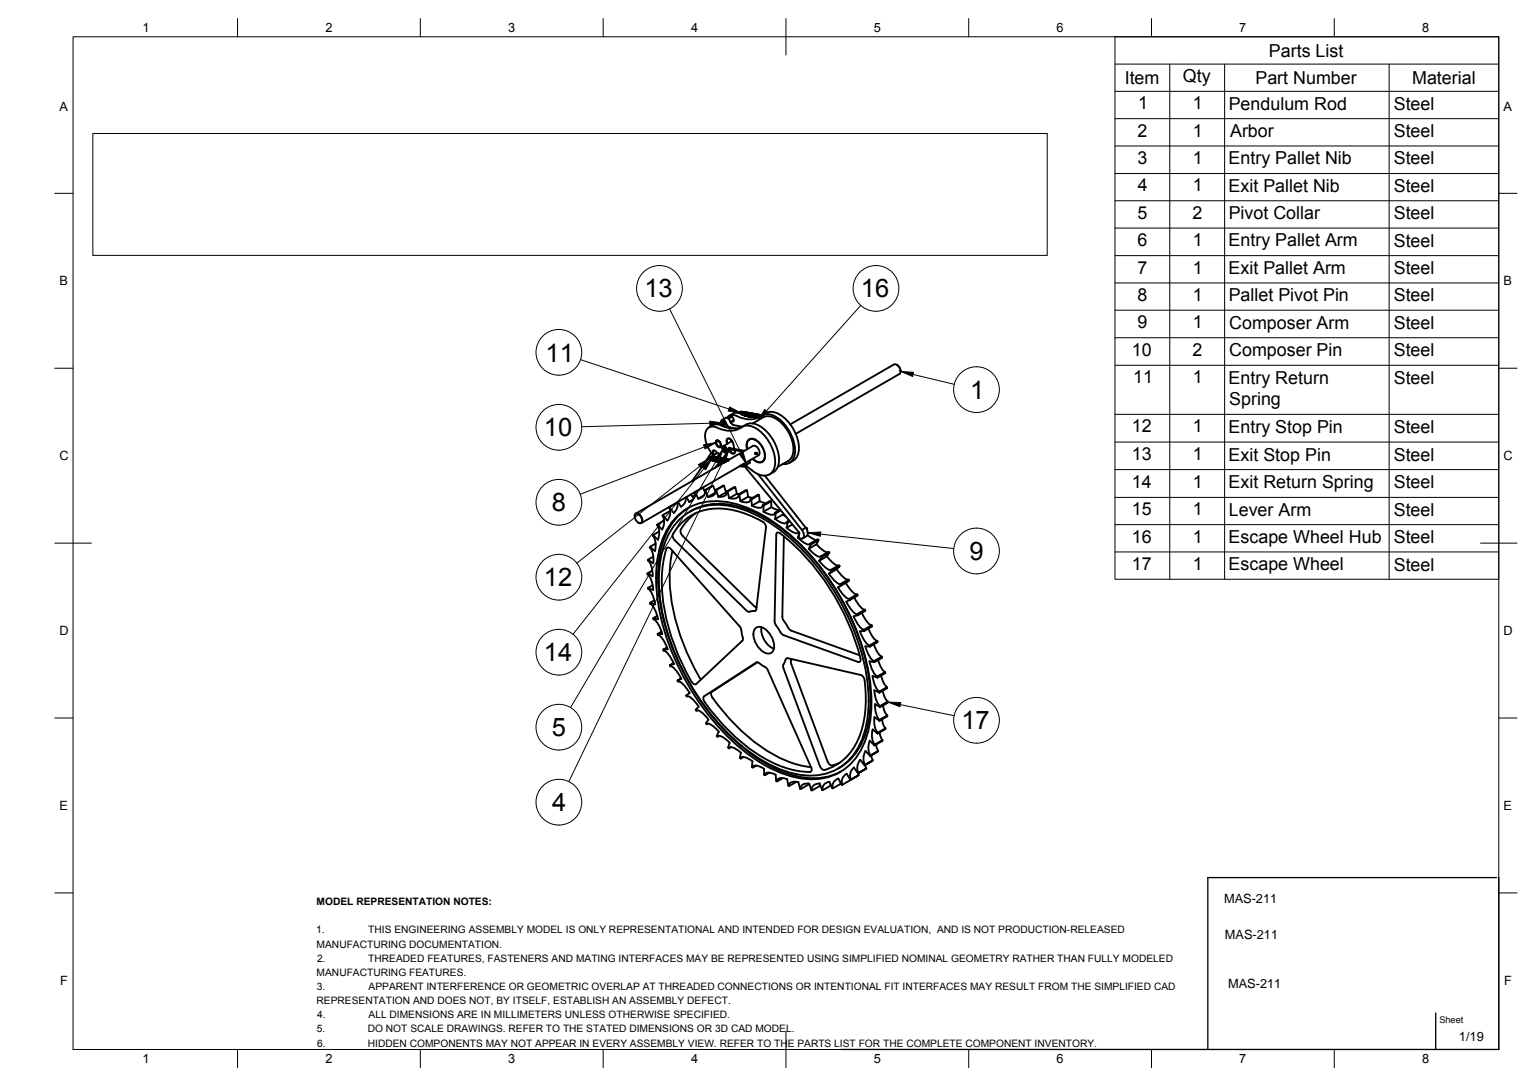
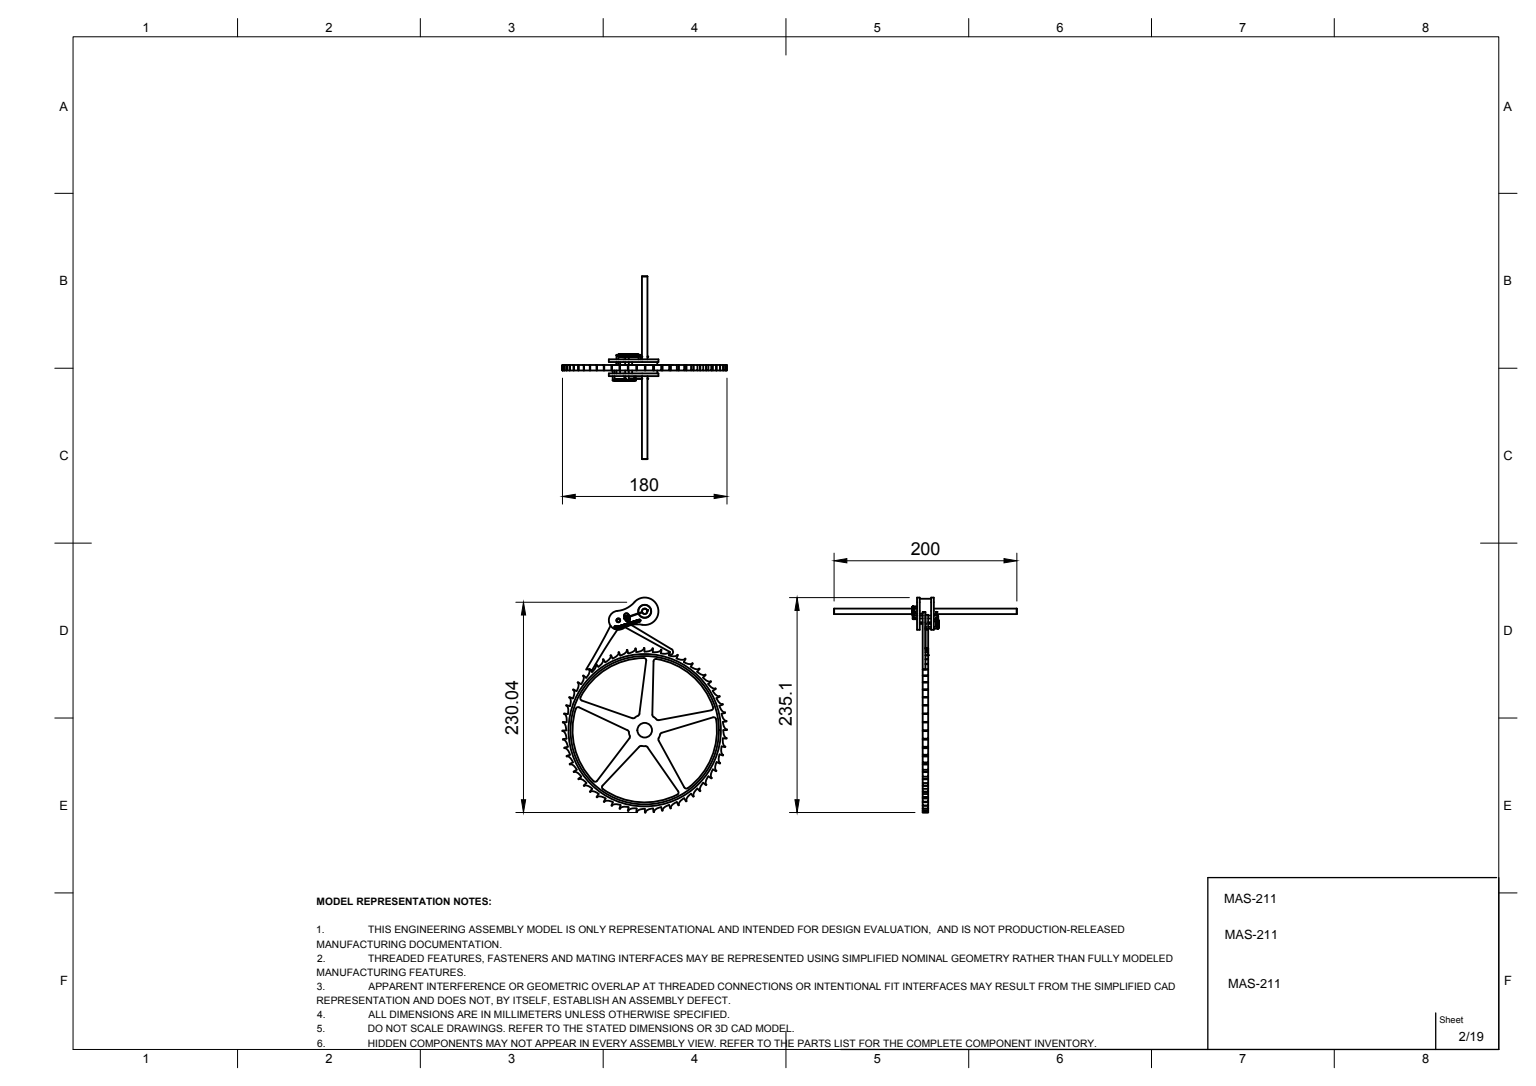
ISO-10303-21;
HEADER;
FILE_DESCRIPTION(
 (''),
 '2;1');
FILE_NAME ( 'MAS-211', '2026-10-05T20:07:59+06:00', ( '' ), ( '' ), 'STEP AP214', 'Unspecified', '' );
FILE_SCHEMA (('AUTOMOTIVE_DESIGN { 1 0 10303 214 3 1 1 }'));
ENDSEC;
DATA;
#10 = MECHANICAL_DESIGN_GEOMETRIC_PRESENTATION_REPRESENTATION('',(#319,#320,
#321,#322,#323,#324,#325,#326,#327,#328,#329,#330,#331,#332,#333,#334,#335,
#336,#337),#196741) ;
#17 = (
BOUNDED_CURVE()
B_SPLINE_CURVE(2,(#114139,#114140,#114141,#114142,#114143,#114144,#114145,
#114146,#114147),.UNSPECIFIED.,.F.,.F.)
B_SPLINE_CURVE_WITH_KNOTS((3,2,2,2,3),(1.42918797785348,1.62618617063892,
1.86180561965816,2.09742506867739,2.29442326146283),.UNSPECIFIED.)
CURVE()
GEOMETRIC_REPRESENTATION_ITEM()
RATIONAL_B_SPLINE_CURVE((1.,1.,1.,0.707106781186548,1.,0.707106781186548,
1.,1.,1.))
REPRESENTATION_ITEM('')
) ;
#18 = (
BOUNDED_CURVE()
B_SPLINE_CURVE(2,(#114327,#114328,#114329,#114330,#114331,#114332,#114333,
#114334,#114335),.UNSPECIFIED.,.F.,.F.)
B_SPLINE_CURVE_WITH_KNOTS((3,2,2,2,3),(1.42918797785348,1.62618617063892,
1.86180561965816,2.09742506867739,2.29442326146283),.UNSPECIFIED.)
CURVE()
GEOMETRIC_REPRESENTATION_ITEM()
RATIONAL_B_SPLINE_CURVE((1.,1.,1.,0.707106781186548,1.,0.707106781186548,
1.,1.,1.))
REPRESENTATION_ITEM('')
) ;
#19 = (
BOUNDED_CURVE()
B_SPLINE_CURVE(3,(#132841,#132842,#132843,#132844,#132845,#132846,#132847,
#132848,#132849,#132850,#132851,#132852,#132853,#132854,#132855,#132856,
#132857,#132858,#132859,#132860,#132861,#132862,#132863,#132864,#132865,
#132866,#132867,#132868,#132869,#132870,#132871,#132872,#132873,#132874,
#132875,#132876,#132877,#132878,#132879,#132880,#132881,#132882,#132883,
#132884,#132885,#132886,#132887,#132888,#132889,#132890,#132891,#132892,
#132893,#132894,#132895,#132896,#132897,#132898,#132899,#132900,#132901,
#132902,#132903,#132904,#132905,#132906,#132907,#132908,#132909,#132910,
#132911,#132912,#132913,#132914,#132915,#132916,#132917,#132918,#132919,
#132920,#132921,#132922,#132923,#132924,#132925,#132926,#132927,#132928,
#132929,#132930,#132931,#132932,#132933,#132934,#132935,#132936,#132937,
#132938,#132939,#132940,#132941,#132942,#132943,#132944,#132945,#132946,
#132947,#132948,#132949,#132950,#132951,#132952,#132953,#132954,#132955,
#132956,#132957,#132958,#132959,#132960,#132961,#132962,#132963,#132964,
#132965,#132966,#132967,#132968,#132969,#132970,#132971,#132972,#132973,
#132974,#132975,#132976,#132977,#132978,#132979,#132980,#132981,#132982,
#132983,#132984,#132985,#132986,#132987,#132988,#132989,#132990,#132991,
#132992,#132993,#132994,#132995,#132996,#132997,#132998,#132999,#133000,
#133001,#133002,#133003,#133004,#133005,#133006,#133007,#133008,#133009,
#133010,#133011,#133012,#133013,#133014,#133015,#133016,#133017,#133018,
#133019,#133020,#133021,#133022,#133023,#133024,#133025,#133026,#133027,
#133028,#133029,#133030,#133031,#133032,#133033,#133034,#133035,#133036,
#133037,#133038,#133039,#133040,#133041,#133042,#133043,#133044,#133045,
#133046,#133047,#133048,#133049,#133050,#133051,#133052,#133053,#133054,
#133055,#133056,#133057,#133058,#133059,#133060,#133061,#133062,#133063,
#133064,#133065,#133066,#133067,#133068,#133069,#133070,#133071,#133072,
#133073,#133074,#133075,#133076,#133077,#133078,#133079,#133080,#133081,
#133082,#133083,#133084,#133085,#133086,#133087,#133088,#133089,#133090,
#133091,#133092,#133093,#133094,#133095,#133096,#133097,#133098,#133099,
#133100,#133101,#133102,#133103,#133104,#133105,#133106,#133107,#133108,
#133109,#133110,#133111,#133112,#133113,#133114,#133115,#133116,#133117,
#133118,#133119,#133120,#133121,#133122,#133123,#133124,#133125,#133126,
#133127,#133128,#133129,#133130,#133131,#133132,#133133,#133134,#133135,
#133136,#133137,#133138,#133139,#133140,#133141,#133142,#133143,#133144,
#133145,#133146,#133147,#133148,#133149,#133150,#133151,#133152,#133153,
#133154,#133155,#133156,#133157,#133158,#133159,#133160,#133161,#133162,
#133163,#133164,#133165,#133166,#133167,#133168,#133169,#133170,#133171,
#133172,#133173,#133174,#133175,#133176,#133177,#133178,#133179,#133180,
#133181,#133182,#133183,#133184,#133185,#133186,#133187,#133188,#133189,
#133190,#133191,#133192,#133193,#133194,#133195,#133196,#133197,#133198,
#133199,#133200,#133201,#133202,#133203,#133204,#133205,#133206,#133207,
#133208,#133209,#133210,#133211,#133212,#133213,#133214,#133215,#133216,
#133217,#133218,#133219,#133220,#133221,#133222,#133223,#133224,#133225,
#133226,#133227,#133228,#133229,#133230,#133231,#133232,#133233,#133234,
#133235,#133236,#133237,#133238,#133239,#133240,#133241,#133242,#133243,
#133244,#133245,#133246,#133247,#133248,#133249,#133250,#133251,#133252,
#133253,#133254,#133255,#133256,#133257,#133258,#133259,#133260,#133261,
#133262,#133263,#133264,#133265,#133266,#133267,#133268,#133269,#133270,
#133271,#133272,#133273,#133274,#133275,#133276,#133277,#133278,#133279,
#133280,#133281,#133282,#133283,#133284,#133285,#133286,#133287,#133288,
#133289,#133290,#133291,#133292,#133293,#133294,#133295,#133296,#133297,
#133298,#133299,#133300,#133301,#133302,#133303,#133304,#133305,#133306,
#133307,#133308,#133309,#133310,#133311,#133312,#133313,#133314,#133315,
#133316,#133317,#133318,#133319,#133320,#133321,#133322,#133323,#133324,
#133325,#133326,#133327,#133328,#133329,#133330,#133331,#133332,#133333,
#133334,#133335,#133336,#133337,#133338,#133339,#133340,#133341,#133342,
#133343,#133344,#133345,#133346,#133347,#133348,#133349,#133350,#133351,
#133352,#133353,#133354,#133355,#133356,#133357,#133358,#133359,#133360,
#133361,#133362,#133363,#133364,#133365,#133366,#133367,#133368,#133369,
#133370,#133371,#133372,#133373,#133374,#133375,#133376,#133377,#133378,
#133379,#133380,#133381,#133382,#133383,#133384,#133385,#133386,#133387,
#133388,#133389,#133390,#133391,#133392,#133393,#133394,#133395,#133396,
#133397,#133398,#133399,#133400,#133401,#133402,#133403,#133404,#133405,
#133406,#133407,#133408,#133409,#133410,#133411,#133412,#133413,#133414,
#133415,#133416,#133417,#133418,#133419,#133420,#133421,#133422,#133423,
#133424,#133425,#133426,#133427,#133428,#133429,#133430,#133431,#133432,
#133433,#133434,#133435,#133436,#133437,#133438,#133439,#133440,#133441,
#133442,#133443,#133444,#133445,#133446,#133447,#133448,#133449,#133450,
#133451,#133452,#133453,#133454,#133455,#133456,#133457,#133458,#133459,
#133460,#133461,#133462,#133463,#133464,#133465,#133466,#133467,#133468,
#133469,#133470,#133471,#133472,#133473,#133474,#133475,#133476,#133477,
#133478,#133479,#133480,#133481,#133482,#133483,#133484,#133485,#133486,
#133487,#133488,#133489,#133490,#133491,#133492,#133493,#133494,#133495,
#133496,#133497,#133498,#133499,#133500,#133501,#133502,#133503,#133504,
#133505,#133506,#133507,#133508,#133509,#133510,#133511,#133512,#133513,
#133514,#133515,#133516,#133517,#133518,#133519,#133520,#133521,#133522,
#133523,#133524,#133525,#133526,#133527,#133528,#133529,#133530,#133531,
#133532,#133533,#133534,#133535,#133536,#133537,#133538,#133539,#133540,
#133541,#133542,#133543,#133544,#133545,#133546,#133547,#133548,#133549,
#133550,#133551,#133552,#133553,#133554,#133555,#133556,#133557,#133558,
#133559,#133560,#133561,#133562,#133563,#133564,#133565,#133566,#133567,
#133568,#133569,#133570,#133571,#133572,#133573,#133574,#133575,#133576,
#133577,#133578,#133579,#133580,#133581,#133582,#133583,#133584,#133585,
#133586,#133587,#133588,#133589,#133590,#133591,#133592,#133593,#133594,
#133595,#133596,#133597,#133598,#133599,#133600,#133601,#133602,#133603,
#133604,#133605,#133606,#133607,#133608,#133609,#133610,#133611,#133612,
#133613,#133614,#133615,#133616,#133617,#133618,#133619,#133620,#133621,
#133622,#133623,#133624,#133625,#133626,#133627,#133628,#133629,#133630,
#133631,#133632,#133633,#133634,#133635,#133636,#133637,#133638,#133639,
#133640,#133641,#133642,#133643,#133644,#133645,#133646,#133647,#133648,
#133649,#133650,#133651,#133652,#133653,#133654,#133655,#133656,#133657,
#133658,#133659,#133660,#133661,#133662,#133663,#133664,#133665,#133666,
#133667,#133668,#133669,#133670,#133671,#133672,#133673,#133674,#133675,
#133676,#133677,#133678,#133679,#133680,#133681,#133682,#133683,#133684,
#133685,#133686,#133687,#133688,#133689,#133690,#133691,#133692,#133693,
#133694,#133695,#133696,#133697,#133698,#133699,#133700,#133701,#133702,
#133703,#133704,#133705,#133706,#133707,#133708,#133709,#133710,#133711,
#133712,#133713,#133714,#133715,#133716,#133717,#133718,#133719,#133720,
#133721,#133722,#133723,#133724,#133725,#133726,#133727,#133728,#133729,
#133730,#133731,#133732,#133733,#133734,#133735,#133736,#133737,#133738,
#133739,#133740,#133741,#133742,#133743,#133744,#133745,#133746,#133747,
#133748,#133749,#133750,#133751,#133752,#133753,#133754,#133755,#133756,
#133757,#133758,#133759,#133760,#133761,#133762,#133763,#133764,#133765,
#133766,#133767,#133768,#133769,#133770,#133771,#133772,#133773,#133774,
#133775,#133776,#133777,#133778,#133779,#133780,#133781,#133782,#133783,
#133784,#133785,#133786,#133787,#133788,#133789,#133790,#133791,#133792,
#133793,#133794,#133795,#133796,#133797,#133798,#133799,#133800,#133801,
#133802,#133803,#133804,#133805,#133806,#133807,#133808,#133809,#133810,
#133811,#133812,#133813,#133814,#133815,#133816,#133817,#133818,#133819,
#133820,#133821,#133822,#133823,#133824,#133825,#133826,#133827,#133828,
#133829,#133830,#133831,#133832,#133833,#133834,#133835,#133836,#133837,
#133838,#133839,#133840,#133841,#133842,#133843,#133844,#133845,#133846,
#133847,#133848,#133849,#133850,#133851,#133852,#133853,#133854,#133855,
#133856,#133857,#133858,#133859,#133860,#133861,#133862,#133863,#133864,
#133865,#133866,#133867,#133868,#133869,#133870,#133871,#133872,#133873,
#133874,#133875,#133876,#133877,#133878,#133879,#133880,#133881,#133882,
#133883,#133884,#133885,#133886,#133887,#133888,#133889,#133890,#133891,
#133892,#133893,#133894,#133895,#133896,#133897,#133898),.UNSPECIFIED.,
 .F.,.F.)
B_SPLINE_CURVE_WITH_KNOTS((4,1,1,1,1,1,1,1,1,1,1,1,1,1,1,1,1,1,1,1,1,1,
1,1,1,1,1,1,1,1,1,1,1,1,1,1,1,1,1,1,1,1,1,1,1,1,1,1,1,1,1,1,1,1,1,1,1,1,
1,1,1,1,1,1,1,1,1,1,1,1,1,1,1,1,1,1,1,1,1,1,1,1,1,1,1,1,1,1,1,1,1,1,1,1,
1,1,1,1,1,1,1,1,1,1,1,1,1,1,1,1,1,1,1,1,1,1,1,1,1,1,1,1,1,1,1,1,1,1,1,1,
1,1,1,1,1,1,1,1,1,1,1,1,1,1,1,1,1,1,1,1,1,1,1,1,1,1,1,1,1,1,1,1,1,1,1,1,
1,1,1,1,1,1,1,1,1,1,1,1,1,1,1,1,1,1,1,1,1,1,1,1,1,1,1,1,1,1,1,1,1,1,1,1,
1,1,1,1,1,1,1,1,1,1,1,1,1,1,1,1,1,1,1,1,1,1,1,1,1,1,1,1,1,1,1,1,1,1,1,1,
1,1,1,1,1,1,1,1,1,1,1,1,1,1,1,1,1,1,1,1,1,1,1,1,1,1,1,1,1,1,1,1,1,1,1,1,
1,1,1,1,1,1,1,1,1,1,1,1,1,1,1,1,1,1,1,1,1,1,1,1,1,1,1,1,1,1,1,1,1,1,1,1,
1,1,1,1,1,1,1,1,1,1,1,1,1,1,1,1,1,1,1,1,1,1,1,1,1,1,1,1,1,1,1,1,1,1,1,1,
1,1,1,1,1,1,1,1,1,1,1,1,1,1,1,1,1,1,1,1,1,1,1,1,1,1,1,1,1,1,1,1,1,1,1,1,
1,1,1,1,1,1,1,1,1,1,1,1,1,1,1,1,1,1,1,1,1,1,1,1,1,1,1,1,1,1,1,1,1,1,1,1,
1,1,1,1,1,1,1,1,1,1,1,1,1,1,1,1,1,1,1,1,1,1,1,1,1,1,1,1,1,1,1,1,1,1,1,1,
1,1,1,1,1,1,1,1,1,1,1,1,1,1,1,1,1,1,1,1,1,1,1,1,1,1,1,1,1,1,1,1,1,1,1,1,
1,1,1,1,1,1,1,1,1,1,1,1,1,1,1,1,1,1,1,1,1,1,1,1,1,1,1,1,1,1,1,1,1,1,1,1,
1,1,1,1,1,1,1,1,1,1,1,1,1,1,1,1,1,1,1,1,1,1,1,1,1,1,1,1,1,1,1,1,1,1,1,1,
1,1,1,1,1,1,1,1,1,1,1,1,1,1,1,1,1,1,1,1,1,1,1,1,1,1,1,1,1,1,1,1,1,1,1,1,
1,1,1,1,1,1,1,1,1,1,1,1,1,1,1,1,1,1,1,1,1,1,1,1,1,1,1,1,1,1,1,1,1,1,1,1,
1,1,1,1,1,1,1,1,1,1,1,1,1,1,1,1,1,1,1,1,1,1,1,1,1,1,1,1,1,1,1,1,1,1,1,1,
1,1,1,1,1,1,1,1,1,1,1,1,1,1,1,1,1,1,1,1,1,1,1,1,1,1,1,1,1,1,1,1,1,1,1,1,
1,1,1,1,1,1,1,1,1,1,1,1,1,1,1,1,1,1,1,1,1,1,1,1,1,1,1,1,1,1,1,1,1,1,1,1,
1,1,1,1,1,1,1,1,1,1,1,1,1,1,1,1,1,1,1,1,1,1,1,1,1,1,1,1,1,1,1,1,1,1,1,1,
1,1,1,1,1,1,1,1,1,1,1,1,1,1,1,1,1,1,1,1,1,1,1,1,1,1,1,1,1,1,1,1,1,1,1,1,
1,1,1,1,1,1,1,1,1,1,1,1,1,1,1,1,1,1,1,1,1,1,1,1,1,1,1,1,1,1,1,1,1,1,1,1,
1,1,1,1,1,1,1,1,1,1,1,1,1,1,1,1,1,1,1,1,1,1,1,1,1,1,1,1,1,1,1,1,1,1,1,1,
1,1,1,1,1,1,1,1,1,1,1,1,1,1,1,1,1,1,1,1,1,1,1,1,1,1,1,1,1,1,1,1,1,1,1,1,
1,1,1,1,1,1,1,1,1,1,1,1,1,1,1,1,1,1,1,1,1,1,1,1,1,1,1,1,1,1,1,1,1,1,1,1,
1,1,1,1,1,1,1,1,1,1,1,1,1,1,1,1,1,1,1,1,1,1,1,1,1,1,1,1,1,1,1,1,1,1,1,1,
1,1,1,1,1,1,1,1,1,1,1,1,1,1,1,1,1,1,1,1,1,1,1,1,1,1,1,1,1,1,1,1,1,1,1,1,
1,1,1,1,1,1,1,1,1,1,1,1,1,1,1,1,1,1,1,1,1,1,1,1,1,4),(0.,0.01797683372391,
0.286633051710584,0.555289278308216,0.823945516665782,1.09260176953922,
1.36125803873948,1.62991432588463,1.89857063164012,2.16722695661301,2.43588330050525,
2.70453966304674,2.9731960431531,3.24185243981471,3.51050885133453,3.77916527610465,
4.04782171198515,4.31647815691489,4.58513460847725,4.85379106430677,5.12244752187208,
5.39110397865606,5.65976043217153,5.92841687990537,6.19707331956994,6.46572974881596,
6.73438616570634,7.00304256821933,7.2716989549161,7.5403553242696,7.809011675483,
8.07766800769526,8.34632432089157,8.61498061505147,8.8836368910788,9.15229314997201,
9.4209493936865,9.68960562442157,9.95826184531348,10.226918059948,10.4955742727586,
10.7642304884925,11.0328867113173,11.3015429448574,11.5701991918227,11.8388554546081,
12.1075117346518,12.3761680332469,12.6448243507434,12.9134806874637,13.1821370428496,
13.450793416388,13.7194498067883,13.9881062128412,14.2567626326955,14.5254190645885,
14.7940755062772,15.0627319555912,15.3313884100611,15.6000448672586,15.8687013246492,
16.1373577797,16.4060142299691,16.6746706729765,16.9433271065265,17.2119835283531,
17.4806399366567,17.7492963295502,18.0179527057767,18.286609063996,18.555265403637,
18.8239217240786,19.0925780255742,19.3612343083975,19.6298905737625,19.898546823017,
20.1672030584666,20.4358592827168,20.7045154992928,20.973171712245,21.2418279262962,
21.5104841459723,21.7791403749736,22.0477966165324,22.316452872948,22.585109146262,
22.8537654375589,23.1224217478187,23.3910780770929,23.6597344254327,23.9283907920352,
24.197047176159,24.4657035763222,24.7343599911301,25.0030164185931,25.2716728568073,
25.5403293034427,25.8089857562333,26.0776422126729,26.3462986702843,26.6149551265448,
26.8836115789212,27.1522680250308,27.4209244624423,27.6895808890659,27.9582373027346,
28.2268937018004,28.4955500845261,28.7642064498512,29.0328627966379,29.3015191245544,
29.5701754332357,29.838831723217,30.1074879950829,30.3761442503694,30.6448004907916,
30.9134567190168,31.1821129380756,31.450769151893,31.7194253649682,31.9880815819663,
32.2567378070174,32.5253940433706,32.7940502938785,33.0627065604467,33.3313628447765,
33.6000191476151,33.8686754696427,34.1373318106287,34.405988170366,34.6746445478242,
34.9433009420458,35.2119573513747,35.480613774244,35.7492702085419,36.0179266522368,
36.2865831029275,36.5552395582669,36.8238960157264,37.0925524727952,37.3612089269773,
37.6298653757534,37.8985218168153,38.1671782477952,38.4358346667239,38.7044910715485,
38.9731474607866,39.2418038328672,39.5104601869391,39.7791165220837,40.0477728382212,
40.3164291352602,40.5850854140292,40.8537416754418,41.1223979213679,41.3910541539077,
41.6597103761025,41.9283665914244,42.1970228042084,42.4656790192,42.7343352406829,
43.0029914723808,43.2716477171096,43.540303977354,43.8089602546436,44.0776165503516,
44.3462728649052,44.614929198697,44.883585551232,45.1522419220568,45.4208983099307,
45.6895547136931,45.9582111315299,46.2268675617156,46.4955240020317,46.7641804503338,
47.0328369041642,47.3014933611089,47.5701498186329,47.8388062742058,48.107462725373,
48.3761191696448,48.6447756048012,48.9134320285537,49.1820884390673,49.4507448344197,
49.7194012133072,49.9880575743413,50.2567139168934,50.5253702402807,50.7940265446884,
51.0626828303152,51.3313390982961,51.5999953498901,51.8686515873141,52.1373078130706,
52.4059640305862,52.6746202437936,52.9432764573682,53.211932675918,53.480588903259,
53.7492451427202,54.0179013967021,54.2865576673334,54.5552139557853,54.823870263115,
55.0925265894471,55.3611829348992,55.6298392987282,55.8984956802486,56.1671520780245,
56.4358084907065,56.7044649163381,56.9731213530494,57.2417777985307,57.5104342505384,
57.7790907065743,58.0477471641719,58.3164036208043,58.5850600739368,58.8537165211707,
59.1223729600609,59.39102938849,59.6596858042645,59.9283422056975,60.1969985910129,
60.4656549590995,60.7343113087676,61.0029676396243,61.2716239512389,61.540280244075,
61.808936518638,62.0775927763821,62.3462490189291,62.6149052488546,62.8835614690812,
63.1522176834332,63.4208738963055,63.6895301124163,63.9581863359981,64.2268425704115,
64.4954988186027,64.7641550825741,65.0328113641112,65.3014676640435,65.5701239831253,
65.8387803211949,66.1074366781083,66.3760930528907,66.6447494446373,66.9134058517341,
67.1820622726558,67.4507187053199,67.7193751477252,67.988031597487,68.256688052277,
68.5253445095709,68.7940009668648,69.0626574216546,69.3313138714164,69.5999703138218,
69.8686267464858,70.1372831674076,70.4059395745042,70.6745959662509,70.9432523410334,
71.2119086979469,71.4805650360164,71.7492213550982,72.0178776550306,72.2865339365675,
72.5551902005389,72.8238464487301,73.0925026831433,73.3611589067251,73.6298151228357,
73.8984713357081,74.1671275500599,74.4357837702864,74.7044400002118,74.9730962427587,
75.2417525005027,75.5104087750655,75.7790650679015,76.047721379516,76.3163777103726,
76.5850340600405,76.853690428127,77.1223468134422,77.391003214875,77.6596596306495,
77.9283160590784,78.1969724979684,78.4656289452021,78.7342853983344,79.0029418549666,
79.2715983125641,79.5402547685998,79.8089112206075,80.0775676660886,80.3462241027997,
80.6148805284312,80.8835369411131,81.1521933388889,81.4208497204091,81.689506084238,
81.9581624296899,82.2268187560219,82.4954750633515,82.7641313518033,83.0327876224345,
83.3014438764161,83.5701001158772,83.838756343218,84.1074125617677,84.3760687753422,
84.6447249885494,84.913381206065,85.1820374318212,85.4506936692451,85.719349920839,
85.9880061888197,86.2566624744465,86.5253187788541,86.7939751022413,87.0626314447932,
87.3312878058273,87.5999441847146,87.8686005800667,88.1372569905802,88.4059134143327,
88.6745698494889,88.9432262937606,89.2118827449277,89.4805392005005,89.7491956580243,
90.0178521149689,90.2865085687992,90.5551650171012,90.8238214574172,91.0924778876028,
91.3611343054394,91.6297907092016,91.8984470970753,92.1671034679,92.4357598204347,
92.7044161542264,92.9730724687798,93.2417287644878,93.5103850417773,93.7790413020216,
94.0476975467502,94.3163537784479,94.5850099999307,94.8536662149221,95.1223224277061,
95.390978643028,95.6596348652226,95.9282910977624,96.1969473436883,96.4656036051009,
96.7342598838697,97.0029161809086,97.2715724970461,97.5402288321905,97.8088851862623,
98.0775415583427,98.3461979475807,98.6148543524051,98.8835107713336,99.1521672023136,
99.4208236433754,99.6894800921513,99.9581365463333,100.226793003402,100.495449460861,
100.7641059162,101.032762366891,101.301418810586,101.570075244884,101.838731667753,
102.107388077082,102.376044471303,102.644700848761,102.913357208498,103.182013549484,
103.450669871511,103.71932617435,103.98798245868,104.256638725248,104.525294975755,
104.793951212108,105.062607437159,105.331263654157,105.599919867233,105.86857608105,
106.137232300108,106.405888528334,106.674544768756,106.943201024042,107.211857295908,
107.480513585889,107.74916989457,108.017826222487,108.286482569273,108.555138934598,
108.823795317324,109.09245171639,109.361108130058,109.629764556682,109.898420994093,
110.167077440202,110.435733892579,110.704390348839,110.97304680645,111.24170326289,
111.51035971568,111.779016162316,112.04767260053,112.316329027993,112.5849854428,
112.853641842963,113.122298227087,113.39095459369,113.659610942029,113.928267271303,
114.196923581563,114.46557987286,114.734236146174,115.002892402589,115.271548644148,
115.540204873149,115.808861092825,116.077517306876,116.346173519828,116.614829736404,
116.883485960654,117.152142196103,117.420798445358,117.689454710722,117.958110993546,
118.226767295041,118.495423615483,118.764079955123,119.032736313343,119.301392689569,
119.570049082462,119.838705490766,120.107361912592,120.376018346142,120.644674789149,
120.913331239418,121.181987694469,121.45064415186,121.719300609057,121.987957063527,
122.256613512841,122.525269954529,122.793926386422,123.062582806276,123.331239212329,
123.599895602729,123.868551976268,124.137208331653,124.405864668374,124.67452098587,
124.943177284465,125.211833564508,125.480489827294,125.749146074259,126.017802307799,
126.286458530624,126.555114746357,126.823770959168,127.092427173802,127.361083394694,
127.629739625429,127.898395869143,128.167052128037,128.435708404064,128.704364698224,
128.97302101142,129.241677343633,129.510333694846,129.7789900642,130.047646450897,
130.31630285341,130.5849592703,130.853615699547,131.122272139211,131.390928586945,
131.659585040461,131.928241497245,132.19689795481,132.46555441064,132.734210862202,
133.002867307132,133.271523743013,133.540180167783,133.808836579303,134.077492975965,
134.346149356071,134.614805718613,134.883462062505,135.152118387478,135.420774693234,
135.689430980379,135.958087249579,136.226743502453,136.49539974081,136.76405596741,
137.032712185392,137.301368398783,137.570024612174,137.838680830155,138.107337056755,
138.375993295112,138.644649547986,138.913305817186,139.181962104332,139.450618410087,
139.71927473506,139.987931078952,140.256587441494,140.525243821601,140.793900218262,
141.062556629782,141.331213054552,141.599869490433,141.868525935363,142.137182386925,
142.405838842755,142.67449530032,142.943151757104,143.21180821062,143.480464658354,
143.749121098019,144.017777527265,144.286433944155,144.555090346668,144.823746733365,
145.092403102719,145.361059453932,145.629715786145,145.898372099341,146.167028393501,
146.435684669529,146.704340928422,146.972997172137,147.241653402872,147.510309623764,
147.778965838398,148.047622051209,148.316278266943,148.584934489768,148.853590723308,
149.122246970274,149.390903233059,149.659559513103,149.928215811698,150.196872129195,
150.465528465915,150.734184821301,151.00284119484,151.27149758524,151.540153991293,
151.808810411148,152.077466843041,152.34612328473,152.614779734044,152.883436188514,
153.152092645711,153.420749103102,153.689405558153,153.958062008422,154.22671845143,
154.49537488498,154.764031306806,155.03268771511,155.301344108004,155.57000048423,
155.838656842449,156.107313182091,156.375969502532,156.644625804028,156.913282086851,
157.181938352216,157.450594601471,157.719250836921,157.987907061171,158.256563277747,
158.525219490699,158.793875704751,159.062531924427,159.331188153428,159.599844394987,
159.868500651403,160.137156924717,160.405813216014,160.674469526274,160.943125855548,
161.211782203888,161.480438570491,161.749094954615,162.017751354778,162.286407769586,
162.555064197049,162.823720635263,163.092377081899,163.361033534689,163.629689991129,
163.898346448741,164.167002905001,164.435659357378,164.704315803488,164.972972240899,
165.241628667523,165.510285081192,165.778941480257,166.047597862983,166.316254228308,
166.584910575095,166.853566903012,167.122223211693,167.390879501675,167.659535773541,
167.928192028827,168.19684826925,168.465504497475,168.734160716534,169.002816930351,
169.271473143427,169.540129360425,169.808785585476,170.077441821829,170.346098072337,
170.614754338905,170.883410623235,171.152066926074,171.420723248102,171.689379589088,
171.958035948825,172.226692326284,172.495348720505,172.764005129834,173.032661552704,
173.301317987002,173.569974430697,173.838630881388,174.107287336727,174.375943794187,
174.644600251255,174.913256705437,175.181913154214,175.450569595276,175.719226026256,
175.987882445184,176.256538850009,176.525195239247,176.793851611328,177.0625079654,
177.331164300545,177.599820616682,177.868476913721,178.137133192491,178.405789453903,
178.674445699829,178.943101932369,179.211758154564,179.480414369886,179.74907058267,
180.017726797662,180.286383019145,180.555039250843,180.823695495572,181.092351755816,
181.361008033106,181.629664328814,181.898320643368,182.16697697716,182.435633329695,
182.70428970052,182.972946088394,183.241602492156,183.510258909993,183.778915340179,
184.047571780495,184.316228228797,184.584884682628,184.853541139572,185.122197597096,
185.39085405267,185.659510503837,185.928166948109,186.196823383265,186.465479807018,
186.734136217531,187.002792612884,187.271448991771,187.540105352806,187.808761695358,
188.077418018745,188.346074323153,188.61473060878,188.883386876761,189.152043128355,
189.420699365779,189.689355591536,189.958011809051,190.226668022259,190.495324235834,
190.763980454383,191.032636681725,191.301292921186,191.569949175168,191.838605445799,
192.107261734251,192.375918041581,192.644574367913,192.913230713365,193.181887077194,
193.450543458715,193.719199856491,193.987856269173,194.256512694805,194.525169131516,
194.793825576997,195.062482029005,195.331138485041,195.599794942639,195.868451399271,
196.137107852404,196.405764299638,196.674420738528,196.943077166957,197.211733582732,
197.480389984165,197.749046369481,198.017702737567,198.286359087236,198.555015418092,
198.823671729707,199.092328022543,199.360984297106,199.62964055485,199.898296797397,
200.166953027323,200.43560924755,200.704265461902,200.972921674774,201.241577890885,
201.510234114467,201.77889034888,202.047546597072,202.316202861043,202.584859142581,
202.853515442513,203.122171761595,203.390828099665,203.659484456579,203.928140831361,
204.196797223108,204.465453630205,204.734110051127,205.002766483791,205.271422926197,
205.540079375959,205.808735830749,206.077392288043,206.346048745337,206.614705200127,
206.883361649889,207.152018092295,207.420674524959,207.689330945881,207.957987352978,
208.226643744725,208.495300119508,208.763956476421,209.032612814491,209.301269133573,
209.569925433505,209.838581715043,210.107237979014,210.375894227206,210.644550461619,
210.913206685201,211.181862901312,211.450519114184,211.719175328536,211.987831548763,
212.256487778689,212.525144021236,212.79380027898,213.062456553543,213.331112846379,
213.599769157994,213.868425488851,214.137081838519,214.405738206606,214.674394591921,
214.943050993354,215.211707409129,215.480363837558,215.749020276448,216.017676723682,
216.286333176815,216.554989633447,216.823646091045,217.092302547081,217.360958999089,
217.62961544457,217.898271881281,218.166928306913,218.435584719595,218.704241117371,
218.972897498892,219.241553862721,219.510210208173,219.778866534505,220.047522841835,
220.316179130287,220.584835400918,220.8534916549,221.122147894361,221.390804121702,
221.659460340252,221.928116553827,222.196772767034,222.46542898455,222.734085210306,
223.00274144773,223.271397699324,223.540053967305,223.808710252932,224.07736655734,
224.346022880728,224.61467922328,224.883335584314,225.151991963201,225.420648358554,
225.689304769068,225.95796119282,226.226617627977,226.495274072249,226.763930523416,
227.032586978989,227.301243436513,227.569899893458,227.838556347288,228.10721279559,
228.375869235907,228.644525666093,228.913182083929,229.181838487692,229.450494875566,
229.719151246391,229.987807598926,230.256463932718,230.525120247271,230.79377654298,
231.062432820269,231.331089080514,231.599745325243,231.868401556941,232.137057778424,
232.405713993415,232.674370206199,232.943026421521,233.211682643716,233.480338876256,
233.748995122182,234.017651383595,234.286307662364,234.554963959403,234.823620275541,
235.092276610685,235.360932964757,235.629589336838,235.898245726076,236.166902130901,
236.43555854983,236.70421498081,236.972871421872,237.241527870648,237.51018432483,
237.778840781899,238.047497239359,238.316153694698,238.584810145389,238.853466589084,
239.122123023382,239.390779446251,239.65943585558,239.928092249802,240.19674862726,
240.465404986998,240.734061327984,241.002717650011,241.27137395285,241.54003023718,
241.808686503748,242.077342754256,242.345998990609,242.614655215661,242.883311432659,
243.151967645734,243.420623859552,243.68928007861,243.957936306836,244.226592547258,
244.495248802545,244.763905074411,245.032561364392,245.301217673074,245.56987400099,
245.838530347777,246.107186713102,246.375843095828,246.644499494894,246.913155908563,
247.181812335186,247.450468772598,247.719125218708,247.987781671084,248.256438127345,
248.525094584956,248.793751041396,249.062407494187,249.331063940822,249.599720379036,
249.8683768065,250.137033221308,250.405689621471,250.674346005595,250.943002372197,
251.211658720537,251.480315049812,251.748971360071,252.017627651368,252.286283924683,
252.554940181098,252.823596422657,253.092252651658,253.360908871335,253.629565085386,
253.898221298338,254.166877514914,254.435533739165,254.704189974614,254.972846223869,
255.241502489234,255.510158772057,255.778815073553,256.047471393995,256.316127733635,
256.584784091854,256.85344046808,257.122096860973,257.390753269276,257.659409691102,
257.928066124652,258.196722567659,258.465379017928,258.734035472978,259.002691930368,
259.271348387566,259.540004842035,259.808661291349,260.077317733037,260.345974164929,
260.614630584783,260.883286990836,261.151943381235,261.420599754774,261.689256110159,
261.957912446879,262.226568764375,262.49522506297,262.763881343014,263.032537605798,
263.301193852763,263.569850086303,263.838506309127,264.107162524861,264.375818737671,
264.644474952305,264.913131173196,265.181787403931,265.450443647645,265.719099906538,
265.987756182565,266.256412476724,266.52506878992,266.793725122132,267.062381473345,
267.331037842698,267.599694229394,267.868350631907,268.137007048797,268.405663478042,
268.674319917706,268.94297636544,269.211632818955,269.480289275739,269.748945733304,
270.017602189133,270.286258640695,270.554915085624,270.823571521504,271.092227946274,
271.360884357793,271.629540754454,271.89819713456,272.166853497101,272.435509840993,
272.704166165965,272.97282247172,273.241478758865,273.510135028065,273.778791280938,
274.047447519295,274.316103745894,274.584759963875,274.853416177266,275.122072390656,
275.390728608637,275.659384835237,275.928041073593,276.196697326466,276.465353595666,
276.734009882811,277.002666188566,277.271322513539,277.53997885743,277.808635219972,
278.077291600077,278.345947996739,278.614604408258,278.883260833028,279.151917268908,
279.420573713837,279.689230165399,279.957886621228,280.226543078793,280.495199535576,
280.763855989092,281.032512436825,281.301168876489,281.569825305735,281.838481722625,
282.107138125138,282.375794511834,282.644450881187,282.9131072324,283.140531716307),
 .UNSPECIFIED.)
CURVE()
GEOMETRIC_REPRESENTATION_ITEM()
RATIONAL_B_SPLINE_CURVE((1.,1.,1.,1.,1.,1.,1.,1.,1.,1.,1.,1.,1.,1.,1.,1.,
1.,1.,1.,1.,1.,1.,1.,1.,1.,1.,1.,1.,1.,1.,1.,1.,1.,1.,1.,1.,1.,1.,1.,1.,
1.,1.,1.,1.,1.,1.,1.,1.,1.,1.,1.,1.,1.,1.,1.,1.,1.,1.,1.,1.,1.,1.,1.,1.,
1.,1.,1.,1.,1.,1.,1.,1.,1.,1.,1.,1.,1.,1.,1.,1.,1.,1.,1.,1.,1.,1.,1.,1.,
1.,1.,1.,1.,1.,1.,1.,1.,1.,1.,1.,1.,1.,1.,1.,1.,1.,1.,1.,1.,1.,1.,1.,1.,
1.,1.,1.,1.,1.,1.,1.,1.,1.,1.,1.,1.,1.,1.,1.,1.,1.,1.,1.,1.,1.,1.,1.,1.,
1.,1.,1.,1.,1.,1.,1.,1.,1.,1.,1.,1.,1.,1.,1.,1.,1.,1.,1.,1.,1.,1.,1.,1.,
1.,1.,1.,1.,1.,1.,1.,1.,1.,1.,1.,1.,1.,1.,1.,1.,1.,1.,1.,1.,1.,1.,1.,1.,
1.,1.,1.,1.,1.,1.,1.,1.,1.,1.,1.,1.,1.,1.,1.,1.,1.,1.,1.,1.,1.,1.,1.,1.,
1.,1.,1.,1.,1.,1.,1.,1.,1.,1.,1.,1.,1.,1.,1.,1.,1.,1.,1.,1.,1.,1.,1.,1.,
1.,1.,1.,1.,1.,1.,1.,1.,1.,1.,1.,1.,1.,1.,1.,1.,1.,1.,1.,1.,1.,1.,1.,1.,
1.,1.,1.,1.,1.,1.,1.,1.,1.,1.,1.,1.,1.,1.,1.,1.,1.,1.,1.,1.,1.,1.,1.,1.,
1.,1.,1.,1.,1.,1.,1.,1.,1.,1.,1.,1.,1.,1.,1.,1.,1.,1.,1.,1.,1.,1.,1.,1.,
1.,1.,1.,1.,1.,1.,1.,1.,1.,1.,1.,1.,1.,1.,1.,1.,1.,1.,1.,1.,1.,1.,1.,1.,
1.,1.,1.,1.,1.,1.,1.,1.,1.,1.,1.,1.,1.,1.,1.,1.,1.,1.,1.,1.,1.,1.,1.,1.,
1.,1.,1.,1.,1.,1.,1.,1.,1.,1.,1.,1.,1.,1.,1.,1.,1.,1.,1.,1.,1.,1.,1.,1.,
1.,1.,1.,1.,1.,1.,1.,1.,1.,1.,1.,1.,1.,1.,1.,1.,1.,1.,1.,1.,1.,1.,1.,1.,
1.,1.,1.,1.,1.,1.,1.,1.,1.,1.,1.,1.,1.,1.,1.,1.,1.,1.,1.,1.,1.,1.,1.,1.,
1.,1.,1.,1.,1.,1.,1.,1.,1.,1.,1.,1.,1.,1.,1.,1.,1.,1.,1.,1.,1.,1.,1.,1.,
1.,1.,1.,1.,1.,1.,1.,1.,1.,1.,1.,1.,1.,1.,1.,1.,1.,1.,1.,1.,1.,1.,1.,1.,
1.,1.,1.,1.,1.,1.,1.,1.,1.,1.,1.,1.,1.,1.,1.,1.,1.,1.,1.,1.,1.,1.,1.,1.,
1.,1.,1.,1.,1.,1.,1.,1.,1.,1.,1.,1.,1.,1.,1.,1.,1.,1.,1.,1.,1.,1.,1.,1.,
1.,1.,1.,1.,1.,1.,1.,1.,1.,1.,1.,1.,1.,1.,1.,1.,1.,1.,1.,1.,1.,1.,1.,1.,
1.,1.,1.,1.,1.,1.,1.,1.,1.,1.,1.,1.,1.,1.,1.,1.,1.,1.,1.,1.,1.,1.,1.,1.,
1.,1.,1.,1.,1.,1.,1.,1.,1.,1.,1.,1.,1.,1.,1.,1.,1.,1.,1.,1.,1.,1.,1.,1.,
1.,1.,1.,1.,1.,1.,1.,1.,1.,1.,1.,1.,1.,1.,1.,1.,1.,1.,1.,1.,1.,1.,1.,1.,
1.,1.,1.,1.,1.,1.,1.,1.,1.,1.,1.,1.,1.,1.,1.,1.,1.,1.,1.,1.,1.,1.,1.,1.,
1.,1.,1.,1.,1.,1.,1.,1.,1.,1.,1.,1.,1.,1.,1.,1.,1.,1.,1.,1.,1.,1.,1.,1.,
1.,1.,1.,1.,1.,1.,1.,1.,1.,1.,1.,1.,1.,1.,1.,1.,1.,1.,1.,1.,1.,1.,1.,1.,
1.,1.,1.,1.,1.,1.,1.,1.,1.,1.,1.,1.,1.,1.,1.,1.,1.,1.,1.,1.,1.,1.,1.,1.,
1.,1.,1.,1.,1.,1.,1.,1.,1.,1.,1.,1.,1.,1.,1.,1.,1.,1.,1.,1.,1.,1.,1.,1.,
1.,1.,1.,1.,1.,1.,1.,1.,1.,1.,1.,1.,1.,1.,1.,1.,1.,1.,1.,1.,1.,1.,1.,1.,
1.,1.,1.,1.,1.,1.,1.,1.,1.,1.,1.,1.,1.,1.,1.,1.,1.,1.,1.,1.,1.,1.,1.,1.,
1.,1.,1.,1.,1.,1.,1.,1.,1.,1.,1.,1.,1.,1.,1.,1.,1.,1.,1.,1.,1.,1.,1.,1.,
1.,1.,1.,1.,1.,1.,1.,1.,1.,1.,1.,1.,1.,1.,1.,1.,1.,1.,1.,1.,1.,1.,1.,1.,
1.,1.,1.,1.,1.,1.,1.,1.,1.,1.,1.,1.,1.,1.,1.,1.,1.,1.,1.,1.,1.,1.,1.,1.,
1.,1.,1.,1.,1.,1.,1.,1.,1.,1.,1.,1.,1.,1.,1.,1.,1.,1.,1.,1.,1.,1.,1.,1.,
1.,1.,1.,1.,1.,1.,1.,1.,1.,1.,1.,1.,1.,1.,1.,1.,1.,1.,1.,1.,1.,1.,1.,1.,
1.,1.,1.,1.,1.,1.,1.,1.,1.,1.,1.,1.,1.,1.,1.,1.,1.,1.,1.,1.,1.,1.,1.,1.,
1.,1.,1.,1.,1.,1.,1.,1.,1.,1.,1.,1.,1.,1.,1.,1.,1.,1.,1.,1.,1.,1.,1.,1.,
1.,1.,1.,1.,1.,1.,1.,1.,1.,1.,1.,1.,1.,1.,1.,1.,1.,1.,1.,1.,1.,1.,1.,1.,
1.,1.,1.,1.,1.,1.,1.,1.,1.,1.,1.,1.,1.,1.,1.,1.,1.,1.,1.,1.,1.,1.,1.,1.,
1.,1.,1.,1.,1.,1.,1.,1.,1.,1.,1.,1.,1.,1.,1.,1.,1.,1.,1.,1.,1.,1.,1.,1.,
1.,1.,1.,1.,1.,1.,1.,1.,1.,1.,1.,1.,1.,1.,1.,1.,1.,1.,1.,1.,1.,1.,1.,1.,
1.,1.,1.,1.,1.,1.,1.,1.,1.,1.))
REPRESENTATION_ITEM('')
) ;
#20 = (
BOUNDED_CURVE()
B_SPLINE_CURVE(3,(#134125,#134126,#134127,#134128,#134129,#134130,#134131),
 .UNSPECIFIED.,.F.,.F.)
B_SPLINE_CURVE_WITH_KNOTS((4,1,1,1,4),(0.,0.0911446219616379,0.182289243923276,
0.273433865884915,0.364578487846551),.UNSPECIFIED.)
CURVE()
GEOMETRIC_REPRESENTATION_ITEM()
RATIONAL_B_SPLINE_CURVE((1.,1.,1.,1.,1.,1.,1.))
REPRESENTATION_ITEM('')
) ;
#21 = (
BOUNDED_CURVE()
B_SPLINE_CURVE(3,(#134347,#134348,#134349,#134350,#134351,#134352,#134353,
#134354,#134355,#134356,#134357,#134358,#134359,#134360,#134361,#134362,
#134363,#134364,#134365),.UNSPECIFIED.,.F.,.F.)
B_SPLINE_CURVE_WITH_KNOTS((4,1,1,1,1,1,1,1,1,1,1,1,1,1,1,1,4),(0.,0.226732296973331,
0.464902013928651,0.70307173088397,0.9298040278573,1.15653632483063,1.39470604178595,
1.63287575874127,1.8596080557146,2.08634035268793,2.32451006964325,2.56267978659857,
2.7894120835719,3.01614438054523,3.25431409750055,3.49248381445586,3.7192161114292),
 .UNSPECIFIED.)
CURVE()
GEOMETRIC_REPRESENTATION_ITEM()
RATIONAL_B_SPLINE_CURVE((1.,1.,1.,1.,1.,1.,1.,1.,1.,1.,1.,1.,1.,1.,1.,1.,
1.,1.,1.))
REPRESENTATION_ITEM('')
) ;
#22 = (
BOUNDED_CURVE()
B_SPLINE_CURVE(3,(#152830,#152831,#152832,#152833,#152834,#152835,#152836,
#152837,#152838,#152839,#152840,#152841,#152842,#152843,#152844,#152845,
#152846,#152847,#152848,#152849,#152850,#152851,#152852,#152853,#152854,
#152855,#152856,#152857,#152858,#152859,#152860,#152861,#152862,#152863,
#152864,#152865,#152866,#152867,#152868,#152869,#152870,#152871,#152872,
#152873,#152874,#152875,#152876,#152877,#152878,#152879,#152880,#152881,
#152882,#152883,#152884,#152885,#152886,#152887,#152888,#152889,#152890,
#152891,#152892,#152893,#152894,#152895,#152896,#152897,#152898,#152899,
#152900,#152901,#152902,#152903,#152904,#152905,#152906,#152907,#152908,
#152909,#152910,#152911,#152912,#152913,#152914,#152915,#152916,#152917,
#152918,#152919,#152920,#152921,#152922,#152923,#152924,#152925,#152926,
#152927,#152928,#152929,#152930,#152931,#152932,#152933,#152934,#152935,
#152936,#152937,#152938,#152939,#152940,#152941,#152942,#152943,#152944,
#152945,#152946,#152947,#152948,#152949,#152950,#152951,#152952,#152953,
#152954,#152955,#152956,#152957,#152958,#152959,#152960,#152961,#152962,
#152963,#152964,#152965,#152966,#152967,#152968,#152969,#152970,#152971,
#152972,#152973,#152974,#152975,#152976,#152977,#152978,#152979,#152980,
#152981,#152982,#152983,#152984,#152985,#152986,#152987,#152988,#152989,
#152990,#152991,#152992,#152993,#152994,#152995,#152996,#152997,#152998,
#152999,#153000,#153001,#153002,#153003,#153004,#153005,#153006,#153007,
#153008,#153009,#153010,#153011,#153012,#153013,#153014,#153015,#153016,
#153017,#153018,#153019,#153020,#153021,#153022,#153023,#153024,#153025,
#153026,#153027,#153028,#153029,#153030,#153031,#153032,#153033,#153034,
#153035,#153036,#153037,#153038,#153039,#153040,#153041,#153042,#153043,
#153044,#153045,#153046,#153047,#153048,#153049,#153050,#153051,#153052,
#153053,#153054,#153055,#153056,#153057,#153058,#153059,#153060,#153061,
#153062,#153063,#153064,#153065,#153066,#153067,#153068,#153069,#153070,
#153071,#153072,#153073,#153074,#153075,#153076,#153077,#153078,#153079,
#153080,#153081,#153082,#153083,#153084,#153085,#153086,#153087,#153088,
#153089,#153090,#153091,#153092,#153093,#153094,#153095,#153096,#153097,
#153098,#153099,#153100,#153101,#153102,#153103,#153104,#153105,#153106,
#153107,#153108,#153109,#153110,#153111,#153112,#153113,#153114,#153115,
#153116,#153117,#153118,#153119,#153120,#153121,#153122,#153123,#153124,
#153125,#153126,#153127,#153128,#153129,#153130,#153131,#153132,#153133,
#153134,#153135,#153136,#153137,#153138,#153139,#153140,#153141,#153142,
#153143,#153144,#153145,#153146,#153147,#153148,#153149,#153150,#153151,
#153152,#153153,#153154,#153155,#153156,#153157,#153158,#153159,#153160,
#153161,#153162,#153163,#153164,#153165,#153166,#153167,#153168,#153169,
#153170,#153171,#153172,#153173,#153174,#153175,#153176,#153177,#153178,
#153179,#153180,#153181,#153182,#153183,#153184,#153185,#153186,#153187,
#153188,#153189,#153190,#153191,#153192,#153193,#153194,#153195,#153196,
#153197,#153198,#153199,#153200,#153201,#153202,#153203,#153204,#153205,
#153206,#153207,#153208,#153209,#153210,#153211,#153212,#153213,#153214,
#153215,#153216,#153217,#153218,#153219,#153220,#153221,#153222,#153223,
#153224,#153225,#153226,#153227,#153228,#153229,#153230,#153231,#153232,
#153233,#153234,#153235,#153236,#153237,#153238,#153239,#153240,#153241,
#153242,#153243,#153244,#153245,#153246,#153247,#153248,#153249,#153250,
#153251,#153252,#153253,#153254,#153255,#153256,#153257,#153258,#153259,
#153260,#153261,#153262,#153263,#153264,#153265,#153266,#153267,#153268,
#153269,#153270,#153271,#153272,#153273,#153274,#153275,#153276,#153277,
#153278,#153279,#153280,#153281,#153282,#153283,#153284,#153285,#153286,
#153287,#153288,#153289,#153290,#153291,#153292,#153293,#153294,#153295,
#153296,#153297,#153298,#153299,#153300,#153301,#153302,#153303,#153304,
#153305,#153306,#153307,#153308,#153309,#153310,#153311,#153312,#153313,
#153314,#153315,#153316,#153317,#153318,#153319,#153320,#153321,#153322,
#153323,#153324,#153325,#153326,#153327,#153328,#153329,#153330,#153331,
#153332,#153333,#153334,#153335,#153336,#153337,#153338,#153339,#153340,
#153341,#153342,#153343,#153344,#153345,#153346,#153347,#153348,#153349,
#153350,#153351,#153352,#153353,#153354,#153355,#153356,#153357,#153358,
#153359,#153360,#153361,#153362,#153363,#153364,#153365,#153366,#153367,
#153368,#153369,#153370,#153371,#153372,#153373,#153374,#153375,#153376,
#153377,#153378,#153379,#153380,#153381,#153382,#153383,#153384,#153385,
#153386,#153387,#153388,#153389,#153390,#153391,#153392,#153393,#153394,
#153395,#153396,#153397,#153398,#153399,#153400,#153401,#153402,#153403,
#153404,#153405,#153406,#153407,#153408,#153409,#153410,#153411,#153412,
#153413,#153414,#153415,#153416,#153417,#153418,#153419,#153420,#153421,
#153422,#153423,#153424,#153425,#153426,#153427,#153428,#153429,#153430,
#153431,#153432,#153433,#153434,#153435,#153436,#153437,#153438,#153439,
#153440,#153441,#153442,#153443,#153444,#153445,#153446,#153447,#153448,
#153449,#153450,#153451,#153452,#153453,#153454,#153455,#153456,#153457,
#153458,#153459,#153460,#153461,#153462,#153463,#153464,#153465,#153466,
#153467,#153468,#153469,#153470,#153471,#153472,#153473,#153474,#153475,
#153476,#153477,#153478,#153479,#153480,#153481,#153482,#153483,#153484,
#153485,#153486,#153487,#153488,#153489,#153490,#153491,#153492,#153493,
#153494,#153495,#153496,#153497,#153498,#153499,#153500,#153501,#153502,
#153503,#153504,#153505,#153506,#153507,#153508,#153509,#153510,#153511,
#153512,#153513,#153514,#153515,#153516,#153517,#153518,#153519,#153520,
#153521,#153522,#153523,#153524,#153525,#153526,#153527,#153528,#153529,
#153530,#153531,#153532,#153533,#153534,#153535,#153536,#153537,#153538,
#153539,#153540,#153541,#153542,#153543,#153544,#153545,#153546,#153547,
#153548,#153549,#153550,#153551,#153552,#153553,#153554,#153555,#153556,
#153557,#153558,#153559,#153560,#153561,#153562,#153563,#153564,#153565,
#153566,#153567,#153568,#153569,#153570,#153571,#153572,#153573,#153574,
#153575,#153576,#153577,#153578,#153579,#153580,#153581,#153582,#153583,
#153584,#153585,#153586,#153587,#153588,#153589,#153590,#153591,#153592,
#153593,#153594,#153595,#153596,#153597,#153598,#153599,#153600,#153601,
#153602,#153603,#153604,#153605,#153606,#153607,#153608,#153609,#153610,
#153611,#153612,#153613,#153614,#153615,#153616,#153617,#153618,#153619,
#153620,#153621,#153622,#153623,#153624,#153625,#153626,#153627,#153628,
#153629,#153630,#153631,#153632,#153633,#153634,#153635,#153636,#153637,
#153638,#153639,#153640,#153641,#153642,#153643,#153644,#153645,#153646,
#153647,#153648,#153649,#153650,#153651,#153652,#153653,#153654,#153655,
#153656,#153657,#153658,#153659,#153660,#153661,#153662,#153663,#153664,
#153665,#153666,#153667,#153668,#153669,#153670,#153671,#153672,#153673,
#153674,#153675,#153676,#153677,#153678,#153679,#153680,#153681,#153682,
#153683,#153684,#153685,#153686,#153687,#153688,#153689,#153690,#153691,
#153692,#153693,#153694,#153695,#153696,#153697,#153698,#153699,#153700,
#153701,#153702,#153703,#153704,#153705,#153706,#153707,#153708,#153709,
#153710,#153711,#153712,#153713,#153714,#153715,#153716,#153717,#153718,
#153719,#153720,#153721,#153722,#153723,#153724,#153725,#153726,#153727,
#153728,#153729,#153730,#153731,#153732,#153733,#153734,#153735,#153736,
#153737,#153738,#153739,#153740,#153741,#153742,#153743,#153744,#153745,
#153746,#153747,#153748,#153749,#153750,#153751,#153752,#153753,#153754,
#153755,#153756,#153757,#153758,#153759,#153760,#153761,#153762,#153763,
#153764,#153765,#153766,#153767,#153768,#153769,#153770,#153771,#153772,
#153773,#153774,#153775,#153776,#153777,#153778,#153779,#153780,#153781,
#153782,#153783,#153784,#153785,#153786,#153787,#153788,#153789,#153790,
#153791,#153792,#153793,#153794,#153795,#153796,#153797,#153798,#153799,
#153800,#153801,#153802,#153803,#153804,#153805,#153806,#153807,#153808,
#153809,#153810,#153811,#153812,#153813,#153814,#153815,#153816,#153817,
#153818,#153819,#153820,#153821,#153822,#153823,#153824,#153825,#153826,
#153827,#153828,#153829,#153830,#153831,#153832,#153833,#153834,#153835,
#153836,#153837,#153838,#153839,#153840,#153841,#153842,#153843,#153844,
#153845,#153846,#153847,#153848,#153849,#153850,#153851,#153852,#153853,
#153854,#153855,#153856,#153857,#153858,#153859,#153860,#153861,#153862,
#153863,#153864,#153865,#153866,#153867,#153868,#153869,#153870,#153871,
#153872,#153873,#153874,#153875,#153876,#153877,#153878,#153879,#153880,
#153881,#153882,#153883,#153884,#153885,#153886,#153887),.UNSPECIFIED.,
 .F.,.F.)
B_SPLINE_CURVE_WITH_KNOTS((4,1,1,1,1,1,1,1,1,1,1,1,1,1,1,1,1,1,1,1,1,1,
1,1,1,1,1,1,1,1,1,1,1,1,1,1,1,1,1,1,1,1,1,1,1,1,1,1,1,1,1,1,1,1,1,1,1,1,
1,1,1,1,1,1,1,1,1,1,1,1,1,1,1,1,1,1,1,1,1,1,1,1,1,1,1,1,1,1,1,1,1,1,1,1,
1,1,1,1,1,1,1,1,1,1,1,1,1,1,1,1,1,1,1,1,1,1,1,1,1,1,1,1,1,1,1,1,1,1,1,1,
1,1,1,1,1,1,1,1,1,1,1,1,1,1,1,1,1,1,1,1,1,1,1,1,1,1,1,1,1,1,1,1,1,1,1,1,
1,1,1,1,1,1,1,1,1,1,1,1,1,1,1,1,1,1,1,1,1,1,1,1,1,1,1,1,1,1,1,1,1,1,1,1,
1,1,1,1,1,1,1,1,1,1,1,1,1,1,1,1,1,1,1,1,1,1,1,1,1,1,1,1,1,1,1,1,1,1,1,1,
1,1,1,1,1,1,1,1,1,1,1,1,1,1,1,1,1,1,1,1,1,1,1,1,1,1,1,1,1,1,1,1,1,1,1,1,
1,1,1,1,1,1,1,1,1,1,1,1,1,1,1,1,1,1,1,1,1,1,1,1,1,1,1,1,1,1,1,1,1,1,1,1,
1,1,1,1,1,1,1,1,1,1,1,1,1,1,1,1,1,1,1,1,1,1,1,1,1,1,1,1,1,1,1,1,1,1,1,1,
1,1,1,1,1,1,1,1,1,1,1,1,1,1,1,1,1,1,1,1,1,1,1,1,1,1,1,1,1,1,1,1,1,1,1,1,
1,1,1,1,1,1,1,1,1,1,1,1,1,1,1,1,1,1,1,1,1,1,1,1,1,1,1,1,1,1,1,1,1,1,1,1,
1,1,1,1,1,1,1,1,1,1,1,1,1,1,1,1,1,1,1,1,1,1,1,1,1,1,1,1,1,1,1,1,1,1,1,1,
1,1,1,1,1,1,1,1,1,1,1,1,1,1,1,1,1,1,1,1,1,1,1,1,1,1,1,1,1,1,1,1,1,1,1,1,
1,1,1,1,1,1,1,1,1,1,1,1,1,1,1,1,1,1,1,1,1,1,1,1,1,1,1,1,1,1,1,1,1,1,1,1,
1,1,1,1,1,1,1,1,1,1,1,1,1,1,1,1,1,1,1,1,1,1,1,1,1,1,1,1,1,1,1,1,1,1,1,1,
1,1,1,1,1,1,1,1,1,1,1,1,1,1,1,1,1,1,1,1,1,1,1,1,1,1,1,1,1,1,1,1,1,1,1,1,
1,1,1,1,1,1,1,1,1,1,1,1,1,1,1,1,1,1,1,1,1,1,1,1,1,1,1,1,1,1,1,1,1,1,1,1,
1,1,1,1,1,1,1,1,1,1,1,1,1,1,1,1,1,1,1,1,1,1,1,1,1,1,1,1,1,1,1,1,1,1,1,1,
1,1,1,1,1,1,1,1,1,1,1,1,1,1,1,1,1,1,1,1,1,1,1,1,1,1,1,1,1,1,1,1,1,1,1,1,
1,1,1,1,1,1,1,1,1,1,1,1,1,1,1,1,1,1,1,1,1,1,1,1,1,1,1,1,1,1,1,1,1,1,1,1,
1,1,1,1,1,1,1,1,1,1,1,1,1,1,1,1,1,1,1,1,1,1,1,1,1,1,1,1,1,1,1,1,1,1,1,1,
1,1,1,1,1,1,1,1,1,1,1,1,1,1,1,1,1,1,1,1,1,1,1,1,1,1,1,1,1,1,1,1,1,1,1,1,
1,1,1,1,1,1,1,1,1,1,1,1,1,1,1,1,1,1,1,1,1,1,1,1,1,1,1,1,1,1,1,1,1,1,1,1,
1,1,1,1,1,1,1,1,1,1,1,1,1,1,1,1,1,1,1,1,1,1,1,1,1,1,1,1,1,1,1,1,1,1,1,1,
1,1,1,1,1,1,1,1,1,1,1,1,1,1,1,1,1,1,1,1,1,1,1,1,1,1,1,1,1,1,1,1,1,1,1,1,
1,1,1,1,1,1,1,1,1,1,1,1,1,1,1,1,1,1,1,1,1,1,1,1,1,1,1,1,1,1,1,1,1,1,1,1,
1,1,1,1,1,1,1,1,1,1,1,1,1,1,1,1,1,1,1,1,1,1,1,1,1,1,1,1,1,1,1,1,1,1,1,1,
1,1,1,1,1,1,1,1,1,1,1,1,1,1,1,1,1,1,1,1,1,1,1,1,1,1,1,1,1,1,1,1,1,1,1,1,
1,1,1,1,1,1,1,1,1,1,1,1,1,1,1,1,1,1,1,1,1,1,1,1,1,4),(0.,0.01797683372391,
0.286633051710584,0.555289278308216,0.823945516665782,1.09260176953922,
1.36125803873948,1.62991432588463,1.89857063164012,2.16722695661301,2.43588330050525,
2.70453966304674,2.9731960431531,3.24185243981471,3.51050885133453,3.77916527610465,
4.04782171198515,4.31647815691489,4.58513460847725,4.85379106430677,5.12244752187208,
5.39110397865606,5.65976043217153,5.92841687990537,6.19707331956994,6.46572974881596,
6.73438616570634,7.00304256821933,7.2716989549161,7.5403553242696,7.809011675483,
8.07766800769526,8.34632432089157,8.61498061505147,8.8836368910788,9.15229314997201,
9.4209493936865,9.68960562442157,9.95826184531348,10.226918059948,10.4955742727586,
10.7642304884925,11.0328867113173,11.3015429448574,11.5701991918227,11.8388554546081,
12.1075117346518,12.3761680332469,12.6448243507434,12.9134806874637,13.1821370428496,
13.450793416388,13.7194498067883,13.9881062128412,14.2567626326955,14.5254190645885,
14.7940755062772,15.0627319555912,15.3313884100611,15.6000448672586,15.8687013246492,
16.1373577797,16.4060142299691,16.6746706729765,16.9433271065265,17.2119835283531,
17.4806399366567,17.7492963295502,18.0179527057767,18.286609063996,18.555265403637,
18.8239217240786,19.0925780255742,19.3612343083975,19.6298905737625,19.898546823017,
20.1672030584666,20.4358592827168,20.7045154992928,20.973171712245,21.2418279262962,
21.5104841459723,21.7791403749736,22.0477966165324,22.316452872948,22.585109146262,
22.8537654375589,23.1224217478187,23.3910780770929,23.6597344254327,23.9283907920352,
24.197047176159,24.4657035763222,24.7343599911301,25.0030164185931,25.2716728568073,
25.5403293034427,25.8089857562333,26.0776422126729,26.3462986702843,26.6149551265448,
26.8836115789212,27.1522680250308,27.4209244624423,27.6895808890659,27.9582373027346,
28.2268937018004,28.4955500845261,28.7642064498512,29.0328627966379,29.3015191245544,
29.5701754332357,29.838831723217,30.1074879950829,30.3761442503694,30.6448004907916,
30.9134567190168,31.1821129380756,31.450769151893,31.7194253649682,31.9880815819663,
32.2567378070174,32.5253940433706,32.7940502938785,33.0627065604467,33.3313628447765,
33.6000191476151,33.8686754696427,34.1373318106287,34.405988170366,34.6746445478242,
34.9433009420458,35.2119573513747,35.480613774244,35.7492702085419,36.0179266522368,
36.2865831029275,36.5552395582669,36.8238960157264,37.0925524727952,37.3612089269773,
37.6298653757534,37.8985218168153,38.1671782477952,38.4358346667239,38.7044910715485,
38.9731474607866,39.2418038328672,39.5104601869391,39.7791165220837,40.0477728382212,
40.3164291352602,40.5850854140292,40.8537416754418,41.1223979213679,41.3910541539077,
41.6597103761025,41.9283665914244,42.1970228042084,42.4656790192,42.7343352406829,
43.0029914723808,43.2716477171096,43.540303977354,43.8089602546436,44.0776165503516,
44.3462728649052,44.614929198697,44.883585551232,45.1522419220568,45.4208983099307,
45.6895547136931,45.9582111315299,46.2268675617156,46.4955240020317,46.7641804503338,
47.0328369041642,47.3014933611089,47.5701498186329,47.8388062742058,48.107462725373,
48.3761191696448,48.6447756048012,48.9134320285537,49.1820884390673,49.4507448344197,
49.7194012133072,49.9880575743413,50.2567139168934,50.5253702402807,50.7940265446884,
51.0626828303152,51.3313390982961,51.5999953498901,51.8686515873141,52.1373078130706,
52.4059640305862,52.6746202437936,52.9432764573682,53.211932675918,53.480588903259,
53.7492451427202,54.0179013967021,54.2865576673334,54.5552139557853,54.823870263115,
55.0925265894471,55.3611829348992,55.6298392987282,55.8984956802486,56.1671520780245,
56.4358084907065,56.7044649163381,56.9731213530494,57.2417777985307,57.5104342505384,
57.7790907065743,58.0477471641719,58.3164036208043,58.5850600739368,58.8537165211707,
59.1223729600609,59.39102938849,59.6596858042645,59.9283422056975,60.1969985910129,
60.4656549590995,60.7343113087676,61.0029676396243,61.2716239512389,61.540280244075,
61.808936518638,62.0775927763821,62.3462490189291,62.6149052488546,62.8835614690812,
63.1522176834332,63.4208738963055,63.6895301124163,63.9581863359981,64.2268425704115,
64.4954988186027,64.7641550825741,65.0328113641112,65.3014676640435,65.5701239831253,
65.8387803211949,66.1074366781083,66.3760930528907,66.6447494446373,66.9134058517341,
67.1820622726558,67.4507187053199,67.7193751477252,67.988031597487,68.256688052277,
68.5253445095709,68.7940009668648,69.0626574216546,69.3313138714164,69.5999703138218,
69.8686267464858,70.1372831674076,70.4059395745042,70.6745959662509,70.9432523410334,
71.2119086979469,71.4805650360164,71.7492213550982,72.0178776550306,72.2865339365675,
72.5551902005389,72.8238464487301,73.0925026831433,73.3611589067251,73.6298151228357,
73.8984713357081,74.1671275500599,74.4357837702864,74.7044400002118,74.9730962427587,
75.2417525005027,75.5104087750655,75.7790650679015,76.047721379516,76.3163777103726,
76.5850340600405,76.853690428127,77.1223468134422,77.391003214875,77.6596596306495,
77.9283160590784,78.1969724979684,78.4656289452021,78.7342853983344,79.0029418549666,
79.2715983125641,79.5402547685998,79.8089112206075,80.0775676660886,80.3462241027997,
80.6148805284312,80.8835369411131,81.1521933388889,81.4208497204091,81.689506084238,
81.9581624296899,82.2268187560219,82.4954750633515,82.7641313518033,83.0327876224345,
83.3014438764161,83.5701001158772,83.838756343218,84.1074125617677,84.3760687753422,
84.6447249885494,84.913381206065,85.1820374318212,85.4506936692451,85.719349920839,
85.9880061888197,86.2566624744465,86.5253187788541,86.7939751022413,87.0626314447932,
87.3312878058273,87.5999441847146,87.8686005800667,88.1372569905802,88.4059134143327,
88.6745698494889,88.9432262937606,89.2118827449277,89.4805392005005,89.7491956580243,
90.0178521149689,90.2865085687992,90.5551650171012,90.8238214574172,91.0924778876028,
91.3611343054394,91.6297907092016,91.8984470970753,92.1671034679,92.4357598204347,
92.7044161542264,92.9730724687798,93.2417287644878,93.5103850417773,93.7790413020216,
94.0476975467502,94.3163537784479,94.5850099999307,94.8536662149221,95.1223224277061,
95.390978643028,95.6596348652226,95.9282910977624,96.1969473436883,96.4656036051009,
96.7342598838697,97.0029161809086,97.2715724970461,97.5402288321905,97.8088851862623,
98.0775415583427,98.3461979475807,98.6148543524051,98.8835107713336,99.1521672023136,
99.4208236433754,99.6894800921513,99.9581365463333,100.226793003402,100.495449460861,
100.7641059162,101.032762366891,101.301418810586,101.570075244884,101.838731667753,
102.107388077082,102.376044471303,102.644700848761,102.913357208498,103.182013549484,
103.450669871511,103.71932617435,103.98798245868,104.256638725248,104.525294975755,
104.793951212108,105.062607437159,105.331263654157,105.599919867233,105.86857608105,
106.137232300108,106.405888528334,106.674544768756,106.943201024042,107.211857295908,
107.480513585889,107.74916989457,108.017826222487,108.286482569273,108.555138934598,
108.823795317324,109.09245171639,109.361108130058,109.629764556682,109.898420994093,
110.167077440202,110.435733892579,110.704390348839,110.97304680645,111.24170326289,
111.51035971568,111.779016162316,112.04767260053,112.316329027993,112.5849854428,
112.853641842963,113.122298227087,113.39095459369,113.659610942029,113.928267271303,
114.196923581563,114.46557987286,114.734236146174,115.002892402589,115.271548644148,
115.540204873149,115.808861092825,116.077517306876,116.346173519828,116.614829736404,
116.883485960654,117.152142196103,117.420798445358,117.689454710722,117.958110993546,
118.226767295041,118.495423615483,118.764079955123,119.032736313343,119.301392689569,
119.570049082462,119.838705490766,120.107361912592,120.376018346142,120.644674789149,
120.913331239418,121.181987694469,121.45064415186,121.719300609057,121.987957063527,
122.256613512841,122.525269954529,122.793926386422,123.062582806276,123.331239212329,
123.599895602729,123.868551976268,124.137208331653,124.405864668374,124.67452098587,
124.943177284465,125.211833564508,125.480489827294,125.749146074259,126.017802307799,
126.286458530624,126.555114746357,126.823770959168,127.092427173802,127.361083394694,
127.629739625429,127.898395869143,128.167052128037,128.435708404064,128.704364698224,
128.97302101142,129.241677343633,129.510333694846,129.7789900642,130.047646450897,
130.31630285341,130.5849592703,130.853615699547,131.122272139211,131.390928586945,
131.659585040461,131.928241497245,132.19689795481,132.46555441064,132.734210862202,
133.002867307132,133.271523743013,133.540180167783,133.808836579303,134.077492975965,
134.346149356071,134.614805718613,134.883462062505,135.152118387478,135.420774693234,
135.689430980379,135.958087249579,136.226743502453,136.49539974081,136.76405596741,
137.032712185392,137.301368398783,137.570024612174,137.838680830155,138.107337056755,
138.375993295112,138.644649547986,138.913305817186,139.181962104332,139.450618410087,
139.71927473506,139.987931078952,140.256587441494,140.525243821601,140.793900218262,
141.062556629782,141.331213054552,141.599869490433,141.868525935363,142.137182386925,
142.405838842755,142.67449530032,142.943151757104,143.21180821062,143.480464658354,
143.749121098019,144.017777527265,144.286433944155,144.555090346668,144.823746733365,
145.092403102719,145.361059453932,145.629715786145,145.898372099341,146.167028393501,
146.435684669529,146.704340928422,146.972997172137,147.241653402872,147.510309623764,
147.778965838398,148.047622051209,148.316278266943,148.584934489768,148.853590723308,
149.122246970274,149.390903233059,149.659559513103,149.928215811698,150.196872129195,
150.465528465915,150.734184821301,151.00284119484,151.27149758524,151.540153991293,
151.808810411148,152.077466843041,152.34612328473,152.614779734044,152.883436188514,
153.152092645711,153.420749103102,153.689405558153,153.958062008422,154.22671845143,
154.49537488498,154.764031306806,155.03268771511,155.301344108004,155.57000048423,
155.838656842449,156.107313182091,156.375969502532,156.644625804028,156.913282086851,
157.181938352216,157.450594601471,157.719250836921,157.987907061171,158.256563277747,
158.525219490699,158.793875704751,159.062531924427,159.331188153428,159.599844394987,
159.868500651403,160.137156924717,160.405813216014,160.674469526274,160.943125855548,
161.211782203888,161.480438570491,161.749094954615,162.017751354778,162.286407769586,
162.555064197049,162.823720635263,163.092377081899,163.361033534689,163.629689991129,
163.898346448741,164.167002905001,164.435659357378,164.704315803488,164.972972240899,
165.241628667523,165.510285081192,165.778941480257,166.047597862983,166.316254228308,
166.584910575095,166.853566903012,167.122223211693,167.390879501675,167.659535773541,
167.928192028827,168.19684826925,168.465504497475,168.734160716534,169.002816930351,
169.271473143427,169.540129360425,169.808785585476,170.077441821829,170.346098072337,
170.614754338905,170.883410623235,171.152066926074,171.420723248102,171.689379589088,
171.958035948825,172.226692326284,172.495348720505,172.764005129834,173.032661552704,
173.301317987002,173.569974430697,173.838630881388,174.107287336727,174.375943794187,
174.644600251255,174.913256705437,175.181913154214,175.450569595276,175.719226026256,
175.987882445184,176.256538850009,176.525195239247,176.793851611328,177.0625079654,
177.331164300545,177.599820616682,177.868476913721,178.137133192491,178.405789453903,
178.674445699829,178.943101932369,179.211758154564,179.480414369886,179.74907058267,
180.017726797662,180.286383019145,180.555039250843,180.823695495572,181.092351755816,
181.361008033106,181.629664328814,181.898320643368,182.16697697716,182.435633329695,
182.70428970052,182.972946088394,183.241602492156,183.510258909993,183.778915340179,
184.047571780495,184.316228228797,184.584884682628,184.853541139572,185.122197597096,
185.39085405267,185.659510503837,185.928166948109,186.196823383265,186.465479807018,
186.734136217531,187.002792612884,187.271448991771,187.540105352806,187.808761695358,
188.077418018745,188.346074323153,188.61473060878,188.883386876761,189.152043128355,
189.420699365779,189.689355591536,189.958011809051,190.226668022259,190.495324235834,
190.763980454383,191.032636681725,191.301292921186,191.569949175168,191.838605445799,
192.107261734251,192.375918041581,192.644574367913,192.913230713365,193.181887077194,
193.450543458715,193.719199856491,193.987856269173,194.256512694805,194.525169131516,
194.793825576997,195.062482029005,195.331138485041,195.599794942639,195.868451399271,
196.137107852404,196.405764299638,196.674420738528,196.943077166957,197.211733582732,
197.480389984165,197.749046369481,198.017702737567,198.286359087236,198.555015418092,
198.823671729707,199.092328022543,199.360984297106,199.62964055485,199.898296797397,
200.166953027323,200.43560924755,200.704265461902,200.972921674774,201.241577890885,
201.510234114467,201.77889034888,202.047546597072,202.316202861043,202.584859142581,
202.853515442513,203.122171761595,203.390828099665,203.659484456579,203.928140831361,
204.196797223108,204.465453630205,204.734110051127,205.002766483791,205.271422926197,
205.540079375959,205.808735830749,206.077392288043,206.346048745337,206.614705200127,
206.883361649889,207.152018092295,207.420674524959,207.689330945881,207.957987352978,
208.226643744725,208.495300119508,208.763956476421,209.032612814491,209.301269133573,
209.569925433505,209.838581715043,210.107237979014,210.375894227206,210.644550461619,
210.913206685201,211.181862901312,211.450519114184,211.719175328536,211.987831548763,
212.256487778689,212.525144021236,212.79380027898,213.062456553543,213.331112846379,
213.599769157994,213.868425488851,214.137081838519,214.405738206606,214.674394591921,
214.943050993354,215.211707409129,215.480363837558,215.749020276448,216.017676723682,
216.286333176815,216.554989633447,216.823646091045,217.092302547081,217.360958999089,
217.62961544457,217.898271881281,218.166928306913,218.435584719595,218.704241117371,
218.972897498892,219.241553862721,219.510210208173,219.778866534505,220.047522841835,
220.316179130287,220.584835400918,220.8534916549,221.122147894361,221.390804121702,
221.659460340252,221.928116553827,222.196772767034,222.46542898455,222.734085210306,
223.00274144773,223.271397699324,223.540053967305,223.808710252932,224.07736655734,
224.346022880728,224.61467922328,224.883335584314,225.151991963201,225.420648358554,
225.689304769068,225.95796119282,226.226617627977,226.495274072249,226.763930523416,
227.032586978989,227.301243436513,227.569899893458,227.838556347288,228.10721279559,
228.375869235907,228.644525666093,228.913182083929,229.181838487692,229.450494875566,
229.719151246391,229.987807598926,230.256463932718,230.525120247271,230.79377654298,
231.062432820269,231.331089080514,231.599745325243,231.868401556941,232.137057778424,
232.405713993415,232.674370206199,232.943026421521,233.211682643716,233.480338876256,
233.748995122182,234.017651383595,234.286307662364,234.554963959403,234.823620275541,
235.092276610685,235.360932964757,235.629589336838,235.898245726076,236.166902130901,
236.43555854983,236.70421498081,236.972871421872,237.241527870648,237.51018432483,
237.778840781899,238.047497239359,238.316153694698,238.584810145389,238.853466589084,
239.122123023382,239.390779446251,239.65943585558,239.928092249802,240.19674862726,
240.465404986998,240.734061327984,241.002717650011,241.27137395285,241.54003023718,
241.808686503748,242.077342754256,242.345998990609,242.614655215661,242.883311432659,
243.151967645734,243.420623859552,243.68928007861,243.957936306836,244.226592547258,
244.495248802545,244.763905074411,245.032561364392,245.301217673074,245.56987400099,
245.838530347777,246.107186713102,246.375843095828,246.644499494894,246.913155908563,
247.181812335186,247.450468772598,247.719125218708,247.987781671084,248.256438127345,
248.525094584956,248.793751041396,249.062407494187,249.331063940822,249.599720379036,
249.8683768065,250.137033221308,250.405689621471,250.674346005595,250.943002372197,
251.211658720537,251.480315049812,251.748971360071,252.017627651368,252.286283924683,
252.554940181098,252.823596422657,253.092252651658,253.360908871335,253.629565085386,
253.898221298338,254.166877514914,254.435533739165,254.704189974614,254.972846223869,
255.241502489234,255.510158772057,255.778815073553,256.047471393995,256.316127733635,
256.584784091854,256.85344046808,257.122096860973,257.390753269276,257.659409691102,
257.928066124652,258.196722567659,258.465379017928,258.734035472978,259.002691930368,
259.271348387566,259.540004842035,259.808661291349,260.077317733037,260.345974164929,
260.614630584783,260.883286990836,261.151943381235,261.420599754774,261.689256110159,
261.957912446879,262.226568764375,262.49522506297,262.763881343014,263.032537605798,
263.301193852763,263.569850086303,263.838506309127,264.107162524861,264.375818737671,
264.644474952305,264.913131173196,265.181787403931,265.450443647645,265.719099906538,
265.987756182565,266.256412476724,266.52506878992,266.793725122132,267.062381473345,
267.331037842698,267.599694229394,267.868350631907,268.137007048797,268.405663478042,
268.674319917706,268.94297636544,269.211632818955,269.480289275739,269.748945733304,
270.017602189133,270.286258640695,270.554915085624,270.823571521504,271.092227946274,
271.360884357793,271.629540754454,271.89819713456,272.166853497101,272.435509840993,
272.704166165965,272.97282247172,273.241478758865,273.510135028065,273.778791280938,
274.047447519295,274.316103745894,274.584759963875,274.853416177266,275.122072390656,
275.390728608637,275.659384835237,275.928041073593,276.196697326466,276.465353595666,
276.734009882811,277.002666188566,277.271322513539,277.53997885743,277.808635219972,
278.077291600077,278.345947996739,278.614604408258,278.883260833028,279.151917268908,
279.420573713837,279.689230165399,279.957886621228,280.226543078793,280.495199535576,
280.763855989092,281.032512436825,281.301168876489,281.569825305735,281.838481722625,
282.107138125138,282.375794511834,282.644450881187,282.9131072324,283.140531716307),
 .UNSPECIFIED.)
CURVE()
GEOMETRIC_REPRESENTATION_ITEM()
RATIONAL_B_SPLINE_CURVE((1.,1.,1.,1.,1.,1.,1.,1.,1.,1.,1.,1.,1.,1.,1.,1.,
1.,1.,1.,1.,1.,1.,1.,1.,1.,1.,1.,1.,1.,1.,1.,1.,1.,1.,1.,1.,1.,1.,1.,1.,
1.,1.,1.,1.,1.,1.,1.,1.,1.,1.,1.,1.,1.,1.,1.,1.,1.,1.,1.,1.,1.,1.,1.,1.,
1.,1.,1.,1.,1.,1.,1.,1.,1.,1.,1.,1.,1.,1.,1.,1.,1.,1.,1.,1.,1.,1.,1.,1.,
1.,1.,1.,1.,1.,1.,1.,1.,1.,1.,1.,1.,1.,1.,1.,1.,1.,1.,1.,1.,1.,1.,1.,1.,
1.,1.,1.,1.,1.,1.,1.,1.,1.,1.,1.,1.,1.,1.,1.,1.,1.,1.,1.,1.,1.,1.,1.,1.,
1.,1.,1.,1.,1.,1.,1.,1.,1.,1.,1.,1.,1.,1.,1.,1.,1.,1.,1.,1.,1.,1.,1.,1.,
1.,1.,1.,1.,1.,1.,1.,1.,1.,1.,1.,1.,1.,1.,1.,1.,1.,1.,1.,1.,1.,1.,1.,1.,
1.,1.,1.,1.,1.,1.,1.,1.,1.,1.,1.,1.,1.,1.,1.,1.,1.,1.,1.,1.,1.,1.,1.,1.,
1.,1.,1.,1.,1.,1.,1.,1.,1.,1.,1.,1.,1.,1.,1.,1.,1.,1.,1.,1.,1.,1.,1.,1.,
1.,1.,1.,1.,1.,1.,1.,1.,1.,1.,1.,1.,1.,1.,1.,1.,1.,1.,1.,1.,1.,1.,1.,1.,
1.,1.,1.,1.,1.,1.,1.,1.,1.,1.,1.,1.,1.,1.,1.,1.,1.,1.,1.,1.,1.,1.,1.,1.,
1.,1.,1.,1.,1.,1.,1.,1.,1.,1.,1.,1.,1.,1.,1.,1.,1.,1.,1.,1.,1.,1.,1.,1.,
1.,1.,1.,1.,1.,1.,1.,1.,1.,1.,1.,1.,1.,1.,1.,1.,1.,1.,1.,1.,1.,1.,1.,1.,
1.,1.,1.,1.,1.,1.,1.,1.,1.,1.,1.,1.,1.,1.,1.,1.,1.,1.,1.,1.,1.,1.,1.,1.,
1.,1.,1.,1.,1.,1.,1.,1.,1.,1.,1.,1.,1.,1.,1.,1.,1.,1.,1.,1.,1.,1.,1.,1.,
1.,1.,1.,1.,1.,1.,1.,1.,1.,1.,1.,1.,1.,1.,1.,1.,1.,1.,1.,1.,1.,1.,1.,1.,
1.,1.,1.,1.,1.,1.,1.,1.,1.,1.,1.,1.,1.,1.,1.,1.,1.,1.,1.,1.,1.,1.,1.,1.,
1.,1.,1.,1.,1.,1.,1.,1.,1.,1.,1.,1.,1.,1.,1.,1.,1.,1.,1.,1.,1.,1.,1.,1.,
1.,1.,1.,1.,1.,1.,1.,1.,1.,1.,1.,1.,1.,1.,1.,1.,1.,1.,1.,1.,1.,1.,1.,1.,
1.,1.,1.,1.,1.,1.,1.,1.,1.,1.,1.,1.,1.,1.,1.,1.,1.,1.,1.,1.,1.,1.,1.,1.,
1.,1.,1.,1.,1.,1.,1.,1.,1.,1.,1.,1.,1.,1.,1.,1.,1.,1.,1.,1.,1.,1.,1.,1.,
1.,1.,1.,1.,1.,1.,1.,1.,1.,1.,1.,1.,1.,1.,1.,1.,1.,1.,1.,1.,1.,1.,1.,1.,
1.,1.,1.,1.,1.,1.,1.,1.,1.,1.,1.,1.,1.,1.,1.,1.,1.,1.,1.,1.,1.,1.,1.,1.,
1.,1.,1.,1.,1.,1.,1.,1.,1.,1.,1.,1.,1.,1.,1.,1.,1.,1.,1.,1.,1.,1.,1.,1.,
1.,1.,1.,1.,1.,1.,1.,1.,1.,1.,1.,1.,1.,1.,1.,1.,1.,1.,1.,1.,1.,1.,1.,1.,
1.,1.,1.,1.,1.,1.,1.,1.,1.,1.,1.,1.,1.,1.,1.,1.,1.,1.,1.,1.,1.,1.,1.,1.,
1.,1.,1.,1.,1.,1.,1.,1.,1.,1.,1.,1.,1.,1.,1.,1.,1.,1.,1.,1.,1.,1.,1.,1.,
1.,1.,1.,1.,1.,1.,1.,1.,1.,1.,1.,1.,1.,1.,1.,1.,1.,1.,1.,1.,1.,1.,1.,1.,
1.,1.,1.,1.,1.,1.,1.,1.,1.,1.,1.,1.,1.,1.,1.,1.,1.,1.,1.,1.,1.,1.,1.,1.,
1.,1.,1.,1.,1.,1.,1.,1.,1.,1.,1.,1.,1.,1.,1.,1.,1.,1.,1.,1.,1.,1.,1.,1.,
1.,1.,1.,1.,1.,1.,1.,1.,1.,1.,1.,1.,1.,1.,1.,1.,1.,1.,1.,1.,1.,1.,1.,1.,
1.,1.,1.,1.,1.,1.,1.,1.,1.,1.,1.,1.,1.,1.,1.,1.,1.,1.,1.,1.,1.,1.,1.,1.,
1.,1.,1.,1.,1.,1.,1.,1.,1.,1.,1.,1.,1.,1.,1.,1.,1.,1.,1.,1.,1.,1.,1.,1.,
1.,1.,1.,1.,1.,1.,1.,1.,1.,1.,1.,1.,1.,1.,1.,1.,1.,1.,1.,1.,1.,1.,1.,1.,
1.,1.,1.,1.,1.,1.,1.,1.,1.,1.,1.,1.,1.,1.,1.,1.,1.,1.,1.,1.,1.,1.,1.,1.,
1.,1.,1.,1.,1.,1.,1.,1.,1.,1.,1.,1.,1.,1.,1.,1.,1.,1.,1.,1.,1.,1.,1.,1.,
1.,1.,1.,1.,1.,1.,1.,1.,1.,1.,1.,1.,1.,1.,1.,1.,1.,1.,1.,1.,1.,1.,1.,1.,
1.,1.,1.,1.,1.,1.,1.,1.,1.,1.,1.,1.,1.,1.,1.,1.,1.,1.,1.,1.,1.,1.,1.,1.,
1.,1.,1.,1.,1.,1.,1.,1.,1.,1.,1.,1.,1.,1.,1.,1.,1.,1.,1.,1.,1.,1.,1.,1.,
1.,1.,1.,1.,1.,1.,1.,1.,1.,1.,1.,1.,1.,1.,1.,1.,1.,1.,1.,1.,1.,1.,1.,1.,
1.,1.,1.,1.,1.,1.,1.,1.,1.,1.,1.,1.,1.,1.,1.,1.,1.,1.,1.,1.,1.,1.,1.,1.,
1.,1.,1.,1.,1.,1.,1.,1.,1.,1.,1.,1.,1.,1.,1.,1.,1.,1.,1.,1.,1.,1.,1.,1.,
1.,1.,1.,1.,1.,1.,1.,1.,1.,1.,1.,1.,1.,1.,1.,1.,1.,1.,1.,1.,1.,1.,1.,1.,
1.,1.,1.,1.,1.,1.,1.,1.,1.,1.))
REPRESENTATION_ITEM('')
) ;
#23 = (
BOUNDED_CURVE()
B_SPLINE_CURVE(3,(#154112,#154113,#154114,#154115,#154116,#154117,#154118),
 .UNSPECIFIED.,.F.,.F.)
B_SPLINE_CURVE_WITH_KNOTS((4,1,1,1,4),(0.,0.0911446219616379,0.182289243923276,
0.273433865884915,0.364578487846551),.UNSPECIFIED.)
CURVE()
GEOMETRIC_REPRESENTATION_ITEM()
RATIONAL_B_SPLINE_CURVE((1.,1.,1.,1.,1.,1.,1.))
REPRESENTATION_ITEM('')
) ;
#24 = (
BOUNDED_CURVE()
B_SPLINE_CURVE(3,(#154334,#154335,#154336,#154337,#154338,#154339,#154340,
#154341,#154342,#154343,#154344,#154345,#154346,#154347,#154348,#154349,
#154350,#154351,#154352),.UNSPECIFIED.,.F.,.F.)
B_SPLINE_CURVE_WITH_KNOTS((4,1,1,1,1,1,1,1,1,1,1,1,1,1,1,1,4),(0.,0.226732296973331,
0.464902013928651,0.70307173088397,0.9298040278573,1.15653632483063,1.39470604178595,
1.63287575874127,1.8596080557146,2.08634035268793,2.32451006964325,2.56267978659857,
2.7894120835719,3.01614438054523,3.25431409750055,3.49248381445586,3.7192161114292),
 .UNSPECIFIED.)
CURVE()
GEOMETRIC_REPRESENTATION_ITEM()
RATIONAL_B_SPLINE_CURVE((1.,1.,1.,1.,1.,1.,1.,1.,1.,1.,1.,1.,1.,1.,1.,1.,
1.,1.,1.))
REPRESENTATION_ITEM('')
) ;
#25 = (
BOUNDED_CURVE()
B_SPLINE_CURVE(2,(#154494,#154495,#154496,#154497,#154498,#154499,#154500,
#154501,#154502),.UNSPECIFIED.,.F.,.F.)
B_SPLINE_CURVE_WITH_KNOTS((3,2,2,2,3),(1.42918797785348,1.62618617063892,
1.86180561965816,2.09742506867739,2.29442326146283),.UNSPECIFIED.)
CURVE()
GEOMETRIC_REPRESENTATION_ITEM()
RATIONAL_B_SPLINE_CURVE((1.,1.,1.,0.707106781186548,1.,0.707106781186548,
1.,1.,1.))
REPRESENTATION_ITEM('')
) ;
#26 = (
BOUNDED_CURVE()
B_SPLINE_CURVE(2,(#154684,#154685,#154686,#154687,#154688,#154689,#154690,
#154691,#154692),.UNSPECIFIED.,.F.,.F.)
B_SPLINE_CURVE_WITH_KNOTS((3,2,2,2,3),(1.42918797785348,1.62618617063892,
1.86180561965816,2.09742506867739,2.29442326146283),.UNSPECIFIED.)
CURVE()
GEOMETRIC_REPRESENTATION_ITEM()
RATIONAL_B_SPLINE_CURVE((1.,1.,1.,0.707106781186548,1.,0.707106781186548,
1.,1.,1.))
REPRESENTATION_ITEM('')
) ;
#27 = (
BOUNDED_CURVE()
B_SPLINE_CURVE(3,(#173354,#173355,#173356,#173357,#173358,#173359,#173360,
#173361,#173362,#173363,#173364,#173365,#173366,#173367,#173368,#173369,
#173370,#173371,#173372,#173373,#173374,#173375,#173376,#173377,#173378,
#173379,#173380,#173381,#173382,#173383,#173384,#173385,#173386,#173387,
#173388,#173389,#173390,#173391,#173392,#173393,#173394,#173395,#173396,
#173397,#173398,#173399,#173400,#173401,#173402,#173403,#173404,#173405,
#173406,#173407,#173408,#173409,#173410,#173411,#173412,#173413,#173414,
#173415,#173416,#173417,#173418,#173419,#173420,#173421,#173422,#173423,
#173424,#173425,#173426,#173427,#173428,#173429,#173430,#173431,#173432,
#173433,#173434,#173435,#173436,#173437,#173438,#173439,#173440,#173441,
#173442,#173443,#173444,#173445,#173446,#173447,#173448,#173449,#173450,
#173451,#173452,#173453,#173454,#173455,#173456,#173457,#173458,#173459,
#173460,#173461,#173462,#173463,#173464,#173465,#173466,#173467,#173468,
#173469,#173470,#173471,#173472,#173473,#173474,#173475,#173476,#173477,
#173478,#173479,#173480,#173481,#173482,#173483,#173484,#173485,#173486,
#173487,#173488,#173489,#173490,#173491,#173492,#173493,#173494,#173495,
#173496,#173497,#173498,#173499,#173500,#173501,#173502,#173503,#173504,
#173505,#173506,#173507,#173508,#173509,#173510,#173511,#173512,#173513,
#173514,#173515,#173516,#173517,#173518,#173519,#173520,#173521,#173522,
#173523,#173524,#173525,#173526,#173527,#173528,#173529,#173530,#173531,
#173532,#173533,#173534,#173535,#173536,#173537,#173538,#173539,#173540,
#173541,#173542,#173543,#173544,#173545,#173546,#173547,#173548,#173549,
#173550,#173551,#173552,#173553,#173554,#173555,#173556,#173557,#173558,
#173559,#173560,#173561,#173562,#173563,#173564,#173565,#173566,#173567,
#173568,#173569,#173570,#173571,#173572,#173573,#173574,#173575,#173576,
#173577,#173578,#173579,#173580,#173581,#173582,#173583,#173584,#173585,
#173586,#173587,#173588,#173589,#173590,#173591,#173592,#173593,#173594,
#173595,#173596,#173597,#173598,#173599,#173600,#173601,#173602,#173603,
#173604,#173605,#173606,#173607,#173608,#173609,#173610,#173611,#173612,
#173613,#173614,#173615,#173616,#173617,#173618,#173619,#173620,#173621,
#173622,#173623,#173624,#173625,#173626,#173627,#173628,#173629,#173630,
#173631,#173632,#173633,#173634,#173635,#173636,#173637,#173638,#173639,
#173640,#173641,#173642,#173643,#173644,#173645,#173646,#173647,#173648,
#173649,#173650,#173651,#173652,#173653,#173654,#173655,#173656,#173657,
#173658,#173659,#173660,#173661,#173662,#173663,#173664,#173665,#173666,
#173667,#173668,#173669,#173670,#173671,#173672,#173673,#173674,#173675,
#173676,#173677,#173678,#173679,#173680,#173681,#173682,#173683,#173684,
#173685,#173686,#173687,#173688,#173689,#173690,#173691,#173692,#173693,
#173694,#173695,#173696,#173697,#173698,#173699,#173700,#173701,#173702,
#173703,#173704,#173705,#173706,#173707,#173708,#173709,#173710,#173711,
#173712,#173713,#173714,#173715,#173716,#173717,#173718,#173719,#173720,
#173721,#173722,#173723,#173724,#173725,#173726,#173727,#173728,#173729,
#173730,#173731,#173732,#173733,#173734,#173735,#173736,#173737,#173738,
#173739,#173740,#173741,#173742,#173743,#173744,#173745,#173746,#173747,
#173748,#173749,#173750,#173751,#173752,#173753,#173754,#173755,#173756,
#173757,#173758,#173759,#173760,#173761,#173762,#173763,#173764,#173765,
#173766,#173767,#173768,#173769,#173770,#173771,#173772,#173773,#173774,
#173775,#173776,#173777,#173778,#173779,#173780,#173781,#173782,#173783,
#173784,#173785,#173786,#173787,#173788,#173789,#173790,#173791,#173792,
#173793,#173794,#173795,#173796,#173797,#173798,#173799,#173800,#173801,
#173802,#173803,#173804,#173805,#173806,#173807,#173808,#173809,#173810,
#173811,#173812,#173813,#173814,#173815,#173816,#173817,#173818,#173819,
#173820,#173821,#173822,#173823,#173824,#173825,#173826,#173827,#173828,
#173829,#173830,#173831,#173832,#173833,#173834,#173835,#173836,#173837,
#173838,#173839,#173840,#173841,#173842,#173843,#173844,#173845,#173846,
#173847,#173848,#173849,#173850,#173851,#173852,#173853,#173854,#173855,
#173856,#173857,#173858,#173859,#173860,#173861,#173862,#173863,#173864,
#173865,#173866,#173867,#173868,#173869,#173870,#173871,#173872,#173873,
#173874,#173875,#173876,#173877,#173878,#173879,#173880,#173881,#173882,
#173883,#173884,#173885,#173886,#173887,#173888,#173889,#173890,#173891,
#173892,#173893,#173894,#173895,#173896,#173897,#173898,#173899,#173900,
#173901,#173902,#173903,#173904,#173905,#173906,#173907,#173908,#173909,
#173910,#173911,#173912,#173913,#173914,#173915,#173916,#173917,#173918,
#173919,#173920,#173921,#173922,#173923,#173924,#173925,#173926,#173927,
#173928,#173929,#173930,#173931,#173932,#173933,#173934,#173935,#173936,
#173937,#173938,#173939,#173940,#173941,#173942,#173943,#173944,#173945,
#173946,#173947,#173948,#173949,#173950,#173951,#173952,#173953,#173954,
#173955,#173956,#173957,#173958,#173959,#173960,#173961,#173962,#173963,
#173964,#173965,#173966,#173967,#173968,#173969,#173970,#173971,#173972,
#173973,#173974,#173975,#173976,#173977,#173978,#173979,#173980,#173981,
#173982,#173983,#173984,#173985,#173986,#173987,#173988,#173989,#173990,
#173991,#173992,#173993,#173994,#173995,#173996,#173997,#173998,#173999,
#174000,#174001,#174002,#174003,#174004,#174005,#174006,#174007,#174008,
#174009,#174010,#174011,#174012,#174013,#174014,#174015,#174016,#174017,
#174018,#174019,#174020,#174021,#174022,#174023,#174024,#174025,#174026,
#174027,#174028,#174029,#174030,#174031,#174032,#174033,#174034,#174035,
#174036,#174037,#174038,#174039,#174040,#174041,#174042,#174043,#174044,
#174045,#174046,#174047,#174048,#174049,#174050,#174051,#174052,#174053,
#174054,#174055,#174056,#174057,#174058,#174059,#174060,#174061,#174062,
#174063,#174064,#174065,#174066,#174067,#174068,#174069,#174070,#174071,
#174072,#174073,#174074,#174075,#174076,#174077,#174078,#174079,#174080,
#174081,#174082,#174083,#174084,#174085,#174086,#174087,#174088,#174089,
#174090,#174091,#174092,#174093,#174094,#174095,#174096,#174097,#174098,
#174099,#174100,#174101,#174102,#174103,#174104,#174105,#174106,#174107,
#174108,#174109,#174110,#174111,#174112,#174113,#174114,#174115,#174116,
#174117,#174118,#174119,#174120,#174121,#174122,#174123,#174124,#174125,
#174126,#174127,#174128,#174129,#174130,#174131,#174132,#174133,#174134,
#174135,#174136,#174137,#174138,#174139,#174140,#174141,#174142,#174143,
#174144,#174145,#174146,#174147,#174148,#174149,#174150,#174151,#174152,
#174153,#174154,#174155,#174156,#174157,#174158,#174159,#174160,#174161,
#174162,#174163,#174164,#174165,#174166,#174167,#174168,#174169,#174170,
#174171,#174172,#174173,#174174,#174175,#174176,#174177,#174178,#174179,
#174180,#174181,#174182,#174183,#174184,#174185,#174186,#174187,#174188,
#174189,#174190,#174191,#174192,#174193,#174194,#174195,#174196,#174197,
#174198,#174199,#174200,#174201,#174202,#174203,#174204,#174205,#174206,
#174207,#174208,#174209,#174210,#174211,#174212,#174213,#174214,#174215,
#174216,#174217,#174218,#174219,#174220,#174221,#174222,#174223,#174224,
#174225,#174226,#174227,#174228,#174229,#174230,#174231,#174232,#174233,
#174234,#174235,#174236,#174237,#174238,#174239,#174240,#174241,#174242,
#174243,#174244,#174245,#174246,#174247,#174248,#174249,#174250,#174251,
#174252,#174253,#174254,#174255,#174256,#174257,#174258,#174259,#174260,
#174261,#174262,#174263,#174264,#174265,#174266,#174267,#174268,#174269,
#174270,#174271,#174272,#174273,#174274,#174275,#174276,#174277,#174278,
#174279,#174280,#174281,#174282,#174283,#174284,#174285,#174286,#174287,
#174288,#174289,#174290,#174291,#174292,#174293,#174294,#174295,#174296,
#174297,#174298,#174299,#174300,#174301,#174302,#174303,#174304,#174305,
#174306,#174307,#174308,#174309,#174310,#174311,#174312,#174313,#174314,
#174315,#174316,#174317,#174318,#174319,#174320,#174321,#174322,#174323,
#174324,#174325,#174326,#174327,#174328,#174329,#174330,#174331,#174332,
#174333,#174334,#174335,#174336,#174337,#174338,#174339,#174340,#174341,
#174342,#174343,#174344,#174345,#174346,#174347,#174348,#174349,#174350,
#174351,#174352,#174353,#174354,#174355,#174356,#174357,#174358,#174359,
#174360,#174361,#174362,#174363,#174364,#174365,#174366,#174367,#174368,
#174369,#174370,#174371,#174372,#174373,#174374,#174375,#174376,#174377,
#174378,#174379,#174380,#174381,#174382,#174383,#174384,#174385,#174386,
#174387,#174388,#174389,#174390,#174391,#174392,#174393,#174394,#174395,
#174396,#174397,#174398,#174399,#174400,#174401,#174402,#174403,#174404,
#174405,#174406,#174407,#174408,#174409,#174410,#174411),.UNSPECIFIED.,
 .F.,.F.)
B_SPLINE_CURVE_WITH_KNOTS((4,1,1,1,1,1,1,1,1,1,1,1,1,1,1,1,1,1,1,1,1,1,
1,1,1,1,1,1,1,1,1,1,1,1,1,1,1,1,1,1,1,1,1,1,1,1,1,1,1,1,1,1,1,1,1,1,1,1,
1,1,1,1,1,1,1,1,1,1,1,1,1,1,1,1,1,1,1,1,1,1,1,1,1,1,1,1,1,1,1,1,1,1,1,1,
1,1,1,1,1,1,1,1,1,1,1,1,1,1,1,1,1,1,1,1,1,1,1,1,1,1,1,1,1,1,1,1,1,1,1,1,
1,1,1,1,1,1,1,1,1,1,1,1,1,1,1,1,1,1,1,1,1,1,1,1,1,1,1,1,1,1,1,1,1,1,1,1,
1,1,1,1,1,1,1,1,1,1,1,1,1,1,1,1,1,1,1,1,1,1,1,1,1,1,1,1,1,1,1,1,1,1,1,1,
1,1,1,1,1,1,1,1,1,1,1,1,1,1,1,1,1,1,1,1,1,1,1,1,1,1,1,1,1,1,1,1,1,1,1,1,
1,1,1,1,1,1,1,1,1,1,1,1,1,1,1,1,1,1,1,1,1,1,1,1,1,1,1,1,1,1,1,1,1,1,1,1,
1,1,1,1,1,1,1,1,1,1,1,1,1,1,1,1,1,1,1,1,1,1,1,1,1,1,1,1,1,1,1,1,1,1,1,1,
1,1,1,1,1,1,1,1,1,1,1,1,1,1,1,1,1,1,1,1,1,1,1,1,1,1,1,1,1,1,1,1,1,1,1,1,
1,1,1,1,1,1,1,1,1,1,1,1,1,1,1,1,1,1,1,1,1,1,1,1,1,1,1,1,1,1,1,1,1,1,1,1,
1,1,1,1,1,1,1,1,1,1,1,1,1,1,1,1,1,1,1,1,1,1,1,1,1,1,1,1,1,1,1,1,1,1,1,1,
1,1,1,1,1,1,1,1,1,1,1,1,1,1,1,1,1,1,1,1,1,1,1,1,1,1,1,1,1,1,1,1,1,1,1,1,
1,1,1,1,1,1,1,1,1,1,1,1,1,1,1,1,1,1,1,1,1,1,1,1,1,1,1,1,1,1,1,1,1,1,1,1,
1,1,1,1,1,1,1,1,1,1,1,1,1,1,1,1,1,1,1,1,1,1,1,1,1,1,1,1,1,1,1,1,1,1,1,1,
1,1,1,1,1,1,1,1,1,1,1,1,1,1,1,1,1,1,1,1,1,1,1,1,1,1,1,1,1,1,1,1,1,1,1,1,
1,1,1,1,1,1,1,1,1,1,1,1,1,1,1,1,1,1,1,1,1,1,1,1,1,1,1,1,1,1,1,1,1,1,1,1,
1,1,1,1,1,1,1,1,1,1,1,1,1,1,1,1,1,1,1,1,1,1,1,1,1,1,1,1,1,1,1,1,1,1,1,1,
1,1,1,1,1,1,1,1,1,1,1,1,1,1,1,1,1,1,1,1,1,1,1,1,1,1,1,1,1,1,1,1,1,1,1,1,
1,1,1,1,1,1,1,1,1,1,1,1,1,1,1,1,1,1,1,1,1,1,1,1,1,1,1,1,1,1,1,1,1,1,1,1,
1,1,1,1,1,1,1,1,1,1,1,1,1,1,1,1,1,1,1,1,1,1,1,1,1,1,1,1,1,1,1,1,1,1,1,1,
1,1,1,1,1,1,1,1,1,1,1,1,1,1,1,1,1,1,1,1,1,1,1,1,1,1,1,1,1,1,1,1,1,1,1,1,
1,1,1,1,1,1,1,1,1,1,1,1,1,1,1,1,1,1,1,1,1,1,1,1,1,1,1,1,1,1,1,1,1,1,1,1,
1,1,1,1,1,1,1,1,1,1,1,1,1,1,1,1,1,1,1,1,1,1,1,1,1,1,1,1,1,1,1,1,1,1,1,1,
1,1,1,1,1,1,1,1,1,1,1,1,1,1,1,1,1,1,1,1,1,1,1,1,1,1,1,1,1,1,1,1,1,1,1,1,
1,1,1,1,1,1,1,1,1,1,1,1,1,1,1,1,1,1,1,1,1,1,1,1,1,1,1,1,1,1,1,1,1,1,1,1,
1,1,1,1,1,1,1,1,1,1,1,1,1,1,1,1,1,1,1,1,1,1,1,1,1,1,1,1,1,1,1,1,1,1,1,1,
1,1,1,1,1,1,1,1,1,1,1,1,1,1,1,1,1,1,1,1,1,1,1,1,1,1,1,1,1,1,1,1,1,1,1,1,
1,1,1,1,1,1,1,1,1,1,1,1,1,1,1,1,1,1,1,1,1,1,1,1,1,1,1,1,1,1,1,1,1,1,1,1,
1,1,1,1,1,1,1,1,1,1,1,1,1,1,1,1,1,1,1,1,1,1,1,1,1,4),(0.,0.01797683372391,
0.286633051710584,0.555289278308216,0.823945516665782,1.09260176953922,
1.36125803873948,1.62991432588463,1.89857063164012,2.16722695661301,2.43588330050525,
2.70453966304674,2.9731960431531,3.24185243981471,3.51050885133453,3.77916527610465,
4.04782171198515,4.31647815691489,4.58513460847725,4.85379106430677,5.12244752187208,
5.39110397865606,5.65976043217153,5.92841687990537,6.19707331956994,6.46572974881596,
6.73438616570634,7.00304256821933,7.2716989549161,7.5403553242696,7.809011675483,
8.07766800769526,8.34632432089157,8.61498061505147,8.8836368910788,9.15229314997201,
9.4209493936865,9.68960562442157,9.95826184531348,10.226918059948,10.4955742727586,
10.7642304884925,11.0328867113173,11.3015429448574,11.5701991918227,11.8388554546081,
12.1075117346518,12.3761680332469,12.6448243507434,12.9134806874637,13.1821370428496,
13.450793416388,13.7194498067883,13.9881062128412,14.2567626326955,14.5254190645885,
14.7940755062772,15.0627319555912,15.3313884100611,15.6000448672586,15.8687013246492,
16.1373577797,16.4060142299691,16.6746706729765,16.9433271065265,17.2119835283531,
17.4806399366567,17.7492963295502,18.0179527057767,18.286609063996,18.555265403637,
18.8239217240786,19.0925780255742,19.3612343083975,19.6298905737625,19.898546823017,
20.1672030584666,20.4358592827168,20.7045154992928,20.973171712245,21.2418279262962,
21.5104841459723,21.7791403749736,22.0477966165324,22.316452872948,22.585109146262,
22.8537654375589,23.1224217478187,23.3910780770929,23.6597344254327,23.9283907920352,
24.197047176159,24.4657035763222,24.7343599911301,25.0030164185931,25.2716728568073,
25.5403293034427,25.8089857562333,26.0776422126729,26.3462986702843,26.6149551265448,
26.8836115789212,27.1522680250308,27.4209244624423,27.6895808890659,27.9582373027346,
28.2268937018004,28.4955500845261,28.7642064498512,29.0328627966379,29.3015191245544,
29.5701754332357,29.838831723217,30.1074879950829,30.3761442503694,30.6448004907916,
30.9134567190168,31.1821129380756,31.450769151893,31.7194253649682,31.9880815819663,
32.2567378070174,32.5253940433706,32.7940502938785,33.0627065604467,33.3313628447765,
33.6000191476151,33.8686754696427,34.1373318106287,34.405988170366,34.6746445478242,
34.9433009420458,35.2119573513747,35.480613774244,35.7492702085419,36.0179266522368,
36.2865831029275,36.5552395582669,36.8238960157264,37.0925524727952,37.3612089269773,
37.6298653757534,37.8985218168153,38.1671782477952,38.4358346667239,38.7044910715485,
38.9731474607866,39.2418038328672,39.5104601869391,39.7791165220837,40.0477728382212,
40.3164291352602,40.5850854140292,40.8537416754418,41.1223979213679,41.3910541539077,
41.6597103761025,41.9283665914244,42.1970228042084,42.4656790192,42.7343352406829,
43.0029914723808,43.2716477171096,43.540303977354,43.8089602546436,44.0776165503516,
44.3462728649052,44.614929198697,44.883585551232,45.1522419220568,45.4208983099307,
45.6895547136931,45.9582111315299,46.2268675617156,46.4955240020317,46.7641804503338,
47.0328369041642,47.3014933611089,47.5701498186329,47.8388062742058,48.107462725373,
48.3761191696448,48.6447756048012,48.9134320285537,49.1820884390673,49.4507448344197,
49.7194012133072,49.9880575743413,50.2567139168934,50.5253702402807,50.7940265446884,
51.0626828303152,51.3313390982961,51.5999953498901,51.8686515873141,52.1373078130706,
52.4059640305862,52.6746202437936,52.9432764573682,53.211932675918,53.480588903259,
53.7492451427202,54.0179013967021,54.2865576673334,54.5552139557853,54.823870263115,
55.0925265894471,55.3611829348992,55.6298392987282,55.8984956802486,56.1671520780245,
56.4358084907065,56.7044649163381,56.9731213530494,57.2417777985307,57.5104342505384,
57.7790907065743,58.0477471641719,58.3164036208043,58.5850600739368,58.8537165211707,
59.1223729600609,59.39102938849,59.6596858042645,59.9283422056975,60.1969985910129,
60.4656549590995,60.7343113087676,61.0029676396243,61.2716239512389,61.540280244075,
61.808936518638,62.0775927763821,62.3462490189291,62.6149052488546,62.8835614690812,
63.1522176834332,63.4208738963055,63.6895301124163,63.9581863359981,64.2268425704115,
64.4954988186027,64.7641550825741,65.0328113641112,65.3014676640435,65.5701239831253,
65.8387803211949,66.1074366781083,66.3760930528907,66.6447494446373,66.9134058517341,
67.1820622726558,67.4507187053199,67.7193751477252,67.988031597487,68.256688052277,
68.5253445095709,68.7940009668648,69.0626574216546,69.3313138714164,69.5999703138218,
69.8686267464858,70.1372831674076,70.4059395745042,70.6745959662509,70.9432523410334,
71.2119086979469,71.4805650360164,71.7492213550982,72.0178776550306,72.2865339365675,
72.5551902005389,72.8238464487301,73.0925026831433,73.3611589067251,73.6298151228357,
73.8984713357081,74.1671275500599,74.4357837702864,74.7044400002118,74.9730962427587,
75.2417525005027,75.5104087750655,75.7790650679015,76.047721379516,76.3163777103726,
76.5850340600405,76.853690428127,77.1223468134422,77.391003214875,77.6596596306495,
77.9283160590784,78.1969724979684,78.4656289452021,78.7342853983344,79.0029418549666,
79.2715983125641,79.5402547685998,79.8089112206075,80.0775676660886,80.3462241027997,
80.6148805284312,80.8835369411131,81.1521933388889,81.4208497204091,81.689506084238,
81.9581624296899,82.2268187560219,82.4954750633515,82.7641313518033,83.0327876224345,
83.3014438764161,83.5701001158772,83.838756343218,84.1074125617677,84.3760687753422,
84.6447249885494,84.913381206065,85.1820374318212,85.4506936692451,85.719349920839,
85.9880061888197,86.2566624744465,86.5253187788541,86.7939751022413,87.0626314447932,
87.3312878058273,87.5999441847146,87.8686005800667,88.1372569905802,88.4059134143327,
88.6745698494889,88.9432262937606,89.2118827449277,89.4805392005005,89.7491956580243,
90.0178521149689,90.2865085687992,90.5551650171012,90.8238214574172,91.0924778876028,
91.3611343054394,91.6297907092016,91.8984470970753,92.1671034679,92.4357598204347,
92.7044161542264,92.9730724687798,93.2417287644878,93.5103850417773,93.7790413020216,
94.0476975467502,94.3163537784479,94.5850099999307,94.8536662149221,95.1223224277061,
95.390978643028,95.6596348652226,95.9282910977624,96.1969473436883,96.4656036051009,
96.7342598838697,97.0029161809086,97.2715724970461,97.5402288321905,97.8088851862623,
98.0775415583427,98.3461979475807,98.6148543524051,98.8835107713336,99.1521672023136,
99.4208236433754,99.6894800921513,99.9581365463333,100.226793003402,100.495449460861,
100.7641059162,101.032762366891,101.301418810586,101.570075244884,101.838731667753,
102.107388077082,102.376044471303,102.644700848761,102.913357208498,103.182013549484,
103.450669871511,103.71932617435,103.98798245868,104.256638725248,104.525294975755,
104.793951212108,105.062607437159,105.331263654157,105.599919867233,105.86857608105,
106.137232300108,106.405888528334,106.674544768756,106.943201024042,107.211857295908,
107.480513585889,107.74916989457,108.017826222487,108.286482569273,108.555138934598,
108.823795317324,109.09245171639,109.361108130058,109.629764556682,109.898420994093,
110.167077440202,110.435733892579,110.704390348839,110.97304680645,111.24170326289,
111.51035971568,111.779016162316,112.04767260053,112.316329027993,112.5849854428,
112.853641842963,113.122298227087,113.39095459369,113.659610942029,113.928267271303,
114.196923581563,114.46557987286,114.734236146174,115.002892402589,115.271548644148,
115.540204873149,115.808861092825,116.077517306876,116.346173519828,116.614829736404,
116.883485960654,117.152142196103,117.420798445358,117.689454710722,117.958110993546,
118.226767295041,118.495423615483,118.764079955123,119.032736313343,119.301392689569,
119.570049082462,119.838705490766,120.107361912592,120.376018346142,120.644674789149,
120.913331239418,121.181987694469,121.45064415186,121.719300609057,121.987957063527,
122.256613512841,122.525269954529,122.793926386422,123.062582806276,123.331239212329,
123.599895602729,123.868551976268,124.137208331653,124.405864668374,124.67452098587,
124.943177284465,125.211833564508,125.480489827294,125.749146074259,126.017802307799,
126.286458530624,126.555114746357,126.823770959168,127.092427173802,127.361083394694,
127.629739625429,127.898395869143,128.167052128037,128.435708404064,128.704364698224,
128.97302101142,129.241677343633,129.510333694846,129.7789900642,130.047646450897,
130.31630285341,130.5849592703,130.853615699547,131.122272139211,131.390928586945,
131.659585040461,131.928241497245,132.19689795481,132.46555441064,132.734210862202,
133.002867307132,133.271523743013,133.540180167783,133.808836579303,134.077492975965,
134.346149356071,134.614805718613,134.883462062505,135.152118387478,135.420774693234,
135.689430980379,135.958087249579,136.226743502453,136.49539974081,136.76405596741,
137.032712185392,137.301368398783,137.570024612174,137.838680830155,138.107337056755,
138.375993295112,138.644649547986,138.913305817186,139.181962104332,139.450618410087,
139.71927473506,139.987931078952,140.256587441494,140.525243821601,140.793900218262,
141.062556629782,141.331213054552,141.599869490433,141.868525935363,142.137182386925,
142.405838842755,142.67449530032,142.943151757104,143.21180821062,143.480464658354,
143.749121098019,144.017777527265,144.286433944155,144.555090346668,144.823746733365,
145.092403102719,145.361059453932,145.629715786145,145.898372099341,146.167028393501,
146.435684669529,146.704340928422,146.972997172137,147.241653402872,147.510309623764,
147.778965838398,148.047622051209,148.316278266943,148.584934489768,148.853590723308,
149.122246970274,149.390903233059,149.659559513103,149.928215811698,150.196872129195,
150.465528465915,150.734184821301,151.00284119484,151.27149758524,151.540153991293,
151.808810411148,152.077466843041,152.34612328473,152.614779734044,152.883436188514,
153.152092645711,153.420749103102,153.689405558153,153.958062008422,154.22671845143,
154.49537488498,154.764031306806,155.03268771511,155.301344108004,155.57000048423,
155.838656842449,156.107313182091,156.375969502532,156.644625804028,156.913282086851,
157.181938352216,157.450594601471,157.719250836921,157.987907061171,158.256563277747,
158.525219490699,158.793875704751,159.062531924427,159.331188153428,159.599844394987,
159.868500651403,160.137156924717,160.405813216014,160.674469526274,160.943125855548,
161.211782203888,161.480438570491,161.749094954615,162.017751354778,162.286407769586,
162.555064197049,162.823720635263,163.092377081899,163.361033534689,163.629689991129,
163.898346448741,164.167002905001,164.435659357378,164.704315803488,164.972972240899,
165.241628667523,165.510285081192,165.778941480257,166.047597862983,166.316254228308,
166.584910575095,166.853566903012,167.122223211693,167.390879501675,167.659535773541,
167.928192028827,168.19684826925,168.465504497475,168.734160716534,169.002816930351,
169.271473143427,169.540129360425,169.808785585476,170.077441821829,170.346098072337,
170.614754338905,170.883410623235,171.152066926074,171.420723248102,171.689379589088,
171.958035948825,172.226692326284,172.495348720505,172.764005129834,173.032661552704,
173.301317987002,173.569974430697,173.838630881388,174.107287336727,174.375943794187,
174.644600251255,174.913256705437,175.181913154214,175.450569595276,175.719226026256,
175.987882445184,176.256538850009,176.525195239247,176.793851611328,177.0625079654,
177.331164300545,177.599820616682,177.868476913721,178.137133192491,178.405789453903,
178.674445699829,178.943101932369,179.211758154564,179.480414369886,179.74907058267,
180.017726797662,180.286383019145,180.555039250843,180.823695495572,181.092351755816,
181.361008033106,181.629664328814,181.898320643368,182.16697697716,182.435633329695,
182.70428970052,182.972946088394,183.241602492156,183.510258909993,183.778915340179,
184.047571780495,184.316228228797,184.584884682628,184.853541139572,185.122197597096,
185.39085405267,185.659510503837,185.928166948109,186.196823383265,186.465479807018,
186.734136217531,187.002792612884,187.271448991771,187.540105352806,187.808761695358,
188.077418018745,188.346074323153,188.61473060878,188.883386876761,189.152043128355,
189.420699365779,189.689355591536,189.958011809051,190.226668022259,190.495324235834,
190.763980454383,191.032636681725,191.301292921186,191.569949175168,191.838605445799,
192.107261734251,192.375918041581,192.644574367913,192.913230713365,193.181887077194,
193.450543458715,193.719199856491,193.987856269173,194.256512694805,194.525169131516,
194.793825576997,195.062482029005,195.331138485041,195.599794942639,195.868451399271,
196.137107852404,196.405764299638,196.674420738528,196.943077166957,197.211733582732,
197.480389984165,197.749046369481,198.017702737567,198.286359087236,198.555015418092,
198.823671729707,199.092328022543,199.360984297106,199.62964055485,199.898296797397,
200.166953027323,200.43560924755,200.704265461902,200.972921674774,201.241577890885,
201.510234114467,201.77889034888,202.047546597072,202.316202861043,202.584859142581,
202.853515442513,203.122171761595,203.390828099665,203.659484456579,203.928140831361,
204.196797223108,204.465453630205,204.734110051127,205.002766483791,205.271422926197,
205.540079375959,205.808735830749,206.077392288043,206.346048745337,206.614705200127,
206.883361649889,207.152018092295,207.420674524959,207.689330945881,207.957987352978,
208.226643744725,208.495300119508,208.763956476421,209.032612814491,209.301269133573,
209.569925433505,209.838581715043,210.107237979014,210.375894227206,210.644550461619,
210.913206685201,211.181862901312,211.450519114184,211.719175328536,211.987831548763,
212.256487778689,212.525144021236,212.79380027898,213.062456553543,213.331112846379,
213.599769157994,213.868425488851,214.137081838519,214.405738206606,214.674394591921,
214.943050993354,215.211707409129,215.480363837558,215.749020276448,216.017676723682,
216.286333176815,216.554989633447,216.823646091045,217.092302547081,217.360958999089,
217.62961544457,217.898271881281,218.166928306913,218.435584719595,218.704241117371,
218.972897498892,219.241553862721,219.510210208173,219.778866534505,220.047522841835,
220.316179130287,220.584835400918,220.8534916549,221.122147894361,221.390804121702,
221.659460340252,221.928116553827,222.196772767034,222.46542898455,222.734085210306,
223.00274144773,223.271397699324,223.540053967305,223.808710252932,224.07736655734,
224.346022880728,224.61467922328,224.883335584314,225.151991963201,225.420648358554,
225.689304769068,225.95796119282,226.226617627977,226.495274072249,226.763930523416,
227.032586978989,227.301243436513,227.569899893458,227.838556347288,228.10721279559,
228.375869235907,228.644525666093,228.913182083929,229.181838487692,229.450494875566,
229.719151246391,229.987807598926,230.256463932718,230.525120247271,230.79377654298,
231.062432820269,231.331089080514,231.599745325243,231.868401556941,232.137057778424,
232.405713993415,232.674370206199,232.943026421521,233.211682643716,233.480338876256,
233.748995122182,234.017651383595,234.286307662364,234.554963959403,234.823620275541,
235.092276610685,235.360932964757,235.629589336838,235.898245726076,236.166902130901,
236.43555854983,236.70421498081,236.972871421872,237.241527870648,237.51018432483,
237.778840781899,238.047497239359,238.316153694698,238.584810145389,238.853466589084,
239.122123023382,239.390779446251,239.65943585558,239.928092249802,240.19674862726,
240.465404986998,240.734061327984,241.002717650011,241.27137395285,241.54003023718,
241.808686503748,242.077342754256,242.345998990609,242.614655215661,242.883311432659,
243.151967645734,243.420623859552,243.68928007861,243.957936306836,244.226592547258,
244.495248802545,244.763905074411,245.032561364392,245.301217673074,245.56987400099,
245.838530347777,246.107186713102,246.375843095828,246.644499494894,246.913155908563,
247.181812335186,247.450468772598,247.719125218708,247.987781671084,248.256438127345,
248.525094584956,248.793751041396,249.062407494187,249.331063940822,249.599720379036,
249.8683768065,250.137033221308,250.405689621471,250.674346005595,250.943002372197,
251.211658720537,251.480315049812,251.748971360071,252.017627651368,252.286283924683,
252.554940181098,252.823596422657,253.092252651658,253.360908871335,253.629565085386,
253.898221298338,254.166877514914,254.435533739165,254.704189974614,254.972846223869,
255.241502489234,255.510158772057,255.778815073553,256.047471393995,256.316127733635,
256.584784091854,256.85344046808,257.122096860973,257.390753269276,257.659409691102,
257.928066124652,258.196722567659,258.465379017928,258.734035472978,259.002691930368,
259.271348387566,259.540004842035,259.808661291349,260.077317733037,260.345974164929,
260.614630584783,260.883286990836,261.151943381235,261.420599754774,261.689256110159,
261.957912446879,262.226568764375,262.49522506297,262.763881343014,263.032537605798,
263.301193852763,263.569850086303,263.838506309127,264.107162524861,264.375818737671,
264.644474952305,264.913131173196,265.181787403931,265.450443647645,265.719099906538,
265.987756182565,266.256412476724,266.52506878992,266.793725122132,267.062381473345,
267.331037842698,267.599694229394,267.868350631907,268.137007048797,268.405663478042,
268.674319917706,268.94297636544,269.211632818955,269.480289275739,269.748945733304,
270.017602189133,270.286258640695,270.554915085624,270.823571521504,271.092227946274,
271.360884357793,271.629540754454,271.89819713456,272.166853497101,272.435509840993,
272.704166165965,272.97282247172,273.241478758865,273.510135028065,273.778791280938,
274.047447519295,274.316103745894,274.584759963875,274.853416177266,275.122072390656,
275.390728608637,275.659384835237,275.928041073593,276.196697326466,276.465353595666,
276.734009882811,277.002666188566,277.271322513539,277.53997885743,277.808635219972,
278.077291600077,278.345947996739,278.614604408258,278.883260833028,279.151917268908,
279.420573713837,279.689230165399,279.957886621228,280.226543078793,280.495199535576,
280.763855989092,281.032512436825,281.301168876489,281.569825305735,281.838481722625,
282.107138125138,282.375794511834,282.644450881187,282.9131072324,283.140531716307),
 .UNSPECIFIED.)
CURVE()
GEOMETRIC_REPRESENTATION_ITEM()
RATIONAL_B_SPLINE_CURVE((1.,1.,1.,1.,1.,1.,1.,1.,1.,1.,1.,1.,1.,1.,1.,1.,
1.,1.,1.,1.,1.,1.,1.,1.,1.,1.,1.,1.,1.,1.,1.,1.,1.,1.,1.,1.,1.,1.,1.,1.,
1.,1.,1.,1.,1.,1.,1.,1.,1.,1.,1.,1.,1.,1.,1.,1.,1.,1.,1.,1.,1.,1.,1.,1.,
1.,1.,1.,1.,1.,1.,1.,1.,1.,1.,1.,1.,1.,1.,1.,1.,1.,1.,1.,1.,1.,1.,1.,1.,
1.,1.,1.,1.,1.,1.,1.,1.,1.,1.,1.,1.,1.,1.,1.,1.,1.,1.,1.,1.,1.,1.,1.,1.,
1.,1.,1.,1.,1.,1.,1.,1.,1.,1.,1.,1.,1.,1.,1.,1.,1.,1.,1.,1.,1.,1.,1.,1.,
1.,1.,1.,1.,1.,1.,1.,1.,1.,1.,1.,1.,1.,1.,1.,1.,1.,1.,1.,1.,1.,1.,1.,1.,
1.,1.,1.,1.,1.,1.,1.,1.,1.,1.,1.,1.,1.,1.,1.,1.,1.,1.,1.,1.,1.,1.,1.,1.,
1.,1.,1.,1.,1.,1.,1.,1.,1.,1.,1.,1.,1.,1.,1.,1.,1.,1.,1.,1.,1.,1.,1.,1.,
1.,1.,1.,1.,1.,1.,1.,1.,1.,1.,1.,1.,1.,1.,1.,1.,1.,1.,1.,1.,1.,1.,1.,1.,
1.,1.,1.,1.,1.,1.,1.,1.,1.,1.,1.,1.,1.,1.,1.,1.,1.,1.,1.,1.,1.,1.,1.,1.,
1.,1.,1.,1.,1.,1.,1.,1.,1.,1.,1.,1.,1.,1.,1.,1.,1.,1.,1.,1.,1.,1.,1.,1.,
1.,1.,1.,1.,1.,1.,1.,1.,1.,1.,1.,1.,1.,1.,1.,1.,1.,1.,1.,1.,1.,1.,1.,1.,
1.,1.,1.,1.,1.,1.,1.,1.,1.,1.,1.,1.,1.,1.,1.,1.,1.,1.,1.,1.,1.,1.,1.,1.,
1.,1.,1.,1.,1.,1.,1.,1.,1.,1.,1.,1.,1.,1.,1.,1.,1.,1.,1.,1.,1.,1.,1.,1.,
1.,1.,1.,1.,1.,1.,1.,1.,1.,1.,1.,1.,1.,1.,1.,1.,1.,1.,1.,1.,1.,1.,1.,1.,
1.,1.,1.,1.,1.,1.,1.,1.,1.,1.,1.,1.,1.,1.,1.,1.,1.,1.,1.,1.,1.,1.,1.,1.,
1.,1.,1.,1.,1.,1.,1.,1.,1.,1.,1.,1.,1.,1.,1.,1.,1.,1.,1.,1.,1.,1.,1.,1.,
1.,1.,1.,1.,1.,1.,1.,1.,1.,1.,1.,1.,1.,1.,1.,1.,1.,1.,1.,1.,1.,1.,1.,1.,
1.,1.,1.,1.,1.,1.,1.,1.,1.,1.,1.,1.,1.,1.,1.,1.,1.,1.,1.,1.,1.,1.,1.,1.,
1.,1.,1.,1.,1.,1.,1.,1.,1.,1.,1.,1.,1.,1.,1.,1.,1.,1.,1.,1.,1.,1.,1.,1.,
1.,1.,1.,1.,1.,1.,1.,1.,1.,1.,1.,1.,1.,1.,1.,1.,1.,1.,1.,1.,1.,1.,1.,1.,
1.,1.,1.,1.,1.,1.,1.,1.,1.,1.,1.,1.,1.,1.,1.,1.,1.,1.,1.,1.,1.,1.,1.,1.,
1.,1.,1.,1.,1.,1.,1.,1.,1.,1.,1.,1.,1.,1.,1.,1.,1.,1.,1.,1.,1.,1.,1.,1.,
1.,1.,1.,1.,1.,1.,1.,1.,1.,1.,1.,1.,1.,1.,1.,1.,1.,1.,1.,1.,1.,1.,1.,1.,
1.,1.,1.,1.,1.,1.,1.,1.,1.,1.,1.,1.,1.,1.,1.,1.,1.,1.,1.,1.,1.,1.,1.,1.,
1.,1.,1.,1.,1.,1.,1.,1.,1.,1.,1.,1.,1.,1.,1.,1.,1.,1.,1.,1.,1.,1.,1.,1.,
1.,1.,1.,1.,1.,1.,1.,1.,1.,1.,1.,1.,1.,1.,1.,1.,1.,1.,1.,1.,1.,1.,1.,1.,
1.,1.,1.,1.,1.,1.,1.,1.,1.,1.,1.,1.,1.,1.,1.,1.,1.,1.,1.,1.,1.,1.,1.,1.,
1.,1.,1.,1.,1.,1.,1.,1.,1.,1.,1.,1.,1.,1.,1.,1.,1.,1.,1.,1.,1.,1.,1.,1.,
1.,1.,1.,1.,1.,1.,1.,1.,1.,1.,1.,1.,1.,1.,1.,1.,1.,1.,1.,1.,1.,1.,1.,1.,
1.,1.,1.,1.,1.,1.,1.,1.,1.,1.,1.,1.,1.,1.,1.,1.,1.,1.,1.,1.,1.,1.,1.,1.,
1.,1.,1.,1.,1.,1.,1.,1.,1.,1.,1.,1.,1.,1.,1.,1.,1.,1.,1.,1.,1.,1.,1.,1.,
1.,1.,1.,1.,1.,1.,1.,1.,1.,1.,1.,1.,1.,1.,1.,1.,1.,1.,1.,1.,1.,1.,1.,1.,
1.,1.,1.,1.,1.,1.,1.,1.,1.,1.,1.,1.,1.,1.,1.,1.,1.,1.,1.,1.,1.,1.,1.,1.,
1.,1.,1.,1.,1.,1.,1.,1.,1.,1.,1.,1.,1.,1.,1.,1.,1.,1.,1.,1.,1.,1.,1.,1.,
1.,1.,1.,1.,1.,1.,1.,1.,1.,1.,1.,1.,1.,1.,1.,1.,1.,1.,1.,1.,1.,1.,1.,1.,
1.,1.,1.,1.,1.,1.,1.,1.,1.,1.,1.,1.,1.,1.,1.,1.,1.,1.,1.,1.,1.,1.,1.,1.,
1.,1.,1.,1.,1.,1.,1.,1.,1.,1.,1.,1.,1.,1.,1.,1.,1.,1.,1.,1.,1.,1.,1.,1.,
1.,1.,1.,1.,1.,1.,1.,1.,1.,1.,1.,1.,1.,1.,1.,1.,1.,1.,1.,1.,1.,1.,1.,1.,
1.,1.,1.,1.,1.,1.,1.,1.,1.,1.,1.,1.,1.,1.,1.,1.,1.,1.,1.,1.,1.,1.,1.,1.,
1.,1.,1.,1.,1.,1.,1.,1.,1.,1.,1.,1.,1.,1.,1.,1.,1.,1.,1.,1.,1.,1.,1.,1.,
1.,1.,1.,1.,1.,1.,1.,1.,1.,1.,1.,1.,1.,1.,1.,1.,1.,1.,1.,1.,1.,1.,1.,1.,
1.,1.,1.,1.,1.,1.,1.,1.,1.,1.,1.,1.,1.,1.,1.,1.,1.,1.,1.,1.,1.,1.,1.,1.,
1.,1.,1.,1.,1.,1.,1.,1.,1.,1.))
REPRESENTATION_ITEM('')
) ;
#28 = (
BOUNDED_CURVE()
B_SPLINE_CURVE(3,(#174481,#174482,#174483,#174484,#174485,#174486,#174487),
 .UNSPECIFIED.,.F.,.F.)
B_SPLINE_CURVE_WITH_KNOTS((4,1,1,1,4),(0.,0.0911446219616379,0.182289243923276,
0.273433865884915,0.364578487846551),.UNSPECIFIED.)
CURVE()
GEOMETRIC_REPRESENTATION_ITEM()
RATIONAL_B_SPLINE_CURVE((1.,1.,1.,1.,1.,1.,1.))
REPRESENTATION_ITEM('')
) ;
#29 = (
BOUNDED_CURVE()
B_SPLINE_CURVE(3,(#174703,#174704,#174705,#174706,#174707,#174708,#174709,
#174710,#174711,#174712,#174713,#174714,#174715,#174716,#174717,#174718,
#174719,#174720,#174721),.UNSPECIFIED.,.F.,.F.)
B_SPLINE_CURVE_WITH_KNOTS((4,1,1,1,1,1,1,1,1,1,1,1,1,1,1,1,4),(0.,0.226732296973331,
0.464902013928651,0.70307173088397,0.9298040278573,1.15653632483063,1.39470604178595,
1.63287575874127,1.8596080557146,2.08634035268793,2.32451006964325,2.56267978659857,
2.7894120835719,3.01614438054523,3.25431409750055,3.49248381445586,3.7192161114292),
 .UNSPECIFIED.)
CURVE()
GEOMETRIC_REPRESENTATION_ITEM()
RATIONAL_B_SPLINE_CURVE((1.,1.,1.,1.,1.,1.,1.,1.,1.,1.,1.,1.,1.,1.,1.,1.,
1.,1.,1.))
REPRESENTATION_ITEM('')
) ;
#30 = (
BOUNDED_CURVE()
B_SPLINE_CURVE(3,(#193341,#193342,#193343,#193344,#193345,#193346,#193347,
#193348,#193349,#193350,#193351,#193352,#193353,#193354,#193355,#193356,
#193357,#193358,#193359,#193360,#193361,#193362,#193363,#193364,#193365,
#193366,#193367,#193368,#193369,#193370,#193371,#193372,#193373,#193374,
#193375,#193376,#193377,#193378,#193379,#193380,#193381,#193382,#193383,
#193384,#193385,#193386,#193387,#193388,#193389,#193390,#193391,#193392,
#193393,#193394,#193395,#193396,#193397,#193398,#193399,#193400,#193401,
#193402,#193403,#193404,#193405,#193406,#193407,#193408,#193409,#193410,
#193411,#193412,#193413,#193414,#193415,#193416,#193417,#193418,#193419,
#193420,#193421,#193422,#193423,#193424,#193425,#193426,#193427,#193428,
#193429,#193430,#193431,#193432,#193433,#193434,#193435,#193436,#193437,
#193438,#193439,#193440,#193441,#193442,#193443,#193444,#193445,#193446,
#193447,#193448,#193449,#193450,#193451,#193452,#193453,#193454,#193455,
#193456,#193457,#193458,#193459,#193460,#193461,#193462,#193463,#193464,
#193465,#193466,#193467,#193468,#193469,#193470,#193471,#193472,#193473,
#193474,#193475,#193476,#193477,#193478,#193479,#193480,#193481,#193482,
#193483,#193484,#193485,#193486,#193487,#193488,#193489,#193490,#193491,
#193492,#193493,#193494,#193495,#193496,#193497,#193498,#193499,#193500,
#193501,#193502,#193503,#193504,#193505,#193506,#193507,#193508,#193509,
#193510,#193511,#193512,#193513,#193514,#193515,#193516,#193517,#193518,
#193519,#193520,#193521,#193522,#193523,#193524,#193525,#193526,#193527,
#193528,#193529,#193530,#193531,#193532,#193533,#193534,#193535,#193536,
#193537,#193538,#193539,#193540,#193541,#193542,#193543,#193544,#193545,
#193546,#193547,#193548,#193549,#193550,#193551,#193552,#193553,#193554,
#193555,#193556,#193557,#193558,#193559,#193560,#193561,#193562,#193563,
#193564,#193565,#193566,#193567,#193568,#193569,#193570,#193571,#193572,
#193573,#193574,#193575,#193576,#193577,#193578,#193579,#193580,#193581,
#193582,#193583,#193584,#193585,#193586,#193587,#193588,#193589,#193590,
#193591,#193592,#193593,#193594,#193595,#193596,#193597,#193598,#193599,
#193600,#193601,#193602,#193603,#193604,#193605,#193606,#193607,#193608,
#193609,#193610,#193611,#193612,#193613,#193614,#193615,#193616,#193617,
#193618,#193619,#193620,#193621,#193622,#193623,#193624,#193625,#193626,
#193627,#193628,#193629,#193630,#193631,#193632,#193633,#193634,#193635,
#193636,#193637,#193638,#193639,#193640,#193641,#193642,#193643,#193644,
#193645,#193646,#193647,#193648,#193649,#193650,#193651,#193652,#193653,
#193654,#193655,#193656,#193657,#193658,#193659,#193660,#193661,#193662,
#193663,#193664,#193665,#193666,#193667,#193668,#193669,#193670,#193671,
#193672,#193673,#193674,#193675,#193676,#193677,#193678,#193679,#193680,
#193681,#193682,#193683,#193684,#193685,#193686,#193687,#193688,#193689,
#193690,#193691,#193692,#193693,#193694,#193695,#193696,#193697,#193698,
#193699,#193700,#193701,#193702,#193703,#193704,#193705,#193706,#193707,
#193708,#193709,#193710,#193711,#193712,#193713,#193714,#193715,#193716,
#193717,#193718,#193719,#193720,#193721,#193722,#193723,#193724,#193725,
#193726,#193727,#193728,#193729,#193730,#193731,#193732,#193733,#193734,
#193735,#193736,#193737,#193738,#193739,#193740,#193741,#193742,#193743,
#193744,#193745,#193746,#193747,#193748,#193749,#193750,#193751,#193752,
#193753,#193754,#193755,#193756,#193757,#193758,#193759,#193760,#193761,
#193762,#193763,#193764,#193765,#193766,#193767,#193768,#193769,#193770,
#193771,#193772,#193773,#193774,#193775,#193776,#193777,#193778,#193779,
#193780,#193781,#193782,#193783,#193784,#193785,#193786,#193787,#193788,
#193789,#193790,#193791,#193792,#193793,#193794,#193795,#193796,#193797,
#193798,#193799,#193800,#193801,#193802,#193803,#193804,#193805,#193806,
#193807,#193808,#193809,#193810,#193811,#193812,#193813,#193814,#193815,
#193816,#193817,#193818,#193819,#193820,#193821,#193822,#193823,#193824,
#193825,#193826,#193827,#193828,#193829,#193830,#193831,#193832,#193833,
#193834,#193835,#193836,#193837,#193838,#193839,#193840,#193841,#193842,
#193843,#193844,#193845,#193846,#193847,#193848,#193849,#193850,#193851,
#193852,#193853,#193854,#193855,#193856,#193857,#193858,#193859,#193860,
#193861,#193862,#193863,#193864,#193865,#193866,#193867,#193868,#193869,
#193870,#193871,#193872,#193873,#193874,#193875,#193876,#193877,#193878,
#193879,#193880,#193881,#193882,#193883,#193884,#193885,#193886,#193887,
#193888,#193889,#193890,#193891,#193892,#193893,#193894,#193895,#193896,
#193897,#193898,#193899,#193900,#193901,#193902,#193903,#193904,#193905,
#193906,#193907,#193908,#193909,#193910,#193911,#193912,#193913,#193914,
#193915,#193916,#193917,#193918,#193919,#193920,#193921,#193922,#193923,
#193924,#193925,#193926,#193927,#193928,#193929,#193930,#193931,#193932,
#193933,#193934,#193935,#193936,#193937,#193938,#193939,#193940,#193941,
#193942,#193943,#193944,#193945,#193946,#193947,#193948,#193949,#193950,
#193951,#193952,#193953,#193954,#193955,#193956,#193957,#193958,#193959,
#193960,#193961,#193962,#193963,#193964,#193965,#193966,#193967,#193968,
#193969,#193970,#193971,#193972,#193973,#193974,#193975,#193976,#193977,
#193978,#193979,#193980,#193981,#193982,#193983,#193984,#193985,#193986,
#193987,#193988,#193989,#193990,#193991,#193992,#193993,#193994,#193995,
#193996,#193997,#193998,#193999,#194000,#194001,#194002,#194003,#194004,
#194005,#194006,#194007,#194008,#194009,#194010,#194011,#194012,#194013,
#194014,#194015,#194016,#194017,#194018,#194019,#194020,#194021,#194022,
#194023,#194024,#194025,#194026,#194027,#194028,#194029,#194030,#194031,
#194032,#194033,#194034,#194035,#194036,#194037,#194038,#194039,#194040,
#194041,#194042,#194043,#194044,#194045,#194046,#194047,#194048,#194049,
#194050,#194051,#194052,#194053,#194054,#194055,#194056,#194057,#194058,
#194059,#194060,#194061,#194062,#194063,#194064,#194065,#194066,#194067,
#194068,#194069,#194070,#194071,#194072,#194073,#194074,#194075,#194076,
#194077,#194078,#194079,#194080,#194081,#194082,#194083,#194084,#194085,
#194086,#194087,#194088,#194089,#194090,#194091,#194092,#194093,#194094,
#194095,#194096,#194097,#194098,#194099,#194100,#194101,#194102,#194103,
#194104,#194105,#194106,#194107,#194108,#194109,#194110,#194111,#194112,
#194113,#194114,#194115,#194116,#194117,#194118,#194119,#194120,#194121,
#194122,#194123,#194124,#194125,#194126,#194127,#194128,#194129,#194130,
#194131,#194132,#194133,#194134,#194135,#194136,#194137,#194138,#194139,
#194140,#194141,#194142,#194143,#194144,#194145,#194146,#194147,#194148,
#194149,#194150,#194151,#194152,#194153,#194154,#194155,#194156,#194157,
#194158,#194159,#194160,#194161,#194162,#194163,#194164,#194165,#194166,
#194167,#194168,#194169,#194170,#194171,#194172,#194173,#194174,#194175,
#194176,#194177,#194178,#194179,#194180,#194181,#194182,#194183,#194184,
#194185,#194186,#194187,#194188,#194189,#194190,#194191,#194192,#194193,
#194194,#194195,#194196,#194197,#194198,#194199,#194200,#194201,#194202,
#194203,#194204,#194205,#194206,#194207,#194208,#194209,#194210,#194211,
#194212,#194213,#194214,#194215,#194216,#194217,#194218,#194219,#194220,
#194221,#194222,#194223,#194224,#194225,#194226,#194227,#194228,#194229,
#194230,#194231,#194232,#194233,#194234,#194235,#194236,#194237,#194238,
#194239,#194240,#194241,#194242,#194243,#194244,#194245,#194246,#194247,
#194248,#194249,#194250,#194251,#194252,#194253,#194254,#194255,#194256,
#194257,#194258,#194259,#194260,#194261,#194262,#194263,#194264,#194265,
#194266,#194267,#194268,#194269,#194270,#194271,#194272,#194273,#194274,
#194275,#194276,#194277,#194278,#194279,#194280,#194281,#194282,#194283,
#194284,#194285,#194286,#194287,#194288,#194289,#194290,#194291,#194292,
#194293,#194294,#194295,#194296,#194297,#194298,#194299,#194300,#194301,
#194302,#194303,#194304,#194305,#194306,#194307,#194308,#194309,#194310,
#194311,#194312,#194313,#194314,#194315,#194316,#194317,#194318,#194319,
#194320,#194321,#194322,#194323,#194324,#194325,#194326,#194327,#194328,
#194329,#194330,#194331,#194332,#194333,#194334,#194335,#194336,#194337,
#194338,#194339,#194340,#194341,#194342,#194343,#194344,#194345,#194346,
#194347,#194348,#194349,#194350,#194351,#194352,#194353,#194354,#194355,
#194356,#194357,#194358,#194359,#194360,#194361,#194362,#194363,#194364,
#194365,#194366,#194367,#194368,#194369,#194370,#194371,#194372,#194373,
#194374,#194375,#194376,#194377,#194378,#194379,#194380,#194381,#194382,
#194383,#194384,#194385,#194386,#194387,#194388,#194389,#194390,#194391,
#194392,#194393,#194394,#194395,#194396,#194397,#194398),.UNSPECIFIED.,
 .F.,.F.)
B_SPLINE_CURVE_WITH_KNOTS((4,1,1,1,1,1,1,1,1,1,1,1,1,1,1,1,1,1,1,1,1,1,
1,1,1,1,1,1,1,1,1,1,1,1,1,1,1,1,1,1,1,1,1,1,1,1,1,1,1,1,1,1,1,1,1,1,1,1,
1,1,1,1,1,1,1,1,1,1,1,1,1,1,1,1,1,1,1,1,1,1,1,1,1,1,1,1,1,1,1,1,1,1,1,1,
1,1,1,1,1,1,1,1,1,1,1,1,1,1,1,1,1,1,1,1,1,1,1,1,1,1,1,1,1,1,1,1,1,1,1,1,
1,1,1,1,1,1,1,1,1,1,1,1,1,1,1,1,1,1,1,1,1,1,1,1,1,1,1,1,1,1,1,1,1,1,1,1,
1,1,1,1,1,1,1,1,1,1,1,1,1,1,1,1,1,1,1,1,1,1,1,1,1,1,1,1,1,1,1,1,1,1,1,1,
1,1,1,1,1,1,1,1,1,1,1,1,1,1,1,1,1,1,1,1,1,1,1,1,1,1,1,1,1,1,1,1,1,1,1,1,
1,1,1,1,1,1,1,1,1,1,1,1,1,1,1,1,1,1,1,1,1,1,1,1,1,1,1,1,1,1,1,1,1,1,1,1,
1,1,1,1,1,1,1,1,1,1,1,1,1,1,1,1,1,1,1,1,1,1,1,1,1,1,1,1,1,1,1,1,1,1,1,1,
1,1,1,1,1,1,1,1,1,1,1,1,1,1,1,1,1,1,1,1,1,1,1,1,1,1,1,1,1,1,1,1,1,1,1,1,
1,1,1,1,1,1,1,1,1,1,1,1,1,1,1,1,1,1,1,1,1,1,1,1,1,1,1,1,1,1,1,1,1,1,1,1,
1,1,1,1,1,1,1,1,1,1,1,1,1,1,1,1,1,1,1,1,1,1,1,1,1,1,1,1,1,1,1,1,1,1,1,1,
1,1,1,1,1,1,1,1,1,1,1,1,1,1,1,1,1,1,1,1,1,1,1,1,1,1,1,1,1,1,1,1,1,1,1,1,
1,1,1,1,1,1,1,1,1,1,1,1,1,1,1,1,1,1,1,1,1,1,1,1,1,1,1,1,1,1,1,1,1,1,1,1,
1,1,1,1,1,1,1,1,1,1,1,1,1,1,1,1,1,1,1,1,1,1,1,1,1,1,1,1,1,1,1,1,1,1,1,1,
1,1,1,1,1,1,1,1,1,1,1,1,1,1,1,1,1,1,1,1,1,1,1,1,1,1,1,1,1,1,1,1,1,1,1,1,
1,1,1,1,1,1,1,1,1,1,1,1,1,1,1,1,1,1,1,1,1,1,1,1,1,1,1,1,1,1,1,1,1,1,1,1,
1,1,1,1,1,1,1,1,1,1,1,1,1,1,1,1,1,1,1,1,1,1,1,1,1,1,1,1,1,1,1,1,1,1,1,1,
1,1,1,1,1,1,1,1,1,1,1,1,1,1,1,1,1,1,1,1,1,1,1,1,1,1,1,1,1,1,1,1,1,1,1,1,
1,1,1,1,1,1,1,1,1,1,1,1,1,1,1,1,1,1,1,1,1,1,1,1,1,1,1,1,1,1,1,1,1,1,1,1,
1,1,1,1,1,1,1,1,1,1,1,1,1,1,1,1,1,1,1,1,1,1,1,1,1,1,1,1,1,1,1,1,1,1,1,1,
1,1,1,1,1,1,1,1,1,1,1,1,1,1,1,1,1,1,1,1,1,1,1,1,1,1,1,1,1,1,1,1,1,1,1,1,
1,1,1,1,1,1,1,1,1,1,1,1,1,1,1,1,1,1,1,1,1,1,1,1,1,1,1,1,1,1,1,1,1,1,1,1,
1,1,1,1,1,1,1,1,1,1,1,1,1,1,1,1,1,1,1,1,1,1,1,1,1,1,1,1,1,1,1,1,1,1,1,1,
1,1,1,1,1,1,1,1,1,1,1,1,1,1,1,1,1,1,1,1,1,1,1,1,1,1,1,1,1,1,1,1,1,1,1,1,
1,1,1,1,1,1,1,1,1,1,1,1,1,1,1,1,1,1,1,1,1,1,1,1,1,1,1,1,1,1,1,1,1,1,1,1,
1,1,1,1,1,1,1,1,1,1,1,1,1,1,1,1,1,1,1,1,1,1,1,1,1,1,1,1,1,1,1,1,1,1,1,1,
1,1,1,1,1,1,1,1,1,1,1,1,1,1,1,1,1,1,1,1,1,1,1,1,1,1,1,1,1,1,1,1,1,1,1,1,
1,1,1,1,1,1,1,1,1,1,1,1,1,1,1,1,1,1,1,1,1,1,1,1,1,1,1,1,1,1,1,1,1,1,1,1,
1,1,1,1,1,1,1,1,1,1,1,1,1,1,1,1,1,1,1,1,1,1,1,1,1,4),(0.,0.01797683372391,
0.286633051710584,0.555289278308216,0.823945516665782,1.09260176953922,
1.36125803873948,1.62991432588463,1.89857063164012,2.16722695661301,2.43588330050525,
2.70453966304674,2.9731960431531,3.24185243981471,3.51050885133453,3.77916527610465,
4.04782171198515,4.31647815691489,4.58513460847725,4.85379106430677,5.12244752187208,
5.39110397865606,5.65976043217153,5.92841687990537,6.19707331956994,6.46572974881596,
6.73438616570634,7.00304256821933,7.2716989549161,7.5403553242696,7.809011675483,
8.07766800769526,8.34632432089157,8.61498061505147,8.8836368910788,9.15229314997201,
9.4209493936865,9.68960562442157,9.95826184531348,10.226918059948,10.4955742727586,
10.7642304884925,11.0328867113173,11.3015429448574,11.5701991918227,11.8388554546081,
12.1075117346518,12.3761680332469,12.6448243507434,12.9134806874637,13.1821370428496,
13.450793416388,13.7194498067883,13.9881062128412,14.2567626326955,14.5254190645885,
14.7940755062772,15.0627319555912,15.3313884100611,15.6000448672586,15.8687013246492,
16.1373577797,16.4060142299691,16.6746706729765,16.9433271065265,17.2119835283531,
17.4806399366567,17.7492963295502,18.0179527057767,18.286609063996,18.555265403637,
18.8239217240786,19.0925780255742,19.3612343083975,19.6298905737625,19.898546823017,
20.1672030584666,20.4358592827168,20.7045154992928,20.973171712245,21.2418279262962,
21.5104841459723,21.7791403749736,22.0477966165324,22.316452872948,22.585109146262,
22.8537654375589,23.1224217478187,23.3910780770929,23.6597344254327,23.9283907920352,
24.197047176159,24.4657035763222,24.7343599911301,25.0030164185931,25.2716728568073,
25.5403293034427,25.8089857562333,26.0776422126729,26.3462986702843,26.6149551265448,
26.8836115789212,27.1522680250308,27.4209244624423,27.6895808890659,27.9582373027346,
28.2268937018004,28.4955500845261,28.7642064498512,29.0328627966379,29.3015191245544,
29.5701754332357,29.838831723217,30.1074879950829,30.3761442503694,30.6448004907916,
30.9134567190168,31.1821129380756,31.450769151893,31.7194253649682,31.9880815819663,
32.2567378070174,32.5253940433706,32.7940502938785,33.0627065604467,33.3313628447765,
33.6000191476151,33.8686754696427,34.1373318106287,34.405988170366,34.6746445478242,
34.9433009420458,35.2119573513747,35.480613774244,35.7492702085419,36.0179266522368,
36.2865831029275,36.5552395582669,36.8238960157264,37.0925524727952,37.3612089269773,
37.6298653757534,37.8985218168153,38.1671782477952,38.4358346667239,38.7044910715485,
38.9731474607866,39.2418038328672,39.5104601869391,39.7791165220837,40.0477728382212,
40.3164291352602,40.5850854140292,40.8537416754418,41.1223979213679,41.3910541539077,
41.6597103761025,41.9283665914244,42.1970228042084,42.4656790192,42.7343352406829,
43.0029914723808,43.2716477171096,43.540303977354,43.8089602546436,44.0776165503516,
44.3462728649052,44.614929198697,44.883585551232,45.1522419220568,45.4208983099307,
45.6895547136931,45.9582111315299,46.2268675617156,46.4955240020317,46.7641804503338,
47.0328369041642,47.3014933611089,47.5701498186329,47.8388062742058,48.107462725373,
48.3761191696448,48.6447756048012,48.9134320285537,49.1820884390673,49.4507448344197,
49.7194012133072,49.9880575743413,50.2567139168934,50.5253702402807,50.7940265446884,
51.0626828303152,51.3313390982961,51.5999953498901,51.8686515873141,52.1373078130706,
52.4059640305862,52.6746202437936,52.9432764573682,53.211932675918,53.480588903259,
53.7492451427202,54.0179013967021,54.2865576673334,54.5552139557853,54.823870263115,
55.0925265894471,55.3611829348992,55.6298392987282,55.8984956802486,56.1671520780245,
56.4358084907065,56.7044649163381,56.9731213530494,57.2417777985307,57.5104342505384,
57.7790907065743,58.0477471641719,58.3164036208043,58.5850600739368,58.8537165211707,
59.1223729600609,59.39102938849,59.6596858042645,59.9283422056975,60.1969985910129,
60.4656549590995,60.7343113087676,61.0029676396243,61.2716239512389,61.540280244075,
61.808936518638,62.0775927763821,62.3462490189291,62.6149052488546,62.8835614690812,
63.1522176834332,63.4208738963055,63.6895301124163,63.9581863359981,64.2268425704115,
64.4954988186027,64.7641550825741,65.0328113641112,65.3014676640435,65.5701239831253,
65.8387803211949,66.1074366781083,66.3760930528907,66.6447494446373,66.9134058517341,
67.1820622726558,67.4507187053199,67.7193751477252,67.988031597487,68.256688052277,
68.5253445095709,68.7940009668648,69.0626574216546,69.3313138714164,69.5999703138218,
69.8686267464858,70.1372831674076,70.4059395745042,70.6745959662509,70.9432523410334,
71.2119086979469,71.4805650360164,71.7492213550982,72.0178776550306,72.2865339365675,
72.5551902005389,72.8238464487301,73.0925026831433,73.3611589067251,73.6298151228357,
73.8984713357081,74.1671275500599,74.4357837702864,74.7044400002118,74.9730962427587,
75.2417525005027,75.5104087750655,75.7790650679015,76.047721379516,76.3163777103726,
76.5850340600405,76.853690428127,77.1223468134422,77.391003214875,77.6596596306495,
77.9283160590784,78.1969724979684,78.4656289452021,78.7342853983344,79.0029418549666,
79.2715983125641,79.5402547685998,79.8089112206075,80.0775676660886,80.3462241027997,
80.6148805284312,80.8835369411131,81.1521933388889,81.4208497204091,81.689506084238,
81.9581624296899,82.2268187560219,82.4954750633515,82.7641313518033,83.0327876224345,
83.3014438764161,83.5701001158772,83.838756343218,84.1074125617677,84.3760687753422,
84.6447249885494,84.913381206065,85.1820374318212,85.4506936692451,85.719349920839,
85.9880061888197,86.2566624744465,86.5253187788541,86.7939751022413,87.0626314447932,
87.3312878058273,87.5999441847146,87.8686005800667,88.1372569905802,88.4059134143327,
88.6745698494889,88.9432262937606,89.2118827449277,89.4805392005005,89.7491956580243,
90.0178521149689,90.2865085687992,90.5551650171012,90.8238214574172,91.0924778876028,
91.3611343054394,91.6297907092016,91.8984470970753,92.1671034679,92.4357598204347,
92.7044161542264,92.9730724687798,93.2417287644878,93.5103850417773,93.7790413020216,
94.0476975467502,94.3163537784479,94.5850099999307,94.8536662149221,95.1223224277061,
95.390978643028,95.6596348652226,95.9282910977624,96.1969473436883,96.4656036051009,
96.7342598838697,97.0029161809086,97.2715724970461,97.5402288321905,97.8088851862623,
98.0775415583427,98.3461979475807,98.6148543524051,98.8835107713336,99.1521672023136,
99.4208236433754,99.6894800921513,99.9581365463333,100.226793003402,100.495449460861,
100.7641059162,101.032762366891,101.301418810586,101.570075244884,101.838731667753,
102.107388077082,102.376044471303,102.644700848761,102.913357208498,103.182013549484,
103.450669871511,103.71932617435,103.98798245868,104.256638725248,104.525294975755,
104.793951212108,105.062607437159,105.331263654157,105.599919867233,105.86857608105,
106.137232300108,106.405888528334,106.674544768756,106.943201024042,107.211857295908,
107.480513585889,107.74916989457,108.017826222487,108.286482569273,108.555138934598,
108.823795317324,109.09245171639,109.361108130058,109.629764556682,109.898420994093,
110.167077440202,110.435733892579,110.704390348839,110.97304680645,111.24170326289,
111.51035971568,111.779016162316,112.04767260053,112.316329027993,112.5849854428,
112.853641842963,113.122298227087,113.39095459369,113.659610942029,113.928267271303,
114.196923581563,114.46557987286,114.734236146174,115.002892402589,115.271548644148,
115.540204873149,115.808861092825,116.077517306876,116.346173519828,116.614829736404,
116.883485960654,117.152142196103,117.420798445358,117.689454710722,117.958110993546,
118.226767295041,118.495423615483,118.764079955123,119.032736313343,119.301392689569,
119.570049082462,119.838705490766,120.107361912592,120.376018346142,120.644674789149,
120.913331239418,121.181987694469,121.45064415186,121.719300609057,121.987957063527,
122.256613512841,122.525269954529,122.793926386422,123.062582806276,123.331239212329,
123.599895602729,123.868551976268,124.137208331653,124.405864668374,124.67452098587,
124.943177284465,125.211833564508,125.480489827294,125.749146074259,126.017802307799,
126.286458530624,126.555114746357,126.823770959168,127.092427173802,127.361083394694,
127.629739625429,127.898395869143,128.167052128037,128.435708404064,128.704364698224,
128.97302101142,129.241677343633,129.510333694846,129.7789900642,130.047646450897,
130.31630285341,130.5849592703,130.853615699547,131.122272139211,131.390928586945,
131.659585040461,131.928241497245,132.19689795481,132.46555441064,132.734210862202,
133.002867307132,133.271523743013,133.540180167783,133.808836579303,134.077492975965,
134.346149356071,134.614805718613,134.883462062505,135.152118387478,135.420774693234,
135.689430980379,135.958087249579,136.226743502453,136.49539974081,136.76405596741,
137.032712185392,137.301368398783,137.570024612174,137.838680830155,138.107337056755,
138.375993295112,138.644649547986,138.913305817186,139.181962104332,139.450618410087,
139.71927473506,139.987931078952,140.256587441494,140.525243821601,140.793900218262,
141.062556629782,141.331213054552,141.599869490433,141.868525935363,142.137182386925,
142.405838842755,142.67449530032,142.943151757104,143.21180821062,143.480464658354,
143.749121098019,144.017777527265,144.286433944155,144.555090346668,144.823746733365,
145.092403102719,145.361059453932,145.629715786145,145.898372099341,146.167028393501,
146.435684669529,146.704340928422,146.972997172137,147.241653402872,147.510309623764,
147.778965838398,148.047622051209,148.316278266943,148.584934489768,148.853590723308,
149.122246970274,149.390903233059,149.659559513103,149.928215811698,150.196872129195,
150.465528465915,150.734184821301,151.00284119484,151.27149758524,151.540153991293,
151.808810411148,152.077466843041,152.34612328473,152.614779734044,152.883436188514,
153.152092645711,153.420749103102,153.689405558153,153.958062008422,154.22671845143,
154.49537488498,154.764031306806,155.03268771511,155.301344108004,155.57000048423,
155.838656842449,156.107313182091,156.375969502532,156.644625804028,156.913282086851,
157.181938352216,157.450594601471,157.719250836921,157.987907061171,158.256563277747,
158.525219490699,158.793875704751,159.062531924427,159.331188153428,159.599844394987,
159.868500651403,160.137156924717,160.405813216014,160.674469526274,160.943125855548,
161.211782203888,161.480438570491,161.749094954615,162.017751354778,162.286407769586,
162.555064197049,162.823720635263,163.092377081899,163.361033534689,163.629689991129,
163.898346448741,164.167002905001,164.435659357378,164.704315803488,164.972972240899,
165.241628667523,165.510285081192,165.778941480257,166.047597862983,166.316254228308,
166.584910575095,166.853566903012,167.122223211693,167.390879501675,167.659535773541,
167.928192028827,168.19684826925,168.465504497475,168.734160716534,169.002816930351,
169.271473143427,169.540129360425,169.808785585476,170.077441821829,170.346098072337,
170.614754338905,170.883410623235,171.152066926074,171.420723248102,171.689379589088,
171.958035948825,172.226692326284,172.495348720505,172.764005129834,173.032661552704,
173.301317987002,173.569974430697,173.838630881388,174.107287336727,174.375943794187,
174.644600251255,174.913256705437,175.181913154214,175.450569595276,175.719226026256,
175.987882445184,176.256538850009,176.525195239247,176.793851611328,177.0625079654,
177.331164300545,177.599820616682,177.868476913721,178.137133192491,178.405789453903,
178.674445699829,178.943101932369,179.211758154564,179.480414369886,179.74907058267,
180.017726797662,180.286383019145,180.555039250843,180.823695495572,181.092351755816,
181.361008033106,181.629664328814,181.898320643368,182.16697697716,182.435633329695,
182.70428970052,182.972946088394,183.241602492156,183.510258909993,183.778915340179,
184.047571780495,184.316228228797,184.584884682628,184.853541139572,185.122197597096,
185.39085405267,185.659510503837,185.928166948109,186.196823383265,186.465479807018,
186.734136217531,187.002792612884,187.271448991771,187.540105352806,187.808761695358,
188.077418018745,188.346074323153,188.61473060878,188.883386876761,189.152043128355,
189.420699365779,189.689355591536,189.958011809051,190.226668022259,190.495324235834,
190.763980454383,191.032636681725,191.301292921186,191.569949175168,191.838605445799,
192.107261734251,192.375918041581,192.644574367913,192.913230713365,193.181887077194,
193.450543458715,193.719199856491,193.987856269173,194.256512694805,194.525169131516,
194.793825576997,195.062482029005,195.331138485041,195.599794942639,195.868451399271,
196.137107852404,196.405764299638,196.674420738528,196.943077166957,197.211733582732,
197.480389984165,197.749046369481,198.017702737567,198.286359087236,198.555015418092,
198.823671729707,199.092328022543,199.360984297106,199.62964055485,199.898296797397,
200.166953027323,200.43560924755,200.704265461902,200.972921674774,201.241577890885,
201.510234114467,201.77889034888,202.047546597072,202.316202861043,202.584859142581,
202.853515442513,203.122171761595,203.390828099665,203.659484456579,203.928140831361,
204.196797223108,204.465453630205,204.734110051127,205.002766483791,205.271422926197,
205.540079375959,205.808735830749,206.077392288043,206.346048745337,206.614705200127,
206.883361649889,207.152018092295,207.420674524959,207.689330945881,207.957987352978,
208.226643744725,208.495300119508,208.763956476421,209.032612814491,209.301269133573,
209.569925433505,209.838581715043,210.107237979014,210.375894227206,210.644550461619,
210.913206685201,211.181862901312,211.450519114184,211.719175328536,211.987831548763,
212.256487778689,212.525144021236,212.79380027898,213.062456553543,213.331112846379,
213.599769157994,213.868425488851,214.137081838519,214.405738206606,214.674394591921,
214.943050993354,215.211707409129,215.480363837558,215.749020276448,216.017676723682,
216.286333176815,216.554989633447,216.823646091045,217.092302547081,217.360958999089,
217.62961544457,217.898271881281,218.166928306913,218.435584719595,218.704241117371,
218.972897498892,219.241553862721,219.510210208173,219.778866534505,220.047522841835,
220.316179130287,220.584835400918,220.8534916549,221.122147894361,221.390804121702,
221.659460340252,221.928116553827,222.196772767034,222.46542898455,222.734085210306,
223.00274144773,223.271397699324,223.540053967305,223.808710252932,224.07736655734,
224.346022880728,224.61467922328,224.883335584314,225.151991963201,225.420648358554,
225.689304769068,225.95796119282,226.226617627977,226.495274072249,226.763930523416,
227.032586978989,227.301243436513,227.569899893458,227.838556347288,228.10721279559,
228.375869235907,228.644525666093,228.913182083929,229.181838487692,229.450494875566,
229.719151246391,229.987807598926,230.256463932718,230.525120247271,230.79377654298,
231.062432820269,231.331089080514,231.599745325243,231.868401556941,232.137057778424,
232.405713993415,232.674370206199,232.943026421521,233.211682643716,233.480338876256,
233.748995122182,234.017651383595,234.286307662364,234.554963959403,234.823620275541,
235.092276610685,235.360932964757,235.629589336838,235.898245726076,236.166902130901,
236.43555854983,236.70421498081,236.972871421872,237.241527870648,237.51018432483,
237.778840781899,238.047497239359,238.316153694698,238.584810145389,238.853466589084,
239.122123023382,239.390779446251,239.65943585558,239.928092249802,240.19674862726,
240.465404986998,240.734061327984,241.002717650011,241.27137395285,241.54003023718,
241.808686503748,242.077342754256,242.345998990609,242.614655215661,242.883311432659,
243.151967645734,243.420623859552,243.68928007861,243.957936306836,244.226592547258,
244.495248802545,244.763905074411,245.032561364392,245.301217673074,245.56987400099,
245.838530347777,246.107186713102,246.375843095828,246.644499494894,246.913155908563,
247.181812335186,247.450468772598,247.719125218708,247.987781671084,248.256438127345,
248.525094584956,248.793751041396,249.062407494187,249.331063940822,249.599720379036,
249.8683768065,250.137033221308,250.405689621471,250.674346005595,250.943002372197,
251.211658720537,251.480315049812,251.748971360071,252.017627651368,252.286283924683,
252.554940181098,252.823596422657,253.092252651658,253.360908871335,253.629565085386,
253.898221298338,254.166877514914,254.435533739165,254.704189974614,254.972846223869,
255.241502489234,255.510158772057,255.778815073553,256.047471393995,256.316127733635,
256.584784091854,256.85344046808,257.122096860973,257.390753269276,257.659409691102,
257.928066124652,258.196722567659,258.465379017928,258.734035472978,259.002691930368,
259.271348387566,259.540004842035,259.808661291349,260.077317733037,260.345974164929,
260.614630584783,260.883286990836,261.151943381235,261.420599754774,261.689256110159,
261.957912446879,262.226568764375,262.49522506297,262.763881343014,263.032537605798,
263.301193852763,263.569850086303,263.838506309127,264.107162524861,264.375818737671,
264.644474952305,264.913131173196,265.181787403931,265.450443647645,265.719099906538,
265.987756182565,266.256412476724,266.52506878992,266.793725122132,267.062381473345,
267.331037842698,267.599694229394,267.868350631907,268.137007048797,268.405663478042,
268.674319917706,268.94297636544,269.211632818955,269.480289275739,269.748945733304,
270.017602189133,270.286258640695,270.554915085624,270.823571521504,271.092227946274,
271.360884357793,271.629540754454,271.89819713456,272.166853497101,272.435509840993,
272.704166165965,272.97282247172,273.241478758865,273.510135028065,273.778791280938,
274.047447519295,274.316103745894,274.584759963875,274.853416177266,275.122072390656,
275.390728608637,275.659384835237,275.928041073593,276.196697326466,276.465353595666,
276.734009882811,277.002666188566,277.271322513539,277.53997885743,277.808635219972,
278.077291600077,278.345947996739,278.614604408258,278.883260833028,279.151917268908,
279.420573713837,279.689230165399,279.957886621228,280.226543078793,280.495199535576,
280.763855989092,281.032512436825,281.301168876489,281.569825305735,281.838481722625,
282.107138125138,282.375794511834,282.644450881187,282.9131072324,283.140531716307),
 .UNSPECIFIED.)
CURVE()
GEOMETRIC_REPRESENTATION_ITEM()
RATIONAL_B_SPLINE_CURVE((1.,1.,1.,1.,1.,1.,1.,1.,1.,1.,1.,1.,1.,1.,1.,1.,
1.,1.,1.,1.,1.,1.,1.,1.,1.,1.,1.,1.,1.,1.,1.,1.,1.,1.,1.,1.,1.,1.,1.,1.,
1.,1.,1.,1.,1.,1.,1.,1.,1.,1.,1.,1.,1.,1.,1.,1.,1.,1.,1.,1.,1.,1.,1.,1.,
1.,1.,1.,1.,1.,1.,1.,1.,1.,1.,1.,1.,1.,1.,1.,1.,1.,1.,1.,1.,1.,1.,1.,1.,
1.,1.,1.,1.,1.,1.,1.,1.,1.,1.,1.,1.,1.,1.,1.,1.,1.,1.,1.,1.,1.,1.,1.,1.,
1.,1.,1.,1.,1.,1.,1.,1.,1.,1.,1.,1.,1.,1.,1.,1.,1.,1.,1.,1.,1.,1.,1.,1.,
1.,1.,1.,1.,1.,1.,1.,1.,1.,1.,1.,1.,1.,1.,1.,1.,1.,1.,1.,1.,1.,1.,1.,1.,
1.,1.,1.,1.,1.,1.,1.,1.,1.,1.,1.,1.,1.,1.,1.,1.,1.,1.,1.,1.,1.,1.,1.,1.,
1.,1.,1.,1.,1.,1.,1.,1.,1.,1.,1.,1.,1.,1.,1.,1.,1.,1.,1.,1.,1.,1.,1.,1.,
1.,1.,1.,1.,1.,1.,1.,1.,1.,1.,1.,1.,1.,1.,1.,1.,1.,1.,1.,1.,1.,1.,1.,1.,
1.,1.,1.,1.,1.,1.,1.,1.,1.,1.,1.,1.,1.,1.,1.,1.,1.,1.,1.,1.,1.,1.,1.,1.,
1.,1.,1.,1.,1.,1.,1.,1.,1.,1.,1.,1.,1.,1.,1.,1.,1.,1.,1.,1.,1.,1.,1.,1.,
1.,1.,1.,1.,1.,1.,1.,1.,1.,1.,1.,1.,1.,1.,1.,1.,1.,1.,1.,1.,1.,1.,1.,1.,
1.,1.,1.,1.,1.,1.,1.,1.,1.,1.,1.,1.,1.,1.,1.,1.,1.,1.,1.,1.,1.,1.,1.,1.,
1.,1.,1.,1.,1.,1.,1.,1.,1.,1.,1.,1.,1.,1.,1.,1.,1.,1.,1.,1.,1.,1.,1.,1.,
1.,1.,1.,1.,1.,1.,1.,1.,1.,1.,1.,1.,1.,1.,1.,1.,1.,1.,1.,1.,1.,1.,1.,1.,
1.,1.,1.,1.,1.,1.,1.,1.,1.,1.,1.,1.,1.,1.,1.,1.,1.,1.,1.,1.,1.,1.,1.,1.,
1.,1.,1.,1.,1.,1.,1.,1.,1.,1.,1.,1.,1.,1.,1.,1.,1.,1.,1.,1.,1.,1.,1.,1.,
1.,1.,1.,1.,1.,1.,1.,1.,1.,1.,1.,1.,1.,1.,1.,1.,1.,1.,1.,1.,1.,1.,1.,1.,
1.,1.,1.,1.,1.,1.,1.,1.,1.,1.,1.,1.,1.,1.,1.,1.,1.,1.,1.,1.,1.,1.,1.,1.,
1.,1.,1.,1.,1.,1.,1.,1.,1.,1.,1.,1.,1.,1.,1.,1.,1.,1.,1.,1.,1.,1.,1.,1.,
1.,1.,1.,1.,1.,1.,1.,1.,1.,1.,1.,1.,1.,1.,1.,1.,1.,1.,1.,1.,1.,1.,1.,1.,
1.,1.,1.,1.,1.,1.,1.,1.,1.,1.,1.,1.,1.,1.,1.,1.,1.,1.,1.,1.,1.,1.,1.,1.,
1.,1.,1.,1.,1.,1.,1.,1.,1.,1.,1.,1.,1.,1.,1.,1.,1.,1.,1.,1.,1.,1.,1.,1.,
1.,1.,1.,1.,1.,1.,1.,1.,1.,1.,1.,1.,1.,1.,1.,1.,1.,1.,1.,1.,1.,1.,1.,1.,
1.,1.,1.,1.,1.,1.,1.,1.,1.,1.,1.,1.,1.,1.,1.,1.,1.,1.,1.,1.,1.,1.,1.,1.,
1.,1.,1.,1.,1.,1.,1.,1.,1.,1.,1.,1.,1.,1.,1.,1.,1.,1.,1.,1.,1.,1.,1.,1.,
1.,1.,1.,1.,1.,1.,1.,1.,1.,1.,1.,1.,1.,1.,1.,1.,1.,1.,1.,1.,1.,1.,1.,1.,
1.,1.,1.,1.,1.,1.,1.,1.,1.,1.,1.,1.,1.,1.,1.,1.,1.,1.,1.,1.,1.,1.,1.,1.,
1.,1.,1.,1.,1.,1.,1.,1.,1.,1.,1.,1.,1.,1.,1.,1.,1.,1.,1.,1.,1.,1.,1.,1.,
1.,1.,1.,1.,1.,1.,1.,1.,1.,1.,1.,1.,1.,1.,1.,1.,1.,1.,1.,1.,1.,1.,1.,1.,
1.,1.,1.,1.,1.,1.,1.,1.,1.,1.,1.,1.,1.,1.,1.,1.,1.,1.,1.,1.,1.,1.,1.,1.,
1.,1.,1.,1.,1.,1.,1.,1.,1.,1.,1.,1.,1.,1.,1.,1.,1.,1.,1.,1.,1.,1.,1.,1.,
1.,1.,1.,1.,1.,1.,1.,1.,1.,1.,1.,1.,1.,1.,1.,1.,1.,1.,1.,1.,1.,1.,1.,1.,
1.,1.,1.,1.,1.,1.,1.,1.,1.,1.,1.,1.,1.,1.,1.,1.,1.,1.,1.,1.,1.,1.,1.,1.,
1.,1.,1.,1.,1.,1.,1.,1.,1.,1.,1.,1.,1.,1.,1.,1.,1.,1.,1.,1.,1.,1.,1.,1.,
1.,1.,1.,1.,1.,1.,1.,1.,1.,1.,1.,1.,1.,1.,1.,1.,1.,1.,1.,1.,1.,1.,1.,1.,
1.,1.,1.,1.,1.,1.,1.,1.,1.,1.,1.,1.,1.,1.,1.,1.,1.,1.,1.,1.,1.,1.,1.,1.,
1.,1.,1.,1.,1.,1.,1.,1.,1.,1.,1.,1.,1.,1.,1.,1.,1.,1.,1.,1.,1.,1.,1.,1.,
1.,1.,1.,1.,1.,1.,1.,1.,1.,1.,1.,1.,1.,1.,1.,1.,1.,1.,1.,1.,1.,1.,1.,1.,
1.,1.,1.,1.,1.,1.,1.,1.,1.,1.,1.,1.,1.,1.,1.,1.,1.,1.,1.,1.,1.,1.,1.,1.,
1.,1.,1.,1.,1.,1.,1.,1.,1.,1.,1.,1.,1.,1.,1.,1.,1.,1.,1.,1.,1.,1.,1.,1.,
1.,1.,1.,1.,1.,1.,1.,1.,1.,1.,1.,1.,1.,1.,1.,1.,1.,1.,1.,1.,1.,1.,1.,1.,
1.,1.,1.,1.,1.,1.,1.,1.,1.,1.,1.,1.,1.,1.,1.,1.,1.,1.,1.,1.,1.,1.,1.,1.,
1.,1.,1.,1.,1.,1.,1.,1.,1.,1.))
REPRESENTATION_ITEM('')
) ;
#31 = (
BOUNDED_CURVE()
B_SPLINE_CURVE(3,(#194468,#194469,#194470,#194471,#194472,#194473,#194474),
 .UNSPECIFIED.,.F.,.F.)
B_SPLINE_CURVE_WITH_KNOTS((4,1,1,1,4),(0.,0.0911446219616379,0.182289243923276,
0.273433865884915,0.364578487846551),.UNSPECIFIED.)
CURVE()
GEOMETRIC_REPRESENTATION_ITEM()
RATIONAL_B_SPLINE_CURVE((1.,1.,1.,1.,1.,1.,1.))
REPRESENTATION_ITEM('')
) ;
#32 = (
BOUNDED_CURVE()
B_SPLINE_CURVE(3,(#194690,#194691,#194692,#194693,#194694,#194695,#194696,
#194697,#194698,#194699,#194700,#194701,#194702,#194703,#194704,#194705,
#194706,#194707,#194708),.UNSPECIFIED.,.F.,.F.)
B_SPLINE_CURVE_WITH_KNOTS((4,1,1,1,1,1,1,1,1,1,1,1,1,1,1,1,4),(0.,0.226732296973331,
0.464902013928651,0.70307173088397,0.9298040278573,1.15653632483063,1.39470604178595,
1.63287575874127,1.8596080557146,2.08634035268793,2.32451006964325,2.56267978659857,
2.7894120835719,3.01614438054523,3.25431409750055,3.49248381445586,3.7192161114292),
 .UNSPECIFIED.)
CURVE()
GEOMETRIC_REPRESENTATION_ITEM()
RATIONAL_B_SPLINE_CURVE((1.,1.,1.,1.,1.,1.,1.,1.,1.,1.,1.,1.,1.,1.,1.,1.,
1.,1.,1.))
REPRESENTATION_ITEM('')
) ;
#33 = (
BOUNDED_SURFACE()
B_SPLINE_SURFACE(2,2,((#114004,#114005,#114006,#114007,#114008,#114009,
#114010,#114011,#114012),(#114013,#114014,#114015,#114016,#114017,#114018,
#114019,#114020,#114021),(#114022,#114023,#114024,#114025,#114026,#114027,
#114028,#114029,#114030)),.UNSPECIFIED.,.F.,.T.,.F.)
B_SPLINE_SURFACE_WITH_KNOTS((3,3),(3,2,2,2,3),(0.,1.05013832301181),(0.,
1.5707963267949,3.1415926535898,4.71238898038469,6.28318530717959),
 .UNSPECIFIED.)
GEOMETRIC_REPRESENTATION_ITEM()
RATIONAL_B_SPLINE_SURFACE(((1.,0.707106781186548,1.,0.707106781186548,1.,
0.707106781186548,1.,0.707106781186548,1.),(0.963886720506905,0.681570836366095,
0.963886720506905,0.681570836366095,0.963886720506905,0.681570836366095,
0.963886720506905,0.681570836366095,0.963886720506905),(1.,0.707106781186548,
1.,0.707106781186548,1.,0.707106781186548,1.,0.707106781186548,1.)))
REPRESENTATION_ITEM('')
SURFACE()
) ;
#34 = (
BOUNDED_SURFACE()
B_SPLINE_SURFACE(2,1,((#114035,#114036),(#114037,#114038),(#114039,#114040),
(#114041,#114042),(#114043,#114044),(#114045,#114046),(#114047,#114048),
(#114049,#114050),(#114051,#114052)),.UNSPECIFIED.,.T.,.F.,.F.)
B_SPLINE_SURFACE_WITH_KNOTS((3,2,2,2,3),(2,2),(0.,1.5707963267949,3.1415926535898,
4.71238898038469,6.28318530717959),(0.,0.0454859585810009),
 .UNSPECIFIED.)
GEOMETRIC_REPRESENTATION_ITEM()
RATIONAL_B_SPLINE_SURFACE(((1.,1.),(0.707106781186548,0.707106781186548),
(1.,1.),(0.707106781186548,0.707106781186548),(1.,1.),(0.707106781186548,
0.707106781186548),(1.,1.),(0.707106781186548,0.707106781186548),(1.,1.)))
REPRESENTATION_ITEM('')
SURFACE()
) ;
#35 = (
BOUNDED_SURFACE()
B_SPLINE_SURFACE(2,2,((#114056,#114057,#114058,#114059,#114060,#114061,
#114062,#114063,#114064),(#114065,#114066,#114067,#114068,#114069,#114070,
#114071,#114072,#114073),(#114074,#114075,#114076,#114077,#114078,#114079,
#114080,#114081,#114082),(#114083,#114084,#114085,#114086,#114087,#114088,
#114089,#114090,#114091),(#114092,#114093,#114094,#114095,#114096,#114097,
#114098,#114099,#114100),(#114101,#114102,#114103,#114104,#114105,#114106,
#114107,#114108,#114109),(#114110,#114111,#114112,#114113,#114114,#114115,
#114116,#114117,#114118),(#114119,#114120,#114121,#114122,#114123,#114124,
#114125,#114126,#114127),(#114128,#114129,#114130,#114131,#114132,#114133,
#114134,#114135,#114136)),.UNSPECIFIED.,.F.,.T.,.F.)
B_SPLINE_SURFACE_WITH_KNOTS((3,2,2,2,3),(3,2,2,2,3),(1.42918797785348,1.62618617063892,
1.86180561965816,2.09742506867739,2.29442326146283),(0.,1.5707963267949,
3.1415926535898,4.71238898038469,6.28318530717959),.UNSPECIFIED.)
GEOMETRIC_REPRESENTATION_ITEM()
RATIONAL_B_SPLINE_SURFACE(((1.,0.707106781186548,1.,0.707106781186548,1.,
0.707106781186548,1.,0.707106781186548,1.),(1.,0.707106781186548,1.,0.707106781186548,
1.,0.707106781186548,1.,0.707106781186548,1.),(1.,0.707106781186548,1.,
0.707106781186548,1.,0.707106781186548,1.,0.707106781186548,1.),(0.707106781186548,
0.5,0.707106781186548,0.5,0.707106781186548,0.5,0.707106781186548,0.5,0.707106781186548),
(1.,0.707106781186548,1.,0.707106781186548,1.,0.707106781186548,1.,0.707106781186548,
1.),(0.707106781186548,0.5,0.707106781186548,0.5,0.707106781186548,0.5,
0.707106781186548,0.5,0.707106781186548),(1.,0.707106781186548,1.,0.707106781186548,
1.,0.707106781186548,1.,0.707106781186548,1.),(1.,0.707106781186548,1.,
0.707106781186548,1.,0.707106781186548,1.,0.707106781186548,1.),(1.,0.707106781186548,
1.,0.707106781186548,1.,0.707106781186548,1.,0.707106781186548,1.)))
REPRESENTATION_ITEM('')
SURFACE()
) ;
#36 = (
BOUNDED_SURFACE()
B_SPLINE_SURFACE(2,1,((#114148,#114149),(#114150,#114151),(#114152,#114153),
(#114154,#114155),(#114156,#114157),(#114158,#114159),(#114160,#114161),
(#114162,#114163),(#114164,#114165)),.UNSPECIFIED.,.T.,.F.,.F.)
B_SPLINE_SURFACE_WITH_KNOTS((3,2,2,2,3),(2,2),(0.,1.5707963267949,3.1415926535898,
4.71238898038469,6.28318530717959),(0.,1.586514041419),.UNSPECIFIED.)
GEOMETRIC_REPRESENTATION_ITEM()
RATIONAL_B_SPLINE_SURFACE(((1.,1.),(0.707106781186548,0.707106781186548),
(1.,1.),(0.707106781186548,0.707106781186548),(1.,1.),(0.707106781186548,
0.707106781186548),(1.,1.),(0.707106781186548,0.707106781186548),(1.,1.)))
REPRESENTATION_ITEM('')
SURFACE()
) ;
#37 = (
BOUNDED_SURFACE()
B_SPLINE_SURFACE(1,2,((#114169,#114170,#114171,#114172,#114173,#114174,
#114175,#114176,#114177),(#114178,#114179,#114180,#114181,#114182,#114183,
#114184,#114185,#114186)),.UNSPECIFIED.,.F.,.T.,.F.)
B_SPLINE_SURFACE_WITH_KNOTS((2,2),(3,2,2,2,3),(15.5153736066212,15.6567949628585),
(0.,1.5707963267949,3.1415926535898,4.71238898038469,6.28318530717959),
 .UNSPECIFIED.)
GEOMETRIC_REPRESENTATION_ITEM()
RATIONAL_B_SPLINE_SURFACE(((1.,0.707106781186548,1.,0.707106781186548,1.,
0.707106781186548,1.,0.707106781186548,1.),(1.,0.707106781186548,1.,0.707106781186548,
1.,0.707106781186548,1.,0.707106781186548,1.)))
REPRESENTATION_ITEM('')
SURFACE()
) ;
#38 = (
BOUNDED_SURFACE()
B_SPLINE_SURFACE(2,2,((#114193,#114194,#114195),(#114196,#114197,#114198),
(#114199,#114200,#114201),(#114202,#114203,#114204),(#114205,#114206,#114207),
(#114208,#114209,#114210),(#114211,#114212,#114213),(#114214,#114215,#114216),
(#114217,#114218,#114219)),.UNSPECIFIED.,.T.,.F.,.F.)
B_SPLINE_SURFACE_WITH_KNOTS((3,2,2,2,3),(3,3),(0.,1.5707963267949,3.1415926535898,
4.71238898038469,6.28318530717959),(0.,1.05013832301181),.UNSPECIFIED.)
GEOMETRIC_REPRESENTATION_ITEM()
RATIONAL_B_SPLINE_SURFACE(((1.,0.963886720506905,1.),(0.707106781186548,
0.681570836366095,0.707106781186548),(1.,0.963886720506905,1.),(0.707106781186548,
0.681570836366095,0.707106781186548),(1.,0.963886720506905,1.),(0.707106781186548,
0.681570836366095,0.707106781186548),(1.,0.963886720506905,1.),(0.707106781186548,
0.681570836366095,0.707106781186548),(1.,0.963886720506905,1.)))
REPRESENTATION_ITEM('')
SURFACE()
) ;
#39 = (
BOUNDED_SURFACE()
B_SPLINE_SURFACE(2,1,((#114224,#114225),(#114226,#114227),(#114228,#114229),
(#114230,#114231),(#114232,#114233),(#114234,#114235),(#114236,#114237),
(#114238,#114239),(#114240,#114241)),.UNSPECIFIED.,.T.,.F.,.F.)
B_SPLINE_SURFACE_WITH_KNOTS((3,2,2,2,3),(2,2),(0.,1.5707963267949,3.1415926535898,
4.71238898038469,6.28318530717959),(0.,0.0454859585810009),
 .UNSPECIFIED.)
GEOMETRIC_REPRESENTATION_ITEM()
RATIONAL_B_SPLINE_SURFACE(((1.,1.),(0.707106781186548,0.707106781186548),
(1.,1.),(0.707106781186548,0.707106781186548),(1.,1.),(0.707106781186548,
0.707106781186548),(1.,1.),(0.707106781186548,0.707106781186548),(1.,1.)))
REPRESENTATION_ITEM('')
SURFACE()
) ;
#40 = (
BOUNDED_SURFACE()
B_SPLINE_SURFACE(2,2,((#114245,#114246,#114247,#114248,#114249,#114250,
#114251,#114252,#114253),(#114254,#114255,#114256,#114257,#114258,#114259,
#114260,#114261,#114262),(#114263,#114264,#114265,#114266,#114267,#114268,
#114269,#114270,#114271),(#114272,#114273,#114274,#114275,#114276,#114277,
#114278,#114279,#114280),(#114281,#114282,#114283,#114284,#114285,#114286,
#114287,#114288,#114289),(#114290,#114291,#114292,#114293,#114294,#114295,
#114296,#114297,#114298),(#114299,#114300,#114301,#114302,#114303,#114304,
#114305,#114306,#114307),(#114308,#114309,#114310,#114311,#114312,#114313,
#114314,#114315,#114316),(#114317,#114318,#114319,#114320,#114321,#114322,
#114323,#114324,#114325)),.UNSPECIFIED.,.T.,.F.,.F.)
B_SPLINE_SURFACE_WITH_KNOTS((3,2,2,2,3),(3,2,2,2,3),(0.,1.5707963267949,
3.1415926535898,4.71238898038469,6.28318530717959),(1.42918797785348,1.62618617063892,
1.86180561965816,2.09742506867739,2.29442326146283),.UNSPECIFIED.)
GEOMETRIC_REPRESENTATION_ITEM()
RATIONAL_B_SPLINE_SURFACE(((1.,1.,1.,0.707106781186548,1.,0.707106781186548,
1.,1.,1.),(0.707106781186548,0.707106781186548,0.707106781186548,0.5,0.707106781186548,
0.5,0.707106781186548,0.707106781186548,0.707106781186548),(1.,1.,1.,0.707106781186548,
1.,0.707106781186548,1.,1.,1.),(0.707106781186548,0.707106781186548,0.707106781186548,
0.5,0.707106781186548,0.5,0.707106781186548,0.707106781186548,0.707106781186548),
(1.,1.,1.,0.707106781186548,1.,0.707106781186548,1.,1.,1.),(0.707106781186548,
0.707106781186548,0.707106781186548,0.5,0.707106781186548,0.5,0.707106781186548,
0.707106781186548,0.707106781186548),(1.,1.,1.,0.707106781186548,1.,0.707106781186548,
1.,1.,1.),(0.707106781186548,0.707106781186548,0.707106781186548,0.5,0.707106781186548,
0.5,0.707106781186548,0.707106781186548,0.707106781186548),(1.,1.,1.,0.707106781186548,
1.,0.707106781186548,1.,1.,1.)))
REPRESENTATION_ITEM('')
SURFACE()
) ;
#41 = (
BOUNDED_SURFACE()
B_SPLINE_SURFACE(2,1,((#114337,#114338),(#114339,#114340),(#114341,#114342),
(#114343,#114344),(#114345,#114346),(#114347,#114348),(#114349,#114350),
(#114351,#114352),(#114353,#114354)),.UNSPECIFIED.,.T.,.F.,.F.)
B_SPLINE_SURFACE_WITH_KNOTS((3,2,2,2,3),(2,2),(0.,1.5707963267949,3.1415926535898,
4.71238898038469,6.28318530717959),(0.,1.586514041419),.UNSPECIFIED.)
GEOMETRIC_REPRESENTATION_ITEM()
RATIONAL_B_SPLINE_SURFACE(((1.,1.),(0.707106781186548,0.707106781186548),
(1.,1.),(0.707106781186548,0.707106781186548),(1.,1.),(0.707106781186548,
0.707106781186548),(1.,1.),(0.707106781186548,0.707106781186548),(1.,1.)))
REPRESENTATION_ITEM('')
SURFACE()
) ;
#42 = (
BOUNDED_SURFACE()
B_SPLINE_SURFACE(2,1,((#114358,#114359),(#114360,#114361),(#114362,#114363),
(#114364,#114365),(#114366,#114367),(#114368,#114369),(#114370,#114371),
(#114372,#114373),(#114374,#114375)),.UNSPECIFIED.,.T.,.F.,.F.)
B_SPLINE_SURFACE_WITH_KNOTS((3,2,2,2,3),(2,2),(0.,1.5707963267949,3.1415926535898,
4.71238898038469,6.28318530717959),(15.5153736066212,15.6567949628585),
 .UNSPECIFIED.)
GEOMETRIC_REPRESENTATION_ITEM()
RATIONAL_B_SPLINE_SURFACE(((1.,1.),(0.707106781186548,0.707106781186548),
(1.,1.),(0.707106781186548,0.707106781186548),(1.,1.),(0.707106781186548,
0.707106781186548),(1.,1.),(0.707106781186548,0.707106781186548),(1.,1.)))
REPRESENTATION_ITEM('')
SURFACE()
) ;
#43 = (
BOUNDED_SURFACE()
B_SPLINE_SURFACE(2,3,((#114380,#114381,#114382,#114383,#114384,#114385,
#114386,#114387,#114388,#114389,#114390,#114391,#114392,#114393,#114394,
#114395,#114396,#114397,#114398,#114399,#114400,#114401,#114402,#114403,
#114404,#114405,#114406,#114407,#114408,#114409,#114410,#114411,#114412,
#114413,#114414,#114415,#114416,#114417,#114418,#114419,#114420,#114421,
#114422,#114423,#114424,#114425,#114426,#114427,#114428,#114429,#114430,
#114431,#114432,#114433,#114434,#114435,#114436,#114437,#114438,#114439,
#114440,#114441,#114442,#114443,#114444,#114445,#114446,#114447,#114448,
#114449,#114450,#114451,#114452,#114453,#114454,#114455,#114456,#114457,
#114458,#114459,#114460,#114461,#114462,#114463,#114464,#114465,#114466,
#114467,#114468,#114469,#114470,#114471,#114472,#114473,#114474,#114475,
#114476,#114477,#114478,#114479,#114480,#114481,#114482,#114483,#114484,
#114485,#114486,#114487,#114488,#114489,#114490,#114491,#114492,#114493,
#114494,#114495,#114496,#114497,#114498,#114499,#114500,#114501,#114502,
#114503,#114504,#114505,#114506,#114507,#114508,#114509,#114510,#114511,
#114512,#114513,#114514,#114515,#114516,#114517,#114518,#114519,#114520,
#114521,#114522,#114523,#114524,#114525,#114526,#114527,#114528,#114529,
#114530,#114531,#114532,#114533,#114534,#114535,#114536,#114537,#114538,
#114539,#114540,#114541,#114542,#114543,#114544,#114545,#114546,#114547,
#114548,#114549,#114550,#114551,#114552,#114553,#114554,#114555,#114556,
#114557,#114558,#114559,#114560,#114561,#114562,#114563,#114564,#114565,
#114566,#114567,#114568,#114569,#114570,#114571,#114572,#114573,#114574,
#114575,#114576,#114577,#114578,#114579,#114580,#114581,#114582,#114583,
#114584,#114585,#114586,#114587,#114588,#114589,#114590,#114591,#114592,
#114593,#114594,#114595,#114596,#114597,#114598,#114599,#114600,#114601,
#114602,#114603,#114604,#114605,#114606,#114607,#114608,#114609,#114610,
#114611,#114612,#114613,#114614,#114615,#114616,#114617,#114618,#114619,
#114620,#114621,#114622,#114623,#114624,#114625,#114626,#114627,#114628,
#114629,#114630,#114631,#114632,#114633,#114634,#114635,#114636,#114637,
#114638,#114639,#114640,#114641,#114642,#114643,#114644,#114645,#114646,
#114647,#114648,#114649,#114650,#114651,#114652,#114653,#114654,#114655,
#114656,#114657,#114658,#114659,#114660,#114661,#114662,#114663,#114664,
#114665,#114666,#114667,#114668,#114669,#114670,#114671,#114672,#114673,
#114674,#114675,#114676,#114677,#114678,#114679,#114680,#114681,#114682,
#114683,#114684,#114685,#114686,#114687,#114688,#114689,#114690,#114691,
#114692,#114693,#114694,#114695,#114696,#114697,#114698,#114699,#114700,
#114701,#114702,#114703,#114704,#114705,#114706,#114707,#114708,#114709,
#114710,#114711,#114712,#114713,#114714,#114715,#114716,#114717,#114718,
#114719,#114720,#114721,#114722,#114723,#114724,#114725,#114726,#114727,
#114728,#114729,#114730,#114731,#114732,#114733,#114734,#114735,#114736,
#114737,#114738,#114739,#114740,#114741,#114742,#114743,#114744,#114745,
#114746,#114747,#114748,#114749,#114750,#114751,#114752,#114753,#114754,
#114755,#114756,#114757,#114758,#114759,#114760,#114761,#114762,#114763,
#114764,#114765,#114766,#114767,#114768,#114769,#114770,#114771,#114772,
#114773,#114774,#114775,#114776,#114777,#114778,#114779,#114780,#114781,
#114782,#114783,#114784,#114785,#114786,#114787,#114788,#114789,#114790,
#114791,#114792,#114793,#114794,#114795,#114796,#114797,#114798,#114799,
#114800,#114801,#114802,#114803,#114804,#114805,#114806,#114807,#114808,
#114809,#114810,#114811,#114812,#114813,#114814,#114815,#114816,#114817,
#114818,#114819,#114820,#114821,#114822,#114823,#114824,#114825,#114826,
#114827,#114828,#114829,#114830,#114831,#114832,#114833,#114834,#114835,
#114836,#114837,#114838,#114839,#114840,#114841,#114842,#114843,#114844,
#114845,#114846,#114847,#114848,#114849,#114850,#114851,#114852,#114853,
#114854,#114855,#114856,#114857,#114858,#114859,#114860,#114861,#114862,
#114863,#114864,#114865,#114866,#114867,#114868,#114869,#114870,#114871,
#114872,#114873,#114874,#114875,#114876,#114877,#114878,#114879,#114880,
#114881,#114882,#114883,#114884,#114885,#114886,#114887,#114888,#114889,
#114890,#114891,#114892,#114893,#114894,#114895,#114896,#114897,#114898,
#114899,#114900,#114901,#114902,#114903,#114904,#114905,#114906,#114907,
#114908,#114909,#114910,#114911,#114912,#114913,#114914,#114915,#114916,
#114917,#114918,#114919,#114920,#114921,#114922,#114923,#114924,#114925,
#114926,#114927,#114928,#114929,#114930,#114931,#114932,#114933,#114934,
#114935,#114936,#114937,#114938,#114939,#114940,#114941,#114942,#114943,
#114944,#114945,#114946,#114947,#114948,#114949,#114950,#114951,#114952,
#114953,#114954,#114955,#114956,#114957,#114958,#114959,#114960,#114961,
#114962,#114963,#114964,#114965,#114966,#114967,#114968,#114969,#114970,
#114971,#114972,#114973,#114974,#114975,#114976,#114977,#114978,#114979,
#114980,#114981,#114982,#114983,#114984,#114985,#114986,#114987,#114988,
#114989,#114990,#114991,#114992,#114993,#114994,#114995,#114996,#114997,
#114998,#114999,#115000,#115001,#115002,#115003,#115004,#115005,#115006,
#115007,#115008,#115009,#115010,#115011,#115012,#115013,#115014,#115015,
#115016,#115017,#115018,#115019,#115020,#115021,#115022,#115023,#115024,
#115025,#115026,#115027,#115028,#115029,#115030,#115031,#115032,#115033,
#115034,#115035,#115036,#115037,#115038,#115039,#115040,#115041,#115042,
#115043,#115044,#115045,#115046,#115047,#115048,#115049,#115050,#115051,
#115052,#115053,#115054,#115055,#115056,#115057,#115058,#115059,#115060,
#115061,#115062,#115063,#115064,#115065,#115066,#115067,#115068,#115069,
#115070,#115071,#115072,#115073,#115074,#115075,#115076,#115077,#115078,
#115079,#115080,#115081,#115082,#115083,#115084,#115085,#115086,#115087,
#115088,#115089,#115090,#115091,#115092,#115093,#115094,#115095,#115096,
#115097,#115098,#115099,#115100,#115101,#115102,#115103,#115104,#115105,
#115106,#115107,#115108,#115109,#115110,#115111,#115112,#115113,#115114,
#115115,#115116,#115117,#115118,#115119,#115120,#115121,#115122,#115123,
#115124,#115125,#115126,#115127,#115128,#115129,#115130,#115131,#115132,
#115133,#115134,#115135,#115136,#115137,#115138,#115139,#115140,#115141,
#115142,#115143,#115144,#115145,#115146,#115147,#115148,#115149,#115150,
#115151,#115152,#115153,#115154,#115155,#115156,#115157,#115158,#115159,
#115160,#115161,#115162,#115163,#115164,#115165,#115166,#115167,#115168,
#115169,#115170,#115171,#115172,#115173,#115174,#115175,#115176,#115177,
#115178,#115179,#115180,#115181,#115182,#115183,#115184,#115185,#115186,
#115187,#115188,#115189,#115190,#115191,#115192,#115193,#115194,#115195,
#115196,#115197,#115198,#115199,#115200,#115201,#115202,#115203,#115204,
#115205,#115206,#115207,#115208,#115209,#115210,#115211,#115212,#115213,
#115214,#115215,#115216,#115217,#115218,#115219,#115220,#115221,#115222,
#115223,#115224,#115225,#115226,#115227,#115228,#115229,#115230,#115231,
#115232,#115233,#115234,#115235,#115236,#115237,#115238,#115239,#115240,
#115241,#115242,#115243,#115244,#115245,#115246,#115247,#115248,#115249,
#115250,#115251,#115252,#115253,#115254,#115255,#115256,#115257,#115258,
#115259,#115260,#115261,#115262,#115263,#115264,#115265,#115266,#115267,
#115268,#115269,#115270,#115271,#115272,#115273,#115274,#115275,#115276,
#115277,#115278,#115279,#115280,#115281,#115282,#115283,#115284,#115285,
#115286,#115287,#115288,#115289,#115290,#115291,#115292,#115293,#115294,
#115295,#115296,#115297,#115298,#115299,#115300,#115301,#115302,#115303,
#115304,#115305,#115306,#115307,#115308,#115309,#115310,#115311,#115312,
#115313,#115314,#115315,#115316,#115317,#115318,#115319,#115320,#115321,
#115322,#115323,#115324,#115325,#115326,#115327,#115328,#115329,#115330,
#115331,#115332,#115333,#115334,#115335,#115336,#115337,#115338,#115339,
#115340,#115341,#115342,#115343,#115344,#115345,#115346,#115347,#115348,
#115349,#115350,#115351,#115352,#115353,#115354,#115355,#115356,#115357,
#115358,#115359,#115360,#115361,#115362,#115363,#115364,#115365,#115366,
#115367,#115368,#115369,#115370,#115371,#115372,#115373,#115374,#115375,
#115376,#115377,#115378,#115379,#115380,#115381,#115382,#115383,#115384,
#115385,#115386,#115387,#115388,#115389,#115390,#115391,#115392,#115393,
#115394,#115395,#115396,#115397,#115398,#115399,#115400,#115401,#115402,
#115403,#115404,#115405,#115406,#115407,#115408,#115409,#115410,#115411,
#115412,#115413,#115414,#115415,#115416,#115417,#115418,#115419,#115420,
#115421,#115422,#115423,#115424,#115425,#115426,#115427,#115428,#115429,
#115430,#115431,#115432,#115433,#115434,#115435,#115436,#115437,#115438,
#115439,#115440,#115441,#115442,#115443,#115444,#115445,#115446,#115447,
#115448,#115449,#115450,#115451,#115452,#115453,#115454,#115455,#115456,
#115457,#115458,#115459,#115460,#115461,#115462,#115463,#115464,#115465,
#115466,#115467,#115468,#115469,#115470,#115471,#115472,#115473,#115474,
#115475,#115476,#115477,#115478,#115479,#115480,#115481,#115482,#115483,
#115484,#115485,#115486,#115487,#115488,#115489,#115490,#115491,#115492,
#115493,#115494,#115495,#115496,#115497,#115498,#115499,#115500,#115501,
#115502,#115503,#115504,#115505,#115506,#115507,#115508,#115509,#115510,
#115511,#115512,#115513,#115514,#115515,#115516,#115517,#115518,#115519,
#115520,#115521,#115522,#115523,#115524,#115525,#115526,#115527,#115528,
#115529,#115530,#115531,#115532,#115533,#115534,#115535,#115536,#115537,
#115538,#115539,#115540,#115541,#115542,#115543,#115544,#115545,#115546,
#115547,#115548,#115549,#115550,#115551,#115552,#115553,#115554,#115555,
#115556,#115557,#115558,#115559,#115560,#115561,#115562,#115563,#115564,
#115565,#115566,#115567,#115568,#115569,#115570,#115571,#115572,#115573,
#115574,#115575,#115576,#115577,#115578,#115579,#115580,#115581,#115582,
#115583,#115584,#115585,#115586,#115587,#115588,#115589,#115590,#115591,
#115592,#115593,#115594,#115595,#115596,#115597,#115598,#115599,#115600,
#115601,#115602,#115603,#115604,#115605,#115606,#115607,#115608,#115609,
#115610,#115611,#115612,#115613,#115614,#115615,#115616,#115617,#115618,
#115619,#115620,#115621,#115622,#115623,#115624,#115625,#115626,#115627,
#115628,#115629,#115630,#115631,#115632,#115633,#115634,#115635,#115636,
#115637,#115638,#115639,#115640,#115641,#115642,#115643,#115644,#115645,
#115646,#115647,#115648,#115649,#115650,#115651,#115652,#115653,#115654,
#115655,#115656,#115657,#115658,#115659,#115660,#115661,#115662,#115663,
#115664,#115665,#115666,#115667,#115668,#115669,#115670,#115671,#115672,
#115673,#115674,#115675,#115676,#115677,#115678,#115679,#115680,#115681,
#115682,#115683,#115684,#115685,#115686,#115687,#115688,#115689,#115690,
#115691,#115692,#115693,#115694,#115695,#115696,#115697,#115698,#115699,
#115700,#115701,#115702,#115703,#115704,#115705,#115706,#115707,#115708,
#115709,#115710,#115711,#115712,#115713,#115714,#115715,#115716,#115717,
#115718,#115719,#115720,#115721,#115722,#115723,#115724,#115725,#115726,
#115727,#115728,#115729,#115730,#115731,#115732,#115733,#115734,#115735,
#115736,#115737,#115738,#115739,#115740,#115741,#115742,#115743,#115744,
#115745,#115746,#115747,#115748,#115749,#115750,#115751,#115752,#115753,
#115754,#115755,#115756,#115757,#115758,#115759,#115760,#115761,#115762,
#115763,#115764,#115765,#115766,#115767,#115768,#115769,#115770,#115771,
#115772,#115773,#115774,#115775,#115776,#115777,#115778,#115779,#115780,
#115781,#115782,#115783,#115784,#115785,#115786,#115787,#115788,#115789,
#115790,#115791,#115792,#115793,#115794,#115795,#115796,#115797,#115798,
#115799,#115800,#115801,#115802,#115803,#115804,#115805,#115806,#115807,
#115808,#115809,#115810,#115811,#115812,#115813,#115814,#115815,#115816,
#115817,#115818,#115819,#115820,#115821,#115822,#115823,#115824,#115825,
#115826,#115827,#115828,#115829,#115830,#115831,#115832,#115833,#115834,
#115835,#115836,#115837,#115838,#115839,#115840,#115841,#115842,#115843,
#115844,#115845,#115846,#115847,#115848,#115849,#115850,#115851,#115852,
#115853,#115854,#115855,#115856,#115857,#115858,#115859,#115860,#115861,
#115862,#115863,#115864,#115865,#115866,#115867,#115868,#115869,#115870,
#115871,#115872,#115873,#115874,#115875,#115876,#115877,#115878,#115879,
#115880,#115881,#115882,#115883,#115884,#115885,#115886,#115887,#115888,
#115889,#115890,#115891,#115892,#115893,#115894,#115895,#115896,#115897,
#115898,#115899,#115900,#115901,#115902,#115903,#115904,#115905,#115906,
#115907,#115908,#115909,#115910,#115911,#115912,#115913,#115914,#115915,
#115916,#115917,#115918,#115919,#115920,#115921,#115922,#115923,#115924,
#115925,#115926,#115927,#115928,#115929,#115930,#115931,#115932,#115933,
#115934,#115935,#115936,#115937,#115938,#115939,#115940,#115941,#115942,
#115943,#115944,#115945,#115946,#115947,#115948,#115949,#115950,#115951,
#115952,#115953,#115954,#115955,#115956,#115957,#115958,#115959,#115960,
#115961,#115962,#115963,#115964,#115965,#115966,#115967,#115968,#115969,
#115970,#115971,#115972,#115973,#115974,#115975,#115976,#115977,#115978,
#115979,#115980,#115981,#115982,#115983,#115984,#115985,#115986,#115987,
#115988,#115989,#115990,#115991,#115992,#115993,#115994,#115995,#115996,
#115997,#115998,#115999,#116000,#116001,#116002,#116003,#116004,#116005,
#116006,#116007,#116008,#116009,#116010,#116011,#116012,#116013,#116014,
#116015,#116016,#116017,#116018,#116019,#116020,#116021,#116022,#116023,
#116024,#116025,#116026,#116027,#116028,#116029,#116030,#116031,#116032,
#116033,#116034,#116035,#116036,#116037,#116038,#116039,#116040,#116041,
#116042,#116043,#116044,#116045,#116046,#116047,#116048,#116049,#116050,
#116051,#116052,#116053,#116054,#116055,#116056,#116057,#116058,#116059,
#116060,#116061,#116062,#116063,#116064,#116065,#116066,#116067,#116068,
#116069,#116070,#116071,#116072,#116073,#116074,#116075,#116076,#116077,
#116078,#116079,#116080,#116081,#116082,#116083,#116084,#116085,#116086,
#116087,#116088,#116089,#116090,#116091,#116092,#116093,#116094,#116095,
#116096,#116097,#116098,#116099,#116100,#116101,#116102,#116103,#116104,
#116105,#116106,#116107,#116108,#116109,#116110,#116111,#116112,#116113,
#116114,#116115,#116116,#116117,#116118,#116119,#116120,#116121,#116122,
#116123,#116124,#116125,#116126,#116127,#116128,#116129,#116130,#116131,
#116132,#116133,#116134,#116135,#116136,#116137,#116138,#116139,#116140,
#116141,#116142,#116143,#116144,#116145,#116146,#116147,#116148,#116149,
#116150,#116151,#116152,#116153,#116154,#116155,#116156,#116157,#116158,
#116159,#116160,#116161,#116162,#116163,#116164,#116165,#116166,#116167,
#116168,#116169,#116170,#116171,#116172,#116173,#116174,#116175,#116176,
#116177,#116178,#116179,#116180,#116181,#116182,#116183,#116184,#116185,
#116186,#116187,#116188,#116189,#116190,#116191,#116192,#116193,#116194,
#116195,#116196,#116197,#116198,#116199,#116200,#116201,#116202,#116203,
#116204,#116205,#116206,#116207,#116208,#116209,#116210,#116211,#116212,
#116213,#116214,#116215,#116216,#116217,#116218,#116219,#116220,#116221,
#116222,#116223,#116224,#116225,#116226,#116227,#116228,#116229,#116230,
#116231,#116232,#116233,#116234,#116235,#116236,#116237,#116238,#116239,
#116240,#116241,#116242,#116243,#116244,#116245,#116246,#116247,#116248,
#116249,#116250,#116251,#116252,#116253,#116254,#116255,#116256,#116257,
#116258,#116259,#116260,#116261,#116262,#116263,#116264,#116265,#116266,
#116267,#116268,#116269,#116270,#116271,#116272,#116273,#116274,#116275,
#116276,#116277,#116278,#116279,#116280,#116281,#116282,#116283,#116284,
#116285,#116286,#116287,#116288,#116289,#116290,#116291,#116292,#116293,
#116294,#116295,#116296,#116297,#116298,#116299,#116300,#116301,#116302,
#116303,#116304,#116305,#116306,#116307,#116308,#116309,#116310,#116311,
#116312,#116313,#116314,#116315,#116316,#116317,#116318,#116319,#116320,
#116321,#116322,#116323,#116324,#116325,#116326,#116327,#116328,#116329,
#116330,#116331,#116332,#116333,#116334,#116335,#116336,#116337,#116338,
#116339,#116340,#116341,#116342,#116343,#116344,#116345,#116346,#116347,
#116348,#116349,#116350,#116351,#116352,#116353,#116354,#116355,#116356,
#116357,#116358,#116359,#116360,#116361,#116362,#116363,#116364,#116365,
#116366,#116367,#116368,#116369,#116370,#116371,#116372,#116373,#116374,
#116375,#116376,#116377,#116378,#116379,#116380,#116381,#116382,#116383,
#116384,#116385,#116386,#116387,#116388,#116389,#116390,#116391,#116392,
#116393,#116394,#116395,#116396,#116397,#116398,#116399,#116400,#116401,
#116402,#116403,#116404,#116405,#116406,#116407,#116408,#116409,#116410,
#116411,#116412,#116413,#116414,#116415,#116416,#116417,#116418,#116419,
#116420,#116421,#116422,#116423,#116424,#116425,#116426,#116427,#116428,
#116429,#116430),(#116431,#116432,#116433,#116434,#116435,#116436,#116437,
#116438,#116439,#116440,#116441,#116442,#116443,#116444,#116445,#116446,
#116447,#116448,#116449,#116450,#116451,#116452,#116453,#116454,#116455,
#116456,#116457,#116458,#116459,#116460,#116461,#116462,#116463,#116464,
#116465,#116466,#116467,#116468,#116469,#116470,#116471,#116472,#116473,
#116474,#116475,#116476,#116477,#116478,#116479,#116480,#116481,#116482,
#116483,#116484,#116485,#116486,#116487,#116488,#116489,#116490,#116491,
#116492,#116493,#116494,#116495,#116496,#116497,#116498,#116499,#116500,
#116501,#116502,#116503,#116504,#116505,#116506,#116507,#116508,#116509,
#116510,#116511,#116512,#116513,#116514,#116515,#116516,#116517,#116518,
#116519,#116520,#116521,#116522,#116523,#116524,#116525,#116526,#116527,
#116528,#116529,#116530,#116531,#116532,#116533,#116534,#116535,#116536,
#116537,#116538,#116539,#116540,#116541,#116542,#116543,#116544,#116545,
#116546,#116547,#116548,#116549,#116550,#116551,#116552,#116553,#116554,
#116555,#116556,#116557,#116558,#116559,#116560,#116561,#116562,#116563,
#116564,#116565,#116566,#116567,#116568,#116569,#116570,#116571,#116572,
#116573,#116574,#116575,#116576,#116577,#116578,#116579,#116580,#116581,
#116582,#116583,#116584,#116585,#116586,#116587,#116588,#116589,#116590,
#116591,#116592,#116593,#116594,#116595,#116596,#116597,#116598,#116599,
#116600,#116601,#116602,#116603,#116604,#116605,#116606,#116607,#116608,
#116609,#116610,#116611,#116612,#116613,#116614,#116615,#116616,#116617,
#116618,#116619,#116620,#116621,#116622,#116623,#116624,#116625,#116626,
#116627,#116628,#116629,#116630,#116631,#116632,#116633,#116634,#116635,
#116636,#116637,#116638,#116639,#116640,#116641,#116642,#116643,#116644,
#116645,#116646,#116647,#116648,#116649,#116650,#116651,#116652,#116653,
#116654,#116655,#116656,#116657,#116658,#116659,#116660,#116661,#116662,
#116663,#116664,#116665,#116666,#116667,#116668,#116669,#116670,#116671,
#116672,#116673,#116674,#116675,#116676,#116677,#116678,#116679,#116680,
#116681,#116682,#116683,#116684,#116685,#116686,#116687,#116688,#116689,
#116690,#116691,#116692,#116693,#116694,#116695,#116696,#116697,#116698,
#116699,#116700,#116701,#116702,#116703,#116704,#116705,#116706,#116707,
#116708,#116709,#116710,#116711,#116712,#116713,#116714,#116715,#116716,
#116717,#116718,#116719,#116720,#116721,#116722,#116723,#116724,#116725,
#116726,#116727,#116728,#116729,#116730,#116731,#116732,#116733,#116734,
#116735,#116736,#116737,#116738,#116739,#116740,#116741,#116742,#116743,
#116744,#116745,#116746,#116747,#116748,#116749,#116750,#116751,#116752,
#116753,#116754,#116755,#116756,#116757,#116758,#116759,#116760,#116761,
#116762,#116763,#116764,#116765,#116766,#116767,#116768,#116769,#116770,
#116771,#116772,#116773,#116774,#116775,#116776,#116777,#116778,#116779,
#116780,#116781,#116782,#116783,#116784,#116785,#116786,#116787,#116788,
#116789,#116790,#116791,#116792,#116793,#116794,#116795,#116796,#116797,
#116798,#116799,#116800,#116801,#116802,#116803,#116804,#116805,#116806,
#116807,#116808,#116809,#116810,#116811,#116812,#116813,#116814,#116815,
#116816,#116817,#116818,#116819,#116820,#116821,#116822,#116823,#116824,
#116825,#116826,#116827,#116828,#116829,#116830,#116831,#116832,#116833,
#116834,#116835,#116836,#116837,#116838,#116839,#116840,#116841,#116842,
#116843,#116844,#116845,#116846,#116847,#116848,#116849,#116850,#116851,
#116852,#116853,#116854,#116855,#116856,#116857,#116858,#116859,#116860,
#116861,#116862,#116863,#116864,#116865,#116866,#116867,#116868,#116869,
#116870,#116871,#116872,#116873,#116874,#116875,#116876,#116877,#116878,
#116879,#116880,#116881,#116882,#116883,#116884,#116885,#116886,#116887,
#116888,#116889,#116890,#116891,#116892,#116893,#116894,#116895,#116896,
#116897,#116898,#116899,#116900,#116901,#116902,#116903,#116904,#116905,
#116906,#116907,#116908,#116909,#116910,#116911,#116912,#116913,#116914,
#116915,#116916,#116917,#116918,#116919,#116920,#116921,#116922,#116923,
#116924,#116925,#116926,#116927,#116928,#116929,#116930,#116931,#116932,
#116933,#116934,#116935,#116936,#116937,#116938,#116939,#116940,#116941,
#116942,#116943,#116944,#116945,#116946,#116947,#116948,#116949,#116950,
#116951,#116952,#116953,#116954,#116955,#116956,#116957,#116958,#116959,
#116960,#116961,#116962,#116963,#116964,#116965,#116966,#116967,#116968,
#116969,#116970,#116971,#116972,#116973,#116974,#116975,#116976,#116977,
#116978,#116979,#116980,#116981,#116982,#116983,#116984,#116985,#116986,
#116987,#116988,#116989,#116990,#116991,#116992,#116993,#116994,#116995,
#116996,#116997,#116998,#116999,#117000,#117001,#117002,#117003,#117004,
#117005,#117006,#117007,#117008,#117009,#117010,#117011,#117012,#117013,
#117014,#117015,#117016,#117017,#117018,#117019,#117020,#117021,#117022,
#117023,#117024,#117025,#117026,#117027,#117028,#117029,#117030,#117031,
#117032,#117033,#117034,#117035,#117036,#117037,#117038,#117039,#117040,
#117041,#117042,#117043,#117044,#117045,#117046,#117047,#117048,#117049,
#117050,#117051,#117052,#117053,#117054,#117055,#117056,#117057,#117058,
#117059,#117060,#117061,#117062,#117063,#117064,#117065,#117066,#117067,
#117068,#117069,#117070,#117071,#117072,#117073,#117074,#117075,#117076,
#117077,#117078,#117079,#117080,#117081,#117082,#117083,#117084,#117085,
#117086,#117087,#117088,#117089,#117090,#117091,#117092,#117093,#117094,
#117095,#117096,#117097,#117098,#117099,#117100,#117101,#117102,#117103,
#117104,#117105,#117106,#117107,#117108,#117109,#117110,#117111,#117112,
#117113,#117114,#117115,#117116,#117117,#117118,#117119,#117120,#117121,
#117122,#117123,#117124,#117125,#117126,#117127,#117128,#117129,#117130,
#117131,#117132,#117133,#117134,#117135,#117136,#117137,#117138,#117139,
#117140,#117141,#117142,#117143,#117144,#117145,#117146,#117147,#117148,
#117149,#117150,#117151,#117152,#117153,#117154,#117155,#117156,#117157,
#117158,#117159,#117160,#117161,#117162,#117163,#117164,#117165,#117166,
#117167,#117168,#117169,#117170,#117171,#117172,#117173,#117174,#117175,
#117176,#117177,#117178,#117179,#117180,#117181,#117182,#117183,#117184,
#117185,#117186,#117187,#117188,#117189,#117190,#117191,#117192,#117193,
#117194,#117195,#117196,#117197,#117198,#117199,#117200,#117201,#117202,
#117203,#117204,#117205,#117206,#117207,#117208,#117209,#117210,#117211,
#117212,#117213,#117214,#117215,#117216,#117217,#117218,#117219,#117220,
#117221,#117222,#117223,#117224,#117225,#117226,#117227,#117228,#117229,
#117230,#117231,#117232,#117233,#117234,#117235,#117236,#117237,#117238,
#117239,#117240,#117241,#117242,#117243,#117244,#117245,#117246,#117247,
#117248,#117249,#117250,#117251,#117252,#117253,#117254,#117255,#117256,
#117257,#117258,#117259,#117260,#117261,#117262,#117263,#117264,#117265,
#117266,#117267,#117268,#117269,#117270,#117271,#117272,#117273,#117274,
#117275,#117276,#117277,#117278,#117279,#117280,#117281,#117282,#117283,
#117284,#117285,#117286,#117287,#117288,#117289,#117290,#117291,#117292,
#117293,#117294,#117295,#117296,#117297,#117298,#117299,#117300,#117301,
#117302,#117303,#117304,#117305,#117306,#117307,#117308,#117309,#117310,
#117311,#117312,#117313,#117314,#117315,#117316,#117317,#117318,#117319,
#117320,#117321,#117322,#117323,#117324,#117325,#117326,#117327,#117328,
#117329,#117330,#117331,#117332,#117333,#117334,#117335,#117336,#117337,
#117338,#117339,#117340,#117341,#117342,#117343,#117344,#117345,#117346,
#117347,#117348,#117349,#117350,#117351,#117352,#117353,#117354,#117355,
#117356,#117357,#117358,#117359,#117360,#117361,#117362,#117363,#117364,
#117365,#117366,#117367,#117368,#117369,#117370,#117371,#117372,#117373,
#117374,#117375,#117376,#117377,#117378,#117379,#117380,#117381,#117382,
#117383,#117384,#117385,#117386,#117387,#117388,#117389,#117390,#117391,
#117392,#117393,#117394,#117395,#117396,#117397,#117398,#117399,#117400,
#117401,#117402,#117403,#117404,#117405,#117406,#117407,#117408,#117409,
#117410,#117411,#117412,#117413,#117414,#117415,#117416,#117417,#117418,
#117419,#117420,#117421,#117422,#117423,#117424,#117425,#117426,#117427,
#117428,#117429,#117430,#117431,#117432,#117433,#117434,#117435,#117436,
#117437,#117438,#117439,#117440,#117441,#117442,#117443,#117444,#117445,
#117446,#117447,#117448,#117449,#117450,#117451,#117452,#117453,#117454,
#117455,#117456,#117457,#117458,#117459,#117460,#117461,#117462,#117463,
#117464,#117465,#117466,#117467,#117468,#117469,#117470,#117471,#117472,
#117473,#117474,#117475,#117476,#117477,#117478,#117479,#117480,#117481,
#117482,#117483,#117484,#117485,#117486,#117487,#117488,#117489,#117490,
#117491,#117492,#117493,#117494,#117495,#117496,#117497,#117498,#117499,
#117500,#117501,#117502,#117503,#117504,#117505,#117506,#117507,#117508,
#117509,#117510,#117511,#117512,#117513,#117514,#117515,#117516,#117517,
#117518,#117519,#117520,#117521,#117522,#117523,#117524,#117525,#117526,
#117527,#117528,#117529,#117530,#117531,#117532,#117533,#117534,#117535,
#117536,#117537,#117538,#117539,#117540,#117541,#117542,#117543,#117544,
#117545,#117546,#117547,#117548,#117549,#117550,#117551,#117552,#117553,
#117554,#117555,#117556,#117557,#117558,#117559,#117560,#117561,#117562,
#117563,#117564,#117565,#117566,#117567,#117568,#117569,#117570,#117571,
#117572,#117573,#117574,#117575,#117576,#117577,#117578,#117579,#117580,
#117581,#117582,#117583,#117584,#117585,#117586,#117587,#117588,#117589,
#117590,#117591,#117592,#117593,#117594,#117595,#117596,#117597,#117598,
#117599,#117600,#117601,#117602,#117603,#117604,#117605,#117606,#117607,
#117608,#117609,#117610,#117611,#117612,#117613,#117614,#117615,#117616,
#117617,#117618,#117619,#117620,#117621,#117622,#117623,#117624,#117625,
#117626,#117627,#117628,#117629,#117630,#117631,#117632,#117633,#117634,
#117635,#117636,#117637,#117638,#117639,#117640,#117641,#117642,#117643,
#117644,#117645,#117646,#117647,#117648,#117649,#117650,#117651,#117652,
#117653,#117654,#117655,#117656,#117657,#117658,#117659,#117660,#117661,
#117662,#117663,#117664,#117665,#117666,#117667,#117668,#117669,#117670,
#117671,#117672,#117673,#117674,#117675,#117676,#117677,#117678,#117679,
#117680,#117681,#117682,#117683,#117684,#117685,#117686,#117687,#117688,
#117689,#117690,#117691,#117692,#117693,#117694,#117695,#117696,#117697,
#117698,#117699,#117700,#117701,#117702,#117703,#117704,#117705,#117706,
#117707,#117708,#117709,#117710,#117711,#117712,#117713,#117714,#117715,
#117716,#117717,#117718,#117719,#117720,#117721,#117722,#117723,#117724,
#117725,#117726,#117727,#117728,#117729,#117730,#117731,#117732,#117733,
#117734,#117735,#117736,#117737,#117738,#117739,#117740,#117741,#117742,
#117743,#117744,#117745,#117746,#117747,#117748,#117749,#117750,#117751,
#117752,#117753,#117754,#117755,#117756,#117757,#117758,#117759,#117760,
#117761,#117762,#117763,#117764,#117765,#117766,#117767,#117768,#117769,
#117770,#117771,#117772,#117773,#117774,#117775,#117776,#117777,#117778,
#117779,#117780,#117781,#117782,#117783,#117784,#117785,#117786,#117787,
#117788,#117789,#117790,#117791,#117792,#117793,#117794,#117795,#117796,
#117797,#117798,#117799,#117800,#117801,#117802,#117803,#117804,#117805,
#117806,#117807,#117808,#117809,#117810,#117811,#117812,#117813,#117814,
#117815,#117816,#117817,#117818,#117819,#117820,#117821,#117822,#117823,
#117824,#117825,#117826,#117827,#117828,#117829,#117830,#117831,#117832,
#117833,#117834,#117835,#117836,#117837,#117838,#117839,#117840,#117841,
#117842,#117843,#117844,#117845,#117846,#117847,#117848,#117849,#117850,
#117851,#117852,#117853,#117854,#117855,#117856,#117857,#117858,#117859,
#117860,#117861,#117862,#117863,#117864,#117865,#117866,#117867,#117868,
#117869,#117870,#117871,#117872,#117873,#117874,#117875,#117876,#117877,
#117878,#117879,#117880,#117881,#117882,#117883,#117884,#117885,#117886,
#117887,#117888,#117889,#117890,#117891,#117892,#117893,#117894,#117895,
#117896,#117897,#117898,#117899,#117900,#117901,#117902,#117903,#117904,
#117905,#117906,#117907,#117908,#117909,#117910,#117911,#117912,#117913,
#117914,#117915,#117916,#117917,#117918,#117919,#117920,#117921,#117922,
#117923,#117924,#117925,#117926,#117927,#117928,#117929,#117930,#117931,
#117932,#117933,#117934,#117935,#117936,#117937,#117938,#117939,#117940,
#117941,#117942,#117943,#117944,#117945,#117946,#117947,#117948,#117949,
#117950,#117951,#117952,#117953,#117954,#117955,#117956,#117957,#117958,
#117959,#117960,#117961,#117962,#117963,#117964,#117965,#117966,#117967,
#117968,#117969,#117970,#117971,#117972,#117973,#117974,#117975,#117976,
#117977,#117978,#117979,#117980,#117981,#117982,#117983,#117984,#117985,
#117986,#117987,#117988,#117989,#117990,#117991,#117992,#117993,#117994,
#117995,#117996,#117997,#117998,#117999,#118000,#118001,#118002,#118003,
#118004,#118005,#118006,#118007,#118008,#118009,#118010,#118011,#118012,
#118013,#118014,#118015,#118016,#118017,#118018,#118019,#118020,#118021,
#118022,#118023,#118024,#118025,#118026,#118027,#118028,#118029,#118030,
#118031,#118032,#118033,#118034,#118035,#118036,#118037,#118038,#118039,
#118040,#118041,#118042,#118043,#118044,#118045,#118046,#118047,#118048,
#118049,#118050,#118051,#118052,#118053,#118054,#118055,#118056,#118057,
#118058,#118059,#118060,#118061,#118062,#118063,#118064,#118065,#118066,
#118067,#118068,#118069,#118070,#118071,#118072,#118073,#118074,#118075,
#118076,#118077,#118078,#118079,#118080,#118081,#118082,#118083,#118084,
#118085,#118086,#118087,#118088,#118089,#118090,#118091,#118092,#118093,
#118094,#118095,#118096,#118097,#118098,#118099,#118100,#118101,#118102,
#118103,#118104,#118105,#118106,#118107,#118108,#118109,#118110,#118111,
#118112,#118113,#118114,#118115,#118116,#118117,#118118,#118119,#118120,
#118121,#118122,#118123,#118124,#118125,#118126,#118127,#118128,#118129,
#118130,#118131,#118132,#118133,#118134,#118135,#118136,#118137,#118138,
#118139,#118140,#118141,#118142,#118143,#118144,#118145,#118146,#118147,
#118148,#118149,#118150,#118151,#118152,#118153,#118154,#118155,#118156,
#118157,#118158,#118159,#118160,#118161,#118162,#118163,#118164,#118165,
#118166,#118167,#118168,#118169,#118170,#118171,#118172,#118173,#118174,
#118175,#118176,#118177,#118178,#118179,#118180,#118181,#118182,#118183,
#118184,#118185,#118186,#118187,#118188,#118189,#118190,#118191,#118192,
#118193,#118194,#118195,#118196,#118197,#118198,#118199,#118200,#118201,
#118202,#118203,#118204,#118205,#118206,#118207,#118208,#118209,#118210,
#118211,#118212,#118213,#118214,#118215,#118216,#118217,#118218,#118219,
#118220,#118221,#118222,#118223,#118224,#118225,#118226,#118227,#118228,
#118229,#118230,#118231,#118232,#118233,#118234,#118235,#118236,#118237,
#118238,#118239,#118240,#118241,#118242,#118243,#118244,#118245,#118246,
#118247,#118248,#118249,#118250,#118251,#118252,#118253,#118254,#118255,
#118256,#118257,#118258,#118259,#118260,#118261,#118262,#118263,#118264,
#118265,#118266,#118267,#118268,#118269,#118270,#118271,#118272,#118273,
#118274,#118275,#118276,#118277,#118278,#118279,#118280,#118281,#118282,
#118283,#118284,#118285,#118286,#118287,#118288,#118289,#118290,#118291,
#118292,#118293,#118294,#118295,#118296,#118297,#118298,#118299,#118300,
#118301,#118302,#118303,#118304,#118305,#118306,#118307,#118308,#118309,
#118310,#118311,#118312,#118313,#118314,#118315,#118316,#118317,#118318,
#118319,#118320,#118321,#118322,#118323,#118324,#118325,#118326,#118327,
#118328,#118329,#118330,#118331,#118332,#118333,#118334,#118335,#118336,
#118337,#118338,#118339,#118340,#118341,#118342,#118343,#118344,#118345,
#118346,#118347,#118348,#118349,#118350,#118351,#118352,#118353,#118354,
#118355,#118356,#118357,#118358,#118359,#118360,#118361,#118362,#118363,
#118364,#118365,#118366,#118367,#118368,#118369,#118370,#118371,#118372,
#118373,#118374,#118375,#118376,#118377,#118378,#118379,#118380,#118381,
#118382,#118383,#118384,#118385,#118386,#118387,#118388,#118389,#118390,
#118391,#118392,#118393,#118394,#118395,#118396,#118397,#118398,#118399,
#118400,#118401,#118402,#118403,#118404,#118405,#118406,#118407,#118408,
#118409,#118410,#118411,#118412,#118413,#118414,#118415,#118416,#118417,
#118418,#118419,#118420,#118421,#118422,#118423,#118424,#118425,#118426,
#118427,#118428,#118429,#118430,#118431,#118432,#118433,#118434,#118435,
#118436,#118437,#118438,#118439,#118440,#118441,#118442,#118443,#118444,
#118445,#118446,#118447,#118448,#118449,#118450,#118451,#118452,#118453,
#118454,#118455,#118456,#118457,#118458,#118459,#118460,#118461,#118462,
#118463,#118464,#118465,#118466,#118467,#118468,#118469,#118470,#118471,
#118472,#118473,#118474,#118475,#118476,#118477,#118478,#118479,#118480,
#118481),(#118482,#118483,#118484,#118485,#118486,#118487,#118488,#118489,
#118490,#118491,#118492,#118493,#118494,#118495,#118496,#118497,#118498,
#118499,#118500,#118501,#118502,#118503,#118504,#118505,#118506,#118507,
#118508,#118509,#118510,#118511,#118512,#118513,#118514,#118515,#118516,
#118517,#118518,#118519,#118520,#118521,#118522,#118523,#118524,#118525,
#118526,#118527,#118528,#118529,#118530,#118531,#118532,#118533,#118534,
#118535,#118536,#118537,#118538,#118539,#118540,#118541,#118542,#118543,
#118544,#118545,#118546,#118547,#118548,#118549,#118550,#118551,#118552,
#118553,#118554,#118555,#118556,#118557,#118558,#118559,#118560,#118561,
#118562,#118563,#118564,#118565,#118566,#118567,#118568,#118569,#118570,
#118571,#118572,#118573,#118574,#118575,#118576,#118577,#118578,#118579,
#118580,#118581,#118582,#118583,#118584,#118585,#118586,#118587,#118588,
#118589,#118590,#118591,#118592,#118593,#118594,#118595,#118596,#118597,
#118598,#118599,#118600,#118601,#118602,#118603,#118604,#118605,#118606,
#118607,#118608,#118609,#118610,#118611,#118612,#118613,#118614,#118615,
#118616,#118617,#118618,#118619,#118620,#118621,#118622,#118623,#118624,
#118625,#118626,#118627,#118628,#118629,#118630,#118631,#118632,#118633,
#118634,#118635,#118636,#118637,#118638,#118639,#118640,#118641,#118642,
#118643,#118644,#118645,#118646,#118647,#118648,#118649,#118650,#118651,
#118652,#118653,#118654,#118655,#118656,#118657,#118658,#118659,#118660,
#118661,#118662,#118663,#118664,#118665,#118666,#118667,#118668,#118669,
#118670,#118671,#118672,#118673,#118674,#118675,#118676,#118677,#118678,
#118679,#118680,#118681,#118682,#118683,#118684,#118685,#118686,#118687,
#118688,#118689,#118690,#118691,#118692,#118693,#118694,#118695,#118696,
#118697,#118698,#118699,#118700,#118701,#118702,#118703,#118704,#118705,
#118706,#118707,#118708,#118709,#118710,#118711,#118712,#118713,#118714,
#118715,#118716,#118717,#118718,#118719,#118720,#118721,#118722,#118723,
#118724,#118725,#118726,#118727,#118728,#118729,#118730,#118731,#118732,
#118733,#118734,#118735,#118736,#118737,#118738,#118739,#118740,#118741,
#118742,#118743,#118744,#118745,#118746,#118747,#118748,#118749,#118750,
#118751,#118752,#118753,#118754,#118755,#118756,#118757,#118758,#118759,
#118760,#118761,#118762,#118763,#118764,#118765,#118766,#118767,#118768,
#118769,#118770,#118771,#118772,#118773,#118774,#118775,#118776,#118777,
#118778,#118779,#118780,#118781,#118782,#118783,#118784,#118785,#118786,
#118787,#118788,#118789,#118790,#118791,#118792,#118793,#118794,#118795,
#118796,#118797,#118798,#118799,#118800,#118801,#118802,#118803,#118804,
#118805,#118806,#118807,#118808,#118809,#118810,#118811,#118812,#118813,
#118814,#118815,#118816,#118817,#118818,#118819,#118820,#118821,#118822,
#118823,#118824,#118825,#118826,#118827,#118828,#118829,#118830,#118831,
#118832,#118833,#118834,#118835,#118836,#118837,#118838,#118839,#118840,
#118841,#118842,#118843,#118844,#118845,#118846,#118847,#118848,#118849,
#118850,#118851,#118852,#118853,#118854,#118855,#118856,#118857,#118858,
#118859,#118860,#118861,#118862,#118863,#118864,#118865,#118866,#118867,
#118868,#118869,#118870,#118871,#118872,#118873,#118874,#118875,#118876,
#118877,#118878,#118879,#118880,#118881,#118882,#118883,#118884,#118885,
#118886,#118887,#118888,#118889,#118890,#118891,#118892,#118893,#118894,
#118895,#118896,#118897,#118898,#118899,#118900,#118901,#118902,#118903,
#118904,#118905,#118906,#118907,#118908,#118909,#118910,#118911,#118912,
#118913,#118914,#118915,#118916,#118917,#118918,#118919,#118920,#118921,
#118922,#118923,#118924,#118925,#118926,#118927,#118928,#118929,#118930,
#118931,#118932,#118933,#118934,#118935,#118936,#118937,#118938,#118939,
#118940,#118941,#118942,#118943,#118944,#118945,#118946,#118947,#118948,
#118949,#118950,#118951,#118952,#118953,#118954,#118955,#118956,#118957,
#118958,#118959,#118960,#118961,#118962,#118963,#118964,#118965,#118966,
#118967,#118968,#118969,#118970,#118971,#118972,#118973,#118974,#118975,
#118976,#118977,#118978,#118979,#118980,#118981,#118982,#118983,#118984,
#118985,#118986,#118987,#118988,#118989,#118990,#118991,#118992,#118993,
#118994,#118995,#118996,#118997,#118998,#118999,#119000,#119001,#119002,
#119003,#119004,#119005,#119006,#119007,#119008,#119009,#119010,#119011,
#119012,#119013,#119014,#119015,#119016,#119017,#119018,#119019,#119020,
#119021,#119022,#119023,#119024,#119025,#119026,#119027,#119028,#119029,
#119030,#119031,#119032,#119033,#119034,#119035,#119036,#119037,#119038,
#119039,#119040,#119041,#119042,#119043,#119044,#119045,#119046,#119047,
#119048,#119049,#119050,#119051,#119052,#119053,#119054,#119055,#119056,
#119057,#119058,#119059,#119060,#119061,#119062,#119063,#119064,#119065,
#119066,#119067,#119068,#119069,#119070,#119071,#119072,#119073,#119074,
#119075,#119076,#119077,#119078,#119079,#119080,#119081,#119082,#119083,
#119084,#119085,#119086,#119087,#119088,#119089,#119090,#119091,#119092,
#119093,#119094,#119095,#119096,#119097,#119098,#119099,#119100,#119101,
#119102,#119103,#119104,#119105,#119106,#119107,#119108,#119109,#119110,
#119111,#119112,#119113,#119114,#119115,#119116,#119117,#119118,#119119,
#119120,#119121,#119122,#119123,#119124,#119125,#119126,#119127,#119128,
#119129,#119130,#119131,#119132,#119133,#119134,#119135,#119136,#119137,
#119138,#119139,#119140,#119141,#119142,#119143,#119144,#119145,#119146,
#119147,#119148,#119149,#119150,#119151,#119152,#119153,#119154,#119155,
#119156,#119157,#119158,#119159,#119160,#119161,#119162,#119163,#119164,
#119165,#119166,#119167,#119168,#119169,#119170,#119171,#119172,#119173,
#119174,#119175,#119176,#119177,#119178,#119179,#119180,#119181,#119182,
#119183,#119184,#119185,#119186,#119187,#119188,#119189,#119190,#119191,
#119192,#119193,#119194,#119195,#119196,#119197,#119198,#119199,#119200,
#119201,#119202,#119203,#119204,#119205,#119206,#119207,#119208,#119209,
#119210,#119211,#119212,#119213,#119214,#119215,#119216,#119217,#119218,
#119219,#119220,#119221,#119222,#119223,#119224,#119225,#119226,#119227,
#119228,#119229,#119230,#119231,#119232,#119233,#119234,#119235,#119236,
#119237,#119238,#119239,#119240,#119241,#119242,#119243,#119244,#119245,
#119246,#119247,#119248,#119249,#119250,#119251,#119252,#119253,#119254,
#119255,#119256,#119257,#119258,#119259,#119260,#119261,#119262,#119263,
#119264,#119265,#119266,#119267,#119268,#119269,#119270,#119271,#119272,
#119273,#119274,#119275,#119276,#119277,#119278,#119279,#119280,#119281,
#119282,#119283,#119284,#119285,#119286,#119287,#119288,#119289,#119290,
#119291,#119292,#119293,#119294,#119295,#119296,#119297,#119298,#119299,
#119300,#119301,#119302,#119303,#119304,#119305,#119306,#119307,#119308,
#119309,#119310,#119311,#119312,#119313,#119314,#119315,#119316,#119317,
#119318,#119319,#119320,#119321,#119322,#119323,#119324,#119325,#119326,
#119327,#119328,#119329,#119330,#119331,#119332,#119333,#119334,#119335,
#119336,#119337,#119338,#119339,#119340,#119341,#119342,#119343,#119344,
#119345,#119346,#119347,#119348,#119349,#119350,#119351,#119352,#119353,
#119354,#119355,#119356,#119357,#119358,#119359,#119360,#119361,#119362,
#119363,#119364,#119365,#119366,#119367,#119368,#119369,#119370,#119371,
#119372,#119373,#119374,#119375,#119376,#119377,#119378,#119379,#119380,
#119381,#119382,#119383,#119384,#119385,#119386,#119387,#119388,#119389,
#119390,#119391,#119392,#119393,#119394,#119395,#119396,#119397,#119398,
#119399,#119400,#119401,#119402,#119403,#119404,#119405,#119406,#119407,
#119408,#119409,#119410,#119411,#119412,#119413,#119414,#119415,#119416,
#119417,#119418,#119419,#119420,#119421,#119422,#119423,#119424,#119425,
#119426,#119427,#119428,#119429,#119430,#119431,#119432,#119433,#119434,
#119435,#119436,#119437,#119438,#119439,#119440,#119441,#119442,#119443,
#119444,#119445,#119446,#119447,#119448,#119449,#119450,#119451,#119452,
#119453,#119454,#119455,#119456,#119457,#119458,#119459,#119460,#119461,
#119462,#119463,#119464,#119465,#119466,#119467,#119468,#119469,#119470,
#119471,#119472,#119473,#119474,#119475,#119476,#119477,#119478,#119479,
#119480,#119481,#119482,#119483,#119484,#119485,#119486,#119487,#119488,
#119489,#119490,#119491,#119492,#119493,#119494,#119495,#119496,#119497,
#119498,#119499,#119500,#119501,#119502,#119503,#119504,#119505,#119506,
#119507,#119508,#119509,#119510,#119511,#119512,#119513,#119514,#119515,
#119516,#119517,#119518,#119519,#119520,#119521,#119522,#119523,#119524,
#119525,#119526,#119527,#119528,#119529,#119530,#119531,#119532,#119533,
#119534,#119535,#119536,#119537,#119538,#119539,#119540,#119541,#119542,
#119543,#119544,#119545,#119546,#119547,#119548,#119549,#119550,#119551,
#119552,#119553,#119554,#119555,#119556,#119557,#119558,#119559,#119560,
#119561,#119562,#119563,#119564,#119565,#119566,#119567,#119568,#119569,
#119570,#119571,#119572,#119573,#119574,#119575,#119576,#119577,#119578,
#119579,#119580,#119581,#119582,#119583,#119584,#119585,#119586,#119587,
#119588,#119589,#119590,#119591,#119592,#119593,#119594,#119595,#119596,
#119597,#119598,#119599,#119600,#119601,#119602,#119603,#119604,#119605,
#119606,#119607,#119608,#119609,#119610,#119611,#119612,#119613,#119614,
#119615,#119616,#119617,#119618,#119619,#119620,#119621,#119622,#119623,
#119624,#119625,#119626,#119627,#119628,#119629,#119630,#119631,#119632,
#119633,#119634,#119635,#119636,#119637,#119638,#119639,#119640,#119641,
#119642,#119643,#119644,#119645,#119646,#119647,#119648,#119649,#119650,
#119651,#119652,#119653,#119654,#119655,#119656,#119657,#119658,#119659,
#119660,#119661,#119662,#119663,#119664,#119665,#119666,#119667,#119668,
#119669,#119670,#119671,#119672,#119673,#119674,#119675,#119676,#119677,
#119678,#119679,#119680,#119681,#119682,#119683,#119684,#119685,#119686,
#119687,#119688,#119689,#119690,#119691,#119692,#119693,#119694,#119695,
#119696,#119697,#119698,#119699,#119700,#119701,#119702,#119703,#119704,
#119705,#119706,#119707,#119708,#119709,#119710,#119711,#119712,#119713,
#119714,#119715,#119716,#119717,#119718,#119719,#119720,#119721,#119722,
#119723,#119724,#119725,#119726,#119727,#119728,#119729,#119730,#119731,
#119732,#119733,#119734,#119735,#119736,#119737,#119738,#119739,#119740,
#119741,#119742,#119743,#119744,#119745,#119746,#119747,#119748,#119749,
#119750,#119751,#119752,#119753,#119754,#119755,#119756,#119757,#119758,
#119759,#119760,#119761,#119762,#119763,#119764,#119765,#119766,#119767,
#119768,#119769,#119770,#119771,#119772,#119773,#119774,#119775,#119776,
#119777,#119778,#119779,#119780,#119781,#119782,#119783,#119784,#119785,
#119786,#119787,#119788,#119789,#119790,#119791,#119792,#119793,#119794,
#119795,#119796,#119797,#119798,#119799,#119800,#119801,#119802,#119803,
#119804,#119805,#119806,#119807,#119808,#119809,#119810,#119811,#119812,
#119813,#119814,#119815,#119816,#119817,#119818,#119819,#119820,#119821,
#119822,#119823,#119824,#119825,#119826,#119827,#119828,#119829,#119830,
#119831,#119832,#119833,#119834,#119835,#119836,#119837,#119838,#119839,
#119840,#119841,#119842,#119843,#119844,#119845,#119846,#119847,#119848,
#119849,#119850,#119851,#119852,#119853,#119854,#119855,#119856,#119857,
#119858,#119859,#119860,#119861,#119862,#119863,#119864,#119865,#119866,
#119867,#119868,#119869,#119870,#119871,#119872,#119873,#119874,#119875,
#119876,#119877,#119878,#119879,#119880,#119881,#119882,#119883,#119884,
#119885,#119886,#119887,#119888,#119889,#119890,#119891,#119892,#119893,
#119894,#119895,#119896,#119897,#119898,#119899,#119900,#119901,#119902,
#119903,#119904,#119905,#119906,#119907,#119908,#119909,#119910,#119911,
#119912,#119913,#119914,#119915,#119916,#119917,#119918,#119919,#119920,
#119921,#119922,#119923,#119924,#119925,#119926,#119927,#119928,#119929,
#119930,#119931,#119932,#119933,#119934,#119935,#119936,#119937,#119938,
#119939,#119940,#119941,#119942,#119943,#119944,#119945,#119946,#119947,
#119948,#119949,#119950,#119951,#119952,#119953,#119954,#119955,#119956,
#119957,#119958,#119959,#119960,#119961,#119962,#119963,#119964,#119965,
#119966,#119967,#119968,#119969,#119970,#119971,#119972,#119973,#119974,
#119975,#119976,#119977,#119978,#119979,#119980,#119981,#119982,#119983,
#119984,#119985,#119986,#119987,#119988,#119989,#119990,#119991,#119992,
#119993,#119994,#119995,#119996,#119997,#119998,#119999,#120000,#120001,
#120002,#120003,#120004,#120005,#120006,#120007,#120008,#120009,#120010,
#120011,#120012,#120013,#120014,#120015,#120016,#120017,#120018,#120019,
#120020,#120021,#120022,#120023,#120024,#120025,#120026,#120027,#120028,
#120029,#120030,#120031,#120032,#120033,#120034,#120035,#120036,#120037,
#120038,#120039,#120040,#120041,#120042,#120043,#120044,#120045,#120046,
#120047,#120048,#120049,#120050,#120051,#120052,#120053,#120054,#120055,
#120056,#120057,#120058,#120059,#120060,#120061,#120062,#120063,#120064,
#120065,#120066,#120067,#120068,#120069,#120070,#120071,#120072,#120073,
#120074,#120075,#120076,#120077,#120078,#120079,#120080,#120081,#120082,
#120083,#120084,#120085,#120086,#120087,#120088,#120089,#120090,#120091,
#120092,#120093,#120094,#120095,#120096,#120097,#120098,#120099,#120100,
#120101,#120102,#120103,#120104,#120105,#120106,#120107,#120108,#120109,
#120110,#120111,#120112,#120113,#120114,#120115,#120116,#120117,#120118,
#120119,#120120,#120121,#120122,#120123,#120124,#120125,#120126,#120127,
#120128,#120129,#120130,#120131,#120132,#120133,#120134,#120135,#120136,
#120137,#120138,#120139,#120140,#120141,#120142,#120143,#120144,#120145,
#120146,#120147,#120148,#120149,#120150,#120151,#120152,#120153,#120154,
#120155,#120156,#120157,#120158,#120159,#120160,#120161,#120162,#120163,
#120164,#120165,#120166,#120167,#120168,#120169,#120170,#120171,#120172,
#120173,#120174,#120175,#120176,#120177,#120178,#120179,#120180,#120181,
#120182,#120183,#120184,#120185,#120186,#120187,#120188,#120189,#120190,
#120191,#120192,#120193,#120194,#120195,#120196,#120197,#120198,#120199,
#120200,#120201,#120202,#120203,#120204,#120205,#120206,#120207,#120208,
#120209,#120210,#120211,#120212,#120213,#120214,#120215,#120216,#120217,
#120218,#120219,#120220,#120221,#120222,#120223,#120224,#120225,#120226,
#120227,#120228,#120229,#120230,#120231,#120232,#120233,#120234,#120235,
#120236,#120237,#120238,#120239,#120240,#120241,#120242,#120243,#120244,
#120245,#120246,#120247,#120248,#120249,#120250,#120251,#120252,#120253,
#120254,#120255,#120256,#120257,#120258,#120259,#120260,#120261,#120262,
#120263,#120264,#120265,#120266,#120267,#120268,#120269,#120270,#120271,
#120272,#120273,#120274,#120275,#120276,#120277,#120278,#120279,#120280,
#120281,#120282,#120283,#120284,#120285,#120286,#120287,#120288,#120289,
#120290,#120291,#120292,#120293,#120294,#120295,#120296,#120297,#120298,
#120299,#120300,#120301,#120302,#120303,#120304,#120305,#120306,#120307,
#120308,#120309,#120310,#120311,#120312,#120313,#120314,#120315,#120316,
#120317,#120318,#120319,#120320,#120321,#120322,#120323,#120324,#120325,
#120326,#120327,#120328,#120329,#120330,#120331,#120332,#120333,#120334,
#120335,#120336,#120337,#120338,#120339,#120340,#120341,#120342,#120343,
#120344,#120345,#120346,#120347,#120348,#120349,#120350,#120351,#120352,
#120353,#120354,#120355,#120356,#120357,#120358,#120359,#120360,#120361,
#120362,#120363,#120364,#120365,#120366,#120367,#120368,#120369,#120370,
#120371,#120372,#120373,#120374,#120375,#120376,#120377,#120378,#120379,
#120380,#120381,#120382,#120383,#120384,#120385,#120386,#120387,#120388,
#120389,#120390,#120391,#120392,#120393,#120394,#120395,#120396,#120397,
#120398,#120399,#120400,#120401,#120402,#120403,#120404,#120405,#120406,
#120407,#120408,#120409,#120410,#120411,#120412,#120413,#120414,#120415,
#120416,#120417,#120418,#120419,#120420,#120421,#120422,#120423,#120424,
#120425,#120426,#120427,#120428,#120429,#120430,#120431,#120432,#120433,
#120434,#120435,#120436,#120437,#120438,#120439,#120440,#120441,#120442,
#120443,#120444,#120445,#120446,#120447,#120448,#120449,#120450,#120451,
#120452,#120453,#120454,#120455,#120456,#120457,#120458,#120459,#120460,
#120461,#120462,#120463,#120464,#120465,#120466,#120467,#120468,#120469,
#120470,#120471,#120472,#120473,#120474,#120475,#120476,#120477,#120478,
#120479,#120480,#120481,#120482,#120483,#120484,#120485,#120486,#120487,
#120488,#120489,#120490,#120491,#120492,#120493,#120494,#120495,#120496,
#120497,#120498,#120499,#120500,#120501,#120502,#120503,#120504,#120505,
#120506,#120507,#120508,#120509,#120510,#120511,#120512,#120513,#120514,
#120515,#120516,#120517,#120518,#120519,#120520,#120521,#120522,#120523,
#120524,#120525,#120526,#120527,#120528,#120529,#120530,#120531,#120532),
(#120533,#120534,#120535,#120536,#120537,#120538,#120539,#120540,#120541,
#120542,#120543,#120544,#120545,#120546,#120547,#120548,#120549,#120550,
#120551,#120552,#120553,#120554,#120555,#120556,#120557,#120558,#120559,
#120560,#120561,#120562,#120563,#120564,#120565,#120566,#120567,#120568,
#120569,#120570,#120571,#120572,#120573,#120574,#120575,#120576,#120577,
#120578,#120579,#120580,#120581,#120582,#120583,#120584,#120585,#120586,
#120587,#120588,#120589,#120590,#120591,#120592,#120593,#120594,#120595,
#120596,#120597,#120598,#120599,#120600,#120601,#120602,#120603,#120604,
#120605,#120606,#120607,#120608,#120609,#120610,#120611,#120612,#120613,
#120614,#120615,#120616,#120617,#120618,#120619,#120620,#120621,#120622,
#120623,#120624,#120625,#120626,#120627,#120628,#120629,#120630,#120631,
#120632,#120633,#120634,#120635,#120636,#120637,#120638,#120639,#120640,
#120641,#120642,#120643,#120644,#120645,#120646,#120647,#120648,#120649,
#120650,#120651,#120652,#120653,#120654,#120655,#120656,#120657,#120658,
#120659,#120660,#120661,#120662,#120663,#120664,#120665,#120666,#120667,
#120668,#120669,#120670,#120671,#120672,#120673,#120674,#120675,#120676,
#120677,#120678,#120679,#120680,#120681,#120682,#120683,#120684,#120685,
#120686,#120687,#120688,#120689,#120690,#120691,#120692,#120693,#120694,
#120695,#120696,#120697,#120698,#120699,#120700,#120701,#120702,#120703,
#120704,#120705,#120706,#120707,#120708,#120709,#120710,#120711,#120712,
#120713,#120714,#120715,#120716,#120717,#120718,#120719,#120720,#120721,
#120722,#120723,#120724,#120725,#120726,#120727,#120728,#120729,#120730,
#120731,#120732,#120733,#120734,#120735,#120736,#120737,#120738,#120739,
#120740,#120741,#120742,#120743,#120744,#120745,#120746,#120747,#120748,
#120749,#120750,#120751,#120752,#120753,#120754,#120755,#120756,#120757,
#120758,#120759,#120760,#120761,#120762,#120763,#120764,#120765,#120766,
#120767,#120768,#120769,#120770,#120771,#120772,#120773,#120774,#120775,
#120776,#120777,#120778,#120779,#120780,#120781,#120782,#120783,#120784,
#120785,#120786,#120787,#120788,#120789,#120790,#120791,#120792,#120793,
#120794,#120795,#120796,#120797,#120798,#120799,#120800,#120801,#120802,
#120803,#120804,#120805,#120806,#120807,#120808,#120809,#120810,#120811,
#120812,#120813,#120814,#120815,#120816,#120817,#120818,#120819,#120820,
#120821,#120822,#120823,#120824,#120825,#120826,#120827,#120828,#120829,
#120830,#120831,#120832,#120833,#120834,#120835,#120836,#120837,#120838,
#120839,#120840,#120841,#120842,#120843,#120844,#120845,#120846,#120847,
#120848,#120849,#120850,#120851,#120852,#120853,#120854,#120855,#120856,
#120857,#120858,#120859,#120860,#120861,#120862,#120863,#120864,#120865,
#120866,#120867,#120868,#120869,#120870,#120871,#120872,#120873,#120874,
#120875,#120876,#120877,#120878,#120879,#120880,#120881,#120882,#120883,
#120884,#120885,#120886,#120887,#120888,#120889,#120890,#120891,#120892,
#120893,#120894,#120895,#120896,#120897,#120898,#120899,#120900,#120901,
#120902,#120903,#120904,#120905,#120906,#120907,#120908,#120909,#120910,
#120911,#120912,#120913,#120914,#120915,#120916,#120917,#120918,#120919,
#120920,#120921,#120922,#120923,#120924,#120925,#120926,#120927,#120928,
#120929,#120930,#120931,#120932,#120933,#120934,#120935,#120936,#120937,
#120938,#120939,#120940,#120941,#120942,#120943,#120944,#120945,#120946,
#120947,#120948,#120949,#120950,#120951,#120952,#120953,#120954,#120955,
#120956,#120957,#120958,#120959,#120960,#120961,#120962,#120963,#120964,
#120965,#120966,#120967,#120968,#120969,#120970,#120971,#120972,#120973,
#120974,#120975,#120976,#120977,#120978,#120979,#120980,#120981,#120982,
#120983,#120984,#120985,#120986,#120987,#120988,#120989,#120990,#120991,
#120992,#120993,#120994,#120995,#120996,#120997,#120998,#120999,#121000,
#121001,#121002,#121003,#121004,#121005,#121006,#121007,#121008,#121009,
#121010,#121011,#121012,#121013,#121014,#121015,#121016,#121017,#121018,
#121019,#121020,#121021,#121022,#121023,#121024,#121025,#121026,#121027,
#121028,#121029,#121030,#121031,#121032,#121033,#121034,#121035,#121036,
#121037,#121038,#121039,#121040,#121041,#121042,#121043,#121044,#121045,
#121046,#121047,#121048,#121049,#121050,#121051,#121052,#121053,#121054,
#121055,#121056,#121057,#121058,#121059,#121060,#121061,#121062,#121063,
#121064,#121065,#121066,#121067,#121068,#121069,#121070,#121071,#121072,
#121073,#121074,#121075,#121076,#121077,#121078,#121079,#121080,#121081,
#121082,#121083,#121084,#121085,#121086,#121087,#121088,#121089,#121090,
#121091,#121092,#121093,#121094,#121095,#121096,#121097,#121098,#121099,
#121100,#121101,#121102,#121103,#121104,#121105,#121106,#121107,#121108,
#121109,#121110,#121111,#121112,#121113,#121114,#121115,#121116,#121117,
#121118,#121119,#121120,#121121,#121122,#121123,#121124,#121125,#121126,
#121127,#121128,#121129,#121130,#121131,#121132,#121133,#121134,#121135,
#121136,#121137,#121138,#121139,#121140,#121141,#121142,#121143,#121144,
#121145,#121146,#121147,#121148,#121149,#121150,#121151,#121152,#121153,
#121154,#121155,#121156,#121157,#121158,#121159,#121160,#121161,#121162,
#121163,#121164,#121165,#121166,#121167,#121168,#121169,#121170,#121171,
#121172,#121173,#121174,#121175,#121176,#121177,#121178,#121179,#121180,
#121181,#121182,#121183,#121184,#121185,#121186,#121187,#121188,#121189,
#121190,#121191,#121192,#121193,#121194,#121195,#121196,#121197,#121198,
#121199,#121200,#121201,#121202,#121203,#121204,#121205,#121206,#121207,
#121208,#121209,#121210,#121211,#121212,#121213,#121214,#121215,#121216,
#121217,#121218,#121219,#121220,#121221,#121222,#121223,#121224,#121225,
#121226,#121227,#121228,#121229,#121230,#121231,#121232,#121233,#121234,
#121235,#121236,#121237,#121238,#121239,#121240,#121241,#121242,#121243,
#121244,#121245,#121246,#121247,#121248,#121249,#121250,#121251,#121252,
#121253,#121254,#121255,#121256,#121257,#121258,#121259,#121260,#121261,
#121262,#121263,#121264,#121265,#121266,#121267,#121268,#121269,#121270,
#121271,#121272,#121273,#121274,#121275,#121276,#121277,#121278,#121279,
#121280,#121281,#121282,#121283,#121284,#121285,#121286,#121287,#121288,
#121289,#121290,#121291,#121292,#121293,#121294,#121295,#121296,#121297,
#121298,#121299,#121300,#121301,#121302,#121303,#121304,#121305,#121306,
#121307,#121308,#121309,#121310,#121311,#121312,#121313,#121314,#121315,
#121316,#121317,#121318,#121319,#121320,#121321,#121322,#121323,#121324,
#121325,#121326,#121327,#121328,#121329,#121330,#121331,#121332,#121333,
#121334,#121335,#121336,#121337,#121338,#121339,#121340,#121341,#121342,
#121343,#121344,#121345,#121346,#121347,#121348,#121349,#121350,#121351,
#121352,#121353,#121354,#121355,#121356,#121357,#121358,#121359,#121360,
#121361,#121362,#121363,#121364,#121365,#121366,#121367,#121368,#121369,
#121370,#121371,#121372,#121373,#121374,#121375,#121376,#121377,#121378,
#121379,#121380,#121381,#121382,#121383,#121384,#121385,#121386,#121387,
#121388,#121389,#121390,#121391,#121392,#121393,#121394,#121395,#121396,
#121397,#121398,#121399,#121400,#121401,#121402,#121403,#121404,#121405,
#121406,#121407,#121408,#121409,#121410,#121411,#121412,#121413,#121414,
#121415,#121416,#121417,#121418,#121419,#121420,#121421,#121422,#121423,
#121424,#121425,#121426,#121427,#121428,#121429,#121430,#121431,#121432,
#121433,#121434,#121435,#121436,#121437,#121438,#121439,#121440,#121441,
#121442,#121443,#121444,#121445,#121446,#121447,#121448,#121449,#121450,
#121451,#121452,#121453,#121454,#121455,#121456,#121457,#121458,#121459,
#121460,#121461,#121462,#121463,#121464,#121465,#121466,#121467,#121468,
#121469,#121470,#121471,#121472,#121473,#121474,#121475,#121476,#121477,
#121478,#121479,#121480,#121481,#121482,#121483,#121484,#121485,#121486,
#121487,#121488,#121489,#121490,#121491,#121492,#121493,#121494,#121495,
#121496,#121497,#121498,#121499,#121500,#121501,#121502,#121503,#121504,
#121505,#121506,#121507,#121508,#121509,#121510,#121511,#121512,#121513,
#121514,#121515,#121516,#121517,#121518,#121519,#121520,#121521,#121522,
#121523,#121524,#121525,#121526,#121527,#121528,#121529,#121530,#121531,
#121532,#121533,#121534,#121535,#121536,#121537,#121538,#121539,#121540,
#121541,#121542,#121543,#121544,#121545,#121546,#121547,#121548,#121549,
#121550,#121551,#121552,#121553,#121554,#121555,#121556,#121557,#121558,
#121559,#121560,#121561,#121562,#121563,#121564,#121565,#121566,#121567,
#121568,#121569,#121570,#121571,#121572,#121573,#121574,#121575,#121576,
#121577,#121578,#121579,#121580,#121581,#121582,#121583,#121584,#121585,
#121586,#121587,#121588,#121589,#121590,#121591,#121592,#121593,#121594,
#121595,#121596,#121597,#121598,#121599,#121600,#121601,#121602,#121603,
#121604,#121605,#121606,#121607,#121608,#121609,#121610,#121611,#121612,
#121613,#121614,#121615,#121616,#121617,#121618,#121619,#121620,#121621,
#121622,#121623,#121624,#121625,#121626,#121627,#121628,#121629,#121630,
#121631,#121632,#121633,#121634,#121635,#121636,#121637,#121638,#121639,
#121640,#121641,#121642,#121643,#121644,#121645,#121646,#121647,#121648,
#121649,#121650,#121651,#121652,#121653,#121654,#121655,#121656,#121657,
#121658,#121659,#121660,#121661,#121662,#121663,#121664,#121665,#121666,
#121667,#121668,#121669,#121670,#121671,#121672,#121673,#121674,#121675,
#121676,#121677,#121678,#121679,#121680,#121681,#121682,#121683,#121684,
#121685,#121686,#121687,#121688,#121689,#121690,#121691,#121692,#121693,
#121694,#121695,#121696,#121697,#121698,#121699,#121700,#121701,#121702,
#121703,#121704,#121705,#121706,#121707,#121708,#121709,#121710,#121711,
#121712,#121713,#121714,#121715,#121716,#121717,#121718,#121719,#121720,
#121721,#121722,#121723,#121724,#121725,#121726,#121727,#121728,#121729,
#121730,#121731,#121732,#121733,#121734,#121735,#121736,#121737,#121738,
#121739,#121740,#121741,#121742,#121743,#121744,#121745,#121746,#121747,
#121748,#121749,#121750,#121751,#121752,#121753,#121754,#121755,#121756,
#121757,#121758,#121759,#121760,#121761,#121762,#121763,#121764,#121765,
#121766,#121767,#121768,#121769,#121770,#121771,#121772,#121773,#121774,
#121775,#121776,#121777,#121778,#121779,#121780,#121781,#121782,#121783,
#121784,#121785,#121786,#121787,#121788,#121789,#121790,#121791,#121792,
#121793,#121794,#121795,#121796,#121797,#121798,#121799,#121800,#121801,
#121802,#121803,#121804,#121805,#121806,#121807,#121808,#121809,#121810,
#121811,#121812,#121813,#121814,#121815,#121816,#121817,#121818,#121819,
#121820,#121821,#121822,#121823,#121824,#121825,#121826,#121827,#121828,
#121829,#121830,#121831,#121832,#121833,#121834,#121835,#121836,#121837,
#121838,#121839,#121840,#121841,#121842,#121843,#121844,#121845,#121846,
#121847,#121848,#121849,#121850,#121851,#121852,#121853,#121854,#121855,
#121856,#121857,#121858,#121859,#121860,#121861,#121862,#121863,#121864,
#121865,#121866,#121867,#121868,#121869,#121870,#121871,#121872,#121873,
#121874,#121875,#121876,#121877,#121878,#121879,#121880,#121881,#121882,
#121883,#121884,#121885,#121886,#121887,#121888,#121889,#121890,#121891,
#121892,#121893,#121894,#121895,#121896,#121897,#121898,#121899,#121900,
#121901,#121902,#121903,#121904,#121905,#121906,#121907,#121908,#121909,
#121910,#121911,#121912,#121913,#121914,#121915,#121916,#121917,#121918,
#121919,#121920,#121921,#121922,#121923,#121924,#121925,#121926,#121927,
#121928,#121929,#121930,#121931,#121932,#121933,#121934,#121935,#121936,
#121937,#121938,#121939,#121940,#121941,#121942,#121943,#121944,#121945,
#121946,#121947,#121948,#121949,#121950,#121951,#121952,#121953,#121954,
#121955,#121956,#121957,#121958,#121959,#121960,#121961,#121962,#121963,
#121964,#121965,#121966,#121967,#121968,#121969,#121970,#121971,#121972,
#121973,#121974,#121975,#121976,#121977,#121978,#121979,#121980,#121981,
#121982,#121983,#121984,#121985,#121986,#121987,#121988,#121989,#121990,
#121991,#121992,#121993,#121994,#121995,#121996,#121997,#121998,#121999,
#122000,#122001,#122002,#122003,#122004,#122005,#122006,#122007,#122008,
#122009,#122010,#122011,#122012,#122013,#122014,#122015,#122016,#122017,
#122018,#122019,#122020,#122021,#122022,#122023,#122024,#122025,#122026,
#122027,#122028,#122029,#122030,#122031,#122032,#122033,#122034,#122035,
#122036,#122037,#122038,#122039,#122040,#122041,#122042,#122043,#122044,
#122045,#122046,#122047,#122048,#122049,#122050,#122051,#122052,#122053,
#122054,#122055,#122056,#122057,#122058,#122059,#122060,#122061,#122062,
#122063,#122064,#122065,#122066,#122067,#122068,#122069,#122070,#122071,
#122072,#122073,#122074,#122075,#122076,#122077,#122078,#122079,#122080,
#122081,#122082,#122083,#122084,#122085,#122086,#122087,#122088,#122089,
#122090,#122091,#122092,#122093,#122094,#122095,#122096,#122097,#122098,
#122099,#122100,#122101,#122102,#122103,#122104,#122105,#122106,#122107,
#122108,#122109,#122110,#122111,#122112,#122113,#122114,#122115,#122116,
#122117,#122118,#122119,#122120,#122121,#122122,#122123,#122124,#122125,
#122126,#122127,#122128,#122129,#122130,#122131,#122132,#122133,#122134,
#122135,#122136,#122137,#122138,#122139,#122140,#122141,#122142,#122143,
#122144,#122145,#122146,#122147,#122148,#122149,#122150,#122151,#122152,
#122153,#122154,#122155,#122156,#122157,#122158,#122159,#122160,#122161,
#122162,#122163,#122164,#122165,#122166,#122167,#122168,#122169,#122170,
#122171,#122172,#122173,#122174,#122175,#122176,#122177,#122178,#122179,
#122180,#122181,#122182,#122183,#122184,#122185,#122186,#122187,#122188,
#122189,#122190,#122191,#122192,#122193,#122194,#122195,#122196,#122197,
#122198,#122199,#122200,#122201,#122202,#122203,#122204,#122205,#122206,
#122207,#122208,#122209,#122210,#122211,#122212,#122213,#122214,#122215,
#122216,#122217,#122218,#122219,#122220,#122221,#122222,#122223,#122224,
#122225,#122226,#122227,#122228,#122229,#122230,#122231,#122232,#122233,
#122234,#122235,#122236,#122237,#122238,#122239,#122240,#122241,#122242,
#122243,#122244,#122245,#122246,#122247,#122248,#122249,#122250,#122251,
#122252,#122253,#122254,#122255,#122256,#122257,#122258,#122259,#122260,
#122261,#122262,#122263,#122264,#122265,#122266,#122267,#122268,#122269,
#122270,#122271,#122272,#122273,#122274,#122275,#122276,#122277,#122278,
#122279,#122280,#122281,#122282,#122283,#122284,#122285,#122286,#122287,
#122288,#122289,#122290,#122291,#122292,#122293,#122294,#122295,#122296,
#122297,#122298,#122299,#122300,#122301,#122302,#122303,#122304,#122305,
#122306,#122307,#122308,#122309,#122310,#122311,#122312,#122313,#122314,
#122315,#122316,#122317,#122318,#122319,#122320,#122321,#122322,#122323,
#122324,#122325,#122326,#122327,#122328,#122329,#122330,#122331,#122332,
#122333,#122334,#122335,#122336,#122337,#122338,#122339,#122340,#122341,
#122342,#122343,#122344,#122345,#122346,#122347,#122348,#122349,#122350,
#122351,#122352,#122353,#122354,#122355,#122356,#122357,#122358,#122359,
#122360,#122361,#122362,#122363,#122364,#122365,#122366,#122367,#122368,
#122369,#122370,#122371,#122372,#122373,#122374,#122375,#122376,#122377,
#122378,#122379,#122380,#122381,#122382,#122383,#122384,#122385,#122386,
#122387,#122388,#122389,#122390,#122391,#122392,#122393,#122394,#122395,
#122396,#122397,#122398,#122399,#122400,#122401,#122402,#122403,#122404,
#122405,#122406,#122407,#122408,#122409,#122410,#122411,#122412,#122413,
#122414,#122415,#122416,#122417,#122418,#122419,#122420,#122421,#122422,
#122423,#122424,#122425,#122426,#122427,#122428,#122429,#122430,#122431,
#122432,#122433,#122434,#122435,#122436,#122437,#122438,#122439,#122440,
#122441,#122442,#122443,#122444,#122445,#122446,#122447,#122448,#122449,
#122450,#122451,#122452,#122453,#122454,#122455,#122456,#122457,#122458,
#122459,#122460,#122461,#122462,#122463,#122464,#122465,#122466,#122467,
#122468,#122469,#122470,#122471,#122472,#122473,#122474,#122475,#122476,
#122477,#122478,#122479,#122480,#122481,#122482,#122483,#122484,#122485,
#122486,#122487,#122488,#122489,#122490,#122491,#122492,#122493,#122494,
#122495,#122496,#122497,#122498,#122499,#122500,#122501,#122502,#122503,
#122504,#122505,#122506,#122507,#122508,#122509,#122510,#122511,#122512,
#122513,#122514,#122515,#122516,#122517,#122518,#122519,#122520,#122521,
#122522,#122523,#122524,#122525,#122526,#122527,#122528,#122529,#122530,
#122531,#122532,#122533,#122534,#122535,#122536,#122537,#122538,#122539,
#122540,#122541,#122542,#122543,#122544,#122545,#122546,#122547,#122548,
#122549,#122550,#122551,#122552,#122553,#122554,#122555,#122556,#122557,
#122558,#122559,#122560,#122561,#122562,#122563,#122564,#122565,#122566,
#122567,#122568,#122569,#122570,#122571,#122572,#122573,#122574,#122575,
#122576,#122577,#122578,#122579,#122580,#122581,#122582,#122583),(#122584,
#122585,#122586,#122587,#122588,#122589,#122590,#122591,#122592,#122593,
#122594,#122595,#122596,#122597,#122598,#122599,#122600,#122601,#122602,
#122603,#122604,#122605,#122606,#122607,#122608,#122609,#122610,#122611,
#122612,#122613,#122614,#122615,#122616,#122617,#122618,#122619,#122620,
#122621,#122622,#122623,#122624,#122625,#122626,#122627,#122628,#122629,
#122630,#122631,#122632,#122633,#122634,#122635,#122636,#122637,#122638,
#122639,#122640,#122641,#122642,#122643,#122644,#122645,#122646,#122647,
#122648,#122649,#122650,#122651,#122652,#122653,#122654,#122655,#122656,
#122657,#122658,#122659,#122660,#122661,#122662,#122663,#122664,#122665,
#122666,#122667,#122668,#122669,#122670,#122671,#122672,#122673,#122674,
#122675,#122676,#122677,#122678,#122679,#122680,#122681,#122682,#122683,
#122684,#122685,#122686,#122687,#122688,#122689,#122690,#122691,#122692,
#122693,#122694,#122695,#122696,#122697,#122698,#122699,#122700,#122701,
#122702,#122703,#122704,#122705,#122706,#122707,#122708,#122709,#122710,
#122711,#122712,#122713,#122714,#122715,#122716,#122717,#122718,#122719,
#122720,#122721,#122722,#122723,#122724,#122725,#122726,#122727,#122728,
#122729,#122730,#122731,#122732,#122733,#122734,#122735,#122736,#122737,
#122738,#122739,#122740,#122741,#122742,#122743,#122744,#122745,#122746,
#122747,#122748,#122749,#122750,#122751,#122752,#122753,#122754,#122755,
#122756,#122757,#122758,#122759,#122760,#122761,#122762,#122763,#122764,
#122765,#122766,#122767,#122768,#122769,#122770,#122771,#122772,#122773,
#122774,#122775,#122776,#122777,#122778,#122779,#122780,#122781,#122782,
#122783,#122784,#122785,#122786,#122787,#122788,#122789,#122790,#122791,
#122792,#122793,#122794,#122795,#122796,#122797,#122798,#122799,#122800,
#122801,#122802,#122803,#122804,#122805,#122806,#122807,#122808,#122809,
#122810,#122811,#122812,#122813,#122814,#122815,#122816,#122817,#122818,
#122819,#122820,#122821,#122822,#122823,#122824,#122825,#122826,#122827,
#122828,#122829,#122830,#122831,#122832,#122833,#122834,#122835,#122836,
#122837,#122838,#122839,#122840,#122841,#122842,#122843,#122844,#122845,
#122846,#122847,#122848,#122849,#122850,#122851,#122852,#122853,#122854,
#122855,#122856,#122857,#122858,#122859,#122860,#122861,#122862,#122863,
#122864,#122865,#122866,#122867,#122868,#122869,#122870,#122871,#122872,
#122873,#122874,#122875,#122876,#122877,#122878,#122879,#122880,#122881,
#122882,#122883,#122884,#122885,#122886,#122887,#122888,#122889,#122890,
#122891,#122892,#122893,#122894,#122895,#122896,#122897,#122898,#122899,
#122900,#122901,#122902,#122903,#122904,#122905,#122906,#122907,#122908,
#122909,#122910,#122911,#122912,#122913,#122914,#122915,#122916,#122917,
#122918,#122919,#122920,#122921,#122922,#122923,#122924,#122925,#122926,
#122927,#122928,#122929,#122930,#122931,#122932,#122933,#122934,#122935,
#122936,#122937,#122938,#122939,#122940,#122941,#122942,#122943,#122944,
#122945,#122946,#122947,#122948,#122949,#122950,#122951,#122952,#122953,
#122954,#122955,#122956,#122957,#122958,#122959,#122960,#122961,#122962,
#122963,#122964,#122965,#122966,#122967,#122968,#122969,#122970,#122971,
#122972,#122973,#122974,#122975,#122976,#122977,#122978,#122979,#122980,
#122981,#122982,#122983,#122984,#122985,#122986,#122987,#122988,#122989,
#122990,#122991,#122992,#122993,#122994,#122995,#122996,#122997,#122998,
#122999,#123000,#123001,#123002,#123003,#123004,#123005,#123006,#123007,
#123008,#123009,#123010,#123011,#123012,#123013,#123014,#123015,#123016,
#123017,#123018,#123019,#123020,#123021,#123022,#123023,#123024,#123025,
#123026,#123027,#123028,#123029,#123030,#123031,#123032,#123033,#123034,
#123035,#123036,#123037,#123038,#123039,#123040,#123041,#123042,#123043,
#123044,#123045,#123046,#123047,#123048,#123049,#123050,#123051,#123052,
#123053,#123054,#123055,#123056,#123057,#123058,#123059,#123060,#123061,
#123062,#123063,#123064,#123065,#123066,#123067,#123068,#123069,#123070,
#123071,#123072,#123073,#123074,#123075,#123076,#123077,#123078,#123079,
#123080,#123081,#123082,#123083,#123084,#123085,#123086,#123087,#123088,
#123089,#123090,#123091,#123092,#123093,#123094,#123095,#123096,#123097,
#123098,#123099,#123100,#123101,#123102,#123103,#123104,#123105,#123106,
#123107,#123108,#123109,#123110,#123111,#123112,#123113,#123114,#123115,
#123116,#123117,#123118,#123119,#123120,#123121,#123122,#123123,#123124,
#123125,#123126,#123127,#123128,#123129,#123130,#123131,#123132,#123133,
#123134,#123135,#123136,#123137,#123138,#123139,#123140,#123141,#123142,
#123143,#123144,#123145,#123146,#123147,#123148,#123149,#123150,#123151,
#123152,#123153,#123154,#123155,#123156,#123157,#123158,#123159,#123160,
#123161,#123162,#123163,#123164,#123165,#123166,#123167,#123168,#123169,
#123170,#123171,#123172,#123173,#123174,#123175,#123176,#123177,#123178,
#123179,#123180,#123181,#123182,#123183,#123184,#123185,#123186,#123187,
#123188,#123189,#123190,#123191,#123192,#123193,#123194,#123195,#123196,
#123197,#123198,#123199,#123200,#123201,#123202,#123203,#123204,#123205,
#123206,#123207,#123208,#123209,#123210,#123211,#123212,#123213,#123214,
#123215,#123216,#123217,#123218,#123219,#123220,#123221,#123222,#123223,
#123224,#123225,#123226,#123227,#123228,#123229,#123230,#123231,#123232,
#123233,#123234,#123235,#123236,#123237,#123238,#123239,#123240,#123241,
#123242,#123243,#123244,#123245,#123246,#123247,#123248,#123249,#123250,
#123251,#123252,#123253,#123254,#123255,#123256,#123257,#123258,#123259,
#123260,#123261,#123262,#123263,#123264,#123265,#123266,#123267,#123268,
#123269,#123270,#123271,#123272,#123273,#123274,#123275,#123276,#123277,
#123278,#123279,#123280,#123281,#123282,#123283,#123284,#123285,#123286,
#123287,#123288,#123289,#123290,#123291,#123292,#123293,#123294,#123295,
#123296,#123297,#123298,#123299,#123300,#123301,#123302,#123303,#123304,
#123305,#123306,#123307,#123308,#123309,#123310,#123311,#123312,#123313,
#123314,#123315,#123316,#123317,#123318,#123319,#123320,#123321,#123322,
#123323,#123324,#123325,#123326,#123327,#123328,#123329,#123330,#123331,
#123332,#123333,#123334,#123335,#123336,#123337,#123338,#123339,#123340,
#123341,#123342,#123343,#123344,#123345,#123346,#123347,#123348,#123349,
#123350,#123351,#123352,#123353,#123354,#123355,#123356,#123357,#123358,
#123359,#123360,#123361,#123362,#123363,#123364,#123365,#123366,#123367,
#123368,#123369,#123370,#123371,#123372,#123373,#123374,#123375,#123376,
#123377,#123378,#123379,#123380,#123381,#123382,#123383,#123384,#123385,
#123386,#123387,#123388,#123389,#123390,#123391,#123392,#123393,#123394,
#123395,#123396,#123397,#123398,#123399,#123400,#123401,#123402,#123403,
#123404,#123405,#123406,#123407,#123408,#123409,#123410,#123411,#123412,
#123413,#123414,#123415,#123416,#123417,#123418,#123419,#123420,#123421,
#123422,#123423,#123424,#123425,#123426,#123427,#123428,#123429,#123430,
#123431,#123432,#123433,#123434,#123435,#123436,#123437,#123438,#123439,
#123440,#123441,#123442,#123443,#123444,#123445,#123446,#123447,#123448,
#123449,#123450,#123451,#123452,#123453,#123454,#123455,#123456,#123457,
#123458,#123459,#123460,#123461,#123462,#123463,#123464,#123465,#123466,
#123467,#123468,#123469,#123470,#123471,#123472,#123473,#123474,#123475,
#123476,#123477,#123478,#123479,#123480,#123481,#123482,#123483,#123484,
#123485,#123486,#123487,#123488,#123489,#123490,#123491,#123492,#123493,
#123494,#123495,#123496,#123497,#123498,#123499,#123500,#123501,#123502,
#123503,#123504,#123505,#123506,#123507,#123508,#123509,#123510,#123511,
#123512,#123513,#123514,#123515,#123516,#123517,#123518,#123519,#123520,
#123521,#123522,#123523,#123524,#123525,#123526,#123527,#123528,#123529,
#123530,#123531,#123532,#123533,#123534,#123535,#123536,#123537,#123538,
#123539,#123540,#123541,#123542,#123543,#123544,#123545,#123546,#123547,
#123548,#123549,#123550,#123551,#123552,#123553,#123554,#123555,#123556,
#123557,#123558,#123559,#123560,#123561,#123562,#123563,#123564,#123565,
#123566,#123567,#123568,#123569,#123570,#123571,#123572,#123573,#123574,
#123575,#123576,#123577,#123578,#123579,#123580,#123581,#123582,#123583,
#123584,#123585,#123586,#123587,#123588,#123589,#123590,#123591,#123592,
#123593,#123594,#123595,#123596,#123597,#123598,#123599,#123600,#123601,
#123602,#123603,#123604,#123605,#123606,#123607,#123608,#123609,#123610,
#123611,#123612,#123613,#123614,#123615,#123616,#123617,#123618,#123619,
#123620,#123621,#123622,#123623,#123624,#123625,#123626,#123627,#123628,
#123629,#123630,#123631,#123632,#123633,#123634,#123635,#123636,#123637,
#123638,#123639,#123640,#123641,#123642,#123643,#123644,#123645,#123646,
#123647,#123648,#123649,#123650,#123651,#123652,#123653,#123654,#123655,
#123656,#123657,#123658,#123659,#123660,#123661,#123662,#123663,#123664,
#123665,#123666,#123667,#123668,#123669,#123670,#123671,#123672,#123673,
#123674,#123675,#123676,#123677,#123678,#123679,#123680,#123681,#123682,
#123683,#123684,#123685,#123686,#123687,#123688,#123689,#123690,#123691,
#123692,#123693,#123694,#123695,#123696,#123697,#123698,#123699,#123700,
#123701,#123702,#123703,#123704,#123705,#123706,#123707,#123708,#123709,
#123710,#123711,#123712,#123713,#123714,#123715,#123716,#123717,#123718,
#123719,#123720,#123721,#123722,#123723,#123724,#123725,#123726,#123727,
#123728,#123729,#123730,#123731,#123732,#123733,#123734,#123735,#123736,
#123737,#123738,#123739,#123740,#123741,#123742,#123743,#123744,#123745,
#123746,#123747,#123748,#123749,#123750,#123751,#123752,#123753,#123754,
#123755,#123756,#123757,#123758,#123759,#123760,#123761,#123762,#123763,
#123764,#123765,#123766,#123767,#123768,#123769,#123770,#123771,#123772,
#123773,#123774,#123775,#123776,#123777,#123778,#123779,#123780,#123781,
#123782,#123783,#123784,#123785,#123786,#123787,#123788,#123789,#123790,
#123791,#123792,#123793,#123794,#123795,#123796,#123797,#123798,#123799,
#123800,#123801,#123802,#123803,#123804,#123805,#123806,#123807,#123808,
#123809,#123810,#123811,#123812,#123813,#123814,#123815,#123816,#123817,
#123818,#123819,#123820,#123821,#123822,#123823,#123824,#123825,#123826,
#123827,#123828,#123829,#123830,#123831,#123832,#123833,#123834,#123835,
#123836,#123837,#123838,#123839,#123840,#123841,#123842,#123843,#123844,
#123845,#123846,#123847,#123848,#123849,#123850,#123851,#123852,#123853,
#123854,#123855,#123856,#123857,#123858,#123859,#123860,#123861,#123862,
#123863,#123864,#123865,#123866,#123867,#123868,#123869,#123870,#123871,
#123872,#123873,#123874,#123875,#123876,#123877,#123878,#123879,#123880,
#123881,#123882,#123883,#123884,#123885,#123886,#123887,#123888,#123889,
#123890,#123891,#123892,#123893,#123894,#123895,#123896,#123897,#123898,
#123899,#123900,#123901,#123902,#123903,#123904,#123905,#123906,#123907,
#123908,#123909,#123910,#123911,#123912,#123913,#123914,#123915,#123916,
#123917,#123918,#123919,#123920,#123921,#123922,#123923,#123924,#123925,
#123926,#123927,#123928,#123929,#123930,#123931,#123932,#123933,#123934,
#123935,#123936,#123937,#123938,#123939,#123940,#123941,#123942,#123943,
#123944,#123945,#123946,#123947,#123948,#123949,#123950,#123951,#123952,
#123953,#123954,#123955,#123956,#123957,#123958,#123959,#123960,#123961,
#123962,#123963,#123964,#123965,#123966,#123967,#123968,#123969,#123970,
#123971,#123972,#123973,#123974,#123975,#123976,#123977,#123978,#123979,
#123980,#123981,#123982,#123983,#123984,#123985,#123986,#123987,#123988,
#123989,#123990,#123991,#123992,#123993,#123994,#123995,#123996,#123997,
#123998,#123999,#124000,#124001,#124002,#124003,#124004,#124005,#124006,
#124007,#124008,#124009,#124010,#124011,#124012,#124013,#124014,#124015,
#124016,#124017,#124018,#124019,#124020,#124021,#124022,#124023,#124024,
#124025,#124026,#124027,#124028,#124029,#124030,#124031,#124032,#124033,
#124034,#124035,#124036,#124037,#124038,#124039,#124040,#124041,#124042,
#124043,#124044,#124045,#124046,#124047,#124048,#124049,#124050,#124051,
#124052,#124053,#124054,#124055,#124056,#124057,#124058,#124059,#124060,
#124061,#124062,#124063,#124064,#124065,#124066,#124067,#124068,#124069,
#124070,#124071,#124072,#124073,#124074,#124075,#124076,#124077,#124078,
#124079,#124080,#124081,#124082,#124083,#124084,#124085,#124086,#124087,
#124088,#124089,#124090,#124091,#124092,#124093,#124094,#124095,#124096,
#124097,#124098,#124099,#124100,#124101,#124102,#124103,#124104,#124105,
#124106,#124107,#124108,#124109,#124110,#124111,#124112,#124113,#124114,
#124115,#124116,#124117,#124118,#124119,#124120,#124121,#124122,#124123,
#124124,#124125,#124126,#124127,#124128,#124129,#124130,#124131,#124132,
#124133,#124134,#124135,#124136,#124137,#124138,#124139,#124140,#124141,
#124142,#124143,#124144,#124145,#124146,#124147,#124148,#124149,#124150,
#124151,#124152,#124153,#124154,#124155,#124156,#124157,#124158,#124159,
#124160,#124161,#124162,#124163,#124164,#124165,#124166,#124167,#124168,
#124169,#124170,#124171,#124172,#124173,#124174,#124175,#124176,#124177,
#124178,#124179,#124180,#124181,#124182,#124183,#124184,#124185,#124186,
#124187,#124188,#124189,#124190,#124191,#124192,#124193,#124194,#124195,
#124196,#124197,#124198,#124199,#124200,#124201,#124202,#124203,#124204,
#124205,#124206,#124207,#124208,#124209,#124210,#124211,#124212,#124213,
#124214,#124215,#124216,#124217,#124218,#124219,#124220,#124221,#124222,
#124223,#124224,#124225,#124226,#124227,#124228,#124229,#124230,#124231,
#124232,#124233,#124234,#124235,#124236,#124237,#124238,#124239,#124240,
#124241,#124242,#124243,#124244,#124245,#124246,#124247,#124248,#124249,
#124250,#124251,#124252,#124253,#124254,#124255,#124256,#124257,#124258,
#124259,#124260,#124261,#124262,#124263,#124264,#124265,#124266,#124267,
#124268,#124269,#124270,#124271,#124272,#124273,#124274,#124275,#124276,
#124277,#124278,#124279,#124280,#124281,#124282,#124283,#124284,#124285,
#124286,#124287,#124288,#124289,#124290,#124291,#124292,#124293,#124294,
#124295,#124296,#124297,#124298,#124299,#124300,#124301,#124302,#124303,
#124304,#124305,#124306,#124307,#124308,#124309,#124310,#124311,#124312,
#124313,#124314,#124315,#124316,#124317,#124318,#124319,#124320,#124321,
#124322,#124323,#124324,#124325,#124326,#124327,#124328,#124329,#124330,
#124331,#124332,#124333,#124334,#124335,#124336,#124337,#124338,#124339,
#124340,#124341,#124342,#124343,#124344,#124345,#124346,#124347,#124348,
#124349,#124350,#124351,#124352,#124353,#124354,#124355,#124356,#124357,
#124358,#124359,#124360,#124361,#124362,#124363,#124364,#124365,#124366,
#124367,#124368,#124369,#124370,#124371,#124372,#124373,#124374,#124375,
#124376,#124377,#124378,#124379,#124380,#124381,#124382,#124383,#124384,
#124385,#124386,#124387,#124388,#124389,#124390,#124391,#124392,#124393,
#124394,#124395,#124396,#124397,#124398,#124399,#124400,#124401,#124402,
#124403,#124404,#124405,#124406,#124407,#124408,#124409,#124410,#124411,
#124412,#124413,#124414,#124415,#124416,#124417,#124418,#124419,#124420,
#124421,#124422,#124423,#124424,#124425,#124426,#124427,#124428,#124429,
#124430,#124431,#124432,#124433,#124434,#124435,#124436,#124437,#124438,
#124439,#124440,#124441,#124442,#124443,#124444,#124445,#124446,#124447,
#124448,#124449,#124450,#124451,#124452,#124453,#124454,#124455,#124456,
#124457,#124458,#124459,#124460,#124461,#124462,#124463,#124464,#124465,
#124466,#124467,#124468,#124469,#124470,#124471,#124472,#124473,#124474,
#124475,#124476,#124477,#124478,#124479,#124480,#124481,#124482,#124483,
#124484,#124485,#124486,#124487,#124488,#124489,#124490,#124491,#124492,
#124493,#124494,#124495,#124496,#124497,#124498,#124499,#124500,#124501,
#124502,#124503,#124504,#124505,#124506,#124507,#124508,#124509,#124510,
#124511,#124512,#124513,#124514,#124515,#124516,#124517,#124518,#124519,
#124520,#124521,#124522,#124523,#124524,#124525,#124526,#124527,#124528,
#124529,#124530,#124531,#124532,#124533,#124534,#124535,#124536,#124537,
#124538,#124539,#124540,#124541,#124542,#124543,#124544,#124545,#124546,
#124547,#124548,#124549,#124550,#124551,#124552,#124553,#124554,#124555,
#124556,#124557,#124558,#124559,#124560,#124561,#124562,#124563,#124564,
#124565,#124566,#124567,#124568,#124569,#124570,#124571,#124572,#124573,
#124574,#124575,#124576,#124577,#124578,#124579,#124580,#124581,#124582,
#124583,#124584,#124585,#124586,#124587,#124588,#124589,#124590,#124591,
#124592,#124593,#124594,#124595,#124596,#124597,#124598,#124599,#124600,
#124601,#124602,#124603,#124604,#124605,#124606,#124607,#124608,#124609,
#124610,#124611,#124612,#124613,#124614,#124615,#124616,#124617,#124618,
#124619,#124620,#124621,#124622,#124623,#124624,#124625,#124626,#124627,
#124628,#124629,#124630,#124631,#124632,#124633,#124634),(#124635,#124636,
#124637,#124638,#124639,#124640,#124641,#124642,#124643,#124644,#124645,
#124646,#124647,#124648,#124649,#124650,#124651,#124652,#124653,#124654,
#124655,#124656,#124657,#124658,#124659,#124660,#124661,#124662,#124663,
#124664,#124665,#124666,#124667,#124668,#124669,#124670,#124671,#124672,
#124673,#124674,#124675,#124676,#124677,#124678,#124679,#124680,#124681,
#124682,#124683,#124684,#124685,#124686,#124687,#124688,#124689,#124690,
#124691,#124692,#124693,#124694,#124695,#124696,#124697,#124698,#124699,
#124700,#124701,#124702,#124703,#124704,#124705,#124706,#124707,#124708,
#124709,#124710,#124711,#124712,#124713,#124714,#124715,#124716,#124717,
#124718,#124719,#124720,#124721,#124722,#124723,#124724,#124725,#124726,
#124727,#124728,#124729,#124730,#124731,#124732,#124733,#124734,#124735,
#124736,#124737,#124738,#124739,#124740,#124741,#124742,#124743,#124744,
#124745,#124746,#124747,#124748,#124749,#124750,#124751,#124752,#124753,
#124754,#124755,#124756,#124757,#124758,#124759,#124760,#124761,#124762,
#124763,#124764,#124765,#124766,#124767,#124768,#124769,#124770,#124771,
#124772,#124773,#124774,#124775,#124776,#124777,#124778,#124779,#124780,
#124781,#124782,#124783,#124784,#124785,#124786,#124787,#124788,#124789,
#124790,#124791,#124792,#124793,#124794,#124795,#124796,#124797,#124798,
#124799,#124800,#124801,#124802,#124803,#124804,#124805,#124806,#124807,
#124808,#124809,#124810,#124811,#124812,#124813,#124814,#124815,#124816,
#124817,#124818,#124819,#124820,#124821,#124822,#124823,#124824,#124825,
#124826,#124827,#124828,#124829,#124830,#124831,#124832,#124833,#124834,
#124835,#124836,#124837,#124838,#124839,#124840,#124841,#124842,#124843,
#124844,#124845,#124846,#124847,#124848,#124849,#124850,#124851,#124852,
#124853,#124854,#124855,#124856,#124857,#124858,#124859,#124860,#124861,
#124862,#124863,#124864,#124865,#124866,#124867,#124868,#124869,#124870,
#124871,#124872,#124873,#124874,#124875,#124876,#124877,#124878,#124879,
#124880,#124881,#124882,#124883,#124884,#124885,#124886,#124887,#124888,
#124889,#124890,#124891,#124892,#124893,#124894,#124895,#124896,#124897,
#124898,#124899,#124900,#124901,#124902,#124903,#124904,#124905,#124906,
#124907,#124908,#124909,#124910,#124911,#124912,#124913,#124914,#124915,
#124916,#124917,#124918,#124919,#124920,#124921,#124922,#124923,#124924,
#124925,#124926,#124927,#124928,#124929,#124930,#124931,#124932,#124933,
#124934,#124935,#124936,#124937,#124938,#124939,#124940,#124941,#124942,
#124943,#124944,#124945,#124946,#124947,#124948,#124949,#124950,#124951,
#124952,#124953,#124954,#124955,#124956,#124957,#124958,#124959,#124960,
#124961,#124962,#124963,#124964,#124965,#124966,#124967,#124968,#124969,
#124970,#124971,#124972,#124973,#124974,#124975,#124976,#124977,#124978,
#124979,#124980,#124981,#124982,#124983,#124984,#124985,#124986,#124987,
#124988,#124989,#124990,#124991,#124992,#124993,#124994,#124995,#124996,
#124997,#124998,#124999,#125000,#125001,#125002,#125003,#125004,#125005,
#125006,#125007,#125008,#125009,#125010,#125011,#125012,#125013,#125014,
#125015,#125016,#125017,#125018,#125019,#125020,#125021,#125022,#125023,
#125024,#125025,#125026,#125027,#125028,#125029,#125030,#125031,#125032,
#125033,#125034,#125035,#125036,#125037,#125038,#125039,#125040,#125041,
#125042,#125043,#125044,#125045,#125046,#125047,#125048,#125049,#125050,
#125051,#125052,#125053,#125054,#125055,#125056,#125057,#125058,#125059,
#125060,#125061,#125062,#125063,#125064,#125065,#125066,#125067,#125068,
#125069,#125070,#125071,#125072,#125073,#125074,#125075,#125076,#125077,
#125078,#125079,#125080,#125081,#125082,#125083,#125084,#125085,#125086,
#125087,#125088,#125089,#125090,#125091,#125092,#125093,#125094,#125095,
#125096,#125097,#125098,#125099,#125100,#125101,#125102,#125103,#125104,
#125105,#125106,#125107,#125108,#125109,#125110,#125111,#125112,#125113,
#125114,#125115,#125116,#125117,#125118,#125119,#125120,#125121,#125122,
#125123,#125124,#125125,#125126,#125127,#125128,#125129,#125130,#125131,
#125132,#125133,#125134,#125135,#125136,#125137,#125138,#125139,#125140,
#125141,#125142,#125143,#125144,#125145,#125146,#125147,#125148,#125149,
#125150,#125151,#125152,#125153,#125154,#125155,#125156,#125157,#125158,
#125159,#125160,#125161,#125162,#125163,#125164,#125165,#125166,#125167,
#125168,#125169,#125170,#125171,#125172,#125173,#125174,#125175,#125176,
#125177,#125178,#125179,#125180,#125181,#125182,#125183,#125184,#125185,
#125186,#125187,#125188,#125189,#125190,#125191,#125192,#125193,#125194,
#125195,#125196,#125197,#125198,#125199,#125200,#125201,#125202,#125203,
#125204,#125205,#125206,#125207,#125208,#125209,#125210,#125211,#125212,
#125213,#125214,#125215,#125216,#125217,#125218,#125219,#125220,#125221,
#125222,#125223,#125224,#125225,#125226,#125227,#125228,#125229,#125230,
#125231,#125232,#125233,#125234,#125235,#125236,#125237,#125238,#125239,
#125240,#125241,#125242,#125243,#125244,#125245,#125246,#125247,#125248,
#125249,#125250,#125251,#125252,#125253,#125254,#125255,#125256,#125257,
#125258,#125259,#125260,#125261,#125262,#125263,#125264,#125265,#125266,
#125267,#125268,#125269,#125270,#125271,#125272,#125273,#125274,#125275,
#125276,#125277,#125278,#125279,#125280,#125281,#125282,#125283,#125284,
#125285,#125286,#125287,#125288,#125289,#125290,#125291,#125292,#125293,
#125294,#125295,#125296,#125297,#125298,#125299,#125300,#125301,#125302,
#125303,#125304,#125305,#125306,#125307,#125308,#125309,#125310,#125311,
#125312,#125313,#125314,#125315,#125316,#125317,#125318,#125319,#125320,
#125321,#125322,#125323,#125324,#125325,#125326,#125327,#125328,#125329,
#125330,#125331,#125332,#125333,#125334,#125335,#125336,#125337,#125338,
#125339,#125340,#125341,#125342,#125343,#125344,#125345,#125346,#125347,
#125348,#125349,#125350,#125351,#125352,#125353,#125354,#125355,#125356,
#125357,#125358,#125359,#125360,#125361,#125362,#125363,#125364,#125365,
#125366,#125367,#125368,#125369,#125370,#125371,#125372,#125373,#125374,
#125375,#125376,#125377,#125378,#125379,#125380,#125381,#125382,#125383,
#125384,#125385,#125386,#125387,#125388,#125389,#125390,#125391,#125392,
#125393,#125394,#125395,#125396,#125397,#125398,#125399,#125400,#125401,
#125402,#125403,#125404,#125405,#125406,#125407,#125408,#125409,#125410,
#125411,#125412,#125413,#125414,#125415,#125416,#125417,#125418,#125419,
#125420,#125421,#125422,#125423,#125424,#125425,#125426,#125427,#125428,
#125429,#125430,#125431,#125432,#125433,#125434,#125435,#125436,#125437,
#125438,#125439,#125440,#125441,#125442,#125443,#125444,#125445,#125446,
#125447,#125448,#125449,#125450,#125451,#125452,#125453,#125454,#125455,
#125456,#125457,#125458,#125459,#125460,#125461,#125462,#125463,#125464,
#125465,#125466,#125467,#125468,#125469,#125470,#125471,#125472,#125473,
#125474,#125475,#125476,#125477,#125478,#125479,#125480,#125481,#125482,
#125483,#125484,#125485,#125486,#125487,#125488,#125489,#125490,#125491,
#125492,#125493,#125494,#125495,#125496,#125497,#125498,#125499,#125500,
#125501,#125502,#125503,#125504,#125505,#125506,#125507,#125508,#125509,
#125510,#125511,#125512,#125513,#125514,#125515,#125516,#125517,#125518,
#125519,#125520,#125521,#125522,#125523,#125524,#125525,#125526,#125527,
#125528,#125529,#125530,#125531,#125532,#125533,#125534,#125535,#125536,
#125537,#125538,#125539,#125540,#125541,#125542,#125543,#125544,#125545,
#125546,#125547,#125548,#125549,#125550,#125551,#125552,#125553,#125554,
#125555,#125556,#125557,#125558,#125559,#125560,#125561,#125562,#125563,
#125564,#125565,#125566,#125567,#125568,#125569,#125570,#125571,#125572,
#125573,#125574,#125575,#125576,#125577,#125578,#125579,#125580,#125581,
#125582,#125583,#125584,#125585,#125586,#125587,#125588,#125589,#125590,
#125591,#125592,#125593,#125594,#125595,#125596,#125597,#125598,#125599,
#125600,#125601,#125602,#125603,#125604,#125605,#125606,#125607,#125608,
#125609,#125610,#125611,#125612,#125613,#125614,#125615,#125616,#125617,
#125618,#125619,#125620,#125621,#125622,#125623,#125624,#125625,#125626,
#125627,#125628,#125629,#125630,#125631,#125632,#125633,#125634,#125635,
#125636,#125637,#125638,#125639,#125640,#125641,#125642,#125643,#125644,
#125645,#125646,#125647,#125648,#125649,#125650,#125651,#125652,#125653,
#125654,#125655,#125656,#125657,#125658,#125659,#125660,#125661,#125662,
#125663,#125664,#125665,#125666,#125667,#125668,#125669,#125670,#125671,
#125672,#125673,#125674,#125675,#125676,#125677,#125678,#125679,#125680,
#125681,#125682,#125683,#125684,#125685,#125686,#125687,#125688,#125689,
#125690,#125691,#125692,#125693,#125694,#125695,#125696,#125697,#125698,
#125699,#125700,#125701,#125702,#125703,#125704,#125705,#125706,#125707,
#125708,#125709,#125710,#125711,#125712,#125713,#125714,#125715,#125716,
#125717,#125718,#125719,#125720,#125721,#125722,#125723,#125724,#125725,
#125726,#125727,#125728,#125729,#125730,#125731,#125732,#125733,#125734,
#125735,#125736,#125737,#125738,#125739,#125740,#125741,#125742,#125743,
#125744,#125745,#125746,#125747,#125748,#125749,#125750,#125751,#125752,
#125753,#125754,#125755,#125756,#125757,#125758,#125759,#125760,#125761,
#125762,#125763,#125764,#125765,#125766,#125767,#125768,#125769,#125770,
#125771,#125772,#125773,#125774,#125775,#125776,#125777,#125778,#125779,
#125780,#125781,#125782,#125783,#125784,#125785,#125786,#125787,#125788,
#125789,#125790,#125791,#125792,#125793,#125794,#125795,#125796,#125797,
#125798,#125799,#125800,#125801,#125802,#125803,#125804,#125805,#125806,
#125807,#125808,#125809,#125810,#125811,#125812,#125813,#125814,#125815,
#125816,#125817,#125818,#125819,#125820,#125821,#125822,#125823,#125824,
#125825,#125826,#125827,#125828,#125829,#125830,#125831,#125832,#125833,
#125834,#125835,#125836,#125837,#125838,#125839,#125840,#125841,#125842,
#125843,#125844,#125845,#125846,#125847,#125848,#125849,#125850,#125851,
#125852,#125853,#125854,#125855,#125856,#125857,#125858,#125859,#125860,
#125861,#125862,#125863,#125864,#125865,#125866,#125867,#125868,#125869,
#125870,#125871,#125872,#125873,#125874,#125875,#125876,#125877,#125878,
#125879,#125880,#125881,#125882,#125883,#125884,#125885,#125886,#125887,
#125888,#125889,#125890,#125891,#125892,#125893,#125894,#125895,#125896,
#125897,#125898,#125899,#125900,#125901,#125902,#125903,#125904,#125905,
#125906,#125907,#125908,#125909,#125910,#125911,#125912,#125913,#125914,
#125915,#125916,#125917,#125918,#125919,#125920,#125921,#125922,#125923,
#125924,#125925,#125926,#125927,#125928,#125929,#125930,#125931,#125932,
#125933,#125934,#125935,#125936,#125937,#125938,#125939,#125940,#125941,
#125942,#125943,#125944,#125945,#125946,#125947,#125948,#125949,#125950,
#125951,#125952,#125953,#125954,#125955,#125956,#125957,#125958,#125959,
#125960,#125961,#125962,#125963,#125964,#125965,#125966,#125967,#125968,
#125969,#125970,#125971,#125972,#125973,#125974,#125975,#125976,#125977,
#125978,#125979,#125980,#125981,#125982,#125983,#125984,#125985,#125986,
#125987,#125988,#125989,#125990,#125991,#125992,#125993,#125994,#125995,
#125996,#125997,#125998,#125999,#126000,#126001,#126002,#126003,#126004,
#126005,#126006,#126007,#126008,#126009,#126010,#126011,#126012,#126013,
#126014,#126015,#126016,#126017,#126018,#126019,#126020,#126021,#126022,
#126023,#126024,#126025,#126026,#126027,#126028,#126029,#126030,#126031,
#126032,#126033,#126034,#126035,#126036,#126037,#126038,#126039,#126040,
#126041,#126042,#126043,#126044,#126045,#126046,#126047,#126048,#126049,
#126050,#126051,#126052,#126053,#126054,#126055,#126056,#126057,#126058,
#126059,#126060,#126061,#126062,#126063,#126064,#126065,#126066,#126067,
#126068,#126069,#126070,#126071,#126072,#126073,#126074,#126075,#126076,
#126077,#126078,#126079,#126080,#126081,#126082,#126083,#126084,#126085,
#126086,#126087,#126088,#126089,#126090,#126091,#126092,#126093,#126094,
#126095,#126096,#126097,#126098,#126099,#126100,#126101,#126102,#126103,
#126104,#126105,#126106,#126107,#126108,#126109,#126110,#126111,#126112,
#126113,#126114,#126115,#126116,#126117,#126118,#126119,#126120,#126121,
#126122,#126123,#126124,#126125,#126126,#126127,#126128,#126129,#126130,
#126131,#126132,#126133,#126134,#126135,#126136,#126137,#126138,#126139,
#126140,#126141,#126142,#126143,#126144,#126145,#126146,#126147,#126148,
#126149,#126150,#126151,#126152,#126153,#126154,#126155,#126156,#126157,
#126158,#126159,#126160,#126161,#126162,#126163,#126164,#126165,#126166,
#126167,#126168,#126169,#126170,#126171,#126172,#126173,#126174,#126175,
#126176,#126177,#126178,#126179,#126180,#126181,#126182,#126183,#126184,
#126185,#126186,#126187,#126188,#126189,#126190,#126191,#126192,#126193,
#126194,#126195,#126196,#126197,#126198,#126199,#126200,#126201,#126202,
#126203,#126204,#126205,#126206,#126207,#126208,#126209,#126210,#126211,
#126212,#126213,#126214,#126215,#126216,#126217,#126218,#126219,#126220,
#126221,#126222,#126223,#126224,#126225,#126226,#126227,#126228,#126229,
#126230,#126231,#126232,#126233,#126234,#126235,#126236,#126237,#126238,
#126239,#126240,#126241,#126242,#126243,#126244,#126245,#126246,#126247,
#126248,#126249,#126250,#126251,#126252,#126253,#126254,#126255,#126256,
#126257,#126258,#126259,#126260,#126261,#126262,#126263,#126264,#126265,
#126266,#126267,#126268,#126269,#126270,#126271,#126272,#126273,#126274,
#126275,#126276,#126277,#126278,#126279,#126280,#126281,#126282,#126283,
#126284,#126285,#126286,#126287,#126288,#126289,#126290,#126291,#126292,
#126293,#126294,#126295,#126296,#126297,#126298,#126299,#126300,#126301,
#126302,#126303,#126304,#126305,#126306,#126307,#126308,#126309,#126310,
#126311,#126312,#126313,#126314,#126315,#126316,#126317,#126318,#126319,
#126320,#126321,#126322,#126323,#126324,#126325,#126326,#126327,#126328,
#126329,#126330,#126331,#126332,#126333,#126334,#126335,#126336,#126337,
#126338,#126339,#126340,#126341,#126342,#126343,#126344,#126345,#126346,
#126347,#126348,#126349,#126350,#126351,#126352,#126353,#126354,#126355,
#126356,#126357,#126358,#126359,#126360,#126361,#126362,#126363,#126364,
#126365,#126366,#126367,#126368,#126369,#126370,#126371,#126372,#126373,
#126374,#126375,#126376,#126377,#126378,#126379,#126380,#126381,#126382,
#126383,#126384,#126385,#126386,#126387,#126388,#126389,#126390,#126391,
#126392,#126393,#126394,#126395,#126396,#126397,#126398,#126399,#126400,
#126401,#126402,#126403,#126404,#126405,#126406,#126407,#126408,#126409,
#126410,#126411,#126412,#126413,#126414,#126415,#126416,#126417,#126418,
#126419,#126420,#126421,#126422,#126423,#126424,#126425,#126426,#126427,
#126428,#126429,#126430,#126431,#126432,#126433,#126434,#126435,#126436,
#126437,#126438,#126439,#126440,#126441,#126442,#126443,#126444,#126445,
#126446,#126447,#126448,#126449,#126450,#126451,#126452,#126453,#126454,
#126455,#126456,#126457,#126458,#126459,#126460,#126461,#126462,#126463,
#126464,#126465,#126466,#126467,#126468,#126469,#126470,#126471,#126472,
#126473,#126474,#126475,#126476,#126477,#126478,#126479,#126480,#126481,
#126482,#126483,#126484,#126485,#126486,#126487,#126488,#126489,#126490,
#126491,#126492,#126493,#126494,#126495,#126496,#126497,#126498,#126499,
#126500,#126501,#126502,#126503,#126504,#126505,#126506,#126507,#126508,
#126509,#126510,#126511,#126512,#126513,#126514,#126515,#126516,#126517,
#126518,#126519,#126520,#126521,#126522,#126523,#126524,#126525,#126526,
#126527,#126528,#126529,#126530,#126531,#126532,#126533,#126534,#126535,
#126536,#126537,#126538,#126539,#126540,#126541,#126542,#126543,#126544,
#126545,#126546,#126547,#126548,#126549,#126550,#126551,#126552,#126553,
#126554,#126555,#126556,#126557,#126558,#126559,#126560,#126561,#126562,
#126563,#126564,#126565,#126566,#126567,#126568,#126569,#126570,#126571,
#126572,#126573,#126574,#126575,#126576,#126577,#126578,#126579,#126580,
#126581,#126582,#126583,#126584,#126585,#126586,#126587,#126588,#126589,
#126590,#126591,#126592,#126593,#126594,#126595,#126596,#126597,#126598,
#126599,#126600,#126601,#126602,#126603,#126604,#126605,#126606,#126607,
#126608,#126609,#126610,#126611,#126612,#126613,#126614,#126615,#126616,
#126617,#126618,#126619,#126620,#126621,#126622,#126623,#126624,#126625,
#126626,#126627,#126628,#126629,#126630,#126631,#126632,#126633,#126634,
#126635,#126636,#126637,#126638,#126639,#126640,#126641,#126642,#126643,
#126644,#126645,#126646,#126647,#126648,#126649,#126650,#126651,#126652,
#126653,#126654,#126655,#126656,#126657,#126658,#126659,#126660,#126661,
#126662,#126663,#126664,#126665,#126666,#126667,#126668,#126669,#126670,
#126671,#126672,#126673,#126674,#126675,#126676,#126677,#126678,#126679,
#126680,#126681,#126682,#126683,#126684,#126685),(#126686,#126687,#126688,
#126689,#126690,#126691,#126692,#126693,#126694,#126695,#126696,#126697,
#126698,#126699,#126700,#126701,#126702,#126703,#126704,#126705,#126706,
#126707,#126708,#126709,#126710,#126711,#126712,#126713,#126714,#126715,
#126716,#126717,#126718,#126719,#126720,#126721,#126722,#126723,#126724,
#126725,#126726,#126727,#126728,#126729,#126730,#126731,#126732,#126733,
#126734,#126735,#126736,#126737,#126738,#126739,#126740,#126741,#126742,
#126743,#126744,#126745,#126746,#126747,#126748,#126749,#126750,#126751,
#126752,#126753,#126754,#126755,#126756,#126757,#126758,#126759,#126760,
#126761,#126762,#126763,#126764,#126765,#126766,#126767,#126768,#126769,
#126770,#126771,#126772,#126773,#126774,#126775,#126776,#126777,#126778,
#126779,#126780,#126781,#126782,#126783,#126784,#126785,#126786,#126787,
#126788,#126789,#126790,#126791,#126792,#126793,#126794,#126795,#126796,
#126797,#126798,#126799,#126800,#126801,#126802,#126803,#126804,#126805,
#126806,#126807,#126808,#126809,#126810,#126811,#126812,#126813,#126814,
#126815,#126816,#126817,#126818,#126819,#126820,#126821,#126822,#126823,
#126824,#126825,#126826,#126827,#126828,#126829,#126830,#126831,#126832,
#126833,#126834,#126835,#126836,#126837,#126838,#126839,#126840,#126841,
#126842,#126843,#126844,#126845,#126846,#126847,#126848,#126849,#126850,
#126851,#126852,#126853,#126854,#126855,#126856,#126857,#126858,#126859,
#126860,#126861,#126862,#126863,#126864,#126865,#126866,#126867,#126868,
#126869,#126870,#126871,#126872,#126873,#126874,#126875,#126876,#126877,
#126878,#126879,#126880,#126881,#126882,#126883,#126884,#126885,#126886,
#126887,#126888,#126889,#126890,#126891,#126892,#126893,#126894,#126895,
#126896,#126897,#126898,#126899,#126900,#126901,#126902,#126903,#126904,
#126905,#126906,#126907,#126908,#126909,#126910,#126911,#126912,#126913,
#126914,#126915,#126916,#126917,#126918,#126919,#126920,#126921,#126922,
#126923,#126924,#126925,#126926,#126927,#126928,#126929,#126930,#126931,
#126932,#126933,#126934,#126935,#126936,#126937,#126938,#126939,#126940,
#126941,#126942,#126943,#126944,#126945,#126946,#126947,#126948,#126949,
#126950,#126951,#126952,#126953,#126954,#126955,#126956,#126957,#126958,
#126959,#126960,#126961,#126962,#126963,#126964,#126965,#126966,#126967,
#126968,#126969,#126970,#126971,#126972,#126973,#126974,#126975,#126976,
#126977,#126978,#126979,#126980,#126981,#126982,#126983,#126984,#126985,
#126986,#126987,#126988,#126989,#126990,#126991,#126992,#126993,#126994,
#126995,#126996,#126997,#126998,#126999,#127000,#127001,#127002,#127003,
#127004,#127005,#127006,#127007,#127008,#127009,#127010,#127011,#127012,
#127013,#127014,#127015,#127016,#127017,#127018,#127019,#127020,#127021,
#127022,#127023,#127024,#127025,#127026,#127027,#127028,#127029,#127030,
#127031,#127032,#127033,#127034,#127035,#127036,#127037,#127038,#127039,
#127040,#127041,#127042,#127043,#127044,#127045,#127046,#127047,#127048,
#127049,#127050,#127051,#127052,#127053,#127054,#127055,#127056,#127057,
#127058,#127059,#127060,#127061,#127062,#127063,#127064,#127065,#127066,
#127067,#127068,#127069,#127070,#127071,#127072,#127073,#127074,#127075,
#127076,#127077,#127078,#127079,#127080,#127081,#127082,#127083,#127084,
#127085,#127086,#127087,#127088,#127089,#127090,#127091,#127092,#127093,
#127094,#127095,#127096,#127097,#127098,#127099,#127100,#127101,#127102,
#127103,#127104,#127105,#127106,#127107,#127108,#127109,#127110,#127111,
#127112,#127113,#127114,#127115,#127116,#127117,#127118,#127119,#127120,
#127121,#127122,#127123,#127124,#127125,#127126,#127127,#127128,#127129,
#127130,#127131,#127132,#127133,#127134,#127135,#127136,#127137,#127138,
#127139,#127140,#127141,#127142,#127143,#127144,#127145,#127146,#127147,
#127148,#127149,#127150,#127151,#127152,#127153,#127154,#127155,#127156,
#127157,#127158,#127159,#127160,#127161,#127162,#127163,#127164,#127165,
#127166,#127167,#127168,#127169,#127170,#127171,#127172,#127173,#127174,
#127175,#127176,#127177,#127178,#127179,#127180,#127181,#127182,#127183,
#127184,#127185,#127186,#127187,#127188,#127189,#127190,#127191,#127192,
#127193,#127194,#127195,#127196,#127197,#127198,#127199,#127200,#127201,
#127202,#127203,#127204,#127205,#127206,#127207,#127208,#127209,#127210,
#127211,#127212,#127213,#127214,#127215,#127216,#127217,#127218,#127219,
#127220,#127221,#127222,#127223,#127224,#127225,#127226,#127227,#127228,
#127229,#127230,#127231,#127232,#127233,#127234,#127235,#127236,#127237,
#127238,#127239,#127240,#127241,#127242,#127243,#127244,#127245,#127246,
#127247,#127248,#127249,#127250,#127251,#127252,#127253,#127254,#127255,
#127256,#127257,#127258,#127259,#127260,#127261,#127262,#127263,#127264,
#127265,#127266,#127267,#127268,#127269,#127270,#127271,#127272,#127273,
#127274,#127275,#127276,#127277,#127278,#127279,#127280,#127281,#127282,
#127283,#127284,#127285,#127286,#127287,#127288,#127289,#127290,#127291,
#127292,#127293,#127294,#127295,#127296,#127297,#127298,#127299,#127300,
#127301,#127302,#127303,#127304,#127305,#127306,#127307,#127308,#127309,
#127310,#127311,#127312,#127313,#127314,#127315,#127316,#127317,#127318,
#127319,#127320,#127321,#127322,#127323,#127324,#127325,#127326,#127327,
#127328,#127329,#127330,#127331,#127332,#127333,#127334,#127335,#127336,
#127337,#127338,#127339,#127340,#127341,#127342,#127343,#127344,#127345,
#127346,#127347,#127348,#127349,#127350,#127351,#127352,#127353,#127354,
#127355,#127356,#127357,#127358,#127359,#127360,#127361,#127362,#127363,
#127364,#127365,#127366,#127367,#127368,#127369,#127370,#127371,#127372,
#127373,#127374,#127375,#127376,#127377,#127378,#127379,#127380,#127381,
#127382,#127383,#127384,#127385,#127386,#127387,#127388,#127389,#127390,
#127391,#127392,#127393,#127394,#127395,#127396,#127397,#127398,#127399,
#127400,#127401,#127402,#127403,#127404,#127405,#127406,#127407,#127408,
#127409,#127410,#127411,#127412,#127413,#127414,#127415,#127416,#127417,
#127418,#127419,#127420,#127421,#127422,#127423,#127424,#127425,#127426,
#127427,#127428,#127429,#127430,#127431,#127432,#127433,#127434,#127435,
#127436,#127437,#127438,#127439,#127440,#127441,#127442,#127443,#127444,
#127445,#127446,#127447,#127448,#127449,#127450,#127451,#127452,#127453,
#127454,#127455,#127456,#127457,#127458,#127459,#127460,#127461,#127462,
#127463,#127464,#127465,#127466,#127467,#127468,#127469,#127470,#127471,
#127472,#127473,#127474,#127475,#127476,#127477,#127478,#127479,#127480,
#127481,#127482,#127483,#127484,#127485,#127486,#127487,#127488,#127489,
#127490,#127491,#127492,#127493,#127494,#127495,#127496,#127497,#127498,
#127499,#127500,#127501,#127502,#127503,#127504,#127505,#127506,#127507,
#127508,#127509,#127510,#127511,#127512,#127513,#127514,#127515,#127516,
#127517,#127518,#127519,#127520,#127521,#127522,#127523,#127524,#127525,
#127526,#127527,#127528,#127529,#127530,#127531,#127532,#127533,#127534,
#127535,#127536,#127537,#127538,#127539,#127540,#127541,#127542,#127543,
#127544,#127545,#127546,#127547,#127548,#127549,#127550,#127551,#127552,
#127553,#127554,#127555,#127556,#127557,#127558,#127559,#127560,#127561,
#127562,#127563,#127564,#127565,#127566,#127567,#127568,#127569,#127570,
#127571,#127572,#127573,#127574,#127575,#127576,#127577,#127578,#127579,
#127580,#127581,#127582,#127583,#127584,#127585,#127586,#127587,#127588,
#127589,#127590,#127591,#127592,#127593,#127594,#127595,#127596,#127597,
#127598,#127599,#127600,#127601,#127602,#127603,#127604,#127605,#127606,
#127607,#127608,#127609,#127610,#127611,#127612,#127613,#127614,#127615,
#127616,#127617,#127618,#127619,#127620,#127621,#127622,#127623,#127624,
#127625,#127626,#127627,#127628,#127629,#127630,#127631,#127632,#127633,
#127634,#127635,#127636,#127637,#127638,#127639,#127640,#127641,#127642,
#127643,#127644,#127645,#127646,#127647,#127648,#127649,#127650,#127651,
#127652,#127653,#127654,#127655,#127656,#127657,#127658,#127659,#127660,
#127661,#127662,#127663,#127664,#127665,#127666,#127667,#127668,#127669,
#127670,#127671,#127672,#127673,#127674,#127675,#127676,#127677,#127678,
#127679,#127680,#127681,#127682,#127683,#127684,#127685,#127686,#127687,
#127688,#127689,#127690,#127691,#127692,#127693,#127694,#127695,#127696,
#127697,#127698,#127699,#127700,#127701,#127702,#127703,#127704,#127705,
#127706,#127707,#127708,#127709,#127710,#127711,#127712,#127713,#127714,
#127715,#127716,#127717,#127718,#127719,#127720,#127721,#127722,#127723,
#127724,#127725,#127726,#127727,#127728,#127729,#127730,#127731,#127732,
#127733,#127734,#127735,#127736,#127737,#127738,#127739,#127740,#127741,
#127742,#127743,#127744,#127745,#127746,#127747,#127748,#127749,#127750,
#127751,#127752,#127753,#127754,#127755,#127756,#127757,#127758,#127759,
#127760,#127761,#127762,#127763,#127764,#127765,#127766,#127767,#127768,
#127769,#127770,#127771,#127772,#127773,#127774,#127775,#127776,#127777,
#127778,#127779,#127780,#127781,#127782,#127783,#127784,#127785,#127786,
#127787,#127788,#127789,#127790,#127791,#127792,#127793,#127794,#127795,
#127796,#127797,#127798,#127799,#127800,#127801,#127802,#127803,#127804,
#127805,#127806,#127807,#127808,#127809,#127810,#127811,#127812,#127813,
#127814,#127815,#127816,#127817,#127818,#127819,#127820,#127821,#127822,
#127823,#127824,#127825,#127826,#127827,#127828,#127829,#127830,#127831,
#127832,#127833,#127834,#127835,#127836,#127837,#127838,#127839,#127840,
#127841,#127842,#127843,#127844,#127845,#127846,#127847,#127848,#127849,
#127850,#127851,#127852,#127853,#127854,#127855,#127856,#127857,#127858,
#127859,#127860,#127861,#127862,#127863,#127864,#127865,#127866,#127867,
#127868,#127869,#127870,#127871,#127872,#127873,#127874,#127875,#127876,
#127877,#127878,#127879,#127880,#127881,#127882,#127883,#127884,#127885,
#127886,#127887,#127888,#127889,#127890,#127891,#127892,#127893,#127894,
#127895,#127896,#127897,#127898,#127899,#127900,#127901,#127902,#127903,
#127904,#127905,#127906,#127907,#127908,#127909,#127910,#127911,#127912,
#127913,#127914,#127915,#127916,#127917,#127918,#127919,#127920,#127921,
#127922,#127923,#127924,#127925,#127926,#127927,#127928,#127929,#127930,
#127931,#127932,#127933,#127934,#127935,#127936,#127937,#127938,#127939,
#127940,#127941,#127942,#127943,#127944,#127945,#127946,#127947,#127948,
#127949,#127950,#127951,#127952,#127953,#127954,#127955,#127956,#127957,
#127958,#127959,#127960,#127961,#127962,#127963,#127964,#127965,#127966,
#127967,#127968,#127969,#127970,#127971,#127972,#127973,#127974,#127975,
#127976,#127977,#127978,#127979,#127980,#127981,#127982,#127983,#127984,
#127985,#127986,#127987,#127988,#127989,#127990,#127991,#127992,#127993,
#127994,#127995,#127996,#127997,#127998,#127999,#128000,#128001,#128002,
#128003,#128004,#128005,#128006,#128007,#128008,#128009,#128010,#128011,
#128012,#128013,#128014,#128015,#128016,#128017,#128018,#128019,#128020,
#128021,#128022,#128023,#128024,#128025,#128026,#128027,#128028,#128029,
#128030,#128031,#128032,#128033,#128034,#128035,#128036,#128037,#128038,
#128039,#128040,#128041,#128042,#128043,#128044,#128045,#128046,#128047,
#128048,#128049,#128050,#128051,#128052,#128053,#128054,#128055,#128056,
#128057,#128058,#128059,#128060,#128061,#128062,#128063,#128064,#128065,
#128066,#128067,#128068,#128069,#128070,#128071,#128072,#128073,#128074,
#128075,#128076,#128077,#128078,#128079,#128080,#128081,#128082,#128083,
#128084,#128085,#128086,#128087,#128088,#128089,#128090,#128091,#128092,
#128093,#128094,#128095,#128096,#128097,#128098,#128099,#128100,#128101,
#128102,#128103,#128104,#128105,#128106,#128107,#128108,#128109,#128110,
#128111,#128112,#128113,#128114,#128115,#128116,#128117,#128118,#128119,
#128120,#128121,#128122,#128123,#128124,#128125,#128126,#128127,#128128,
#128129,#128130,#128131,#128132,#128133,#128134,#128135,#128136,#128137,
#128138,#128139,#128140,#128141,#128142,#128143,#128144,#128145,#128146,
#128147,#128148,#128149,#128150,#128151,#128152,#128153,#128154,#128155,
#128156,#128157,#128158,#128159,#128160,#128161,#128162,#128163,#128164,
#128165,#128166,#128167,#128168,#128169,#128170,#128171,#128172,#128173,
#128174,#128175,#128176,#128177,#128178,#128179,#128180,#128181,#128182,
#128183,#128184,#128185,#128186,#128187,#128188,#128189,#128190,#128191,
#128192,#128193,#128194,#128195,#128196,#128197,#128198,#128199,#128200,
#128201,#128202,#128203,#128204,#128205,#128206,#128207,#128208,#128209,
#128210,#128211,#128212,#128213,#128214,#128215,#128216,#128217,#128218,
#128219,#128220,#128221,#128222,#128223,#128224,#128225,#128226,#128227,
#128228,#128229,#128230,#128231,#128232,#128233,#128234,#128235,#128236,
#128237,#128238,#128239,#128240,#128241,#128242,#128243,#128244,#128245,
#128246,#128247,#128248,#128249,#128250,#128251,#128252,#128253,#128254,
#128255,#128256,#128257,#128258,#128259,#128260,#128261,#128262,#128263,
#128264,#128265,#128266,#128267,#128268,#128269,#128270,#128271,#128272,
#128273,#128274,#128275,#128276,#128277,#128278,#128279,#128280,#128281,
#128282,#128283,#128284,#128285,#128286,#128287,#128288,#128289,#128290,
#128291,#128292,#128293,#128294,#128295,#128296,#128297,#128298,#128299,
#128300,#128301,#128302,#128303,#128304,#128305,#128306,#128307,#128308,
#128309,#128310,#128311,#128312,#128313,#128314,#128315,#128316,#128317,
#128318,#128319,#128320,#128321,#128322,#128323,#128324,#128325,#128326,
#128327,#128328,#128329,#128330,#128331,#128332,#128333,#128334,#128335,
#128336,#128337,#128338,#128339,#128340,#128341,#128342,#128343,#128344,
#128345,#128346,#128347,#128348,#128349,#128350,#128351,#128352,#128353,
#128354,#128355,#128356,#128357,#128358,#128359,#128360,#128361,#128362,
#128363,#128364,#128365,#128366,#128367,#128368,#128369,#128370,#128371,
#128372,#128373,#128374,#128375,#128376,#128377,#128378,#128379,#128380,
#128381,#128382,#128383,#128384,#128385,#128386,#128387,#128388,#128389,
#128390,#128391,#128392,#128393,#128394,#128395,#128396,#128397,#128398,
#128399,#128400,#128401,#128402,#128403,#128404,#128405,#128406,#128407,
#128408,#128409,#128410,#128411,#128412,#128413,#128414,#128415,#128416,
#128417,#128418,#128419,#128420,#128421,#128422,#128423,#128424,#128425,
#128426,#128427,#128428,#128429,#128430,#128431,#128432,#128433,#128434,
#128435,#128436,#128437,#128438,#128439,#128440,#128441,#128442,#128443,
#128444,#128445,#128446,#128447,#128448,#128449,#128450,#128451,#128452,
#128453,#128454,#128455,#128456,#128457,#128458,#128459,#128460,#128461,
#128462,#128463,#128464,#128465,#128466,#128467,#128468,#128469,#128470,
#128471,#128472,#128473,#128474,#128475,#128476,#128477,#128478,#128479,
#128480,#128481,#128482,#128483,#128484,#128485,#128486,#128487,#128488,
#128489,#128490,#128491,#128492,#128493,#128494,#128495,#128496,#128497,
#128498,#128499,#128500,#128501,#128502,#128503,#128504,#128505,#128506,
#128507,#128508,#128509,#128510,#128511,#128512,#128513,#128514,#128515,
#128516,#128517,#128518,#128519,#128520,#128521,#128522,#128523,#128524,
#128525,#128526,#128527,#128528,#128529,#128530,#128531,#128532,#128533,
#128534,#128535,#128536,#128537,#128538,#128539,#128540,#128541,#128542,
#128543,#128544,#128545,#128546,#128547,#128548,#128549,#128550,#128551,
#128552,#128553,#128554,#128555,#128556,#128557,#128558,#128559,#128560,
#128561,#128562,#128563,#128564,#128565,#128566,#128567,#128568,#128569,
#128570,#128571,#128572,#128573,#128574,#128575,#128576,#128577,#128578,
#128579,#128580,#128581,#128582,#128583,#128584,#128585,#128586,#128587,
#128588,#128589,#128590,#128591,#128592,#128593,#128594,#128595,#128596,
#128597,#128598,#128599,#128600,#128601,#128602,#128603,#128604,#128605,
#128606,#128607,#128608,#128609,#128610,#128611,#128612,#128613,#128614,
#128615,#128616,#128617,#128618,#128619,#128620,#128621,#128622,#128623,
#128624,#128625,#128626,#128627,#128628,#128629,#128630,#128631,#128632,
#128633,#128634,#128635,#128636,#128637,#128638,#128639,#128640,#128641,
#128642,#128643,#128644,#128645,#128646,#128647,#128648,#128649,#128650,
#128651,#128652,#128653,#128654,#128655,#128656,#128657,#128658,#128659,
#128660,#128661,#128662,#128663,#128664,#128665,#128666,#128667,#128668,
#128669,#128670,#128671,#128672,#128673,#128674,#128675,#128676,#128677,
#128678,#128679,#128680,#128681,#128682,#128683,#128684,#128685,#128686,
#128687,#128688,#128689,#128690,#128691,#128692,#128693,#128694,#128695,
#128696,#128697,#128698,#128699,#128700,#128701,#128702,#128703,#128704,
#128705,#128706,#128707,#128708,#128709,#128710,#128711,#128712,#128713,
#128714,#128715,#128716,#128717,#128718,#128719,#128720,#128721,#128722,
#128723,#128724,#128725,#128726,#128727,#128728,#128729,#128730,#128731,
#128732,#128733,#128734,#128735,#128736),(#128737,#128738,#128739,#128740,
#128741,#128742,#128743,#128744,#128745,#128746,#128747,#128748,#128749,
#128750,#128751,#128752,#128753,#128754,#128755,#128756,#128757,#128758,
#128759,#128760,#128761,#128762,#128763,#128764,#128765,#128766,#128767,
#128768,#128769,#128770,#128771,#128772,#128773,#128774,#128775,#128776,
#128777,#128778,#128779,#128780,#128781,#128782,#128783,#128784,#128785,
#128786,#128787,#128788,#128789,#128790,#128791,#128792,#128793,#128794,
#128795,#128796,#128797,#128798,#128799,#128800,#128801,#128802,#128803,
#128804,#128805,#128806,#128807,#128808,#128809,#128810,#128811,#128812,
#128813,#128814,#128815,#128816,#128817,#128818,#128819,#128820,#128821,
#128822,#128823,#128824,#128825,#128826,#128827,#128828,#128829,#128830,
#128831,#128832,#128833,#128834,#128835,#128836,#128837,#128838,#128839,
#128840,#128841,#128842,#128843,#128844,#128845,#128846,#128847,#128848,
#128849,#128850,#128851,#128852,#128853,#128854,#128855,#128856,#128857,
#128858,#128859,#128860,#128861,#128862,#128863,#128864,#128865,#128866,
#128867,#128868,#128869,#128870,#128871,#128872,#128873,#128874,#128875,
#128876,#128877,#128878,#128879,#128880,#128881,#128882,#128883,#128884,
#128885,#128886,#128887,#128888,#128889,#128890,#128891,#128892,#128893,
#128894,#128895,#128896,#128897,#128898,#128899,#128900,#128901,#128902,
#128903,#128904,#128905,#128906,#128907,#128908,#128909,#128910,#128911,
#128912,#128913,#128914,#128915,#128916,#128917,#128918,#128919,#128920,
#128921,#128922,#128923,#128924,#128925,#128926,#128927,#128928,#128929,
#128930,#128931,#128932,#128933,#128934,#128935,#128936,#128937,#128938,
#128939,#128940,#128941,#128942,#128943,#128944,#128945,#128946,#128947,
#128948,#128949,#128950,#128951,#128952,#128953,#128954,#128955,#128956,
#128957,#128958,#128959,#128960,#128961,#128962,#128963,#128964,#128965,
#128966,#128967,#128968,#128969,#128970,#128971,#128972,#128973,#128974,
#128975,#128976,#128977,#128978,#128979,#128980,#128981,#128982,#128983,
#128984,#128985,#128986,#128987,#128988,#128989,#128990,#128991,#128992,
#128993,#128994,#128995,#128996,#128997,#128998,#128999,#129000,#129001,
#129002,#129003,#129004,#129005,#129006,#129007,#129008,#129009,#129010,
#129011,#129012,#129013,#129014,#129015,#129016,#129017,#129018,#129019,
#129020,#129021,#129022,#129023,#129024,#129025,#129026,#129027,#129028,
#129029,#129030,#129031,#129032,#129033,#129034,#129035,#129036,#129037,
#129038,#129039,#129040,#129041,#129042,#129043,#129044,#129045,#129046,
#129047,#129048,#129049,#129050,#129051,#129052,#129053,#129054,#129055,
#129056,#129057,#129058,#129059,#129060,#129061,#129062,#129063,#129064,
#129065,#129066,#129067,#129068,#129069,#129070,#129071,#129072,#129073,
#129074,#129075,#129076,#129077,#129078,#129079,#129080,#129081,#129082,
#129083,#129084,#129085,#129086,#129087,#129088,#129089,#129090,#129091,
#129092,#129093,#129094,#129095,#129096,#129097,#129098,#129099,#129100,
#129101,#129102,#129103,#129104,#129105,#129106,#129107,#129108,#129109,
#129110,#129111,#129112,#129113,#129114,#129115,#129116,#129117,#129118,
#129119,#129120,#129121,#129122,#129123,#129124,#129125,#129126,#129127,
#129128,#129129,#129130,#129131,#129132,#129133,#129134,#129135,#129136,
#129137,#129138,#129139,#129140,#129141,#129142,#129143,#129144,#129145,
#129146,#129147,#129148,#129149,#129150,#129151,#129152,#129153,#129154,
#129155,#129156,#129157,#129158,#129159,#129160,#129161,#129162,#129163,
#129164,#129165,#129166,#129167,#129168,#129169,#129170,#129171,#129172,
#129173,#129174,#129175,#129176,#129177,#129178,#129179,#129180,#129181,
#129182,#129183,#129184,#129185,#129186,#129187,#129188,#129189,#129190,
#129191,#129192,#129193,#129194,#129195,#129196,#129197,#129198,#129199,
#129200,#129201,#129202,#129203,#129204,#129205,#129206,#129207,#129208,
#129209,#129210,#129211,#129212,#129213,#129214,#129215,#129216,#129217,
#129218,#129219,#129220,#129221,#129222,#129223,#129224,#129225,#129226,
#129227,#129228,#129229,#129230,#129231,#129232,#129233,#129234,#129235,
#129236,#129237,#129238,#129239,#129240,#129241,#129242,#129243,#129244,
#129245,#129246,#129247,#129248,#129249,#129250,#129251,#129252,#129253,
#129254,#129255,#129256,#129257,#129258,#129259,#129260,#129261,#129262,
#129263,#129264,#129265,#129266,#129267,#129268,#129269,#129270,#129271,
#129272,#129273,#129274,#129275,#129276,#129277,#129278,#129279,#129280,
#129281,#129282,#129283,#129284,#129285,#129286,#129287,#129288,#129289,
#129290,#129291,#129292,#129293,#129294,#129295,#129296,#129297,#129298,
#129299,#129300,#129301,#129302,#129303,#129304,#129305,#129306,#129307,
#129308,#129309,#129310,#129311,#129312,#129313,#129314,#129315,#129316,
#129317,#129318,#129319,#129320,#129321,#129322,#129323,#129324,#129325,
#129326,#129327,#129328,#129329,#129330,#129331,#129332,#129333,#129334,
#129335,#129336,#129337,#129338,#129339,#129340,#129341,#129342,#129343,
#129344,#129345,#129346,#129347,#129348,#129349,#129350,#129351,#129352,
#129353,#129354,#129355,#129356,#129357,#129358,#129359,#129360,#129361,
#129362,#129363,#129364,#129365,#129366,#129367,#129368,#129369,#129370,
#129371,#129372,#129373,#129374,#129375,#129376,#129377,#129378,#129379,
#129380,#129381,#129382,#129383,#129384,#129385,#129386,#129387,#129388,
#129389,#129390,#129391,#129392,#129393,#129394,#129395,#129396,#129397,
#129398,#129399,#129400,#129401,#129402,#129403,#129404,#129405,#129406,
#129407,#129408,#129409,#129410,#129411,#129412,#129413,#129414,#129415,
#129416,#129417,#129418,#129419,#129420,#129421,#129422,#129423,#129424,
#129425,#129426,#129427,#129428,#129429,#129430,#129431,#129432,#129433,
#129434,#129435,#129436,#129437,#129438,#129439,#129440,#129441,#129442,
#129443,#129444,#129445,#129446,#129447,#129448,#129449,#129450,#129451,
#129452,#129453,#129454,#129455,#129456,#129457,#129458,#129459,#129460,
#129461,#129462,#129463,#129464,#129465,#129466,#129467,#129468,#129469,
#129470,#129471,#129472,#129473,#129474,#129475,#129476,#129477,#129478,
#129479,#129480,#129481,#129482,#129483,#129484,#129485,#129486,#129487,
#129488,#129489,#129490,#129491,#129492,#129493,#129494,#129495,#129496,
#129497,#129498,#129499,#129500,#129501,#129502,#129503,#129504,#129505,
#129506,#129507,#129508,#129509,#129510,#129511,#129512,#129513,#129514,
#129515,#129516,#129517,#129518,#129519,#129520,#129521,#129522,#129523,
#129524,#129525,#129526,#129527,#129528,#129529,#129530,#129531,#129532,
#129533,#129534,#129535,#129536,#129537,#129538,#129539,#129540,#129541,
#129542,#129543,#129544,#129545,#129546,#129547,#129548,#129549,#129550,
#129551,#129552,#129553,#129554,#129555,#129556,#129557,#129558,#129559,
#129560,#129561,#129562,#129563,#129564,#129565,#129566,#129567,#129568,
#129569,#129570,#129571,#129572,#129573,#129574,#129575,#129576,#129577,
#129578,#129579,#129580,#129581,#129582,#129583,#129584,#129585,#129586,
#129587,#129588,#129589,#129590,#129591,#129592,#129593,#129594,#129595,
#129596,#129597,#129598,#129599,#129600,#129601,#129602,#129603,#129604,
#129605,#129606,#129607,#129608,#129609,#129610,#129611,#129612,#129613,
#129614,#129615,#129616,#129617,#129618,#129619,#129620,#129621,#129622,
#129623,#129624,#129625,#129626,#129627,#129628,#129629,#129630,#129631,
#129632,#129633,#129634,#129635,#129636,#129637,#129638,#129639,#129640,
#129641,#129642,#129643,#129644,#129645,#129646,#129647,#129648,#129649,
#129650,#129651,#129652,#129653,#129654,#129655,#129656,#129657,#129658,
#129659,#129660,#129661,#129662,#129663,#129664,#129665,#129666,#129667,
#129668,#129669,#129670,#129671,#129672,#129673,#129674,#129675,#129676,
#129677,#129678,#129679,#129680,#129681,#129682,#129683,#129684,#129685,
#129686,#129687,#129688,#129689,#129690,#129691,#129692,#129693,#129694,
#129695,#129696,#129697,#129698,#129699,#129700,#129701,#129702,#129703,
#129704,#129705,#129706,#129707,#129708,#129709,#129710,#129711,#129712,
#129713,#129714,#129715,#129716,#129717,#129718,#129719,#129720,#129721,
#129722,#129723,#129724,#129725,#129726,#129727,#129728,#129729,#129730,
#129731,#129732,#129733,#129734,#129735,#129736,#129737,#129738,#129739,
#129740,#129741,#129742,#129743,#129744,#129745,#129746,#129747,#129748,
#129749,#129750,#129751,#129752,#129753,#129754,#129755,#129756,#129757,
#129758,#129759,#129760,#129761,#129762,#129763,#129764,#129765,#129766,
#129767,#129768,#129769,#129770,#129771,#129772,#129773,#129774,#129775,
#129776,#129777,#129778,#129779,#129780,#129781,#129782,#129783,#129784,
#129785,#129786,#129787,#129788,#129789,#129790,#129791,#129792,#129793,
#129794,#129795,#129796,#129797,#129798,#129799,#129800,#129801,#129802,
#129803,#129804,#129805,#129806,#129807,#129808,#129809,#129810,#129811,
#129812,#129813,#129814,#129815,#129816,#129817,#129818,#129819,#129820,
#129821,#129822,#129823,#129824,#129825,#129826,#129827,#129828,#129829,
#129830,#129831,#129832,#129833,#129834,#129835,#129836,#129837,#129838,
#129839,#129840,#129841,#129842,#129843,#129844,#129845,#129846,#129847,
#129848,#129849,#129850,#129851,#129852,#129853,#129854,#129855,#129856,
#129857,#129858,#129859,#129860,#129861,#129862,#129863,#129864,#129865,
#129866,#129867,#129868,#129869,#129870,#129871,#129872,#129873,#129874,
#129875,#129876,#129877,#129878,#129879,#129880,#129881,#129882,#129883,
#129884,#129885,#129886,#129887,#129888,#129889,#129890,#129891,#129892,
#129893,#129894,#129895,#129896,#129897,#129898,#129899,#129900,#129901,
#129902,#129903,#129904,#129905,#129906,#129907,#129908,#129909,#129910,
#129911,#129912,#129913,#129914,#129915,#129916,#129917,#129918,#129919,
#129920,#129921,#129922,#129923,#129924,#129925,#129926,#129927,#129928,
#129929,#129930,#129931,#129932,#129933,#129934,#129935,#129936,#129937,
#129938,#129939,#129940,#129941,#129942,#129943,#129944,#129945,#129946,
#129947,#129948,#129949,#129950,#129951,#129952,#129953,#129954,#129955,
#129956,#129957,#129958,#129959,#129960,#129961,#129962,#129963,#129964,
#129965,#129966,#129967,#129968,#129969,#129970,#129971,#129972,#129973,
#129974,#129975,#129976,#129977,#129978,#129979,#129980,#129981,#129982,
#129983,#129984,#129985,#129986,#129987,#129988,#129989,#129990,#129991,
#129992,#129993,#129994,#129995,#129996,#129997,#129998,#129999,#130000,
#130001,#130002,#130003,#130004,#130005,#130006,#130007,#130008,#130009,
#130010,#130011,#130012,#130013,#130014,#130015,#130016,#130017,#130018,
#130019,#130020,#130021,#130022,#130023,#130024,#130025,#130026,#130027,
#130028,#130029,#130030,#130031,#130032,#130033,#130034,#130035,#130036,
#130037,#130038,#130039,#130040,#130041,#130042,#130043,#130044,#130045,
#130046,#130047,#130048,#130049,#130050,#130051,#130052,#130053,#130054,
#130055,#130056,#130057,#130058,#130059,#130060,#130061,#130062,#130063,
#130064,#130065,#130066,#130067,#130068,#130069,#130070,#130071,#130072,
#130073,#130074,#130075,#130076,#130077,#130078,#130079,#130080,#130081,
#130082,#130083,#130084,#130085,#130086,#130087,#130088,#130089,#130090,
#130091,#130092,#130093,#130094,#130095,#130096,#130097,#130098,#130099,
#130100,#130101,#130102,#130103,#130104,#130105,#130106,#130107,#130108,
#130109,#130110,#130111,#130112,#130113,#130114,#130115,#130116,#130117,
#130118,#130119,#130120,#130121,#130122,#130123,#130124,#130125,#130126,
#130127,#130128,#130129,#130130,#130131,#130132,#130133,#130134,#130135,
#130136,#130137,#130138,#130139,#130140,#130141,#130142,#130143,#130144,
#130145,#130146,#130147,#130148,#130149,#130150,#130151,#130152,#130153,
#130154,#130155,#130156,#130157,#130158,#130159,#130160,#130161,#130162,
#130163,#130164,#130165,#130166,#130167,#130168,#130169,#130170,#130171,
#130172,#130173,#130174,#130175,#130176,#130177,#130178,#130179,#130180,
#130181,#130182,#130183,#130184,#130185,#130186,#130187,#130188,#130189,
#130190,#130191,#130192,#130193,#130194,#130195,#130196,#130197,#130198,
#130199,#130200,#130201,#130202,#130203,#130204,#130205,#130206,#130207,
#130208,#130209,#130210,#130211,#130212,#130213,#130214,#130215,#130216,
#130217,#130218,#130219,#130220,#130221,#130222,#130223,#130224,#130225,
#130226,#130227,#130228,#130229,#130230,#130231,#130232,#130233,#130234,
#130235,#130236,#130237,#130238,#130239,#130240,#130241,#130242,#130243,
#130244,#130245,#130246,#130247,#130248,#130249,#130250,#130251,#130252,
#130253,#130254,#130255,#130256,#130257,#130258,#130259,#130260,#130261,
#130262,#130263,#130264,#130265,#130266,#130267,#130268,#130269,#130270,
#130271,#130272,#130273,#130274,#130275,#130276,#130277,#130278,#130279,
#130280,#130281,#130282,#130283,#130284,#130285,#130286,#130287,#130288,
#130289,#130290,#130291,#130292,#130293,#130294,#130295,#130296,#130297,
#130298,#130299,#130300,#130301,#130302,#130303,#130304,#130305,#130306,
#130307,#130308,#130309,#130310,#130311,#130312,#130313,#130314,#130315,
#130316,#130317,#130318,#130319,#130320,#130321,#130322,#130323,#130324,
#130325,#130326,#130327,#130328,#130329,#130330,#130331,#130332,#130333,
#130334,#130335,#130336,#130337,#130338,#130339,#130340,#130341,#130342,
#130343,#130344,#130345,#130346,#130347,#130348,#130349,#130350,#130351,
#130352,#130353,#130354,#130355,#130356,#130357,#130358,#130359,#130360,
#130361,#130362,#130363,#130364,#130365,#130366,#130367,#130368,#130369,
#130370,#130371,#130372,#130373,#130374,#130375,#130376,#130377,#130378,
#130379,#130380,#130381,#130382,#130383,#130384,#130385,#130386,#130387,
#130388,#130389,#130390,#130391,#130392,#130393,#130394,#130395,#130396,
#130397,#130398,#130399,#130400,#130401,#130402,#130403,#130404,#130405,
#130406,#130407,#130408,#130409,#130410,#130411,#130412,#130413,#130414,
#130415,#130416,#130417,#130418,#130419,#130420,#130421,#130422,#130423,
#130424,#130425,#130426,#130427,#130428,#130429,#130430,#130431,#130432,
#130433,#130434,#130435,#130436,#130437,#130438,#130439,#130440,#130441,
#130442,#130443,#130444,#130445,#130446,#130447,#130448,#130449,#130450,
#130451,#130452,#130453,#130454,#130455,#130456,#130457,#130458,#130459,
#130460,#130461,#130462,#130463,#130464,#130465,#130466,#130467,#130468,
#130469,#130470,#130471,#130472,#130473,#130474,#130475,#130476,#130477,
#130478,#130479,#130480,#130481,#130482,#130483,#130484,#130485,#130486,
#130487,#130488,#130489,#130490,#130491,#130492,#130493,#130494,#130495,
#130496,#130497,#130498,#130499,#130500,#130501,#130502,#130503,#130504,
#130505,#130506,#130507,#130508,#130509,#130510,#130511,#130512,#130513,
#130514,#130515,#130516,#130517,#130518,#130519,#130520,#130521,#130522,
#130523,#130524,#130525,#130526,#130527,#130528,#130529,#130530,#130531,
#130532,#130533,#130534,#130535,#130536,#130537,#130538,#130539,#130540,
#130541,#130542,#130543,#130544,#130545,#130546,#130547,#130548,#130549,
#130550,#130551,#130552,#130553,#130554,#130555,#130556,#130557,#130558,
#130559,#130560,#130561,#130562,#130563,#130564,#130565,#130566,#130567,
#130568,#130569,#130570,#130571,#130572,#130573,#130574,#130575,#130576,
#130577,#130578,#130579,#130580,#130581,#130582,#130583,#130584,#130585,
#130586,#130587,#130588,#130589,#130590,#130591,#130592,#130593,#130594,
#130595,#130596,#130597,#130598,#130599,#130600,#130601,#130602,#130603,
#130604,#130605,#130606,#130607,#130608,#130609,#130610,#130611,#130612,
#130613,#130614,#130615,#130616,#130617,#130618,#130619,#130620,#130621,
#130622,#130623,#130624,#130625,#130626,#130627,#130628,#130629,#130630,
#130631,#130632,#130633,#130634,#130635,#130636,#130637,#130638,#130639,
#130640,#130641,#130642,#130643,#130644,#130645,#130646,#130647,#130648,
#130649,#130650,#130651,#130652,#130653,#130654,#130655,#130656,#130657,
#130658,#130659,#130660,#130661,#130662,#130663,#130664,#130665,#130666,
#130667,#130668,#130669,#130670,#130671,#130672,#130673,#130674,#130675,
#130676,#130677,#130678,#130679,#130680,#130681,#130682,#130683,#130684,
#130685,#130686,#130687,#130688,#130689,#130690,#130691,#130692,#130693,
#130694,#130695,#130696,#130697,#130698,#130699,#130700,#130701,#130702,
#130703,#130704,#130705,#130706,#130707,#130708,#130709,#130710,#130711,
#130712,#130713,#130714,#130715,#130716,#130717,#130718,#130719,#130720,
#130721,#130722,#130723,#130724,#130725,#130726,#130727,#130728,#130729,
#130730,#130731,#130732,#130733,#130734,#130735,#130736,#130737,#130738,
#130739,#130740,#130741,#130742,#130743,#130744,#130745,#130746,#130747,
#130748,#130749,#130750,#130751,#130752,#130753,#130754,#130755,#130756,
#130757,#130758,#130759,#130760,#130761,#130762,#130763,#130764,#130765,
#130766,#130767,#130768,#130769,#130770,#130771,#130772,#130773,#130774,
#130775,#130776,#130777,#130778,#130779,#130780,#130781,#130782,#130783,
#130784,#130785,#130786,#130787),(#130788,#130789,#130790,#130791,#130792,
#130793,#130794,#130795,#130796,#130797,#130798,#130799,#130800,#130801,
#130802,#130803,#130804,#130805,#130806,#130807,#130808,#130809,#130810,
#130811,#130812,#130813,#130814,#130815,#130816,#130817,#130818,#130819,
#130820,#130821,#130822,#130823,#130824,#130825,#130826,#130827,#130828,
#130829,#130830,#130831,#130832,#130833,#130834,#130835,#130836,#130837,
#130838,#130839,#130840,#130841,#130842,#130843,#130844,#130845,#130846,
#130847,#130848,#130849,#130850,#130851,#130852,#130853,#130854,#130855,
#130856,#130857,#130858,#130859,#130860,#130861,#130862,#130863,#130864,
#130865,#130866,#130867,#130868,#130869,#130870,#130871,#130872,#130873,
#130874,#130875,#130876,#130877,#130878,#130879,#130880,#130881,#130882,
#130883,#130884,#130885,#130886,#130887,#130888,#130889,#130890,#130891,
#130892,#130893,#130894,#130895,#130896,#130897,#130898,#130899,#130900,
#130901,#130902,#130903,#130904,#130905,#130906,#130907,#130908,#130909,
#130910,#130911,#130912,#130913,#130914,#130915,#130916,#130917,#130918,
#130919,#130920,#130921,#130922,#130923,#130924,#130925,#130926,#130927,
#130928,#130929,#130930,#130931,#130932,#130933,#130934,#130935,#130936,
#130937,#130938,#130939,#130940,#130941,#130942,#130943,#130944,#130945,
#130946,#130947,#130948,#130949,#130950,#130951,#130952,#130953,#130954,
#130955,#130956,#130957,#130958,#130959,#130960,#130961,#130962,#130963,
#130964,#130965,#130966,#130967,#130968,#130969,#130970,#130971,#130972,
#130973,#130974,#130975,#130976,#130977,#130978,#130979,#130980,#130981,
#130982,#130983,#130984,#130985,#130986,#130987,#130988,#130989,#130990,
#130991,#130992,#130993,#130994,#130995,#130996,#130997,#130998,#130999,
#131000,#131001,#131002,#131003,#131004,#131005,#131006,#131007,#131008,
#131009,#131010,#131011,#131012,#131013,#131014,#131015,#131016,#131017,
#131018,#131019,#131020,#131021,#131022,#131023,#131024,#131025,#131026,
#131027,#131028,#131029,#131030,#131031,#131032,#131033,#131034,#131035,
#131036,#131037,#131038,#131039,#131040,#131041,#131042,#131043,#131044,
#131045,#131046,#131047,#131048,#131049,#131050,#131051,#131052,#131053,
#131054,#131055,#131056,#131057,#131058,#131059,#131060,#131061,#131062,
#131063,#131064,#131065,#131066,#131067,#131068,#131069,#131070,#131071,
#131072,#131073,#131074,#131075,#131076,#131077,#131078,#131079,#131080,
#131081,#131082,#131083,#131084,#131085,#131086,#131087,#131088,#131089,
#131090,#131091,#131092,#131093,#131094,#131095,#131096,#131097,#131098,
#131099,#131100,#131101,#131102,#131103,#131104,#131105,#131106,#131107,
#131108,#131109,#131110,#131111,#131112,#131113,#131114,#131115,#131116,
#131117,#131118,#131119,#131120,#131121,#131122,#131123,#131124,#131125,
#131126,#131127,#131128,#131129,#131130,#131131,#131132,#131133,#131134,
#131135,#131136,#131137,#131138,#131139,#131140,#131141,#131142,#131143,
#131144,#131145,#131146,#131147,#131148,#131149,#131150,#131151,#131152,
#131153,#131154,#131155,#131156,#131157,#131158,#131159,#131160,#131161,
#131162,#131163,#131164,#131165,#131166,#131167,#131168,#131169,#131170,
#131171,#131172,#131173,#131174,#131175,#131176,#131177,#131178,#131179,
#131180,#131181,#131182,#131183,#131184,#131185,#131186,#131187,#131188,
#131189,#131190,#131191,#131192,#131193,#131194,#131195,#131196,#131197,
#131198,#131199,#131200,#131201,#131202,#131203,#131204,#131205,#131206,
#131207,#131208,#131209,#131210,#131211,#131212,#131213,#131214,#131215,
#131216,#131217,#131218,#131219,#131220,#131221,#131222,#131223,#131224,
#131225,#131226,#131227,#131228,#131229,#131230,#131231,#131232,#131233,
#131234,#131235,#131236,#131237,#131238,#131239,#131240,#131241,#131242,
#131243,#131244,#131245,#131246,#131247,#131248,#131249,#131250,#131251,
#131252,#131253,#131254,#131255,#131256,#131257,#131258,#131259,#131260,
#131261,#131262,#131263,#131264,#131265,#131266,#131267,#131268,#131269,
#131270,#131271,#131272,#131273,#131274,#131275,#131276,#131277,#131278,
#131279,#131280,#131281,#131282,#131283,#131284,#131285,#131286,#131287,
#131288,#131289,#131290,#131291,#131292,#131293,#131294,#131295,#131296,
#131297,#131298,#131299,#131300,#131301,#131302,#131303,#131304,#131305,
#131306,#131307,#131308,#131309,#131310,#131311,#131312,#131313,#131314,
#131315,#131316,#131317,#131318,#131319,#131320,#131321,#131322,#131323,
#131324,#131325,#131326,#131327,#131328,#131329,#131330,#131331,#131332,
#131333,#131334,#131335,#131336,#131337,#131338,#131339,#131340,#131341,
#131342,#131343,#131344,#131345,#131346,#131347,#131348,#131349,#131350,
#131351,#131352,#131353,#131354,#131355,#131356,#131357,#131358,#131359,
#131360,#131361,#131362,#131363,#131364,#131365,#131366,#131367,#131368,
#131369,#131370,#131371,#131372,#131373,#131374,#131375,#131376,#131377,
#131378,#131379,#131380,#131381,#131382,#131383,#131384,#131385,#131386,
#131387,#131388,#131389,#131390,#131391,#131392,#131393,#131394,#131395,
#131396,#131397,#131398,#131399,#131400,#131401,#131402,#131403,#131404,
#131405,#131406,#131407,#131408,#131409,#131410,#131411,#131412,#131413,
#131414,#131415,#131416,#131417,#131418,#131419,#131420,#131421,#131422,
#131423,#131424,#131425,#131426,#131427,#131428,#131429,#131430,#131431,
#131432,#131433,#131434,#131435,#131436,#131437,#131438,#131439,#131440,
#131441,#131442,#131443,#131444,#131445,#131446,#131447,#131448,#131449,
#131450,#131451,#131452,#131453,#131454,#131455,#131456,#131457,#131458,
#131459,#131460,#131461,#131462,#131463,#131464,#131465,#131466,#131467,
#131468,#131469,#131470,#131471,#131472,#131473,#131474,#131475,#131476,
#131477,#131478,#131479,#131480,#131481,#131482,#131483,#131484,#131485,
#131486,#131487,#131488,#131489,#131490,#131491,#131492,#131493,#131494,
#131495,#131496,#131497,#131498,#131499,#131500,#131501,#131502,#131503,
#131504,#131505,#131506,#131507,#131508,#131509,#131510,#131511,#131512,
#131513,#131514,#131515,#131516,#131517,#131518,#131519,#131520,#131521,
#131522,#131523,#131524,#131525,#131526,#131527,#131528,#131529,#131530,
#131531,#131532,#131533,#131534,#131535,#131536,#131537,#131538,#131539,
#131540,#131541,#131542,#131543,#131544,#131545,#131546,#131547,#131548,
#131549,#131550,#131551,#131552,#131553,#131554,#131555,#131556,#131557,
#131558,#131559,#131560,#131561,#131562,#131563,#131564,#131565,#131566,
#131567,#131568,#131569,#131570,#131571,#131572,#131573,#131574,#131575,
#131576,#131577,#131578,#131579,#131580,#131581,#131582,#131583,#131584,
#131585,#131586,#131587,#131588,#131589,#131590,#131591,#131592,#131593,
#131594,#131595,#131596,#131597,#131598,#131599,#131600,#131601,#131602,
#131603,#131604,#131605,#131606,#131607,#131608,#131609,#131610,#131611,
#131612,#131613,#131614,#131615,#131616,#131617,#131618,#131619,#131620,
#131621,#131622,#131623,#131624,#131625,#131626,#131627,#131628,#131629,
#131630,#131631,#131632,#131633,#131634,#131635,#131636,#131637,#131638,
#131639,#131640,#131641,#131642,#131643,#131644,#131645,#131646,#131647,
#131648,#131649,#131650,#131651,#131652,#131653,#131654,#131655,#131656,
#131657,#131658,#131659,#131660,#131661,#131662,#131663,#131664,#131665,
#131666,#131667,#131668,#131669,#131670,#131671,#131672,#131673,#131674,
#131675,#131676,#131677,#131678,#131679,#131680,#131681,#131682,#131683,
#131684,#131685,#131686,#131687,#131688,#131689,#131690,#131691,#131692,
#131693,#131694,#131695,#131696,#131697,#131698,#131699,#131700,#131701,
#131702,#131703,#131704,#131705,#131706,#131707,#131708,#131709,#131710,
#131711,#131712,#131713,#131714,#131715,#131716,#131717,#131718,#131719,
#131720,#131721,#131722,#131723,#131724,#131725,#131726,#131727,#131728,
#131729,#131730,#131731,#131732,#131733,#131734,#131735,#131736,#131737,
#131738,#131739,#131740,#131741,#131742,#131743,#131744,#131745,#131746,
#131747,#131748,#131749,#131750,#131751,#131752,#131753,#131754,#131755,
#131756,#131757,#131758,#131759,#131760,#131761,#131762,#131763,#131764,
#131765,#131766,#131767,#131768,#131769,#131770,#131771,#131772,#131773,
#131774,#131775,#131776,#131777,#131778,#131779,#131780,#131781,#131782,
#131783,#131784,#131785,#131786,#131787,#131788,#131789,#131790,#131791,
#131792,#131793,#131794,#131795,#131796,#131797,#131798,#131799,#131800,
#131801,#131802,#131803,#131804,#131805,#131806,#131807,#131808,#131809,
#131810,#131811,#131812,#131813,#131814,#131815,#131816,#131817,#131818,
#131819,#131820,#131821,#131822,#131823,#131824,#131825,#131826,#131827,
#131828,#131829,#131830,#131831,#131832,#131833,#131834,#131835,#131836,
#131837,#131838,#131839,#131840,#131841,#131842,#131843,#131844,#131845,
#131846,#131847,#131848,#131849,#131850,#131851,#131852,#131853,#131854,
#131855,#131856,#131857,#131858,#131859,#131860,#131861,#131862,#131863,
#131864,#131865,#131866,#131867,#131868,#131869,#131870,#131871,#131872,
#131873,#131874,#131875,#131876,#131877,#131878,#131879,#131880,#131881,
#131882,#131883,#131884,#131885,#131886,#131887,#131888,#131889,#131890,
#131891,#131892,#131893,#131894,#131895,#131896,#131897,#131898,#131899,
#131900,#131901,#131902,#131903,#131904,#131905,#131906,#131907,#131908,
#131909,#131910,#131911,#131912,#131913,#131914,#131915,#131916,#131917,
#131918,#131919,#131920,#131921,#131922,#131923,#131924,#131925,#131926,
#131927,#131928,#131929,#131930,#131931,#131932,#131933,#131934,#131935,
#131936,#131937,#131938,#131939,#131940,#131941,#131942,#131943,#131944,
#131945,#131946,#131947,#131948,#131949,#131950,#131951,#131952,#131953,
#131954,#131955,#131956,#131957,#131958,#131959,#131960,#131961,#131962,
#131963,#131964,#131965,#131966,#131967,#131968,#131969,#131970,#131971,
#131972,#131973,#131974,#131975,#131976,#131977,#131978,#131979,#131980,
#131981,#131982,#131983,#131984,#131985,#131986,#131987,#131988,#131989,
#131990,#131991,#131992,#131993,#131994,#131995,#131996,#131997,#131998,
#131999,#132000,#132001,#132002,#132003,#132004,#132005,#132006,#132007,
#132008,#132009,#132010,#132011,#132012,#132013,#132014,#132015,#132016,
#132017,#132018,#132019,#132020,#132021,#132022,#132023,#132024,#132025,
#132026,#132027,#132028,#132029,#132030,#132031,#132032,#132033,#132034,
#132035,#132036,#132037,#132038,#132039,#132040,#132041,#132042,#132043,
#132044,#132045,#132046,#132047,#132048,#132049,#132050,#132051,#132052,
#132053,#132054,#132055,#132056,#132057,#132058,#132059,#132060,#132061,
#132062,#132063,#132064,#132065,#132066,#132067,#132068,#132069,#132070,
#132071,#132072,#132073,#132074,#132075,#132076,#132077,#132078,#132079,
#132080,#132081,#132082,#132083,#132084,#132085,#132086,#132087,#132088,
#132089,#132090,#132091,#132092,#132093,#132094,#132095,#132096,#132097,
#132098,#132099,#132100,#132101,#132102,#132103,#132104,#132105,#132106,
#132107,#132108,#132109,#132110,#132111,#132112,#132113,#132114,#132115,
#132116,#132117,#132118,#132119,#132120,#132121,#132122,#132123,#132124,
#132125,#132126,#132127,#132128,#132129,#132130,#132131,#132132,#132133,
#132134,#132135,#132136,#132137,#132138,#132139,#132140,#132141,#132142,
#132143,#132144,#132145,#132146,#132147,#132148,#132149,#132150,#132151,
#132152,#132153,#132154,#132155,#132156,#132157,#132158,#132159,#132160,
#132161,#132162,#132163,#132164,#132165,#132166,#132167,#132168,#132169,
#132170,#132171,#132172,#132173,#132174,#132175,#132176,#132177,#132178,
#132179,#132180,#132181,#132182,#132183,#132184,#132185,#132186,#132187,
#132188,#132189,#132190,#132191,#132192,#132193,#132194,#132195,#132196,
#132197,#132198,#132199,#132200,#132201,#132202,#132203,#132204,#132205,
#132206,#132207,#132208,#132209,#132210,#132211,#132212,#132213,#132214,
#132215,#132216,#132217,#132218,#132219,#132220,#132221,#132222,#132223,
#132224,#132225,#132226,#132227,#132228,#132229,#132230,#132231,#132232,
#132233,#132234,#132235,#132236,#132237,#132238,#132239,#132240,#132241,
#132242,#132243,#132244,#132245,#132246,#132247,#132248,#132249,#132250,
#132251,#132252,#132253,#132254,#132255,#132256,#132257,#132258,#132259,
#132260,#132261,#132262,#132263,#132264,#132265,#132266,#132267,#132268,
#132269,#132270,#132271,#132272,#132273,#132274,#132275,#132276,#132277,
#132278,#132279,#132280,#132281,#132282,#132283,#132284,#132285,#132286,
#132287,#132288,#132289,#132290,#132291,#132292,#132293,#132294,#132295,
#132296,#132297,#132298,#132299,#132300,#132301,#132302,#132303,#132304,
#132305,#132306,#132307,#132308,#132309,#132310,#132311,#132312,#132313,
#132314,#132315,#132316,#132317,#132318,#132319,#132320,#132321,#132322,
#132323,#132324,#132325,#132326,#132327,#132328,#132329,#132330,#132331,
#132332,#132333,#132334,#132335,#132336,#132337,#132338,#132339,#132340,
#132341,#132342,#132343,#132344,#132345,#132346,#132347,#132348,#132349,
#132350,#132351,#132352,#132353,#132354,#132355,#132356,#132357,#132358,
#132359,#132360,#132361,#132362,#132363,#132364,#132365,#132366,#132367,
#132368,#132369,#132370,#132371,#132372,#132373,#132374,#132375,#132376,
#132377,#132378,#132379,#132380,#132381,#132382,#132383,#132384,#132385,
#132386,#132387,#132388,#132389,#132390,#132391,#132392,#132393,#132394,
#132395,#132396,#132397,#132398,#132399,#132400,#132401,#132402,#132403,
#132404,#132405,#132406,#132407,#132408,#132409,#132410,#132411,#132412,
#132413,#132414,#132415,#132416,#132417,#132418,#132419,#132420,#132421,
#132422,#132423,#132424,#132425,#132426,#132427,#132428,#132429,#132430,
#132431,#132432,#132433,#132434,#132435,#132436,#132437,#132438,#132439,
#132440,#132441,#132442,#132443,#132444,#132445,#132446,#132447,#132448,
#132449,#132450,#132451,#132452,#132453,#132454,#132455,#132456,#132457,
#132458,#132459,#132460,#132461,#132462,#132463,#132464,#132465,#132466,
#132467,#132468,#132469,#132470,#132471,#132472,#132473,#132474,#132475,
#132476,#132477,#132478,#132479,#132480,#132481,#132482,#132483,#132484,
#132485,#132486,#132487,#132488,#132489,#132490,#132491,#132492,#132493,
#132494,#132495,#132496,#132497,#132498,#132499,#132500,#132501,#132502,
#132503,#132504,#132505,#132506,#132507,#132508,#132509,#132510,#132511,
#132512,#132513,#132514,#132515,#132516,#132517,#132518,#132519,#132520,
#132521,#132522,#132523,#132524,#132525,#132526,#132527,#132528,#132529,
#132530,#132531,#132532,#132533,#132534,#132535,#132536,#132537,#132538,
#132539,#132540,#132541,#132542,#132543,#132544,#132545,#132546,#132547,
#132548,#132549,#132550,#132551,#132552,#132553,#132554,#132555,#132556,
#132557,#132558,#132559,#132560,#132561,#132562,#132563,#132564,#132565,
#132566,#132567,#132568,#132569,#132570,#132571,#132572,#132573,#132574,
#132575,#132576,#132577,#132578,#132579,#132580,#132581,#132582,#132583,
#132584,#132585,#132586,#132587,#132588,#132589,#132590,#132591,#132592,
#132593,#132594,#132595,#132596,#132597,#132598,#132599,#132600,#132601,
#132602,#132603,#132604,#132605,#132606,#132607,#132608,#132609,#132610,
#132611,#132612,#132613,#132614,#132615,#132616,#132617,#132618,#132619,
#132620,#132621,#132622,#132623,#132624,#132625,#132626,#132627,#132628,
#132629,#132630,#132631,#132632,#132633,#132634,#132635,#132636,#132637,
#132638,#132639,#132640,#132641,#132642,#132643,#132644,#132645,#132646,
#132647,#132648,#132649,#132650,#132651,#132652,#132653,#132654,#132655,
#132656,#132657,#132658,#132659,#132660,#132661,#132662,#132663,#132664,
#132665,#132666,#132667,#132668,#132669,#132670,#132671,#132672,#132673,
#132674,#132675,#132676,#132677,#132678,#132679,#132680,#132681,#132682,
#132683,#132684,#132685,#132686,#132687,#132688,#132689,#132690,#132691,
#132692,#132693,#132694,#132695,#132696,#132697,#132698,#132699,#132700,
#132701,#132702,#132703,#132704,#132705,#132706,#132707,#132708,#132709,
#132710,#132711,#132712,#132713,#132714,#132715,#132716,#132717,#132718,
#132719,#132720,#132721,#132722,#132723,#132724,#132725,#132726,#132727,
#132728,#132729,#132730,#132731,#132732,#132733,#132734,#132735,#132736,
#132737,#132738,#132739,#132740,#132741,#132742,#132743,#132744,#132745,
#132746,#132747,#132748,#132749,#132750,#132751,#132752,#132753,#132754,
#132755,#132756,#132757,#132758,#132759,#132760,#132761,#132762,#132763,
#132764,#132765,#132766,#132767,#132768,#132769,#132770,#132771,#132772,
#132773,#132774,#132775,#132776,#132777,#132778,#132779,#132780,#132781,
#132782,#132783,#132784,#132785,#132786,#132787,#132788,#132789,#132790,
#132791,#132792,#132793,#132794,#132795,#132796,#132797,#132798,#132799,
#132800,#132801,#132802,#132803,#132804,#132805,#132806,#132807,#132808,
#132809,#132810,#132811,#132812,#132813,#132814,#132815,#132816,#132817,
#132818,#132819,#132820,#132821,#132822,#132823,#132824,#132825,#132826,
#132827,#132828,#132829,#132830,#132831,#132832,#132833,#132834,#132835,
#132836,#132837,#132838)),.UNSPECIFIED.,.T.,.F.,.F.)
B_SPLINE_SURFACE_WITH_KNOTS((3,2,2,2,3),(4,1,1,1,1,1,1,1,1,1,1,1,1,1,1,
1,1,1,1,1,1,1,1,1,1,1,1,1,1,1,1,1,1,1,1,1,1,1,1,1,1,1,1,1,1,1,1,1,1,1,1,
1,1,1,1,1,1,1,1,1,1,1,1,1,1,1,1,1,1,1,1,1,1,1,1,1,1,1,1,1,1,1,1,1,1,1,1,
1,1,1,1,1,1,1,1,1,1,1,1,1,1,1,1,1,1,1,1,1,1,1,1,1,1,1,1,1,1,1,1,1,1,1,1,
1,1,1,1,1,1,1,1,1,1,1,1,1,1,1,1,1,1,1,1,1,1,1,1,1,1,1,1,1,1,1,1,1,1,1,1,
1,1,1,1,1,1,1,1,1,1,1,1,1,1,1,1,1,1,1,1,1,1,1,1,1,1,1,1,1,1,1,1,1,1,1,1,
1,1,1,1,1,1,1,1,1,1,1,1,1,1,1,1,1,1,1,1,1,1,1,1,1,1,1,1,1,1,1,1,1,1,1,1,
1,1,1,1,1,1,1,1,1,1,1,1,1,1,1,1,1,1,1,1,1,1,1,1,1,1,1,1,1,1,1,1,1,1,1,1,
1,1,1,1,1,1,1,1,1,1,1,1,1,1,1,1,1,1,1,1,1,1,1,1,1,1,1,1,1,1,1,1,1,1,1,1,
1,1,1,1,1,1,1,1,1,1,1,1,1,1,1,1,1,1,1,1,1,1,1,1,1,1,1,1,1,1,1,1,1,1,1,1,
1,1,1,1,1,1,1,1,1,1,1,1,1,1,1,1,1,1,1,1,1,1,1,1,1,1,1,1,1,1,1,1,1,1,1,1,
1,1,1,1,1,1,1,1,1,1,1,1,1,1,1,1,1,1,1,1,1,1,1,1,1,1,1,1,1,1,1,1,1,1,1,1,
1,1,1,1,1,1,1,1,1,1,1,1,1,1,1,1,1,1,1,1,1,1,1,1,1,1,1,1,1,1,1,1,1,1,1,1,
1,1,1,1,1,1,1,1,1,1,1,1,1,1,1,1,1,1,1,1,1,1,1,1,1,1,1,1,1,1,1,1,1,1,1,1,
1,1,1,1,1,1,1,1,1,1,1,1,1,1,1,1,1,1,1,1,1,1,1,1,1,1,1,1,1,1,1,1,1,1,1,1,
1,1,1,1,1,1,1,1,1,1,1,1,1,1,1,1,1,1,1,1,1,1,1,1,1,1,1,1,1,1,1,1,1,1,1,1,
1,1,1,1,1,1,1,1,1,1,1,1,1,1,1,1,1,1,1,1,1,1,1,1,1,1,1,1,1,1,1,1,1,1,1,1,
1,1,1,1,1,1,1,1,1,1,1,1,1,1,1,1,1,1,1,1,1,1,1,1,1,1,1,1,1,1,1,1,1,1,1,1,
1,1,1,1,1,1,1,1,1,1,1,1,1,1,1,1,1,1,1,1,1,1,1,1,1,1,1,1,1,1,1,1,1,1,1,1,
1,1,1,1,1,1,1,1,1,1,1,1,1,1,1,1,1,1,1,1,1,1,1,1,1,1,1,1,1,1,1,1,1,1,1,1,
1,1,1,1,1,1,1,1,1,1,1,1,1,1,1,1,1,1,1,1,1,1,1,1,1,1,1,1,1,1,1,1,1,1,1,1,
1,1,1,1,1,1,1,1,1,1,1,1,1,1,1,1,1,1,1,1,1,1,1,1,1,1,1,1,1,1,1,1,1,1,1,1,
1,1,1,1,1,1,1,1,1,1,1,1,1,1,1,1,1,1,1,1,1,1,1,1,1,1,1,1,1,1,1,1,1,1,1,1,
1,1,1,1,1,1,1,1,1,1,1,1,1,1,1,1,1,1,1,1,1,1,1,1,1,1,1,1,1,1,1,1,1,1,1,1,
1,1,1,1,1,1,1,1,1,1,1,1,1,1,1,1,1,1,1,1,1,1,1,1,1,1,1,1,1,1,1,1,1,1,1,1,
1,1,1,1,1,1,1,1,1,1,1,1,1,1,1,1,1,1,1,1,1,1,1,1,1,1,1,1,1,1,1,1,1,1,1,1,
1,1,1,1,1,1,1,1,1,1,1,1,1,1,1,1,1,1,1,1,1,1,1,1,1,1,1,1,1,1,1,1,1,1,1,1,
1,1,1,1,1,1,1,1,1,1,1,1,1,1,1,1,1,1,1,1,1,1,1,1,1,1,1,1,1,1,1,1,1,1,1,1,
1,1,1,1,1,1,1,1,1,1,1,1,1,1,1,1,1,1,1,1,1,1,1,1,1,1,1,1,1,1,1,1,1,1,1,1,
1,1,1,1,1,1,1,1,1,1,1,1,1,1,1,1,1,1,1,1,1,1,1,1,1,1,1,1,1,1,1,1,1,1,1,1,
1,1,1,1,1,1,1,1,1,1,1,1,1,1,1,1,1,1,1,1,1,1,1,1,1,1,1,1,1,1,1,1,1,1,1,1,
1,1,1,1,1,1,1,1,1,1,1,1,1,1,1,1,1,1,1,1,1,1,1,1,1,1,1,1,1,1,1,1,1,1,1,1,
1,1,1,1,1,1,1,1,1,1,1,1,1,1,1,1,1,1,1,1,1,1,1,1,1,1,1,1,1,1,1,1,1,1,1,1,
1,1,1,1,1,1,1,1,1,1,1,1,1,1,1,1,1,1,1,1,1,1,1,1,1,1,1,1,1,1,1,1,1,1,1,1,
1,1,1,1,1,1,1,1,1,1,1,1,1,1,1,1,1,1,1,1,1,1,1,1,1,1,1,1,1,1,1,1,1,1,1,1,
1,1,1,1,1,1,1,1,1,1,1,1,1,1,1,1,1,1,1,1,1,1,1,1,1,1,1,1,1,1,1,1,1,1,1,1,
1,1,1,1,1,1,1,1,1,1,1,1,1,1,1,1,1,1,1,1,1,1,1,1,1,1,1,1,1,1,1,1,1,1,1,1,
1,1,1,1,1,1,1,1,1,1,1,1,1,1,1,1,1,1,1,1,1,1,1,1,1,1,1,1,1,1,1,1,1,1,1,1,
1,1,1,1,1,1,1,1,1,1,1,1,1,1,1,1,1,1,1,1,1,1,1,1,1,1,1,1,1,1,1,1,1,1,1,1,
1,1,1,1,1,1,1,1,1,1,1,1,1,1,1,1,1,1,1,1,1,1,1,1,1,1,1,1,1,1,1,1,1,1,1,1,
1,1,1,1,1,1,1,1,1,1,1,1,1,1,1,1,1,1,1,1,1,1,1,1,1,1,1,1,1,1,1,1,1,1,1,1,
1,1,1,1,1,1,1,1,1,1,1,1,1,1,1,1,1,1,1,1,1,1,1,1,1,1,1,1,1,1,1,1,1,1,1,1,
1,1,1,1,1,1,1,1,1,1,1,1,1,1,1,1,1,1,1,1,1,1,1,1,1,1,1,1,1,1,1,1,1,1,1,1,
1,1,1,1,1,1,1,1,1,1,1,1,1,1,1,1,1,1,1,1,1,1,1,1,1,1,1,1,1,1,1,1,1,1,1,1,
1,1,1,1,1,1,1,1,1,1,1,1,1,1,1,1,1,1,1,1,1,1,1,1,1,1,1,1,1,1,1,1,1,1,1,1,
1,1,1,1,1,1,1,1,1,1,1,1,1,1,1,1,1,1,1,1,1,1,1,1,1,1,1,1,1,1,1,1,1,1,1,1,
1,1,1,1,1,1,1,1,1,1,1,1,1,1,1,1,1,1,1,1,1,1,1,1,1,1,1,1,1,1,1,1,1,1,1,1,
1,1,1,1,1,1,1,1,1,1,1,1,1,1,1,1,1,1,1,1,1,1,1,1,1,1,1,1,1,1,1,1,1,1,1,1,
1,1,1,1,1,1,1,1,1,1,1,1,1,1,1,1,1,1,1,1,1,1,1,1,1,1,1,1,1,1,1,1,1,1,1,1,
1,1,1,1,1,1,1,1,1,1,1,1,1,1,1,1,1,1,1,1,1,1,1,1,1,1,1,1,1,1,1,1,1,1,1,1,
1,1,1,1,1,1,1,1,1,1,1,1,1,1,1,1,1,1,1,1,1,1,1,1,1,1,1,1,1,1,1,1,1,1,1,1,
1,1,1,1,1,1,1,1,1,1,1,1,1,1,1,1,1,1,1,1,1,1,1,1,1,1,1,1,1,1,1,1,1,1,1,1,
1,1,1,1,1,1,1,1,1,1,1,1,1,1,1,1,1,1,1,1,1,1,1,1,1,1,1,1,1,1,1,1,1,1,1,1,
1,1,1,1,1,1,1,1,1,1,1,1,1,1,1,1,1,1,1,1,1,1,1,1,1,1,1,1,1,1,1,1,1,1,1,1,
1,1,1,1,1,1,1,1,1,1,1,1,1,1,1,1,1,1,1,1,1,1,1,1,1,1,1,1,1,1,1,1,1,1,1,1,
1,1,1,1,1,1,1,1,1,1,1,1,1,1,1,1,1,1,1,1,1,1,1,1,1,1,1,1,1,1,1,1,1,1,1,1,
1,1,1,1,1,1,1,1,1,1,1,1,1,1,1,1,1,1,1,1,1,1,1,1,1,1,1,1,1,1,1,1,1,1,1,1,
1,1,1,1,1,1,1,1,1,1,1,1,1,1,1,1,1,4),(0.,0.117809724509617,0.235619449019234,
0.353429173528852,0.471238898038469),(0.,0.01797683372391,0.286633051710584,
0.555289278308216,0.823945516665782,1.09260176953922,1.36125803873948,1.62991432588463,
1.89857063164012,2.16722695661301,2.43588330050525,2.70453966304674,2.9731960431531,
3.24185243981471,3.51050885133453,3.77916527610465,4.04782171198515,4.31647815691489,
4.58513460847725,4.85379106430677,5.12244752187208,5.39110397865606,5.65976043217153,
5.92841687990537,6.19707331956994,6.46572974881596,6.73438616570634,7.00304256821933,
7.2716989549161,7.5403553242696,7.809011675483,8.07766800769526,8.34632432089157,
8.61498061505147,8.8836368910788,9.15229314997201,9.4209493936865,9.68960562442157,
9.95826184531348,10.226918059948,10.4955742727586,10.7642304884925,11.0328867113173,
11.3015429448574,11.5701991918227,11.8388554546081,12.1075117346518,12.3761680332469,
12.6448243507434,12.9134806874637,13.1821370428496,13.450793416388,13.7194498067883,
13.9881062128412,14.2567626326955,14.5254190645885,14.7940755062772,15.0627319555912,
15.3313884100611,15.6000448672586,15.8687013246492,16.1373577797,16.4060142299691,
16.6746706729765,16.9433271065265,17.2119835283531,17.4806399366567,17.7492963295502,
18.0179527057767,18.286609063996,18.555265403637,18.8239217240786,19.0925780255742,
19.3612343083975,19.6298905737625,19.898546823017,20.1672030584666,20.4358592827168,
20.7045154992928,20.973171712245,21.2418279262962,21.5104841459723,21.7791403749736,
22.0477966165324,22.316452872948,22.585109146262,22.8537654375589,23.1224217478187,
23.3910780770929,23.6597344254327,23.9283907920352,24.197047176159,24.4657035763222,
24.7343599911301,25.0030164185931,25.2716728568073,25.5403293034427,25.8089857562333,
26.0776422126729,26.3462986702843,26.6149551265448,26.8836115789212,27.1522680250308,
27.4209244624423,27.6895808890659,27.9582373027346,28.2268937018004,28.4955500845261,
28.7642064498512,29.0328627966379,29.3015191245544,29.5701754332357,29.838831723217,
30.1074879950829,30.3761442503694,30.6448004907916,30.9134567190168,31.1821129380756,
31.450769151893,31.7194253649682,31.9880815819663,32.2567378070174,32.5253940433706,
32.7940502938785,33.0627065604467,33.3313628447765,33.6000191476151,33.8686754696427,
34.1373318106287,34.405988170366,34.6746445478242,34.9433009420458,35.2119573513747,
35.480613774244,35.7492702085419,36.0179266522368,36.2865831029275,36.5552395582669,
36.8238960157264,37.0925524727952,37.3612089269773,37.6298653757534,37.8985218168153,
38.1671782477952,38.4358346667239,38.7044910715485,38.9731474607866,39.2418038328672,
39.5104601869391,39.7791165220837,40.0477728382212,40.3164291352602,40.5850854140292,
40.8537416754418,41.1223979213679,41.3910541539077,41.6597103761025,41.9283665914244,
42.1970228042084,42.4656790192,42.7343352406829,43.0029914723808,43.2716477171096,
43.540303977354,43.8089602546436,44.0776165503516,44.3462728649052,44.614929198697,
44.883585551232,45.1522419220568,45.4208983099307,45.6895547136931,45.9582111315299,
46.2268675617156,46.4955240020317,46.7641804503338,47.0328369041642,47.3014933611089,
47.5701498186329,47.8388062742058,48.107462725373,48.3761191696448,48.6447756048012,
48.9134320285537,49.1820884390673,49.4507448344197,49.7194012133072,49.9880575743413,
50.2567139168934,50.5253702402807,50.7940265446884,51.0626828303152,51.3313390982961,
51.5999953498901,51.8686515873141,52.1373078130706,52.4059640305862,52.6746202437936,
52.9432764573682,53.211932675918,53.480588903259,53.7492451427202,54.0179013967021,
54.2865576673334,54.5552139557853,54.823870263115,55.0925265894471,55.3611829348992,
55.6298392987282,55.8984956802486,56.1671520780245,56.4358084907065,56.7044649163381,
56.9731213530494,57.2417777985307,57.5104342505384,57.7790907065743,58.0477471641719,
58.3164036208043,58.5850600739368,58.8537165211707,59.1223729600609,59.39102938849,
59.6596858042645,59.9283422056975,60.1969985910129,60.4656549590995,60.7343113087676,
61.0029676396243,61.2716239512389,61.540280244075,61.808936518638,62.0775927763821,
62.3462490189291,62.6149052488546,62.8835614690812,63.1522176834332,63.4208738963055,
63.6895301124163,63.9581863359981,64.2268425704115,64.4954988186027,64.7641550825741,
65.0328113641112,65.3014676640435,65.5701239831253,65.8387803211949,66.1074366781083,
66.3760930528907,66.6447494446373,66.9134058517341,67.1820622726558,67.4507187053199,
67.7193751477252,67.988031597487,68.256688052277,68.5253445095709,68.7940009668648,
69.0626574216546,69.3313138714164,69.5999703138218,69.8686267464858,70.1372831674076,
70.4059395745042,70.6745959662509,70.9432523410334,71.2119086979469,71.4805650360164,
71.7492213550982,72.0178776550306,72.2865339365675,72.5551902005389,72.8238464487301,
73.0925026831433,73.3611589067251,73.6298151228357,73.8984713357081,74.1671275500599,
74.4357837702864,74.7044400002118,74.9730962427587,75.2417525005027,75.5104087750655,
75.7790650679015,76.047721379516,76.3163777103726,76.5850340600405,76.853690428127,
77.1223468134422,77.391003214875,77.6596596306495,77.9283160590784,78.1969724979684,
78.4656289452021,78.7342853983344,79.0029418549666,79.2715983125641,79.5402547685998,
79.8089112206075,80.0775676660886,80.3462241027997,80.6148805284312,80.8835369411131,
81.1521933388889,81.4208497204091,81.689506084238,81.9581624296899,82.2268187560219,
82.4954750633515,82.7641313518033,83.0327876224345,83.3014438764161,83.5701001158772,
83.838756343218,84.1074125617677,84.3760687753422,84.6447249885494,84.913381206065,
85.1820374318212,85.4506936692451,85.719349920839,85.9880061888197,86.2566624744465,
86.5253187788541,86.7939751022413,87.0626314447932,87.3312878058273,87.5999441847146,
87.8686005800667,88.1372569905802,88.4059134143327,88.6745698494889,88.9432262937606,
89.2118827449277,89.4805392005005,89.7491956580243,90.0178521149689,90.2865085687992,
90.5551650171012,90.8238214574172,91.0924778876028,91.3611343054394,91.6297907092016,
91.8984470970753,92.1671034679,92.4357598204347,92.7044161542264,92.9730724687798,
93.2417287644878,93.5103850417773,93.7790413020216,94.0476975467502,94.3163537784479,
94.5850099999307,94.8536662149221,95.1223224277061,95.390978643028,95.6596348652226,
95.9282910977624,96.1969473436883,96.4656036051009,96.7342598838697,97.0029161809086,
97.2715724970461,97.5402288321905,97.8088851862623,98.0775415583427,98.3461979475807,
98.6148543524051,98.8835107713336,99.1521672023136,99.4208236433754,99.6894800921513,
99.9581365463333,100.226793003402,100.495449460861,100.7641059162,101.032762366891,
101.301418810586,101.570075244884,101.838731667753,102.107388077082,102.376044471303,
102.644700848761,102.913357208498,103.182013549484,103.450669871511,103.71932617435,
103.98798245868,104.256638725248,104.525294975755,104.793951212108,105.062607437159,
105.331263654157,105.599919867233,105.86857608105,106.137232300108,106.405888528334,
106.674544768756,106.943201024042,107.211857295908,107.480513585889,107.74916989457,
108.017826222487,108.286482569273,108.555138934598,108.823795317324,109.09245171639,
109.361108130058,109.629764556682,109.898420994093,110.167077440202,110.435733892579,
110.704390348839,110.97304680645,111.24170326289,111.51035971568,111.779016162316,
112.04767260053,112.316329027993,112.5849854428,112.853641842963,113.122298227087,
113.39095459369,113.659610942029,113.928267271303,114.196923581563,114.46557987286,
114.734236146174,115.002892402589,115.271548644148,115.540204873149,115.808861092825,
116.077517306876,116.346173519828,116.614829736404,116.883485960654,117.152142196103,
117.420798445358,117.689454710722,117.958110993546,118.226767295041,118.495423615483,
118.764079955123,119.032736313343,119.301392689569,119.570049082462,119.838705490766,
120.107361912592,120.376018346142,120.644674789149,120.913331239418,121.181987694469,
121.45064415186,121.719300609057,121.987957063527,122.256613512841,122.525269954529,
122.793926386422,123.062582806276,123.331239212329,123.599895602729,123.868551976268,
124.137208331653,124.405864668374,124.67452098587,124.943177284465,125.211833564508,
125.480489827294,125.749146074259,126.017802307799,126.286458530624,126.555114746357,
126.823770959168,127.092427173802,127.361083394694,127.629739625429,127.898395869143,
128.167052128037,128.435708404064,128.704364698224,128.97302101142,129.241677343633,
129.510333694846,129.7789900642,130.047646450897,130.31630285341,130.5849592703,
130.853615699547,131.122272139211,131.390928586945,131.659585040461,131.928241497245,
132.19689795481,132.46555441064,132.734210862202,133.002867307132,133.271523743013,
133.540180167783,133.808836579303,134.077492975965,134.346149356071,134.614805718613,
134.883462062505,135.152118387478,135.420774693234,135.689430980379,135.958087249579,
136.226743502453,136.49539974081,136.76405596741,137.032712185392,137.301368398783,
137.570024612174,137.838680830155,138.107337056755,138.375993295112,138.644649547986,
138.913305817186,139.181962104332,139.450618410087,139.71927473506,139.987931078952,
140.256587441494,140.525243821601,140.793900218262,141.062556629782,141.331213054552,
141.599869490433,141.868525935363,142.137182386925,142.405838842755,142.67449530032,
142.943151757104,143.21180821062,143.480464658354,143.749121098019,144.017777527265,
144.286433944155,144.555090346668,144.823746733365,145.092403102719,145.361059453932,
145.629715786145,145.898372099341,146.167028393501,146.435684669529,146.704340928422,
146.972997172137,147.241653402872,147.510309623764,147.778965838398,148.047622051209,
148.316278266943,148.584934489768,148.853590723308,149.122246970274,149.390903233059,
149.659559513103,149.928215811698,150.196872129195,150.465528465915,150.734184821301,
151.00284119484,151.27149758524,151.540153991293,151.808810411148,152.077466843041,
152.34612328473,152.614779734044,152.883436188514,153.152092645711,153.420749103102,
153.689405558153,153.958062008422,154.22671845143,154.49537488498,154.764031306806,
155.03268771511,155.301344108004,155.57000048423,155.838656842449,156.107313182091,
156.375969502532,156.644625804028,156.913282086851,157.181938352216,157.450594601471,
157.719250836921,157.987907061171,158.256563277747,158.525219490699,158.793875704751,
159.062531924427,159.331188153428,159.599844394987,159.868500651403,160.137156924717,
160.405813216014,160.674469526274,160.943125855548,161.211782203888,161.480438570491,
161.749094954615,162.017751354778,162.286407769586,162.555064197049,162.823720635263,
163.092377081899,163.361033534689,163.629689991129,163.898346448741,164.167002905001,
164.435659357378,164.704315803488,164.972972240899,165.241628667523,165.510285081192,
165.778941480257,166.047597862983,166.316254228308,166.584910575095,166.853566903012,
167.122223211693,167.390879501675,167.659535773541,167.928192028827,168.19684826925,
168.465504497475,168.734160716534,169.002816930351,169.271473143427,169.540129360425,
169.808785585476,170.077441821829,170.346098072337,170.614754338905,170.883410623235,
171.152066926074,171.420723248102,171.689379589088,171.958035948825,172.226692326284,
172.495348720505,172.764005129834,173.032661552704,173.301317987002,173.569974430697,
173.838630881388,174.107287336727,174.375943794187,174.644600251255,174.913256705437,
175.181913154214,175.450569595276,175.719226026256,175.987882445184,176.256538850009,
176.525195239247,176.793851611328,177.0625079654,177.331164300545,177.599820616682,
177.868476913721,178.137133192491,178.405789453903,178.674445699829,178.943101932369,
179.211758154564,179.480414369886,179.74907058267,180.017726797662,180.286383019145,
180.555039250843,180.823695495572,181.092351755816,181.361008033106,181.629664328814,
181.898320643368,182.16697697716,182.435633329695,182.70428970052,182.972946088394,
183.241602492156,183.510258909993,183.778915340179,184.047571780495,184.316228228797,
184.584884682628,184.853541139572,185.122197597096,185.39085405267,185.659510503837,
185.928166948109,186.196823383265,186.465479807018,186.734136217531,187.002792612884,
187.271448991771,187.540105352806,187.808761695358,188.077418018745,188.346074323153,
188.61473060878,188.883386876761,189.152043128355,189.420699365779,189.689355591536,
189.958011809051,190.226668022259,190.495324235834,190.763980454383,191.032636681725,
191.301292921186,191.569949175168,191.838605445799,192.107261734251,192.375918041581,
192.644574367913,192.913230713365,193.181887077194,193.450543458715,193.719199856491,
193.987856269173,194.256512694805,194.525169131516,194.793825576997,195.062482029005,
195.331138485041,195.599794942639,195.868451399271,196.137107852404,196.405764299638,
196.674420738528,196.943077166957,197.211733582732,197.480389984165,197.749046369481,
198.017702737567,198.286359087236,198.555015418092,198.823671729707,199.092328022543,
199.360984297106,199.62964055485,199.898296797397,200.166953027323,200.43560924755,
200.704265461902,200.972921674774,201.241577890885,201.510234114467,201.77889034888,
202.047546597072,202.316202861043,202.584859142581,202.853515442513,203.122171761595,
203.390828099665,203.659484456579,203.928140831361,204.196797223108,204.465453630205,
204.734110051127,205.002766483791,205.271422926197,205.540079375959,205.808735830749,
206.077392288043,206.346048745337,206.614705200127,206.883361649889,207.152018092295,
207.420674524959,207.689330945881,207.957987352978,208.226643744725,208.495300119508,
208.763956476421,209.032612814491,209.301269133573,209.569925433505,209.838581715043,
210.107237979014,210.375894227206,210.644550461619,210.913206685201,211.181862901312,
211.450519114184,211.719175328536,211.987831548763,212.256487778689,212.525144021236,
212.79380027898,213.062456553543,213.331112846379,213.599769157994,213.868425488851,
214.137081838519,214.405738206606,214.674394591921,214.943050993354,215.211707409129,
215.480363837558,215.749020276448,216.017676723682,216.286333176815,216.554989633447,
216.823646091045,217.092302547081,217.360958999089,217.62961544457,217.898271881281,
218.166928306913,218.435584719595,218.704241117371,218.972897498892,219.241553862721,
219.510210208173,219.778866534505,220.047522841835,220.316179130287,220.584835400918,
220.8534916549,221.122147894361,221.390804121702,221.659460340252,221.928116553827,
222.196772767034,222.46542898455,222.734085210306,223.00274144773,223.271397699324,
223.540053967305,223.808710252932,224.07736655734,224.346022880728,224.61467922328,
224.883335584314,225.151991963201,225.420648358554,225.689304769068,225.95796119282,
226.226617627977,226.495274072249,226.763930523416,227.032586978989,227.301243436513,
227.569899893458,227.838556347288,228.10721279559,228.375869235907,228.644525666093,
228.913182083929,229.181838487692,229.450494875566,229.719151246391,229.987807598926,
230.256463932718,230.525120247271,230.79377654298,231.062432820269,231.331089080514,
231.599745325243,231.868401556941,232.137057778424,232.405713993415,232.674370206199,
232.943026421521,233.211682643716,233.480338876256,233.748995122182,234.017651383595,
234.286307662364,234.554963959403,234.823620275541,235.092276610685,235.360932964757,
235.629589336838,235.898245726076,236.166902130901,236.43555854983,236.70421498081,
236.972871421872,237.241527870648,237.51018432483,237.778840781899,238.047497239359,
238.316153694698,238.584810145389,238.853466589084,239.122123023382,239.390779446251,
239.65943585558,239.928092249802,240.19674862726,240.465404986998,240.734061327984,
241.002717650011,241.27137395285,241.54003023718,241.808686503748,242.077342754256,
242.345998990609,242.614655215661,242.883311432659,243.151967645734,243.420623859552,
243.68928007861,243.957936306836,244.226592547258,244.495248802545,244.763905074411,
245.032561364392,245.301217673074,245.56987400099,245.838530347777,246.107186713102,
246.375843095828,246.644499494894,246.913155908563,247.181812335186,247.450468772598,
247.719125218708,247.987781671084,248.256438127345,248.525094584956,248.793751041396,
249.062407494187,249.331063940822,249.599720379036,249.8683768065,250.137033221308,
250.405689621471,250.674346005595,250.943002372197,251.211658720537,251.480315049812,
251.748971360071,252.017627651368,252.286283924683,252.554940181098,252.823596422657,
253.092252651658,253.360908871335,253.629565085386,253.898221298338,254.166877514914,
254.435533739165,254.704189974614,254.972846223869,255.241502489234,255.510158772057,
255.778815073553,256.047471393995,256.316127733635,256.584784091854,256.85344046808,
257.122096860973,257.390753269276,257.659409691102,257.928066124652,258.196722567659,
258.465379017928,258.734035472978,259.002691930368,259.271348387566,259.540004842035,
259.808661291349,260.077317733037,260.345974164929,260.614630584783,260.883286990836,
261.151943381235,261.420599754774,261.689256110159,261.957912446879,262.226568764375,
262.49522506297,262.763881343014,263.032537605798,263.301193852763,263.569850086303,
263.838506309127,264.107162524861,264.375818737671,264.644474952305,264.913131173196,
265.181787403931,265.450443647645,265.719099906538,265.987756182565,266.256412476724,
266.52506878992,266.793725122132,267.062381473345,267.331037842698,267.599694229394,
267.868350631907,268.137007048797,268.405663478042,268.674319917706,268.94297636544,
269.211632818955,269.480289275739,269.748945733304,270.017602189133,270.286258640695,
270.554915085624,270.823571521504,271.092227946274,271.360884357793,271.629540754454,
271.89819713456,272.166853497101,272.435509840993,272.704166165965,272.97282247172,
273.241478758865,273.510135028065,273.778791280938,274.047447519295,274.316103745894,
274.584759963875,274.853416177266,275.122072390656,275.390728608637,275.659384835237,
275.928041073593,276.196697326466,276.465353595666,276.734009882811,277.002666188566,
277.271322513539,277.53997885743,277.808635219972,278.077291600077,278.345947996739,
278.614604408258,278.883260833028,279.151917268908,279.420573713837,279.689230165399,
279.957886621228,280.226543078793,280.495199535576,280.763855989092,281.032512436825,
281.301168876489,281.569825305735,281.838481722625,282.107138125138,282.375794511834,
282.644450881187,282.9131072324,283.181763564612,283.450419877808,283.719076171967,
283.987732447994,284.256388706887,284.525044950601,284.793701181336,285.062357402228,
285.331013616862,285.599669829672,285.868326045405,286.136982268229,286.405638501769,
286.674294748734,286.942951011519,287.211607291562,287.480263590157,287.748919907653,
288.017576244373,288.286232599758,288.554888973296,288.823545363696,289.092201769749,
289.360858189603,289.629514621495,289.898171063183,290.166827512497,290.435483966966,
290.704140424163,290.972796881554,291.241453336604,291.510109786873,291.77876622988,
292.047422663429,292.316079085255,292.584735493559,292.853391886452,293.122048262678,
293.390704620897,293.659360960537,293.928017280978,294.196673582474,294.465329865297,
294.733986130661,295.002642379915,295.271298615364,295.539954839614,295.808611056189,
296.077267269141,296.345923483192,296.614579702867,296.883235931868,297.151892173427,
297.420548429842,297.689204703155,297.957860994452,298.226517304711,298.495173633985,
298.763829982324,299.032486348927,299.30114273305,299.569799133212,299.83845554802,
300.107111975482,300.375768413696,300.644424860331,300.913081313121,301.181737769561,
301.450394227172,301.719050683432,301.987707135808,302.256363581917,302.525020019328,
302.793676445951,303.062332859619,303.330989258684,303.59964564141,303.868302006734,
304.136958353521,304.405614681437,304.674270990118,304.942927280098,305.211583551964,
305.48023980725,305.748896047671,306.017552275896,306.286208494954,306.554864708772,
306.823520921846,307.092177138844,307.360833363895,307.629489600247,307.898145850755,
308.166802117323,308.435458401652,308.70411470449,308.972771026517,309.241427367503,
309.51008372724,309.778740104698,310.047396498919,310.316052908247,310.584709331116,
310.853365765414,311.122022209108,311.390678659798,311.659335115137,311.927991572596,
312.196648029665,312.465304483846,312.733960932622,313.002617373684,313.271273804663,
313.539930223591,313.808586628416,314.077243017653,314.345899389733,314.614555743805,
314.883212078949,315.151868395086,315.420524692125,315.689180970894,315.957837232306,
316.226493478231,316.495149710771,316.763805932965,317.032462148286,317.30111836107,
317.569774576061,317.838430797543,318.107087029241,318.375743273969,318.644399534213,
318.913055811502,319.18171210721,319.450368421763,319.719024755555,319.987681108089,
320.256337478914,320.524993866787,320.793650270549,321.062306688385,321.33096311857,
321.599619558886,321.868276007188,322.136932461018,322.405588917962,322.674245375486,
322.942901831059,323.211558282225,323.480214726497,323.748871161653,324.017527585405,
324.286183995918,324.55484039127,324.823496770157,325.09215313119,325.360809473742,
325.629465797129,325.898122101536,326.166778387163,326.435434655143,326.704090906737,
326.97274714416,327.241403369916,327.510059587432,327.778715800638,328.047372014213,
328.316028232762,328.584684460102,328.853340699563,329.121996953545,329.390653224175,
329.659309512627,329.927965819956,330.196622146288,330.46527849174,330.733934855568,
331.002591237088,331.271247634863,331.539904047545,331.808560473176,332.077216909887,
332.345873355368,332.614529807375,332.883186263411,333.151842721008,333.42049917764,
333.689155630772,333.957812078005,334.226468516895,334.495124945324,334.763781361098,
335.03243776253,335.301094147845,335.569750515931,335.838406865599,336.107063196455,
336.375719508069,336.644375800905,336.913032075468,337.181688333211,337.450344575758,
337.719000805683,337.987657025909,338.256313240261,338.524969453133,338.793625669243,
339.062281892824,339.330938127237,339.599594375428,339.868250639399,340.136906920936,
340.405563220868,340.674219539949,340.942875878019,341.211532234932,341.480188609714,
341.74884500146,342.017501408557,342.286157829478,342.554814262142,342.823470704547,
343.092127154308,343.360783609098,343.629440066391,343.898096523685,344.166752978475,
344.435409428236,344.704065870641,344.972722303305,345.241378724226,345.510035131323,
345.778691523069,346.047347897851,346.316004254764,346.584660592834,346.853316911915,
347.121973211847,347.390629493384,347.659285757355,347.927942005546,348.196598239959,
348.46525446354,348.733910679651,349.002566892523,349.271223106874,349.5398793271,
349.808535557025,350.077191799572,350.345848057315,350.614504331878,350.883160624714,
351.151816936328,351.420473267184,351.689129616852,351.957785984938,352.226442370253,
352.495098771685,352.76375518746,353.032411615888,353.301068054778,353.569724502012,
353.838380955144,354.107037411776,354.375693869373,354.644350325408,354.913006777416,
355.181663222896,355.450319659607,355.718976085238,355.98763249792,356.256288895695,
356.524945277215,356.793601641044,357.062257986496,357.330914312827,357.599570620156,
357.868226908608,358.136883179239,358.40553943322,358.674195672681,358.942851900021,
359.211508118571,359.480164332145,359.748820545352,360.017476762867,360.286132988623,
360.554789226047,360.82344547764,361.09210174562,361.360758031247,361.629414335654,
361.898070659041,362.166727001593,362.435383362626,362.704039741513,362.972696136865,
363.241352547378,363.510008971131,363.778665406287,364.047321850558,364.315978301725,
364.584634757297,364.853291214821,365.121947671765,365.390604125595,365.659260573897,
365.927917014213,366.196573444398,366.465229862234,366.733886265996,367.002542653869,
367.271199024694,367.539855377228,367.808511711019,368.077168025573,368.34582432128,
368.614480598569,368.883136858813,369.151793103542,369.420449335239,369.689105556722,
369.957761771713,370.226417984496,370.495074199818,370.763730422012,371.032386654551,
371.301042900477,371.569699161889,371.838355440658,372.107011737697,372.375668053834,
372.644324388978,372.912980743049,373.18163711513,373.450293504367,373.718949909191,
373.98760632812,374.256262759099,374.524919200161,374.793575648936,375.062232103118,
375.330888560186,375.599545017646,375.868201472985,376.136857923675,376.40551436737,
376.674170801667,376.942827224536,377.211483633864,377.480140028085,377.748796405543,
378.01745276528,378.286109106266,378.554765428293,378.823421731131,379.092078015461,
379.360734282028,379.629390532536,379.898046768888,380.166702993939,380.435359210937,
380.704015424011,380.972671637828,381.241327856887,381.509984085112,381.778640325533,
382.047296580819,382.315952852685,382.584609142666,382.853265451347,383.121921779263,
383.390578126049,383.659234491374,383.927890874099,384.196547273165,384.465203686833,
384.733860113456,385.002516550867,385.271172996977,385.539829449352,385.808485905613,
386.077142363224,386.345798819663,386.614455272453,386.883111719088,387.151768157302,
387.420424584764,387.689080999572,387.957737399735,388.226393783858,388.49505015046,
388.7637064988,389.032362828074,389.301019138333,389.56967542963,389.838331702943,
390.106987959358,390.375644200917,390.644300429918,390.912956649593,391.181612863644,
391.450269076596,391.718925293171,391.987581517421,392.25623775287,392.524894002124,
392.793550267489,393.062206550312,393.330862851807,393.599519172248,393.868175511888,
394.136831870107,394.405488246334,394.674144639227,394.94280104753,395.211457469356,
395.480113902905,395.748770345913,396.017426796181,396.286083251232,396.554739708622,
396.823396165819,397.092052620289,397.360709069602,397.629365511291,397.898021943183,
398.166678363037,398.43533476909,398.703991159489,398.972647533028,399.241303888413,
399.509960225133,399.778616542629,400.047272841224,400.315929121267,400.584585384052,
400.853241631017,401.121897864557,401.390554087381,401.659210303115,401.927866515925,
402.196522730559,402.465178951451,402.733835182185,403.002491425899,403.271147684792,
403.539803960819,403.808460254978,404.077116568174,404.345772900386,404.614429251599,
404.883085620952,405.151742007649,405.420398410161,405.689054827051,405.957711256297,
406.226367695961,406.495024143695,406.76368059721,407.032337053993,407.300993511558,
407.569649967387,407.838306418949,408.106962863879,408.375619299759,408.644275724528,
408.912932136048,409.181588532709,409.450244912815,409.718901275356,409.987557619248,
410.25621394422,410.524870249975,410.79352653712,411.06218280632,411.330839059193,
411.599495297549,411.868151524149,412.13680774213,412.40546395552,412.674120168911,
412.942776386892,413.211432613491,413.480088851848,413.748745104721,414.017401373921,
414.286057661065,414.55471396682,414.823370291793,415.092026635685,415.360682998226,
415.629339378332,415.897995774993,416.166652186512,416.435308611282,416.703965047162,
416.972621492092,417.241277943654,417.509934399483,417.778590857048,418.047247313831,
418.315903767346,418.58456021508,418.853216654744,419.121873083989,419.390529500879,
419.659185903392,419.927842290088,420.196498659441,420.465155010654,420.733811342866,
421.002467656062,421.271123950222,421.539780226249,421.808436485141,422.077092728855,
422.34574895959,422.614405180482,422.883061395116,423.151717607926,423.42037382366,
423.689030046484,423.957686280024,424.226342526988,424.494998789773,424.763655069817,
425.032311368411,425.300967685907,425.569624022627,425.838280378013,426.106936751551,
426.375593141951,426.644249548003,426.912905967857,427.18156239975,427.450218841438,
427.718875290752,427.987531745221,428.256188202418,428.524844659809,428.793501114859,
429.062157565128,429.330814008135,429.599470441684,429.868126863511,430.136783271814,
430.405439664707,430.674096040933,430.942752399152,431.211408738792,431.480065059233,
431.748721360729,432.017377643552,432.286033908916,432.554690158171,432.823346393619,
433.092002617869,433.360658834445,433.629315047397,433.897971261447,434.166627481123,
434.435283710124,434.703939951682,434.972596208097,435.241252481411,435.509908772707,
435.778565082967,436.047221412241,436.31587776058,436.584534127182,436.853190511305,
437.121846911468,437.390503326275,437.659159753738,437.927816191952,438.196472638587,
438.465129091377,438.733785547816,439.002442005427,439.271098461688,439.539754914064,
439.808411360173,440.077067797584,440.345724224207,440.614380637875,440.883037036941,
441.151693419666,441.420349784991,441.689006131777,441.957662459693,442.226318768374,
442.494975058355,442.763631330221,443.032287585506,443.300943825928,443.569600054153,
443.838256273211,444.106912487028,444.375568700103,444.644224917101,444.912881142151,
445.181537378504,445.450193629011,445.718849895579,445.987506179909,446.256162482747,
446.524818804774,446.79347514576,447.062131505496,447.330787882954,447.599444277176,
447.868100686504,448.136757109373,448.40541354367,448.674069987365,448.942726438055,
449.211382893394,449.480039350853,449.748695807921,450.017352262103,450.286008710879,
450.55466515194,450.82332158292,451.091978001848,451.360634406672,451.62929079591,
451.89794716799,452.166603522061,452.435259857205,452.703916173343,452.972572470381,
453.24122874915,453.509885010562,453.778541256488,454.047197489028,454.315853711222,
454.584509926543,454.853166139327,455.121822354318,455.3904785758,455.659134807498,
455.927791052226,456.19644731247,456.465103589759,456.733759885467,457.00241620002,
457.271072533811,457.539728886346,457.80838525717,458.077041645044,458.345698048806,
458.614354466642,458.883010896827,459.151667337143,459.420323785445,459.688980239275,
459.957636696219,460.226293153743,460.494949609316,460.763606060482,461.032262504754,
461.300918939909,461.569575363662,461.838231774175,462.106888169527,462.375544548414,
462.644200909447,462.912857251999,463.181513575386,463.450169879794,463.71882616542,
463.987482433401,464.256138684994,464.524794922418,464.793451148174,465.062107365689,
465.330763578896,465.59941979247,465.86807601102,466.13673223836,466.405388477821,
466.674044731802,466.942701002433,467.211357290885,467.480013598214,467.748669924546,
468.017326269997,468.285982633826,468.554639015346,468.823295413121,469.091951825803,
469.360608251434,469.629264688145,469.897921133626,470.166577585633,470.435234041669,
470.703890499266,470.972546955898,471.24120340903,471.509859856263,471.778516295153,
472.047172723582,472.315829139356,472.584485540789,472.853141926103,473.12179829419,
473.390454643857,473.659110974714,473.927767286328,474.196423579164,474.465079853726,
474.73373611147,475.002392354016,475.271048583941,475.539704804167,475.808361018519,
476.077017231391,476.345673447501,476.614329671083,476.882985905496,477.151642153686,
477.420298417658,477.688954699194,477.957610999126,478.226267318208,478.494923656277,
478.76358001319,479.032236387973,479.300892779719,479.569549186815,479.838205607737,
480.106862040401,480.375518482806,480.644174932567,480.912831387357,481.18148784465,
481.450144301944,481.718800756733,481.987457206495,482.2561136489,482.524770081563,
482.793426502485,483.062082909582,483.330739301328,483.59939567611,483.868052033023,
484.136708371092,484.405364690174,484.674020990106,484.942677271643,485.211333535614,
485.479989783805,485.748646018218,486.017302241799,486.28595845791,486.554614670781,
486.823270885133,487.091927105359,487.360583335284,487.629239577831,487.897895835574,
488.166552110137,488.435208402973,488.703864714587,488.972521045443,489.241177395111,
489.509833763197,489.778490148512,490.047146549945,490.315802965719,490.584459394147,
490.853115833037,491.12177228027,491.390428733402,491.659085190034,491.927741647632,
492.196398103667,492.465054555674,492.733711001155,493.002367437866,493.271023863497,
493.539680276179,493.808336673954,494.076993055474,494.345649419303,494.614305764754,
494.882962091086,495.151618398416,495.420274686867,495.688930957498,495.95758721148,
496.22624345094,496.494899678281,496.76355589683,497.032212110404,497.300868323611,
497.569524541126,497.838180766882,498.106837004306,498.3754932559,498.64414952388,
498.912805809507,499.181462113914,499.450118437301,499.718774779852,499.987431140886,
500.256087519773,500.524743915125,500.793400325638,501.06205674939,501.330713184546,
501.599369628818,501.868026079984,502.136682535557,502.40533899308,502.673995450025,
502.942651903855,503.211308352156,503.479964792472,503.748621222657,504.017277640494,
504.285934044256,504.554590432129,504.823246802954,505.091903155488,505.360559489279,
505.629215803832,505.89787209954,506.166528376829,506.435184637073,506.703840881801,
506.972497113499,507.241153334981,507.509809549972,507.778465762756,508.047121978078,
508.315778200272,508.584434432811,508.853090678737,509.121746940149,509.390403218918,
509.659059515956,509.927715832093,510.196372167238,510.465028521309,510.733684893389,
511.002341282627,511.270997687451,511.53965410638,511.808310537359,512.076966978421,
512.345623427198,512.614279881382,512.882936338452,513.151592795914,513.420249251254,
513.688905701946,513.957562145643,514.226218579942,514.494875002812,514.763531412143,
515.032187806366,515.300844183826,515.569500543564,515.838156884552,516.106813206581,
516.375469509421,516.644125793752,516.912782060321,517.181438310831,517.450094547186,
517.718750772238,517.987406989238,518.256063202315,518.524719416134,518.793375635194,
519.062031863421,519.330688103845,519.599344359133,519.868000631,520.136656920983,
520.405313229665,520.673969557583,520.942625904371,521.211282269698,521.479938652425,
521.748595051492,522.017251465163,522.285907891788,522.554564329201,522.823220775312,
523.091877227689,523.360533683951,523.629190141564,523.897846598005,524.166503050797,
524.435159497434,524.70381593565,524.972472363114,525.241128777924,525.509785178088,
525.778441562214,526.047097928818,526.315754277159,526.584410606435,526.853066916696,
527.121723207994,527.390379481309,527.659035737726,527.927691979287,528.19634820829,
528.465004427967,528.73366064202,529.002316854973,529.270973071551,529.539629295803,
529.808285531254,530.07694178051,530.345598045876,530.614254328701,530.882910630198,
531.151566950641,531.420223290284,531.688879648504,531.957536024733,532.226192417628,
532.494848825933,532.76350524776,533.032161681312,533.30081812432,533.569474574591,
533.838131029643,534.106787487035,534.375443944235,534.644100398706,534.912756848021,
535.181413289711,535.450069721605,535.718726141461,535.987382547516,536.256038937917,
536.524695311458,536.793351666845,537.062008003567,537.330664321065,537.599320619661,
537.867976899706,538.136633162493,538.40528940946,538.673945643001,538.942601865828,
539.211258081563,539.479914294375,539.748570509011,540.017226729904,540.285882960641,
540.554539204357,540.823195463252,541.09185173928,541.360508033441,541.629164346639,
541.897820678853,542.166477030068,542.435133399423,542.703789786121,542.972446188636,
543.241102605527,543.509759034775,543.778415474441,544.047071922176,544.315728375693,
544.584384832479,544.853041290046,545.121697745877,545.390354197441,545.659010642372,
545.927667078254,546.196323503025,546.464979914547,546.733636311202,547.002292691334,
547.270949053789,547.539605397955,547.808261722147,548.076918029812,548.345574313508,
548.614230583738,548.882886864851,549.151542935882,549.420199787641,549.68885445376,
549.957511414581),.UNSPECIFIED.)
GEOMETRIC_REPRESENTATION_ITEM()
RATIONAL_B_SPLINE_SURFACE(((1.,1.,1.,1.,1.,1.,1.,1.,1.,1.,1.,1.,1.,1.,1.,
1.,1.,1.,1.,1.,1.,1.,1.,1.,1.,1.,1.,1.,1.,1.,1.,1.,1.,1.,1.,1.,1.,1.,1.,
1.,1.,1.,1.,1.,1.,1.,1.,1.,1.,1.,1.,1.,1.,1.,1.,1.,1.,1.,1.,1.,1.,1.,1.,
1.,1.,1.,1.,1.,1.,1.,1.,1.,1.,1.,1.,1.,1.,1.,1.,1.,1.,1.,1.,1.,1.,1.,1.,
1.,1.,1.,1.,1.,1.,1.,1.,1.,1.,1.,1.,1.,1.,1.,1.,1.,1.,1.,1.,1.,1.,1.,1.,
1.,1.,1.,1.,1.,1.,1.,1.,1.,1.,1.,1.,1.,1.,1.,1.,1.,1.,1.,1.,1.,1.,1.,1.,
1.,1.,1.,1.,1.,1.,1.,1.,1.,1.,1.,1.,1.,1.,1.,1.,1.,1.,1.,1.,1.,1.,1.,1.,
1.,1.,1.,1.,1.,1.,1.,1.,1.,1.,1.,1.,1.,1.,1.,1.,1.,1.,1.,1.,1.,1.,1.,1.,
1.,1.,1.,1.,1.,1.,1.,1.,1.,1.,1.,1.,1.,1.,1.,1.,1.,1.,1.,1.,1.,1.,1.,1.,
1.,1.,1.,1.,1.,1.,1.,1.,1.,1.,1.,1.,1.,1.,1.,1.,1.,1.,1.,1.,1.,1.,1.,1.,
1.,1.,1.,1.,1.,1.,1.,1.,1.,1.,1.,1.,1.,1.,1.,1.,1.,1.,1.,1.,1.,1.,1.,1.,
1.,1.,1.,1.,1.,1.,1.,1.,1.,1.,1.,1.,1.,1.,1.,1.,1.,1.,1.,1.,1.,1.,1.,1.,
1.,1.,1.,1.,1.,1.,1.,1.,1.,1.,1.,1.,1.,1.,1.,1.,1.,1.,1.,1.,1.,1.,1.,1.,
1.,1.,1.,1.,1.,1.,1.,1.,1.,1.,1.,1.,1.,1.,1.,1.,1.,1.,1.,1.,1.,1.,1.,1.,
1.,1.,1.,1.,1.,1.,1.,1.,1.,1.,1.,1.,1.,1.,1.,1.,1.,1.,1.,1.,1.,1.,1.,1.,
1.,1.,1.,1.,1.,1.,1.,1.,1.,1.,1.,1.,1.,1.,1.,1.,1.,1.,1.,1.,1.,1.,1.,1.,
1.,1.,1.,1.,1.,1.,1.,1.,1.,1.,1.,1.,1.,1.,1.,1.,1.,1.,1.,1.,1.,1.,1.,1.,
1.,1.,1.,1.,1.,1.,1.,1.,1.,1.,1.,1.,1.,1.,1.,1.,1.,1.,1.,1.,1.,1.,1.,1.,
1.,1.,1.,1.,1.,1.,1.,1.,1.,1.,1.,1.,1.,1.,1.,1.,1.,1.,1.,1.,1.,1.,1.,1.,
1.,1.,1.,1.,1.,1.,1.,1.,1.,1.,1.,1.,1.,1.,1.,1.,1.,1.,1.,1.,1.,1.,1.,1.,
1.,1.,1.,1.,1.,1.,1.,1.,1.,1.,1.,1.,1.,1.,1.,1.,1.,1.,1.,1.,1.,1.,1.,1.,
1.,1.,1.,1.,1.,1.,1.,1.,1.,1.,1.,1.,1.,1.,1.,1.,1.,1.,1.,1.,1.,1.,1.,1.,
1.,1.,1.,1.,1.,1.,1.,1.,1.,1.,1.,1.,1.,1.,1.,1.,1.,1.,1.,1.,1.,1.,1.,1.,
1.,1.,1.,1.,1.,1.,1.,1.,1.,1.,1.,1.,1.,1.,1.,1.,1.,1.,1.,1.,1.,1.,1.,1.,
1.,1.,1.,1.,1.,1.,1.,1.,1.,1.,1.,1.,1.,1.,1.,1.,1.,1.,1.,1.,1.,1.,1.,1.,
1.,1.,1.,1.,1.,1.,1.,1.,1.,1.,1.,1.,1.,1.,1.,1.,1.,1.,1.,1.,1.,1.,1.,1.,
1.,1.,1.,1.,1.,1.,1.,1.,1.,1.,1.,1.,1.,1.,1.,1.,1.,1.,1.,1.,1.,1.,1.,1.,
1.,1.,1.,1.,1.,1.,1.,1.,1.,1.,1.,1.,1.,1.,1.,1.,1.,1.,1.,1.,1.,1.,1.,1.,
1.,1.,1.,1.,1.,1.,1.,1.,1.,1.,1.,1.,1.,1.,1.,1.,1.,1.,1.,1.,1.,1.,1.,1.,
1.,1.,1.,1.,1.,1.,1.,1.,1.,1.,1.,1.,1.,1.,1.,1.,1.,1.,1.,1.,1.,1.,1.,1.,
1.,1.,1.,1.,1.,1.,1.,1.,1.,1.,1.,1.,1.,1.,1.,1.,1.,1.,1.,1.,1.,1.,1.,1.,
1.,1.,1.,1.,1.,1.,1.,1.,1.,1.,1.,1.,1.,1.,1.,1.,1.,1.,1.,1.,1.,1.,1.,1.,
1.,1.,1.,1.,1.,1.,1.,1.,1.,1.,1.,1.,1.,1.,1.,1.,1.,1.,1.,1.,1.,1.,1.,1.,
1.,1.,1.,1.,1.,1.,1.,1.,1.,1.,1.,1.,1.,1.,1.,1.,1.,1.,1.,1.,1.,1.,1.,1.,
1.,1.,1.,1.,1.,1.,1.,1.,1.,1.,1.,1.,1.,1.,1.,1.,1.,1.,1.,1.,1.,1.,1.,1.,
1.,1.,1.,1.,1.,1.,1.,1.,1.,1.,1.,1.,1.,1.,1.,1.,1.,1.,1.,1.,1.,1.,1.,1.,
1.,1.,1.,1.,1.,1.,1.,1.,1.,1.,1.,1.,1.,1.,1.,1.,1.,1.,1.,1.,1.,1.,1.,1.,
1.,1.,1.,1.,1.,1.,1.,1.,1.,1.,1.,1.,1.,1.,1.,1.,1.,1.,1.,1.,1.,1.,1.,1.,
1.,1.,1.,1.,1.,1.,1.,1.,1.,1.,1.,1.,1.,1.,1.,1.,1.,1.,1.,1.,1.,1.,1.,1.,
1.,1.,1.,1.,1.,1.,1.,1.,1.,1.,1.,1.,1.,1.,1.,1.,1.,1.,1.,1.,1.,1.,1.,1.,
1.,1.,1.,1.,1.,1.,1.,1.,1.,1.,1.,1.,1.,1.,1.,1.,1.,1.,1.,1.,1.,1.,1.,1.,
1.,1.,1.,1.,1.,1.,1.,1.,1.,1.,1.,1.,1.,1.,1.,1.,1.,1.,1.,1.,1.,1.,1.,1.,
1.,1.,1.,1.,1.,1.,1.,1.,1.,1.,1.,1.,1.,1.,1.,1.,1.,1.,1.,1.,1.,1.,1.,1.,
1.,1.,1.,1.,1.,1.,1.,1.,1.,1.,1.,1.,1.,1.,1.,1.,1.,1.,1.,1.,1.,1.,1.,1.,
1.,1.,1.,1.,1.,1.,1.,1.,1.,1.,1.,1.,1.,1.,1.,1.,1.,1.,1.,1.,1.,1.,1.,1.,
1.,1.,1.,1.,1.,1.,1.,1.,1.,1.,1.,1.,1.,1.,1.,1.,1.,1.,1.,1.,1.,1.,1.,1.,
1.,1.,1.,1.,1.,1.,1.,1.,1.,1.,1.,1.,1.,1.,1.,1.,1.,1.,1.,1.,1.,1.,1.,1.,
1.,1.,1.,1.,1.,1.,1.,1.,1.,1.,1.,1.,1.,1.,1.,1.,1.,1.,1.,1.,1.,1.,1.,1.,
1.,1.,1.,1.,1.,1.,1.,1.,1.,1.,1.,1.,1.,1.,1.,1.,1.,1.,1.,1.,1.,1.,1.,1.,
1.,1.,1.,1.,1.,1.,1.,1.,1.,1.,1.,1.,1.,1.,1.,1.,1.,1.,1.,1.,1.,1.,1.,1.,
1.,1.,1.,1.,1.,1.,1.,1.,1.,1.,1.,1.,1.,1.,1.,1.,1.,1.,1.,1.,1.,1.,1.,1.,
1.,1.,1.,1.,1.,1.,1.,1.,1.,1.,1.,1.,1.,1.,1.,1.,1.,1.,1.,1.,1.,1.,1.,1.,
1.,1.,1.,1.,1.,1.,1.,1.,1.,1.,1.,1.,1.,1.,1.,1.,1.,1.,1.,1.,1.,1.,1.,1.,
1.,1.,1.,1.,1.,1.,1.,1.,1.,1.,1.,1.,1.,1.,1.,1.,1.,1.,1.,1.,1.,1.,1.,1.,
1.,1.,1.,1.,1.,1.,1.,1.,1.,1.,1.,1.,1.,1.,1.,1.,1.,1.,1.,1.,1.,1.,1.,1.,
1.,1.,1.,1.,1.,1.,1.,1.,1.,1.,1.,1.,1.,1.,1.,1.,1.,1.,1.,1.,1.,1.,1.,1.,
1.,1.,1.,1.,1.,1.,1.,1.,1.,1.,1.,1.,1.,1.,1.,1.,1.,1.,1.,1.,1.,1.,1.,1.,
1.,1.,1.,1.,1.,1.,1.,1.,1.,1.,1.,1.,1.,1.,1.,1.,1.,1.,1.,1.,1.,1.,1.,1.,
1.,1.,1.,1.,1.,1.,1.,1.,1.,1.,1.,1.,1.,1.,1.,1.,1.,1.,1.,1.,1.,1.,1.,1.,
1.,1.,1.,1.,1.,1.,1.,1.,1.,1.,1.,1.,1.,1.,1.,1.,1.,1.,1.,1.,1.,1.,1.,1.,
1.,1.,1.,1.,1.,1.,1.,1.,1.,1.,1.,1.,1.,1.,1.,1.,1.,1.,1.,1.,1.,1.,1.,1.,
1.,1.,1.,1.,1.,1.,1.,1.,1.,1.,1.,1.,1.,1.,1.,1.,1.,1.,1.,1.,1.,1.,1.,1.,
1.,1.,1.,1.,1.,1.,1.,1.,1.,1.,1.,1.,1.,1.,1.,1.,1.,1.,1.,1.,1.,1.,1.,1.,
1.,1.,1.,1.,1.,1.,1.,1.,1.,1.,1.,1.,1.,1.,1.,1.,1.,1.,1.,1.,1.,1.,1.,1.,
1.,1.,1.,1.,1.,1.,1.,1.,1.,1.,1.,1.,1.,1.,1.,1.,1.,1.,1.,1.,1.,1.,1.,1.,
1.,1.,1.,1.,1.,1.,1.,1.,1.,1.,1.,1.,1.,1.,1.,1.,1.,1.,1.,1.,1.,1.,1.,1.,
1.,1.,1.,1.,1.,1.,1.,1.,1.,1.,1.,1.,1.,1.,1.,1.,1.,1.,1.,1.,1.,1.,1.,1.,
1.,1.,1.,1.,1.,1.,1.,1.,1.,1.,1.,1.,1.,1.,1.,1.,1.,1.,1.,1.,1.,1.,1.,1.,
1.,1.,1.,1.,1.,1.,1.,1.,1.,1.,1.,1.,1.,1.,1.,1.,1.,1.,1.,1.,1.,1.,1.,1.,
1.,1.,1.,1.,1.,1.,1.,1.,1.,1.,1.,1.,1.,1.,1.,1.,1.,1.,1.,1.,1.,1.,1.,1.,
1.,1.,1.,1.,1.,1.,1.,1.,1.,1.,1.,1.,1.,1.,1.,1.,1.,1.,1.,1.,1.,1.,1.,1.,
1.,1.,1.,1.,1.,1.,1.,1.,1.,1.,1.,1.,1.,1.,1.,1.,1.,1.,1.,1.,1.,1.,1.,1.,
1.,1.,1.,1.,1.,1.,1.,1.,1.,1.,1.,1.,1.,1.,1.,1.,1.,1.,1.,1.,1.,1.,1.,1.,
1.,1.,1.,1.,1.,1.,1.,1.,1.,1.,1.,1.,1.,1.,1.,1.,1.,1.,1.,1.,1.,1.,1.,1.,
1.,1.,1.,1.,1.,1.,1.,1.,1.,1.,1.,1.,1.,1.,1.,1.,1.,1.,1.,1.,1.,1.,1.,1.,
1.,1.,1.,1.,1.,1.,1.,1.,1.,1.,1.,1.,1.,1.,1.,1.,1.,1.,1.,1.,1.,1.,1.,1.,
1.,1.,1.,1.,1.,1.,1.,1.,1.,1.,1.,1.,1.,1.,1.,1.,1.,1.,1.,1.,1.,1.,1.,1.,
1.,1.,1.,1.,1.,1.,1.,1.,1.,1.,1.,1.,1.,1.,1.,1.,1.,1.,1.,1.,1.,1.,1.,1.,
1.,1.,1.,1.,1.,1.,1.,1.,1.,1.,1.,1.,1.,1.,1.,1.,1.,1.,1.,1.,1.,1.,1.,1.,
1.,1.,1.,1.,1.,1.,1.,1.,1.,1.,1.,1.,1.,1.,1.,1.,1.,1.,1.,1.,1.,1.,1.,1.,
1.,1.,1.,1.,1.,1.,1.,1.,1.,1.,1.,1.,1.,1.,1.,1.,1.,1.,1.,1.,1.,1.,1.,1.,
1.,1.,1.,1.,1.,1.,1.,1.,1.,1.,1.,1.,1.,1.,1.,1.,1.,1.,1.,1.,1.,1.,1.,1.,
1.,1.,1.,1.,1.,1.,1.,1.,1.,1.,1.,1.,1.,1.,1.,1.,1.,1.,1.,1.,1.,1.,1.,1.,
1.,1.,1.,1.,1.,1.,1.,1.,1.,1.,1.,1.,1.,1.,1.,1.,1.,1.,1.,1.,1.,1.,1.,1.,
1.,1.,1.,1.,1.,1.,1.,1.,1.,1.,1.,1.,1.,1.,1.,1.,1.,1.,1.,1.,1.,1.,1.,1.,
1.,1.,1.,1.,1.,1.,1.,1.,1.,1.,1.,1.,1.,1.,1.,1.,1.,1.,1.,1.),(0.707106781186548,
0.707106781186548,0.707106781186548,0.707106781186547,0.707106781186547,
0.707106781186548,0.707106781186547,0.707106781186547,0.707106781186547,
0.707106781186547,0.707106781186547,0.707106781186548,0.707106781186548,
0.707106781186548,0.707106781186547,0.707106781186548,0.707106781186547,
0.707106781186547,0.707106781186548,0.707106781186547,0.707106781186548,
0.707106781186547,0.707106781186548,0.707106781186547,0.707106781186548,
0.707106781186547,0.707106781186547,0.707106781186547,0.707106781186547,
0.707106781186547,0.707106781186548,0.707106781186547,0.707106781186547,
0.707106781186548,0.707106781186547,0.707106781186547,0.707106781186548,
0.707106781186547,0.707106781186547,0.707106781186548,0.707106781186548,
0.707106781186547,0.707106781186548,0.707106781186547,0.707106781186547,
0.707106781186547,0.707106781186548,0.707106781186548,0.707106781186547,
0.707106781186547,0.707106781186548,0.707106781186547,0.707106781186548,
0.707106781186547,0.707106781186547,0.707106781186547,0.707106781186547,
0.707106781186547,0.707106781186548,0.707106781186547,0.707106781186548,
0.707106781186547,0.707106781186548,0.707106781186547,0.707106781186548,
0.707106781186547,0.707106781186547,0.707106781186548,0.707106781186547,
0.707106781186547,0.707106781186548,0.707106781186547,0.707106781186548,
0.707106781186547,0.707106781186548,0.707106781186548,0.707106781186547,
0.707106781186548,0.707106781186547,0.707106781186547,0.707106781186548,
0.707106781186547,0.707106781186547,0.707106781186547,0.707106781186548,
0.707106781186547,0.707106781186547,0.707106781186547,0.707106781186547,
0.707106781186547,0.707106781186547,0.707106781186548,0.707106781186548,
0.707106781186547,0.707106781186548,0.707106781186547,0.707106781186548,
0.707106781186548,0.707106781186547,0.707106781186548,0.707106781186548,
0.707106781186548,0.707106781186547,0.707106781186548,0.707106781186547,
0.707106781186548,0.707106781186548,0.707106781186548,0.707106781186547,
0.707106781186547,0.707106781186547,0.707106781186548,0.707106781186548,
0.707106781186548,0.707106781186547,0.707106781186547,0.707106781186547,
0.707106781186548,0.707106781186548,0.707106781186547,0.707106781186547,
0.707106781186548,0.707106781186547,0.707106781186547,0.707106781186547,
0.707106781186547,0.707106781186548,0.707106781186547,0.707106781186548,
0.707106781186547,0.707106781186547,0.707106781186547,0.707106781186548,
0.707106781186548,0.707106781186547,0.707106781186548,0.707106781186548,
0.707106781186547,0.707106781186548,0.707106781186547,0.707106781186548,
0.707106781186547,0.707106781186548,0.707106781186547,0.707106781186547,
0.707106781186548,0.707106781186547,0.707106781186547,0.707106781186548,
0.707106781186547,0.707106781186547,0.707106781186548,0.707106781186547,
0.707106781186548,0.707106781186547,0.707106781186547,0.707106781186548,
0.707106781186548,0.707106781186547,0.707106781186548,0.707106781186547,
0.707106781186548,0.707106781186547,0.707106781186548,0.707106781186547,
0.707106781186548,0.707106781186547,0.707106781186548,0.707106781186547,
0.707106781186548,0.707106781186547,0.707106781186548,0.707106781186547,
0.707106781186547,0.707106781186548,0.707106781186547,0.707106781186548,
0.707106781186547,0.707106781186548,0.707106781186547,0.707106781186548,
0.707106781186547,0.707106781186547,0.707106781186548,0.707106781186547,
0.707106781186548,0.707106781186548,0.707106781186548,0.707106781186547,
0.707106781186547,0.707106781186547,0.707106781186547,0.707106781186548,
0.707106781186547,0.707106781186548,0.707106781186548,0.707106781186547,
0.707106781186547,0.707106781186548,0.707106781186548,0.707106781186547,
0.707106781186547,0.707106781186548,0.707106781186547,0.707106781186548,
0.707106781186547,0.707106781186547,0.707106781186547,0.707106781186547,
0.707106781186547,0.707106781186547,0.707106781186547,0.707106781186548,
0.707106781186547,0.707106781186548,0.707106781186547,0.707106781186548,
0.707106781186548,0.707106781186547,0.707106781186548,0.707106781186548,
0.707106781186548,0.707106781186548,0.707106781186547,0.707106781186548,
0.707106781186547,0.707106781186548,0.707106781186547,0.707106781186547,
0.707106781186548,0.707106781186548,0.707106781186547,0.707106781186547,
0.707106781186547,0.707106781186547,0.707106781186547,0.707106781186548,
0.707106781186548,0.707106781186547,0.707106781186547,0.707106781186548,
0.707106781186548,0.707106781186547,0.707106781186548,0.707106781186547,
0.707106781186548,0.707106781186548,0.707106781186547,0.707106781186547,
0.707106781186548,0.707106781186547,0.707106781186547,0.707106781186548,
0.707106781186547,0.707106781186548,0.707106781186547,0.707106781186548,
0.707106781186547,0.707106781186547,0.707106781186548,0.707106781186548,
0.707106781186547,0.707106781186547,0.707106781186548,0.707106781186547,
0.707106781186547,0.707106781186548,0.707106781186547,0.707106781186548,
0.707106781186547,0.707106781186548,0.707106781186547,0.707106781186548,
0.707106781186547,0.707106781186547,0.707106781186547,0.707106781186547,
0.707106781186547,0.707106781186547,0.707106781186548,0.707106781186547,
0.707106781186548,0.707106781186547,0.707106781186548,0.707106781186548,
0.707106781186547,0.707106781186548,0.707106781186548,0.707106781186547,
0.707106781186548,0.707106781186547,0.707106781186547,0.707106781186547,
0.707106781186548,0.707106781186547,0.707106781186547,0.707106781186548,
0.707106781186547,0.707106781186548,0.707106781186547,0.707106781186547,
0.707106781186547,0.707106781186548,0.707106781186548,0.707106781186547,
0.707106781186548,0.707106781186548,0.707106781186547,0.707106781186548,
0.707106781186547,0.707106781186548,0.707106781186548,0.707106781186547,
0.707106781186548,0.707106781186548,0.707106781186548,0.707106781186547,
0.707106781186547,0.707106781186548,0.707106781186547,0.707106781186548,
0.707106781186547,0.707106781186547,0.707106781186548,0.707106781186548,
0.707106781186548,0.707106781186547,0.707106781186547,0.707106781186548,
0.707106781186548,0.707106781186547,0.707106781186547,0.707106781186548,
0.707106781186547,0.707106781186547,0.707106781186548,0.707106781186548,
0.707106781186547,0.707106781186547,0.707106781186547,0.707106781186548,
0.707106781186547,0.707106781186547,0.707106781186547,0.707106781186548,
0.707106781186548,0.707106781186547,0.707106781186548,0.707106781186547,
0.707106781186548,0.707106781186547,0.707106781186548,0.707106781186548,
0.707106781186547,0.707106781186547,0.707106781186548,0.707106781186547,
0.707106781186547,0.707106781186548,0.707106781186547,0.707106781186548,
0.707106781186548,0.707106781186547,0.707106781186548,0.707106781186547,
0.707106781186547,0.707106781186547,0.707106781186548,0.707106781186548,
0.707106781186548,0.707106781186547,0.707106781186548,0.707106781186547,
0.707106781186548,0.707106781186547,0.707106781186547,0.707106781186547,
0.707106781186547,0.707106781186548,0.707106781186548,0.707106781186547,
0.707106781186547,0.707106781186548,0.707106781186547,0.707106781186548,
0.707106781186547,0.707106781186548,0.707106781186547,0.707106781186547,
0.707106781186548,0.707106781186547,0.707106781186548,0.707106781186547,
0.707106781186548,0.707106781186548,0.707106781186547,0.707106781186548,
0.707106781186547,0.707106781186548,0.707106781186548,0.707106781186547,
0.707106781186548,0.707106781186547,0.707106781186547,0.707106781186548,
0.707106781186547,0.707106781186548,0.707106781186547,0.707106781186548,
0.707106781186547,0.707106781186547,0.707106781186548,0.707106781186548,
0.707106781186548,0.707106781186548,0.707106781186547,0.707106781186548,
0.707106781186548,0.707106781186548,0.707106781186547,0.707106781186548,
0.707106781186548,0.707106781186548,0.707106781186547,0.707106781186547,
0.707106781186548,0.707106781186547,0.707106781186548,0.707106781186547,
0.707106781186548,0.707106781186548,0.707106781186547,0.707106781186547,
0.707106781186548,0.707106781186547,0.707106781186548,0.707106781186547,
0.707106781186548,0.707106781186548,0.707106781186547,0.707106781186547,
0.707106781186547,0.707106781186548,0.707106781186548,0.707106781186547,
0.707106781186547,0.707106781186548,0.707106781186548,0.707106781186548,
0.707106781186548,0.707106781186547,0.707106781186547,0.707106781186548,
0.707106781186548,0.707106781186547,0.707106781186548,0.707106781186547,
0.707106781186548,0.707106781186547,0.707106781186548,0.707106781186547,
0.707106781186547,0.707106781186548,0.707106781186547,0.707106781186547,
0.707106781186548,0.707106781186547,0.707106781186548,0.707106781186547,
0.707106781186548,0.707106781186547,0.707106781186548,0.707106781186547,
0.707106781186548,0.707106781186547,0.707106781186548,0.707106781186547,
0.707106781186547,0.707106781186548,0.707106781186548,0.707106781186547,
0.707106781186547,0.707106781186547,0.707106781186548,0.707106781186547,
0.707106781186548,0.707106781186547,0.707106781186548,0.707106781186547,
0.707106781186548,0.707106781186547,0.707106781186547,0.707106781186547,
0.707106781186548,0.707106781186547,0.707106781186548,0.707106781186548,
0.707106781186547,0.707106781186548,0.707106781186547,0.707106781186547,
0.707106781186548,0.707106781186547,0.707106781186547,0.707106781186548,
0.707106781186547,0.707106781186547,0.707106781186547,0.707106781186547,
0.707106781186548,0.707106781186547,0.707106781186547,0.707106781186547,
0.707106781186548,0.707106781186547,0.707106781186547,0.707106781186548,
0.707106781186548,0.707106781186547,0.707106781186548,0.707106781186548,
0.707106781186547,0.707106781186547,0.707106781186548,0.707106781186547,
0.707106781186547,0.707106781186548,0.707106781186547,0.707106781186547,
0.707106781186547,0.707106781186548,0.707106781186547,0.707106781186548,
0.707106781186547,0.707106781186548,0.707106781186547,0.707106781186548,
0.707106781186547,0.707106781186548,0.707106781186547,0.707106781186548,
0.707106781186548,0.707106781186547,0.707106781186547,0.707106781186548,
0.707106781186547,0.707106781186548,0.707106781186547,0.707106781186548,
0.707106781186548,0.707106781186547,0.707106781186548,0.707106781186547,
0.707106781186548,0.707106781186548,0.707106781186547,0.707106781186547,
0.707106781186548,0.707106781186547,0.707106781186548,0.707106781186547,
0.707106781186548,0.707106781186547,0.707106781186548,0.707106781186547,
0.707106781186547,0.707106781186547,0.707106781186547,0.707106781186547,
0.707106781186547,0.707106781186547,0.707106781186547,0.707106781186548,
0.707106781186547,0.707106781186548,0.707106781186547,0.707106781186547,
0.707106781186548,0.707106781186547,0.707106781186548,0.707106781186547,
0.707106781186547,0.707106781186548,0.707106781186547,0.707106781186548,
0.707106781186547,0.707106781186548,0.707106781186547,0.707106781186548,
0.707106781186547,0.707106781186548,0.707106781186547,0.707106781186548,
0.707106781186547,0.707106781186548,0.707106781186548,0.707106781186547,
0.707106781186548,0.707106781186547,0.707106781186547,0.707106781186547,
0.707106781186548,0.707106781186547,0.707106781186547,0.707106781186547,
0.707106781186548,0.707106781186547,0.707106781186547,0.707106781186548,
0.707106781186547,0.707106781186547,0.707106781186547,0.707106781186547,
0.707106781186548,0.707106781186547,0.707106781186547,0.707106781186547,
0.707106781186548,0.707106781186548,0.707106781186548,0.707106781186548,
0.707106781186547,0.707106781186548,0.707106781186547,0.707106781186547,
0.707106781186548,0.707106781186547,0.707106781186548,0.707106781186547,
0.707106781186547,0.707106781186548,0.707106781186547,0.707106781186547,
0.707106781186547,0.707106781186547,0.707106781186548,0.707106781186548,
0.707106781186547,0.707106781186547,0.707106781186548,0.707106781186547,
0.707106781186548,0.707106781186547,0.707106781186548,0.707106781186548,
0.707106781186547,0.707106781186547,0.707106781186548,0.707106781186548,
0.707106781186547,0.707106781186548,0.707106781186548,0.707106781186547,
0.707106781186548,0.707106781186548,0.707106781186548,0.707106781186547,
0.707106781186548,0.707106781186547,0.707106781186548,0.707106781186547,
0.707106781186548,0.707106781186547,0.707106781186548,0.707106781186547,
0.707106781186548,0.707106781186548,0.707106781186547,0.707106781186547,
0.707106781186548,0.707106781186547,0.707106781186548,0.707106781186547,
0.707106781186548,0.707106781186548,0.707106781186548,0.707106781186548,
0.707106781186548,0.707106781186547,0.707106781186547,0.707106781186547,
0.707106781186547,0.707106781186548,0.707106781186547,0.707106781186548,
0.707106781186547,0.707106781186547,0.707106781186548,0.707106781186548,
0.707106781186547,0.707106781186548,0.707106781186547,0.707106781186548,
0.707106781186548,0.707106781186547,0.707106781186547,0.707106781186548,
0.707106781186547,0.707106781186548,0.707106781186547,0.707106781186548,
0.707106781186547,0.707106781186548,0.707106781186547,0.707106781186548,
0.707106781186547,0.707106781186548,0.707106781186547,0.707106781186548,
0.707106781186548,0.707106781186547,0.707106781186548,0.707106781186547,
0.707106781186548,0.707106781186547,0.707106781186548,0.707106781186548,
0.707106781186548,0.707106781186547,0.707106781186547,0.707106781186548,
0.707106781186548,0.707106781186547,0.707106781186547,0.707106781186547,
0.707106781186548,0.707106781186547,0.707106781186548,0.707106781186547,
0.707106781186548,0.707106781186547,0.707106781186547,0.707106781186547,
0.707106781186548,0.707106781186547,0.707106781186548,0.707106781186547,
0.707106781186548,0.707106781186547,0.707106781186548,0.707106781186547,
0.707106781186547,0.707106781186548,0.707106781186547,0.707106781186547,
0.707106781186548,0.707106781186547,0.707106781186547,0.707106781186548,
0.707106781186547,0.707106781186547,0.707106781186547,0.707106781186548,
0.707106781186547,0.707106781186548,0.707106781186547,0.707106781186547,
0.707106781186547,0.707106781186548,0.707106781186548,0.707106781186547,
0.707106781186547,0.707106781186548,0.707106781186548,0.707106781186548,
0.707106781186547,0.707106781186548,0.707106781186547,0.707106781186548,
0.707106781186547,0.707106781186548,0.707106781186547,0.707106781186547,
0.707106781186547,0.707106781186547,0.707106781186548,0.707106781186547,
0.707106781186548,0.707106781186548,0.707106781186547,0.707106781186548,
0.707106781186547,0.707106781186547,0.707106781186547,0.707106781186547,
0.707106781186548,0.707106781186547,0.707106781186548,0.707106781186547,
0.707106781186548,0.707106781186548,0.707106781186547,0.707106781186548,
0.707106781186547,0.707106781186547,0.707106781186547,0.707106781186547,
0.707106781186548,0.707106781186547,0.707106781186548,0.707106781186548,
0.707106781186547,0.707106781186548,0.707106781186547,0.707106781186548,
0.707106781186547,0.707106781186547,0.707106781186548,0.707106781186547,
0.707106781186548,0.707106781186548,0.707106781186547,0.707106781186547,
0.707106781186548,0.707106781186548,0.707106781186547,0.707106781186547,
0.707106781186548,0.707106781186547,0.707106781186547,0.707106781186548,
0.707106781186547,0.707106781186547,0.707106781186548,0.707106781186547,
0.707106781186548,0.707106781186547,0.707106781186547,0.707106781186548,
0.707106781186547,0.707106781186548,0.707106781186547,0.707106781186548,
0.707106781186547,0.707106781186547,0.707106781186547,0.707106781186548,
0.707106781186547,0.707106781186548,0.707106781186547,0.707106781186548,
0.707106781186548,0.707106781186548,0.707106781186548,0.707106781186547,
0.707106781186547,0.707106781186547,0.707106781186548,0.707106781186547,
0.707106781186548,0.707106781186547,0.707106781186547,0.707106781186548,
0.707106781186547,0.707106781186547,0.707106781186548,0.707106781186547,
0.707106781186547,0.707106781186548,0.707106781186548,0.707106781186547,
0.707106781186548,0.707106781186547,0.707106781186547,0.707106781186548,
0.707106781186547,0.707106781186548,0.707106781186547,0.707106781186548,
0.707106781186547,0.707106781186547,0.707106781186547,0.707106781186548,
0.707106781186547,0.707106781186548,0.707106781186547,0.707106781186548,
0.707106781186547,0.707106781186547,0.707106781186548,0.707106781186548,
0.707106781186548,0.707106781186547,0.707106781186548,0.707106781186547,
0.707106781186548,0.707106781186547,0.707106781186548,0.707106781186547,
0.707106781186548,0.707106781186548,0.707106781186547,0.707106781186547,
0.707106781186547,0.707106781186548,0.707106781186547,0.707106781186547,
0.707106781186548,0.707106781186547,0.707106781186547,0.707106781186548,
0.707106781186547,0.707106781186548,0.707106781186548,0.707106781186548,
0.707106781186547,0.707106781186548,0.707106781186547,0.707106781186548,
0.707106781186547,0.707106781186548,0.707106781186547,0.707106781186548,
0.707106781186547,0.707106781186548,0.707106781186547,0.707106781186548,
0.707106781186548,0.707106781186547,0.707106781186548,0.707106781186547,
0.707106781186548,0.707106781186548,0.707106781186547,0.707106781186547,
0.707106781186548,0.707106781186547,0.707106781186547,0.707106781186548,
0.707106781186547,0.707106781186548,0.707106781186548,0.707106781186547,
0.707106781186548,0.707106781186548,0.707106781186548,0.707106781186548,
0.707106781186548,0.707106781186547,0.707106781186548,0.707106781186548,
0.707106781186548,0.707106781186547,0.707106781186548,0.707106781186547,
0.707106781186548,0.707106781186547,0.707106781186548,0.707106781186547,
0.707106781186548,0.707106781186547,0.707106781186548,0.707106781186547,
0.707106781186547,0.707106781186548,0.707106781186547,0.707106781186547,
0.707106781186548,0.707106781186547,0.707106781186548,0.707106781186547,
0.707106781186548,0.707106781186547,0.707106781186548,0.707106781186547,
0.707106781186547,0.707106781186548,0.707106781186547,0.707106781186547,
0.707106781186548,0.707106781186547,0.707106781186548,0.707106781186547,
0.707106781186547,0.707106781186548,0.707106781186548,0.707106781186547,
0.707106781186548,0.707106781186547,0.707106781186547,0.707106781186547,
0.707106781186548,0.707106781186547,0.707106781186547,0.707106781186548,
0.707106781186547,0.707106781186547,0.707106781186547,0.707106781186548,
0.707106781186548,0.707106781186547,0.707106781186548,0.707106781186547,
0.707106781186548,0.707106781186547,0.707106781186547,0.707106781186548,
0.707106781186547,0.707106781186548,0.707106781186547,0.707106781186547,
0.707106781186547,0.707106781186547,0.707106781186548,0.707106781186547,
0.707106781186547,0.707106781186547,0.707106781186547,0.707106781186547,
0.707106781186548,0.707106781186547,0.707106781186547,0.707106781186547,
0.707106781186547,0.707106781186548,0.707106781186547,0.707106781186548,
0.707106781186547,0.707106781186547,0.707106781186548,0.707106781186547,
0.707106781186548,0.707106781186547,0.707106781186547,0.707106781186548,
0.707106781186547,0.707106781186547,0.707106781186548,0.707106781186547,
0.707106781186547,0.707106781186547,0.707106781186547,0.707106781186548,
0.707106781186547,0.707106781186548,0.707106781186548,0.707106781186547,
0.707106781186548,0.707106781186548,0.707106781186547,0.707106781186547,
0.707106781186548,0.707106781186547,0.707106781186547,0.707106781186547,
0.707106781186548,0.707106781186547,0.707106781186547,0.707106781186548,
0.707106781186547,0.707106781186548,0.707106781186547,0.707106781186548,
0.707106781186547,0.707106781186547,0.707106781186548,0.707106781186547,
0.707106781186548,0.707106781186547,0.707106781186548,0.707106781186547,
0.707106781186548,0.707106781186547,0.707106781186548,0.707106781186547,
0.707106781186547,0.707106781186547,0.707106781186547,0.707106781186548,
0.707106781186548,0.707106781186547,0.707106781186548,0.707106781186548,
0.707106781186547,0.707106781186548,0.707106781186547,0.707106781186547,
0.707106781186548,0.707106781186547,0.707106781186547,0.707106781186547,
0.707106781186547,0.707106781186548,0.707106781186547,0.707106781186547,
0.707106781186547,0.707106781186548,0.707106781186547,0.707106781186547,
0.707106781186548,0.707106781186547,0.707106781186548,0.707106781186548,
0.707106781186547,0.707106781186548,0.707106781186547,0.707106781186548,
0.707106781186547,0.707106781186548,0.707106781186547,0.707106781186547,
0.707106781186548,0.707106781186547,0.707106781186548,0.707106781186548,
0.707106781186547,0.707106781186547,0.707106781186548,0.707106781186547,
0.707106781186548,0.707106781186547,0.707106781186548,0.707106781186547,
0.707106781186547,0.707106781186548,0.707106781186548,0.707106781186547,
0.707106781186548,0.707106781186548,0.707106781186547,0.707106781186548,
0.707106781186548,0.707106781186547,0.707106781186548,0.707106781186547,
0.707106781186548,0.707106781186547,0.707106781186548,0.707106781186547,
0.707106781186548,0.707106781186547,0.707106781186547,0.707106781186548,
0.707106781186547,0.707106781186547,0.707106781186548,0.707106781186547,
0.707106781186548,0.707106781186548,0.707106781186547,0.707106781186547,
0.707106781186547,0.707106781186548,0.707106781186547,0.707106781186548,
0.707106781186548,0.707106781186547,0.707106781186548,0.707106781186547,
0.707106781186548,0.707106781186547,0.707106781186548,0.707106781186547,
0.707106781186547,0.707106781186548,0.707106781186548,0.707106781186548,
0.707106781186547,0.707106781186548,0.707106781186548,0.707106781186547,
0.707106781186548,0.707106781186547,0.707106781186548,0.707106781186548,
0.707106781186548,0.707106781186548,0.707106781186548,0.707106781186548,
0.707106781186547,0.707106781186547,0.707106781186548,0.707106781186547,
0.707106781186547,0.707106781186548,0.707106781186547,0.707106781186547,
0.707106781186548,0.707106781186547,0.707106781186548,0.707106781186547,
0.707106781186548,0.707106781186547,0.707106781186547,0.707106781186547,
0.707106781186548,0.707106781186547,0.707106781186547,0.707106781186548,
0.707106781186547,0.707106781186548,0.707106781186547,0.707106781186548,
0.707106781186547,0.707106781186547,0.707106781186547,0.707106781186547,
0.707106781186548,0.707106781186547,0.707106781186547,0.707106781186548,
0.707106781186548,0.707106781186547,0.707106781186548,0.707106781186547,
0.707106781186548,0.707106781186547,0.707106781186547,0.707106781186548,
0.707106781186547,0.707106781186548,0.707106781186547,0.707106781186548,
0.707106781186547,0.707106781186548,0.707106781186548,0.707106781186547,
0.707106781186548,0.707106781186547,0.707106781186547,0.707106781186548,
0.707106781186547,0.707106781186547,0.707106781186548,0.707106781186548,
0.707106781186548,0.707106781186547,0.707106781186548,0.707106781186547,
0.707106781186547,0.707106781186547,0.707106781186548,0.707106781186547,
0.707106781186548,0.707106781186548,0.707106781186548,0.707106781186547,
0.707106781186547,0.707106781186547,0.707106781186547,0.707106781186548,
0.707106781186547,0.707106781186547,0.707106781186548,0.707106781186547,
0.707106781186548,0.707106781186547,0.707106781186547,0.707106781186548,
0.707106781186547,0.707106781186548,0.707106781186547,0.707106781186548,
0.707106781186547,0.707106781186547,0.707106781186547,0.707106781186547,
0.707106781186547,0.707106781186547,0.707106781186548,0.707106781186547,
0.707106781186547,0.707106781186548,0.707106781186548,0.707106781186547,
0.707106781186548,0.707106781186548,0.707106781186547,0.707106781186547,
0.707106781186548,0.707106781186547,0.707106781186547,0.707106781186548,
0.707106781186547,0.707106781186548,0.707106781186548,0.707106781186548,
0.707106781186547,0.707106781186547,0.707106781186547,0.707106781186547,
0.707106781186548,0.707106781186548,0.707106781186548,0.707106781186547,
0.707106781186548,0.707106781186547,0.707106781186548,0.707106781186548,
0.707106781186547,0.707106781186548,0.707106781186547,0.707106781186548,
0.707106781186548,0.707106781186547,0.707106781186547,0.707106781186548,
0.707106781186547,0.707106781186548,0.707106781186547,0.707106781186548,
0.707106781186548,0.707106781186548,0.707106781186547,0.707106781186548,
0.707106781186547,0.707106781186547,0.707106781186547,0.707106781186547,
0.707106781186548,0.707106781186548,0.707106781186547,0.707106781186547,
0.707106781186547,0.707106781186548,0.707106781186547,0.707106781186547,
0.707106781186548,0.707106781186547,0.707106781186548,0.707106781186548,
0.707106781186548,0.707106781186547,0.707106781186547,0.707106781186547,
0.707106781186547,0.707106781186548,0.707106781186548,0.707106781186547,
0.707106781186548,0.707106781186547,0.707106781186548,0.707106781186548,
0.707106781186547,0.707106781186548,0.707106781186547,0.707106781186548,
0.707106781186547,0.707106781186547,0.707106781186547,0.707106781186548,
0.707106781186547,0.707106781186548,0.707106781186547,0.707106781186548,
0.707106781186547,0.707106781186548,0.707106781186547,0.707106781186548,
0.707106781186547,0.707106781186547,0.707106781186548,0.707106781186547,
0.707106781186548,0.707106781186547,0.707106781186547,0.707106781186548,
0.707106781186548,0.707106781186547,0.707106781186548,0.707106781186548,
0.707106781186547,0.707106781186548,0.707106781186547,0.707106781186548,
0.707106781186547,0.707106781186547,0.707106781186547,0.707106781186548,
0.707106781186547,0.707106781186547,0.707106781186548,0.707106781186547,
0.707106781186548,0.707106781186547,0.707106781186548,0.707106781186548,
0.707106781186547,0.707106781186548,0.707106781186547,0.707106781186548,
0.707106781186548,0.707106781186548,0.707106781186548,0.707106781186547,
0.707106781186547,0.707106781186548,0.707106781186547,0.707106781186547,
0.707106781186548,0.707106781186548,0.707106781186547,0.707106781186547,
0.707106781186548,0.707106781186547,0.707106781186547,0.707106781186548,
0.707106781186547,0.707106781186548,0.707106781186547,0.707106781186548,
0.707106781186547,0.707106781186547,0.707106781186547,0.707106781186548,
0.707106781186547,0.707106781186547,0.707106781186548,0.707106781186547,
0.707106781186548,0.707106781186548,0.707106781186548,0.707106781186547,
0.707106781186547,0.707106781186547,0.707106781186548,0.707106781186548,
0.707106781186547,0.707106781186547,0.707106781186547,0.707106781186547,
0.707106781186548,0.707106781186548,0.707106781186547,0.707106781186547,
0.707106781186547,0.707106781186548,0.707106781186548,0.707106781186547,
0.707106781186548,0.707106781186547,0.707106781186548,0.707106781186547,
0.707106781186548,0.707106781186548,0.707106781186547,0.707106781186548,
0.707106781186548,0.707106781186548,0.707106781186547,0.707106781186547,
0.707106781186547,0.707106781186548,0.707106781186548,0.707106781186548,
0.707106781186547,0.707106781186547,0.707106781186548,0.707106781186548,
0.707106781186547,0.707106781186548,0.707106781186547,0.707106781186547,
0.707106781186548,0.707106781186547,0.707106781186548,0.707106781186547,
0.707106781186547,0.707106781186548,0.707106781186547,0.707106781186548,
0.707106781186548,0.707106781186547,0.707106781186547,0.707106781186548,
0.707106781186547,0.707106781186548,0.707106781186547,0.707106781186547,
0.707106781186548,0.707106781186547,0.707106781186548,0.707106781186547,
0.707106781186548,0.707106781186547,0.707106781186547,0.707106781186548,
0.707106781186547,0.707106781186547,0.707106781186547,0.707106781186547,
0.707106781186547,0.707106781186547,0.707106781186548,0.707106781186547,
0.707106781186548,0.707106781186548,0.707106781186548,0.707106781186547,
0.707106781186547,0.707106781186547,0.707106781186548,0.707106781186547,
0.707106781186548,0.707106781186547,0.707106781186547,0.707106781186548,
0.707106781186547,0.707106781186547,0.707106781186547,0.707106781186547,
0.707106781186547,0.707106781186548,0.707106781186547,0.707106781186548,
0.707106781186547,0.707106781186547,0.707106781186548,0.707106781186548,
0.707106781186547,0.707106781186547,0.707106781186547,0.707106781186548,
0.707106781186547,0.707106781186547,0.707106781186548,0.707106781186548,
0.707106781186547,0.707106781186548,0.707106781186547,0.707106781186548,
0.707106781186548,0.707106781186547,0.707106781186547,0.707106781186547,
0.707106781186548,0.707106781186548,0.707106781186547,0.707106781186548,
0.707106781186547,0.707106781186548,0.707106781186548,0.707106781186547,
0.707106781186548,0.707106781186547,0.707106781186547,0.707106781186547,
0.707106781186548,0.707106781186547,0.707106781186548,0.707106781186547,
0.707106781186548,0.707106781186547,0.707106781186547,0.707106781186547,
0.707106781186547,0.707106781186547,0.707106781186548,0.707106781186547,
0.707106781186548,0.707106781186547,0.707106781186548,0.707106781186547,
0.707106781186548,0.707106781186547,0.707106781186547,0.707106781186547,
0.707106781186547,0.707106781186547,0.707106781186548,0.707106781186548,
0.707106781186548,0.707106781186547,0.707106781186548,0.707106781186547,
0.707106781186548,0.707106781186547,0.707106781186547,0.707106781186548,
0.707106781186547,0.707106781186548,0.707106781186547,0.707106781186547,
0.707106781186547,0.707106781186548,0.707106781186548,0.707106781186547,
0.707106781186548,0.707106781186547,0.707106781186548,0.707106781186548,
0.707106781186547,0.707106781186548,0.707106781186547,0.707106781186548,
0.707106781186548,0.707106781186547,0.707106781186547,0.707106781186547,
0.707106781186547,0.707106781186547,0.707106781186547,0.707106781186548,
0.707106781186548,0.707106781186547,0.707106781186548,0.707106781186547,
0.707106781186547,0.707106781186548,0.707106781186547,0.707106781186547,
0.707106781186548,0.707106781186547,0.707106781186547,0.707106781186547,
0.707106781186548,0.707106781186547,0.707106781186547,0.707106781186548,
0.707106781186547,0.707106781186548,0.707106781186548,0.707106781186547,
0.707106781186547,0.707106781186547,0.707106781186548,0.707106781186547,
0.707106781186547,0.707106781186548,0.707106781186548,0.707106781186548,
0.707106781186548,0.707106781186547,0.707106781186548,0.707106781186548,
0.707106781186547,0.707106781186547,0.707106781186548,0.707106781186547,
0.707106781186548,0.707106781186547,0.707106781186547,0.707106781186548,
0.707106781186547,0.707106781186547,0.707106781186548,0.707106781186547,
0.707106781186548,0.707106781186547,0.707106781186548,0.707106781186547,
0.707106781186548,0.707106781186547,0.707106781186548,0.707106781186547,
0.707106781186548,0.707106781186548,0.707106781186547,0.707106781186547,
0.707106781186548,0.707106781186548,0.707106781186547,0.707106781186547,
0.707106781186547,0.707106781186547,0.707106781186547,0.707106781186548,
0.707106781186547,0.707106781186547,0.707106781186548,0.707106781186547,
0.707106781186548,0.707106781186548,0.707106781186547,0.707106781186548,
0.707106781186547,0.707106781186548,0.707106781186547,0.707106781186548,
0.707106781186547,0.707106781186547,0.707106781186547,0.707106781186547,
0.707106781186547,0.707106781186547,0.707106781186548,0.707106781186547,
0.707106781186548,0.707106781186547,0.707106781186547,0.707106781186547,
0.707106781186548,0.707106781186547,0.707106781186548,0.707106781186548,
0.707106781186547,0.707106781186547,0.707106781186548,0.707106781186547,
0.707106781186548,0.707106781186547,0.707106781186548,0.707106781186547,
0.707106781186548,0.707106781186547,0.707106781186547,0.707106781186548,
0.707106781186547,0.707106781186548,0.707106781186547,0.707106781186548,
0.707106781186548,0.707106781186548,0.707106781186548,0.707106781186547,
0.707106781186548,0.707106781186548,0.707106781186548,0.707106781186547,
0.707106781186548,0.707106781186548,0.707106781186547,0.707106781186548,
0.707106781186547,0.707106781186548,0.707106781186547,0.707106781186547,
0.707106781186547,0.707106781186548,0.707106781186548,0.707106781186547,
0.707106781186548,0.707106781186547,0.707106781186548,0.707106781186547,
0.707106781186548,0.707106781186548,0.707106781186547,0.707106781186548,
0.707106781186547,0.707106781186547,0.707106781186548,0.707106781186547,
0.707106781186547,0.707106781186547,0.707106781186548,0.707106781186547,
0.707106781186548,0.707106781186548,0.707106781186547,0.707106781186548,
0.707106781186547,0.707106781186548,0.707106781186548,0.707106781186548,
0.707106781186548,0.707106781186547,0.707106781186548,0.707106781186547,
0.707106781186548,0.707106781186547,0.707106781186548,0.707106781186547,
0.707106781186547,0.707106781186547,0.707106781186547,0.707106781186548,
0.707106781186547,0.707106781186548,0.707106781186547,0.707106781186547,
0.707106781186548,0.707106781186547,0.707106781186548,0.707106781186547,
0.707106781186548,0.707106781186547,0.707106781186548,0.707106781186548,
0.707106781186548,0.707106781186548,0.707106781186547,0.707106781186548,
0.707106781186548,0.707106781186547,0.707106781186548,0.707106781186547,
0.707106781186548,0.707106781186547,0.707106781186548,0.707106781186547,
0.707106781186547,0.707106781186548,0.707106781186547,0.707106781186548,
0.707106781186547,0.707106781186547,0.707106781186548,0.707106781186547,
0.707106781186548,0.707106781186547,0.707106781186547,0.707106781186548,
0.707106781186548,0.707106781186548,0.707106781186548,0.707106781186548,
0.707106781186548,0.707106781186548,0.707106781186548,0.707106781186548,
0.707106781186547,0.707106781186548,0.707106781186547,0.707106781186547,
0.707106781186548,0.707106781186547,0.707106781186548,0.707106781186548,
0.707106781186547,0.707106781186547,0.707106781186548,0.707106781186548,
0.707106781186547,0.707106781186547,0.707106781186547,0.707106781186547,
0.707106781186547,0.707106781186548,0.707106781186547,0.707106781186548,
0.707106781186548,0.707106781186548,0.707106781186547,0.707106781186548,
0.707106781186547,0.707106781186548,0.707106781186547,0.707106781186548,
0.707106781186547,0.707106781186548,0.707106781186548,0.707106781186547,
0.707106781186547,0.707106781186548,0.707106781186548,0.707106781186548,
0.707106781186547,0.707106781186547,0.707106781186548,0.707106781186547,
0.707106781186547,0.707106781186548,0.707106781186547,0.707106781186548,
0.707106781186547,0.707106781186547,0.707106781186548,0.707106781186548,
0.707106781186548,0.707106781186547,0.707106781186547,0.707106781186548,
0.707106781186547,0.707106781186548,0.707106781186547,0.707106781186548,
0.707106781186547,0.707106781186548,0.707106781186548,0.707106781186547,
0.707106781186548,0.707106781186547,0.707106781186548,0.707106781186547,
0.707106781186547,0.707106781186547,0.707106781186548,0.707106781186547,
0.707106781186548,0.707106781186547,0.707106781186547,0.707106781186547,
0.707106781186548,0.707106781186547,0.707106781186547,0.707106781186548,
0.707106781186548,0.707106781186547,0.707106781186548,0.707106781186547,
0.707106781186548,0.707106781186548,0.707106781186547,0.707106781186548,
0.707106781186547,0.707106781186547,0.707106781186548,0.707106781186547,
0.707106781186547,0.707106781186547,0.707106781186548,0.707106781186547,
0.707106781186548,0.707106781186547,0.707106781186548,0.707106781186548,
0.707106781186548,0.707106781186547,0.707106781186548,0.707106781186548,
0.707106781186548,0.707106781186547,0.707106781186548,0.707106781186547,
0.707106781186547,0.707106781186548,0.707106781186547,0.707106781186547,
0.707106781186548,0.707106781186548,0.707106781186547,0.707106781186548,
0.707106781186547,0.707106781186548,0.707106781186548,0.707106781186547,
0.707106781186548,0.707106781186547,0.707106781186548,0.707106781186547,
0.707106781186548,0.707106781186547,0.707106781186548,0.707106781186548,
0.707106781186548,0.707106781186547,0.707106781186548,0.707106781186548,
0.707106781186547,0.707106781186547,0.707106781186548,0.707106781186547,
0.707106781186548,0.707106781186548,0.707106781186547,0.707106781186548,
0.707106781186548,0.707106781186547,0.707106781186548,0.707106781186548,
0.707106781186547,0.707106781186547,0.707106781186548,0.707106781186547,
0.707106781186548,0.707106781186547,0.707106781186548,0.707106781186547,
0.707106781186548,0.707106781186548,0.707106781186548,0.707106781186547,
0.707106781186548,0.707106781186547,0.707106781186548,0.707106781186547,
0.707106781186548,0.707106781186547,0.707106781186548,0.707106781186547,
0.707106781186548,0.707106781186547,0.707106781186548,0.707106781186547,
0.707106781186547,0.707106781186547,0.707106781186548,0.707106781186547,
0.707106781186548,0.707106781186547,0.707106781186548,0.707106781186547,
0.707106781186548,0.707106781186547,0.707106781186548,0.707106781186548,
0.707106781186548,0.707106781186547,0.707106781186548,0.707106781186547,
0.707106781186548,0.707106781186548,0.707106781186547,0.707106781186548,
0.707106781186547,0.707106781186548,0.707106781186547,0.707106781186548,
0.707106781186547,0.707106781186548,0.707106781186547,0.707106781186547,
0.707106781186547,0.707106781186548,0.707106781186547,0.707106781186547,
0.707106781186548,0.707106781186547,0.707106781186548,0.707106781186547,
0.707106781186547,0.707106781186548,0.707106781186547,0.707106781186548,
0.707106781186547,0.707106781186548,0.707106781186548,0.707106781186548,
0.707106781186547,0.707106781186547,0.707106781186548,0.707106781186548,
0.707106781186547,0.707106781186548,0.707106781186547,0.707106781186547,
0.707106781186547,0.707106781186548,0.707106781186547,0.707106781186548,
0.707106781186547,0.707106781186548,0.707106781186548,0.707106781186548,
0.707106781186547,0.707106781186547,0.707106781186547,0.707106781186547,
0.707106781186547,0.707106781186547,0.707106781186548,0.707106781186547,
0.707106781186548,0.707106781186547,0.707106781186548,0.707106781186547,
0.707106781186547,0.707106781186548,0.707106781186547,0.707106781186547,
0.707106781186548,0.707106781186548,0.707106781186547,0.707106781186547,
0.707106781186547,0.707106781186548,0.707106781186547,0.707106781186547,
0.707106781186548,0.707106781186548),(1.,1.,1.,1.,1.,1.,1.,1.,1.,1.,1.,
1.,1.,1.,1.,1.,1.,1.,1.,1.,1.,1.,1.,1.,1.,1.,1.,1.,1.,1.,1.,1.,1.,1.,1.,
1.,1.,1.,1.,1.,1.,1.,1.,1.,1.,1.,1.,1.,1.,1.,1.,1.,1.,1.,1.,1.,1.,1.,1.,
1.,1.,1.,1.,1.,1.,1.,1.,1.,1.,1.,1.,1.,1.,1.,1.,1.,1.,1.,1.,1.,1.,1.,1.,
1.,1.,1.,1.,1.,1.,1.,1.,1.,1.,1.,1.,1.,1.,1.,1.,1.,1.,1.,1.,1.,1.,1.,1.,
1.,1.,1.,1.,1.,1.,1.,1.,1.,1.,1.,1.,1.,1.,1.,1.,1.,1.,1.,1.,1.,1.,1.,1.,
1.,1.,1.,1.,1.,1.,1.,1.,1.,1.,1.,1.,1.,1.,1.,1.,1.,1.,1.,1.,1.,1.,1.,1.,
1.,1.,1.,1.,1.,1.,1.,1.,1.,1.,1.,1.,1.,1.,1.,1.,1.,1.,1.,1.,1.,1.,1.,1.,
1.,1.,1.,1.,1.,1.,1.,1.,1.,1.,1.,1.,1.,1.,1.,1.,1.,1.,1.,1.,1.,1.,1.,1.,
1.,1.,1.,1.,1.,1.,1.,1.,1.,1.,1.,1.,1.,1.,1.,1.,1.,1.,1.,1.,1.,1.,1.,1.,
1.,1.,1.,1.,1.,1.,1.,1.,1.,1.,1.,1.,1.,1.,1.,1.,1.,1.,1.,1.,1.,1.,1.,1.,
1.,1.,1.,1.,1.,1.,1.,1.,1.,1.,1.,1.,1.,1.,1.,1.,1.,1.,1.,1.,1.,1.,1.,1.,
1.,1.,1.,1.,1.,1.,1.,1.,1.,1.,1.,1.,1.,1.,1.,1.,1.,1.,1.,1.,1.,1.,1.,1.,
1.,1.,1.,1.,1.,1.,1.,1.,1.,1.,1.,1.,1.,1.,1.,1.,1.,1.,1.,1.,1.,1.,1.,1.,
1.,1.,1.,1.,1.,1.,1.,1.,1.,1.,1.,1.,1.,1.,1.,1.,1.,1.,1.,1.,1.,1.,1.,1.,
1.,1.,1.,1.,1.,1.,1.,1.,1.,1.,1.,1.,1.,1.,1.,1.,1.,1.,1.,1.,1.,1.,1.,1.,
1.,1.,1.,1.,1.,1.,1.,1.,1.,1.,1.,1.,1.,1.,1.,1.,1.,1.,1.,1.,1.,1.,1.,1.,
1.,1.,1.,1.,1.,1.,1.,1.,1.,1.,1.,1.,1.,1.,1.,1.,1.,1.,1.,1.,1.,1.,1.,1.,
1.,1.,1.,1.,1.,1.,1.,1.,1.,1.,1.,1.,1.,1.,1.,1.,1.,1.,1.,1.,1.,1.,1.,1.,
1.,1.,1.,1.,1.,1.,1.,1.,1.,1.,1.,1.,1.,1.,1.,1.,1.,1.,1.,1.,1.,1.,1.,1.,
1.,1.,1.,1.,1.,1.,1.,1.,1.,1.,1.,1.,1.,1.,1.,1.,1.,1.,1.,1.,1.,1.,1.,1.,
1.,1.,1.,1.,1.,1.,1.,1.,1.,1.,1.,1.,1.,1.,1.,1.,1.,1.,1.,1.,1.,1.,1.,1.,
1.,1.,1.,1.,1.,1.,1.,1.,1.,1.,1.,1.,1.,1.,1.,1.,1.,1.,1.,1.,1.,1.,1.,1.,
1.,1.,1.,1.,1.,1.,1.,1.,1.,1.,1.,1.,1.,1.,1.,1.,1.,1.,1.,1.,1.,1.,1.,1.,
1.,1.,1.,1.,1.,1.,1.,1.,1.,1.,1.,1.,1.,1.,1.,1.,1.,1.,1.,1.,1.,1.,1.,1.,
1.,1.,1.,1.,1.,1.,1.,1.,1.,1.,1.,1.,1.,1.,1.,1.,1.,1.,1.,1.,1.,1.,1.,1.,
1.,1.,1.,1.,1.,1.,1.,1.,1.,1.,1.,1.,1.,1.,1.,1.,1.,1.,1.,1.,1.,1.,1.,1.,
1.,1.,1.,1.,1.,1.,1.,1.,1.,1.,1.,1.,1.,1.,1.,1.,1.,1.,1.,1.,1.,1.,1.,1.,
1.,1.,1.,1.,1.,1.,1.,1.,1.,1.,1.,1.,1.,1.,1.,1.,1.,1.,1.,1.,1.,1.,1.,1.,
1.,1.,1.,1.,1.,1.,1.,1.,1.,1.,1.,1.,1.,1.,1.,1.,1.,1.,1.,1.,1.,1.,1.,1.,
1.,1.,1.,1.,1.,1.,1.,1.,1.,1.,1.,1.,1.,1.,1.,1.,1.,1.,1.,1.,1.,1.,1.,1.,
1.,1.,1.,1.,1.,1.,1.,1.,1.,1.,1.,1.,1.,1.,1.,1.,1.,1.,1.,1.,1.,1.,1.,1.,
1.,1.,1.,1.,1.,1.,1.,1.,1.,1.,1.,1.,1.,1.,1.,1.,1.,1.,1.,1.,1.,1.,1.,1.,
1.,1.,1.,1.,1.,1.,1.,1.,1.,1.,1.,1.,1.,1.,1.,1.,1.,1.,1.,1.,1.,1.,1.,1.,
1.,1.,1.,1.,1.,1.,1.,1.,1.,1.,1.,1.,1.,1.,1.,1.,1.,1.,1.,1.,1.,1.,1.,1.,
1.,1.,1.,1.,1.,1.,1.,1.,1.,1.,1.,1.,1.,1.,1.,1.,1.,1.,1.,1.,1.,1.,1.,1.,
1.,1.,1.,1.,1.,1.,1.,1.,1.,1.,1.,1.,1.,1.,1.,1.,1.,1.,1.,1.,1.,1.,1.,1.,
1.,1.,1.,1.,1.,1.,1.,1.,1.,1.,1.,1.,1.,1.,1.,1.,1.,1.,1.,1.,1.,1.,1.,1.,
1.,1.,1.,1.,1.,1.,1.,1.,1.,1.,1.,1.,1.,1.,1.,1.,1.,1.,1.,1.,1.,1.,1.,1.,
1.,1.,1.,1.,1.,1.,1.,1.,1.,1.,1.,1.,1.,1.,1.,1.,1.,1.,1.,1.,1.,1.,1.,1.,
1.,1.,1.,1.,1.,1.,1.,1.,1.,1.,1.,1.,1.,1.,1.,1.,1.,1.,1.,1.,1.,1.,1.,1.,
1.,1.,1.,1.,1.,1.,1.,1.,1.,1.,1.,1.,1.,1.,1.,1.,1.,1.,1.,1.,1.,1.,1.,1.,
1.,1.,1.,1.,1.,1.,1.,1.,1.,1.,1.,1.,1.,1.,1.,1.,1.,1.,1.,1.,1.,1.,1.,1.,
1.,1.,1.,1.,1.,1.,1.,1.,1.,1.,1.,1.,1.,1.,1.,1.,1.,1.,1.,1.,1.,1.,1.,1.,
1.,1.,1.,1.,1.,1.,1.,1.,1.,1.,1.,1.,1.,1.,1.,1.,1.,1.,1.,1.,1.,1.,1.,1.,
1.,1.,1.,1.,1.,1.,1.,1.,1.,1.,1.,1.,1.,1.,1.,1.,1.,1.,1.,1.,1.,1.,1.,1.,
1.,1.,1.,1.,1.,1.,1.,1.,1.,1.,1.,1.,1.,1.,1.,1.,1.,1.,1.,1.,1.,1.,1.,1.,
1.,1.,1.,1.,1.,1.,1.,1.,1.,1.,1.,1.,1.,1.,1.,1.,1.,1.,1.,1.,1.,1.,1.,1.,
1.,1.,1.,1.,1.,1.,1.,1.,1.,1.,1.,1.,1.,1.,1.,1.,1.,1.,1.,1.,1.,1.,1.,1.,
1.,1.,1.,1.,1.,1.,1.,1.,1.,1.,1.,1.,1.,1.,1.,1.,1.,1.,1.,1.,1.,1.,1.,1.,
1.,1.,1.,1.,1.,1.,1.,1.,1.,1.,1.,1.,1.,1.,1.,1.,1.,1.,1.,1.,1.,1.,1.,1.,
1.,1.,1.,1.,1.,1.,1.,1.,1.,1.,1.,1.,1.,1.,1.,1.,1.,1.,1.,1.,1.,1.,1.,1.,
1.,1.,1.,1.,1.,1.,1.,1.,1.,1.,1.,1.,1.,1.,1.,1.,1.,1.,1.,1.,1.,1.,1.,1.,
1.,1.,1.,1.,1.,1.,1.,1.,1.,1.,1.,1.,1.,1.,1.,1.,1.,1.,1.,1.,1.,1.,1.,1.,
1.,1.,1.,1.,1.,1.,1.,1.,1.,1.,1.,1.,1.,1.,1.,1.,1.,1.,1.,1.,1.,1.,1.,1.,
1.,1.,1.,1.,1.,1.,1.,1.,1.,1.,1.,1.,1.,1.,1.,1.,1.,1.,1.,1.,1.,1.,1.,1.,
1.,1.,1.,1.,1.,1.,1.,1.,1.,1.,1.,1.,1.,1.,1.,1.,1.,1.,1.,1.,1.,1.,1.,1.,
1.,1.,1.,1.,1.,1.,1.,1.,1.,1.,1.,1.,1.,1.,1.,1.,1.,1.,1.,1.,1.,1.,1.,1.,
1.,1.,1.,1.,1.,1.,1.,1.,1.,1.,1.,1.,1.,1.,1.,1.,1.,1.,1.,1.,1.,1.,1.,1.,
1.,1.,1.,1.,1.,1.,1.,1.,1.,1.,1.,1.,1.,1.,1.,1.,1.,1.,1.,1.,1.,1.,1.,1.,
1.,1.,1.,1.,1.,1.,1.,1.,1.,1.,1.,1.,1.,1.,1.,1.,1.,1.,1.,1.,1.,1.,1.,1.,
1.,1.,1.,1.,1.,1.,1.,1.,1.,1.,1.,1.,1.,1.,1.,1.,1.,1.,1.,1.,1.,1.,1.,1.,
1.,1.,1.,1.,1.,1.,1.,1.,1.,1.,1.,1.,1.,1.,1.,1.,1.,1.,1.,1.,1.,1.,1.,1.,
1.,1.,1.,1.,1.,1.,1.,1.,1.,1.,1.,1.,1.,1.,1.,1.,1.,1.,1.,1.,1.,1.,1.,1.,
1.,1.,1.,1.,1.,1.,1.,1.,1.,1.,1.,1.,1.,1.,1.,1.,1.,1.,1.,1.,1.,1.,1.,1.,
1.,1.,1.,1.,1.,1.,1.,1.,1.,1.,1.,1.,1.,1.,1.,1.,1.,1.,1.,1.,1.,1.,1.,1.,
1.,1.,1.,1.,1.,1.,1.,1.,1.,1.,1.,1.,1.,1.,1.,1.,1.,1.,1.,1.,1.,1.,1.,1.,
1.,1.,1.,1.,1.,1.,1.,1.,1.,1.,1.,1.,1.,1.,1.,1.,1.,1.,1.,1.,1.,1.,1.,1.,
1.,1.,1.,1.,1.,1.,1.,1.,1.,1.,1.,1.,1.,1.,1.,1.,1.,1.,1.,1.,1.,1.,1.,1.,
1.,1.,1.,1.,1.,1.,1.,1.,1.,1.,1.,1.,1.,1.,1.,1.,1.,1.,1.,1.,1.,1.,1.,1.,
1.,1.,1.,1.,1.,1.,1.,1.,1.,1.,1.,1.,1.,1.,1.,1.,1.,1.,1.,1.,1.,1.,1.,1.,
1.,1.,1.,1.,1.,1.,1.,1.,1.,1.,1.,1.,1.,1.,1.,1.,1.,1.,1.,1.,1.,1.,1.,1.,
1.,1.,1.,1.,1.,1.,1.,1.,1.,1.,1.,1.,1.,1.,1.,1.,1.,1.,1.,1.,1.,1.,1.,1.,
1.,1.,1.,1.,1.,1.,1.,1.,1.,1.,1.,1.,1.,1.,1.,1.,1.,1.,1.,1.,1.,1.,1.,1.,
1.,1.,1.,1.,1.,1.,1.,1.,1.,1.,1.,1.,1.,1.,1.,1.,1.,1.,1.,1.,1.,1.,1.,1.,
1.,1.,1.,1.,1.,1.,1.,1.,1.,1.,1.,1.,1.,1.,1.,1.,1.,1.,1.,1.,1.,1.,1.,1.,
1.,1.,1.,1.,1.,1.,1.,1.,1.,1.,1.,1.,1.,1.,1.,1.,1.,1.,1.,1.,1.,1.,1.,1.,
1.,1.,1.,1.,1.,1.,1.,1.,1.,1.,1.,1.,1.,1.,1.,1.,1.,1.,1.,1.,1.,1.,1.,1.,
1.,1.,1.,1.,1.,1.,1.,1.,1.,1.,1.,1.,1.,1.,1.,1.,1.,1.,1.,1.,1.,1.,1.,1.,
1.,1.,1.,1.,1.,1.,1.,1.,1.,1.,1.,1.,1.,1.,1.,1.,1.,1.,1.,1.,1.,1.,1.,1.,
1.,1.,1.,1.,1.,1.,1.,1.,1.,1.,1.,1.,1.,1.,1.,1.,1.,1.,1.,1.,1.,1.,1.,1.,
1.,1.,1.,1.,1.,1.,1.,1.,1.,1.,1.,1.,1.,1.,1.,1.,1.,1.,1.,1.,1.,1.,1.,1.,
1.,1.,1.,1.,1.,1.,1.,1.,1.,1.,1.,1.,1.,1.,1.,1.,1.,1.,1.,1.,1.,1.,1.,1.,
1.,1.,1.,1.,1.,1.,1.,1.,1.,1.,1.,1.,1.,1.,1.,1.,1.,1.,1.,1.,1.,1.,1.,1.,
1.,1.,1.,1.,1.,1.,1.,1.,1.,1.,1.,1.,1.,1.,1.,1.,1.,1.,1.,1.,1.,1.,1.,1.,
1.,1.,1.,1.,1.,1.,1.,1.,1.,1.,1.,1.,1.,1.,1.,1.,1.,1.,1.,1.,1.,1.,1.,1.),
(0.707106781186548,0.707106781186548,0.707106781186548,0.707106781186547,
0.707106781186547,0.707106781186548,0.707106781186547,0.707106781186547,
0.707106781186547,0.707106781186547,0.707106781186547,0.707106781186548,
0.707106781186548,0.707106781186548,0.707106781186547,0.707106781186548,
0.707106781186547,0.707106781186547,0.707106781186548,0.707106781186547,
0.707106781186548,0.707106781186547,0.707106781186548,0.707106781186547,
0.707106781186548,0.707106781186547,0.707106781186547,0.707106781186547,
0.707106781186547,0.707106781186547,0.707106781186548,0.707106781186547,
0.707106781186547,0.707106781186548,0.707106781186547,0.707106781186547,
0.707106781186548,0.707106781186547,0.707106781186547,0.707106781186548,
0.707106781186548,0.707106781186547,0.707106781186548,0.707106781186547,
0.707106781186547,0.707106781186547,0.707106781186548,0.707106781186548,
0.707106781186547,0.707106781186547,0.707106781186548,0.707106781186547,
0.707106781186548,0.707106781186547,0.707106781186547,0.707106781186547,
0.707106781186547,0.707106781186547,0.707106781186548,0.707106781186547,
0.707106781186548,0.707106781186547,0.707106781186548,0.707106781186547,
0.707106781186548,0.707106781186547,0.707106781186547,0.707106781186548,
0.707106781186547,0.707106781186547,0.707106781186548,0.707106781186547,
0.707106781186548,0.707106781186547,0.707106781186548,0.707106781186548,
0.707106781186547,0.707106781186548,0.707106781186547,0.707106781186547,
0.707106781186548,0.707106781186547,0.707106781186547,0.707106781186547,
0.707106781186548,0.707106781186547,0.707106781186547,0.707106781186547,
0.707106781186547,0.707106781186547,0.707106781186547,0.707106781186548,
0.707106781186548,0.707106781186547,0.707106781186548,0.707106781186547,
0.707106781186548,0.707106781186548,0.707106781186547,0.707106781186548,
0.707106781186548,0.707106781186548,0.707106781186547,0.707106781186548,
0.707106781186547,0.707106781186548,0.707106781186548,0.707106781186548,
0.707106781186547,0.707106781186547,0.707106781186547,0.707106781186548,
0.707106781186548,0.707106781186548,0.707106781186547,0.707106781186547,
0.707106781186547,0.707106781186548,0.707106781186548,0.707106781186547,
0.707106781186547,0.707106781186548,0.707106781186547,0.707106781186547,
0.707106781186547,0.707106781186547,0.707106781186548,0.707106781186547,
0.707106781186548,0.707106781186547,0.707106781186547,0.707106781186547,
0.707106781186548,0.707106781186548,0.707106781186547,0.707106781186548,
0.707106781186548,0.707106781186547,0.707106781186548,0.707106781186547,
0.707106781186548,0.707106781186547,0.707106781186548,0.707106781186547,
0.707106781186547,0.707106781186548,0.707106781186547,0.707106781186547,
0.707106781186548,0.707106781186547,0.707106781186547,0.707106781186548,
0.707106781186547,0.707106781186548,0.707106781186547,0.707106781186547,
0.707106781186548,0.707106781186548,0.707106781186547,0.707106781186548,
0.707106781186547,0.707106781186548,0.707106781186547,0.707106781186548,
0.707106781186547,0.707106781186548,0.707106781186547,0.707106781186548,
0.707106781186547,0.707106781186548,0.707106781186547,0.707106781186548,
0.707106781186547,0.707106781186547,0.707106781186548,0.707106781186547,
0.707106781186548,0.707106781186547,0.707106781186548,0.707106781186547,
0.707106781186548,0.707106781186547,0.707106781186547,0.707106781186548,
0.707106781186547,0.707106781186548,0.707106781186548,0.707106781186548,
0.707106781186547,0.707106781186547,0.707106781186547,0.707106781186547,
0.707106781186548,0.707106781186547,0.707106781186548,0.707106781186548,
0.707106781186547,0.707106781186547,0.707106781186548,0.707106781186548,
0.707106781186547,0.707106781186547,0.707106781186548,0.707106781186547,
0.707106781186548,0.707106781186547,0.707106781186547,0.707106781186547,
0.707106781186547,0.707106781186547,0.707106781186547,0.707106781186547,
0.707106781186548,0.707106781186547,0.707106781186548,0.707106781186547,
0.707106781186548,0.707106781186548,0.707106781186547,0.707106781186548,
0.707106781186548,0.707106781186548,0.707106781186548,0.707106781186547,
0.707106781186548,0.707106781186547,0.707106781186548,0.707106781186547,
0.707106781186547,0.707106781186548,0.707106781186548,0.707106781186547,
0.707106781186547,0.707106781186547,0.707106781186547,0.707106781186547,
0.707106781186548,0.707106781186548,0.707106781186547,0.707106781186547,
0.707106781186548,0.707106781186548,0.707106781186547,0.707106781186548,
0.707106781186547,0.707106781186548,0.707106781186548,0.707106781186547,
0.707106781186547,0.707106781186548,0.707106781186547,0.707106781186547,
0.707106781186548,0.707106781186547,0.707106781186548,0.707106781186547,
0.707106781186548,0.707106781186547,0.707106781186547,0.707106781186548,
0.707106781186548,0.707106781186547,0.707106781186547,0.707106781186548,
0.707106781186547,0.707106781186547,0.707106781186548,0.707106781186547,
0.707106781186548,0.707106781186547,0.707106781186548,0.707106781186547,
0.707106781186548,0.707106781186547,0.707106781186547,0.707106781186547,
0.707106781186547,0.707106781186547,0.707106781186547,0.707106781186548,
0.707106781186547,0.707106781186548,0.707106781186547,0.707106781186548,
0.707106781186548,0.707106781186547,0.707106781186548,0.707106781186548,
0.707106781186547,0.707106781186548,0.707106781186547,0.707106781186547,
0.707106781186547,0.707106781186548,0.707106781186547,0.707106781186547,
0.707106781186548,0.707106781186547,0.707106781186548,0.707106781186547,
0.707106781186547,0.707106781186547,0.707106781186548,0.707106781186548,
0.707106781186547,0.707106781186548,0.707106781186548,0.707106781186547,
0.707106781186548,0.707106781186547,0.707106781186548,0.707106781186548,
0.707106781186547,0.707106781186548,0.707106781186548,0.707106781186548,
0.707106781186547,0.707106781186547,0.707106781186548,0.707106781186547,
0.707106781186548,0.707106781186547,0.707106781186547,0.707106781186548,
0.707106781186548,0.707106781186548,0.707106781186547,0.707106781186547,
0.707106781186548,0.707106781186548,0.707106781186547,0.707106781186547,
0.707106781186548,0.707106781186547,0.707106781186547,0.707106781186548,
0.707106781186548,0.707106781186547,0.707106781186547,0.707106781186547,
0.707106781186548,0.707106781186547,0.707106781186547,0.707106781186547,
0.707106781186548,0.707106781186548,0.707106781186547,0.707106781186548,
0.707106781186547,0.707106781186548,0.707106781186547,0.707106781186548,
0.707106781186548,0.707106781186547,0.707106781186547,0.707106781186548,
0.707106781186547,0.707106781186547,0.707106781186548,0.707106781186547,
0.707106781186548,0.707106781186548,0.707106781186547,0.707106781186548,
0.707106781186547,0.707106781186547,0.707106781186547,0.707106781186548,
0.707106781186548,0.707106781186548,0.707106781186547,0.707106781186548,
0.707106781186547,0.707106781186548,0.707106781186547,0.707106781186547,
0.707106781186547,0.707106781186547,0.707106781186548,0.707106781186548,
0.707106781186547,0.707106781186547,0.707106781186548,0.707106781186547,
0.707106781186548,0.707106781186547,0.707106781186548,0.707106781186547,
0.707106781186547,0.707106781186548,0.707106781186547,0.707106781186548,
0.707106781186547,0.707106781186548,0.707106781186548,0.707106781186547,
0.707106781186548,0.707106781186547,0.707106781186548,0.707106781186548,
0.707106781186547,0.707106781186548,0.707106781186547,0.707106781186547,
0.707106781186548,0.707106781186547,0.707106781186548,0.707106781186547,
0.707106781186548,0.707106781186547,0.707106781186547,0.707106781186548,
0.707106781186548,0.707106781186548,0.707106781186548,0.707106781186547,
0.707106781186548,0.707106781186548,0.707106781186548,0.707106781186547,
0.707106781186548,0.707106781186548,0.707106781186548,0.707106781186547,
0.707106781186547,0.707106781186548,0.707106781186547,0.707106781186548,
0.707106781186547,0.707106781186548,0.707106781186548,0.707106781186547,
0.707106781186547,0.707106781186548,0.707106781186547,0.707106781186548,
0.707106781186547,0.707106781186548,0.707106781186548,0.707106781186547,
0.707106781186547,0.707106781186547,0.707106781186548,0.707106781186548,
0.707106781186547,0.707106781186547,0.707106781186548,0.707106781186548,
0.707106781186548,0.707106781186548,0.707106781186547,0.707106781186547,
0.707106781186548,0.707106781186548,0.707106781186547,0.707106781186548,
0.707106781186547,0.707106781186548,0.707106781186547,0.707106781186548,
0.707106781186547,0.707106781186547,0.707106781186548,0.707106781186547,
0.707106781186547,0.707106781186548,0.707106781186547,0.707106781186548,
0.707106781186547,0.707106781186548,0.707106781186547,0.707106781186548,
0.707106781186547,0.707106781186548,0.707106781186547,0.707106781186548,
0.707106781186547,0.707106781186547,0.707106781186548,0.707106781186548,
0.707106781186547,0.707106781186547,0.707106781186547,0.707106781186548,
0.707106781186547,0.707106781186548,0.707106781186547,0.707106781186548,
0.707106781186547,0.707106781186548,0.707106781186547,0.707106781186547,
0.707106781186547,0.707106781186548,0.707106781186547,0.707106781186548,
0.707106781186548,0.707106781186547,0.707106781186548,0.707106781186547,
0.707106781186547,0.707106781186548,0.707106781186547,0.707106781186547,
0.707106781186548,0.707106781186547,0.707106781186547,0.707106781186547,
0.707106781186547,0.707106781186548,0.707106781186547,0.707106781186547,
0.707106781186547,0.707106781186548,0.707106781186547,0.707106781186547,
0.707106781186548,0.707106781186548,0.707106781186547,0.707106781186548,
0.707106781186548,0.707106781186547,0.707106781186547,0.707106781186548,
0.707106781186547,0.707106781186547,0.707106781186548,0.707106781186547,
0.707106781186547,0.707106781186547,0.707106781186548,0.707106781186547,
0.707106781186548,0.707106781186547,0.707106781186548,0.707106781186547,
0.707106781186548,0.707106781186547,0.707106781186548,0.707106781186547,
0.707106781186548,0.707106781186548,0.707106781186547,0.707106781186547,
0.707106781186548,0.707106781186547,0.707106781186548,0.707106781186547,
0.707106781186548,0.707106781186548,0.707106781186547,0.707106781186548,
0.707106781186547,0.707106781186548,0.707106781186548,0.707106781186547,
0.707106781186547,0.707106781186548,0.707106781186547,0.707106781186548,
0.707106781186547,0.707106781186548,0.707106781186547,0.707106781186548,
0.707106781186547,0.707106781186547,0.707106781186547,0.707106781186547,
0.707106781186547,0.707106781186547,0.707106781186547,0.707106781186547,
0.707106781186548,0.707106781186547,0.707106781186548,0.707106781186547,
0.707106781186547,0.707106781186548,0.707106781186547,0.707106781186548,
0.707106781186547,0.707106781186547,0.707106781186548,0.707106781186547,
0.707106781186548,0.707106781186547,0.707106781186548,0.707106781186547,
0.707106781186548,0.707106781186547,0.707106781186548,0.707106781186547,
0.707106781186548,0.707106781186547,0.707106781186548,0.707106781186548,
0.707106781186547,0.707106781186548,0.707106781186547,0.707106781186547,
0.707106781186547,0.707106781186548,0.707106781186547,0.707106781186547,
0.707106781186547,0.707106781186548,0.707106781186547,0.707106781186547,
0.707106781186548,0.707106781186547,0.707106781186547,0.707106781186547,
0.707106781186547,0.707106781186548,0.707106781186547,0.707106781186547,
0.707106781186547,0.707106781186548,0.707106781186548,0.707106781186548,
0.707106781186548,0.707106781186547,0.707106781186548,0.707106781186547,
0.707106781186547,0.707106781186548,0.707106781186547,0.707106781186548,
0.707106781186547,0.707106781186547,0.707106781186548,0.707106781186547,
0.707106781186547,0.707106781186547,0.707106781186547,0.707106781186548,
0.707106781186548,0.707106781186547,0.707106781186547,0.707106781186548,
0.707106781186547,0.707106781186548,0.707106781186547,0.707106781186548,
0.707106781186548,0.707106781186547,0.707106781186547,0.707106781186548,
0.707106781186548,0.707106781186547,0.707106781186548,0.707106781186548,
0.707106781186547,0.707106781186548,0.707106781186548,0.707106781186548,
0.707106781186547,0.707106781186548,0.707106781186547,0.707106781186548,
0.707106781186547,0.707106781186548,0.707106781186547,0.707106781186548,
0.707106781186547,0.707106781186548,0.707106781186548,0.707106781186547,
0.707106781186547,0.707106781186548,0.707106781186547,0.707106781186548,
0.707106781186547,0.707106781186548,0.707106781186548,0.707106781186548,
0.707106781186548,0.707106781186548,0.707106781186547,0.707106781186547,
0.707106781186547,0.707106781186547,0.707106781186548,0.707106781186547,
0.707106781186548,0.707106781186547,0.707106781186547,0.707106781186548,
0.707106781186548,0.707106781186547,0.707106781186548,0.707106781186547,
0.707106781186548,0.707106781186548,0.707106781186547,0.707106781186547,
0.707106781186548,0.707106781186547,0.707106781186548,0.707106781186547,
0.707106781186548,0.707106781186547,0.707106781186548,0.707106781186547,
0.707106781186548,0.707106781186547,0.707106781186548,0.707106781186547,
0.707106781186548,0.707106781186548,0.707106781186547,0.707106781186548,
0.707106781186547,0.707106781186548,0.707106781186547,0.707106781186548,
0.707106781186548,0.707106781186548,0.707106781186547,0.707106781186547,
0.707106781186548,0.707106781186548,0.707106781186547,0.707106781186547,
0.707106781186547,0.707106781186548,0.707106781186547,0.707106781186548,
0.707106781186547,0.707106781186548,0.707106781186547,0.707106781186547,
0.707106781186547,0.707106781186548,0.707106781186547,0.707106781186548,
0.707106781186547,0.707106781186548,0.707106781186547,0.707106781186548,
0.707106781186547,0.707106781186547,0.707106781186548,0.707106781186547,
0.707106781186547,0.707106781186548,0.707106781186547,0.707106781186547,
0.707106781186548,0.707106781186547,0.707106781186547,0.707106781186547,
0.707106781186548,0.707106781186547,0.707106781186548,0.707106781186547,
0.707106781186547,0.707106781186547,0.707106781186548,0.707106781186548,
0.707106781186547,0.707106781186547,0.707106781186548,0.707106781186548,
0.707106781186548,0.707106781186547,0.707106781186548,0.707106781186547,
0.707106781186548,0.707106781186547,0.707106781186548,0.707106781186547,
0.707106781186547,0.707106781186547,0.707106781186547,0.707106781186548,
0.707106781186547,0.707106781186548,0.707106781186548,0.707106781186547,
0.707106781186548,0.707106781186547,0.707106781186547,0.707106781186547,
0.707106781186547,0.707106781186548,0.707106781186547,0.707106781186548,
0.707106781186547,0.707106781186548,0.707106781186548,0.707106781186547,
0.707106781186548,0.707106781186547,0.707106781186547,0.707106781186547,
0.707106781186547,0.707106781186548,0.707106781186547,0.707106781186548,
0.707106781186548,0.707106781186547,0.707106781186548,0.707106781186547,
0.707106781186548,0.707106781186547,0.707106781186547,0.707106781186548,
0.707106781186547,0.707106781186548,0.707106781186548,0.707106781186547,
0.707106781186547,0.707106781186548,0.707106781186548,0.707106781186547,
0.707106781186547,0.707106781186548,0.707106781186547,0.707106781186547,
0.707106781186548,0.707106781186547,0.707106781186547,0.707106781186548,
0.707106781186547,0.707106781186548,0.707106781186547,0.707106781186547,
0.707106781186548,0.707106781186547,0.707106781186548,0.707106781186547,
0.707106781186548,0.707106781186547,0.707106781186547,0.707106781186547,
0.707106781186548,0.707106781186547,0.707106781186548,0.707106781186547,
0.707106781186548,0.707106781186548,0.707106781186548,0.707106781186548,
0.707106781186547,0.707106781186547,0.707106781186547,0.707106781186548,
0.707106781186547,0.707106781186548,0.707106781186547,0.707106781186547,
0.707106781186548,0.707106781186547,0.707106781186547,0.707106781186548,
0.707106781186547,0.707106781186547,0.707106781186548,0.707106781186548,
0.707106781186547,0.707106781186548,0.707106781186547,0.707106781186547,
0.707106781186548,0.707106781186547,0.707106781186548,0.707106781186547,
0.707106781186548,0.707106781186547,0.707106781186547,0.707106781186547,
0.707106781186548,0.707106781186547,0.707106781186548,0.707106781186547,
0.707106781186548,0.707106781186547,0.707106781186547,0.707106781186548,
0.707106781186548,0.707106781186548,0.707106781186547,0.707106781186548,
0.707106781186547,0.707106781186548,0.707106781186547,0.707106781186548,
0.707106781186547,0.707106781186548,0.707106781186548,0.707106781186547,
0.707106781186547,0.707106781186547,0.707106781186548,0.707106781186547,
0.707106781186547,0.707106781186548,0.707106781186547,0.707106781186547,
0.707106781186548,0.707106781186547,0.707106781186548,0.707106781186548,
0.707106781186548,0.707106781186547,0.707106781186548,0.707106781186547,
0.707106781186548,0.707106781186547,0.707106781186548,0.707106781186547,
0.707106781186548,0.707106781186547,0.707106781186548,0.707106781186547,
0.707106781186548,0.707106781186548,0.707106781186547,0.707106781186548,
0.707106781186547,0.707106781186548,0.707106781186548,0.707106781186547,
0.707106781186547,0.707106781186548,0.707106781186547,0.707106781186547,
0.707106781186548,0.707106781186547,0.707106781186548,0.707106781186548,
0.707106781186547,0.707106781186548,0.707106781186548,0.707106781186548,
0.707106781186548,0.707106781186548,0.707106781186547,0.707106781186548,
0.707106781186548,0.707106781186548,0.707106781186547,0.707106781186548,
0.707106781186547,0.707106781186548,0.707106781186547,0.707106781186548,
0.707106781186547,0.707106781186548,0.707106781186547,0.707106781186548,
0.707106781186547,0.707106781186547,0.707106781186548,0.707106781186547,
0.707106781186547,0.707106781186548,0.707106781186547,0.707106781186548,
0.707106781186547,0.707106781186548,0.707106781186547,0.707106781186548,
0.707106781186547,0.707106781186547,0.707106781186548,0.707106781186547,
0.707106781186547,0.707106781186548,0.707106781186547,0.707106781186548,
0.707106781186547,0.707106781186547,0.707106781186548,0.707106781186548,
0.707106781186547,0.707106781186548,0.707106781186547,0.707106781186547,
0.707106781186547,0.707106781186548,0.707106781186547,0.707106781186547,
0.707106781186548,0.707106781186547,0.707106781186547,0.707106781186547,
0.707106781186548,0.707106781186548,0.707106781186547,0.707106781186548,
0.707106781186547,0.707106781186548,0.707106781186547,0.707106781186547,
0.707106781186548,0.707106781186547,0.707106781186548,0.707106781186547,
0.707106781186547,0.707106781186547,0.707106781186547,0.707106781186548,
0.707106781186547,0.707106781186547,0.707106781186547,0.707106781186547,
0.707106781186547,0.707106781186548,0.707106781186547,0.707106781186547,
0.707106781186547,0.707106781186547,0.707106781186548,0.707106781186547,
0.707106781186548,0.707106781186547,0.707106781186547,0.707106781186548,
0.707106781186547,0.707106781186548,0.707106781186547,0.707106781186547,
0.707106781186548,0.707106781186547,0.707106781186547,0.707106781186548,
0.707106781186547,0.707106781186547,0.707106781186547,0.707106781186547,
0.707106781186548,0.707106781186547,0.707106781186548,0.707106781186548,
0.707106781186547,0.707106781186548,0.707106781186548,0.707106781186547,
0.707106781186547,0.707106781186548,0.707106781186547,0.707106781186547,
0.707106781186547,0.707106781186548,0.707106781186547,0.707106781186547,
0.707106781186548,0.707106781186547,0.707106781186548,0.707106781186547,
0.707106781186548,0.707106781186547,0.707106781186547,0.707106781186548,
0.707106781186547,0.707106781186548,0.707106781186547,0.707106781186548,
0.707106781186547,0.707106781186548,0.707106781186547,0.707106781186548,
0.707106781186547,0.707106781186547,0.707106781186547,0.707106781186547,
0.707106781186548,0.707106781186548,0.707106781186547,0.707106781186548,
0.707106781186548,0.707106781186547,0.707106781186548,0.707106781186547,
0.707106781186547,0.707106781186548,0.707106781186547,0.707106781186547,
0.707106781186547,0.707106781186547,0.707106781186548,0.707106781186547,
0.707106781186547,0.707106781186547,0.707106781186548,0.707106781186547,
0.707106781186547,0.707106781186548,0.707106781186547,0.707106781186548,
0.707106781186548,0.707106781186547,0.707106781186548,0.707106781186547,
0.707106781186548,0.707106781186547,0.707106781186548,0.707106781186547,
0.707106781186547,0.707106781186548,0.707106781186547,0.707106781186548,
0.707106781186548,0.707106781186547,0.707106781186547,0.707106781186548,
0.707106781186547,0.707106781186548,0.707106781186547,0.707106781186548,
0.707106781186547,0.707106781186547,0.707106781186548,0.707106781186548,
0.707106781186547,0.707106781186548,0.707106781186548,0.707106781186547,
0.707106781186548,0.707106781186548,0.707106781186547,0.707106781186548,
0.707106781186547,0.707106781186548,0.707106781186547,0.707106781186548,
0.707106781186547,0.707106781186548,0.707106781186547,0.707106781186547,
0.707106781186548,0.707106781186547,0.707106781186547,0.707106781186548,
0.707106781186547,0.707106781186548,0.707106781186548,0.707106781186547,
0.707106781186547,0.707106781186547,0.707106781186548,0.707106781186547,
0.707106781186548,0.707106781186548,0.707106781186547,0.707106781186548,
0.707106781186547,0.707106781186548,0.707106781186547,0.707106781186548,
0.707106781186547,0.707106781186547,0.707106781186548,0.707106781186548,
0.707106781186548,0.707106781186547,0.707106781186548,0.707106781186548,
0.707106781186547,0.707106781186548,0.707106781186547,0.707106781186548,
0.707106781186548,0.707106781186548,0.707106781186548,0.707106781186548,
0.707106781186548,0.707106781186547,0.707106781186547,0.707106781186548,
0.707106781186547,0.707106781186547,0.707106781186548,0.707106781186547,
0.707106781186547,0.707106781186548,0.707106781186547,0.707106781186548,
0.707106781186547,0.707106781186548,0.707106781186547,0.707106781186547,
0.707106781186547,0.707106781186548,0.707106781186547,0.707106781186547,
0.707106781186548,0.707106781186547,0.707106781186548,0.707106781186547,
0.707106781186548,0.707106781186547,0.707106781186547,0.707106781186547,
0.707106781186547,0.707106781186548,0.707106781186547,0.707106781186547,
0.707106781186548,0.707106781186548,0.707106781186547,0.707106781186548,
0.707106781186547,0.707106781186548,0.707106781186547,0.707106781186547,
0.707106781186548,0.707106781186547,0.707106781186548,0.707106781186547,
0.707106781186548,0.707106781186547,0.707106781186548,0.707106781186548,
0.707106781186547,0.707106781186548,0.707106781186547,0.707106781186547,
0.707106781186548,0.707106781186547,0.707106781186547,0.707106781186548,
0.707106781186548,0.707106781186548,0.707106781186547,0.707106781186548,
0.707106781186547,0.707106781186547,0.707106781186547,0.707106781186548,
0.707106781186547,0.707106781186548,0.707106781186548,0.707106781186548,
0.707106781186547,0.707106781186547,0.707106781186547,0.707106781186547,
0.707106781186548,0.707106781186547,0.707106781186547,0.707106781186548,
0.707106781186547,0.707106781186548,0.707106781186547,0.707106781186547,
0.707106781186548,0.707106781186547,0.707106781186548,0.707106781186547,
0.707106781186548,0.707106781186547,0.707106781186547,0.707106781186547,
0.707106781186547,0.707106781186547,0.707106781186547,0.707106781186548,
0.707106781186547,0.707106781186547,0.707106781186548,0.707106781186548,
0.707106781186547,0.707106781186548,0.707106781186548,0.707106781186547,
0.707106781186547,0.707106781186548,0.707106781186547,0.707106781186547,
0.707106781186548,0.707106781186547,0.707106781186548,0.707106781186548,
0.707106781186548,0.707106781186547,0.707106781186547,0.707106781186547,
0.707106781186547,0.707106781186548,0.707106781186548,0.707106781186548,
0.707106781186547,0.707106781186548,0.707106781186547,0.707106781186548,
0.707106781186548,0.707106781186547,0.707106781186548,0.707106781186547,
0.707106781186548,0.707106781186548,0.707106781186547,0.707106781186547,
0.707106781186548,0.707106781186547,0.707106781186548,0.707106781186547,
0.707106781186548,0.707106781186548,0.707106781186548,0.707106781186547,
0.707106781186548,0.707106781186547,0.707106781186547,0.707106781186547,
0.707106781186547,0.707106781186548,0.707106781186548,0.707106781186547,
0.707106781186547,0.707106781186547,0.707106781186548,0.707106781186547,
0.707106781186547,0.707106781186548,0.707106781186547,0.707106781186548,
0.707106781186548,0.707106781186548,0.707106781186547,0.707106781186547,
0.707106781186547,0.707106781186547,0.707106781186548,0.707106781186548,
0.707106781186547,0.707106781186548,0.707106781186547,0.707106781186548,
0.707106781186548,0.707106781186547,0.707106781186548,0.707106781186547,
0.707106781186548,0.707106781186547,0.707106781186547,0.707106781186547,
0.707106781186548,0.707106781186547,0.707106781186548,0.707106781186547,
0.707106781186548,0.707106781186547,0.707106781186548,0.707106781186547,
0.707106781186548,0.707106781186547,0.707106781186547,0.707106781186548,
0.707106781186547,0.707106781186548,0.707106781186547,0.707106781186547,
0.707106781186548,0.707106781186548,0.707106781186547,0.707106781186548,
0.707106781186548,0.707106781186547,0.707106781186548,0.707106781186547,
0.707106781186548,0.707106781186547,0.707106781186547,0.707106781186547,
0.707106781186548,0.707106781186547,0.707106781186547,0.707106781186548,
0.707106781186547,0.707106781186548,0.707106781186547,0.707106781186548,
0.707106781186548,0.707106781186547,0.707106781186548,0.707106781186547,
0.707106781186548,0.707106781186548,0.707106781186548,0.707106781186548,
0.707106781186547,0.707106781186547,0.707106781186548,0.707106781186547,
0.707106781186547,0.707106781186548,0.707106781186548,0.707106781186547,
0.707106781186547,0.707106781186548,0.707106781186547,0.707106781186547,
0.707106781186548,0.707106781186547,0.707106781186548,0.707106781186547,
0.707106781186548,0.707106781186547,0.707106781186547,0.707106781186547,
0.707106781186548,0.707106781186547,0.707106781186547,0.707106781186548,
0.707106781186547,0.707106781186548,0.707106781186548,0.707106781186548,
0.707106781186547,0.707106781186547,0.707106781186547,0.707106781186548,
0.707106781186548,0.707106781186547,0.707106781186547,0.707106781186547,
0.707106781186547,0.707106781186548,0.707106781186548,0.707106781186547,
0.707106781186547,0.707106781186547,0.707106781186548,0.707106781186548,
0.707106781186547,0.707106781186548,0.707106781186547,0.707106781186548,
0.707106781186547,0.707106781186548,0.707106781186548,0.707106781186547,
0.707106781186548,0.707106781186548,0.707106781186548,0.707106781186547,
0.707106781186547,0.707106781186547,0.707106781186548,0.707106781186548,
0.707106781186548,0.707106781186547,0.707106781186547,0.707106781186548,
0.707106781186548,0.707106781186547,0.707106781186548,0.707106781186547,
0.707106781186547,0.707106781186548,0.707106781186547,0.707106781186548,
0.707106781186547,0.707106781186547,0.707106781186548,0.707106781186547,
0.707106781186548,0.707106781186548,0.707106781186547,0.707106781186547,
0.707106781186548,0.707106781186547,0.707106781186548,0.707106781186547,
0.707106781186547,0.707106781186548,0.707106781186547,0.707106781186548,
0.707106781186547,0.707106781186548,0.707106781186547,0.707106781186547,
0.707106781186548,0.707106781186547,0.707106781186547,0.707106781186547,
0.707106781186547,0.707106781186547,0.707106781186547,0.707106781186548,
0.707106781186547,0.707106781186548,0.707106781186548,0.707106781186548,
0.707106781186547,0.707106781186547,0.707106781186547,0.707106781186548,
0.707106781186547,0.707106781186548,0.707106781186547,0.707106781186547,
0.707106781186548,0.707106781186547,0.707106781186547,0.707106781186547,
0.707106781186547,0.707106781186547,0.707106781186548,0.707106781186547,
0.707106781186548,0.707106781186547,0.707106781186547,0.707106781186548,
0.707106781186548,0.707106781186547,0.707106781186547,0.707106781186547,
0.707106781186548,0.707106781186547,0.707106781186547,0.707106781186548,
0.707106781186548,0.707106781186547,0.707106781186548,0.707106781186547,
0.707106781186548,0.707106781186548,0.707106781186547,0.707106781186547,
0.707106781186547,0.707106781186548,0.707106781186548,0.707106781186547,
0.707106781186548,0.707106781186547,0.707106781186548,0.707106781186548,
0.707106781186547,0.707106781186548,0.707106781186547,0.707106781186547,
0.707106781186547,0.707106781186548,0.707106781186547,0.707106781186548,
0.707106781186547,0.707106781186548,0.707106781186547,0.707106781186547,
0.707106781186547,0.707106781186547,0.707106781186547,0.707106781186548,
0.707106781186547,0.707106781186548,0.707106781186547,0.707106781186548,
0.707106781186547,0.707106781186548,0.707106781186547,0.707106781186547,
0.707106781186547,0.707106781186547,0.707106781186547,0.707106781186548,
0.707106781186548,0.707106781186548,0.707106781186547,0.707106781186548,
0.707106781186547,0.707106781186548,0.707106781186547,0.707106781186547,
0.707106781186548,0.707106781186547,0.707106781186548,0.707106781186547,
0.707106781186547,0.707106781186547,0.707106781186548,0.707106781186548,
0.707106781186547,0.707106781186548,0.707106781186547,0.707106781186548,
0.707106781186548,0.707106781186547,0.707106781186548,0.707106781186547,
0.707106781186548,0.707106781186548,0.707106781186547,0.707106781186547,
0.707106781186547,0.707106781186547,0.707106781186547,0.707106781186547,
0.707106781186548,0.707106781186548,0.707106781186547,0.707106781186548,
0.707106781186547,0.707106781186547,0.707106781186548,0.707106781186547,
0.707106781186547,0.707106781186548,0.707106781186547,0.707106781186547,
0.707106781186547,0.707106781186548,0.707106781186547,0.707106781186547,
0.707106781186548,0.707106781186547,0.707106781186548,0.707106781186548,
0.707106781186547,0.707106781186547,0.707106781186547,0.707106781186548,
0.707106781186547,0.707106781186547,0.707106781186548,0.707106781186548,
0.707106781186548,0.707106781186548,0.707106781186547,0.707106781186548,
0.707106781186548,0.707106781186547,0.707106781186547,0.707106781186548,
0.707106781186547,0.707106781186548,0.707106781186547,0.707106781186547,
0.707106781186548,0.707106781186547,0.707106781186547,0.707106781186548,
0.707106781186547,0.707106781186548,0.707106781186547,0.707106781186548,
0.707106781186547,0.707106781186548,0.707106781186547,0.707106781186548,
0.707106781186547,0.707106781186548,0.707106781186548,0.707106781186547,
0.707106781186547,0.707106781186548,0.707106781186548,0.707106781186547,
0.707106781186547,0.707106781186547,0.707106781186547,0.707106781186547,
0.707106781186548,0.707106781186547,0.707106781186547,0.707106781186548,
0.707106781186547,0.707106781186548,0.707106781186548,0.707106781186547,
0.707106781186548,0.707106781186547,0.707106781186548,0.707106781186547,
0.707106781186548,0.707106781186547,0.707106781186547,0.707106781186547,
0.707106781186547,0.707106781186547,0.707106781186547,0.707106781186548,
0.707106781186547,0.707106781186548,0.707106781186547,0.707106781186547,
0.707106781186547,0.707106781186548,0.707106781186547,0.707106781186548,
0.707106781186548,0.707106781186547,0.707106781186547,0.707106781186548,
0.707106781186547,0.707106781186548,0.707106781186547,0.707106781186548,
0.707106781186547,0.707106781186548,0.707106781186547,0.707106781186547,
0.707106781186548,0.707106781186547,0.707106781186548,0.707106781186547,
0.707106781186548,0.707106781186548,0.707106781186548,0.707106781186548,
0.707106781186547,0.707106781186548,0.707106781186548,0.707106781186548,
0.707106781186547,0.707106781186548,0.707106781186548,0.707106781186547,
0.707106781186548,0.707106781186547,0.707106781186548,0.707106781186547,
0.707106781186547,0.707106781186547,0.707106781186548,0.707106781186548,
0.707106781186547,0.707106781186548,0.707106781186547,0.707106781186548,
0.707106781186547,0.707106781186548,0.707106781186548,0.707106781186547,
0.707106781186548,0.707106781186547,0.707106781186547,0.707106781186548,
0.707106781186547,0.707106781186547,0.707106781186547,0.707106781186548,
0.707106781186547,0.707106781186548,0.707106781186548,0.707106781186547,
0.707106781186548,0.707106781186547,0.707106781186548,0.707106781186548,
0.707106781186548,0.707106781186548,0.707106781186547,0.707106781186548,
0.707106781186547,0.707106781186548,0.707106781186547,0.707106781186548,
0.707106781186547,0.707106781186547,0.707106781186547,0.707106781186547,
0.707106781186548,0.707106781186547,0.707106781186548,0.707106781186547,
0.707106781186547,0.707106781186548,0.707106781186547,0.707106781186548,
0.707106781186547,0.707106781186548,0.707106781186547,0.707106781186548,
0.707106781186548,0.707106781186548,0.707106781186548,0.707106781186547,
0.707106781186548,0.707106781186548,0.707106781186547,0.707106781186548,
0.707106781186547,0.707106781186548,0.707106781186547,0.707106781186548,
0.707106781186547,0.707106781186547,0.707106781186548,0.707106781186547,
0.707106781186548,0.707106781186547,0.707106781186547,0.707106781186548,
0.707106781186547,0.707106781186548,0.707106781186547,0.707106781186547,
0.707106781186548,0.707106781186548,0.707106781186548,0.707106781186548,
0.707106781186548,0.707106781186548,0.707106781186548,0.707106781186548,
0.707106781186548,0.707106781186547,0.707106781186548,0.707106781186547,
0.707106781186547,0.707106781186548,0.707106781186547,0.707106781186548,
0.707106781186548,0.707106781186547,0.707106781186547,0.707106781186548,
0.707106781186548,0.707106781186547,0.707106781186547,0.707106781186547,
0.707106781186547,0.707106781186547,0.707106781186548,0.707106781186547,
0.707106781186548,0.707106781186548,0.707106781186548,0.707106781186547,
0.707106781186548,0.707106781186547,0.707106781186548,0.707106781186547,
0.707106781186548,0.707106781186547,0.707106781186548,0.707106781186548,
0.707106781186547,0.707106781186547,0.707106781186548,0.707106781186548,
0.707106781186548,0.707106781186547,0.707106781186547,0.707106781186548,
0.707106781186547,0.707106781186547,0.707106781186548,0.707106781186547,
0.707106781186548,0.707106781186547,0.707106781186547,0.707106781186548,
0.707106781186548,0.707106781186548,0.707106781186547,0.707106781186547,
0.707106781186548,0.707106781186547,0.707106781186548,0.707106781186547,
0.707106781186548,0.707106781186547,0.707106781186548,0.707106781186548,
0.707106781186547,0.707106781186548,0.707106781186547,0.707106781186548,
0.707106781186547,0.707106781186547,0.707106781186547,0.707106781186548,
0.707106781186547,0.707106781186548,0.707106781186547,0.707106781186547,
0.707106781186547,0.707106781186548,0.707106781186547,0.707106781186547,
0.707106781186548,0.707106781186548,0.707106781186547,0.707106781186548,
0.707106781186547,0.707106781186548,0.707106781186548,0.707106781186547,
0.707106781186548,0.707106781186547,0.707106781186547,0.707106781186548,
0.707106781186547,0.707106781186547,0.707106781186547,0.707106781186548,
0.707106781186547,0.707106781186548,0.707106781186547,0.707106781186548,
0.707106781186548,0.707106781186548,0.707106781186547,0.707106781186548,
0.707106781186548,0.707106781186548,0.707106781186547,0.707106781186548,
0.707106781186547,0.707106781186547,0.707106781186548,0.707106781186547,
0.707106781186547,0.707106781186548,0.707106781186548,0.707106781186547,
0.707106781186548,0.707106781186547,0.707106781186548,0.707106781186548,
0.707106781186547,0.707106781186548,0.707106781186547,0.707106781186548,
0.707106781186547,0.707106781186548,0.707106781186547,0.707106781186548,
0.707106781186548,0.707106781186548,0.707106781186547,0.707106781186548,
0.707106781186548,0.707106781186547,0.707106781186547,0.707106781186548,
0.707106781186547,0.707106781186548,0.707106781186548,0.707106781186547,
0.707106781186548,0.707106781186548,0.707106781186547,0.707106781186548,
0.707106781186548,0.707106781186547,0.707106781186547,0.707106781186548,
0.707106781186547,0.707106781186548,0.707106781186547,0.707106781186548,
0.707106781186547,0.707106781186548,0.707106781186548,0.707106781186548,
0.707106781186547,0.707106781186548,0.707106781186547,0.707106781186548,
0.707106781186547,0.707106781186548,0.707106781186547,0.707106781186548,
0.707106781186547,0.707106781186548,0.707106781186547,0.707106781186548,
0.707106781186547,0.707106781186547,0.707106781186547,0.707106781186548,
0.707106781186547,0.707106781186548,0.707106781186547,0.707106781186548,
0.707106781186547,0.707106781186548,0.707106781186547,0.707106781186548,
0.707106781186548,0.707106781186548,0.707106781186547,0.707106781186548,
0.707106781186547,0.707106781186548,0.707106781186548,0.707106781186547,
0.707106781186548,0.707106781186547,0.707106781186548,0.707106781186547,
0.707106781186548,0.707106781186547,0.707106781186548,0.707106781186547,
0.707106781186547,0.707106781186547,0.707106781186548,0.707106781186547,
0.707106781186547,0.707106781186548,0.707106781186547,0.707106781186548,
0.707106781186547,0.707106781186547,0.707106781186548,0.707106781186547,
0.707106781186548,0.707106781186547,0.707106781186548,0.707106781186548,
0.707106781186548,0.707106781186547,0.707106781186547,0.707106781186548,
0.707106781186548,0.707106781186547,0.707106781186548,0.707106781186547,
0.707106781186547,0.707106781186547,0.707106781186548,0.707106781186547,
0.707106781186548,0.707106781186547,0.707106781186548,0.707106781186548,
0.707106781186548,0.707106781186547,0.707106781186547,0.707106781186547,
0.707106781186547,0.707106781186547,0.707106781186547,0.707106781186548,
0.707106781186547,0.707106781186548,0.707106781186547,0.707106781186548,
0.707106781186547,0.707106781186547,0.707106781186548,0.707106781186547,
0.707106781186547,0.707106781186548,0.707106781186548,0.707106781186547,
0.707106781186547,0.707106781186547,0.707106781186548,0.707106781186547,
0.707106781186547,0.707106781186548,0.707106781186548),(1.,1.,1.,1.,1.,
1.,1.,1.,1.,1.,1.,1.,1.,1.,1.,1.,1.,1.,1.,1.,1.,1.,1.,1.,1.,1.,1.,1.,1.,
1.,1.,1.,1.,1.,1.,1.,1.,1.,1.,1.,1.,1.,1.,1.,1.,1.,1.,1.,1.,1.,1.,1.,1.,
1.,1.,1.,1.,1.,1.,1.,1.,1.,1.,1.,1.,1.,1.,1.,1.,1.,1.,1.,1.,1.,1.,1.,1.,
1.,1.,1.,1.,1.,1.,1.,1.,1.,1.,1.,1.,1.,1.,1.,1.,1.,1.,1.,1.,1.,1.,1.,1.,
1.,1.,1.,1.,1.,1.,1.,1.,1.,1.,1.,1.,1.,1.,1.,1.,1.,1.,1.,1.,1.,1.,1.,1.,
1.,1.,1.,1.,1.,1.,1.,1.,1.,1.,1.,1.,1.,1.,1.,1.,1.,1.,1.,1.,1.,1.,1.,1.,
1.,1.,1.,1.,1.,1.,1.,1.,1.,1.,1.,1.,1.,1.,1.,1.,1.,1.,1.,1.,1.,1.,1.,1.,
1.,1.,1.,1.,1.,1.,1.,1.,1.,1.,1.,1.,1.,1.,1.,1.,1.,1.,1.,1.,1.,1.,1.,1.,
1.,1.,1.,1.,1.,1.,1.,1.,1.,1.,1.,1.,1.,1.,1.,1.,1.,1.,1.,1.,1.,1.,1.,1.,
1.,1.,1.,1.,1.,1.,1.,1.,1.,1.,1.,1.,1.,1.,1.,1.,1.,1.,1.,1.,1.,1.,1.,1.,
1.,1.,1.,1.,1.,1.,1.,1.,1.,1.,1.,1.,1.,1.,1.,1.,1.,1.,1.,1.,1.,1.,1.,1.,
1.,1.,1.,1.,1.,1.,1.,1.,1.,1.,1.,1.,1.,1.,1.,1.,1.,1.,1.,1.,1.,1.,1.,1.,
1.,1.,1.,1.,1.,1.,1.,1.,1.,1.,1.,1.,1.,1.,1.,1.,1.,1.,1.,1.,1.,1.,1.,1.,
1.,1.,1.,1.,1.,1.,1.,1.,1.,1.,1.,1.,1.,1.,1.,1.,1.,1.,1.,1.,1.,1.,1.,1.,
1.,1.,1.,1.,1.,1.,1.,1.,1.,1.,1.,1.,1.,1.,1.,1.,1.,1.,1.,1.,1.,1.,1.,1.,
1.,1.,1.,1.,1.,1.,1.,1.,1.,1.,1.,1.,1.,1.,1.,1.,1.,1.,1.,1.,1.,1.,1.,1.,
1.,1.,1.,1.,1.,1.,1.,1.,1.,1.,1.,1.,1.,1.,1.,1.,1.,1.,1.,1.,1.,1.,1.,1.,
1.,1.,1.,1.,1.,1.,1.,1.,1.,1.,1.,1.,1.,1.,1.,1.,1.,1.,1.,1.,1.,1.,1.,1.,
1.,1.,1.,1.,1.,1.,1.,1.,1.,1.,1.,1.,1.,1.,1.,1.,1.,1.,1.,1.,1.,1.,1.,1.,
1.,1.,1.,1.,1.,1.,1.,1.,1.,1.,1.,1.,1.,1.,1.,1.,1.,1.,1.,1.,1.,1.,1.,1.,
1.,1.,1.,1.,1.,1.,1.,1.,1.,1.,1.,1.,1.,1.,1.,1.,1.,1.,1.,1.,1.,1.,1.,1.,
1.,1.,1.,1.,1.,1.,1.,1.,1.,1.,1.,1.,1.,1.,1.,1.,1.,1.,1.,1.,1.,1.,1.,1.,
1.,1.,1.,1.,1.,1.,1.,1.,1.,1.,1.,1.,1.,1.,1.,1.,1.,1.,1.,1.,1.,1.,1.,1.,
1.,1.,1.,1.,1.,1.,1.,1.,1.,1.,1.,1.,1.,1.,1.,1.,1.,1.,1.,1.,1.,1.,1.,1.,
1.,1.,1.,1.,1.,1.,1.,1.,1.,1.,1.,1.,1.,1.,1.,1.,1.,1.,1.,1.,1.,1.,1.,1.,
1.,1.,1.,1.,1.,1.,1.,1.,1.,1.,1.,1.,1.,1.,1.,1.,1.,1.,1.,1.,1.,1.,1.,1.,
1.,1.,1.,1.,1.,1.,1.,1.,1.,1.,1.,1.,1.,1.,1.,1.,1.,1.,1.,1.,1.,1.,1.,1.,
1.,1.,1.,1.,1.,1.,1.,1.,1.,1.,1.,1.,1.,1.,1.,1.,1.,1.,1.,1.,1.,1.,1.,1.,
1.,1.,1.,1.,1.,1.,1.,1.,1.,1.,1.,1.,1.,1.,1.,1.,1.,1.,1.,1.,1.,1.,1.,1.,
1.,1.,1.,1.,1.,1.,1.,1.,1.,1.,1.,1.,1.,1.,1.,1.,1.,1.,1.,1.,1.,1.,1.,1.,
1.,1.,1.,1.,1.,1.,1.,1.,1.,1.,1.,1.,1.,1.,1.,1.,1.,1.,1.,1.,1.,1.,1.,1.,
1.,1.,1.,1.,1.,1.,1.,1.,1.,1.,1.,1.,1.,1.,1.,1.,1.,1.,1.,1.,1.,1.,1.,1.,
1.,1.,1.,1.,1.,1.,1.,1.,1.,1.,1.,1.,1.,1.,1.,1.,1.,1.,1.,1.,1.,1.,1.,1.,
1.,1.,1.,1.,1.,1.,1.,1.,1.,1.,1.,1.,1.,1.,1.,1.,1.,1.,1.,1.,1.,1.,1.,1.,
1.,1.,1.,1.,1.,1.,1.,1.,1.,1.,1.,1.,1.,1.,1.,1.,1.,1.,1.,1.,1.,1.,1.,1.,
1.,1.,1.,1.,1.,1.,1.,1.,1.,1.,1.,1.,1.,1.,1.,1.,1.,1.,1.,1.,1.,1.,1.,1.,
1.,1.,1.,1.,1.,1.,1.,1.,1.,1.,1.,1.,1.,1.,1.,1.,1.,1.,1.,1.,1.,1.,1.,1.,
1.,1.,1.,1.,1.,1.,1.,1.,1.,1.,1.,1.,1.,1.,1.,1.,1.,1.,1.,1.,1.,1.,1.,1.,
1.,1.,1.,1.,1.,1.,1.,1.,1.,1.,1.,1.,1.,1.,1.,1.,1.,1.,1.,1.,1.,1.,1.,1.,
1.,1.,1.,1.,1.,1.,1.,1.,1.,1.,1.,1.,1.,1.,1.,1.,1.,1.,1.,1.,1.,1.,1.,1.,
1.,1.,1.,1.,1.,1.,1.,1.,1.,1.,1.,1.,1.,1.,1.,1.,1.,1.,1.,1.,1.,1.,1.,1.,
1.,1.,1.,1.,1.,1.,1.,1.,1.,1.,1.,1.,1.,1.,1.,1.,1.,1.,1.,1.,1.,1.,1.,1.,
1.,1.,1.,1.,1.,1.,1.,1.,1.,1.,1.,1.,1.,1.,1.,1.,1.,1.,1.,1.,1.,1.,1.,1.,
1.,1.,1.,1.,1.,1.,1.,1.,1.,1.,1.,1.,1.,1.,1.,1.,1.,1.,1.,1.,1.,1.,1.,1.,
1.,1.,1.,1.,1.,1.,1.,1.,1.,1.,1.,1.,1.,1.,1.,1.,1.,1.,1.,1.,1.,1.,1.,1.,
1.,1.,1.,1.,1.,1.,1.,1.,1.,1.,1.,1.,1.,1.,1.,1.,1.,1.,1.,1.,1.,1.,1.,1.,
1.,1.,1.,1.,1.,1.,1.,1.,1.,1.,1.,1.,1.,1.,1.,1.,1.,1.,1.,1.,1.,1.,1.,1.,
1.,1.,1.,1.,1.,1.,1.,1.,1.,1.,1.,1.,1.,1.,1.,1.,1.,1.,1.,1.,1.,1.,1.,1.,
1.,1.,1.,1.,1.,1.,1.,1.,1.,1.,1.,1.,1.,1.,1.,1.,1.,1.,1.,1.,1.,1.,1.,1.,
1.,1.,1.,1.,1.,1.,1.,1.,1.,1.,1.,1.,1.,1.,1.,1.,1.,1.,1.,1.,1.,1.,1.,1.,
1.,1.,1.,1.,1.,1.,1.,1.,1.,1.,1.,1.,1.,1.,1.,1.,1.,1.,1.,1.,1.,1.,1.,1.,
1.,1.,1.,1.,1.,1.,1.,1.,1.,1.,1.,1.,1.,1.,1.,1.,1.,1.,1.,1.,1.,1.,1.,1.,
1.,1.,1.,1.,1.,1.,1.,1.,1.,1.,1.,1.,1.,1.,1.,1.,1.,1.,1.,1.,1.,1.,1.,1.,
1.,1.,1.,1.,1.,1.,1.,1.,1.,1.,1.,1.,1.,1.,1.,1.,1.,1.,1.,1.,1.,1.,1.,1.,
1.,1.,1.,1.,1.,1.,1.,1.,1.,1.,1.,1.,1.,1.,1.,1.,1.,1.,1.,1.,1.,1.,1.,1.,
1.,1.,1.,1.,1.,1.,1.,1.,1.,1.,1.,1.,1.,1.,1.,1.,1.,1.,1.,1.,1.,1.,1.,1.,
1.,1.,1.,1.,1.,1.,1.,1.,1.,1.,1.,1.,1.,1.,1.,1.,1.,1.,1.,1.,1.,1.,1.,1.,
1.,1.,1.,1.,1.,1.,1.,1.,1.,1.,1.,1.,1.,1.,1.,1.,1.,1.,1.,1.,1.,1.,1.,1.,
1.,1.,1.,1.,1.,1.,1.,1.,1.,1.,1.,1.,1.,1.,1.,1.,1.,1.,1.,1.,1.,1.,1.,1.,
1.,1.,1.,1.,1.,1.,1.,1.,1.,1.,1.,1.,1.,1.,1.,1.,1.,1.,1.,1.,1.,1.,1.,1.,
1.,1.,1.,1.,1.,1.,1.,1.,1.,1.,1.,1.,1.,1.,1.,1.,1.,1.,1.,1.,1.,1.,1.,1.,
1.,1.,1.,1.,1.,1.,1.,1.,1.,1.,1.,1.,1.,1.,1.,1.,1.,1.,1.,1.,1.,1.,1.,1.,
1.,1.,1.,1.,1.,1.,1.,1.,1.,1.,1.,1.,1.,1.,1.,1.,1.,1.,1.,1.,1.,1.,1.,1.,
1.,1.,1.,1.,1.,1.,1.,1.,1.,1.,1.,1.,1.,1.,1.,1.,1.,1.,1.,1.,1.,1.,1.,1.,
1.,1.,1.,1.,1.,1.,1.,1.,1.,1.,1.,1.,1.,1.,1.,1.,1.,1.,1.,1.,1.,1.,1.,1.,
1.,1.,1.,1.,1.,1.,1.,1.,1.,1.,1.,1.,1.,1.,1.,1.,1.,1.,1.,1.,1.,1.,1.,1.,
1.,1.,1.,1.,1.,1.,1.,1.,1.,1.,1.,1.,1.,1.,1.,1.,1.,1.,1.,1.,1.,1.,1.,1.,
1.,1.,1.,1.,1.,1.,1.,1.,1.,1.,1.,1.,1.,1.,1.,1.,1.,1.,1.,1.,1.,1.,1.,1.,
1.,1.,1.,1.,1.,1.,1.,1.,1.,1.,1.,1.,1.,1.,1.,1.,1.,1.,1.,1.,1.,1.,1.,1.,
1.,1.,1.,1.,1.,1.,1.,1.,1.,1.,1.,1.,1.,1.,1.,1.,1.,1.,1.,1.,1.,1.,1.,1.,
1.,1.,1.,1.,1.,1.,1.,1.,1.,1.,1.,1.,1.,1.,1.,1.,1.,1.,1.,1.,1.,1.,1.,1.,
1.,1.,1.,1.,1.,1.,1.,1.,1.,1.,1.,1.,1.,1.,1.,1.,1.,1.,1.,1.,1.,1.,1.,1.,
1.,1.,1.,1.,1.,1.,1.,1.,1.,1.,1.,1.,1.,1.,1.,1.,1.,1.,1.,1.,1.,1.,1.,1.,
1.,1.,1.,1.,1.,1.,1.,1.,1.,1.,1.,1.,1.,1.,1.,1.,1.,1.,1.,1.,1.,1.,1.,1.,
1.,1.,1.,1.,1.,1.,1.,1.,1.,1.,1.,1.,1.,1.,1.,1.,1.,1.,1.,1.,1.,1.,1.,1.,
1.,1.,1.,1.,1.,1.,1.,1.,1.,1.,1.,1.,1.,1.,1.,1.,1.,1.,1.,1.,1.,1.,1.,1.,
1.,1.,1.,1.,1.,1.,1.,1.,1.,1.,1.,1.,1.,1.,1.,1.,1.,1.,1.,1.,1.,1.,1.,1.,
1.,1.,1.,1.,1.,1.,1.,1.,1.,1.,1.,1.,1.,1.,1.,1.,1.,1.,1.,1.,1.,1.,1.,1.,
1.,1.,1.,1.,1.,1.,1.,1.,1.,1.,1.,1.,1.,1.,1.,1.,1.,1.,1.,1.,1.,1.,1.,1.,
1.,1.,1.,1.,1.,1.,1.,1.,1.,1.,1.,1.,1.,1.,1.,1.,1.,1.,1.,1.,1.,1.,1.,1.,
1.,1.,1.,1.,1.,1.,1.,1.,1.,1.,1.,1.,1.,1.,1.,1.,1.,1.,1.,1.,1.,1.,1.,1.,
1.,1.,1.,1.,1.,1.,1.,1.,1.,1.,1.,1.,1.,1.,1.,1.,1.,1.,1.,1.,1.,1.,1.,1.,
1.,1.,1.,1.,1.,1.,1.,1.,1.,1.,1.,1.,1.,1.,1.,1.,1.,1.,1.,1.,1.,1.,1.,1.,
1.,1.,1.,1.,1.,1.,1.,1.,1.,1.,1.,1.,1.,1.,1.,1.,1.,1.,1.,1.,1.,1.,1.,1.,
1.,1.,1.,1.,1.,1.,1.,1.,1.,1.,1.,1.,1.,1.,1.,1.,1.,1.,1.,1.,1.,1.,1.,1.,
1.,1.,1.,1.,1.,1.),(0.707106781186548,0.707106781186548,0.707106781186548,
0.707106781186547,0.707106781186547,0.707106781186548,0.707106781186547,
0.707106781186547,0.707106781186547,0.707106781186547,0.707106781186547,
0.707106781186548,0.707106781186548,0.707106781186548,0.707106781186547,
0.707106781186548,0.707106781186547,0.707106781186547,0.707106781186548,
0.707106781186547,0.707106781186548,0.707106781186547,0.707106781186548,
0.707106781186547,0.707106781186548,0.707106781186547,0.707106781186547,
0.707106781186547,0.707106781186547,0.707106781186547,0.707106781186548,
0.707106781186547,0.707106781186547,0.707106781186548,0.707106781186547,
0.707106781186547,0.707106781186548,0.707106781186547,0.707106781186547,
0.707106781186548,0.707106781186548,0.707106781186547,0.707106781186548,
0.707106781186547,0.707106781186547,0.707106781186547,0.707106781186548,
0.707106781186548,0.707106781186547,0.707106781186547,0.707106781186548,
0.707106781186547,0.707106781186548,0.707106781186547,0.707106781186547,
0.707106781186547,0.707106781186547,0.707106781186547,0.707106781186548,
0.707106781186547,0.707106781186548,0.707106781186547,0.707106781186548,
0.707106781186547,0.707106781186548,0.707106781186547,0.707106781186547,
0.707106781186548,0.707106781186547,0.707106781186547,0.707106781186548,
0.707106781186547,0.707106781186548,0.707106781186547,0.707106781186548,
0.707106781186548,0.707106781186547,0.707106781186548,0.707106781186547,
0.707106781186547,0.707106781186548,0.707106781186547,0.707106781186547,
0.707106781186547,0.707106781186548,0.707106781186547,0.707106781186547,
0.707106781186547,0.707106781186547,0.707106781186547,0.707106781186547,
0.707106781186548,0.707106781186548,0.707106781186547,0.707106781186548,
0.707106781186547,0.707106781186548,0.707106781186548,0.707106781186547,
0.707106781186548,0.707106781186548,0.707106781186548,0.707106781186547,
0.707106781186548,0.707106781186547,0.707106781186548,0.707106781186548,
0.707106781186548,0.707106781186547,0.707106781186547,0.707106781186547,
0.707106781186548,0.707106781186548,0.707106781186548,0.707106781186547,
0.707106781186547,0.707106781186547,0.707106781186548,0.707106781186548,
0.707106781186547,0.707106781186547,0.707106781186548,0.707106781186547,
0.707106781186547,0.707106781186547,0.707106781186547,0.707106781186548,
0.707106781186547,0.707106781186548,0.707106781186547,0.707106781186547,
0.707106781186547,0.707106781186548,0.707106781186548,0.707106781186547,
0.707106781186548,0.707106781186548,0.707106781186547,0.707106781186548,
0.707106781186547,0.707106781186548,0.707106781186547,0.707106781186548,
0.707106781186547,0.707106781186547,0.707106781186548,0.707106781186547,
0.707106781186547,0.707106781186548,0.707106781186547,0.707106781186547,
0.707106781186548,0.707106781186547,0.707106781186548,0.707106781186547,
0.707106781186547,0.707106781186548,0.707106781186548,0.707106781186547,
0.707106781186548,0.707106781186547,0.707106781186548,0.707106781186547,
0.707106781186548,0.707106781186547,0.707106781186548,0.707106781186547,
0.707106781186548,0.707106781186547,0.707106781186548,0.707106781186547,
0.707106781186548,0.707106781186547,0.707106781186547,0.707106781186548,
0.707106781186547,0.707106781186548,0.707106781186547,0.707106781186548,
0.707106781186547,0.707106781186548,0.707106781186547,0.707106781186547,
0.707106781186548,0.707106781186547,0.707106781186548,0.707106781186548,
0.707106781186548,0.707106781186547,0.707106781186547,0.707106781186547,
0.707106781186547,0.707106781186548,0.707106781186547,0.707106781186548,
0.707106781186548,0.707106781186547,0.707106781186547,0.707106781186548,
0.707106781186548,0.707106781186547,0.707106781186547,0.707106781186548,
0.707106781186547,0.707106781186548,0.707106781186547,0.707106781186547,
0.707106781186547,0.707106781186547,0.707106781186547,0.707106781186547,
0.707106781186547,0.707106781186548,0.707106781186547,0.707106781186548,
0.707106781186547,0.707106781186548,0.707106781186548,0.707106781186547,
0.707106781186548,0.707106781186548,0.707106781186548,0.707106781186548,
0.707106781186547,0.707106781186548,0.707106781186547,0.707106781186548,
0.707106781186547,0.707106781186547,0.707106781186548,0.707106781186548,
0.707106781186547,0.707106781186547,0.707106781186547,0.707106781186547,
0.707106781186547,0.707106781186548,0.707106781186548,0.707106781186547,
0.707106781186547,0.707106781186548,0.707106781186548,0.707106781186547,
0.707106781186548,0.707106781186547,0.707106781186548,0.707106781186548,
0.707106781186547,0.707106781186547,0.707106781186548,0.707106781186547,
0.707106781186547,0.707106781186548,0.707106781186547,0.707106781186548,
0.707106781186547,0.707106781186548,0.707106781186547,0.707106781186547,
0.707106781186548,0.707106781186548,0.707106781186547,0.707106781186547,
0.707106781186548,0.707106781186547,0.707106781186547,0.707106781186548,
0.707106781186547,0.707106781186548,0.707106781186547,0.707106781186548,
0.707106781186547,0.707106781186548,0.707106781186547,0.707106781186547,
0.707106781186547,0.707106781186547,0.707106781186547,0.707106781186547,
0.707106781186548,0.707106781186547,0.707106781186548,0.707106781186547,
0.707106781186548,0.707106781186548,0.707106781186547,0.707106781186548,
0.707106781186548,0.707106781186547,0.707106781186548,0.707106781186547,
0.707106781186547,0.707106781186547,0.707106781186548,0.707106781186547,
0.707106781186547,0.707106781186548,0.707106781186547,0.707106781186548,
0.707106781186547,0.707106781186547,0.707106781186547,0.707106781186548,
0.707106781186548,0.707106781186547,0.707106781186548,0.707106781186548,
0.707106781186547,0.707106781186548,0.707106781186547,0.707106781186548,
0.707106781186548,0.707106781186547,0.707106781186548,0.707106781186548,
0.707106781186548,0.707106781186547,0.707106781186547,0.707106781186548,
0.707106781186547,0.707106781186548,0.707106781186547,0.707106781186547,
0.707106781186548,0.707106781186548,0.707106781186548,0.707106781186547,
0.707106781186547,0.707106781186548,0.707106781186548,0.707106781186547,
0.707106781186547,0.707106781186548,0.707106781186547,0.707106781186547,
0.707106781186548,0.707106781186548,0.707106781186547,0.707106781186547,
0.707106781186547,0.707106781186548,0.707106781186547,0.707106781186547,
0.707106781186547,0.707106781186548,0.707106781186548,0.707106781186547,
0.707106781186548,0.707106781186547,0.707106781186548,0.707106781186547,
0.707106781186548,0.707106781186548,0.707106781186547,0.707106781186547,
0.707106781186548,0.707106781186547,0.707106781186547,0.707106781186548,
0.707106781186547,0.707106781186548,0.707106781186548,0.707106781186547,
0.707106781186548,0.707106781186547,0.707106781186547,0.707106781186547,
0.707106781186548,0.707106781186548,0.707106781186548,0.707106781186547,
0.707106781186548,0.707106781186547,0.707106781186548,0.707106781186547,
0.707106781186547,0.707106781186547,0.707106781186547,0.707106781186548,
0.707106781186548,0.707106781186547,0.707106781186547,0.707106781186548,
0.707106781186547,0.707106781186548,0.707106781186547,0.707106781186548,
0.707106781186547,0.707106781186547,0.707106781186548,0.707106781186547,
0.707106781186548,0.707106781186547,0.707106781186548,0.707106781186548,
0.707106781186547,0.707106781186548,0.707106781186547,0.707106781186548,
0.707106781186548,0.707106781186547,0.707106781186548,0.707106781186547,
0.707106781186547,0.707106781186548,0.707106781186547,0.707106781186548,
0.707106781186547,0.707106781186548,0.707106781186547,0.707106781186547,
0.707106781186548,0.707106781186548,0.707106781186548,0.707106781186548,
0.707106781186547,0.707106781186548,0.707106781186548,0.707106781186548,
0.707106781186547,0.707106781186548,0.707106781186548,0.707106781186548,
0.707106781186547,0.707106781186547,0.707106781186548,0.707106781186547,
0.707106781186548,0.707106781186547,0.707106781186548,0.707106781186548,
0.707106781186547,0.707106781186547,0.707106781186548,0.707106781186547,
0.707106781186548,0.707106781186547,0.707106781186548,0.707106781186548,
0.707106781186547,0.707106781186547,0.707106781186547,0.707106781186548,
0.707106781186548,0.707106781186547,0.707106781186547,0.707106781186548,
0.707106781186548,0.707106781186548,0.707106781186548,0.707106781186547,
0.707106781186547,0.707106781186548,0.707106781186548,0.707106781186547,
0.707106781186548,0.707106781186547,0.707106781186548,0.707106781186547,
0.707106781186548,0.707106781186547,0.707106781186547,0.707106781186548,
0.707106781186547,0.707106781186547,0.707106781186548,0.707106781186547,
0.707106781186548,0.707106781186547,0.707106781186548,0.707106781186547,
0.707106781186548,0.707106781186547,0.707106781186548,0.707106781186547,
0.707106781186548,0.707106781186547,0.707106781186547,0.707106781186548,
0.707106781186548,0.707106781186547,0.707106781186547,0.707106781186547,
0.707106781186548,0.707106781186547,0.707106781186548,0.707106781186547,
0.707106781186548,0.707106781186547,0.707106781186548,0.707106781186547,
0.707106781186547,0.707106781186547,0.707106781186548,0.707106781186547,
0.707106781186548,0.707106781186548,0.707106781186547,0.707106781186548,
0.707106781186547,0.707106781186547,0.707106781186548,0.707106781186547,
0.707106781186547,0.707106781186548,0.707106781186547,0.707106781186547,
0.707106781186547,0.707106781186547,0.707106781186548,0.707106781186547,
0.707106781186547,0.707106781186547,0.707106781186548,0.707106781186547,
0.707106781186547,0.707106781186548,0.707106781186548,0.707106781186547,
0.707106781186548,0.707106781186548,0.707106781186547,0.707106781186547,
0.707106781186548,0.707106781186547,0.707106781186547,0.707106781186548,
0.707106781186547,0.707106781186547,0.707106781186547,0.707106781186548,
0.707106781186547,0.707106781186548,0.707106781186547,0.707106781186548,
0.707106781186547,0.707106781186548,0.707106781186547,0.707106781186548,
0.707106781186547,0.707106781186548,0.707106781186548,0.707106781186547,
0.707106781186547,0.707106781186548,0.707106781186547,0.707106781186548,
0.707106781186547,0.707106781186548,0.707106781186548,0.707106781186547,
0.707106781186548,0.707106781186547,0.707106781186548,0.707106781186548,
0.707106781186547,0.707106781186547,0.707106781186548,0.707106781186547,
0.707106781186548,0.707106781186547,0.707106781186548,0.707106781186547,
0.707106781186548,0.707106781186547,0.707106781186547,0.707106781186547,
0.707106781186547,0.707106781186547,0.707106781186547,0.707106781186547,
0.707106781186547,0.707106781186548,0.707106781186547,0.707106781186548,
0.707106781186547,0.707106781186547,0.707106781186548,0.707106781186547,
0.707106781186548,0.707106781186547,0.707106781186547,0.707106781186548,
0.707106781186547,0.707106781186548,0.707106781186547,0.707106781186548,
0.707106781186547,0.707106781186548,0.707106781186547,0.707106781186548,
0.707106781186547,0.707106781186548,0.707106781186547,0.707106781186548,
0.707106781186548,0.707106781186547,0.707106781186548,0.707106781186547,
0.707106781186547,0.707106781186547,0.707106781186548,0.707106781186547,
0.707106781186547,0.707106781186547,0.707106781186548,0.707106781186547,
0.707106781186547,0.707106781186548,0.707106781186547,0.707106781186547,
0.707106781186547,0.707106781186547,0.707106781186548,0.707106781186547,
0.707106781186547,0.707106781186547,0.707106781186548,0.707106781186548,
0.707106781186548,0.707106781186548,0.707106781186547,0.707106781186548,
0.707106781186547,0.707106781186547,0.707106781186548,0.707106781186547,
0.707106781186548,0.707106781186547,0.707106781186547,0.707106781186548,
0.707106781186547,0.707106781186547,0.707106781186547,0.707106781186547,
0.707106781186548,0.707106781186548,0.707106781186547,0.707106781186547,
0.707106781186548,0.707106781186547,0.707106781186548,0.707106781186547,
0.707106781186548,0.707106781186548,0.707106781186547,0.707106781186547,
0.707106781186548,0.707106781186548,0.707106781186547,0.707106781186548,
0.707106781186548,0.707106781186547,0.707106781186548,0.707106781186548,
0.707106781186548,0.707106781186547,0.707106781186548,0.707106781186547,
0.707106781186548,0.707106781186547,0.707106781186548,0.707106781186547,
0.707106781186548,0.707106781186547,0.707106781186548,0.707106781186548,
0.707106781186547,0.707106781186547,0.707106781186548,0.707106781186547,
0.707106781186548,0.707106781186547,0.707106781186548,0.707106781186548,
0.707106781186548,0.707106781186548,0.707106781186548,0.707106781186547,
0.707106781186547,0.707106781186547,0.707106781186547,0.707106781186548,
0.707106781186547,0.707106781186548,0.707106781186547,0.707106781186547,
0.707106781186548,0.707106781186548,0.707106781186547,0.707106781186548,
0.707106781186547,0.707106781186548,0.707106781186548,0.707106781186547,
0.707106781186547,0.707106781186548,0.707106781186547,0.707106781186548,
0.707106781186547,0.707106781186548,0.707106781186547,0.707106781186548,
0.707106781186547,0.707106781186548,0.707106781186547,0.707106781186548,
0.707106781186547,0.707106781186548,0.707106781186548,0.707106781186547,
0.707106781186548,0.707106781186547,0.707106781186548,0.707106781186547,
0.707106781186548,0.707106781186548,0.707106781186548,0.707106781186547,
0.707106781186547,0.707106781186548,0.707106781186548,0.707106781186547,
0.707106781186547,0.707106781186547,0.707106781186548,0.707106781186547,
0.707106781186548,0.707106781186547,0.707106781186548,0.707106781186547,
0.707106781186547,0.707106781186547,0.707106781186548,0.707106781186547,
0.707106781186548,0.707106781186547,0.707106781186548,0.707106781186547,
0.707106781186548,0.707106781186547,0.707106781186547,0.707106781186548,
0.707106781186547,0.707106781186547,0.707106781186548,0.707106781186547,
0.707106781186547,0.707106781186548,0.707106781186547,0.707106781186547,
0.707106781186547,0.707106781186548,0.707106781186547,0.707106781186548,
0.707106781186547,0.707106781186547,0.707106781186547,0.707106781186548,
0.707106781186548,0.707106781186547,0.707106781186547,0.707106781186548,
0.707106781186548,0.707106781186548,0.707106781186547,0.707106781186548,
0.707106781186547,0.707106781186548,0.707106781186547,0.707106781186548,
0.707106781186547,0.707106781186547,0.707106781186547,0.707106781186547,
0.707106781186548,0.707106781186547,0.707106781186548,0.707106781186548,
0.707106781186547,0.707106781186548,0.707106781186547,0.707106781186547,
0.707106781186547,0.707106781186547,0.707106781186548,0.707106781186547,
0.707106781186548,0.707106781186547,0.707106781186548,0.707106781186548,
0.707106781186547,0.707106781186548,0.707106781186547,0.707106781186547,
0.707106781186547,0.707106781186547,0.707106781186548,0.707106781186547,
0.707106781186548,0.707106781186548,0.707106781186547,0.707106781186548,
0.707106781186547,0.707106781186548,0.707106781186547,0.707106781186547,
0.707106781186548,0.707106781186547,0.707106781186548,0.707106781186548,
0.707106781186547,0.707106781186547,0.707106781186548,0.707106781186548,
0.707106781186547,0.707106781186547,0.707106781186548,0.707106781186547,
0.707106781186547,0.707106781186548,0.707106781186547,0.707106781186547,
0.707106781186548,0.707106781186547,0.707106781186548,0.707106781186547,
0.707106781186547,0.707106781186548,0.707106781186547,0.707106781186548,
0.707106781186547,0.707106781186548,0.707106781186547,0.707106781186547,
0.707106781186547,0.707106781186548,0.707106781186547,0.707106781186548,
0.707106781186547,0.707106781186548,0.707106781186548,0.707106781186548,
0.707106781186548,0.707106781186547,0.707106781186547,0.707106781186547,
0.707106781186548,0.707106781186547,0.707106781186548,0.707106781186547,
0.707106781186547,0.707106781186548,0.707106781186547,0.707106781186547,
0.707106781186548,0.707106781186547,0.707106781186547,0.707106781186548,
0.707106781186548,0.707106781186547,0.707106781186548,0.707106781186547,
0.707106781186547,0.707106781186548,0.707106781186547,0.707106781186548,
0.707106781186547,0.707106781186548,0.707106781186547,0.707106781186547,
0.707106781186547,0.707106781186548,0.707106781186547,0.707106781186548,
0.707106781186547,0.707106781186548,0.707106781186547,0.707106781186547,
0.707106781186548,0.707106781186548,0.707106781186548,0.707106781186547,
0.707106781186548,0.707106781186547,0.707106781186548,0.707106781186547,
0.707106781186548,0.707106781186547,0.707106781186548,0.707106781186548,
0.707106781186547,0.707106781186547,0.707106781186547,0.707106781186548,
0.707106781186547,0.707106781186547,0.707106781186548,0.707106781186547,
0.707106781186547,0.707106781186548,0.707106781186547,0.707106781186548,
0.707106781186548,0.707106781186548,0.707106781186547,0.707106781186548,
0.707106781186547,0.707106781186548,0.707106781186547,0.707106781186548,
0.707106781186547,0.707106781186548,0.707106781186547,0.707106781186548,
0.707106781186547,0.707106781186548,0.707106781186548,0.707106781186547,
0.707106781186548,0.707106781186547,0.707106781186548,0.707106781186548,
0.707106781186547,0.707106781186547,0.707106781186548,0.707106781186547,
0.707106781186547,0.707106781186548,0.707106781186547,0.707106781186548,
0.707106781186548,0.707106781186547,0.707106781186548,0.707106781186548,
0.707106781186548,0.707106781186548,0.707106781186548,0.707106781186547,
0.707106781186548,0.707106781186548,0.707106781186548,0.707106781186547,
0.707106781186548,0.707106781186547,0.707106781186548,0.707106781186547,
0.707106781186548,0.707106781186547,0.707106781186548,0.707106781186547,
0.707106781186548,0.707106781186547,0.707106781186547,0.707106781186548,
0.707106781186547,0.707106781186547,0.707106781186548,0.707106781186547,
0.707106781186548,0.707106781186547,0.707106781186548,0.707106781186547,
0.707106781186548,0.707106781186547,0.707106781186547,0.707106781186548,
0.707106781186547,0.707106781186547,0.707106781186548,0.707106781186547,
0.707106781186548,0.707106781186547,0.707106781186547,0.707106781186548,
0.707106781186548,0.707106781186547,0.707106781186548,0.707106781186547,
0.707106781186547,0.707106781186547,0.707106781186548,0.707106781186547,
0.707106781186547,0.707106781186548,0.707106781186547,0.707106781186547,
0.707106781186547,0.707106781186548,0.707106781186548,0.707106781186547,
0.707106781186548,0.707106781186547,0.707106781186548,0.707106781186547,
0.707106781186547,0.707106781186548,0.707106781186547,0.707106781186548,
0.707106781186547,0.707106781186547,0.707106781186547,0.707106781186547,
0.707106781186548,0.707106781186547,0.707106781186547,0.707106781186547,
0.707106781186547,0.707106781186547,0.707106781186548,0.707106781186547,
0.707106781186547,0.707106781186547,0.707106781186547,0.707106781186548,
0.707106781186547,0.707106781186548,0.707106781186547,0.707106781186547,
0.707106781186548,0.707106781186547,0.707106781186548,0.707106781186547,
0.707106781186547,0.707106781186548,0.707106781186547,0.707106781186547,
0.707106781186548,0.707106781186547,0.707106781186547,0.707106781186547,
0.707106781186547,0.707106781186548,0.707106781186547,0.707106781186548,
0.707106781186548,0.707106781186547,0.707106781186548,0.707106781186548,
0.707106781186547,0.707106781186547,0.707106781186548,0.707106781186547,
0.707106781186547,0.707106781186547,0.707106781186548,0.707106781186547,
0.707106781186547,0.707106781186548,0.707106781186547,0.707106781186548,
0.707106781186547,0.707106781186548,0.707106781186547,0.707106781186547,
0.707106781186548,0.707106781186547,0.707106781186548,0.707106781186547,
0.707106781186548,0.707106781186547,0.707106781186548,0.707106781186547,
0.707106781186548,0.707106781186547,0.707106781186547,0.707106781186547,
0.707106781186547,0.707106781186548,0.707106781186548,0.707106781186547,
0.707106781186548,0.707106781186548,0.707106781186547,0.707106781186548,
0.707106781186547,0.707106781186547,0.707106781186548,0.707106781186547,
0.707106781186547,0.707106781186547,0.707106781186547,0.707106781186548,
0.707106781186547,0.707106781186547,0.707106781186547,0.707106781186548,
0.707106781186547,0.707106781186547,0.707106781186548,0.707106781186547,
0.707106781186548,0.707106781186548,0.707106781186547,0.707106781186548,
0.707106781186547,0.707106781186548,0.707106781186547,0.707106781186548,
0.707106781186547,0.707106781186547,0.707106781186548,0.707106781186547,
0.707106781186548,0.707106781186548,0.707106781186547,0.707106781186547,
0.707106781186548,0.707106781186547,0.707106781186548,0.707106781186547,
0.707106781186548,0.707106781186547,0.707106781186547,0.707106781186548,
0.707106781186548,0.707106781186547,0.707106781186548,0.707106781186548,
0.707106781186547,0.707106781186548,0.707106781186548,0.707106781186547,
0.707106781186548,0.707106781186547,0.707106781186548,0.707106781186547,
0.707106781186548,0.707106781186547,0.707106781186548,0.707106781186547,
0.707106781186547,0.707106781186548,0.707106781186547,0.707106781186547,
0.707106781186548,0.707106781186547,0.707106781186548,0.707106781186548,
0.707106781186547,0.707106781186547,0.707106781186547,0.707106781186548,
0.707106781186547,0.707106781186548,0.707106781186548,0.707106781186547,
0.707106781186548,0.707106781186547,0.707106781186548,0.707106781186547,
0.707106781186548,0.707106781186547,0.707106781186547,0.707106781186548,
0.707106781186548,0.707106781186548,0.707106781186547,0.707106781186548,
0.707106781186548,0.707106781186547,0.707106781186548,0.707106781186547,
0.707106781186548,0.707106781186548,0.707106781186548,0.707106781186548,
0.707106781186548,0.707106781186548,0.707106781186547,0.707106781186547,
0.707106781186548,0.707106781186547,0.707106781186547,0.707106781186548,
0.707106781186547,0.707106781186547,0.707106781186548,0.707106781186547,
0.707106781186548,0.707106781186547,0.707106781186548,0.707106781186547,
0.707106781186547,0.707106781186547,0.707106781186548,0.707106781186547,
0.707106781186547,0.707106781186548,0.707106781186547,0.707106781186548,
0.707106781186547,0.707106781186548,0.707106781186547,0.707106781186547,
0.707106781186547,0.707106781186547,0.707106781186548,0.707106781186547,
0.707106781186547,0.707106781186548,0.707106781186548,0.707106781186547,
0.707106781186548,0.707106781186547,0.707106781186548,0.707106781186547,
0.707106781186547,0.707106781186548,0.707106781186547,0.707106781186548,
0.707106781186547,0.707106781186548,0.707106781186547,0.707106781186548,
0.707106781186548,0.707106781186547,0.707106781186548,0.707106781186547,
0.707106781186547,0.707106781186548,0.707106781186547,0.707106781186547,
0.707106781186548,0.707106781186548,0.707106781186548,0.707106781186547,
0.707106781186548,0.707106781186547,0.707106781186547,0.707106781186547,
0.707106781186548,0.707106781186547,0.707106781186548,0.707106781186548,
0.707106781186548,0.707106781186547,0.707106781186547,0.707106781186547,
0.707106781186547,0.707106781186548,0.707106781186547,0.707106781186547,
0.707106781186548,0.707106781186547,0.707106781186548,0.707106781186547,
0.707106781186547,0.707106781186548,0.707106781186547,0.707106781186548,
0.707106781186547,0.707106781186548,0.707106781186547,0.707106781186547,
0.707106781186547,0.707106781186547,0.707106781186547,0.707106781186547,
0.707106781186548,0.707106781186547,0.707106781186547,0.707106781186548,
0.707106781186548,0.707106781186547,0.707106781186548,0.707106781186548,
0.707106781186547,0.707106781186547,0.707106781186548,0.707106781186547,
0.707106781186547,0.707106781186548,0.707106781186547,0.707106781186548,
0.707106781186548,0.707106781186548,0.707106781186547,0.707106781186547,
0.707106781186547,0.707106781186547,0.707106781186548,0.707106781186548,
0.707106781186548,0.707106781186547,0.707106781186548,0.707106781186547,
0.707106781186548,0.707106781186548,0.707106781186547,0.707106781186548,
0.707106781186547,0.707106781186548,0.707106781186548,0.707106781186547,
0.707106781186547,0.707106781186548,0.707106781186547,0.707106781186548,
0.707106781186547,0.707106781186548,0.707106781186548,0.707106781186548,
0.707106781186547,0.707106781186548,0.707106781186547,0.707106781186547,
0.707106781186547,0.707106781186547,0.707106781186548,0.707106781186548,
0.707106781186547,0.707106781186547,0.707106781186547,0.707106781186548,
0.707106781186547,0.707106781186547,0.707106781186548,0.707106781186547,
0.707106781186548,0.707106781186548,0.707106781186548,0.707106781186547,
0.707106781186547,0.707106781186547,0.707106781186547,0.707106781186548,
0.707106781186548,0.707106781186547,0.707106781186548,0.707106781186547,
0.707106781186548,0.707106781186548,0.707106781186547,0.707106781186548,
0.707106781186547,0.707106781186548,0.707106781186547,0.707106781186547,
0.707106781186547,0.707106781186548,0.707106781186547,0.707106781186548,
0.707106781186547,0.707106781186548,0.707106781186547,0.707106781186548,
0.707106781186547,0.707106781186548,0.707106781186547,0.707106781186547,
0.707106781186548,0.707106781186547,0.707106781186548,0.707106781186547,
0.707106781186547,0.707106781186548,0.707106781186548,0.707106781186547,
0.707106781186548,0.707106781186548,0.707106781186547,0.707106781186548,
0.707106781186547,0.707106781186548,0.707106781186547,0.707106781186547,
0.707106781186547,0.707106781186548,0.707106781186547,0.707106781186547,
0.707106781186548,0.707106781186547,0.707106781186548,0.707106781186547,
0.707106781186548,0.707106781186548,0.707106781186547,0.707106781186548,
0.707106781186547,0.707106781186548,0.707106781186548,0.707106781186548,
0.707106781186548,0.707106781186547,0.707106781186547,0.707106781186548,
0.707106781186547,0.707106781186547,0.707106781186548,0.707106781186548,
0.707106781186547,0.707106781186547,0.707106781186548,0.707106781186547,
0.707106781186547,0.707106781186548,0.707106781186547,0.707106781186548,
0.707106781186547,0.707106781186548,0.707106781186547,0.707106781186547,
0.707106781186547,0.707106781186548,0.707106781186547,0.707106781186547,
0.707106781186548,0.707106781186547,0.707106781186548,0.707106781186548,
0.707106781186548,0.707106781186547,0.707106781186547,0.707106781186547,
0.707106781186548,0.707106781186548,0.707106781186547,0.707106781186547,
0.707106781186547,0.707106781186547,0.707106781186548,0.707106781186548,
0.707106781186547,0.707106781186547,0.707106781186547,0.707106781186548,
0.707106781186548,0.707106781186547,0.707106781186548,0.707106781186547,
0.707106781186548,0.707106781186547,0.707106781186548,0.707106781186548,
0.707106781186547,0.707106781186548,0.707106781186548,0.707106781186548,
0.707106781186547,0.707106781186547,0.707106781186547,0.707106781186548,
0.707106781186548,0.707106781186548,0.707106781186547,0.707106781186547,
0.707106781186548,0.707106781186548,0.707106781186547,0.707106781186548,
0.707106781186547,0.707106781186547,0.707106781186548,0.707106781186547,
0.707106781186548,0.707106781186547,0.707106781186547,0.707106781186548,
0.707106781186547,0.707106781186548,0.707106781186548,0.707106781186547,
0.707106781186547,0.707106781186548,0.707106781186547,0.707106781186548,
0.707106781186547,0.707106781186547,0.707106781186548,0.707106781186547,
0.707106781186548,0.707106781186547,0.707106781186548,0.707106781186547,
0.707106781186547,0.707106781186548,0.707106781186547,0.707106781186547,
0.707106781186547,0.707106781186547,0.707106781186547,0.707106781186547,
0.707106781186548,0.707106781186547,0.707106781186548,0.707106781186548,
0.707106781186548,0.707106781186547,0.707106781186547,0.707106781186547,
0.707106781186548,0.707106781186547,0.707106781186548,0.707106781186547,
0.707106781186547,0.707106781186548,0.707106781186547,0.707106781186547,
0.707106781186547,0.707106781186547,0.707106781186547,0.707106781186548,
0.707106781186547,0.707106781186548,0.707106781186547,0.707106781186547,
0.707106781186548,0.707106781186548,0.707106781186547,0.707106781186547,
0.707106781186547,0.707106781186548,0.707106781186547,0.707106781186547,
0.707106781186548,0.707106781186548,0.707106781186547,0.707106781186548,
0.707106781186547,0.707106781186548,0.707106781186548,0.707106781186547,
0.707106781186547,0.707106781186547,0.707106781186548,0.707106781186548,
0.707106781186547,0.707106781186548,0.707106781186547,0.707106781186548,
0.707106781186548,0.707106781186547,0.707106781186548,0.707106781186547,
0.707106781186547,0.707106781186547,0.707106781186548,0.707106781186547,
0.707106781186548,0.707106781186547,0.707106781186548,0.707106781186547,
0.707106781186547,0.707106781186547,0.707106781186547,0.707106781186547,
0.707106781186548,0.707106781186547,0.707106781186548,0.707106781186547,
0.707106781186548,0.707106781186547,0.707106781186548,0.707106781186547,
0.707106781186547,0.707106781186547,0.707106781186547,0.707106781186547,
0.707106781186548,0.707106781186548,0.707106781186548,0.707106781186547,
0.707106781186548,0.707106781186547,0.707106781186548,0.707106781186547,
0.707106781186547,0.707106781186548,0.707106781186547,0.707106781186548,
0.707106781186547,0.707106781186547,0.707106781186547,0.707106781186548,
0.707106781186548,0.707106781186547,0.707106781186548,0.707106781186547,
0.707106781186548,0.707106781186548,0.707106781186547,0.707106781186548,
0.707106781186547,0.707106781186548,0.707106781186548,0.707106781186547,
0.707106781186547,0.707106781186547,0.707106781186547,0.707106781186547,
0.707106781186547,0.707106781186548,0.707106781186548,0.707106781186547,
0.707106781186548,0.707106781186547,0.707106781186547,0.707106781186548,
0.707106781186547,0.707106781186547,0.707106781186548,0.707106781186547,
0.707106781186547,0.707106781186547,0.707106781186548,0.707106781186547,
0.707106781186547,0.707106781186548,0.707106781186547,0.707106781186548,
0.707106781186548,0.707106781186547,0.707106781186547,0.707106781186547,
0.707106781186548,0.707106781186547,0.707106781186547,0.707106781186548,
0.707106781186548,0.707106781186548,0.707106781186548,0.707106781186547,
0.707106781186548,0.707106781186548,0.707106781186547,0.707106781186547,
0.707106781186548,0.707106781186547,0.707106781186548,0.707106781186547,
0.707106781186547,0.707106781186548,0.707106781186547,0.707106781186547,
0.707106781186548,0.707106781186547,0.707106781186548,0.707106781186547,
0.707106781186548,0.707106781186547,0.707106781186548,0.707106781186547,
0.707106781186548,0.707106781186547,0.707106781186548,0.707106781186548,
0.707106781186547,0.707106781186547,0.707106781186548,0.707106781186548,
0.707106781186547,0.707106781186547,0.707106781186547,0.707106781186547,
0.707106781186547,0.707106781186548,0.707106781186547,0.707106781186547,
0.707106781186548,0.707106781186547,0.707106781186548,0.707106781186548,
0.707106781186547,0.707106781186548,0.707106781186547,0.707106781186548,
0.707106781186547,0.707106781186548,0.707106781186547,0.707106781186547,
0.707106781186547,0.707106781186547,0.707106781186547,0.707106781186547,
0.707106781186548,0.707106781186547,0.707106781186548,0.707106781186547,
0.707106781186547,0.707106781186547,0.707106781186548,0.707106781186547,
0.707106781186548,0.707106781186548,0.707106781186547,0.707106781186547,
0.707106781186548,0.707106781186547,0.707106781186548,0.707106781186547,
0.707106781186548,0.707106781186547,0.707106781186548,0.707106781186547,
0.707106781186547,0.707106781186548,0.707106781186547,0.707106781186548,
0.707106781186547,0.707106781186548,0.707106781186548,0.707106781186548,
0.707106781186548,0.707106781186547,0.707106781186548,0.707106781186548,
0.707106781186548,0.707106781186547,0.707106781186548,0.707106781186548,
0.707106781186547,0.707106781186548,0.707106781186547,0.707106781186548,
0.707106781186547,0.707106781186547,0.707106781186547,0.707106781186548,
0.707106781186548,0.707106781186547,0.707106781186548,0.707106781186547,
0.707106781186548,0.707106781186547,0.707106781186548,0.707106781186548,
0.707106781186547,0.707106781186548,0.707106781186547,0.707106781186547,
0.707106781186548,0.707106781186547,0.707106781186547,0.707106781186547,
0.707106781186548,0.707106781186547,0.707106781186548,0.707106781186548,
0.707106781186547,0.707106781186548,0.707106781186547,0.707106781186548,
0.707106781186548,0.707106781186548,0.707106781186548,0.707106781186547,
0.707106781186548,0.707106781186547,0.707106781186548,0.707106781186547,
0.707106781186548,0.707106781186547,0.707106781186547,0.707106781186547,
0.707106781186547,0.707106781186548,0.707106781186547,0.707106781186548,
0.707106781186547,0.707106781186547,0.707106781186548,0.707106781186547,
0.707106781186548,0.707106781186547,0.707106781186548,0.707106781186547,
0.707106781186548,0.707106781186548,0.707106781186548,0.707106781186548,
0.707106781186547,0.707106781186548,0.707106781186548,0.707106781186547,
0.707106781186548,0.707106781186547,0.707106781186548,0.707106781186547,
0.707106781186548,0.707106781186547,0.707106781186547,0.707106781186548,
0.707106781186547,0.707106781186548,0.707106781186547,0.707106781186547,
0.707106781186548,0.707106781186547,0.707106781186548,0.707106781186547,
0.707106781186547,0.707106781186548,0.707106781186548,0.707106781186548,
0.707106781186548,0.707106781186548,0.707106781186548,0.707106781186548,
0.707106781186548,0.707106781186548,0.707106781186547,0.707106781186548,
0.707106781186547,0.707106781186547,0.707106781186548,0.707106781186547,
0.707106781186548,0.707106781186548,0.707106781186547,0.707106781186547,
0.707106781186548,0.707106781186548,0.707106781186547,0.707106781186547,
0.707106781186547,0.707106781186547,0.707106781186547,0.707106781186548,
0.707106781186547,0.707106781186548,0.707106781186548,0.707106781186548,
0.707106781186547,0.707106781186548,0.707106781186547,0.707106781186548,
0.707106781186547,0.707106781186548,0.707106781186547,0.707106781186548,
0.707106781186548,0.707106781186547,0.707106781186547,0.707106781186548,
0.707106781186548,0.707106781186548,0.707106781186547,0.707106781186547,
0.707106781186548,0.707106781186547,0.707106781186547,0.707106781186548,
0.707106781186547,0.707106781186548,0.707106781186547,0.707106781186547,
0.707106781186548,0.707106781186548,0.707106781186548,0.707106781186547,
0.707106781186547,0.707106781186548,0.707106781186547,0.707106781186548,
0.707106781186547,0.707106781186548,0.707106781186547,0.707106781186548,
0.707106781186548,0.707106781186547,0.707106781186548,0.707106781186547,
0.707106781186548,0.707106781186547,0.707106781186547,0.707106781186547,
0.707106781186548,0.707106781186547,0.707106781186548,0.707106781186547,
0.707106781186547,0.707106781186547,0.707106781186548,0.707106781186547,
0.707106781186547,0.707106781186548,0.707106781186548,0.707106781186547,
0.707106781186548,0.707106781186547,0.707106781186548,0.707106781186548,
0.707106781186547,0.707106781186548,0.707106781186547,0.707106781186547,
0.707106781186548,0.707106781186547,0.707106781186547,0.707106781186547,
0.707106781186548,0.707106781186547,0.707106781186548,0.707106781186547,
0.707106781186548,0.707106781186548,0.707106781186548,0.707106781186547,
0.707106781186548,0.707106781186548,0.707106781186548,0.707106781186547,
0.707106781186548,0.707106781186547,0.707106781186547,0.707106781186548,
0.707106781186547,0.707106781186547,0.707106781186548,0.707106781186548,
0.707106781186547,0.707106781186548,0.707106781186547,0.707106781186548,
0.707106781186548,0.707106781186547,0.707106781186548,0.707106781186547,
0.707106781186548,0.707106781186547,0.707106781186548,0.707106781186547,
0.707106781186548,0.707106781186548,0.707106781186548,0.707106781186547,
0.707106781186548,0.707106781186548,0.707106781186547,0.707106781186547,
0.707106781186548,0.707106781186547,0.707106781186548,0.707106781186548,
0.707106781186547,0.707106781186548,0.707106781186548,0.707106781186547,
0.707106781186548,0.707106781186548,0.707106781186547,0.707106781186547,
0.707106781186548,0.707106781186547,0.707106781186548,0.707106781186547,
0.707106781186548,0.707106781186547,0.707106781186548,0.707106781186548,
0.707106781186548,0.707106781186547,0.707106781186548,0.707106781186547,
0.707106781186548,0.707106781186547,0.707106781186548,0.707106781186547,
0.707106781186548,0.707106781186547,0.707106781186548,0.707106781186547,
0.707106781186548,0.707106781186547,0.707106781186547,0.707106781186547,
0.707106781186548,0.707106781186547,0.707106781186548,0.707106781186547,
0.707106781186548,0.707106781186547,0.707106781186548,0.707106781186547,
0.707106781186548,0.707106781186548,0.707106781186548,0.707106781186547,
0.707106781186548,0.707106781186547,0.707106781186548,0.707106781186548,
0.707106781186547,0.707106781186548,0.707106781186547,0.707106781186548,
0.707106781186547,0.707106781186548,0.707106781186547,0.707106781186548,
0.707106781186547,0.707106781186547,0.707106781186547,0.707106781186548,
0.707106781186547,0.707106781186547,0.707106781186548,0.707106781186547,
0.707106781186548,0.707106781186547,0.707106781186547,0.707106781186548,
0.707106781186547,0.707106781186548,0.707106781186547,0.707106781186548,
0.707106781186548,0.707106781186548,0.707106781186547,0.707106781186547,
0.707106781186548,0.707106781186548,0.707106781186547,0.707106781186548,
0.707106781186547,0.707106781186547,0.707106781186547,0.707106781186548,
0.707106781186547,0.707106781186548,0.707106781186547,0.707106781186548,
0.707106781186548,0.707106781186548,0.707106781186547,0.707106781186547,
0.707106781186547,0.707106781186547,0.707106781186547,0.707106781186547,
0.707106781186548,0.707106781186547,0.707106781186548,0.707106781186547,
0.707106781186548,0.707106781186547,0.707106781186547,0.707106781186548,
0.707106781186547,0.707106781186547,0.707106781186548,0.707106781186548,
0.707106781186547,0.707106781186547,0.707106781186547,0.707106781186548,
0.707106781186547,0.707106781186547,0.707106781186548,0.707106781186548),
(1.,1.,1.,1.,1.,1.,1.,1.,1.,1.,1.,1.,1.,1.,1.,1.,1.,1.,1.,1.,1.,1.,1.,1.,
1.,1.,1.,1.,1.,1.,1.,1.,1.,1.,1.,1.,1.,1.,1.,1.,1.,1.,1.,1.,1.,1.,1.,1.,
1.,1.,1.,1.,1.,1.,1.,1.,1.,1.,1.,1.,1.,1.,1.,1.,1.,1.,1.,1.,1.,1.,1.,1.,
1.,1.,1.,1.,1.,1.,1.,1.,1.,1.,1.,1.,1.,1.,1.,1.,1.,1.,1.,1.,1.,1.,1.,1.,
1.,1.,1.,1.,1.,1.,1.,1.,1.,1.,1.,1.,1.,1.,1.,1.,1.,1.,1.,1.,1.,1.,1.,1.,
1.,1.,1.,1.,1.,1.,1.,1.,1.,1.,1.,1.,1.,1.,1.,1.,1.,1.,1.,1.,1.,1.,1.,1.,
1.,1.,1.,1.,1.,1.,1.,1.,1.,1.,1.,1.,1.,1.,1.,1.,1.,1.,1.,1.,1.,1.,1.,1.,
1.,1.,1.,1.,1.,1.,1.,1.,1.,1.,1.,1.,1.,1.,1.,1.,1.,1.,1.,1.,1.,1.,1.,1.,
1.,1.,1.,1.,1.,1.,1.,1.,1.,1.,1.,1.,1.,1.,1.,1.,1.,1.,1.,1.,1.,1.,1.,1.,
1.,1.,1.,1.,1.,1.,1.,1.,1.,1.,1.,1.,1.,1.,1.,1.,1.,1.,1.,1.,1.,1.,1.,1.,
1.,1.,1.,1.,1.,1.,1.,1.,1.,1.,1.,1.,1.,1.,1.,1.,1.,1.,1.,1.,1.,1.,1.,1.,
1.,1.,1.,1.,1.,1.,1.,1.,1.,1.,1.,1.,1.,1.,1.,1.,1.,1.,1.,1.,1.,1.,1.,1.,
1.,1.,1.,1.,1.,1.,1.,1.,1.,1.,1.,1.,1.,1.,1.,1.,1.,1.,1.,1.,1.,1.,1.,1.,
1.,1.,1.,1.,1.,1.,1.,1.,1.,1.,1.,1.,1.,1.,1.,1.,1.,1.,1.,1.,1.,1.,1.,1.,
1.,1.,1.,1.,1.,1.,1.,1.,1.,1.,1.,1.,1.,1.,1.,1.,1.,1.,1.,1.,1.,1.,1.,1.,
1.,1.,1.,1.,1.,1.,1.,1.,1.,1.,1.,1.,1.,1.,1.,1.,1.,1.,1.,1.,1.,1.,1.,1.,
1.,1.,1.,1.,1.,1.,1.,1.,1.,1.,1.,1.,1.,1.,1.,1.,1.,1.,1.,1.,1.,1.,1.,1.,
1.,1.,1.,1.,1.,1.,1.,1.,1.,1.,1.,1.,1.,1.,1.,1.,1.,1.,1.,1.,1.,1.,1.,1.,
1.,1.,1.,1.,1.,1.,1.,1.,1.,1.,1.,1.,1.,1.,1.,1.,1.,1.,1.,1.,1.,1.,1.,1.,
1.,1.,1.,1.,1.,1.,1.,1.,1.,1.,1.,1.,1.,1.,1.,1.,1.,1.,1.,1.,1.,1.,1.,1.,
1.,1.,1.,1.,1.,1.,1.,1.,1.,1.,1.,1.,1.,1.,1.,1.,1.,1.,1.,1.,1.,1.,1.,1.,
1.,1.,1.,1.,1.,1.,1.,1.,1.,1.,1.,1.,1.,1.,1.,1.,1.,1.,1.,1.,1.,1.,1.,1.,
1.,1.,1.,1.,1.,1.,1.,1.,1.,1.,1.,1.,1.,1.,1.,1.,1.,1.,1.,1.,1.,1.,1.,1.,
1.,1.,1.,1.,1.,1.,1.,1.,1.,1.,1.,1.,1.,1.,1.,1.,1.,1.,1.,1.,1.,1.,1.,1.,
1.,1.,1.,1.,1.,1.,1.,1.,1.,1.,1.,1.,1.,1.,1.,1.,1.,1.,1.,1.,1.,1.,1.,1.,
1.,1.,1.,1.,1.,1.,1.,1.,1.,1.,1.,1.,1.,1.,1.,1.,1.,1.,1.,1.,1.,1.,1.,1.,
1.,1.,1.,1.,1.,1.,1.,1.,1.,1.,1.,1.,1.,1.,1.,1.,1.,1.,1.,1.,1.,1.,1.,1.,
1.,1.,1.,1.,1.,1.,1.,1.,1.,1.,1.,1.,1.,1.,1.,1.,1.,1.,1.,1.,1.,1.,1.,1.,
1.,1.,1.,1.,1.,1.,1.,1.,1.,1.,1.,1.,1.,1.,1.,1.,1.,1.,1.,1.,1.,1.,1.,1.,
1.,1.,1.,1.,1.,1.,1.,1.,1.,1.,1.,1.,1.,1.,1.,1.,1.,1.,1.,1.,1.,1.,1.,1.,
1.,1.,1.,1.,1.,1.,1.,1.,1.,1.,1.,1.,1.,1.,1.,1.,1.,1.,1.,1.,1.,1.,1.,1.,
1.,1.,1.,1.,1.,1.,1.,1.,1.,1.,1.,1.,1.,1.,1.,1.,1.,1.,1.,1.,1.,1.,1.,1.,
1.,1.,1.,1.,1.,1.,1.,1.,1.,1.,1.,1.,1.,1.,1.,1.,1.,1.,1.,1.,1.,1.,1.,1.,
1.,1.,1.,1.,1.,1.,1.,1.,1.,1.,1.,1.,1.,1.,1.,1.,1.,1.,1.,1.,1.,1.,1.,1.,
1.,1.,1.,1.,1.,1.,1.,1.,1.,1.,1.,1.,1.,1.,1.,1.,1.,1.,1.,1.,1.,1.,1.,1.,
1.,1.,1.,1.,1.,1.,1.,1.,1.,1.,1.,1.,1.,1.,1.,1.,1.,1.,1.,1.,1.,1.,1.,1.,
1.,1.,1.,1.,1.,1.,1.,1.,1.,1.,1.,1.,1.,1.,1.,1.,1.,1.,1.,1.,1.,1.,1.,1.,
1.,1.,1.,1.,1.,1.,1.,1.,1.,1.,1.,1.,1.,1.,1.,1.,1.,1.,1.,1.,1.,1.,1.,1.,
1.,1.,1.,1.,1.,1.,1.,1.,1.,1.,1.,1.,1.,1.,1.,1.,1.,1.,1.,1.,1.,1.,1.,1.,
1.,1.,1.,1.,1.,1.,1.,1.,1.,1.,1.,1.,1.,1.,1.,1.,1.,1.,1.,1.,1.,1.,1.,1.,
1.,1.,1.,1.,1.,1.,1.,1.,1.,1.,1.,1.,1.,1.,1.,1.,1.,1.,1.,1.,1.,1.,1.,1.,
1.,1.,1.,1.,1.,1.,1.,1.,1.,1.,1.,1.,1.,1.,1.,1.,1.,1.,1.,1.,1.,1.,1.,1.,
1.,1.,1.,1.,1.,1.,1.,1.,1.,1.,1.,1.,1.,1.,1.,1.,1.,1.,1.,1.,1.,1.,1.,1.,
1.,1.,1.,1.,1.,1.,1.,1.,1.,1.,1.,1.,1.,1.,1.,1.,1.,1.,1.,1.,1.,1.,1.,1.,
1.,1.,1.,1.,1.,1.,1.,1.,1.,1.,1.,1.,1.,1.,1.,1.,1.,1.,1.,1.,1.,1.,1.,1.,
1.,1.,1.,1.,1.,1.,1.,1.,1.,1.,1.,1.,1.,1.,1.,1.,1.,1.,1.,1.,1.,1.,1.,1.,
1.,1.,1.,1.,1.,1.,1.,1.,1.,1.,1.,1.,1.,1.,1.,1.,1.,1.,1.,1.,1.,1.,1.,1.,
1.,1.,1.,1.,1.,1.,1.,1.,1.,1.,1.,1.,1.,1.,1.,1.,1.,1.,1.,1.,1.,1.,1.,1.,
1.,1.,1.,1.,1.,1.,1.,1.,1.,1.,1.,1.,1.,1.,1.,1.,1.,1.,1.,1.,1.,1.,1.,1.,
1.,1.,1.,1.,1.,1.,1.,1.,1.,1.,1.,1.,1.,1.,1.,1.,1.,1.,1.,1.,1.,1.,1.,1.,
1.,1.,1.,1.,1.,1.,1.,1.,1.,1.,1.,1.,1.,1.,1.,1.,1.,1.,1.,1.,1.,1.,1.,1.,
1.,1.,1.,1.,1.,1.,1.,1.,1.,1.,1.,1.,1.,1.,1.,1.,1.,1.,1.,1.,1.,1.,1.,1.,
1.,1.,1.,1.,1.,1.,1.,1.,1.,1.,1.,1.,1.,1.,1.,1.,1.,1.,1.,1.,1.,1.,1.,1.,
1.,1.,1.,1.,1.,1.,1.,1.,1.,1.,1.,1.,1.,1.,1.,1.,1.,1.,1.,1.,1.,1.,1.,1.,
1.,1.,1.,1.,1.,1.,1.,1.,1.,1.,1.,1.,1.,1.,1.,1.,1.,1.,1.,1.,1.,1.,1.,1.,
1.,1.,1.,1.,1.,1.,1.,1.,1.,1.,1.,1.,1.,1.,1.,1.,1.,1.,1.,1.,1.,1.,1.,1.,
1.,1.,1.,1.,1.,1.,1.,1.,1.,1.,1.,1.,1.,1.,1.,1.,1.,1.,1.,1.,1.,1.,1.,1.,
1.,1.,1.,1.,1.,1.,1.,1.,1.,1.,1.,1.,1.,1.,1.,1.,1.,1.,1.,1.,1.,1.,1.,1.,
1.,1.,1.,1.,1.,1.,1.,1.,1.,1.,1.,1.,1.,1.,1.,1.,1.,1.,1.,1.,1.,1.,1.,1.,
1.,1.,1.,1.,1.,1.,1.,1.,1.,1.,1.,1.,1.,1.,1.,1.,1.,1.,1.,1.,1.,1.,1.,1.,
1.,1.,1.,1.,1.,1.,1.,1.,1.,1.,1.,1.,1.,1.,1.,1.,1.,1.,1.,1.,1.,1.,1.,1.,
1.,1.,1.,1.,1.,1.,1.,1.,1.,1.,1.,1.,1.,1.,1.,1.,1.,1.,1.,1.,1.,1.,1.,1.,
1.,1.,1.,1.,1.,1.,1.,1.,1.,1.,1.,1.,1.,1.,1.,1.,1.,1.,1.,1.,1.,1.,1.,1.,
1.,1.,1.,1.,1.,1.,1.,1.,1.,1.,1.,1.,1.,1.,1.,1.,1.,1.,1.,1.,1.,1.,1.,1.,
1.,1.,1.,1.,1.,1.,1.,1.,1.,1.,1.,1.,1.,1.,1.,1.,1.,1.,1.,1.,1.,1.,1.,1.,
1.,1.,1.,1.,1.,1.,1.,1.,1.,1.,1.,1.,1.,1.,1.,1.,1.,1.,1.,1.,1.,1.,1.,1.,
1.,1.,1.,1.,1.,1.,1.,1.,1.,1.,1.,1.,1.,1.,1.,1.,1.,1.,1.,1.,1.,1.,1.,1.,
1.,1.,1.,1.,1.,1.,1.,1.,1.,1.,1.,1.,1.,1.,1.,1.,1.,1.,1.,1.,1.,1.,1.,1.,
1.,1.,1.,1.,1.,1.,1.,1.,1.,1.,1.,1.,1.,1.,1.,1.,1.,1.,1.,1.,1.,1.,1.,1.,
1.,1.,1.,1.,1.,1.,1.,1.,1.,1.,1.,1.,1.,1.,1.,1.,1.,1.,1.,1.,1.,1.,1.,1.,
1.,1.,1.,1.,1.,1.,1.,1.,1.,1.,1.,1.,1.,1.,1.,1.,1.,1.,1.,1.,1.,1.,1.,1.,
1.,1.,1.,1.,1.,1.,1.,1.,1.,1.,1.,1.,1.,1.,1.,1.,1.,1.,1.,1.,1.,1.,1.,1.,
1.,1.,1.,1.,1.,1.,1.,1.,1.,1.,1.,1.,1.,1.,1.,1.,1.,1.,1.,1.,1.,1.,1.,1.,
1.,1.,1.,1.,1.,1.,1.,1.,1.,1.,1.,1.,1.,1.,1.,1.,1.,1.,1.,1.,1.,1.,1.,1.,
1.,1.,1.,1.,1.,1.,1.,1.,1.,1.,1.,1.,1.,1.,1.,1.,1.,1.,1.,1.,1.,1.,1.,1.,
1.,1.,1.,1.,1.,1.,1.,1.,1.,1.,1.,1.,1.,1.,1.,1.,1.,1.,1.,1.,1.,1.,1.,1.,
1.,1.,1.,1.,1.,1.,1.,1.,1.,1.,1.,1.,1.,1.,1.,1.,1.,1.,1.,1.,1.,1.,1.,1.,
1.,1.,1.,1.,1.,1.,1.,1.,1.,1.,1.,1.,1.,1.,1.,1.,1.,1.,1.,1.,1.,1.,1.,1.,
1.,1.,1.,1.,1.,1.,1.,1.,1.,1.,1.,1.,1.,1.,1.,1.,1.,1.,1.,1.,1.,1.,1.,1.,
1.,1.,1.,1.,1.,1.,1.,1.,1.,1.,1.,1.,1.,1.,1.,1.,1.,1.,1.,1.,1.,1.,1.,1.,
1.,1.,1.,1.,1.,1.,1.,1.,1.,1.,1.,1.,1.,1.,1.,1.,1.,1.,1.,1.,1.,1.,1.,1.,
1.,1.,1.,1.,1.,1.,1.,1.,1.,1.,1.,1.,1.,1.,1.,1.,1.,1.,1.,1.,1.,1.,1.,1.,
1.,1.,1.,1.,1.,1.,1.,1.,1.,1.,1.,1.,1.,1.,1.,1.,1.,1.,1.,1.,1.,1.,1.,1.,
1.,1.,1.,1.,1.,1.,1.,1.,1.,1.,1.,1.,1.,1.,1.,1.,1.,1.,1.,1.,1.,1.,1.,1.,
1.,1.,1.,1.,1.,1.,1.,1.,1.,1.,1.,1.,1.,1.,1.,1.,1.,1.,1.,1.,1.,1.,1.,1.,
1.,1.,1.,1.,1.,1.,1.,1.,1.,1.,1.),(0.707106781186548,0.707106781186548,
0.707106781186548,0.707106781186547,0.707106781186547,0.707106781186548,
0.707106781186547,0.707106781186547,0.707106781186547,0.707106781186547,
0.707106781186547,0.707106781186548,0.707106781186548,0.707106781186548,
0.707106781186547,0.707106781186548,0.707106781186547,0.707106781186547,
0.707106781186548,0.707106781186547,0.707106781186548,0.707106781186547,
0.707106781186548,0.707106781186547,0.707106781186548,0.707106781186547,
0.707106781186547,0.707106781186547,0.707106781186547,0.707106781186547,
0.707106781186548,0.707106781186547,0.707106781186547,0.707106781186548,
0.707106781186547,0.707106781186547,0.707106781186548,0.707106781186547,
0.707106781186547,0.707106781186548,0.707106781186548,0.707106781186547,
0.707106781186548,0.707106781186547,0.707106781186547,0.707106781186547,
0.707106781186548,0.707106781186548,0.707106781186547,0.707106781186547,
0.707106781186548,0.707106781186547,0.707106781186548,0.707106781186547,
0.707106781186547,0.707106781186547,0.707106781186547,0.707106781186547,
0.707106781186548,0.707106781186547,0.707106781186548,0.707106781186547,
0.707106781186548,0.707106781186547,0.707106781186548,0.707106781186547,
0.707106781186547,0.707106781186548,0.707106781186547,0.707106781186547,
0.707106781186548,0.707106781186547,0.707106781186548,0.707106781186547,
0.707106781186548,0.707106781186548,0.707106781186547,0.707106781186548,
0.707106781186547,0.707106781186547,0.707106781186548,0.707106781186547,
0.707106781186547,0.707106781186547,0.707106781186548,0.707106781186547,
0.707106781186547,0.707106781186547,0.707106781186547,0.707106781186547,
0.707106781186547,0.707106781186548,0.707106781186548,0.707106781186547,
0.707106781186548,0.707106781186547,0.707106781186548,0.707106781186548,
0.707106781186547,0.707106781186548,0.707106781186548,0.707106781186548,
0.707106781186547,0.707106781186548,0.707106781186547,0.707106781186548,
0.707106781186548,0.707106781186548,0.707106781186547,0.707106781186547,
0.707106781186547,0.707106781186548,0.707106781186548,0.707106781186548,
0.707106781186547,0.707106781186547,0.707106781186547,0.707106781186548,
0.707106781186548,0.707106781186547,0.707106781186547,0.707106781186548,
0.707106781186547,0.707106781186547,0.707106781186547,0.707106781186547,
0.707106781186548,0.707106781186547,0.707106781186548,0.707106781186547,
0.707106781186547,0.707106781186547,0.707106781186548,0.707106781186548,
0.707106781186547,0.707106781186548,0.707106781186548,0.707106781186547,
0.707106781186548,0.707106781186547,0.707106781186548,0.707106781186547,
0.707106781186548,0.707106781186547,0.707106781186547,0.707106781186548,
0.707106781186547,0.707106781186547,0.707106781186548,0.707106781186547,
0.707106781186547,0.707106781186548,0.707106781186547,0.707106781186548,
0.707106781186547,0.707106781186547,0.707106781186548,0.707106781186548,
0.707106781186547,0.707106781186548,0.707106781186547,0.707106781186548,
0.707106781186547,0.707106781186548,0.707106781186547,0.707106781186548,
0.707106781186547,0.707106781186548,0.707106781186547,0.707106781186548,
0.707106781186547,0.707106781186548,0.707106781186547,0.707106781186547,
0.707106781186548,0.707106781186547,0.707106781186548,0.707106781186547,
0.707106781186548,0.707106781186547,0.707106781186548,0.707106781186547,
0.707106781186547,0.707106781186548,0.707106781186547,0.707106781186548,
0.707106781186548,0.707106781186548,0.707106781186547,0.707106781186547,
0.707106781186547,0.707106781186547,0.707106781186548,0.707106781186547,
0.707106781186548,0.707106781186548,0.707106781186547,0.707106781186547,
0.707106781186548,0.707106781186548,0.707106781186547,0.707106781186547,
0.707106781186548,0.707106781186547,0.707106781186548,0.707106781186547,
0.707106781186547,0.707106781186547,0.707106781186547,0.707106781186547,
0.707106781186547,0.707106781186547,0.707106781186548,0.707106781186547,
0.707106781186548,0.707106781186547,0.707106781186548,0.707106781186548,
0.707106781186547,0.707106781186548,0.707106781186548,0.707106781186548,
0.707106781186548,0.707106781186547,0.707106781186548,0.707106781186547,
0.707106781186548,0.707106781186547,0.707106781186547,0.707106781186548,
0.707106781186548,0.707106781186547,0.707106781186547,0.707106781186547,
0.707106781186547,0.707106781186547,0.707106781186548,0.707106781186548,
0.707106781186547,0.707106781186547,0.707106781186548,0.707106781186548,
0.707106781186547,0.707106781186548,0.707106781186547,0.707106781186548,
0.707106781186548,0.707106781186547,0.707106781186547,0.707106781186548,
0.707106781186547,0.707106781186547,0.707106781186548,0.707106781186547,
0.707106781186548,0.707106781186547,0.707106781186548,0.707106781186547,
0.707106781186547,0.707106781186548,0.707106781186548,0.707106781186547,
0.707106781186547,0.707106781186548,0.707106781186547,0.707106781186547,
0.707106781186548,0.707106781186547,0.707106781186548,0.707106781186547,
0.707106781186548,0.707106781186547,0.707106781186548,0.707106781186547,
0.707106781186547,0.707106781186547,0.707106781186547,0.707106781186547,
0.707106781186547,0.707106781186548,0.707106781186547,0.707106781186548,
0.707106781186547,0.707106781186548,0.707106781186548,0.707106781186547,
0.707106781186548,0.707106781186548,0.707106781186547,0.707106781186548,
0.707106781186547,0.707106781186547,0.707106781186547,0.707106781186548,
0.707106781186547,0.707106781186547,0.707106781186548,0.707106781186547,
0.707106781186548,0.707106781186547,0.707106781186547,0.707106781186547,
0.707106781186548,0.707106781186548,0.707106781186547,0.707106781186548,
0.707106781186548,0.707106781186547,0.707106781186548,0.707106781186547,
0.707106781186548,0.707106781186548,0.707106781186547,0.707106781186548,
0.707106781186548,0.707106781186548,0.707106781186547,0.707106781186547,
0.707106781186548,0.707106781186547,0.707106781186548,0.707106781186547,
0.707106781186547,0.707106781186548,0.707106781186548,0.707106781186548,
0.707106781186547,0.707106781186547,0.707106781186548,0.707106781186548,
0.707106781186547,0.707106781186547,0.707106781186548,0.707106781186547,
0.707106781186547,0.707106781186548,0.707106781186548,0.707106781186547,
0.707106781186547,0.707106781186547,0.707106781186548,0.707106781186547,
0.707106781186547,0.707106781186547,0.707106781186548,0.707106781186548,
0.707106781186547,0.707106781186548,0.707106781186547,0.707106781186548,
0.707106781186547,0.707106781186548,0.707106781186548,0.707106781186547,
0.707106781186547,0.707106781186548,0.707106781186547,0.707106781186547,
0.707106781186548,0.707106781186547,0.707106781186548,0.707106781186548,
0.707106781186547,0.707106781186548,0.707106781186547,0.707106781186547,
0.707106781186547,0.707106781186548,0.707106781186548,0.707106781186548,
0.707106781186547,0.707106781186548,0.707106781186547,0.707106781186548,
0.707106781186547,0.707106781186547,0.707106781186547,0.707106781186547,
0.707106781186548,0.707106781186548,0.707106781186547,0.707106781186547,
0.707106781186548,0.707106781186547,0.707106781186548,0.707106781186547,
0.707106781186548,0.707106781186547,0.707106781186547,0.707106781186548,
0.707106781186547,0.707106781186548,0.707106781186547,0.707106781186548,
0.707106781186548,0.707106781186547,0.707106781186548,0.707106781186547,
0.707106781186548,0.707106781186548,0.707106781186547,0.707106781186548,
0.707106781186547,0.707106781186547,0.707106781186548,0.707106781186547,
0.707106781186548,0.707106781186547,0.707106781186548,0.707106781186547,
0.707106781186547,0.707106781186548,0.707106781186548,0.707106781186548,
0.707106781186548,0.707106781186547,0.707106781186548,0.707106781186548,
0.707106781186548,0.707106781186547,0.707106781186548,0.707106781186548,
0.707106781186548,0.707106781186547,0.707106781186547,0.707106781186548,
0.707106781186547,0.707106781186548,0.707106781186547,0.707106781186548,
0.707106781186548,0.707106781186547,0.707106781186547,0.707106781186548,
0.707106781186547,0.707106781186548,0.707106781186547,0.707106781186548,
0.707106781186548,0.707106781186547,0.707106781186547,0.707106781186547,
0.707106781186548,0.707106781186548,0.707106781186547,0.707106781186547,
0.707106781186548,0.707106781186548,0.707106781186548,0.707106781186548,
0.707106781186547,0.707106781186547,0.707106781186548,0.707106781186548,
0.707106781186547,0.707106781186548,0.707106781186547,0.707106781186548,
0.707106781186547,0.707106781186548,0.707106781186547,0.707106781186547,
0.707106781186548,0.707106781186547,0.707106781186547,0.707106781186548,
0.707106781186547,0.707106781186548,0.707106781186547,0.707106781186548,
0.707106781186547,0.707106781186548,0.707106781186547,0.707106781186548,
0.707106781186547,0.707106781186548,0.707106781186547,0.707106781186547,
0.707106781186548,0.707106781186548,0.707106781186547,0.707106781186547,
0.707106781186547,0.707106781186548,0.707106781186547,0.707106781186548,
0.707106781186547,0.707106781186548,0.707106781186547,0.707106781186548,
0.707106781186547,0.707106781186547,0.707106781186547,0.707106781186548,
0.707106781186547,0.707106781186548,0.707106781186548,0.707106781186547,
0.707106781186548,0.707106781186547,0.707106781186547,0.707106781186548,
0.707106781186547,0.707106781186547,0.707106781186548,0.707106781186547,
0.707106781186547,0.707106781186547,0.707106781186547,0.707106781186548,
0.707106781186547,0.707106781186547,0.707106781186547,0.707106781186548,
0.707106781186547,0.707106781186547,0.707106781186548,0.707106781186548,
0.707106781186547,0.707106781186548,0.707106781186548,0.707106781186547,
0.707106781186547,0.707106781186548,0.707106781186547,0.707106781186547,
0.707106781186548,0.707106781186547,0.707106781186547,0.707106781186547,
0.707106781186548,0.707106781186547,0.707106781186548,0.707106781186547,
0.707106781186548,0.707106781186547,0.707106781186548,0.707106781186547,
0.707106781186548,0.707106781186547,0.707106781186548,0.707106781186548,
0.707106781186547,0.707106781186547,0.707106781186548,0.707106781186547,
0.707106781186548,0.707106781186547,0.707106781186548,0.707106781186548,
0.707106781186547,0.707106781186548,0.707106781186547,0.707106781186548,
0.707106781186548,0.707106781186547,0.707106781186547,0.707106781186548,
0.707106781186547,0.707106781186548,0.707106781186547,0.707106781186548,
0.707106781186547,0.707106781186548,0.707106781186547,0.707106781186547,
0.707106781186547,0.707106781186547,0.707106781186547,0.707106781186547,
0.707106781186547,0.707106781186547,0.707106781186548,0.707106781186547,
0.707106781186548,0.707106781186547,0.707106781186547,0.707106781186548,
0.707106781186547,0.707106781186548,0.707106781186547,0.707106781186547,
0.707106781186548,0.707106781186547,0.707106781186548,0.707106781186547,
0.707106781186548,0.707106781186547,0.707106781186548,0.707106781186547,
0.707106781186548,0.707106781186547,0.707106781186548,0.707106781186547,
0.707106781186548,0.707106781186548,0.707106781186547,0.707106781186548,
0.707106781186547,0.707106781186547,0.707106781186547,0.707106781186548,
0.707106781186547,0.707106781186547,0.707106781186547,0.707106781186548,
0.707106781186547,0.707106781186547,0.707106781186548,0.707106781186547,
0.707106781186547,0.707106781186547,0.707106781186547,0.707106781186548,
0.707106781186547,0.707106781186547,0.707106781186547,0.707106781186548,
0.707106781186548,0.707106781186548,0.707106781186548,0.707106781186547,
0.707106781186548,0.707106781186547,0.707106781186547,0.707106781186548,
0.707106781186547,0.707106781186548,0.707106781186547,0.707106781186547,
0.707106781186548,0.707106781186547,0.707106781186547,0.707106781186547,
0.707106781186547,0.707106781186548,0.707106781186548,0.707106781186547,
0.707106781186547,0.707106781186548,0.707106781186547,0.707106781186548,
0.707106781186547,0.707106781186548,0.707106781186548,0.707106781186547,
0.707106781186547,0.707106781186548,0.707106781186548,0.707106781186547,
0.707106781186548,0.707106781186548,0.707106781186547,0.707106781186548,
0.707106781186548,0.707106781186548,0.707106781186547,0.707106781186548,
0.707106781186547,0.707106781186548,0.707106781186547,0.707106781186548,
0.707106781186547,0.707106781186548,0.707106781186547,0.707106781186548,
0.707106781186548,0.707106781186547,0.707106781186547,0.707106781186548,
0.707106781186547,0.707106781186548,0.707106781186547,0.707106781186548,
0.707106781186548,0.707106781186548,0.707106781186548,0.707106781186548,
0.707106781186547,0.707106781186547,0.707106781186547,0.707106781186547,
0.707106781186548,0.707106781186547,0.707106781186548,0.707106781186547,
0.707106781186547,0.707106781186548,0.707106781186548,0.707106781186547,
0.707106781186548,0.707106781186547,0.707106781186548,0.707106781186548,
0.707106781186547,0.707106781186547,0.707106781186548,0.707106781186547,
0.707106781186548,0.707106781186547,0.707106781186548,0.707106781186547,
0.707106781186548,0.707106781186547,0.707106781186548,0.707106781186547,
0.707106781186548,0.707106781186547,0.707106781186548,0.707106781186548,
0.707106781186547,0.707106781186548,0.707106781186547,0.707106781186548,
0.707106781186547,0.707106781186548,0.707106781186548,0.707106781186548,
0.707106781186547,0.707106781186547,0.707106781186548,0.707106781186548,
0.707106781186547,0.707106781186547,0.707106781186547,0.707106781186548,
0.707106781186547,0.707106781186548,0.707106781186547,0.707106781186548,
0.707106781186547,0.707106781186547,0.707106781186547,0.707106781186548,
0.707106781186547,0.707106781186548,0.707106781186547,0.707106781186548,
0.707106781186547,0.707106781186548,0.707106781186547,0.707106781186547,
0.707106781186548,0.707106781186547,0.707106781186547,0.707106781186548,
0.707106781186547,0.707106781186547,0.707106781186548,0.707106781186547,
0.707106781186547,0.707106781186547,0.707106781186548,0.707106781186547,
0.707106781186548,0.707106781186547,0.707106781186547,0.707106781186547,
0.707106781186548,0.707106781186548,0.707106781186547,0.707106781186547,
0.707106781186548,0.707106781186548,0.707106781186548,0.707106781186547,
0.707106781186548,0.707106781186547,0.707106781186548,0.707106781186547,
0.707106781186548,0.707106781186547,0.707106781186547,0.707106781186547,
0.707106781186547,0.707106781186548,0.707106781186547,0.707106781186548,
0.707106781186548,0.707106781186547,0.707106781186548,0.707106781186547,
0.707106781186547,0.707106781186547,0.707106781186547,0.707106781186548,
0.707106781186547,0.707106781186548,0.707106781186547,0.707106781186548,
0.707106781186548,0.707106781186547,0.707106781186548,0.707106781186547,
0.707106781186547,0.707106781186547,0.707106781186547,0.707106781186548,
0.707106781186547,0.707106781186548,0.707106781186548,0.707106781186547,
0.707106781186548,0.707106781186547,0.707106781186548,0.707106781186547,
0.707106781186547,0.707106781186548,0.707106781186547,0.707106781186548,
0.707106781186548,0.707106781186547,0.707106781186547,0.707106781186548,
0.707106781186548,0.707106781186547,0.707106781186547,0.707106781186548,
0.707106781186547,0.707106781186547,0.707106781186548,0.707106781186547,
0.707106781186547,0.707106781186548,0.707106781186547,0.707106781186548,
0.707106781186547,0.707106781186547,0.707106781186548,0.707106781186547,
0.707106781186548,0.707106781186547,0.707106781186548,0.707106781186547,
0.707106781186547,0.707106781186547,0.707106781186548,0.707106781186547,
0.707106781186548,0.707106781186547,0.707106781186548,0.707106781186548,
0.707106781186548,0.707106781186548,0.707106781186547,0.707106781186547,
0.707106781186547,0.707106781186548,0.707106781186547,0.707106781186548,
0.707106781186547,0.707106781186547,0.707106781186548,0.707106781186547,
0.707106781186547,0.707106781186548,0.707106781186547,0.707106781186547,
0.707106781186548,0.707106781186548,0.707106781186547,0.707106781186548,
0.707106781186547,0.707106781186547,0.707106781186548,0.707106781186547,
0.707106781186548,0.707106781186547,0.707106781186548,0.707106781186547,
0.707106781186547,0.707106781186547,0.707106781186548,0.707106781186547,
0.707106781186548,0.707106781186547,0.707106781186548,0.707106781186547,
0.707106781186547,0.707106781186548,0.707106781186548,0.707106781186548,
0.707106781186547,0.707106781186548,0.707106781186547,0.707106781186548,
0.707106781186547,0.707106781186548,0.707106781186547,0.707106781186548,
0.707106781186548,0.707106781186547,0.707106781186547,0.707106781186547,
0.707106781186548,0.707106781186547,0.707106781186547,0.707106781186548,
0.707106781186547,0.707106781186547,0.707106781186548,0.707106781186547,
0.707106781186548,0.707106781186548,0.707106781186548,0.707106781186547,
0.707106781186548,0.707106781186547,0.707106781186548,0.707106781186547,
0.707106781186548,0.707106781186547,0.707106781186548,0.707106781186547,
0.707106781186548,0.707106781186547,0.707106781186548,0.707106781186548,
0.707106781186547,0.707106781186548,0.707106781186547,0.707106781186548,
0.707106781186548,0.707106781186547,0.707106781186547,0.707106781186548,
0.707106781186547,0.707106781186547,0.707106781186548,0.707106781186547,
0.707106781186548,0.707106781186548,0.707106781186547,0.707106781186548,
0.707106781186548,0.707106781186548,0.707106781186548,0.707106781186548,
0.707106781186547,0.707106781186548,0.707106781186548,0.707106781186548,
0.707106781186547,0.707106781186548,0.707106781186547,0.707106781186548,
0.707106781186547,0.707106781186548,0.707106781186547,0.707106781186548,
0.707106781186547,0.707106781186548,0.707106781186547,0.707106781186547,
0.707106781186548,0.707106781186547,0.707106781186547,0.707106781186548,
0.707106781186547,0.707106781186548,0.707106781186547,0.707106781186548,
0.707106781186547,0.707106781186548,0.707106781186547,0.707106781186547,
0.707106781186548,0.707106781186547,0.707106781186547,0.707106781186548,
0.707106781186547,0.707106781186548,0.707106781186547,0.707106781186547,
0.707106781186548,0.707106781186548,0.707106781186547,0.707106781186548,
0.707106781186547,0.707106781186547,0.707106781186547,0.707106781186548,
0.707106781186547,0.707106781186547,0.707106781186548,0.707106781186547,
0.707106781186547,0.707106781186547,0.707106781186548,0.707106781186548,
0.707106781186547,0.707106781186548,0.707106781186547,0.707106781186548,
0.707106781186547,0.707106781186547,0.707106781186548,0.707106781186547,
0.707106781186548,0.707106781186547,0.707106781186547,0.707106781186547,
0.707106781186547,0.707106781186548,0.707106781186547,0.707106781186547,
0.707106781186547,0.707106781186547,0.707106781186547,0.707106781186548,
0.707106781186547,0.707106781186547,0.707106781186547,0.707106781186547,
0.707106781186548,0.707106781186547,0.707106781186548,0.707106781186547,
0.707106781186547,0.707106781186548,0.707106781186547,0.707106781186548,
0.707106781186547,0.707106781186547,0.707106781186548,0.707106781186547,
0.707106781186547,0.707106781186548,0.707106781186547,0.707106781186547,
0.707106781186547,0.707106781186547,0.707106781186548,0.707106781186547,
0.707106781186548,0.707106781186548,0.707106781186547,0.707106781186548,
0.707106781186548,0.707106781186547,0.707106781186547,0.707106781186548,
0.707106781186547,0.707106781186547,0.707106781186547,0.707106781186548,
0.707106781186547,0.707106781186547,0.707106781186548,0.707106781186547,
0.707106781186548,0.707106781186547,0.707106781186548,0.707106781186547,
0.707106781186547,0.707106781186548,0.707106781186547,0.707106781186548,
0.707106781186547,0.707106781186548,0.707106781186547,0.707106781186548,
0.707106781186547,0.707106781186548,0.707106781186547,0.707106781186547,
0.707106781186547,0.707106781186547,0.707106781186548,0.707106781186548,
0.707106781186547,0.707106781186548,0.707106781186548,0.707106781186547,
0.707106781186548,0.707106781186547,0.707106781186547,0.707106781186548,
0.707106781186547,0.707106781186547,0.707106781186547,0.707106781186547,
0.707106781186548,0.707106781186547,0.707106781186547,0.707106781186547,
0.707106781186548,0.707106781186547,0.707106781186547,0.707106781186548,
0.707106781186547,0.707106781186548,0.707106781186548,0.707106781186547,
0.707106781186548,0.707106781186547,0.707106781186548,0.707106781186547,
0.707106781186548,0.707106781186547,0.707106781186547,0.707106781186548,
0.707106781186547,0.707106781186548,0.707106781186548,0.707106781186547,
0.707106781186547,0.707106781186548,0.707106781186547,0.707106781186548,
0.707106781186547,0.707106781186548,0.707106781186547,0.707106781186547,
0.707106781186548,0.707106781186548,0.707106781186547,0.707106781186548,
0.707106781186548,0.707106781186547,0.707106781186548,0.707106781186548,
0.707106781186547,0.707106781186548,0.707106781186547,0.707106781186548,
0.707106781186547,0.707106781186548,0.707106781186547,0.707106781186548,
0.707106781186547,0.707106781186547,0.707106781186548,0.707106781186547,
0.707106781186547,0.707106781186548,0.707106781186547,0.707106781186548,
0.707106781186548,0.707106781186547,0.707106781186547,0.707106781186547,
0.707106781186548,0.707106781186547,0.707106781186548,0.707106781186548,
0.707106781186547,0.707106781186548,0.707106781186547,0.707106781186548,
0.707106781186547,0.707106781186548,0.707106781186547,0.707106781186547,
0.707106781186548,0.707106781186548,0.707106781186548,0.707106781186547,
0.707106781186548,0.707106781186548,0.707106781186547,0.707106781186548,
0.707106781186547,0.707106781186548,0.707106781186548,0.707106781186548,
0.707106781186548,0.707106781186548,0.707106781186548,0.707106781186547,
0.707106781186547,0.707106781186548,0.707106781186547,0.707106781186547,
0.707106781186548,0.707106781186547,0.707106781186547,0.707106781186548,
0.707106781186547,0.707106781186548,0.707106781186547,0.707106781186548,
0.707106781186547,0.707106781186547,0.707106781186547,0.707106781186548,
0.707106781186547,0.707106781186547,0.707106781186548,0.707106781186547,
0.707106781186548,0.707106781186547,0.707106781186548,0.707106781186547,
0.707106781186547,0.707106781186547,0.707106781186547,0.707106781186548,
0.707106781186547,0.707106781186547,0.707106781186548,0.707106781186548,
0.707106781186547,0.707106781186548,0.707106781186547,0.707106781186548,
0.707106781186547,0.707106781186547,0.707106781186548,0.707106781186547,
0.707106781186548,0.707106781186547,0.707106781186548,0.707106781186547,
0.707106781186548,0.707106781186548,0.707106781186547,0.707106781186548,
0.707106781186547,0.707106781186547,0.707106781186548,0.707106781186547,
0.707106781186547,0.707106781186548,0.707106781186548,0.707106781186548,
0.707106781186547,0.707106781186548,0.707106781186547,0.707106781186547,
0.707106781186547,0.707106781186548,0.707106781186547,0.707106781186548,
0.707106781186548,0.707106781186548,0.707106781186547,0.707106781186547,
0.707106781186547,0.707106781186547,0.707106781186548,0.707106781186547,
0.707106781186547,0.707106781186548,0.707106781186547,0.707106781186548,
0.707106781186547,0.707106781186547,0.707106781186548,0.707106781186547,
0.707106781186548,0.707106781186547,0.707106781186548,0.707106781186547,
0.707106781186547,0.707106781186547,0.707106781186547,0.707106781186547,
0.707106781186547,0.707106781186548,0.707106781186547,0.707106781186547,
0.707106781186548,0.707106781186548,0.707106781186547,0.707106781186548,
0.707106781186548,0.707106781186547,0.707106781186547,0.707106781186548,
0.707106781186547,0.707106781186547,0.707106781186548,0.707106781186547,
0.707106781186548,0.707106781186548,0.707106781186548,0.707106781186547,
0.707106781186547,0.707106781186547,0.707106781186547,0.707106781186548,
0.707106781186548,0.707106781186548,0.707106781186547,0.707106781186548,
0.707106781186547,0.707106781186548,0.707106781186548,0.707106781186547,
0.707106781186548,0.707106781186547,0.707106781186548,0.707106781186548,
0.707106781186547,0.707106781186547,0.707106781186548,0.707106781186547,
0.707106781186548,0.707106781186547,0.707106781186548,0.707106781186548,
0.707106781186548,0.707106781186547,0.707106781186548,0.707106781186547,
0.707106781186547,0.707106781186547,0.707106781186547,0.707106781186548,
0.707106781186548,0.707106781186547,0.707106781186547,0.707106781186547,
0.707106781186548,0.707106781186547,0.707106781186547,0.707106781186548,
0.707106781186547,0.707106781186548,0.707106781186548,0.707106781186548,
0.707106781186547,0.707106781186547,0.707106781186547,0.707106781186547,
0.707106781186548,0.707106781186548,0.707106781186547,0.707106781186548,
0.707106781186547,0.707106781186548,0.707106781186548,0.707106781186547,
0.707106781186548,0.707106781186547,0.707106781186548,0.707106781186547,
0.707106781186547,0.707106781186547,0.707106781186548,0.707106781186547,
0.707106781186548,0.707106781186547,0.707106781186548,0.707106781186547,
0.707106781186548,0.707106781186547,0.707106781186548,0.707106781186547,
0.707106781186547,0.707106781186548,0.707106781186547,0.707106781186548,
0.707106781186547,0.707106781186547,0.707106781186548,0.707106781186548,
0.707106781186547,0.707106781186548,0.707106781186548,0.707106781186547,
0.707106781186548,0.707106781186547,0.707106781186548,0.707106781186547,
0.707106781186547,0.707106781186547,0.707106781186548,0.707106781186547,
0.707106781186547,0.707106781186548,0.707106781186547,0.707106781186548,
0.707106781186547,0.707106781186548,0.707106781186548,0.707106781186547,
0.707106781186548,0.707106781186547,0.707106781186548,0.707106781186548,
0.707106781186548,0.707106781186548,0.707106781186547,0.707106781186547,
0.707106781186548,0.707106781186547,0.707106781186547,0.707106781186548,
0.707106781186548,0.707106781186547,0.707106781186547,0.707106781186548,
0.707106781186547,0.707106781186547,0.707106781186548,0.707106781186547,
0.707106781186548,0.707106781186547,0.707106781186548,0.707106781186547,
0.707106781186547,0.707106781186547,0.707106781186548,0.707106781186547,
0.707106781186547,0.707106781186548,0.707106781186547,0.707106781186548,
0.707106781186548,0.707106781186548,0.707106781186547,0.707106781186547,
0.707106781186547,0.707106781186548,0.707106781186548,0.707106781186547,
0.707106781186547,0.707106781186547,0.707106781186547,0.707106781186548,
0.707106781186548,0.707106781186547,0.707106781186547,0.707106781186547,
0.707106781186548,0.707106781186548,0.707106781186547,0.707106781186548,
0.707106781186547,0.707106781186548,0.707106781186547,0.707106781186548,
0.707106781186548,0.707106781186547,0.707106781186548,0.707106781186548,
0.707106781186548,0.707106781186547,0.707106781186547,0.707106781186547,
0.707106781186548,0.707106781186548,0.707106781186548,0.707106781186547,
0.707106781186547,0.707106781186548,0.707106781186548,0.707106781186547,
0.707106781186548,0.707106781186547,0.707106781186547,0.707106781186548,
0.707106781186547,0.707106781186548,0.707106781186547,0.707106781186547,
0.707106781186548,0.707106781186547,0.707106781186548,0.707106781186548,
0.707106781186547,0.707106781186547,0.707106781186548,0.707106781186547,
0.707106781186548,0.707106781186547,0.707106781186547,0.707106781186548,
0.707106781186547,0.707106781186548,0.707106781186547,0.707106781186548,
0.707106781186547,0.707106781186547,0.707106781186548,0.707106781186547,
0.707106781186547,0.707106781186547,0.707106781186547,0.707106781186547,
0.707106781186547,0.707106781186548,0.707106781186547,0.707106781186548,
0.707106781186548,0.707106781186548,0.707106781186547,0.707106781186547,
0.707106781186547,0.707106781186548,0.707106781186547,0.707106781186548,
0.707106781186547,0.707106781186547,0.707106781186548,0.707106781186547,
0.707106781186547,0.707106781186547,0.707106781186547,0.707106781186547,
0.707106781186548,0.707106781186547,0.707106781186548,0.707106781186547,
0.707106781186547,0.707106781186548,0.707106781186548,0.707106781186547,
0.707106781186547,0.707106781186547,0.707106781186548,0.707106781186547,
0.707106781186547,0.707106781186548,0.707106781186548,0.707106781186547,
0.707106781186548,0.707106781186547,0.707106781186548,0.707106781186548,
0.707106781186547,0.707106781186547,0.707106781186547,0.707106781186548,
0.707106781186548,0.707106781186547,0.707106781186548,0.707106781186547,
0.707106781186548,0.707106781186548,0.707106781186547,0.707106781186548,
0.707106781186547,0.707106781186547,0.707106781186547,0.707106781186548,
0.707106781186547,0.707106781186548,0.707106781186547,0.707106781186548,
0.707106781186547,0.707106781186547,0.707106781186547,0.707106781186547,
0.707106781186547,0.707106781186548,0.707106781186547,0.707106781186548,
0.707106781186547,0.707106781186548,0.707106781186547,0.707106781186548,
0.707106781186547,0.707106781186547,0.707106781186547,0.707106781186547,
0.707106781186547,0.707106781186548,0.707106781186548,0.707106781186548,
0.707106781186547,0.707106781186548,0.707106781186547,0.707106781186548,
0.707106781186547,0.707106781186547,0.707106781186548,0.707106781186547,
0.707106781186548,0.707106781186547,0.707106781186547,0.707106781186547,
0.707106781186548,0.707106781186548,0.707106781186547,0.707106781186548,
0.707106781186547,0.707106781186548,0.707106781186548,0.707106781186547,
0.707106781186548,0.707106781186547,0.707106781186548,0.707106781186548,
0.707106781186547,0.707106781186547,0.707106781186547,0.707106781186547,
0.707106781186547,0.707106781186547,0.707106781186548,0.707106781186548,
0.707106781186547,0.707106781186548,0.707106781186547,0.707106781186547,
0.707106781186548,0.707106781186547,0.707106781186547,0.707106781186548,
0.707106781186547,0.707106781186547,0.707106781186547,0.707106781186548,
0.707106781186547,0.707106781186547,0.707106781186548,0.707106781186547,
0.707106781186548,0.707106781186548,0.707106781186547,0.707106781186547,
0.707106781186547,0.707106781186548,0.707106781186547,0.707106781186547,
0.707106781186548,0.707106781186548,0.707106781186548,0.707106781186548,
0.707106781186547,0.707106781186548,0.707106781186548,0.707106781186547,
0.707106781186547,0.707106781186548,0.707106781186547,0.707106781186548,
0.707106781186547,0.707106781186547,0.707106781186548,0.707106781186547,
0.707106781186547,0.707106781186548,0.707106781186547,0.707106781186548,
0.707106781186547,0.707106781186548,0.707106781186547,0.707106781186548,
0.707106781186547,0.707106781186548,0.707106781186547,0.707106781186548,
0.707106781186548,0.707106781186547,0.707106781186547,0.707106781186548,
0.707106781186548,0.707106781186547,0.707106781186547,0.707106781186547,
0.707106781186547,0.707106781186547,0.707106781186548,0.707106781186547,
0.707106781186547,0.707106781186548,0.707106781186547,0.707106781186548,
0.707106781186548,0.707106781186547,0.707106781186548,0.707106781186547,
0.707106781186548,0.707106781186547,0.707106781186548,0.707106781186547,
0.707106781186547,0.707106781186547,0.707106781186547,0.707106781186547,
0.707106781186547,0.707106781186548,0.707106781186547,0.707106781186548,
0.707106781186547,0.707106781186547,0.707106781186547,0.707106781186548,
0.707106781186547,0.707106781186548,0.707106781186548,0.707106781186547,
0.707106781186547,0.707106781186548,0.707106781186547,0.707106781186548,
0.707106781186547,0.707106781186548,0.707106781186547,0.707106781186548,
0.707106781186547,0.707106781186547,0.707106781186548,0.707106781186547,
0.707106781186548,0.707106781186547,0.707106781186548,0.707106781186548,
0.707106781186548,0.707106781186548,0.707106781186547,0.707106781186548,
0.707106781186548,0.707106781186548,0.707106781186547,0.707106781186548,
0.707106781186548,0.707106781186547,0.707106781186548,0.707106781186547,
0.707106781186548,0.707106781186547,0.707106781186547,0.707106781186547,
0.707106781186548,0.707106781186548,0.707106781186547,0.707106781186548,
0.707106781186547,0.707106781186548,0.707106781186547,0.707106781186548,
0.707106781186548,0.707106781186547,0.707106781186548,0.707106781186547,
0.707106781186547,0.707106781186548,0.707106781186547,0.707106781186547,
0.707106781186547,0.707106781186548,0.707106781186547,0.707106781186548,
0.707106781186548,0.707106781186547,0.707106781186548,0.707106781186547,
0.707106781186548,0.707106781186548,0.707106781186548,0.707106781186548,
0.707106781186547,0.707106781186548,0.707106781186547,0.707106781186548,
0.707106781186547,0.707106781186548,0.707106781186547,0.707106781186547,
0.707106781186547,0.707106781186547,0.707106781186548,0.707106781186547,
0.707106781186548,0.707106781186547,0.707106781186547,0.707106781186548,
0.707106781186547,0.707106781186548,0.707106781186547,0.707106781186548,
0.707106781186547,0.707106781186548,0.707106781186548,0.707106781186548,
0.707106781186548,0.707106781186547,0.707106781186548,0.707106781186548,
0.707106781186547,0.707106781186548,0.707106781186547,0.707106781186548,
0.707106781186547,0.707106781186548,0.707106781186547,0.707106781186547,
0.707106781186548,0.707106781186547,0.707106781186548,0.707106781186547,
0.707106781186547,0.707106781186548,0.707106781186547,0.707106781186548,
0.707106781186547,0.707106781186547,0.707106781186548,0.707106781186548,
0.707106781186548,0.707106781186548,0.707106781186548,0.707106781186548,
0.707106781186548,0.707106781186548,0.707106781186548,0.707106781186547,
0.707106781186548,0.707106781186547,0.707106781186547,0.707106781186548,
0.707106781186547,0.707106781186548,0.707106781186548,0.707106781186547,
0.707106781186547,0.707106781186548,0.707106781186548,0.707106781186547,
0.707106781186547,0.707106781186547,0.707106781186547,0.707106781186547,
0.707106781186548,0.707106781186547,0.707106781186548,0.707106781186548,
0.707106781186548,0.707106781186547,0.707106781186548,0.707106781186547,
0.707106781186548,0.707106781186547,0.707106781186548,0.707106781186547,
0.707106781186548,0.707106781186548,0.707106781186547,0.707106781186547,
0.707106781186548,0.707106781186548,0.707106781186548,0.707106781186547,
0.707106781186547,0.707106781186548,0.707106781186547,0.707106781186547,
0.707106781186548,0.707106781186547,0.707106781186548,0.707106781186547,
0.707106781186547,0.707106781186548,0.707106781186548,0.707106781186548,
0.707106781186547,0.707106781186547,0.707106781186548,0.707106781186547,
0.707106781186548,0.707106781186547,0.707106781186548,0.707106781186547,
0.707106781186548,0.707106781186548,0.707106781186547,0.707106781186548,
0.707106781186547,0.707106781186548,0.707106781186547,0.707106781186547,
0.707106781186547,0.707106781186548,0.707106781186547,0.707106781186548,
0.707106781186547,0.707106781186547,0.707106781186547,0.707106781186548,
0.707106781186547,0.707106781186547,0.707106781186548,0.707106781186548,
0.707106781186547,0.707106781186548,0.707106781186547,0.707106781186548,
0.707106781186548,0.707106781186547,0.707106781186548,0.707106781186547,
0.707106781186547,0.707106781186548,0.707106781186547,0.707106781186547,
0.707106781186547,0.707106781186548,0.707106781186547,0.707106781186548,
0.707106781186547,0.707106781186548,0.707106781186548,0.707106781186548,
0.707106781186547,0.707106781186548,0.707106781186548,0.707106781186548,
0.707106781186547,0.707106781186548,0.707106781186547,0.707106781186547,
0.707106781186548,0.707106781186547,0.707106781186547,0.707106781186548,
0.707106781186548,0.707106781186547,0.707106781186548,0.707106781186547,
0.707106781186548,0.707106781186548,0.707106781186547,0.707106781186548,
0.707106781186547,0.707106781186548,0.707106781186547,0.707106781186548,
0.707106781186547,0.707106781186548,0.707106781186548,0.707106781186548,
0.707106781186547,0.707106781186548,0.707106781186548,0.707106781186547,
0.707106781186547,0.707106781186548,0.707106781186547,0.707106781186548,
0.707106781186548,0.707106781186547,0.707106781186548,0.707106781186548,
0.707106781186547,0.707106781186548,0.707106781186548,0.707106781186547,
0.707106781186547,0.707106781186548,0.707106781186547,0.707106781186548,
0.707106781186547,0.707106781186548,0.707106781186547,0.707106781186548,
0.707106781186548,0.707106781186548,0.707106781186547,0.707106781186548,
0.707106781186547,0.707106781186548,0.707106781186547,0.707106781186548,
0.707106781186547,0.707106781186548,0.707106781186547,0.707106781186548,
0.707106781186547,0.707106781186548,0.707106781186547,0.707106781186547,
0.707106781186547,0.707106781186548,0.707106781186547,0.707106781186548,
0.707106781186547,0.707106781186548,0.707106781186547,0.707106781186548,
0.707106781186547,0.707106781186548,0.707106781186548,0.707106781186548,
0.707106781186547,0.707106781186548,0.707106781186547,0.707106781186548,
0.707106781186548,0.707106781186547,0.707106781186548,0.707106781186547,
0.707106781186548,0.707106781186547,0.707106781186548,0.707106781186547,
0.707106781186548,0.707106781186547,0.707106781186547,0.707106781186547,
0.707106781186548,0.707106781186547,0.707106781186547,0.707106781186548,
0.707106781186547,0.707106781186548,0.707106781186547,0.707106781186547,
0.707106781186548,0.707106781186547,0.707106781186548,0.707106781186547,
0.707106781186548,0.707106781186548,0.707106781186548,0.707106781186547,
0.707106781186547,0.707106781186548,0.707106781186548,0.707106781186547,
0.707106781186548,0.707106781186547,0.707106781186547,0.707106781186547,
0.707106781186548,0.707106781186547,0.707106781186548,0.707106781186547,
0.707106781186548,0.707106781186548,0.707106781186548,0.707106781186547,
0.707106781186547,0.707106781186547,0.707106781186547,0.707106781186547,
0.707106781186547,0.707106781186548,0.707106781186547,0.707106781186548,
0.707106781186547,0.707106781186548,0.707106781186547,0.707106781186547,
0.707106781186548,0.707106781186547,0.707106781186547,0.707106781186548,
0.707106781186548,0.707106781186547,0.707106781186547,0.707106781186547,
0.707106781186548,0.707106781186547,0.707106781186547,0.707106781186548,
0.707106781186548),(1.,1.,1.,1.,1.,1.,1.,1.,1.,1.,1.,1.,1.,1.,1.,1.,1.,
1.,1.,1.,1.,1.,1.,1.,1.,1.,1.,1.,1.,1.,1.,1.,1.,1.,1.,1.,1.,1.,1.,1.,1.,
1.,1.,1.,1.,1.,1.,1.,1.,1.,1.,1.,1.,1.,1.,1.,1.,1.,1.,1.,1.,1.,1.,1.,1.,
1.,1.,1.,1.,1.,1.,1.,1.,1.,1.,1.,1.,1.,1.,1.,1.,1.,1.,1.,1.,1.,1.,1.,1.,
1.,1.,1.,1.,1.,1.,1.,1.,1.,1.,1.,1.,1.,1.,1.,1.,1.,1.,1.,1.,1.,1.,1.,1.,
1.,1.,1.,1.,1.,1.,1.,1.,1.,1.,1.,1.,1.,1.,1.,1.,1.,1.,1.,1.,1.,1.,1.,1.,
1.,1.,1.,1.,1.,1.,1.,1.,1.,1.,1.,1.,1.,1.,1.,1.,1.,1.,1.,1.,1.,1.,1.,1.,
1.,1.,1.,1.,1.,1.,1.,1.,1.,1.,1.,1.,1.,1.,1.,1.,1.,1.,1.,1.,1.,1.,1.,1.,
1.,1.,1.,1.,1.,1.,1.,1.,1.,1.,1.,1.,1.,1.,1.,1.,1.,1.,1.,1.,1.,1.,1.,1.,
1.,1.,1.,1.,1.,1.,1.,1.,1.,1.,1.,1.,1.,1.,1.,1.,1.,1.,1.,1.,1.,1.,1.,1.,
1.,1.,1.,1.,1.,1.,1.,1.,1.,1.,1.,1.,1.,1.,1.,1.,1.,1.,1.,1.,1.,1.,1.,1.,
1.,1.,1.,1.,1.,1.,1.,1.,1.,1.,1.,1.,1.,1.,1.,1.,1.,1.,1.,1.,1.,1.,1.,1.,
1.,1.,1.,1.,1.,1.,1.,1.,1.,1.,1.,1.,1.,1.,1.,1.,1.,1.,1.,1.,1.,1.,1.,1.,
1.,1.,1.,1.,1.,1.,1.,1.,1.,1.,1.,1.,1.,1.,1.,1.,1.,1.,1.,1.,1.,1.,1.,1.,
1.,1.,1.,1.,1.,1.,1.,1.,1.,1.,1.,1.,1.,1.,1.,1.,1.,1.,1.,1.,1.,1.,1.,1.,
1.,1.,1.,1.,1.,1.,1.,1.,1.,1.,1.,1.,1.,1.,1.,1.,1.,1.,1.,1.,1.,1.,1.,1.,
1.,1.,1.,1.,1.,1.,1.,1.,1.,1.,1.,1.,1.,1.,1.,1.,1.,1.,1.,1.,1.,1.,1.,1.,
1.,1.,1.,1.,1.,1.,1.,1.,1.,1.,1.,1.,1.,1.,1.,1.,1.,1.,1.,1.,1.,1.,1.,1.,
1.,1.,1.,1.,1.,1.,1.,1.,1.,1.,1.,1.,1.,1.,1.,1.,1.,1.,1.,1.,1.,1.,1.,1.,
1.,1.,1.,1.,1.,1.,1.,1.,1.,1.,1.,1.,1.,1.,1.,1.,1.,1.,1.,1.,1.,1.,1.,1.,
1.,1.,1.,1.,1.,1.,1.,1.,1.,1.,1.,1.,1.,1.,1.,1.,1.,1.,1.,1.,1.,1.,1.,1.,
1.,1.,1.,1.,1.,1.,1.,1.,1.,1.,1.,1.,1.,1.,1.,1.,1.,1.,1.,1.,1.,1.,1.,1.,
1.,1.,1.,1.,1.,1.,1.,1.,1.,1.,1.,1.,1.,1.,1.,1.,1.,1.,1.,1.,1.,1.,1.,1.,
1.,1.,1.,1.,1.,1.,1.,1.,1.,1.,1.,1.,1.,1.,1.,1.,1.,1.,1.,1.,1.,1.,1.,1.,
1.,1.,1.,1.,1.,1.,1.,1.,1.,1.,1.,1.,1.,1.,1.,1.,1.,1.,1.,1.,1.,1.,1.,1.,
1.,1.,1.,1.,1.,1.,1.,1.,1.,1.,1.,1.,1.,1.,1.,1.,1.,1.,1.,1.,1.,1.,1.,1.,
1.,1.,1.,1.,1.,1.,1.,1.,1.,1.,1.,1.,1.,1.,1.,1.,1.,1.,1.,1.,1.,1.,1.,1.,
1.,1.,1.,1.,1.,1.,1.,1.,1.,1.,1.,1.,1.,1.,1.,1.,1.,1.,1.,1.,1.,1.,1.,1.,
1.,1.,1.,1.,1.,1.,1.,1.,1.,1.,1.,1.,1.,1.,1.,1.,1.,1.,1.,1.,1.,1.,1.,1.,
1.,1.,1.,1.,1.,1.,1.,1.,1.,1.,1.,1.,1.,1.,1.,1.,1.,1.,1.,1.,1.,1.,1.,1.,
1.,1.,1.,1.,1.,1.,1.,1.,1.,1.,1.,1.,1.,1.,1.,1.,1.,1.,1.,1.,1.,1.,1.,1.,
1.,1.,1.,1.,1.,1.,1.,1.,1.,1.,1.,1.,1.,1.,1.,1.,1.,1.,1.,1.,1.,1.,1.,1.,
1.,1.,1.,1.,1.,1.,1.,1.,1.,1.,1.,1.,1.,1.,1.,1.,1.,1.,1.,1.,1.,1.,1.,1.,
1.,1.,1.,1.,1.,1.,1.,1.,1.,1.,1.,1.,1.,1.,1.,1.,1.,1.,1.,1.,1.,1.,1.,1.,
1.,1.,1.,1.,1.,1.,1.,1.,1.,1.,1.,1.,1.,1.,1.,1.,1.,1.,1.,1.,1.,1.,1.,1.,
1.,1.,1.,1.,1.,1.,1.,1.,1.,1.,1.,1.,1.,1.,1.,1.,1.,1.,1.,1.,1.,1.,1.,1.,
1.,1.,1.,1.,1.,1.,1.,1.,1.,1.,1.,1.,1.,1.,1.,1.,1.,1.,1.,1.,1.,1.,1.,1.,
1.,1.,1.,1.,1.,1.,1.,1.,1.,1.,1.,1.,1.,1.,1.,1.,1.,1.,1.,1.,1.,1.,1.,1.,
1.,1.,1.,1.,1.,1.,1.,1.,1.,1.,1.,1.,1.,1.,1.,1.,1.,1.,1.,1.,1.,1.,1.,1.,
1.,1.,1.,1.,1.,1.,1.,1.,1.,1.,1.,1.,1.,1.,1.,1.,1.,1.,1.,1.,1.,1.,1.,1.,
1.,1.,1.,1.,1.,1.,1.,1.,1.,1.,1.,1.,1.,1.,1.,1.,1.,1.,1.,1.,1.,1.,1.,1.,
1.,1.,1.,1.,1.,1.,1.,1.,1.,1.,1.,1.,1.,1.,1.,1.,1.,1.,1.,1.,1.,1.,1.,1.,
1.,1.,1.,1.,1.,1.,1.,1.,1.,1.,1.,1.,1.,1.,1.,1.,1.,1.,1.,1.,1.,1.,1.,1.,
1.,1.,1.,1.,1.,1.,1.,1.,1.,1.,1.,1.,1.,1.,1.,1.,1.,1.,1.,1.,1.,1.,1.,1.,
1.,1.,1.,1.,1.,1.,1.,1.,1.,1.,1.,1.,1.,1.,1.,1.,1.,1.,1.,1.,1.,1.,1.,1.,
1.,1.,1.,1.,1.,1.,1.,1.,1.,1.,1.,1.,1.,1.,1.,1.,1.,1.,1.,1.,1.,1.,1.,1.,
1.,1.,1.,1.,1.,1.,1.,1.,1.,1.,1.,1.,1.,1.,1.,1.,1.,1.,1.,1.,1.,1.,1.,1.,
1.,1.,1.,1.,1.,1.,1.,1.,1.,1.,1.,1.,1.,1.,1.,1.,1.,1.,1.,1.,1.,1.,1.,1.,
1.,1.,1.,1.,1.,1.,1.,1.,1.,1.,1.,1.,1.,1.,1.,1.,1.,1.,1.,1.,1.,1.,1.,1.,
1.,1.,1.,1.,1.,1.,1.,1.,1.,1.,1.,1.,1.,1.,1.,1.,1.,1.,1.,1.,1.,1.,1.,1.,
1.,1.,1.,1.,1.,1.,1.,1.,1.,1.,1.,1.,1.,1.,1.,1.,1.,1.,1.,1.,1.,1.,1.,1.,
1.,1.,1.,1.,1.,1.,1.,1.,1.,1.,1.,1.,1.,1.,1.,1.,1.,1.,1.,1.,1.,1.,1.,1.,
1.,1.,1.,1.,1.,1.,1.,1.,1.,1.,1.,1.,1.,1.,1.,1.,1.,1.,1.,1.,1.,1.,1.,1.,
1.,1.,1.,1.,1.,1.,1.,1.,1.,1.,1.,1.,1.,1.,1.,1.,1.,1.,1.,1.,1.,1.,1.,1.,
1.,1.,1.,1.,1.,1.,1.,1.,1.,1.,1.,1.,1.,1.,1.,1.,1.,1.,1.,1.,1.,1.,1.,1.,
1.,1.,1.,1.,1.,1.,1.,1.,1.,1.,1.,1.,1.,1.,1.,1.,1.,1.,1.,1.,1.,1.,1.,1.,
1.,1.,1.,1.,1.,1.,1.,1.,1.,1.,1.,1.,1.,1.,1.,1.,1.,1.,1.,1.,1.,1.,1.,1.,
1.,1.,1.,1.,1.,1.,1.,1.,1.,1.,1.,1.,1.,1.,1.,1.,1.,1.,1.,1.,1.,1.,1.,1.,
1.,1.,1.,1.,1.,1.,1.,1.,1.,1.,1.,1.,1.,1.,1.,1.,1.,1.,1.,1.,1.,1.,1.,1.,
1.,1.,1.,1.,1.,1.,1.,1.,1.,1.,1.,1.,1.,1.,1.,1.,1.,1.,1.,1.,1.,1.,1.,1.,
1.,1.,1.,1.,1.,1.,1.,1.,1.,1.,1.,1.,1.,1.,1.,1.,1.,1.,1.,1.,1.,1.,1.,1.,
1.,1.,1.,1.,1.,1.,1.,1.,1.,1.,1.,1.,1.,1.,1.,1.,1.,1.,1.,1.,1.,1.,1.,1.,
1.,1.,1.,1.,1.,1.,1.,1.,1.,1.,1.,1.,1.,1.,1.,1.,1.,1.,1.,1.,1.,1.,1.,1.,
1.,1.,1.,1.,1.,1.,1.,1.,1.,1.,1.,1.,1.,1.,1.,1.,1.,1.,1.,1.,1.,1.,1.,1.,
1.,1.,1.,1.,1.,1.,1.,1.,1.,1.,1.,1.,1.,1.,1.,1.,1.,1.,1.,1.,1.,1.,1.,1.,
1.,1.,1.,1.,1.,1.,1.,1.,1.,1.,1.,1.,1.,1.,1.,1.,1.,1.,1.,1.,1.,1.,1.,1.,
1.,1.,1.,1.,1.,1.,1.,1.,1.,1.,1.,1.,1.,1.,1.,1.,1.,1.,1.,1.,1.,1.,1.,1.,
1.,1.,1.,1.,1.,1.,1.,1.,1.,1.,1.,1.,1.,1.,1.,1.,1.,1.,1.,1.,1.,1.,1.,1.,
1.,1.,1.,1.,1.,1.,1.,1.,1.,1.,1.,1.,1.,1.,1.,1.,1.,1.,1.,1.,1.,1.,1.,1.,
1.,1.,1.,1.,1.,1.,1.,1.,1.,1.,1.,1.,1.,1.,1.,1.,1.,1.,1.,1.,1.,1.,1.,1.,
1.,1.,1.,1.,1.,1.,1.,1.,1.,1.,1.,1.,1.,1.,1.,1.,1.,1.,1.,1.,1.,1.,1.,1.,
1.,1.,1.,1.,1.,1.,1.,1.,1.,1.,1.,1.,1.,1.,1.,1.,1.,1.,1.,1.,1.,1.,1.,1.,
1.,1.,1.,1.,1.,1.,1.,1.,1.,1.,1.,1.,1.,1.,1.,1.,1.,1.,1.,1.,1.,1.,1.,1.,
1.,1.,1.,1.,1.,1.,1.,1.,1.,1.,1.,1.,1.,1.,1.,1.,1.,1.,1.,1.,1.,1.,1.,1.,
1.,1.,1.,1.,1.,1.,1.,1.,1.,1.,1.,1.,1.,1.,1.,1.,1.,1.,1.,1.,1.,1.,1.,1.,
1.,1.,1.,1.,1.,1.,1.,1.,1.,1.,1.,1.,1.,1.,1.,1.,1.,1.,1.,1.,1.,1.,1.,1.,
1.,1.,1.,1.,1.,1.,1.,1.,1.,1.,1.,1.,1.,1.,1.,1.,1.,1.,1.,1.,1.,1.,1.,1.,
1.,1.,1.,1.,1.,1.,1.,1.,1.,1.,1.,1.,1.,1.,1.,1.,1.,1.,1.,1.,1.,1.,1.,1.,
1.,1.,1.,1.,1.,1.,1.,1.,1.,1.,1.,1.,1.,1.,1.,1.,1.,1.,1.,1.,1.,1.,1.,1.,
1.,1.,1.,1.,1.,1.,1.,1.,1.,1.,1.,1.,1.,1.,1.,1.,1.,1.,1.,1.,1.,1.,1.,1.,
1.,1.,1.,1.,1.,1.,1.,1.,1.,1.,1.,1.,1.,1.,1.,1.,1.,1.,1.,1.,1.,1.,1.,1.,
1.,1.,1.,1.,1.,1.,1.,1.,1.,1.,1.,1.,1.,1.,1.,1.,1.,1.,1.,1.,1.,1.,1.,1.,
1.,1.,1.,1.,1.,1.,1.,1.,1.,1.,1.,1.,1.,1.,1.,1.,1.,1.,1.,1.,1.,1.,1.,1.,
1.,1.,1.,1.,1.,1.,1.,1.,1.,1.,1.,1.,1.,1.,1.,1.,1.,1.,1.,1.,1.,1.,1.,1.,
1.,1.,1.,1.,1.,1.,1.,1.,1.,1.,1.,1.,1.,1.,1.,1.,1.,1.,1.,1.,1.,1.,1.,1.,
1.,1.,1.,1.,1.,1.,1.,1.,1.,1.,1.,1.,1.,1.,1.,1.,1.,1.)))
REPRESENTATION_ITEM('')
SURFACE()
) ;
#44 = (
BOUNDED_SURFACE()
B_SPLINE_SURFACE(3,2,((#134061,#134062,#134063,#134064,#134065,#134066,
#134067,#134068,#134069),(#134070,#134071,#134072,#134073,#134074,#134075,
#134076,#134077,#134078),(#134079,#134080,#134081,#134082,#134083,#134084,
#134085,#134086,#134087),(#134088,#134089,#134090,#134091,#134092,#134093,
#134094,#134095,#134096),(#134097,#134098,#134099,#134100,#134101,#134102,
#134103,#134104,#134105),(#134106,#134107,#134108,#134109,#134110,#134111,
#134112,#134113,#134114),(#134115,#134116,#134117,#134118,#134119,#134120,
#134121,#134122,#134123)),.UNSPECIFIED.,.F.,.T.,.F.)
B_SPLINE_SURFACE_WITH_KNOTS((4,1,1,1,4),(3,2,2,2,3),(0.,0.0911446219616379,
0.182289243923276,0.273433865884915,0.364578487846551),(0.,0.117809724509617,
0.235619449019234,0.353429173528852,0.471238898038469),.UNSPECIFIED.)
GEOMETRIC_REPRESENTATION_ITEM()
RATIONAL_B_SPLINE_SURFACE(((1.,0.707106781186548,1.,0.707106781186548,1.,
0.707106781186548,1.,0.707106781186548,1.),(1.,0.707106781186548,1.,0.707106781186548,
1.,0.707106781186548,1.,0.707106781186548,1.),(1.,0.707106781186547,1.,
0.707106781186547,1.,0.707106781186547,1.,0.707106781186547,1.),(1.,0.707106781186548,
1.,0.707106781186548,1.,0.707106781186548,1.,0.707106781186548,1.),(1.,
0.707106781186547,1.,0.707106781186547,1.,0.707106781186547,1.,0.707106781186547,
1.),(1.,0.707106781186548,1.,0.707106781186548,1.,0.707106781186548,1.,
0.707106781186548,1.),(1.,0.707106781186548,1.,0.707106781186548,1.,0.707106781186548,
1.,0.707106781186548,1.)))
REPRESENTATION_ITEM('')
SURFACE()
) ;
#45 = (
BOUNDED_SURFACE()
B_SPLINE_SURFACE(3,2,((#134133,#134134,#134135,#134136,#134137,#134138,
#134139,#134140,#134141),(#134142,#134143,#134144,#134145,#134146,#134147,
#134148,#134149,#134150),(#134151,#134152,#134153,#134154,#134155,#134156,
#134157,#134158,#134159),(#134160,#134161,#134162,#134163,#134164,#134165,
#134166,#134167,#134168)),.UNSPECIFIED.,.F.,.T.,.F.)
B_SPLINE_SURFACE_WITH_KNOTS((4,4),(3,2,2,2,3),(0.,1.1454147408364),(0.,
0.117809724509617,0.235619449019234,0.353429173528852,0.471238898038469),
 .UNSPECIFIED.)
GEOMETRIC_REPRESENTATION_ITEM()
RATIONAL_B_SPLINE_SURFACE(((1.,0.707106781186548,1.,0.707106781186548,1.,
0.707106781186548,1.,0.707106781186548,1.),(1.,0.707106781186548,1.,0.707106781186548,
1.,0.707106781186548,1.,0.707106781186548,1.),(1.,0.707106781186547,1.,
0.707106781186547,1.,0.707106781186547,1.,0.707106781186547,1.),(1.,0.707106781186548,
1.,0.707106781186548,1.,0.707106781186548,1.,0.707106781186548,1.)))
REPRESENTATION_ITEM('')
SURFACE()
) ;
#46 = (
BOUNDED_SURFACE()
B_SPLINE_SURFACE(3,2,((#134176,#134177,#134178,#134179,#134180,#134181,
#134182,#134183,#134184),(#134185,#134186,#134187,#134188,#134189,#134190,
#134191,#134192,#134193),(#134194,#134195,#134196,#134197,#134198,#134199,
#134200,#134201,#134202),(#134203,#134204,#134205,#134206,#134207,#134208,
#134209,#134210,#134211),(#134212,#134213,#134214,#134215,#134216,#134217,
#134218,#134219,#134220),(#134221,#134222,#134223,#134224,#134225,#134226,
#134227,#134228,#134229),(#134230,#134231,#134232,#134233,#134234,#134235,
#134236,#134237,#134238),(#134239,#134240,#134241,#134242,#134243,#134244,
#134245,#134246,#134247),(#134248,#134249,#134250,#134251,#134252,#134253,
#134254,#134255,#134256),(#134257,#134258,#134259,#134260,#134261,#134262,
#134263,#134264,#134265),(#134266,#134267,#134268,#134269,#134270,#134271,
#134272,#134273,#134274),(#134275,#134276,#134277,#134278,#134279,#134280,
#134281,#134282,#134283),(#134284,#134285,#134286,#134287,#134288,#134289,
#134290,#134291,#134292),(#134293,#134294,#134295,#134296,#134297,#134298,
#134299,#134300,#134301),(#134302,#134303,#134304,#134305,#134306,#134307,
#134308,#134309,#134310),(#134311,#134312,#134313,#134314,#134315,#134316,
#134317,#134318,#134319),(#134320,#134321,#134322,#134323,#134324,#134325,
#134326,#134327,#134328),(#134329,#134330,#134331,#134332,#134333,#134334,
#134335,#134336,#134337),(#134338,#134339,#134340,#134341,#134342,#134343,
#134344,#134345,#134346)),.UNSPECIFIED.,.F.,.T.,.F.)
B_SPLINE_SURFACE_WITH_KNOTS((4,1,1,1,1,1,1,1,1,1,1,1,1,1,1,1,4),(3,2,2,
2,3),(0.,0.226732296973331,0.464902013928651,0.70307173088397,0.9298040278573,
1.15653632483063,1.39470604178595,1.63287575874127,1.8596080557146,2.08634035268793,
2.32451006964325,2.56267978659857,2.7894120835719,3.01614438054523,3.25431409750055,
3.49248381445586,3.7192161114292),(0.,0.117809724509617,0.235619449019234,
0.353429173528852,0.471238898038469),.UNSPECIFIED.)
GEOMETRIC_REPRESENTATION_ITEM()
RATIONAL_B_SPLINE_SURFACE(((1.,0.707106781186548,1.,0.707106781186548,1.,
0.707106781186548,1.,0.707106781186548,1.),(1.,0.707106781186547,1.,0.707106781186547,
1.,0.707106781186547,1.,0.707106781186547,1.),(1.,0.707106781186548,1.,
0.707106781186548,1.,0.707106781186548,1.,0.707106781186548,1.),(1.,0.707106781186547,
1.,0.707106781186547,1.,0.707106781186547,1.,0.707106781186547,1.),(1.,
0.707106781186548,1.,0.707106781186548,1.,0.707106781186548,1.,0.707106781186548,
1.),(1.,0.707106781186547,1.,0.707106781186547,1.,0.707106781186547,1.,
0.707106781186547,1.),(1.,0.707106781186548,1.,0.707106781186548,1.,0.707106781186548,
1.,0.707106781186548,1.),(1.,0.707106781186547,1.,0.707106781186547,1.,
0.707106781186547,1.,0.707106781186547,1.),(1.,0.707106781186547,1.,0.707106781186547,
1.,0.707106781186547,1.,0.707106781186547,1.),(1.,0.707106781186547,1.,
0.707106781186547,1.,0.707106781186547,1.,0.707106781186547,1.),(1.,0.707106781186548,
1.,0.707106781186548,1.,0.707106781186548,1.,0.707106781186548,1.),(1.,
0.707106781186547,1.,0.707106781186547,1.,0.707106781186547,1.,0.707106781186547,
1.),(1.,0.707106781186547,1.,0.707106781186547,1.,0.707106781186547,1.,
0.707106781186547,1.),(1.,0.707106781186547,1.,0.707106781186547,1.,0.707106781186547,
1.,0.707106781186547,1.),(1.,0.707106781186547,1.,0.707106781186547,1.,
0.707106781186547,1.,0.707106781186547,1.),(1.,0.707106781186547,1.,0.707106781186547,
1.,0.707106781186547,1.,0.707106781186547,1.),(1.,0.707106781186548,1.,
0.707106781186548,1.,0.707106781186548,1.,0.707106781186548,1.),(1.,0.707106781186547,
1.,0.707106781186547,1.,0.707106781186547,1.,0.707106781186547,1.),(1.,
0.707106781186548,1.,0.707106781186548,1.,0.707106781186548,1.,0.707106781186548,
1.)))
REPRESENTATION_ITEM('')
SURFACE()
) ;
#47 = (
BOUNDED_SURFACE()
B_SPLINE_SURFACE(2,3,((#134369,#134370,#134371,#134372,#134373,#134374,
#134375,#134376,#134377,#134378,#134379,#134380,#134381,#134382,#134383,
#134384,#134385,#134386,#134387,#134388,#134389,#134390,#134391,#134392,
#134393,#134394,#134395,#134396,#134397,#134398,#134399,#134400,#134401,
#134402,#134403,#134404,#134405,#134406,#134407,#134408,#134409,#134410,
#134411,#134412,#134413,#134414,#134415,#134416,#134417,#134418,#134419,
#134420,#134421,#134422,#134423,#134424,#134425,#134426,#134427,#134428,
#134429,#134430,#134431,#134432,#134433,#134434,#134435,#134436,#134437,
#134438,#134439,#134440,#134441,#134442,#134443,#134444,#134445,#134446,
#134447,#134448,#134449,#134450,#134451,#134452,#134453,#134454,#134455,
#134456,#134457,#134458,#134459,#134460,#134461,#134462,#134463,#134464,
#134465,#134466,#134467,#134468,#134469,#134470,#134471,#134472,#134473,
#134474,#134475,#134476,#134477,#134478,#134479,#134480,#134481,#134482,
#134483,#134484,#134485,#134486,#134487,#134488,#134489,#134490,#134491,
#134492,#134493,#134494,#134495,#134496,#134497,#134498,#134499,#134500,
#134501,#134502,#134503,#134504,#134505,#134506,#134507,#134508,#134509,
#134510,#134511,#134512,#134513,#134514,#134515,#134516,#134517,#134518,
#134519,#134520,#134521,#134522,#134523,#134524,#134525,#134526,#134527,
#134528,#134529,#134530,#134531,#134532,#134533,#134534,#134535,#134536,
#134537,#134538,#134539,#134540,#134541,#134542,#134543,#134544,#134545,
#134546,#134547,#134548,#134549,#134550,#134551,#134552,#134553,#134554,
#134555,#134556,#134557,#134558,#134559,#134560,#134561,#134562,#134563,
#134564,#134565,#134566,#134567,#134568,#134569,#134570,#134571,#134572,
#134573,#134574,#134575,#134576,#134577,#134578,#134579,#134580,#134581,
#134582,#134583,#134584,#134585,#134586,#134587,#134588,#134589,#134590,
#134591,#134592,#134593,#134594,#134595,#134596,#134597,#134598,#134599,
#134600,#134601,#134602,#134603,#134604,#134605,#134606,#134607,#134608,
#134609,#134610,#134611,#134612,#134613,#134614,#134615,#134616,#134617,
#134618,#134619,#134620,#134621,#134622,#134623,#134624,#134625,#134626,
#134627,#134628,#134629,#134630,#134631,#134632,#134633,#134634,#134635,
#134636,#134637,#134638,#134639,#134640,#134641,#134642,#134643,#134644,
#134645,#134646,#134647,#134648,#134649,#134650,#134651,#134652,#134653,
#134654,#134655,#134656,#134657,#134658,#134659,#134660,#134661,#134662,
#134663,#134664,#134665,#134666,#134667,#134668,#134669,#134670,#134671,
#134672,#134673,#134674,#134675,#134676,#134677,#134678,#134679,#134680,
#134681,#134682,#134683,#134684,#134685,#134686,#134687,#134688,#134689,
#134690,#134691,#134692,#134693,#134694,#134695,#134696,#134697,#134698,
#134699,#134700,#134701,#134702,#134703,#134704,#134705,#134706,#134707,
#134708,#134709,#134710,#134711,#134712,#134713,#134714,#134715,#134716,
#134717,#134718,#134719,#134720,#134721,#134722,#134723,#134724,#134725,
#134726,#134727,#134728,#134729,#134730,#134731,#134732,#134733,#134734,
#134735,#134736,#134737,#134738,#134739,#134740,#134741,#134742,#134743,
#134744,#134745,#134746,#134747,#134748,#134749,#134750,#134751,#134752,
#134753,#134754,#134755,#134756,#134757,#134758,#134759,#134760,#134761,
#134762,#134763,#134764,#134765,#134766,#134767,#134768,#134769,#134770,
#134771,#134772,#134773,#134774,#134775,#134776,#134777,#134778,#134779,
#134780,#134781,#134782,#134783,#134784,#134785,#134786,#134787,#134788,
#134789,#134790,#134791,#134792,#134793,#134794,#134795,#134796,#134797,
#134798,#134799,#134800,#134801,#134802,#134803,#134804,#134805,#134806,
#134807,#134808,#134809,#134810,#134811,#134812,#134813,#134814,#134815,
#134816,#134817,#134818,#134819,#134820,#134821,#134822,#134823,#134824,
#134825,#134826,#134827,#134828,#134829,#134830,#134831,#134832,#134833,
#134834,#134835,#134836,#134837,#134838,#134839,#134840,#134841,#134842,
#134843,#134844,#134845,#134846,#134847,#134848,#134849,#134850,#134851,
#134852,#134853,#134854,#134855,#134856,#134857,#134858,#134859,#134860,
#134861,#134862,#134863,#134864,#134865,#134866,#134867,#134868,#134869,
#134870,#134871,#134872,#134873,#134874,#134875,#134876,#134877,#134878,
#134879,#134880,#134881,#134882,#134883,#134884,#134885,#134886,#134887,
#134888,#134889,#134890,#134891,#134892,#134893,#134894,#134895,#134896,
#134897,#134898,#134899,#134900,#134901,#134902,#134903,#134904,#134905,
#134906,#134907,#134908,#134909,#134910,#134911,#134912,#134913,#134914,
#134915,#134916,#134917,#134918,#134919,#134920,#134921,#134922,#134923,
#134924,#134925,#134926,#134927,#134928,#134929,#134930,#134931,#134932,
#134933,#134934,#134935,#134936,#134937,#134938,#134939,#134940,#134941,
#134942,#134943,#134944,#134945,#134946,#134947,#134948,#134949,#134950,
#134951,#134952,#134953,#134954,#134955,#134956,#134957,#134958,#134959,
#134960,#134961,#134962,#134963,#134964,#134965,#134966,#134967,#134968,
#134969,#134970,#134971,#134972,#134973,#134974,#134975,#134976,#134977,
#134978,#134979,#134980,#134981,#134982,#134983,#134984,#134985,#134986,
#134987,#134988,#134989,#134990,#134991,#134992,#134993,#134994,#134995,
#134996,#134997,#134998,#134999,#135000,#135001,#135002,#135003,#135004,
#135005,#135006,#135007,#135008,#135009,#135010,#135011,#135012,#135013,
#135014,#135015,#135016,#135017,#135018,#135019,#135020,#135021,#135022,
#135023,#135024,#135025,#135026,#135027,#135028,#135029,#135030,#135031,
#135032,#135033,#135034,#135035,#135036,#135037,#135038,#135039,#135040,
#135041,#135042,#135043,#135044,#135045,#135046,#135047,#135048,#135049,
#135050,#135051,#135052,#135053,#135054,#135055,#135056,#135057,#135058,
#135059,#135060,#135061,#135062,#135063,#135064,#135065,#135066,#135067,
#135068,#135069,#135070,#135071,#135072,#135073,#135074,#135075,#135076,
#135077,#135078,#135079,#135080,#135081,#135082,#135083,#135084,#135085,
#135086,#135087,#135088,#135089,#135090,#135091,#135092,#135093,#135094,
#135095,#135096,#135097,#135098,#135099,#135100,#135101,#135102,#135103,
#135104,#135105,#135106,#135107,#135108,#135109,#135110,#135111,#135112,
#135113,#135114,#135115,#135116,#135117,#135118,#135119,#135120,#135121,
#135122,#135123,#135124,#135125,#135126,#135127,#135128,#135129,#135130,
#135131,#135132,#135133,#135134,#135135,#135136,#135137,#135138,#135139,
#135140,#135141,#135142,#135143,#135144,#135145,#135146,#135147,#135148,
#135149,#135150,#135151,#135152,#135153,#135154,#135155,#135156,#135157,
#135158,#135159,#135160,#135161,#135162,#135163,#135164,#135165,#135166,
#135167,#135168,#135169,#135170,#135171,#135172,#135173,#135174,#135175,
#135176,#135177,#135178,#135179,#135180,#135181,#135182,#135183,#135184,
#135185,#135186,#135187,#135188,#135189,#135190,#135191,#135192,#135193,
#135194,#135195,#135196,#135197,#135198,#135199,#135200,#135201,#135202,
#135203,#135204,#135205,#135206,#135207,#135208,#135209,#135210,#135211,
#135212,#135213,#135214,#135215,#135216,#135217,#135218,#135219,#135220,
#135221,#135222,#135223,#135224,#135225,#135226,#135227,#135228,#135229,
#135230,#135231,#135232,#135233,#135234,#135235,#135236,#135237,#135238,
#135239,#135240,#135241,#135242,#135243,#135244,#135245,#135246,#135247,
#135248,#135249,#135250,#135251,#135252,#135253,#135254,#135255,#135256,
#135257,#135258,#135259,#135260,#135261,#135262,#135263,#135264,#135265,
#135266,#135267,#135268,#135269,#135270,#135271,#135272,#135273,#135274,
#135275,#135276,#135277,#135278,#135279,#135280,#135281,#135282,#135283,
#135284,#135285,#135286,#135287,#135288,#135289,#135290,#135291,#135292,
#135293,#135294,#135295,#135296,#135297,#135298,#135299,#135300,#135301,
#135302,#135303,#135304,#135305,#135306,#135307,#135308,#135309,#135310,
#135311,#135312,#135313,#135314,#135315,#135316,#135317,#135318,#135319,
#135320,#135321,#135322,#135323,#135324,#135325,#135326,#135327,#135328,
#135329,#135330,#135331,#135332,#135333,#135334,#135335,#135336,#135337,
#135338,#135339,#135340,#135341,#135342,#135343,#135344,#135345,#135346,
#135347,#135348,#135349,#135350,#135351,#135352,#135353,#135354,#135355,
#135356,#135357,#135358,#135359,#135360,#135361,#135362,#135363,#135364,
#135365,#135366,#135367,#135368,#135369,#135370,#135371,#135372,#135373,
#135374,#135375,#135376,#135377,#135378,#135379,#135380,#135381,#135382,
#135383,#135384,#135385,#135386,#135387,#135388,#135389,#135390,#135391,
#135392,#135393,#135394,#135395,#135396,#135397,#135398,#135399,#135400,
#135401,#135402,#135403,#135404,#135405,#135406,#135407,#135408,#135409,
#135410,#135411,#135412,#135413,#135414,#135415,#135416,#135417,#135418,
#135419,#135420,#135421,#135422,#135423,#135424,#135425,#135426,#135427,
#135428,#135429,#135430,#135431,#135432,#135433,#135434,#135435,#135436,
#135437,#135438,#135439,#135440,#135441,#135442,#135443,#135444,#135445,
#135446,#135447,#135448,#135449,#135450,#135451,#135452,#135453,#135454,
#135455,#135456,#135457,#135458,#135459,#135460,#135461,#135462,#135463,
#135464,#135465,#135466,#135467,#135468,#135469,#135470,#135471,#135472,
#135473,#135474,#135475,#135476,#135477,#135478,#135479,#135480,#135481,
#135482,#135483,#135484,#135485,#135486,#135487,#135488,#135489,#135490,
#135491,#135492,#135493,#135494,#135495,#135496,#135497,#135498,#135499,
#135500,#135501,#135502,#135503,#135504,#135505,#135506,#135507,#135508,
#135509,#135510,#135511,#135512,#135513,#135514,#135515,#135516,#135517,
#135518,#135519,#135520,#135521,#135522,#135523,#135524,#135525,#135526,
#135527,#135528,#135529,#135530,#135531,#135532,#135533,#135534,#135535,
#135536,#135537,#135538,#135539,#135540,#135541,#135542,#135543,#135544,
#135545,#135546,#135547,#135548,#135549,#135550,#135551,#135552,#135553,
#135554,#135555,#135556,#135557,#135558,#135559,#135560,#135561,#135562,
#135563,#135564,#135565,#135566,#135567,#135568,#135569,#135570,#135571,
#135572,#135573,#135574,#135575,#135576,#135577,#135578,#135579,#135580,
#135581,#135582,#135583,#135584,#135585,#135586,#135587,#135588,#135589,
#135590,#135591,#135592,#135593,#135594,#135595,#135596,#135597,#135598,
#135599,#135600,#135601,#135602,#135603,#135604,#135605,#135606,#135607,
#135608,#135609,#135610,#135611,#135612,#135613,#135614,#135615,#135616,
#135617,#135618,#135619,#135620,#135621,#135622,#135623,#135624,#135625,
#135626,#135627,#135628,#135629,#135630,#135631,#135632,#135633,#135634,
#135635,#135636,#135637,#135638,#135639,#135640,#135641,#135642,#135643,
#135644,#135645,#135646,#135647,#135648,#135649,#135650,#135651,#135652,
#135653,#135654,#135655,#135656,#135657,#135658,#135659,#135660,#135661,
#135662,#135663,#135664,#135665,#135666,#135667,#135668,#135669,#135670,
#135671,#135672,#135673,#135674,#135675,#135676,#135677,#135678,#135679,
#135680,#135681,#135682,#135683,#135684,#135685,#135686,#135687,#135688,
#135689,#135690,#135691,#135692,#135693,#135694,#135695,#135696,#135697,
#135698,#135699,#135700,#135701,#135702,#135703,#135704,#135705,#135706,
#135707,#135708,#135709,#135710,#135711,#135712,#135713,#135714,#135715,
#135716,#135717,#135718,#135719,#135720,#135721,#135722,#135723,#135724,
#135725,#135726,#135727,#135728,#135729,#135730,#135731,#135732,#135733,
#135734,#135735,#135736,#135737,#135738,#135739,#135740,#135741,#135742,
#135743,#135744,#135745,#135746,#135747,#135748,#135749,#135750,#135751,
#135752,#135753,#135754,#135755,#135756,#135757,#135758,#135759,#135760,
#135761,#135762,#135763,#135764,#135765,#135766,#135767,#135768,#135769,
#135770,#135771,#135772,#135773,#135774,#135775,#135776,#135777,#135778,
#135779,#135780,#135781,#135782,#135783,#135784,#135785,#135786,#135787,
#135788,#135789,#135790,#135791,#135792,#135793,#135794,#135795,#135796,
#135797,#135798,#135799,#135800,#135801,#135802,#135803,#135804,#135805,
#135806,#135807,#135808,#135809,#135810,#135811,#135812,#135813,#135814,
#135815,#135816,#135817,#135818,#135819,#135820,#135821,#135822,#135823,
#135824,#135825,#135826,#135827,#135828,#135829,#135830,#135831,#135832,
#135833,#135834,#135835,#135836,#135837,#135838,#135839,#135840,#135841,
#135842,#135843,#135844,#135845,#135846,#135847,#135848,#135849,#135850,
#135851,#135852,#135853,#135854,#135855,#135856,#135857,#135858,#135859,
#135860,#135861,#135862,#135863,#135864,#135865,#135866,#135867,#135868,
#135869,#135870,#135871,#135872,#135873,#135874,#135875,#135876,#135877,
#135878,#135879,#135880,#135881,#135882,#135883,#135884,#135885,#135886,
#135887,#135888,#135889,#135890,#135891,#135892,#135893,#135894,#135895,
#135896,#135897,#135898,#135899,#135900,#135901,#135902,#135903,#135904,
#135905,#135906,#135907,#135908,#135909,#135910,#135911,#135912,#135913,
#135914,#135915,#135916,#135917,#135918,#135919,#135920,#135921,#135922,
#135923,#135924,#135925,#135926,#135927,#135928,#135929,#135930,#135931,
#135932,#135933,#135934,#135935,#135936,#135937,#135938,#135939,#135940,
#135941,#135942,#135943,#135944,#135945,#135946,#135947,#135948,#135949,
#135950,#135951,#135952,#135953,#135954,#135955,#135956,#135957,#135958,
#135959,#135960,#135961,#135962,#135963,#135964,#135965,#135966,#135967,
#135968,#135969,#135970,#135971,#135972,#135973,#135974,#135975,#135976,
#135977,#135978,#135979,#135980,#135981,#135982,#135983,#135984,#135985,
#135986,#135987,#135988,#135989,#135990,#135991,#135992,#135993,#135994,
#135995,#135996,#135997,#135998,#135999,#136000,#136001,#136002,#136003,
#136004,#136005,#136006,#136007,#136008,#136009,#136010,#136011,#136012,
#136013,#136014,#136015,#136016,#136017,#136018,#136019,#136020,#136021,
#136022,#136023,#136024,#136025,#136026,#136027,#136028,#136029,#136030,
#136031,#136032,#136033,#136034,#136035,#136036,#136037,#136038,#136039,
#136040,#136041,#136042,#136043,#136044,#136045,#136046,#136047,#136048,
#136049,#136050,#136051,#136052,#136053,#136054,#136055,#136056,#136057,
#136058,#136059,#136060,#136061,#136062,#136063,#136064,#136065,#136066,
#136067,#136068,#136069,#136070,#136071,#136072,#136073,#136074,#136075,
#136076,#136077,#136078,#136079,#136080,#136081,#136082,#136083,#136084,
#136085,#136086,#136087,#136088,#136089,#136090,#136091,#136092,#136093,
#136094,#136095,#136096,#136097,#136098,#136099,#136100,#136101,#136102,
#136103,#136104,#136105,#136106,#136107,#136108,#136109,#136110,#136111,
#136112,#136113,#136114,#136115,#136116,#136117,#136118,#136119,#136120,
#136121,#136122,#136123,#136124,#136125,#136126,#136127,#136128,#136129,
#136130,#136131,#136132,#136133,#136134,#136135,#136136,#136137,#136138,
#136139,#136140,#136141,#136142,#136143,#136144,#136145,#136146,#136147,
#136148,#136149,#136150,#136151,#136152,#136153,#136154,#136155,#136156,
#136157,#136158,#136159,#136160,#136161,#136162,#136163,#136164,#136165,
#136166,#136167,#136168,#136169,#136170,#136171,#136172,#136173,#136174,
#136175,#136176,#136177,#136178,#136179,#136180,#136181,#136182,#136183,
#136184,#136185,#136186,#136187,#136188,#136189,#136190,#136191,#136192,
#136193,#136194,#136195,#136196,#136197,#136198,#136199,#136200,#136201,
#136202,#136203,#136204,#136205,#136206,#136207,#136208,#136209,#136210,
#136211,#136212,#136213,#136214,#136215,#136216,#136217,#136218,#136219,
#136220,#136221,#136222,#136223,#136224,#136225,#136226,#136227,#136228,
#136229,#136230,#136231,#136232,#136233,#136234,#136235,#136236,#136237,
#136238,#136239,#136240,#136241,#136242,#136243,#136244,#136245,#136246,
#136247,#136248,#136249,#136250,#136251,#136252,#136253,#136254,#136255,
#136256,#136257,#136258,#136259,#136260,#136261,#136262,#136263,#136264,
#136265,#136266,#136267,#136268,#136269,#136270,#136271,#136272,#136273,
#136274,#136275,#136276,#136277,#136278,#136279,#136280,#136281,#136282,
#136283,#136284,#136285,#136286,#136287,#136288,#136289,#136290,#136291,
#136292,#136293,#136294,#136295,#136296,#136297,#136298,#136299,#136300,
#136301,#136302,#136303,#136304,#136305,#136306,#136307,#136308,#136309,
#136310,#136311,#136312,#136313,#136314,#136315,#136316,#136317,#136318,
#136319,#136320,#136321,#136322,#136323,#136324,#136325,#136326,#136327,
#136328,#136329,#136330,#136331,#136332,#136333,#136334,#136335,#136336,
#136337,#136338,#136339,#136340,#136341,#136342,#136343,#136344,#136345,
#136346,#136347,#136348,#136349,#136350,#136351,#136352,#136353,#136354,
#136355,#136356,#136357,#136358,#136359,#136360,#136361,#136362,#136363,
#136364,#136365,#136366,#136367,#136368,#136369,#136370,#136371,#136372,
#136373,#136374,#136375,#136376,#136377,#136378,#136379,#136380,#136381,
#136382,#136383,#136384,#136385,#136386,#136387,#136388,#136389,#136390,
#136391,#136392,#136393,#136394,#136395,#136396,#136397,#136398,#136399,
#136400,#136401,#136402,#136403,#136404,#136405,#136406,#136407,#136408,
#136409,#136410,#136411,#136412,#136413,#136414,#136415,#136416,#136417,
#136418,#136419),(#136420,#136421,#136422,#136423,#136424,#136425,#136426,
#136427,#136428,#136429,#136430,#136431,#136432,#136433,#136434,#136435,
#136436,#136437,#136438,#136439,#136440,#136441,#136442,#136443,#136444,
#136445,#136446,#136447,#136448,#136449,#136450,#136451,#136452,#136453,
#136454,#136455,#136456,#136457,#136458,#136459,#136460,#136461,#136462,
#136463,#136464,#136465,#136466,#136467,#136468,#136469,#136470,#136471,
#136472,#136473,#136474,#136475,#136476,#136477,#136478,#136479,#136480,
#136481,#136482,#136483,#136484,#136485,#136486,#136487,#136488,#136489,
#136490,#136491,#136492,#136493,#136494,#136495,#136496,#136497,#136498,
#136499,#136500,#136501,#136502,#136503,#136504,#136505,#136506,#136507,
#136508,#136509,#136510,#136511,#136512,#136513,#136514,#136515,#136516,
#136517,#136518,#136519,#136520,#136521,#136522,#136523,#136524,#136525,
#136526,#136527,#136528,#136529,#136530,#136531,#136532,#136533,#136534,
#136535,#136536,#136537,#136538,#136539,#136540,#136541,#136542,#136543,
#136544,#136545,#136546,#136547,#136548,#136549,#136550,#136551,#136552,
#136553,#136554,#136555,#136556,#136557,#136558,#136559,#136560,#136561,
#136562,#136563,#136564,#136565,#136566,#136567,#136568,#136569,#136570,
#136571,#136572,#136573,#136574,#136575,#136576,#136577,#136578,#136579,
#136580,#136581,#136582,#136583,#136584,#136585,#136586,#136587,#136588,
#136589,#136590,#136591,#136592,#136593,#136594,#136595,#136596,#136597,
#136598,#136599,#136600,#136601,#136602,#136603,#136604,#136605,#136606,
#136607,#136608,#136609,#136610,#136611,#136612,#136613,#136614,#136615,
#136616,#136617,#136618,#136619,#136620,#136621,#136622,#136623,#136624,
#136625,#136626,#136627,#136628,#136629,#136630,#136631,#136632,#136633,
#136634,#136635,#136636,#136637,#136638,#136639,#136640,#136641,#136642,
#136643,#136644,#136645,#136646,#136647,#136648,#136649,#136650,#136651,
#136652,#136653,#136654,#136655,#136656,#136657,#136658,#136659,#136660,
#136661,#136662,#136663,#136664,#136665,#136666,#136667,#136668,#136669,
#136670,#136671,#136672,#136673,#136674,#136675,#136676,#136677,#136678,
#136679,#136680,#136681,#136682,#136683,#136684,#136685,#136686,#136687,
#136688,#136689,#136690,#136691,#136692,#136693,#136694,#136695,#136696,
#136697,#136698,#136699,#136700,#136701,#136702,#136703,#136704,#136705,
#136706,#136707,#136708,#136709,#136710,#136711,#136712,#136713,#136714,
#136715,#136716,#136717,#136718,#136719,#136720,#136721,#136722,#136723,
#136724,#136725,#136726,#136727,#136728,#136729,#136730,#136731,#136732,
#136733,#136734,#136735,#136736,#136737,#136738,#136739,#136740,#136741,
#136742,#136743,#136744,#136745,#136746,#136747,#136748,#136749,#136750,
#136751,#136752,#136753,#136754,#136755,#136756,#136757,#136758,#136759,
#136760,#136761,#136762,#136763,#136764,#136765,#136766,#136767,#136768,
#136769,#136770,#136771,#136772,#136773,#136774,#136775,#136776,#136777,
#136778,#136779,#136780,#136781,#136782,#136783,#136784,#136785,#136786,
#136787,#136788,#136789,#136790,#136791,#136792,#136793,#136794,#136795,
#136796,#136797,#136798,#136799,#136800,#136801,#136802,#136803,#136804,
#136805,#136806,#136807,#136808,#136809,#136810,#136811,#136812,#136813,
#136814,#136815,#136816,#136817,#136818,#136819,#136820,#136821,#136822,
#136823,#136824,#136825,#136826,#136827,#136828,#136829,#136830,#136831,
#136832,#136833,#136834,#136835,#136836,#136837,#136838,#136839,#136840,
#136841,#136842,#136843,#136844,#136845,#136846,#136847,#136848,#136849,
#136850,#136851,#136852,#136853,#136854,#136855,#136856,#136857,#136858,
#136859,#136860,#136861,#136862,#136863,#136864,#136865,#136866,#136867,
#136868,#136869,#136870,#136871,#136872,#136873,#136874,#136875,#136876,
#136877,#136878,#136879,#136880,#136881,#136882,#136883,#136884,#136885,
#136886,#136887,#136888,#136889,#136890,#136891,#136892,#136893,#136894,
#136895,#136896,#136897,#136898,#136899,#136900,#136901,#136902,#136903,
#136904,#136905,#136906,#136907,#136908,#136909,#136910,#136911,#136912,
#136913,#136914,#136915,#136916,#136917,#136918,#136919,#136920,#136921,
#136922,#136923,#136924,#136925,#136926,#136927,#136928,#136929,#136930,
#136931,#136932,#136933,#136934,#136935,#136936,#136937,#136938,#136939,
#136940,#136941,#136942,#136943,#136944,#136945,#136946,#136947,#136948,
#136949,#136950,#136951,#136952,#136953,#136954,#136955,#136956,#136957,
#136958,#136959,#136960,#136961,#136962,#136963,#136964,#136965,#136966,
#136967,#136968,#136969,#136970,#136971,#136972,#136973,#136974,#136975,
#136976,#136977,#136978,#136979,#136980,#136981,#136982,#136983,#136984,
#136985,#136986,#136987,#136988,#136989,#136990,#136991,#136992,#136993,
#136994,#136995,#136996,#136997,#136998,#136999,#137000,#137001,#137002,
#137003,#137004,#137005,#137006,#137007,#137008,#137009,#137010,#137011,
#137012,#137013,#137014,#137015,#137016,#137017,#137018,#137019,#137020,
#137021,#137022,#137023,#137024,#137025,#137026,#137027,#137028,#137029,
#137030,#137031,#137032,#137033,#137034,#137035,#137036,#137037,#137038,
#137039,#137040,#137041,#137042,#137043,#137044,#137045,#137046,#137047,
#137048,#137049,#137050,#137051,#137052,#137053,#137054,#137055,#137056,
#137057,#137058,#137059,#137060,#137061,#137062,#137063,#137064,#137065,
#137066,#137067,#137068,#137069,#137070,#137071,#137072,#137073,#137074,
#137075,#137076,#137077,#137078,#137079,#137080,#137081,#137082,#137083,
#137084,#137085,#137086,#137087,#137088,#137089,#137090,#137091,#137092,
#137093,#137094,#137095,#137096,#137097,#137098,#137099,#137100,#137101,
#137102,#137103,#137104,#137105,#137106,#137107,#137108,#137109,#137110,
#137111,#137112,#137113,#137114,#137115,#137116,#137117,#137118,#137119,
#137120,#137121,#137122,#137123,#137124,#137125,#137126,#137127,#137128,
#137129,#137130,#137131,#137132,#137133,#137134,#137135,#137136,#137137,
#137138,#137139,#137140,#137141,#137142,#137143,#137144,#137145,#137146,
#137147,#137148,#137149,#137150,#137151,#137152,#137153,#137154,#137155,
#137156,#137157,#137158,#137159,#137160,#137161,#137162,#137163,#137164,
#137165,#137166,#137167,#137168,#137169,#137170,#137171,#137172,#137173,
#137174,#137175,#137176,#137177,#137178,#137179,#137180,#137181,#137182,
#137183,#137184,#137185,#137186,#137187,#137188,#137189,#137190,#137191,
#137192,#137193,#137194,#137195,#137196,#137197,#137198,#137199,#137200,
#137201,#137202,#137203,#137204,#137205,#137206,#137207,#137208,#137209,
#137210,#137211,#137212,#137213,#137214,#137215,#137216,#137217,#137218,
#137219,#137220,#137221,#137222,#137223,#137224,#137225,#137226,#137227,
#137228,#137229,#137230,#137231,#137232,#137233,#137234,#137235,#137236,
#137237,#137238,#137239,#137240,#137241,#137242,#137243,#137244,#137245,
#137246,#137247,#137248,#137249,#137250,#137251,#137252,#137253,#137254,
#137255,#137256,#137257,#137258,#137259,#137260,#137261,#137262,#137263,
#137264,#137265,#137266,#137267,#137268,#137269,#137270,#137271,#137272,
#137273,#137274,#137275,#137276,#137277,#137278,#137279,#137280,#137281,
#137282,#137283,#137284,#137285,#137286,#137287,#137288,#137289,#137290,
#137291,#137292,#137293,#137294,#137295,#137296,#137297,#137298,#137299,
#137300,#137301,#137302,#137303,#137304,#137305,#137306,#137307,#137308,
#137309,#137310,#137311,#137312,#137313,#137314,#137315,#137316,#137317,
#137318,#137319,#137320,#137321,#137322,#137323,#137324,#137325,#137326,
#137327,#137328,#137329,#137330,#137331,#137332,#137333,#137334,#137335,
#137336,#137337,#137338,#137339,#137340,#137341,#137342,#137343,#137344,
#137345,#137346,#137347,#137348,#137349,#137350,#137351,#137352,#137353,
#137354,#137355,#137356,#137357,#137358,#137359,#137360,#137361,#137362,
#137363,#137364,#137365,#137366,#137367,#137368,#137369,#137370,#137371,
#137372,#137373,#137374,#137375,#137376,#137377,#137378,#137379,#137380,
#137381,#137382,#137383,#137384,#137385,#137386,#137387,#137388,#137389,
#137390,#137391,#137392,#137393,#137394,#137395,#137396,#137397,#137398,
#137399,#137400,#137401,#137402,#137403,#137404,#137405,#137406,#137407,
#137408,#137409,#137410,#137411,#137412,#137413,#137414,#137415,#137416,
#137417,#137418,#137419,#137420,#137421,#137422,#137423,#137424,#137425,
#137426,#137427,#137428,#137429,#137430,#137431,#137432,#137433,#137434,
#137435,#137436,#137437,#137438,#137439,#137440,#137441,#137442,#137443,
#137444,#137445,#137446,#137447,#137448,#137449,#137450,#137451,#137452,
#137453,#137454,#137455,#137456,#137457,#137458,#137459,#137460,#137461,
#137462,#137463,#137464,#137465,#137466,#137467,#137468,#137469,#137470,
#137471,#137472,#137473,#137474,#137475,#137476,#137477,#137478,#137479,
#137480,#137481,#137482,#137483,#137484,#137485,#137486,#137487,#137488,
#137489,#137490,#137491,#137492,#137493,#137494,#137495,#137496,#137497,
#137498,#137499,#137500,#137501,#137502,#137503,#137504,#137505,#137506,
#137507,#137508,#137509,#137510,#137511,#137512,#137513,#137514,#137515,
#137516,#137517,#137518,#137519,#137520,#137521,#137522,#137523,#137524,
#137525,#137526,#137527,#137528,#137529,#137530,#137531,#137532,#137533,
#137534,#137535,#137536,#137537,#137538,#137539,#137540,#137541,#137542,
#137543,#137544,#137545,#137546,#137547,#137548,#137549,#137550,#137551,
#137552,#137553,#137554,#137555,#137556,#137557,#137558,#137559,#137560,
#137561,#137562,#137563,#137564,#137565,#137566,#137567,#137568,#137569,
#137570,#137571,#137572,#137573,#137574,#137575,#137576,#137577,#137578,
#137579,#137580,#137581,#137582,#137583,#137584,#137585,#137586,#137587,
#137588,#137589,#137590,#137591,#137592,#137593,#137594,#137595,#137596,
#137597,#137598,#137599,#137600,#137601,#137602,#137603,#137604,#137605,
#137606,#137607,#137608,#137609,#137610,#137611,#137612,#137613,#137614,
#137615,#137616,#137617,#137618,#137619,#137620,#137621,#137622,#137623,
#137624,#137625,#137626,#137627,#137628,#137629,#137630,#137631,#137632,
#137633,#137634,#137635,#137636,#137637,#137638,#137639,#137640,#137641,
#137642,#137643,#137644,#137645,#137646,#137647,#137648,#137649,#137650,
#137651,#137652,#137653,#137654,#137655,#137656,#137657,#137658,#137659,
#137660,#137661,#137662,#137663,#137664,#137665,#137666,#137667,#137668,
#137669,#137670,#137671,#137672,#137673,#137674,#137675,#137676,#137677,
#137678,#137679,#137680,#137681,#137682,#137683,#137684,#137685,#137686,
#137687,#137688,#137689,#137690,#137691,#137692,#137693,#137694,#137695,
#137696,#137697,#137698,#137699,#137700,#137701,#137702,#137703,#137704,
#137705,#137706,#137707,#137708,#137709,#137710,#137711,#137712,#137713,
#137714,#137715,#137716,#137717,#137718,#137719,#137720,#137721,#137722,
#137723,#137724,#137725,#137726,#137727,#137728,#137729,#137730,#137731,
#137732,#137733,#137734,#137735,#137736,#137737,#137738,#137739,#137740,
#137741,#137742,#137743,#137744,#137745,#137746,#137747,#137748,#137749,
#137750,#137751,#137752,#137753,#137754,#137755,#137756,#137757,#137758,
#137759,#137760,#137761,#137762,#137763,#137764,#137765,#137766,#137767,
#137768,#137769,#137770,#137771,#137772,#137773,#137774,#137775,#137776,
#137777,#137778,#137779,#137780,#137781,#137782,#137783,#137784,#137785,
#137786,#137787,#137788,#137789,#137790,#137791,#137792,#137793,#137794,
#137795,#137796,#137797,#137798,#137799,#137800,#137801,#137802,#137803,
#137804,#137805,#137806,#137807,#137808,#137809,#137810,#137811,#137812,
#137813,#137814,#137815,#137816,#137817,#137818,#137819,#137820,#137821,
#137822,#137823,#137824,#137825,#137826,#137827,#137828,#137829,#137830,
#137831,#137832,#137833,#137834,#137835,#137836,#137837,#137838,#137839,
#137840,#137841,#137842,#137843,#137844,#137845,#137846,#137847,#137848,
#137849,#137850,#137851,#137852,#137853,#137854,#137855,#137856,#137857,
#137858,#137859,#137860,#137861,#137862,#137863,#137864,#137865,#137866,
#137867,#137868,#137869,#137870,#137871,#137872,#137873,#137874,#137875,
#137876,#137877,#137878,#137879,#137880,#137881,#137882,#137883,#137884,
#137885,#137886,#137887,#137888,#137889,#137890,#137891,#137892,#137893,
#137894,#137895,#137896,#137897,#137898,#137899,#137900,#137901,#137902,
#137903,#137904,#137905,#137906,#137907,#137908,#137909,#137910,#137911,
#137912,#137913,#137914,#137915,#137916,#137917,#137918,#137919,#137920,
#137921,#137922,#137923,#137924,#137925,#137926,#137927,#137928,#137929,
#137930,#137931,#137932,#137933,#137934,#137935,#137936,#137937,#137938,
#137939,#137940,#137941,#137942,#137943,#137944,#137945,#137946,#137947,
#137948,#137949,#137950,#137951,#137952,#137953,#137954,#137955,#137956,
#137957,#137958,#137959,#137960,#137961,#137962,#137963,#137964,#137965,
#137966,#137967,#137968,#137969,#137970,#137971,#137972,#137973,#137974,
#137975,#137976,#137977,#137978,#137979,#137980,#137981,#137982,#137983,
#137984,#137985,#137986,#137987,#137988,#137989,#137990,#137991,#137992,
#137993,#137994,#137995,#137996,#137997,#137998,#137999,#138000,#138001,
#138002,#138003,#138004,#138005,#138006,#138007,#138008,#138009,#138010,
#138011,#138012,#138013,#138014,#138015,#138016,#138017,#138018,#138019,
#138020,#138021,#138022,#138023,#138024,#138025,#138026,#138027,#138028,
#138029,#138030,#138031,#138032,#138033,#138034,#138035,#138036,#138037,
#138038,#138039,#138040,#138041,#138042,#138043,#138044,#138045,#138046,
#138047,#138048,#138049,#138050,#138051,#138052,#138053,#138054,#138055,
#138056,#138057,#138058,#138059,#138060,#138061,#138062,#138063,#138064,
#138065,#138066,#138067,#138068,#138069,#138070,#138071,#138072,#138073,
#138074,#138075,#138076,#138077,#138078,#138079,#138080,#138081,#138082,
#138083,#138084,#138085,#138086,#138087,#138088,#138089,#138090,#138091,
#138092,#138093,#138094,#138095,#138096,#138097,#138098,#138099,#138100,
#138101,#138102,#138103,#138104,#138105,#138106,#138107,#138108,#138109,
#138110,#138111,#138112,#138113,#138114,#138115,#138116,#138117,#138118,
#138119,#138120,#138121,#138122,#138123,#138124,#138125,#138126,#138127,
#138128,#138129,#138130,#138131,#138132,#138133,#138134,#138135,#138136,
#138137,#138138,#138139,#138140,#138141,#138142,#138143,#138144,#138145,
#138146,#138147,#138148,#138149,#138150,#138151,#138152,#138153,#138154,
#138155,#138156,#138157,#138158,#138159,#138160,#138161,#138162,#138163,
#138164,#138165,#138166,#138167,#138168,#138169,#138170,#138171,#138172,
#138173,#138174,#138175,#138176,#138177,#138178,#138179,#138180,#138181,
#138182,#138183,#138184,#138185,#138186,#138187,#138188,#138189,#138190,
#138191,#138192,#138193,#138194,#138195,#138196,#138197,#138198,#138199,
#138200,#138201,#138202,#138203,#138204,#138205,#138206,#138207,#138208,
#138209,#138210,#138211,#138212,#138213,#138214,#138215,#138216,#138217,
#138218,#138219,#138220,#138221,#138222,#138223,#138224,#138225,#138226,
#138227,#138228,#138229,#138230,#138231,#138232,#138233,#138234,#138235,
#138236,#138237,#138238,#138239,#138240,#138241,#138242,#138243,#138244,
#138245,#138246,#138247,#138248,#138249,#138250,#138251,#138252,#138253,
#138254,#138255,#138256,#138257,#138258,#138259,#138260,#138261,#138262,
#138263,#138264,#138265,#138266,#138267,#138268,#138269,#138270,#138271,
#138272,#138273,#138274,#138275,#138276,#138277,#138278,#138279,#138280,
#138281,#138282,#138283,#138284,#138285,#138286,#138287,#138288,#138289,
#138290,#138291,#138292,#138293,#138294,#138295,#138296,#138297,#138298,
#138299,#138300,#138301,#138302,#138303,#138304,#138305,#138306,#138307,
#138308,#138309,#138310,#138311,#138312,#138313,#138314,#138315,#138316,
#138317,#138318,#138319,#138320,#138321,#138322,#138323,#138324,#138325,
#138326,#138327,#138328,#138329,#138330,#138331,#138332,#138333,#138334,
#138335,#138336,#138337,#138338,#138339,#138340,#138341,#138342,#138343,
#138344,#138345,#138346,#138347,#138348,#138349,#138350,#138351,#138352,
#138353,#138354,#138355,#138356,#138357,#138358,#138359,#138360,#138361,
#138362,#138363,#138364,#138365,#138366,#138367,#138368,#138369,#138370,
#138371,#138372,#138373,#138374,#138375,#138376,#138377,#138378,#138379,
#138380,#138381,#138382,#138383,#138384,#138385,#138386,#138387,#138388,
#138389,#138390,#138391,#138392,#138393,#138394,#138395,#138396,#138397,
#138398,#138399,#138400,#138401,#138402,#138403,#138404,#138405,#138406,
#138407,#138408,#138409,#138410,#138411,#138412,#138413,#138414,#138415,
#138416,#138417,#138418,#138419,#138420,#138421,#138422,#138423,#138424,
#138425,#138426,#138427,#138428,#138429,#138430,#138431,#138432,#138433,
#138434,#138435,#138436,#138437,#138438,#138439,#138440,#138441,#138442,
#138443,#138444,#138445,#138446,#138447,#138448,#138449,#138450,#138451,
#138452,#138453,#138454,#138455,#138456,#138457,#138458,#138459,#138460,
#138461,#138462,#138463,#138464,#138465,#138466,#138467,#138468,#138469,
#138470),(#138471,#138472,#138473,#138474,#138475,#138476,#138477,#138478,
#138479,#138480,#138481,#138482,#138483,#138484,#138485,#138486,#138487,
#138488,#138489,#138490,#138491,#138492,#138493,#138494,#138495,#138496,
#138497,#138498,#138499,#138500,#138501,#138502,#138503,#138504,#138505,
#138506,#138507,#138508,#138509,#138510,#138511,#138512,#138513,#138514,
#138515,#138516,#138517,#138518,#138519,#138520,#138521,#138522,#138523,
#138524,#138525,#138526,#138527,#138528,#138529,#138530,#138531,#138532,
#138533,#138534,#138535,#138536,#138537,#138538,#138539,#138540,#138541,
#138542,#138543,#138544,#138545,#138546,#138547,#138548,#138549,#138550,
#138551,#138552,#138553,#138554,#138555,#138556,#138557,#138558,#138559,
#138560,#138561,#138562,#138563,#138564,#138565,#138566,#138567,#138568,
#138569,#138570,#138571,#138572,#138573,#138574,#138575,#138576,#138577,
#138578,#138579,#138580,#138581,#138582,#138583,#138584,#138585,#138586,
#138587,#138588,#138589,#138590,#138591,#138592,#138593,#138594,#138595,
#138596,#138597,#138598,#138599,#138600,#138601,#138602,#138603,#138604,
#138605,#138606,#138607,#138608,#138609,#138610,#138611,#138612,#138613,
#138614,#138615,#138616,#138617,#138618,#138619,#138620,#138621,#138622,
#138623,#138624,#138625,#138626,#138627,#138628,#138629,#138630,#138631,
#138632,#138633,#138634,#138635,#138636,#138637,#138638,#138639,#138640,
#138641,#138642,#138643,#138644,#138645,#138646,#138647,#138648,#138649,
#138650,#138651,#138652,#138653,#138654,#138655,#138656,#138657,#138658,
#138659,#138660,#138661,#138662,#138663,#138664,#138665,#138666,#138667,
#138668,#138669,#138670,#138671,#138672,#138673,#138674,#138675,#138676,
#138677,#138678,#138679,#138680,#138681,#138682,#138683,#138684,#138685,
#138686,#138687,#138688,#138689,#138690,#138691,#138692,#138693,#138694,
#138695,#138696,#138697,#138698,#138699,#138700,#138701,#138702,#138703,
#138704,#138705,#138706,#138707,#138708,#138709,#138710,#138711,#138712,
#138713,#138714,#138715,#138716,#138717,#138718,#138719,#138720,#138721,
#138722,#138723,#138724,#138725,#138726,#138727,#138728,#138729,#138730,
#138731,#138732,#138733,#138734,#138735,#138736,#138737,#138738,#138739,
#138740,#138741,#138742,#138743,#138744,#138745,#138746,#138747,#138748,
#138749,#138750,#138751,#138752,#138753,#138754,#138755,#138756,#138757,
#138758,#138759,#138760,#138761,#138762,#138763,#138764,#138765,#138766,
#138767,#138768,#138769,#138770,#138771,#138772,#138773,#138774,#138775,
#138776,#138777,#138778,#138779,#138780,#138781,#138782,#138783,#138784,
#138785,#138786,#138787,#138788,#138789,#138790,#138791,#138792,#138793,
#138794,#138795,#138796,#138797,#138798,#138799,#138800,#138801,#138802,
#138803,#138804,#138805,#138806,#138807,#138808,#138809,#138810,#138811,
#138812,#138813,#138814,#138815,#138816,#138817,#138818,#138819,#138820,
#138821,#138822,#138823,#138824,#138825,#138826,#138827,#138828,#138829,
#138830,#138831,#138832,#138833,#138834,#138835,#138836,#138837,#138838,
#138839,#138840,#138841,#138842,#138843,#138844,#138845,#138846,#138847,
#138848,#138849,#138850,#138851,#138852,#138853,#138854,#138855,#138856,
#138857,#138858,#138859,#138860,#138861,#138862,#138863,#138864,#138865,
#138866,#138867,#138868,#138869,#138870,#138871,#138872,#138873,#138874,
#138875,#138876,#138877,#138878,#138879,#138880,#138881,#138882,#138883,
#138884,#138885,#138886,#138887,#138888,#138889,#138890,#138891,#138892,
#138893,#138894,#138895,#138896,#138897,#138898,#138899,#138900,#138901,
#138902,#138903,#138904,#138905,#138906,#138907,#138908,#138909,#138910,
#138911,#138912,#138913,#138914,#138915,#138916,#138917,#138918,#138919,
#138920,#138921,#138922,#138923,#138924,#138925,#138926,#138927,#138928,
#138929,#138930,#138931,#138932,#138933,#138934,#138935,#138936,#138937,
#138938,#138939,#138940,#138941,#138942,#138943,#138944,#138945,#138946,
#138947,#138948,#138949,#138950,#138951,#138952,#138953,#138954,#138955,
#138956,#138957,#138958,#138959,#138960,#138961,#138962,#138963,#138964,
#138965,#138966,#138967,#138968,#138969,#138970,#138971,#138972,#138973,
#138974,#138975,#138976,#138977,#138978,#138979,#138980,#138981,#138982,
#138983,#138984,#138985,#138986,#138987,#138988,#138989,#138990,#138991,
#138992,#138993,#138994,#138995,#138996,#138997,#138998,#138999,#139000,
#139001,#139002,#139003,#139004,#139005,#139006,#139007,#139008,#139009,
#139010,#139011,#139012,#139013,#139014,#139015,#139016,#139017,#139018,
#139019,#139020,#139021,#139022,#139023,#139024,#139025,#139026,#139027,
#139028,#139029,#139030,#139031,#139032,#139033,#139034,#139035,#139036,
#139037,#139038,#139039,#139040,#139041,#139042,#139043,#139044,#139045,
#139046,#139047,#139048,#139049,#139050,#139051,#139052,#139053,#139054,
#139055,#139056,#139057,#139058,#139059,#139060,#139061,#139062,#139063,
#139064,#139065,#139066,#139067,#139068,#139069,#139070,#139071,#139072,
#139073,#139074,#139075,#139076,#139077,#139078,#139079,#139080,#139081,
#139082,#139083,#139084,#139085,#139086,#139087,#139088,#139089,#139090,
#139091,#139092,#139093,#139094,#139095,#139096,#139097,#139098,#139099,
#139100,#139101,#139102,#139103,#139104,#139105,#139106,#139107,#139108,
#139109,#139110,#139111,#139112,#139113,#139114,#139115,#139116,#139117,
#139118,#139119,#139120,#139121,#139122,#139123,#139124,#139125,#139126,
#139127,#139128,#139129,#139130,#139131,#139132,#139133,#139134,#139135,
#139136,#139137,#139138,#139139,#139140,#139141,#139142,#139143,#139144,
#139145,#139146,#139147,#139148,#139149,#139150,#139151,#139152,#139153,
#139154,#139155,#139156,#139157,#139158,#139159,#139160,#139161,#139162,
#139163,#139164,#139165,#139166,#139167,#139168,#139169,#139170,#139171,
#139172,#139173,#139174,#139175,#139176,#139177,#139178,#139179,#139180,
#139181,#139182,#139183,#139184,#139185,#139186,#139187,#139188,#139189,
#139190,#139191,#139192,#139193,#139194,#139195,#139196,#139197,#139198,
#139199,#139200,#139201,#139202,#139203,#139204,#139205,#139206,#139207,
#139208,#139209,#139210,#139211,#139212,#139213,#139214,#139215,#139216,
#139217,#139218,#139219,#139220,#139221,#139222,#139223,#139224,#139225,
#139226,#139227,#139228,#139229,#139230,#139231,#139232,#139233,#139234,
#139235,#139236,#139237,#139238,#139239,#139240,#139241,#139242,#139243,
#139244,#139245,#139246,#139247,#139248,#139249,#139250,#139251,#139252,
#139253,#139254,#139255,#139256,#139257,#139258,#139259,#139260,#139261,
#139262,#139263,#139264,#139265,#139266,#139267,#139268,#139269,#139270,
#139271,#139272,#139273,#139274,#139275,#139276,#139277,#139278,#139279,
#139280,#139281,#139282,#139283,#139284,#139285,#139286,#139287,#139288,
#139289,#139290,#139291,#139292,#139293,#139294,#139295,#139296,#139297,
#139298,#139299,#139300,#139301,#139302,#139303,#139304,#139305,#139306,
#139307,#139308,#139309,#139310,#139311,#139312,#139313,#139314,#139315,
#139316,#139317,#139318,#139319,#139320,#139321,#139322,#139323,#139324,
#139325,#139326,#139327,#139328,#139329,#139330,#139331,#139332,#139333,
#139334,#139335,#139336,#139337,#139338,#139339,#139340,#139341,#139342,
#139343,#139344,#139345,#139346,#139347,#139348,#139349,#139350,#139351,
#139352,#139353,#139354,#139355,#139356,#139357,#139358,#139359,#139360,
#139361,#139362,#139363,#139364,#139365,#139366,#139367,#139368,#139369,
#139370,#139371,#139372,#139373,#139374,#139375,#139376,#139377,#139378,
#139379,#139380,#139381,#139382,#139383,#139384,#139385,#139386,#139387,
#139388,#139389,#139390,#139391,#139392,#139393,#139394,#139395,#139396,
#139397,#139398,#139399,#139400,#139401,#139402,#139403,#139404,#139405,
#139406,#139407,#139408,#139409,#139410,#139411,#139412,#139413,#139414,
#139415,#139416,#139417,#139418,#139419,#139420,#139421,#139422,#139423,
#139424,#139425,#139426,#139427,#139428,#139429,#139430,#139431,#139432,
#139433,#139434,#139435,#139436,#139437,#139438,#139439,#139440,#139441,
#139442,#139443,#139444,#139445,#139446,#139447,#139448,#139449,#139450,
#139451,#139452,#139453,#139454,#139455,#139456,#139457,#139458,#139459,
#139460,#139461,#139462,#139463,#139464,#139465,#139466,#139467,#139468,
#139469,#139470,#139471,#139472,#139473,#139474,#139475,#139476,#139477,
#139478,#139479,#139480,#139481,#139482,#139483,#139484,#139485,#139486,
#139487,#139488,#139489,#139490,#139491,#139492,#139493,#139494,#139495,
#139496,#139497,#139498,#139499,#139500,#139501,#139502,#139503,#139504,
#139505,#139506,#139507,#139508,#139509,#139510,#139511,#139512,#139513,
#139514,#139515,#139516,#139517,#139518,#139519,#139520,#139521,#139522,
#139523,#139524,#139525,#139526,#139527,#139528,#139529,#139530,#139531,
#139532,#139533,#139534,#139535,#139536,#139537,#139538,#139539,#139540,
#139541,#139542,#139543,#139544,#139545,#139546,#139547,#139548,#139549,
#139550,#139551,#139552,#139553,#139554,#139555,#139556,#139557,#139558,
#139559,#139560,#139561,#139562,#139563,#139564,#139565,#139566,#139567,
#139568,#139569,#139570,#139571,#139572,#139573,#139574,#139575,#139576,
#139577,#139578,#139579,#139580,#139581,#139582,#139583,#139584,#139585,
#139586,#139587,#139588,#139589,#139590,#139591,#139592,#139593,#139594,
#139595,#139596,#139597,#139598,#139599,#139600,#139601,#139602,#139603,
#139604,#139605,#139606,#139607,#139608,#139609,#139610,#139611,#139612,
#139613,#139614,#139615,#139616,#139617,#139618,#139619,#139620,#139621,
#139622,#139623,#139624,#139625,#139626,#139627,#139628,#139629,#139630,
#139631,#139632,#139633,#139634,#139635,#139636,#139637,#139638,#139639,
#139640,#139641,#139642,#139643,#139644,#139645,#139646,#139647,#139648,
#139649,#139650,#139651,#139652,#139653,#139654,#139655,#139656,#139657,
#139658,#139659,#139660,#139661,#139662,#139663,#139664,#139665,#139666,
#139667,#139668,#139669,#139670,#139671,#139672,#139673,#139674,#139675,
#139676,#139677,#139678,#139679,#139680,#139681,#139682,#139683,#139684,
#139685,#139686,#139687,#139688,#139689,#139690,#139691,#139692,#139693,
#139694,#139695,#139696,#139697,#139698,#139699,#139700,#139701,#139702,
#139703,#139704,#139705,#139706,#139707,#139708,#139709,#139710,#139711,
#139712,#139713,#139714,#139715,#139716,#139717,#139718,#139719,#139720,
#139721,#139722,#139723,#139724,#139725,#139726,#139727,#139728,#139729,
#139730,#139731,#139732,#139733,#139734,#139735,#139736,#139737,#139738,
#139739,#139740,#139741,#139742,#139743,#139744,#139745,#139746,#139747,
#139748,#139749,#139750,#139751,#139752,#139753,#139754,#139755,#139756,
#139757,#139758,#139759,#139760,#139761,#139762,#139763,#139764,#139765,
#139766,#139767,#139768,#139769,#139770,#139771,#139772,#139773,#139774,
#139775,#139776,#139777,#139778,#139779,#139780,#139781,#139782,#139783,
#139784,#139785,#139786,#139787,#139788,#139789,#139790,#139791,#139792,
#139793,#139794,#139795,#139796,#139797,#139798,#139799,#139800,#139801,
#139802,#139803,#139804,#139805,#139806,#139807,#139808,#139809,#139810,
#139811,#139812,#139813,#139814,#139815,#139816,#139817,#139818,#139819,
#139820,#139821,#139822,#139823,#139824,#139825,#139826,#139827,#139828,
#139829,#139830,#139831,#139832,#139833,#139834,#139835,#139836,#139837,
#139838,#139839,#139840,#139841,#139842,#139843,#139844,#139845,#139846,
#139847,#139848,#139849,#139850,#139851,#139852,#139853,#139854,#139855,
#139856,#139857,#139858,#139859,#139860,#139861,#139862,#139863,#139864,
#139865,#139866,#139867,#139868,#139869,#139870,#139871,#139872,#139873,
#139874,#139875,#139876,#139877,#139878,#139879,#139880,#139881,#139882,
#139883,#139884,#139885,#139886,#139887,#139888,#139889,#139890,#139891,
#139892,#139893,#139894,#139895,#139896,#139897,#139898,#139899,#139900,
#139901,#139902,#139903,#139904,#139905,#139906,#139907,#139908,#139909,
#139910,#139911,#139912,#139913,#139914,#139915,#139916,#139917,#139918,
#139919,#139920,#139921,#139922,#139923,#139924,#139925,#139926,#139927,
#139928,#139929,#139930,#139931,#139932,#139933,#139934,#139935,#139936,
#139937,#139938,#139939,#139940,#139941,#139942,#139943,#139944,#139945,
#139946,#139947,#139948,#139949,#139950,#139951,#139952,#139953,#139954,
#139955,#139956,#139957,#139958,#139959,#139960,#139961,#139962,#139963,
#139964,#139965,#139966,#139967,#139968,#139969,#139970,#139971,#139972,
#139973,#139974,#139975,#139976,#139977,#139978,#139979,#139980,#139981,
#139982,#139983,#139984,#139985,#139986,#139987,#139988,#139989,#139990,
#139991,#139992,#139993,#139994,#139995,#139996,#139997,#139998,#139999,
#140000,#140001,#140002,#140003,#140004,#140005,#140006,#140007,#140008,
#140009,#140010,#140011,#140012,#140013,#140014,#140015,#140016,#140017,
#140018,#140019,#140020,#140021,#140022,#140023,#140024,#140025,#140026,
#140027,#140028,#140029,#140030,#140031,#140032,#140033,#140034,#140035,
#140036,#140037,#140038,#140039,#140040,#140041,#140042,#140043,#140044,
#140045,#140046,#140047,#140048,#140049,#140050,#140051,#140052,#140053,
#140054,#140055,#140056,#140057,#140058,#140059,#140060,#140061,#140062,
#140063,#140064,#140065,#140066,#140067,#140068,#140069,#140070,#140071,
#140072,#140073,#140074,#140075,#140076,#140077,#140078,#140079,#140080,
#140081,#140082,#140083,#140084,#140085,#140086,#140087,#140088,#140089,
#140090,#140091,#140092,#140093,#140094,#140095,#140096,#140097,#140098,
#140099,#140100,#140101,#140102,#140103,#140104,#140105,#140106,#140107,
#140108,#140109,#140110,#140111,#140112,#140113,#140114,#140115,#140116,
#140117,#140118,#140119,#140120,#140121,#140122,#140123,#140124,#140125,
#140126,#140127,#140128,#140129,#140130,#140131,#140132,#140133,#140134,
#140135,#140136,#140137,#140138,#140139,#140140,#140141,#140142,#140143,
#140144,#140145,#140146,#140147,#140148,#140149,#140150,#140151,#140152,
#140153,#140154,#140155,#140156,#140157,#140158,#140159,#140160,#140161,
#140162,#140163,#140164,#140165,#140166,#140167,#140168,#140169,#140170,
#140171,#140172,#140173,#140174,#140175,#140176,#140177,#140178,#140179,
#140180,#140181,#140182,#140183,#140184,#140185,#140186,#140187,#140188,
#140189,#140190,#140191,#140192,#140193,#140194,#140195,#140196,#140197,
#140198,#140199,#140200,#140201,#140202,#140203,#140204,#140205,#140206,
#140207,#140208,#140209,#140210,#140211,#140212,#140213,#140214,#140215,
#140216,#140217,#140218,#140219,#140220,#140221,#140222,#140223,#140224,
#140225,#140226,#140227,#140228,#140229,#140230,#140231,#140232,#140233,
#140234,#140235,#140236,#140237,#140238,#140239,#140240,#140241,#140242,
#140243,#140244,#140245,#140246,#140247,#140248,#140249,#140250,#140251,
#140252,#140253,#140254,#140255,#140256,#140257,#140258,#140259,#140260,
#140261,#140262,#140263,#140264,#140265,#140266,#140267,#140268,#140269,
#140270,#140271,#140272,#140273,#140274,#140275,#140276,#140277,#140278,
#140279,#140280,#140281,#140282,#140283,#140284,#140285,#140286,#140287,
#140288,#140289,#140290,#140291,#140292,#140293,#140294,#140295,#140296,
#140297,#140298,#140299,#140300,#140301,#140302,#140303,#140304,#140305,
#140306,#140307,#140308,#140309,#140310,#140311,#140312,#140313,#140314,
#140315,#140316,#140317,#140318,#140319,#140320,#140321,#140322,#140323,
#140324,#140325,#140326,#140327,#140328,#140329,#140330,#140331,#140332,
#140333,#140334,#140335,#140336,#140337,#140338,#140339,#140340,#140341,
#140342,#140343,#140344,#140345,#140346,#140347,#140348,#140349,#140350,
#140351,#140352,#140353,#140354,#140355,#140356,#140357,#140358,#140359,
#140360,#140361,#140362,#140363,#140364,#140365,#140366,#140367,#140368,
#140369,#140370,#140371,#140372,#140373,#140374,#140375,#140376,#140377,
#140378,#140379,#140380,#140381,#140382,#140383,#140384,#140385,#140386,
#140387,#140388,#140389,#140390,#140391,#140392,#140393,#140394,#140395,
#140396,#140397,#140398,#140399,#140400,#140401,#140402,#140403,#140404,
#140405,#140406,#140407,#140408,#140409,#140410,#140411,#140412,#140413,
#140414,#140415,#140416,#140417,#140418,#140419,#140420,#140421,#140422,
#140423,#140424,#140425,#140426,#140427,#140428,#140429,#140430,#140431,
#140432,#140433,#140434,#140435,#140436,#140437,#140438,#140439,#140440,
#140441,#140442,#140443,#140444,#140445,#140446,#140447,#140448,#140449,
#140450,#140451,#140452,#140453,#140454,#140455,#140456,#140457,#140458,
#140459,#140460,#140461,#140462,#140463,#140464,#140465,#140466,#140467,
#140468,#140469,#140470,#140471,#140472,#140473,#140474,#140475,#140476,
#140477,#140478,#140479,#140480,#140481,#140482,#140483,#140484,#140485,
#140486,#140487,#140488,#140489,#140490,#140491,#140492,#140493,#140494,
#140495,#140496,#140497,#140498,#140499,#140500,#140501,#140502,#140503,
#140504,#140505,#140506,#140507,#140508,#140509,#140510,#140511,#140512,
#140513,#140514,#140515,#140516,#140517,#140518,#140519,#140520,#140521),
(#140522,#140523,#140524,#140525,#140526,#140527,#140528,#140529,#140530,
#140531,#140532,#140533,#140534,#140535,#140536,#140537,#140538,#140539,
#140540,#140541,#140542,#140543,#140544,#140545,#140546,#140547,#140548,
#140549,#140550,#140551,#140552,#140553,#140554,#140555,#140556,#140557,
#140558,#140559,#140560,#140561,#140562,#140563,#140564,#140565,#140566,
#140567,#140568,#140569,#140570,#140571,#140572,#140573,#140574,#140575,
#140576,#140577,#140578,#140579,#140580,#140581,#140582,#140583,#140584,
#140585,#140586,#140587,#140588,#140589,#140590,#140591,#140592,#140593,
#140594,#140595,#140596,#140597,#140598,#140599,#140600,#140601,#140602,
#140603,#140604,#140605,#140606,#140607,#140608,#140609,#140610,#140611,
#140612,#140613,#140614,#140615,#140616,#140617,#140618,#140619,#140620,
#140621,#140622,#140623,#140624,#140625,#140626,#140627,#140628,#140629,
#140630,#140631,#140632,#140633,#140634,#140635,#140636,#140637,#140638,
#140639,#140640,#140641,#140642,#140643,#140644,#140645,#140646,#140647,
#140648,#140649,#140650,#140651,#140652,#140653,#140654,#140655,#140656,
#140657,#140658,#140659,#140660,#140661,#140662,#140663,#140664,#140665,
#140666,#140667,#140668,#140669,#140670,#140671,#140672,#140673,#140674,
#140675,#140676,#140677,#140678,#140679,#140680,#140681,#140682,#140683,
#140684,#140685,#140686,#140687,#140688,#140689,#140690,#140691,#140692,
#140693,#140694,#140695,#140696,#140697,#140698,#140699,#140700,#140701,
#140702,#140703,#140704,#140705,#140706,#140707,#140708,#140709,#140710,
#140711,#140712,#140713,#140714,#140715,#140716,#140717,#140718,#140719,
#140720,#140721,#140722,#140723,#140724,#140725,#140726,#140727,#140728,
#140729,#140730,#140731,#140732,#140733,#140734,#140735,#140736,#140737,
#140738,#140739,#140740,#140741,#140742,#140743,#140744,#140745,#140746,
#140747,#140748,#140749,#140750,#140751,#140752,#140753,#140754,#140755,
#140756,#140757,#140758,#140759,#140760,#140761,#140762,#140763,#140764,
#140765,#140766,#140767,#140768,#140769,#140770,#140771,#140772,#140773,
#140774,#140775,#140776,#140777,#140778,#140779,#140780,#140781,#140782,
#140783,#140784,#140785,#140786,#140787,#140788,#140789,#140790,#140791,
#140792,#140793,#140794,#140795,#140796,#140797,#140798,#140799,#140800,
#140801,#140802,#140803,#140804,#140805,#140806,#140807,#140808,#140809,
#140810,#140811,#140812,#140813,#140814,#140815,#140816,#140817,#140818,
#140819,#140820,#140821,#140822,#140823,#140824,#140825,#140826,#140827,
#140828,#140829,#140830,#140831,#140832,#140833,#140834,#140835,#140836,
#140837,#140838,#140839,#140840,#140841,#140842,#140843,#140844,#140845,
#140846,#140847,#140848,#140849,#140850,#140851,#140852,#140853,#140854,
#140855,#140856,#140857,#140858,#140859,#140860,#140861,#140862,#140863,
#140864,#140865,#140866,#140867,#140868,#140869,#140870,#140871,#140872,
#140873,#140874,#140875,#140876,#140877,#140878,#140879,#140880,#140881,
#140882,#140883,#140884,#140885,#140886,#140887,#140888,#140889,#140890,
#140891,#140892,#140893,#140894,#140895,#140896,#140897,#140898,#140899,
#140900,#140901,#140902,#140903,#140904,#140905,#140906,#140907,#140908,
#140909,#140910,#140911,#140912,#140913,#140914,#140915,#140916,#140917,
#140918,#140919,#140920,#140921,#140922,#140923,#140924,#140925,#140926,
#140927,#140928,#140929,#140930,#140931,#140932,#140933,#140934,#140935,
#140936,#140937,#140938,#140939,#140940,#140941,#140942,#140943,#140944,
#140945,#140946,#140947,#140948,#140949,#140950,#140951,#140952,#140953,
#140954,#140955,#140956,#140957,#140958,#140959,#140960,#140961,#140962,
#140963,#140964,#140965,#140966,#140967,#140968,#140969,#140970,#140971,
#140972,#140973,#140974,#140975,#140976,#140977,#140978,#140979,#140980,
#140981,#140982,#140983,#140984,#140985,#140986,#140987,#140988,#140989,
#140990,#140991,#140992,#140993,#140994,#140995,#140996,#140997,#140998,
#140999,#141000,#141001,#141002,#141003,#141004,#141005,#141006,#141007,
#141008,#141009,#141010,#141011,#141012,#141013,#141014,#141015,#141016,
#141017,#141018,#141019,#141020,#141021,#141022,#141023,#141024,#141025,
#141026,#141027,#141028,#141029,#141030,#141031,#141032,#141033,#141034,
#141035,#141036,#141037,#141038,#141039,#141040,#141041,#141042,#141043,
#141044,#141045,#141046,#141047,#141048,#141049,#141050,#141051,#141052,
#141053,#141054,#141055,#141056,#141057,#141058,#141059,#141060,#141061,
#141062,#141063,#141064,#141065,#141066,#141067,#141068,#141069,#141070,
#141071,#141072,#141073,#141074,#141075,#141076,#141077,#141078,#141079,
#141080,#141081,#141082,#141083,#141084,#141085,#141086,#141087,#141088,
#141089,#141090,#141091,#141092,#141093,#141094,#141095,#141096,#141097,
#141098,#141099,#141100,#141101,#141102,#141103,#141104,#141105,#141106,
#141107,#141108,#141109,#141110,#141111,#141112,#141113,#141114,#141115,
#141116,#141117,#141118,#141119,#141120,#141121,#141122,#141123,#141124,
#141125,#141126,#141127,#141128,#141129,#141130,#141131,#141132,#141133,
#141134,#141135,#141136,#141137,#141138,#141139,#141140,#141141,#141142,
#141143,#141144,#141145,#141146,#141147,#141148,#141149,#141150,#141151,
#141152,#141153,#141154,#141155,#141156,#141157,#141158,#141159,#141160,
#141161,#141162,#141163,#141164,#141165,#141166,#141167,#141168,#141169,
#141170,#141171,#141172,#141173,#141174,#141175,#141176,#141177,#141178,
#141179,#141180,#141181,#141182,#141183,#141184,#141185,#141186,#141187,
#141188,#141189,#141190,#141191,#141192,#141193,#141194,#141195,#141196,
#141197,#141198,#141199,#141200,#141201,#141202,#141203,#141204,#141205,
#141206,#141207,#141208,#141209,#141210,#141211,#141212,#141213,#141214,
#141215,#141216,#141217,#141218,#141219,#141220,#141221,#141222,#141223,
#141224,#141225,#141226,#141227,#141228,#141229,#141230,#141231,#141232,
#141233,#141234,#141235,#141236,#141237,#141238,#141239,#141240,#141241,
#141242,#141243,#141244,#141245,#141246,#141247,#141248,#141249,#141250,
#141251,#141252,#141253,#141254,#141255,#141256,#141257,#141258,#141259,
#141260,#141261,#141262,#141263,#141264,#141265,#141266,#141267,#141268,
#141269,#141270,#141271,#141272,#141273,#141274,#141275,#141276,#141277,
#141278,#141279,#141280,#141281,#141282,#141283,#141284,#141285,#141286,
#141287,#141288,#141289,#141290,#141291,#141292,#141293,#141294,#141295,
#141296,#141297,#141298,#141299,#141300,#141301,#141302,#141303,#141304,
#141305,#141306,#141307,#141308,#141309,#141310,#141311,#141312,#141313,
#141314,#141315,#141316,#141317,#141318,#141319,#141320,#141321,#141322,
#141323,#141324,#141325,#141326,#141327,#141328,#141329,#141330,#141331,
#141332,#141333,#141334,#141335,#141336,#141337,#141338,#141339,#141340,
#141341,#141342,#141343,#141344,#141345,#141346,#141347,#141348,#141349,
#141350,#141351,#141352,#141353,#141354,#141355,#141356,#141357,#141358,
#141359,#141360,#141361,#141362,#141363,#141364,#141365,#141366,#141367,
#141368,#141369,#141370,#141371,#141372,#141373,#141374,#141375,#141376,
#141377,#141378,#141379,#141380,#141381,#141382,#141383,#141384,#141385,
#141386,#141387,#141388,#141389,#141390,#141391,#141392,#141393,#141394,
#141395,#141396,#141397,#141398,#141399,#141400,#141401,#141402,#141403,
#141404,#141405,#141406,#141407,#141408,#141409,#141410,#141411,#141412,
#141413,#141414,#141415,#141416,#141417,#141418,#141419,#141420,#141421,
#141422,#141423,#141424,#141425,#141426,#141427,#141428,#141429,#141430,
#141431,#141432,#141433,#141434,#141435,#141436,#141437,#141438,#141439,
#141440,#141441,#141442,#141443,#141444,#141445,#141446,#141447,#141448,
#141449,#141450,#141451,#141452,#141453,#141454,#141455,#141456,#141457,
#141458,#141459,#141460,#141461,#141462,#141463,#141464,#141465,#141466,
#141467,#141468,#141469,#141470,#141471,#141472,#141473,#141474,#141475,
#141476,#141477,#141478,#141479,#141480,#141481,#141482,#141483,#141484,
#141485,#141486,#141487,#141488,#141489,#141490,#141491,#141492,#141493,
#141494,#141495,#141496,#141497,#141498,#141499,#141500,#141501,#141502,
#141503,#141504,#141505,#141506,#141507,#141508,#141509,#141510,#141511,
#141512,#141513,#141514,#141515,#141516,#141517,#141518,#141519,#141520,
#141521,#141522,#141523,#141524,#141525,#141526,#141527,#141528,#141529,
#141530,#141531,#141532,#141533,#141534,#141535,#141536,#141537,#141538,
#141539,#141540,#141541,#141542,#141543,#141544,#141545,#141546,#141547,
#141548,#141549,#141550,#141551,#141552,#141553,#141554,#141555,#141556,
#141557,#141558,#141559,#141560,#141561,#141562,#141563,#141564,#141565,
#141566,#141567,#141568,#141569,#141570,#141571,#141572,#141573,#141574,
#141575,#141576,#141577,#141578,#141579,#141580,#141581,#141582,#141583,
#141584,#141585,#141586,#141587,#141588,#141589,#141590,#141591,#141592,
#141593,#141594,#141595,#141596,#141597,#141598,#141599,#141600,#141601,
#141602,#141603,#141604,#141605,#141606,#141607,#141608,#141609,#141610,
#141611,#141612,#141613,#141614,#141615,#141616,#141617,#141618,#141619,
#141620,#141621,#141622,#141623,#141624,#141625,#141626,#141627,#141628,
#141629,#141630,#141631,#141632,#141633,#141634,#141635,#141636,#141637,
#141638,#141639,#141640,#141641,#141642,#141643,#141644,#141645,#141646,
#141647,#141648,#141649,#141650,#141651,#141652,#141653,#141654,#141655,
#141656,#141657,#141658,#141659,#141660,#141661,#141662,#141663,#141664,
#141665,#141666,#141667,#141668,#141669,#141670,#141671,#141672,#141673,
#141674,#141675,#141676,#141677,#141678,#141679,#141680,#141681,#141682,
#141683,#141684,#141685,#141686,#141687,#141688,#141689,#141690,#141691,
#141692,#141693,#141694,#141695,#141696,#141697,#141698,#141699,#141700,
#141701,#141702,#141703,#141704,#141705,#141706,#141707,#141708,#141709,
#141710,#141711,#141712,#141713,#141714,#141715,#141716,#141717,#141718,
#141719,#141720,#141721,#141722,#141723,#141724,#141725,#141726,#141727,
#141728,#141729,#141730,#141731,#141732,#141733,#141734,#141735,#141736,
#141737,#141738,#141739,#141740,#141741,#141742,#141743,#141744,#141745,
#141746,#141747,#141748,#141749,#141750,#141751,#141752,#141753,#141754,
#141755,#141756,#141757,#141758,#141759,#141760,#141761,#141762,#141763,
#141764,#141765,#141766,#141767,#141768,#141769,#141770,#141771,#141772,
#141773,#141774,#141775,#141776,#141777,#141778,#141779,#141780,#141781,
#141782,#141783,#141784,#141785,#141786,#141787,#141788,#141789,#141790,
#141791,#141792,#141793,#141794,#141795,#141796,#141797,#141798,#141799,
#141800,#141801,#141802,#141803,#141804,#141805,#141806,#141807,#141808,
#141809,#141810,#141811,#141812,#141813,#141814,#141815,#141816,#141817,
#141818,#141819,#141820,#141821,#141822,#141823,#141824,#141825,#141826,
#141827,#141828,#141829,#141830,#141831,#141832,#141833,#141834,#141835,
#141836,#141837,#141838,#141839,#141840,#141841,#141842,#141843,#141844,
#141845,#141846,#141847,#141848,#141849,#141850,#141851,#141852,#141853,
#141854,#141855,#141856,#141857,#141858,#141859,#141860,#141861,#141862,
#141863,#141864,#141865,#141866,#141867,#141868,#141869,#141870,#141871,
#141872,#141873,#141874,#141875,#141876,#141877,#141878,#141879,#141880,
#141881,#141882,#141883,#141884,#141885,#141886,#141887,#141888,#141889,
#141890,#141891,#141892,#141893,#141894,#141895,#141896,#141897,#141898,
#141899,#141900,#141901,#141902,#141903,#141904,#141905,#141906,#141907,
#141908,#141909,#141910,#141911,#141912,#141913,#141914,#141915,#141916,
#141917,#141918,#141919,#141920,#141921,#141922,#141923,#141924,#141925,
#141926,#141927,#141928,#141929,#141930,#141931,#141932,#141933,#141934,
#141935,#141936,#141937,#141938,#141939,#141940,#141941,#141942,#141943,
#141944,#141945,#141946,#141947,#141948,#141949,#141950,#141951,#141952,
#141953,#141954,#141955,#141956,#141957,#141958,#141959,#141960,#141961,
#141962,#141963,#141964,#141965,#141966,#141967,#141968,#141969,#141970,
#141971,#141972,#141973,#141974,#141975,#141976,#141977,#141978,#141979,
#141980,#141981,#141982,#141983,#141984,#141985,#141986,#141987,#141988,
#141989,#141990,#141991,#141992,#141993,#141994,#141995,#141996,#141997,
#141998,#141999,#142000,#142001,#142002,#142003,#142004,#142005,#142006,
#142007,#142008,#142009,#142010,#142011,#142012,#142013,#142014,#142015,
#142016,#142017,#142018,#142019,#142020,#142021,#142022,#142023,#142024,
#142025,#142026,#142027,#142028,#142029,#142030,#142031,#142032,#142033,
#142034,#142035,#142036,#142037,#142038,#142039,#142040,#142041,#142042,
#142043,#142044,#142045,#142046,#142047,#142048,#142049,#142050,#142051,
#142052,#142053,#142054,#142055,#142056,#142057,#142058,#142059,#142060,
#142061,#142062,#142063,#142064,#142065,#142066,#142067,#142068,#142069,
#142070,#142071,#142072,#142073,#142074,#142075,#142076,#142077,#142078,
#142079,#142080,#142081,#142082,#142083,#142084,#142085,#142086,#142087,
#142088,#142089,#142090,#142091,#142092,#142093,#142094,#142095,#142096,
#142097,#142098,#142099,#142100,#142101,#142102,#142103,#142104,#142105,
#142106,#142107,#142108,#142109,#142110,#142111,#142112,#142113,#142114,
#142115,#142116,#142117,#142118,#142119,#142120,#142121,#142122,#142123,
#142124,#142125,#142126,#142127,#142128,#142129,#142130,#142131,#142132,
#142133,#142134,#142135,#142136,#142137,#142138,#142139,#142140,#142141,
#142142,#142143,#142144,#142145,#142146,#142147,#142148,#142149,#142150,
#142151,#142152,#142153,#142154,#142155,#142156,#142157,#142158,#142159,
#142160,#142161,#142162,#142163,#142164,#142165,#142166,#142167,#142168,
#142169,#142170,#142171,#142172,#142173,#142174,#142175,#142176,#142177,
#142178,#142179,#142180,#142181,#142182,#142183,#142184,#142185,#142186,
#142187,#142188,#142189,#142190,#142191,#142192,#142193,#142194,#142195,
#142196,#142197,#142198,#142199,#142200,#142201,#142202,#142203,#142204,
#142205,#142206,#142207,#142208,#142209,#142210,#142211,#142212,#142213,
#142214,#142215,#142216,#142217,#142218,#142219,#142220,#142221,#142222,
#142223,#142224,#142225,#142226,#142227,#142228,#142229,#142230,#142231,
#142232,#142233,#142234,#142235,#142236,#142237,#142238,#142239,#142240,
#142241,#142242,#142243,#142244,#142245,#142246,#142247,#142248,#142249,
#142250,#142251,#142252,#142253,#142254,#142255,#142256,#142257,#142258,
#142259,#142260,#142261,#142262,#142263,#142264,#142265,#142266,#142267,
#142268,#142269,#142270,#142271,#142272,#142273,#142274,#142275,#142276,
#142277,#142278,#142279,#142280,#142281,#142282,#142283,#142284,#142285,
#142286,#142287,#142288,#142289,#142290,#142291,#142292,#142293,#142294,
#142295,#142296,#142297,#142298,#142299,#142300,#142301,#142302,#142303,
#142304,#142305,#142306,#142307,#142308,#142309,#142310,#142311,#142312,
#142313,#142314,#142315,#142316,#142317,#142318,#142319,#142320,#142321,
#142322,#142323,#142324,#142325,#142326,#142327,#142328,#142329,#142330,
#142331,#142332,#142333,#142334,#142335,#142336,#142337,#142338,#142339,
#142340,#142341,#142342,#142343,#142344,#142345,#142346,#142347,#142348,
#142349,#142350,#142351,#142352,#142353,#142354,#142355,#142356,#142357,
#142358,#142359,#142360,#142361,#142362,#142363,#142364,#142365,#142366,
#142367,#142368,#142369,#142370,#142371,#142372,#142373,#142374,#142375,
#142376,#142377,#142378,#142379,#142380,#142381,#142382,#142383,#142384,
#142385,#142386,#142387,#142388,#142389,#142390,#142391,#142392,#142393,
#142394,#142395,#142396,#142397,#142398,#142399,#142400,#142401,#142402,
#142403,#142404,#142405,#142406,#142407,#142408,#142409,#142410,#142411,
#142412,#142413,#142414,#142415,#142416,#142417,#142418,#142419,#142420,
#142421,#142422,#142423,#142424,#142425,#142426,#142427,#142428,#142429,
#142430,#142431,#142432,#142433,#142434,#142435,#142436,#142437,#142438,
#142439,#142440,#142441,#142442,#142443,#142444,#142445,#142446,#142447,
#142448,#142449,#142450,#142451,#142452,#142453,#142454,#142455,#142456,
#142457,#142458,#142459,#142460,#142461,#142462,#142463,#142464,#142465,
#142466,#142467,#142468,#142469,#142470,#142471,#142472,#142473,#142474,
#142475,#142476,#142477,#142478,#142479,#142480,#142481,#142482,#142483,
#142484,#142485,#142486,#142487,#142488,#142489,#142490,#142491,#142492,
#142493,#142494,#142495,#142496,#142497,#142498,#142499,#142500,#142501,
#142502,#142503,#142504,#142505,#142506,#142507,#142508,#142509,#142510,
#142511,#142512,#142513,#142514,#142515,#142516,#142517,#142518,#142519,
#142520,#142521,#142522,#142523,#142524,#142525,#142526,#142527,#142528,
#142529,#142530,#142531,#142532,#142533,#142534,#142535,#142536,#142537,
#142538,#142539,#142540,#142541,#142542,#142543,#142544,#142545,#142546,
#142547,#142548,#142549,#142550,#142551,#142552,#142553,#142554,#142555,
#142556,#142557,#142558,#142559,#142560,#142561,#142562,#142563,#142564,
#142565,#142566,#142567,#142568,#142569,#142570,#142571,#142572),(#142573,
#142574,#142575,#142576,#142577,#142578,#142579,#142580,#142581,#142582,
#142583,#142584,#142585,#142586,#142587,#142588,#142589,#142590,#142591,
#142592,#142593,#142594,#142595,#142596,#142597,#142598,#142599,#142600,
#142601,#142602,#142603,#142604,#142605,#142606,#142607,#142608,#142609,
#142610,#142611,#142612,#142613,#142614,#142615,#142616,#142617,#142618,
#142619,#142620,#142621,#142622,#142623,#142624,#142625,#142626,#142627,
#142628,#142629,#142630,#142631,#142632,#142633,#142634,#142635,#142636,
#142637,#142638,#142639,#142640,#142641,#142642,#142643,#142644,#142645,
#142646,#142647,#142648,#142649,#142650,#142651,#142652,#142653,#142654,
#142655,#142656,#142657,#142658,#142659,#142660,#142661,#142662,#142663,
#142664,#142665,#142666,#142667,#142668,#142669,#142670,#142671,#142672,
#142673,#142674,#142675,#142676,#142677,#142678,#142679,#142680,#142681,
#142682,#142683,#142684,#142685,#142686,#142687,#142688,#142689,#142690,
#142691,#142692,#142693,#142694,#142695,#142696,#142697,#142698,#142699,
#142700,#142701,#142702,#142703,#142704,#142705,#142706,#142707,#142708,
#142709,#142710,#142711,#142712,#142713,#142714,#142715,#142716,#142717,
#142718,#142719,#142720,#142721,#142722,#142723,#142724,#142725,#142726,
#142727,#142728,#142729,#142730,#142731,#142732,#142733,#142734,#142735,
#142736,#142737,#142738,#142739,#142740,#142741,#142742,#142743,#142744,
#142745,#142746,#142747,#142748,#142749,#142750,#142751,#142752,#142753,
#142754,#142755,#142756,#142757,#142758,#142759,#142760,#142761,#142762,
#142763,#142764,#142765,#142766,#142767,#142768,#142769,#142770,#142771,
#142772,#142773,#142774,#142775,#142776,#142777,#142778,#142779,#142780,
#142781,#142782,#142783,#142784,#142785,#142786,#142787,#142788,#142789,
#142790,#142791,#142792,#142793,#142794,#142795,#142796,#142797,#142798,
#142799,#142800,#142801,#142802,#142803,#142804,#142805,#142806,#142807,
#142808,#142809,#142810,#142811,#142812,#142813,#142814,#142815,#142816,
#142817,#142818,#142819,#142820,#142821,#142822,#142823,#142824,#142825,
#142826,#142827,#142828,#142829,#142830,#142831,#142832,#142833,#142834,
#142835,#142836,#142837,#142838,#142839,#142840,#142841,#142842,#142843,
#142844,#142845,#142846,#142847,#142848,#142849,#142850,#142851,#142852,
#142853,#142854,#142855,#142856,#142857,#142858,#142859,#142860,#142861,
#142862,#142863,#142864,#142865,#142866,#142867,#142868,#142869,#142870,
#142871,#142872,#142873,#142874,#142875,#142876,#142877,#142878,#142879,
#142880,#142881,#142882,#142883,#142884,#142885,#142886,#142887,#142888,
#142889,#142890,#142891,#142892,#142893,#142894,#142895,#142896,#142897,
#142898,#142899,#142900,#142901,#142902,#142903,#142904,#142905,#142906,
#142907,#142908,#142909,#142910,#142911,#142912,#142913,#142914,#142915,
#142916,#142917,#142918,#142919,#142920,#142921,#142922,#142923,#142924,
#142925,#142926,#142927,#142928,#142929,#142930,#142931,#142932,#142933,
#142934,#142935,#142936,#142937,#142938,#142939,#142940,#142941,#142942,
#142943,#142944,#142945,#142946,#142947,#142948,#142949,#142950,#142951,
#142952,#142953,#142954,#142955,#142956,#142957,#142958,#142959,#142960,
#142961,#142962,#142963,#142964,#142965,#142966,#142967,#142968,#142969,
#142970,#142971,#142972,#142973,#142974,#142975,#142976,#142977,#142978,
#142979,#142980,#142981,#142982,#142983,#142984,#142985,#142986,#142987,
#142988,#142989,#142990,#142991,#142992,#142993,#142994,#142995,#142996,
#142997,#142998,#142999,#143000,#143001,#143002,#143003,#143004,#143005,
#143006,#143007,#143008,#143009,#143010,#143011,#143012,#143013,#143014,
#143015,#143016,#143017,#143018,#143019,#143020,#143021,#143022,#143023,
#143024,#143025,#143026,#143027,#143028,#143029,#143030,#143031,#143032,
#143033,#143034,#143035,#143036,#143037,#143038,#143039,#143040,#143041,
#143042,#143043,#143044,#143045,#143046,#143047,#143048,#143049,#143050,
#143051,#143052,#143053,#143054,#143055,#143056,#143057,#143058,#143059,
#143060,#143061,#143062,#143063,#143064,#143065,#143066,#143067,#143068,
#143069,#143070,#143071,#143072,#143073,#143074,#143075,#143076,#143077,
#143078,#143079,#143080,#143081,#143082,#143083,#143084,#143085,#143086,
#143087,#143088,#143089,#143090,#143091,#143092,#143093,#143094,#143095,
#143096,#143097,#143098,#143099,#143100,#143101,#143102,#143103,#143104,
#143105,#143106,#143107,#143108,#143109,#143110,#143111,#143112,#143113,
#143114,#143115,#143116,#143117,#143118,#143119,#143120,#143121,#143122,
#143123,#143124,#143125,#143126,#143127,#143128,#143129,#143130,#143131,
#143132,#143133,#143134,#143135,#143136,#143137,#143138,#143139,#143140,
#143141,#143142,#143143,#143144,#143145,#143146,#143147,#143148,#143149,
#143150,#143151,#143152,#143153,#143154,#143155,#143156,#143157,#143158,
#143159,#143160,#143161,#143162,#143163,#143164,#143165,#143166,#143167,
#143168,#143169,#143170,#143171,#143172,#143173,#143174,#143175,#143176,
#143177,#143178,#143179,#143180,#143181,#143182,#143183,#143184,#143185,
#143186,#143187,#143188,#143189,#143190,#143191,#143192,#143193,#143194,
#143195,#143196,#143197,#143198,#143199,#143200,#143201,#143202,#143203,
#143204,#143205,#143206,#143207,#143208,#143209,#143210,#143211,#143212,
#143213,#143214,#143215,#143216,#143217,#143218,#143219,#143220,#143221,
#143222,#143223,#143224,#143225,#143226,#143227,#143228,#143229,#143230,
#143231,#143232,#143233,#143234,#143235,#143236,#143237,#143238,#143239,
#143240,#143241,#143242,#143243,#143244,#143245,#143246,#143247,#143248,
#143249,#143250,#143251,#143252,#143253,#143254,#143255,#143256,#143257,
#143258,#143259,#143260,#143261,#143262,#143263,#143264,#143265,#143266,
#143267,#143268,#143269,#143270,#143271,#143272,#143273,#143274,#143275,
#143276,#143277,#143278,#143279,#143280,#143281,#143282,#143283,#143284,
#143285,#143286,#143287,#143288,#143289,#143290,#143291,#143292,#143293,
#143294,#143295,#143296,#143297,#143298,#143299,#143300,#143301,#143302,
#143303,#143304,#143305,#143306,#143307,#143308,#143309,#143310,#143311,
#143312,#143313,#143314,#143315,#143316,#143317,#143318,#143319,#143320,
#143321,#143322,#143323,#143324,#143325,#143326,#143327,#143328,#143329,
#143330,#143331,#143332,#143333,#143334,#143335,#143336,#143337,#143338,
#143339,#143340,#143341,#143342,#143343,#143344,#143345,#143346,#143347,
#143348,#143349,#143350,#143351,#143352,#143353,#143354,#143355,#143356,
#143357,#143358,#143359,#143360,#143361,#143362,#143363,#143364,#143365,
#143366,#143367,#143368,#143369,#143370,#143371,#143372,#143373,#143374,
#143375,#143376,#143377,#143378,#143379,#143380,#143381,#143382,#143383,
#143384,#143385,#143386,#143387,#143388,#143389,#143390,#143391,#143392,
#143393,#143394,#143395,#143396,#143397,#143398,#143399,#143400,#143401,
#143402,#143403,#143404,#143405,#143406,#143407,#143408,#143409,#143410,
#143411,#143412,#143413,#143414,#143415,#143416,#143417,#143418,#143419,
#143420,#143421,#143422,#143423,#143424,#143425,#143426,#143427,#143428,
#143429,#143430,#143431,#143432,#143433,#143434,#143435,#143436,#143437,
#143438,#143439,#143440,#143441,#143442,#143443,#143444,#143445,#143446,
#143447,#143448,#143449,#143450,#143451,#143452,#143453,#143454,#143455,
#143456,#143457,#143458,#143459,#143460,#143461,#143462,#143463,#143464,
#143465,#143466,#143467,#143468,#143469,#143470,#143471,#143472,#143473,
#143474,#143475,#143476,#143477,#143478,#143479,#143480,#143481,#143482,
#143483,#143484,#143485,#143486,#143487,#143488,#143489,#143490,#143491,
#143492,#143493,#143494,#143495,#143496,#143497,#143498,#143499,#143500,
#143501,#143502,#143503,#143504,#143505,#143506,#143507,#143508,#143509,
#143510,#143511,#143512,#143513,#143514,#143515,#143516,#143517,#143518,
#143519,#143520,#143521,#143522,#143523,#143524,#143525,#143526,#143527,
#143528,#143529,#143530,#143531,#143532,#143533,#143534,#143535,#143536,
#143537,#143538,#143539,#143540,#143541,#143542,#143543,#143544,#143545,
#143546,#143547,#143548,#143549,#143550,#143551,#143552,#143553,#143554,
#143555,#143556,#143557,#143558,#143559,#143560,#143561,#143562,#143563,
#143564,#143565,#143566,#143567,#143568,#143569,#143570,#143571,#143572,
#143573,#143574,#143575,#143576,#143577,#143578,#143579,#143580,#143581,
#143582,#143583,#143584,#143585,#143586,#143587,#143588,#143589,#143590,
#143591,#143592,#143593,#143594,#143595,#143596,#143597,#143598,#143599,
#143600,#143601,#143602,#143603,#143604,#143605,#143606,#143607,#143608,
#143609,#143610,#143611,#143612,#143613,#143614,#143615,#143616,#143617,
#143618,#143619,#143620,#143621,#143622,#143623,#143624,#143625,#143626,
#143627,#143628,#143629,#143630,#143631,#143632,#143633,#143634,#143635,
#143636,#143637,#143638,#143639,#143640,#143641,#143642,#143643,#143644,
#143645,#143646,#143647,#143648,#143649,#143650,#143651,#143652,#143653,
#143654,#143655,#143656,#143657,#143658,#143659,#143660,#143661,#143662,
#143663,#143664,#143665,#143666,#143667,#143668,#143669,#143670,#143671,
#143672,#143673,#143674,#143675,#143676,#143677,#143678,#143679,#143680,
#143681,#143682,#143683,#143684,#143685,#143686,#143687,#143688,#143689,
#143690,#143691,#143692,#143693,#143694,#143695,#143696,#143697,#143698,
#143699,#143700,#143701,#143702,#143703,#143704,#143705,#143706,#143707,
#143708,#143709,#143710,#143711,#143712,#143713,#143714,#143715,#143716,
#143717,#143718,#143719,#143720,#143721,#143722,#143723,#143724,#143725,
#143726,#143727,#143728,#143729,#143730,#143731,#143732,#143733,#143734,
#143735,#143736,#143737,#143738,#143739,#143740,#143741,#143742,#143743,
#143744,#143745,#143746,#143747,#143748,#143749,#143750,#143751,#143752,
#143753,#143754,#143755,#143756,#143757,#143758,#143759,#143760,#143761,
#143762,#143763,#143764,#143765,#143766,#143767,#143768,#143769,#143770,
#143771,#143772,#143773,#143774,#143775,#143776,#143777,#143778,#143779,
#143780,#143781,#143782,#143783,#143784,#143785,#143786,#143787,#143788,
#143789,#143790,#143791,#143792,#143793,#143794,#143795,#143796,#143797,
#143798,#143799,#143800,#143801,#143802,#143803,#143804,#143805,#143806,
#143807,#143808,#143809,#143810,#143811,#143812,#143813,#143814,#143815,
#143816,#143817,#143818,#143819,#143820,#143821,#143822,#143823,#143824,
#143825,#143826,#143827,#143828,#143829,#143830,#143831,#143832,#143833,
#143834,#143835,#143836,#143837,#143838,#143839,#143840,#143841,#143842,
#143843,#143844,#143845,#143846,#143847,#143848,#143849,#143850,#143851,
#143852,#143853,#143854,#143855,#143856,#143857,#143858,#143859,#143860,
#143861,#143862,#143863,#143864,#143865,#143866,#143867,#143868,#143869,
#143870,#143871,#143872,#143873,#143874,#143875,#143876,#143877,#143878,
#143879,#143880,#143881,#143882,#143883,#143884,#143885,#143886,#143887,
#143888,#143889,#143890,#143891,#143892,#143893,#143894,#143895,#143896,
#143897,#143898,#143899,#143900,#143901,#143902,#143903,#143904,#143905,
#143906,#143907,#143908,#143909,#143910,#143911,#143912,#143913,#143914,
#143915,#143916,#143917,#143918,#143919,#143920,#143921,#143922,#143923,
#143924,#143925,#143926,#143927,#143928,#143929,#143930,#143931,#143932,
#143933,#143934,#143935,#143936,#143937,#143938,#143939,#143940,#143941,
#143942,#143943,#143944,#143945,#143946,#143947,#143948,#143949,#143950,
#143951,#143952,#143953,#143954,#143955,#143956,#143957,#143958,#143959,
#143960,#143961,#143962,#143963,#143964,#143965,#143966,#143967,#143968,
#143969,#143970,#143971,#143972,#143973,#143974,#143975,#143976,#143977,
#143978,#143979,#143980,#143981,#143982,#143983,#143984,#143985,#143986,
#143987,#143988,#143989,#143990,#143991,#143992,#143993,#143994,#143995,
#143996,#143997,#143998,#143999,#144000,#144001,#144002,#144003,#144004,
#144005,#144006,#144007,#144008,#144009,#144010,#144011,#144012,#144013,
#144014,#144015,#144016,#144017,#144018,#144019,#144020,#144021,#144022,
#144023,#144024,#144025,#144026,#144027,#144028,#144029,#144030,#144031,
#144032,#144033,#144034,#144035,#144036,#144037,#144038,#144039,#144040,
#144041,#144042,#144043,#144044,#144045,#144046,#144047,#144048,#144049,
#144050,#144051,#144052,#144053,#144054,#144055,#144056,#144057,#144058,
#144059,#144060,#144061,#144062,#144063,#144064,#144065,#144066,#144067,
#144068,#144069,#144070,#144071,#144072,#144073,#144074,#144075,#144076,
#144077,#144078,#144079,#144080,#144081,#144082,#144083,#144084,#144085,
#144086,#144087,#144088,#144089,#144090,#144091,#144092,#144093,#144094,
#144095,#144096,#144097,#144098,#144099,#144100,#144101,#144102,#144103,
#144104,#144105,#144106,#144107,#144108,#144109,#144110,#144111,#144112,
#144113,#144114,#144115,#144116,#144117,#144118,#144119,#144120,#144121,
#144122,#144123,#144124,#144125,#144126,#144127,#144128,#144129,#144130,
#144131,#144132,#144133,#144134,#144135,#144136,#144137,#144138,#144139,
#144140,#144141,#144142,#144143,#144144,#144145,#144146,#144147,#144148,
#144149,#144150,#144151,#144152,#144153,#144154,#144155,#144156,#144157,
#144158,#144159,#144160,#144161,#144162,#144163,#144164,#144165,#144166,
#144167,#144168,#144169,#144170,#144171,#144172,#144173,#144174,#144175,
#144176,#144177,#144178,#144179,#144180,#144181,#144182,#144183,#144184,
#144185,#144186,#144187,#144188,#144189,#144190,#144191,#144192,#144193,
#144194,#144195,#144196,#144197,#144198,#144199,#144200,#144201,#144202,
#144203,#144204,#144205,#144206,#144207,#144208,#144209,#144210,#144211,
#144212,#144213,#144214,#144215,#144216,#144217,#144218,#144219,#144220,
#144221,#144222,#144223,#144224,#144225,#144226,#144227,#144228,#144229,
#144230,#144231,#144232,#144233,#144234,#144235,#144236,#144237,#144238,
#144239,#144240,#144241,#144242,#144243,#144244,#144245,#144246,#144247,
#144248,#144249,#144250,#144251,#144252,#144253,#144254,#144255,#144256,
#144257,#144258,#144259,#144260,#144261,#144262,#144263,#144264,#144265,
#144266,#144267,#144268,#144269,#144270,#144271,#144272,#144273,#144274,
#144275,#144276,#144277,#144278,#144279,#144280,#144281,#144282,#144283,
#144284,#144285,#144286,#144287,#144288,#144289,#144290,#144291,#144292,
#144293,#144294,#144295,#144296,#144297,#144298,#144299,#144300,#144301,
#144302,#144303,#144304,#144305,#144306,#144307,#144308,#144309,#144310,
#144311,#144312,#144313,#144314,#144315,#144316,#144317,#144318,#144319,
#144320,#144321,#144322,#144323,#144324,#144325,#144326,#144327,#144328,
#144329,#144330,#144331,#144332,#144333,#144334,#144335,#144336,#144337,
#144338,#144339,#144340,#144341,#144342,#144343,#144344,#144345,#144346,
#144347,#144348,#144349,#144350,#144351,#144352,#144353,#144354,#144355,
#144356,#144357,#144358,#144359,#144360,#144361,#144362,#144363,#144364,
#144365,#144366,#144367,#144368,#144369,#144370,#144371,#144372,#144373,
#144374,#144375,#144376,#144377,#144378,#144379,#144380,#144381,#144382,
#144383,#144384,#144385,#144386,#144387,#144388,#144389,#144390,#144391,
#144392,#144393,#144394,#144395,#144396,#144397,#144398,#144399,#144400,
#144401,#144402,#144403,#144404,#144405,#144406,#144407,#144408,#144409,
#144410,#144411,#144412,#144413,#144414,#144415,#144416,#144417,#144418,
#144419,#144420,#144421,#144422,#144423,#144424,#144425,#144426,#144427,
#144428,#144429,#144430,#144431,#144432,#144433,#144434,#144435,#144436,
#144437,#144438,#144439,#144440,#144441,#144442,#144443,#144444,#144445,
#144446,#144447,#144448,#144449,#144450,#144451,#144452,#144453,#144454,
#144455,#144456,#144457,#144458,#144459,#144460,#144461,#144462,#144463,
#144464,#144465,#144466,#144467,#144468,#144469,#144470,#144471,#144472,
#144473,#144474,#144475,#144476,#144477,#144478,#144479,#144480,#144481,
#144482,#144483,#144484,#144485,#144486,#144487,#144488,#144489,#144490,
#144491,#144492,#144493,#144494,#144495,#144496,#144497,#144498,#144499,
#144500,#144501,#144502,#144503,#144504,#144505,#144506,#144507,#144508,
#144509,#144510,#144511,#144512,#144513,#144514,#144515,#144516,#144517,
#144518,#144519,#144520,#144521,#144522,#144523,#144524,#144525,#144526,
#144527,#144528,#144529,#144530,#144531,#144532,#144533,#144534,#144535,
#144536,#144537,#144538,#144539,#144540,#144541,#144542,#144543,#144544,
#144545,#144546,#144547,#144548,#144549,#144550,#144551,#144552,#144553,
#144554,#144555,#144556,#144557,#144558,#144559,#144560,#144561,#144562,
#144563,#144564,#144565,#144566,#144567,#144568,#144569,#144570,#144571,
#144572,#144573,#144574,#144575,#144576,#144577,#144578,#144579,#144580,
#144581,#144582,#144583,#144584,#144585,#144586,#144587,#144588,#144589,
#144590,#144591,#144592,#144593,#144594,#144595,#144596,#144597,#144598,
#144599,#144600,#144601,#144602,#144603,#144604,#144605,#144606,#144607,
#144608,#144609,#144610,#144611,#144612,#144613,#144614,#144615,#144616,
#144617,#144618,#144619,#144620,#144621,#144622,#144623),(#144624,#144625,
#144626,#144627,#144628,#144629,#144630,#144631,#144632,#144633,#144634,
#144635,#144636,#144637,#144638,#144639,#144640,#144641,#144642,#144643,
#144644,#144645,#144646,#144647,#144648,#144649,#144650,#144651,#144652,
#144653,#144654,#144655,#144656,#144657,#144658,#144659,#144660,#144661,
#144662,#144663,#144664,#144665,#144666,#144667,#144668,#144669,#144670,
#144671,#144672,#144673,#144674,#144675,#144676,#144677,#144678,#144679,
#144680,#144681,#144682,#144683,#144684,#144685,#144686,#144687,#144688,
#144689,#144690,#144691,#144692,#144693,#144694,#144695,#144696,#144697,
#144698,#144699,#144700,#144701,#144702,#144703,#144704,#144705,#144706,
#144707,#144708,#144709,#144710,#144711,#144712,#144713,#144714,#144715,
#144716,#144717,#144718,#144719,#144720,#144721,#144722,#144723,#144724,
#144725,#144726,#144727,#144728,#144729,#144730,#144731,#144732,#144733,
#144734,#144735,#144736,#144737,#144738,#144739,#144740,#144741,#144742,
#144743,#144744,#144745,#144746,#144747,#144748,#144749,#144750,#144751,
#144752,#144753,#144754,#144755,#144756,#144757,#144758,#144759,#144760,
#144761,#144762,#144763,#144764,#144765,#144766,#144767,#144768,#144769,
#144770,#144771,#144772,#144773,#144774,#144775,#144776,#144777,#144778,
#144779,#144780,#144781,#144782,#144783,#144784,#144785,#144786,#144787,
#144788,#144789,#144790,#144791,#144792,#144793,#144794,#144795,#144796,
#144797,#144798,#144799,#144800,#144801,#144802,#144803,#144804,#144805,
#144806,#144807,#144808,#144809,#144810,#144811,#144812,#144813,#144814,
#144815,#144816,#144817,#144818,#144819,#144820,#144821,#144822,#144823,
#144824,#144825,#144826,#144827,#144828,#144829,#144830,#144831,#144832,
#144833,#144834,#144835,#144836,#144837,#144838,#144839,#144840,#144841,
#144842,#144843,#144844,#144845,#144846,#144847,#144848,#144849,#144850,
#144851,#144852,#144853,#144854,#144855,#144856,#144857,#144858,#144859,
#144860,#144861,#144862,#144863,#144864,#144865,#144866,#144867,#144868,
#144869,#144870,#144871,#144872,#144873,#144874,#144875,#144876,#144877,
#144878,#144879,#144880,#144881,#144882,#144883,#144884,#144885,#144886,
#144887,#144888,#144889,#144890,#144891,#144892,#144893,#144894,#144895,
#144896,#144897,#144898,#144899,#144900,#144901,#144902,#144903,#144904,
#144905,#144906,#144907,#144908,#144909,#144910,#144911,#144912,#144913,
#144914,#144915,#144916,#144917,#144918,#144919,#144920,#144921,#144922,
#144923,#144924,#144925,#144926,#144927,#144928,#144929,#144930,#144931,
#144932,#144933,#144934,#144935,#144936,#144937,#144938,#144939,#144940,
#144941,#144942,#144943,#144944,#144945,#144946,#144947,#144948,#144949,
#144950,#144951,#144952,#144953,#144954,#144955,#144956,#144957,#144958,
#144959,#144960,#144961,#144962,#144963,#144964,#144965,#144966,#144967,
#144968,#144969,#144970,#144971,#144972,#144973,#144974,#144975,#144976,
#144977,#144978,#144979,#144980,#144981,#144982,#144983,#144984,#144985,
#144986,#144987,#144988,#144989,#144990,#144991,#144992,#144993,#144994,
#144995,#144996,#144997,#144998,#144999,#145000,#145001,#145002,#145003,
#145004,#145005,#145006,#145007,#145008,#145009,#145010,#145011,#145012,
#145013,#145014,#145015,#145016,#145017,#145018,#145019,#145020,#145021,
#145022,#145023,#145024,#145025,#145026,#145027,#145028,#145029,#145030,
#145031,#145032,#145033,#145034,#145035,#145036,#145037,#145038,#145039,
#145040,#145041,#145042,#145043,#145044,#145045,#145046,#145047,#145048,
#145049,#145050,#145051,#145052,#145053,#145054,#145055,#145056,#145057,
#145058,#145059,#145060,#145061,#145062,#145063,#145064,#145065,#145066,
#145067,#145068,#145069,#145070,#145071,#145072,#145073,#145074,#145075,
#145076,#145077,#145078,#145079,#145080,#145081,#145082,#145083,#145084,
#145085,#145086,#145087,#145088,#145089,#145090,#145091,#145092,#145093,
#145094,#145095,#145096,#145097,#145098,#145099,#145100,#145101,#145102,
#145103,#145104,#145105,#145106,#145107,#145108,#145109,#145110,#145111,
#145112,#145113,#145114,#145115,#145116,#145117,#145118,#145119,#145120,
#145121,#145122,#145123,#145124,#145125,#145126,#145127,#145128,#145129,
#145130,#145131,#145132,#145133,#145134,#145135,#145136,#145137,#145138,
#145139,#145140,#145141,#145142,#145143,#145144,#145145,#145146,#145147,
#145148,#145149,#145150,#145151,#145152,#145153,#145154,#145155,#145156,
#145157,#145158,#145159,#145160,#145161,#145162,#145163,#145164,#145165,
#145166,#145167,#145168,#145169,#145170,#145171,#145172,#145173,#145174,
#145175,#145176,#145177,#145178,#145179,#145180,#145181,#145182,#145183,
#145184,#145185,#145186,#145187,#145188,#145189,#145190,#145191,#145192,
#145193,#145194,#145195,#145196,#145197,#145198,#145199,#145200,#145201,
#145202,#145203,#145204,#145205,#145206,#145207,#145208,#145209,#145210,
#145211,#145212,#145213,#145214,#145215,#145216,#145217,#145218,#145219,
#145220,#145221,#145222,#145223,#145224,#145225,#145226,#145227,#145228,
#145229,#145230,#145231,#145232,#145233,#145234,#145235,#145236,#145237,
#145238,#145239,#145240,#145241,#145242,#145243,#145244,#145245,#145246,
#145247,#145248,#145249,#145250,#145251,#145252,#145253,#145254,#145255,
#145256,#145257,#145258,#145259,#145260,#145261,#145262,#145263,#145264,
#145265,#145266,#145267,#145268,#145269,#145270,#145271,#145272,#145273,
#145274,#145275,#145276,#145277,#145278,#145279,#145280,#145281,#145282,
#145283,#145284,#145285,#145286,#145287,#145288,#145289,#145290,#145291,
#145292,#145293,#145294,#145295,#145296,#145297,#145298,#145299,#145300,
#145301,#145302,#145303,#145304,#145305,#145306,#145307,#145308,#145309,
#145310,#145311,#145312,#145313,#145314,#145315,#145316,#145317,#145318,
#145319,#145320,#145321,#145322,#145323,#145324,#145325,#145326,#145327,
#145328,#145329,#145330,#145331,#145332,#145333,#145334,#145335,#145336,
#145337,#145338,#145339,#145340,#145341,#145342,#145343,#145344,#145345,
#145346,#145347,#145348,#145349,#145350,#145351,#145352,#145353,#145354,
#145355,#145356,#145357,#145358,#145359,#145360,#145361,#145362,#145363,
#145364,#145365,#145366,#145367,#145368,#145369,#145370,#145371,#145372,
#145373,#145374,#145375,#145376,#145377,#145378,#145379,#145380,#145381,
#145382,#145383,#145384,#145385,#145386,#145387,#145388,#145389,#145390,
#145391,#145392,#145393,#145394,#145395,#145396,#145397,#145398,#145399,
#145400,#145401,#145402,#145403,#145404,#145405,#145406,#145407,#145408,
#145409,#145410,#145411,#145412,#145413,#145414,#145415,#145416,#145417,
#145418,#145419,#145420,#145421,#145422,#145423,#145424,#145425,#145426,
#145427,#145428,#145429,#145430,#145431,#145432,#145433,#145434,#145435,
#145436,#145437,#145438,#145439,#145440,#145441,#145442,#145443,#145444,
#145445,#145446,#145447,#145448,#145449,#145450,#145451,#145452,#145453,
#145454,#145455,#145456,#145457,#145458,#145459,#145460,#145461,#145462,
#145463,#145464,#145465,#145466,#145467,#145468,#145469,#145470,#145471,
#145472,#145473,#145474,#145475,#145476,#145477,#145478,#145479,#145480,
#145481,#145482,#145483,#145484,#145485,#145486,#145487,#145488,#145489,
#145490,#145491,#145492,#145493,#145494,#145495,#145496,#145497,#145498,
#145499,#145500,#145501,#145502,#145503,#145504,#145505,#145506,#145507,
#145508,#145509,#145510,#145511,#145512,#145513,#145514,#145515,#145516,
#145517,#145518,#145519,#145520,#145521,#145522,#145523,#145524,#145525,
#145526,#145527,#145528,#145529,#145530,#145531,#145532,#145533,#145534,
#145535,#145536,#145537,#145538,#145539,#145540,#145541,#145542,#145543,
#145544,#145545,#145546,#145547,#145548,#145549,#145550,#145551,#145552,
#145553,#145554,#145555,#145556,#145557,#145558,#145559,#145560,#145561,
#145562,#145563,#145564,#145565,#145566,#145567,#145568,#145569,#145570,
#145571,#145572,#145573,#145574,#145575,#145576,#145577,#145578,#145579,
#145580,#145581,#145582,#145583,#145584,#145585,#145586,#145587,#145588,
#145589,#145590,#145591,#145592,#145593,#145594,#145595,#145596,#145597,
#145598,#145599,#145600,#145601,#145602,#145603,#145604,#145605,#145606,
#145607,#145608,#145609,#145610,#145611,#145612,#145613,#145614,#145615,
#145616,#145617,#145618,#145619,#145620,#145621,#145622,#145623,#145624,
#145625,#145626,#145627,#145628,#145629,#145630,#145631,#145632,#145633,
#145634,#145635,#145636,#145637,#145638,#145639,#145640,#145641,#145642,
#145643,#145644,#145645,#145646,#145647,#145648,#145649,#145650,#145651,
#145652,#145653,#145654,#145655,#145656,#145657,#145658,#145659,#145660,
#145661,#145662,#145663,#145664,#145665,#145666,#145667,#145668,#145669,
#145670,#145671,#145672,#145673,#145674,#145675,#145676,#145677,#145678,
#145679,#145680,#145681,#145682,#145683,#145684,#145685,#145686,#145687,
#145688,#145689,#145690,#145691,#145692,#145693,#145694,#145695,#145696,
#145697,#145698,#145699,#145700,#145701,#145702,#145703,#145704,#145705,
#145706,#145707,#145708,#145709,#145710,#145711,#145712,#145713,#145714,
#145715,#145716,#145717,#145718,#145719,#145720,#145721,#145722,#145723,
#145724,#145725,#145726,#145727,#145728,#145729,#145730,#145731,#145732,
#145733,#145734,#145735,#145736,#145737,#145738,#145739,#145740,#145741,
#145742,#145743,#145744,#145745,#145746,#145747,#145748,#145749,#145750,
#145751,#145752,#145753,#145754,#145755,#145756,#145757,#145758,#145759,
#145760,#145761,#145762,#145763,#145764,#145765,#145766,#145767,#145768,
#145769,#145770,#145771,#145772,#145773,#145774,#145775,#145776,#145777,
#145778,#145779,#145780,#145781,#145782,#145783,#145784,#145785,#145786,
#145787,#145788,#145789,#145790,#145791,#145792,#145793,#145794,#145795,
#145796,#145797,#145798,#145799,#145800,#145801,#145802,#145803,#145804,
#145805,#145806,#145807,#145808,#145809,#145810,#145811,#145812,#145813,
#145814,#145815,#145816,#145817,#145818,#145819,#145820,#145821,#145822,
#145823,#145824,#145825,#145826,#145827,#145828,#145829,#145830,#145831,
#145832,#145833,#145834,#145835,#145836,#145837,#145838,#145839,#145840,
#145841,#145842,#145843,#145844,#145845,#145846,#145847,#145848,#145849,
#145850,#145851,#145852,#145853,#145854,#145855,#145856,#145857,#145858,
#145859,#145860,#145861,#145862,#145863,#145864,#145865,#145866,#145867,
#145868,#145869,#145870,#145871,#145872,#145873,#145874,#145875,#145876,
#145877,#145878,#145879,#145880,#145881,#145882,#145883,#145884,#145885,
#145886,#145887,#145888,#145889,#145890,#145891,#145892,#145893,#145894,
#145895,#145896,#145897,#145898,#145899,#145900,#145901,#145902,#145903,
#145904,#145905,#145906,#145907,#145908,#145909,#145910,#145911,#145912,
#145913,#145914,#145915,#145916,#145917,#145918,#145919,#145920,#145921,
#145922,#145923,#145924,#145925,#145926,#145927,#145928,#145929,#145930,
#145931,#145932,#145933,#145934,#145935,#145936,#145937,#145938,#145939,
#145940,#145941,#145942,#145943,#145944,#145945,#145946,#145947,#145948,
#145949,#145950,#145951,#145952,#145953,#145954,#145955,#145956,#145957,
#145958,#145959,#145960,#145961,#145962,#145963,#145964,#145965,#145966,
#145967,#145968,#145969,#145970,#145971,#145972,#145973,#145974,#145975,
#145976,#145977,#145978,#145979,#145980,#145981,#145982,#145983,#145984,
#145985,#145986,#145987,#145988,#145989,#145990,#145991,#145992,#145993,
#145994,#145995,#145996,#145997,#145998,#145999,#146000,#146001,#146002,
#146003,#146004,#146005,#146006,#146007,#146008,#146009,#146010,#146011,
#146012,#146013,#146014,#146015,#146016,#146017,#146018,#146019,#146020,
#146021,#146022,#146023,#146024,#146025,#146026,#146027,#146028,#146029,
#146030,#146031,#146032,#146033,#146034,#146035,#146036,#146037,#146038,
#146039,#146040,#146041,#146042,#146043,#146044,#146045,#146046,#146047,
#146048,#146049,#146050,#146051,#146052,#146053,#146054,#146055,#146056,
#146057,#146058,#146059,#146060,#146061,#146062,#146063,#146064,#146065,
#146066,#146067,#146068,#146069,#146070,#146071,#146072,#146073,#146074,
#146075,#146076,#146077,#146078,#146079,#146080,#146081,#146082,#146083,
#146084,#146085,#146086,#146087,#146088,#146089,#146090,#146091,#146092,
#146093,#146094,#146095,#146096,#146097,#146098,#146099,#146100,#146101,
#146102,#146103,#146104,#146105,#146106,#146107,#146108,#146109,#146110,
#146111,#146112,#146113,#146114,#146115,#146116,#146117,#146118,#146119,
#146120,#146121,#146122,#146123,#146124,#146125,#146126,#146127,#146128,
#146129,#146130,#146131,#146132,#146133,#146134,#146135,#146136,#146137,
#146138,#146139,#146140,#146141,#146142,#146143,#146144,#146145,#146146,
#146147,#146148,#146149,#146150,#146151,#146152,#146153,#146154,#146155,
#146156,#146157,#146158,#146159,#146160,#146161,#146162,#146163,#146164,
#146165,#146166,#146167,#146168,#146169,#146170,#146171,#146172,#146173,
#146174,#146175,#146176,#146177,#146178,#146179,#146180,#146181,#146182,
#146183,#146184,#146185,#146186,#146187,#146188,#146189,#146190,#146191,
#146192,#146193,#146194,#146195,#146196,#146197,#146198,#146199,#146200,
#146201,#146202,#146203,#146204,#146205,#146206,#146207,#146208,#146209,
#146210,#146211,#146212,#146213,#146214,#146215,#146216,#146217,#146218,
#146219,#146220,#146221,#146222,#146223,#146224,#146225,#146226,#146227,
#146228,#146229,#146230,#146231,#146232,#146233,#146234,#146235,#146236,
#146237,#146238,#146239,#146240,#146241,#146242,#146243,#146244,#146245,
#146246,#146247,#146248,#146249,#146250,#146251,#146252,#146253,#146254,
#146255,#146256,#146257,#146258,#146259,#146260,#146261,#146262,#146263,
#146264,#146265,#146266,#146267,#146268,#146269,#146270,#146271,#146272,
#146273,#146274,#146275,#146276,#146277,#146278,#146279,#146280,#146281,
#146282,#146283,#146284,#146285,#146286,#146287,#146288,#146289,#146290,
#146291,#146292,#146293,#146294,#146295,#146296,#146297,#146298,#146299,
#146300,#146301,#146302,#146303,#146304,#146305,#146306,#146307,#146308,
#146309,#146310,#146311,#146312,#146313,#146314,#146315,#146316,#146317,
#146318,#146319,#146320,#146321,#146322,#146323,#146324,#146325,#146326,
#146327,#146328,#146329,#146330,#146331,#146332,#146333,#146334,#146335,
#146336,#146337,#146338,#146339,#146340,#146341,#146342,#146343,#146344,
#146345,#146346,#146347,#146348,#146349,#146350,#146351,#146352,#146353,
#146354,#146355,#146356,#146357,#146358,#146359,#146360,#146361,#146362,
#146363,#146364,#146365,#146366,#146367,#146368,#146369,#146370,#146371,
#146372,#146373,#146374,#146375,#146376,#146377,#146378,#146379,#146380,
#146381,#146382,#146383,#146384,#146385,#146386,#146387,#146388,#146389,
#146390,#146391,#146392,#146393,#146394,#146395,#146396,#146397,#146398,
#146399,#146400,#146401,#146402,#146403,#146404,#146405,#146406,#146407,
#146408,#146409,#146410,#146411,#146412,#146413,#146414,#146415,#146416,
#146417,#146418,#146419,#146420,#146421,#146422,#146423,#146424,#146425,
#146426,#146427,#146428,#146429,#146430,#146431,#146432,#146433,#146434,
#146435,#146436,#146437,#146438,#146439,#146440,#146441,#146442,#146443,
#146444,#146445,#146446,#146447,#146448,#146449,#146450,#146451,#146452,
#146453,#146454,#146455,#146456,#146457,#146458,#146459,#146460,#146461,
#146462,#146463,#146464,#146465,#146466,#146467,#146468,#146469,#146470,
#146471,#146472,#146473,#146474,#146475,#146476,#146477,#146478,#146479,
#146480,#146481,#146482,#146483,#146484,#146485,#146486,#146487,#146488,
#146489,#146490,#146491,#146492,#146493,#146494,#146495,#146496,#146497,
#146498,#146499,#146500,#146501,#146502,#146503,#146504,#146505,#146506,
#146507,#146508,#146509,#146510,#146511,#146512,#146513,#146514,#146515,
#146516,#146517,#146518,#146519,#146520,#146521,#146522,#146523,#146524,
#146525,#146526,#146527,#146528,#146529,#146530,#146531,#146532,#146533,
#146534,#146535,#146536,#146537,#146538,#146539,#146540,#146541,#146542,
#146543,#146544,#146545,#146546,#146547,#146548,#146549,#146550,#146551,
#146552,#146553,#146554,#146555,#146556,#146557,#146558,#146559,#146560,
#146561,#146562,#146563,#146564,#146565,#146566,#146567,#146568,#146569,
#146570,#146571,#146572,#146573,#146574,#146575,#146576,#146577,#146578,
#146579,#146580,#146581,#146582,#146583,#146584,#146585,#146586,#146587,
#146588,#146589,#146590,#146591,#146592,#146593,#146594,#146595,#146596,
#146597,#146598,#146599,#146600,#146601,#146602,#146603,#146604,#146605,
#146606,#146607,#146608,#146609,#146610,#146611,#146612,#146613,#146614,
#146615,#146616,#146617,#146618,#146619,#146620,#146621,#146622,#146623,
#146624,#146625,#146626,#146627,#146628,#146629,#146630,#146631,#146632,
#146633,#146634,#146635,#146636,#146637,#146638,#146639,#146640,#146641,
#146642,#146643,#146644,#146645,#146646,#146647,#146648,#146649,#146650,
#146651,#146652,#146653,#146654,#146655,#146656,#146657,#146658,#146659,
#146660,#146661,#146662,#146663,#146664,#146665,#146666,#146667,#146668,
#146669,#146670,#146671,#146672,#146673,#146674),(#146675,#146676,#146677,
#146678,#146679,#146680,#146681,#146682,#146683,#146684,#146685,#146686,
#146687,#146688,#146689,#146690,#146691,#146692,#146693,#146694,#146695,
#146696,#146697,#146698,#146699,#146700,#146701,#146702,#146703,#146704,
#146705,#146706,#146707,#146708,#146709,#146710,#146711,#146712,#146713,
#146714,#146715,#146716,#146717,#146718,#146719,#146720,#146721,#146722,
#146723,#146724,#146725,#146726,#146727,#146728,#146729,#146730,#146731,
#146732,#146733,#146734,#146735,#146736,#146737,#146738,#146739,#146740,
#146741,#146742,#146743,#146744,#146745,#146746,#146747,#146748,#146749,
#146750,#146751,#146752,#146753,#146754,#146755,#146756,#146757,#146758,
#146759,#146760,#146761,#146762,#146763,#146764,#146765,#146766,#146767,
#146768,#146769,#146770,#146771,#146772,#146773,#146774,#146775,#146776,
#146777,#146778,#146779,#146780,#146781,#146782,#146783,#146784,#146785,
#146786,#146787,#146788,#146789,#146790,#146791,#146792,#146793,#146794,
#146795,#146796,#146797,#146798,#146799,#146800,#146801,#146802,#146803,
#146804,#146805,#146806,#146807,#146808,#146809,#146810,#146811,#146812,
#146813,#146814,#146815,#146816,#146817,#146818,#146819,#146820,#146821,
#146822,#146823,#146824,#146825,#146826,#146827,#146828,#146829,#146830,
#146831,#146832,#146833,#146834,#146835,#146836,#146837,#146838,#146839,
#146840,#146841,#146842,#146843,#146844,#146845,#146846,#146847,#146848,
#146849,#146850,#146851,#146852,#146853,#146854,#146855,#146856,#146857,
#146858,#146859,#146860,#146861,#146862,#146863,#146864,#146865,#146866,
#146867,#146868,#146869,#146870,#146871,#146872,#146873,#146874,#146875,
#146876,#146877,#146878,#146879,#146880,#146881,#146882,#146883,#146884,
#146885,#146886,#146887,#146888,#146889,#146890,#146891,#146892,#146893,
#146894,#146895,#146896,#146897,#146898,#146899,#146900,#146901,#146902,
#146903,#146904,#146905,#146906,#146907,#146908,#146909,#146910,#146911,
#146912,#146913,#146914,#146915,#146916,#146917,#146918,#146919,#146920,
#146921,#146922,#146923,#146924,#146925,#146926,#146927,#146928,#146929,
#146930,#146931,#146932,#146933,#146934,#146935,#146936,#146937,#146938,
#146939,#146940,#146941,#146942,#146943,#146944,#146945,#146946,#146947,
#146948,#146949,#146950,#146951,#146952,#146953,#146954,#146955,#146956,
#146957,#146958,#146959,#146960,#146961,#146962,#146963,#146964,#146965,
#146966,#146967,#146968,#146969,#146970,#146971,#146972,#146973,#146974,
#146975,#146976,#146977,#146978,#146979,#146980,#146981,#146982,#146983,
#146984,#146985,#146986,#146987,#146988,#146989,#146990,#146991,#146992,
#146993,#146994,#146995,#146996,#146997,#146998,#146999,#147000,#147001,
#147002,#147003,#147004,#147005,#147006,#147007,#147008,#147009,#147010,
#147011,#147012,#147013,#147014,#147015,#147016,#147017,#147018,#147019,
#147020,#147021,#147022,#147023,#147024,#147025,#147026,#147027,#147028,
#147029,#147030,#147031,#147032,#147033,#147034,#147035,#147036,#147037,
#147038,#147039,#147040,#147041,#147042,#147043,#147044,#147045,#147046,
#147047,#147048,#147049,#147050,#147051,#147052,#147053,#147054,#147055,
#147056,#147057,#147058,#147059,#147060,#147061,#147062,#147063,#147064,
#147065,#147066,#147067,#147068,#147069,#147070,#147071,#147072,#147073,
#147074,#147075,#147076,#147077,#147078,#147079,#147080,#147081,#147082,
#147083,#147084,#147085,#147086,#147087,#147088,#147089,#147090,#147091,
#147092,#147093,#147094,#147095,#147096,#147097,#147098,#147099,#147100,
#147101,#147102,#147103,#147104,#147105,#147106,#147107,#147108,#147109,
#147110,#147111,#147112,#147113,#147114,#147115,#147116,#147117,#147118,
#147119,#147120,#147121,#147122,#147123,#147124,#147125,#147126,#147127,
#147128,#147129,#147130,#147131,#147132,#147133,#147134,#147135,#147136,
#147137,#147138,#147139,#147140,#147141,#147142,#147143,#147144,#147145,
#147146,#147147,#147148,#147149,#147150,#147151,#147152,#147153,#147154,
#147155,#147156,#147157,#147158,#147159,#147160,#147161,#147162,#147163,
#147164,#147165,#147166,#147167,#147168,#147169,#147170,#147171,#147172,
#147173,#147174,#147175,#147176,#147177,#147178,#147179,#147180,#147181,
#147182,#147183,#147184,#147185,#147186,#147187,#147188,#147189,#147190,
#147191,#147192,#147193,#147194,#147195,#147196,#147197,#147198,#147199,
#147200,#147201,#147202,#147203,#147204,#147205,#147206,#147207,#147208,
#147209,#147210,#147211,#147212,#147213,#147214,#147215,#147216,#147217,
#147218,#147219,#147220,#147221,#147222,#147223,#147224,#147225,#147226,
#147227,#147228,#147229,#147230,#147231,#147232,#147233,#147234,#147235,
#147236,#147237,#147238,#147239,#147240,#147241,#147242,#147243,#147244,
#147245,#147246,#147247,#147248,#147249,#147250,#147251,#147252,#147253,
#147254,#147255,#147256,#147257,#147258,#147259,#147260,#147261,#147262,
#147263,#147264,#147265,#147266,#147267,#147268,#147269,#147270,#147271,
#147272,#147273,#147274,#147275,#147276,#147277,#147278,#147279,#147280,
#147281,#147282,#147283,#147284,#147285,#147286,#147287,#147288,#147289,
#147290,#147291,#147292,#147293,#147294,#147295,#147296,#147297,#147298,
#147299,#147300,#147301,#147302,#147303,#147304,#147305,#147306,#147307,
#147308,#147309,#147310,#147311,#147312,#147313,#147314,#147315,#147316,
#147317,#147318,#147319,#147320,#147321,#147322,#147323,#147324,#147325,
#147326,#147327,#147328,#147329,#147330,#147331,#147332,#147333,#147334,
#147335,#147336,#147337,#147338,#147339,#147340,#147341,#147342,#147343,
#147344,#147345,#147346,#147347,#147348,#147349,#147350,#147351,#147352,
#147353,#147354,#147355,#147356,#147357,#147358,#147359,#147360,#147361,
#147362,#147363,#147364,#147365,#147366,#147367,#147368,#147369,#147370,
#147371,#147372,#147373,#147374,#147375,#147376,#147377,#147378,#147379,
#147380,#147381,#147382,#147383,#147384,#147385,#147386,#147387,#147388,
#147389,#147390,#147391,#147392,#147393,#147394,#147395,#147396,#147397,
#147398,#147399,#147400,#147401,#147402,#147403,#147404,#147405,#147406,
#147407,#147408,#147409,#147410,#147411,#147412,#147413,#147414,#147415,
#147416,#147417,#147418,#147419,#147420,#147421,#147422,#147423,#147424,
#147425,#147426,#147427,#147428,#147429,#147430,#147431,#147432,#147433,
#147434,#147435,#147436,#147437,#147438,#147439,#147440,#147441,#147442,
#147443,#147444,#147445,#147446,#147447,#147448,#147449,#147450,#147451,
#147452,#147453,#147454,#147455,#147456,#147457,#147458,#147459,#147460,
#147461,#147462,#147463,#147464,#147465,#147466,#147467,#147468,#147469,
#147470,#147471,#147472,#147473,#147474,#147475,#147476,#147477,#147478,
#147479,#147480,#147481,#147482,#147483,#147484,#147485,#147486,#147487,
#147488,#147489,#147490,#147491,#147492,#147493,#147494,#147495,#147496,
#147497,#147498,#147499,#147500,#147501,#147502,#147503,#147504,#147505,
#147506,#147507,#147508,#147509,#147510,#147511,#147512,#147513,#147514,
#147515,#147516,#147517,#147518,#147519,#147520,#147521,#147522,#147523,
#147524,#147525,#147526,#147527,#147528,#147529,#147530,#147531,#147532,
#147533,#147534,#147535,#147536,#147537,#147538,#147539,#147540,#147541,
#147542,#147543,#147544,#147545,#147546,#147547,#147548,#147549,#147550,
#147551,#147552,#147553,#147554,#147555,#147556,#147557,#147558,#147559,
#147560,#147561,#147562,#147563,#147564,#147565,#147566,#147567,#147568,
#147569,#147570,#147571,#147572,#147573,#147574,#147575,#147576,#147577,
#147578,#147579,#147580,#147581,#147582,#147583,#147584,#147585,#147586,
#147587,#147588,#147589,#147590,#147591,#147592,#147593,#147594,#147595,
#147596,#147597,#147598,#147599,#147600,#147601,#147602,#147603,#147604,
#147605,#147606,#147607,#147608,#147609,#147610,#147611,#147612,#147613,
#147614,#147615,#147616,#147617,#147618,#147619,#147620,#147621,#147622,
#147623,#147624,#147625,#147626,#147627,#147628,#147629,#147630,#147631,
#147632,#147633,#147634,#147635,#147636,#147637,#147638,#147639,#147640,
#147641,#147642,#147643,#147644,#147645,#147646,#147647,#147648,#147649,
#147650,#147651,#147652,#147653,#147654,#147655,#147656,#147657,#147658,
#147659,#147660,#147661,#147662,#147663,#147664,#147665,#147666,#147667,
#147668,#147669,#147670,#147671,#147672,#147673,#147674,#147675,#147676,
#147677,#147678,#147679,#147680,#147681,#147682,#147683,#147684,#147685,
#147686,#147687,#147688,#147689,#147690,#147691,#147692,#147693,#147694,
#147695,#147696,#147697,#147698,#147699,#147700,#147701,#147702,#147703,
#147704,#147705,#147706,#147707,#147708,#147709,#147710,#147711,#147712,
#147713,#147714,#147715,#147716,#147717,#147718,#147719,#147720,#147721,
#147722,#147723,#147724,#147725,#147726,#147727,#147728,#147729,#147730,
#147731,#147732,#147733,#147734,#147735,#147736,#147737,#147738,#147739,
#147740,#147741,#147742,#147743,#147744,#147745,#147746,#147747,#147748,
#147749,#147750,#147751,#147752,#147753,#147754,#147755,#147756,#147757,
#147758,#147759,#147760,#147761,#147762,#147763,#147764,#147765,#147766,
#147767,#147768,#147769,#147770,#147771,#147772,#147773,#147774,#147775,
#147776,#147777,#147778,#147779,#147780,#147781,#147782,#147783,#147784,
#147785,#147786,#147787,#147788,#147789,#147790,#147791,#147792,#147793,
#147794,#147795,#147796,#147797,#147798,#147799,#147800,#147801,#147802,
#147803,#147804,#147805,#147806,#147807,#147808,#147809,#147810,#147811,
#147812,#147813,#147814,#147815,#147816,#147817,#147818,#147819,#147820,
#147821,#147822,#147823,#147824,#147825,#147826,#147827,#147828,#147829,
#147830,#147831,#147832,#147833,#147834,#147835,#147836,#147837,#147838,
#147839,#147840,#147841,#147842,#147843,#147844,#147845,#147846,#147847,
#147848,#147849,#147850,#147851,#147852,#147853,#147854,#147855,#147856,
#147857,#147858,#147859,#147860,#147861,#147862,#147863,#147864,#147865,
#147866,#147867,#147868,#147869,#147870,#147871,#147872,#147873,#147874,
#147875,#147876,#147877,#147878,#147879,#147880,#147881,#147882,#147883,
#147884,#147885,#147886,#147887,#147888,#147889,#147890,#147891,#147892,
#147893,#147894,#147895,#147896,#147897,#147898,#147899,#147900,#147901,
#147902,#147903,#147904,#147905,#147906,#147907,#147908,#147909,#147910,
#147911,#147912,#147913,#147914,#147915,#147916,#147917,#147918,#147919,
#147920,#147921,#147922,#147923,#147924,#147925,#147926,#147927,#147928,
#147929,#147930,#147931,#147932,#147933,#147934,#147935,#147936,#147937,
#147938,#147939,#147940,#147941,#147942,#147943,#147944,#147945,#147946,
#147947,#147948,#147949,#147950,#147951,#147952,#147953,#147954,#147955,
#147956,#147957,#147958,#147959,#147960,#147961,#147962,#147963,#147964,
#147965,#147966,#147967,#147968,#147969,#147970,#147971,#147972,#147973,
#147974,#147975,#147976,#147977,#147978,#147979,#147980,#147981,#147982,
#147983,#147984,#147985,#147986,#147987,#147988,#147989,#147990,#147991,
#147992,#147993,#147994,#147995,#147996,#147997,#147998,#147999,#148000,
#148001,#148002,#148003,#148004,#148005,#148006,#148007,#148008,#148009,
#148010,#148011,#148012,#148013,#148014,#148015,#148016,#148017,#148018,
#148019,#148020,#148021,#148022,#148023,#148024,#148025,#148026,#148027,
#148028,#148029,#148030,#148031,#148032,#148033,#148034,#148035,#148036,
#148037,#148038,#148039,#148040,#148041,#148042,#148043,#148044,#148045,
#148046,#148047,#148048,#148049,#148050,#148051,#148052,#148053,#148054,
#148055,#148056,#148057,#148058,#148059,#148060,#148061,#148062,#148063,
#148064,#148065,#148066,#148067,#148068,#148069,#148070,#148071,#148072,
#148073,#148074,#148075,#148076,#148077,#148078,#148079,#148080,#148081,
#148082,#148083,#148084,#148085,#148086,#148087,#148088,#148089,#148090,
#148091,#148092,#148093,#148094,#148095,#148096,#148097,#148098,#148099,
#148100,#148101,#148102,#148103,#148104,#148105,#148106,#148107,#148108,
#148109,#148110,#148111,#148112,#148113,#148114,#148115,#148116,#148117,
#148118,#148119,#148120,#148121,#148122,#148123,#148124,#148125,#148126,
#148127,#148128,#148129,#148130,#148131,#148132,#148133,#148134,#148135,
#148136,#148137,#148138,#148139,#148140,#148141,#148142,#148143,#148144,
#148145,#148146,#148147,#148148,#148149,#148150,#148151,#148152,#148153,
#148154,#148155,#148156,#148157,#148158,#148159,#148160,#148161,#148162,
#148163,#148164,#148165,#148166,#148167,#148168,#148169,#148170,#148171,
#148172,#148173,#148174,#148175,#148176,#148177,#148178,#148179,#148180,
#148181,#148182,#148183,#148184,#148185,#148186,#148187,#148188,#148189,
#148190,#148191,#148192,#148193,#148194,#148195,#148196,#148197,#148198,
#148199,#148200,#148201,#148202,#148203,#148204,#148205,#148206,#148207,
#148208,#148209,#148210,#148211,#148212,#148213,#148214,#148215,#148216,
#148217,#148218,#148219,#148220,#148221,#148222,#148223,#148224,#148225,
#148226,#148227,#148228,#148229,#148230,#148231,#148232,#148233,#148234,
#148235,#148236,#148237,#148238,#148239,#148240,#148241,#148242,#148243,
#148244,#148245,#148246,#148247,#148248,#148249,#148250,#148251,#148252,
#148253,#148254,#148255,#148256,#148257,#148258,#148259,#148260,#148261,
#148262,#148263,#148264,#148265,#148266,#148267,#148268,#148269,#148270,
#148271,#148272,#148273,#148274,#148275,#148276,#148277,#148278,#148279,
#148280,#148281,#148282,#148283,#148284,#148285,#148286,#148287,#148288,
#148289,#148290,#148291,#148292,#148293,#148294,#148295,#148296,#148297,
#148298,#148299,#148300,#148301,#148302,#148303,#148304,#148305,#148306,
#148307,#148308,#148309,#148310,#148311,#148312,#148313,#148314,#148315,
#148316,#148317,#148318,#148319,#148320,#148321,#148322,#148323,#148324,
#148325,#148326,#148327,#148328,#148329,#148330,#148331,#148332,#148333,
#148334,#148335,#148336,#148337,#148338,#148339,#148340,#148341,#148342,
#148343,#148344,#148345,#148346,#148347,#148348,#148349,#148350,#148351,
#148352,#148353,#148354,#148355,#148356,#148357,#148358,#148359,#148360,
#148361,#148362,#148363,#148364,#148365,#148366,#148367,#148368,#148369,
#148370,#148371,#148372,#148373,#148374,#148375,#148376,#148377,#148378,
#148379,#148380,#148381,#148382,#148383,#148384,#148385,#148386,#148387,
#148388,#148389,#148390,#148391,#148392,#148393,#148394,#148395,#148396,
#148397,#148398,#148399,#148400,#148401,#148402,#148403,#148404,#148405,
#148406,#148407,#148408,#148409,#148410,#148411,#148412,#148413,#148414,
#148415,#148416,#148417,#148418,#148419,#148420,#148421,#148422,#148423,
#148424,#148425,#148426,#148427,#148428,#148429,#148430,#148431,#148432,
#148433,#148434,#148435,#148436,#148437,#148438,#148439,#148440,#148441,
#148442,#148443,#148444,#148445,#148446,#148447,#148448,#148449,#148450,
#148451,#148452,#148453,#148454,#148455,#148456,#148457,#148458,#148459,
#148460,#148461,#148462,#148463,#148464,#148465,#148466,#148467,#148468,
#148469,#148470,#148471,#148472,#148473,#148474,#148475,#148476,#148477,
#148478,#148479,#148480,#148481,#148482,#148483,#148484,#148485,#148486,
#148487,#148488,#148489,#148490,#148491,#148492,#148493,#148494,#148495,
#148496,#148497,#148498,#148499,#148500,#148501,#148502,#148503,#148504,
#148505,#148506,#148507,#148508,#148509,#148510,#148511,#148512,#148513,
#148514,#148515,#148516,#148517,#148518,#148519,#148520,#148521,#148522,
#148523,#148524,#148525,#148526,#148527,#148528,#148529,#148530,#148531,
#148532,#148533,#148534,#148535,#148536,#148537,#148538,#148539,#148540,
#148541,#148542,#148543,#148544,#148545,#148546,#148547,#148548,#148549,
#148550,#148551,#148552,#148553,#148554,#148555,#148556,#148557,#148558,
#148559,#148560,#148561,#148562,#148563,#148564,#148565,#148566,#148567,
#148568,#148569,#148570,#148571,#148572,#148573,#148574,#148575,#148576,
#148577,#148578,#148579,#148580,#148581,#148582,#148583,#148584,#148585,
#148586,#148587,#148588,#148589,#148590,#148591,#148592,#148593,#148594,
#148595,#148596,#148597,#148598,#148599,#148600,#148601,#148602,#148603,
#148604,#148605,#148606,#148607,#148608,#148609,#148610,#148611,#148612,
#148613,#148614,#148615,#148616,#148617,#148618,#148619,#148620,#148621,
#148622,#148623,#148624,#148625,#148626,#148627,#148628,#148629,#148630,
#148631,#148632,#148633,#148634,#148635,#148636,#148637,#148638,#148639,
#148640,#148641,#148642,#148643,#148644,#148645,#148646,#148647,#148648,
#148649,#148650,#148651,#148652,#148653,#148654,#148655,#148656,#148657,
#148658,#148659,#148660,#148661,#148662,#148663,#148664,#148665,#148666,
#148667,#148668,#148669,#148670,#148671,#148672,#148673,#148674,#148675,
#148676,#148677,#148678,#148679,#148680,#148681,#148682,#148683,#148684,
#148685,#148686,#148687,#148688,#148689,#148690,#148691,#148692,#148693,
#148694,#148695,#148696,#148697,#148698,#148699,#148700,#148701,#148702,
#148703,#148704,#148705,#148706,#148707,#148708,#148709,#148710,#148711,
#148712,#148713,#148714,#148715,#148716,#148717,#148718,#148719,#148720,
#148721,#148722,#148723,#148724,#148725),(#148726,#148727,#148728,#148729,
#148730,#148731,#148732,#148733,#148734,#148735,#148736,#148737,#148738,
#148739,#148740,#148741,#148742,#148743,#148744,#148745,#148746,#148747,
#148748,#148749,#148750,#148751,#148752,#148753,#148754,#148755,#148756,
#148757,#148758,#148759,#148760,#148761,#148762,#148763,#148764,#148765,
#148766,#148767,#148768,#148769,#148770,#148771,#148772,#148773,#148774,
#148775,#148776,#148777,#148778,#148779,#148780,#148781,#148782,#148783,
#148784,#148785,#148786,#148787,#148788,#148789,#148790,#148791,#148792,
#148793,#148794,#148795,#148796,#148797,#148798,#148799,#148800,#148801,
#148802,#148803,#148804,#148805,#148806,#148807,#148808,#148809,#148810,
#148811,#148812,#148813,#148814,#148815,#148816,#148817,#148818,#148819,
#148820,#148821,#148822,#148823,#148824,#148825,#148826,#148827,#148828,
#148829,#148830,#148831,#148832,#148833,#148834,#148835,#148836,#148837,
#148838,#148839,#148840,#148841,#148842,#148843,#148844,#148845,#148846,
#148847,#148848,#148849,#148850,#148851,#148852,#148853,#148854,#148855,
#148856,#148857,#148858,#148859,#148860,#148861,#148862,#148863,#148864,
#148865,#148866,#148867,#148868,#148869,#148870,#148871,#148872,#148873,
#148874,#148875,#148876,#148877,#148878,#148879,#148880,#148881,#148882,
#148883,#148884,#148885,#148886,#148887,#148888,#148889,#148890,#148891,
#148892,#148893,#148894,#148895,#148896,#148897,#148898,#148899,#148900,
#148901,#148902,#148903,#148904,#148905,#148906,#148907,#148908,#148909,
#148910,#148911,#148912,#148913,#148914,#148915,#148916,#148917,#148918,
#148919,#148920,#148921,#148922,#148923,#148924,#148925,#148926,#148927,
#148928,#148929,#148930,#148931,#148932,#148933,#148934,#148935,#148936,
#148937,#148938,#148939,#148940,#148941,#148942,#148943,#148944,#148945,
#148946,#148947,#148948,#148949,#148950,#148951,#148952,#148953,#148954,
#148955,#148956,#148957,#148958,#148959,#148960,#148961,#148962,#148963,
#148964,#148965,#148966,#148967,#148968,#148969,#148970,#148971,#148972,
#148973,#148974,#148975,#148976,#148977,#148978,#148979,#148980,#148981,
#148982,#148983,#148984,#148985,#148986,#148987,#148988,#148989,#148990,
#148991,#148992,#148993,#148994,#148995,#148996,#148997,#148998,#148999,
#149000,#149001,#149002,#149003,#149004,#149005,#149006,#149007,#149008,
#149009,#149010,#149011,#149012,#149013,#149014,#149015,#149016,#149017,
#149018,#149019,#149020,#149021,#149022,#149023,#149024,#149025,#149026,
#149027,#149028,#149029,#149030,#149031,#149032,#149033,#149034,#149035,
#149036,#149037,#149038,#149039,#149040,#149041,#149042,#149043,#149044,
#149045,#149046,#149047,#149048,#149049,#149050,#149051,#149052,#149053,
#149054,#149055,#149056,#149057,#149058,#149059,#149060,#149061,#149062,
#149063,#149064,#149065,#149066,#149067,#149068,#149069,#149070,#149071,
#149072,#149073,#149074,#149075,#149076,#149077,#149078,#149079,#149080,
#149081,#149082,#149083,#149084,#149085,#149086,#149087,#149088,#149089,
#149090,#149091,#149092,#149093,#149094,#149095,#149096,#149097,#149098,
#149099,#149100,#149101,#149102,#149103,#149104,#149105,#149106,#149107,
#149108,#149109,#149110,#149111,#149112,#149113,#149114,#149115,#149116,
#149117,#149118,#149119,#149120,#149121,#149122,#149123,#149124,#149125,
#149126,#149127,#149128,#149129,#149130,#149131,#149132,#149133,#149134,
#149135,#149136,#149137,#149138,#149139,#149140,#149141,#149142,#149143,
#149144,#149145,#149146,#149147,#149148,#149149,#149150,#149151,#149152,
#149153,#149154,#149155,#149156,#149157,#149158,#149159,#149160,#149161,
#149162,#149163,#149164,#149165,#149166,#149167,#149168,#149169,#149170,
#149171,#149172,#149173,#149174,#149175,#149176,#149177,#149178,#149179,
#149180,#149181,#149182,#149183,#149184,#149185,#149186,#149187,#149188,
#149189,#149190,#149191,#149192,#149193,#149194,#149195,#149196,#149197,
#149198,#149199,#149200,#149201,#149202,#149203,#149204,#149205,#149206,
#149207,#149208,#149209,#149210,#149211,#149212,#149213,#149214,#149215,
#149216,#149217,#149218,#149219,#149220,#149221,#149222,#149223,#149224,
#149225,#149226,#149227,#149228,#149229,#149230,#149231,#149232,#149233,
#149234,#149235,#149236,#149237,#149238,#149239,#149240,#149241,#149242,
#149243,#149244,#149245,#149246,#149247,#149248,#149249,#149250,#149251,
#149252,#149253,#149254,#149255,#149256,#149257,#149258,#149259,#149260,
#149261,#149262,#149263,#149264,#149265,#149266,#149267,#149268,#149269,
#149270,#149271,#149272,#149273,#149274,#149275,#149276,#149277,#149278,
#149279,#149280,#149281,#149282,#149283,#149284,#149285,#149286,#149287,
#149288,#149289,#149290,#149291,#149292,#149293,#149294,#149295,#149296,
#149297,#149298,#149299,#149300,#149301,#149302,#149303,#149304,#149305,
#149306,#149307,#149308,#149309,#149310,#149311,#149312,#149313,#149314,
#149315,#149316,#149317,#149318,#149319,#149320,#149321,#149322,#149323,
#149324,#149325,#149326,#149327,#149328,#149329,#149330,#149331,#149332,
#149333,#149334,#149335,#149336,#149337,#149338,#149339,#149340,#149341,
#149342,#149343,#149344,#149345,#149346,#149347,#149348,#149349,#149350,
#149351,#149352,#149353,#149354,#149355,#149356,#149357,#149358,#149359,
#149360,#149361,#149362,#149363,#149364,#149365,#149366,#149367,#149368,
#149369,#149370,#149371,#149372,#149373,#149374,#149375,#149376,#149377,
#149378,#149379,#149380,#149381,#149382,#149383,#149384,#149385,#149386,
#149387,#149388,#149389,#149390,#149391,#149392,#149393,#149394,#149395,
#149396,#149397,#149398,#149399,#149400,#149401,#149402,#149403,#149404,
#149405,#149406,#149407,#149408,#149409,#149410,#149411,#149412,#149413,
#149414,#149415,#149416,#149417,#149418,#149419,#149420,#149421,#149422,
#149423,#149424,#149425,#149426,#149427,#149428,#149429,#149430,#149431,
#149432,#149433,#149434,#149435,#149436,#149437,#149438,#149439,#149440,
#149441,#149442,#149443,#149444,#149445,#149446,#149447,#149448,#149449,
#149450,#149451,#149452,#149453,#149454,#149455,#149456,#149457,#149458,
#149459,#149460,#149461,#149462,#149463,#149464,#149465,#149466,#149467,
#149468,#149469,#149470,#149471,#149472,#149473,#149474,#149475,#149476,
#149477,#149478,#149479,#149480,#149481,#149482,#149483,#149484,#149485,
#149486,#149487,#149488,#149489,#149490,#149491,#149492,#149493,#149494,
#149495,#149496,#149497,#149498,#149499,#149500,#149501,#149502,#149503,
#149504,#149505,#149506,#149507,#149508,#149509,#149510,#149511,#149512,
#149513,#149514,#149515,#149516,#149517,#149518,#149519,#149520,#149521,
#149522,#149523,#149524,#149525,#149526,#149527,#149528,#149529,#149530,
#149531,#149532,#149533,#149534,#149535,#149536,#149537,#149538,#149539,
#149540,#149541,#149542,#149543,#149544,#149545,#149546,#149547,#149548,
#149549,#149550,#149551,#149552,#149553,#149554,#149555,#149556,#149557,
#149558,#149559,#149560,#149561,#149562,#149563,#149564,#149565,#149566,
#149567,#149568,#149569,#149570,#149571,#149572,#149573,#149574,#149575,
#149576,#149577,#149578,#149579,#149580,#149581,#149582,#149583,#149584,
#149585,#149586,#149587,#149588,#149589,#149590,#149591,#149592,#149593,
#149594,#149595,#149596,#149597,#149598,#149599,#149600,#149601,#149602,
#149603,#149604,#149605,#149606,#149607,#149608,#149609,#149610,#149611,
#149612,#149613,#149614,#149615,#149616,#149617,#149618,#149619,#149620,
#149621,#149622,#149623,#149624,#149625,#149626,#149627,#149628,#149629,
#149630,#149631,#149632,#149633,#149634,#149635,#149636,#149637,#149638,
#149639,#149640,#149641,#149642,#149643,#149644,#149645,#149646,#149647,
#149648,#149649,#149650,#149651,#149652,#149653,#149654,#149655,#149656,
#149657,#149658,#149659,#149660,#149661,#149662,#149663,#149664,#149665,
#149666,#149667,#149668,#149669,#149670,#149671,#149672,#149673,#149674,
#149675,#149676,#149677,#149678,#149679,#149680,#149681,#149682,#149683,
#149684,#149685,#149686,#149687,#149688,#149689,#149690,#149691,#149692,
#149693,#149694,#149695,#149696,#149697,#149698,#149699,#149700,#149701,
#149702,#149703,#149704,#149705,#149706,#149707,#149708,#149709,#149710,
#149711,#149712,#149713,#149714,#149715,#149716,#149717,#149718,#149719,
#149720,#149721,#149722,#149723,#149724,#149725,#149726,#149727,#149728,
#149729,#149730,#149731,#149732,#149733,#149734,#149735,#149736,#149737,
#149738,#149739,#149740,#149741,#149742,#149743,#149744,#149745,#149746,
#149747,#149748,#149749,#149750,#149751,#149752,#149753,#149754,#149755,
#149756,#149757,#149758,#149759,#149760,#149761,#149762,#149763,#149764,
#149765,#149766,#149767,#149768,#149769,#149770,#149771,#149772,#149773,
#149774,#149775,#149776,#149777,#149778,#149779,#149780,#149781,#149782,
#149783,#149784,#149785,#149786,#149787,#149788,#149789,#149790,#149791,
#149792,#149793,#149794,#149795,#149796,#149797,#149798,#149799,#149800,
#149801,#149802,#149803,#149804,#149805,#149806,#149807,#149808,#149809,
#149810,#149811,#149812,#149813,#149814,#149815,#149816,#149817,#149818,
#149819,#149820,#149821,#149822,#149823,#149824,#149825,#149826,#149827,
#149828,#149829,#149830,#149831,#149832,#149833,#149834,#149835,#149836,
#149837,#149838,#149839,#149840,#149841,#149842,#149843,#149844,#149845,
#149846,#149847,#149848,#149849,#149850,#149851,#149852,#149853,#149854,
#149855,#149856,#149857,#149858,#149859,#149860,#149861,#149862,#149863,
#149864,#149865,#149866,#149867,#149868,#149869,#149870,#149871,#149872,
#149873,#149874,#149875,#149876,#149877,#149878,#149879,#149880,#149881,
#149882,#149883,#149884,#149885,#149886,#149887,#149888,#149889,#149890,
#149891,#149892,#149893,#149894,#149895,#149896,#149897,#149898,#149899,
#149900,#149901,#149902,#149903,#149904,#149905,#149906,#149907,#149908,
#149909,#149910,#149911,#149912,#149913,#149914,#149915,#149916,#149917,
#149918,#149919,#149920,#149921,#149922,#149923,#149924,#149925,#149926,
#149927,#149928,#149929,#149930,#149931,#149932,#149933,#149934,#149935,
#149936,#149937,#149938,#149939,#149940,#149941,#149942,#149943,#149944,
#149945,#149946,#149947,#149948,#149949,#149950,#149951,#149952,#149953,
#149954,#149955,#149956,#149957,#149958,#149959,#149960,#149961,#149962,
#149963,#149964,#149965,#149966,#149967,#149968,#149969,#149970,#149971,
#149972,#149973,#149974,#149975,#149976,#149977,#149978,#149979,#149980,
#149981,#149982,#149983,#149984,#149985,#149986,#149987,#149988,#149989,
#149990,#149991,#149992,#149993,#149994,#149995,#149996,#149997,#149998,
#149999,#150000,#150001,#150002,#150003,#150004,#150005,#150006,#150007,
#150008,#150009,#150010,#150011,#150012,#150013,#150014,#150015,#150016,
#150017,#150018,#150019,#150020,#150021,#150022,#150023,#150024,#150025,
#150026,#150027,#150028,#150029,#150030,#150031,#150032,#150033,#150034,
#150035,#150036,#150037,#150038,#150039,#150040,#150041,#150042,#150043,
#150044,#150045,#150046,#150047,#150048,#150049,#150050,#150051,#150052,
#150053,#150054,#150055,#150056,#150057,#150058,#150059,#150060,#150061,
#150062,#150063,#150064,#150065,#150066,#150067,#150068,#150069,#150070,
#150071,#150072,#150073,#150074,#150075,#150076,#150077,#150078,#150079,
#150080,#150081,#150082,#150083,#150084,#150085,#150086,#150087,#150088,
#150089,#150090,#150091,#150092,#150093,#150094,#150095,#150096,#150097,
#150098,#150099,#150100,#150101,#150102,#150103,#150104,#150105,#150106,
#150107,#150108,#150109,#150110,#150111,#150112,#150113,#150114,#150115,
#150116,#150117,#150118,#150119,#150120,#150121,#150122,#150123,#150124,
#150125,#150126,#150127,#150128,#150129,#150130,#150131,#150132,#150133,
#150134,#150135,#150136,#150137,#150138,#150139,#150140,#150141,#150142,
#150143,#150144,#150145,#150146,#150147,#150148,#150149,#150150,#150151,
#150152,#150153,#150154,#150155,#150156,#150157,#150158,#150159,#150160,
#150161,#150162,#150163,#150164,#150165,#150166,#150167,#150168,#150169,
#150170,#150171,#150172,#150173,#150174,#150175,#150176,#150177,#150178,
#150179,#150180,#150181,#150182,#150183,#150184,#150185,#150186,#150187,
#150188,#150189,#150190,#150191,#150192,#150193,#150194,#150195,#150196,
#150197,#150198,#150199,#150200,#150201,#150202,#150203,#150204,#150205,
#150206,#150207,#150208,#150209,#150210,#150211,#150212,#150213,#150214,
#150215,#150216,#150217,#150218,#150219,#150220,#150221,#150222,#150223,
#150224,#150225,#150226,#150227,#150228,#150229,#150230,#150231,#150232,
#150233,#150234,#150235,#150236,#150237,#150238,#150239,#150240,#150241,
#150242,#150243,#150244,#150245,#150246,#150247,#150248,#150249,#150250,
#150251,#150252,#150253,#150254,#150255,#150256,#150257,#150258,#150259,
#150260,#150261,#150262,#150263,#150264,#150265,#150266,#150267,#150268,
#150269,#150270,#150271,#150272,#150273,#150274,#150275,#150276,#150277,
#150278,#150279,#150280,#150281,#150282,#150283,#150284,#150285,#150286,
#150287,#150288,#150289,#150290,#150291,#150292,#150293,#150294,#150295,
#150296,#150297,#150298,#150299,#150300,#150301,#150302,#150303,#150304,
#150305,#150306,#150307,#150308,#150309,#150310,#150311,#150312,#150313,
#150314,#150315,#150316,#150317,#150318,#150319,#150320,#150321,#150322,
#150323,#150324,#150325,#150326,#150327,#150328,#150329,#150330,#150331,
#150332,#150333,#150334,#150335,#150336,#150337,#150338,#150339,#150340,
#150341,#150342,#150343,#150344,#150345,#150346,#150347,#150348,#150349,
#150350,#150351,#150352,#150353,#150354,#150355,#150356,#150357,#150358,
#150359,#150360,#150361,#150362,#150363,#150364,#150365,#150366,#150367,
#150368,#150369,#150370,#150371,#150372,#150373,#150374,#150375,#150376,
#150377,#150378,#150379,#150380,#150381,#150382,#150383,#150384,#150385,
#150386,#150387,#150388,#150389,#150390,#150391,#150392,#150393,#150394,
#150395,#150396,#150397,#150398,#150399,#150400,#150401,#150402,#150403,
#150404,#150405,#150406,#150407,#150408,#150409,#150410,#150411,#150412,
#150413,#150414,#150415,#150416,#150417,#150418,#150419,#150420,#150421,
#150422,#150423,#150424,#150425,#150426,#150427,#150428,#150429,#150430,
#150431,#150432,#150433,#150434,#150435,#150436,#150437,#150438,#150439,
#150440,#150441,#150442,#150443,#150444,#150445,#150446,#150447,#150448,
#150449,#150450,#150451,#150452,#150453,#150454,#150455,#150456,#150457,
#150458,#150459,#150460,#150461,#150462,#150463,#150464,#150465,#150466,
#150467,#150468,#150469,#150470,#150471,#150472,#150473,#150474,#150475,
#150476,#150477,#150478,#150479,#150480,#150481,#150482,#150483,#150484,
#150485,#150486,#150487,#150488,#150489,#150490,#150491,#150492,#150493,
#150494,#150495,#150496,#150497,#150498,#150499,#150500,#150501,#150502,
#150503,#150504,#150505,#150506,#150507,#150508,#150509,#150510,#150511,
#150512,#150513,#150514,#150515,#150516,#150517,#150518,#150519,#150520,
#150521,#150522,#150523,#150524,#150525,#150526,#150527,#150528,#150529,
#150530,#150531,#150532,#150533,#150534,#150535,#150536,#150537,#150538,
#150539,#150540,#150541,#150542,#150543,#150544,#150545,#150546,#150547,
#150548,#150549,#150550,#150551,#150552,#150553,#150554,#150555,#150556,
#150557,#150558,#150559,#150560,#150561,#150562,#150563,#150564,#150565,
#150566,#150567,#150568,#150569,#150570,#150571,#150572,#150573,#150574,
#150575,#150576,#150577,#150578,#150579,#150580,#150581,#150582,#150583,
#150584,#150585,#150586,#150587,#150588,#150589,#150590,#150591,#150592,
#150593,#150594,#150595,#150596,#150597,#150598,#150599,#150600,#150601,
#150602,#150603,#150604,#150605,#150606,#150607,#150608,#150609,#150610,
#150611,#150612,#150613,#150614,#150615,#150616,#150617,#150618,#150619,
#150620,#150621,#150622,#150623,#150624,#150625,#150626,#150627,#150628,
#150629,#150630,#150631,#150632,#150633,#150634,#150635,#150636,#150637,
#150638,#150639,#150640,#150641,#150642,#150643,#150644,#150645,#150646,
#150647,#150648,#150649,#150650,#150651,#150652,#150653,#150654,#150655,
#150656,#150657,#150658,#150659,#150660,#150661,#150662,#150663,#150664,
#150665,#150666,#150667,#150668,#150669,#150670,#150671,#150672,#150673,
#150674,#150675,#150676,#150677,#150678,#150679,#150680,#150681,#150682,
#150683,#150684,#150685,#150686,#150687,#150688,#150689,#150690,#150691,
#150692,#150693,#150694,#150695,#150696,#150697,#150698,#150699,#150700,
#150701,#150702,#150703,#150704,#150705,#150706,#150707,#150708,#150709,
#150710,#150711,#150712,#150713,#150714,#150715,#150716,#150717,#150718,
#150719,#150720,#150721,#150722,#150723,#150724,#150725,#150726,#150727,
#150728,#150729,#150730,#150731,#150732,#150733,#150734,#150735,#150736,
#150737,#150738,#150739,#150740,#150741,#150742,#150743,#150744,#150745,
#150746,#150747,#150748,#150749,#150750,#150751,#150752,#150753,#150754,
#150755,#150756,#150757,#150758,#150759,#150760,#150761,#150762,#150763,
#150764,#150765,#150766,#150767,#150768,#150769,#150770,#150771,#150772,
#150773,#150774,#150775,#150776),(#150777,#150778,#150779,#150780,#150781,
#150782,#150783,#150784,#150785,#150786,#150787,#150788,#150789,#150790,
#150791,#150792,#150793,#150794,#150795,#150796,#150797,#150798,#150799,
#150800,#150801,#150802,#150803,#150804,#150805,#150806,#150807,#150808,
#150809,#150810,#150811,#150812,#150813,#150814,#150815,#150816,#150817,
#150818,#150819,#150820,#150821,#150822,#150823,#150824,#150825,#150826,
#150827,#150828,#150829,#150830,#150831,#150832,#150833,#150834,#150835,
#150836,#150837,#150838,#150839,#150840,#150841,#150842,#150843,#150844,
#150845,#150846,#150847,#150848,#150849,#150850,#150851,#150852,#150853,
#150854,#150855,#150856,#150857,#150858,#150859,#150860,#150861,#150862,
#150863,#150864,#150865,#150866,#150867,#150868,#150869,#150870,#150871,
#150872,#150873,#150874,#150875,#150876,#150877,#150878,#150879,#150880,
#150881,#150882,#150883,#150884,#150885,#150886,#150887,#150888,#150889,
#150890,#150891,#150892,#150893,#150894,#150895,#150896,#150897,#150898,
#150899,#150900,#150901,#150902,#150903,#150904,#150905,#150906,#150907,
#150908,#150909,#150910,#150911,#150912,#150913,#150914,#150915,#150916,
#150917,#150918,#150919,#150920,#150921,#150922,#150923,#150924,#150925,
#150926,#150927,#150928,#150929,#150930,#150931,#150932,#150933,#150934,
#150935,#150936,#150937,#150938,#150939,#150940,#150941,#150942,#150943,
#150944,#150945,#150946,#150947,#150948,#150949,#150950,#150951,#150952,
#150953,#150954,#150955,#150956,#150957,#150958,#150959,#150960,#150961,
#150962,#150963,#150964,#150965,#150966,#150967,#150968,#150969,#150970,
#150971,#150972,#150973,#150974,#150975,#150976,#150977,#150978,#150979,
#150980,#150981,#150982,#150983,#150984,#150985,#150986,#150987,#150988,
#150989,#150990,#150991,#150992,#150993,#150994,#150995,#150996,#150997,
#150998,#150999,#151000,#151001,#151002,#151003,#151004,#151005,#151006,
#151007,#151008,#151009,#151010,#151011,#151012,#151013,#151014,#151015,
#151016,#151017,#151018,#151019,#151020,#151021,#151022,#151023,#151024,
#151025,#151026,#151027,#151028,#151029,#151030,#151031,#151032,#151033,
#151034,#151035,#151036,#151037,#151038,#151039,#151040,#151041,#151042,
#151043,#151044,#151045,#151046,#151047,#151048,#151049,#151050,#151051,
#151052,#151053,#151054,#151055,#151056,#151057,#151058,#151059,#151060,
#151061,#151062,#151063,#151064,#151065,#151066,#151067,#151068,#151069,
#151070,#151071,#151072,#151073,#151074,#151075,#151076,#151077,#151078,
#151079,#151080,#151081,#151082,#151083,#151084,#151085,#151086,#151087,
#151088,#151089,#151090,#151091,#151092,#151093,#151094,#151095,#151096,
#151097,#151098,#151099,#151100,#151101,#151102,#151103,#151104,#151105,
#151106,#151107,#151108,#151109,#151110,#151111,#151112,#151113,#151114,
#151115,#151116,#151117,#151118,#151119,#151120,#151121,#151122,#151123,
#151124,#151125,#151126,#151127,#151128,#151129,#151130,#151131,#151132,
#151133,#151134,#151135,#151136,#151137,#151138,#151139,#151140,#151141,
#151142,#151143,#151144,#151145,#151146,#151147,#151148,#151149,#151150,
#151151,#151152,#151153,#151154,#151155,#151156,#151157,#151158,#151159,
#151160,#151161,#151162,#151163,#151164,#151165,#151166,#151167,#151168,
#151169,#151170,#151171,#151172,#151173,#151174,#151175,#151176,#151177,
#151178,#151179,#151180,#151181,#151182,#151183,#151184,#151185,#151186,
#151187,#151188,#151189,#151190,#151191,#151192,#151193,#151194,#151195,
#151196,#151197,#151198,#151199,#151200,#151201,#151202,#151203,#151204,
#151205,#151206,#151207,#151208,#151209,#151210,#151211,#151212,#151213,
#151214,#151215,#151216,#151217,#151218,#151219,#151220,#151221,#151222,
#151223,#151224,#151225,#151226,#151227,#151228,#151229,#151230,#151231,
#151232,#151233,#151234,#151235,#151236,#151237,#151238,#151239,#151240,
#151241,#151242,#151243,#151244,#151245,#151246,#151247,#151248,#151249,
#151250,#151251,#151252,#151253,#151254,#151255,#151256,#151257,#151258,
#151259,#151260,#151261,#151262,#151263,#151264,#151265,#151266,#151267,
#151268,#151269,#151270,#151271,#151272,#151273,#151274,#151275,#151276,
#151277,#151278,#151279,#151280,#151281,#151282,#151283,#151284,#151285,
#151286,#151287,#151288,#151289,#151290,#151291,#151292,#151293,#151294,
#151295,#151296,#151297,#151298,#151299,#151300,#151301,#151302,#151303,
#151304,#151305,#151306,#151307,#151308,#151309,#151310,#151311,#151312,
#151313,#151314,#151315,#151316,#151317,#151318,#151319,#151320,#151321,
#151322,#151323,#151324,#151325,#151326,#151327,#151328,#151329,#151330,
#151331,#151332,#151333,#151334,#151335,#151336,#151337,#151338,#151339,
#151340,#151341,#151342,#151343,#151344,#151345,#151346,#151347,#151348,
#151349,#151350,#151351,#151352,#151353,#151354,#151355,#151356,#151357,
#151358,#151359,#151360,#151361,#151362,#151363,#151364,#151365,#151366,
#151367,#151368,#151369,#151370,#151371,#151372,#151373,#151374,#151375,
#151376,#151377,#151378,#151379,#151380,#151381,#151382,#151383,#151384,
#151385,#151386,#151387,#151388,#151389,#151390,#151391,#151392,#151393,
#151394,#151395,#151396,#151397,#151398,#151399,#151400,#151401,#151402,
#151403,#151404,#151405,#151406,#151407,#151408,#151409,#151410,#151411,
#151412,#151413,#151414,#151415,#151416,#151417,#151418,#151419,#151420,
#151421,#151422,#151423,#151424,#151425,#151426,#151427,#151428,#151429,
#151430,#151431,#151432,#151433,#151434,#151435,#151436,#151437,#151438,
#151439,#151440,#151441,#151442,#151443,#151444,#151445,#151446,#151447,
#151448,#151449,#151450,#151451,#151452,#151453,#151454,#151455,#151456,
#151457,#151458,#151459,#151460,#151461,#151462,#151463,#151464,#151465,
#151466,#151467,#151468,#151469,#151470,#151471,#151472,#151473,#151474,
#151475,#151476,#151477,#151478,#151479,#151480,#151481,#151482,#151483,
#151484,#151485,#151486,#151487,#151488,#151489,#151490,#151491,#151492,
#151493,#151494,#151495,#151496,#151497,#151498,#151499,#151500,#151501,
#151502,#151503,#151504,#151505,#151506,#151507,#151508,#151509,#151510,
#151511,#151512,#151513,#151514,#151515,#151516,#151517,#151518,#151519,
#151520,#151521,#151522,#151523,#151524,#151525,#151526,#151527,#151528,
#151529,#151530,#151531,#151532,#151533,#151534,#151535,#151536,#151537,
#151538,#151539,#151540,#151541,#151542,#151543,#151544,#151545,#151546,
#151547,#151548,#151549,#151550,#151551,#151552,#151553,#151554,#151555,
#151556,#151557,#151558,#151559,#151560,#151561,#151562,#151563,#151564,
#151565,#151566,#151567,#151568,#151569,#151570,#151571,#151572,#151573,
#151574,#151575,#151576,#151577,#151578,#151579,#151580,#151581,#151582,
#151583,#151584,#151585,#151586,#151587,#151588,#151589,#151590,#151591,
#151592,#151593,#151594,#151595,#151596,#151597,#151598,#151599,#151600,
#151601,#151602,#151603,#151604,#151605,#151606,#151607,#151608,#151609,
#151610,#151611,#151612,#151613,#151614,#151615,#151616,#151617,#151618,
#151619,#151620,#151621,#151622,#151623,#151624,#151625,#151626,#151627,
#151628,#151629,#151630,#151631,#151632,#151633,#151634,#151635,#151636,
#151637,#151638,#151639,#151640,#151641,#151642,#151643,#151644,#151645,
#151646,#151647,#151648,#151649,#151650,#151651,#151652,#151653,#151654,
#151655,#151656,#151657,#151658,#151659,#151660,#151661,#151662,#151663,
#151664,#151665,#151666,#151667,#151668,#151669,#151670,#151671,#151672,
#151673,#151674,#151675,#151676,#151677,#151678,#151679,#151680,#151681,
#151682,#151683,#151684,#151685,#151686,#151687,#151688,#151689,#151690,
#151691,#151692,#151693,#151694,#151695,#151696,#151697,#151698,#151699,
#151700,#151701,#151702,#151703,#151704,#151705,#151706,#151707,#151708,
#151709,#151710,#151711,#151712,#151713,#151714,#151715,#151716,#151717,
#151718,#151719,#151720,#151721,#151722,#151723,#151724,#151725,#151726,
#151727,#151728,#151729,#151730,#151731,#151732,#151733,#151734,#151735,
#151736,#151737,#151738,#151739,#151740,#151741,#151742,#151743,#151744,
#151745,#151746,#151747,#151748,#151749,#151750,#151751,#151752,#151753,
#151754,#151755,#151756,#151757,#151758,#151759,#151760,#151761,#151762,
#151763,#151764,#151765,#151766,#151767,#151768,#151769,#151770,#151771,
#151772,#151773,#151774,#151775,#151776,#151777,#151778,#151779,#151780,
#151781,#151782,#151783,#151784,#151785,#151786,#151787,#151788,#151789,
#151790,#151791,#151792,#151793,#151794,#151795,#151796,#151797,#151798,
#151799,#151800,#151801,#151802,#151803,#151804,#151805,#151806,#151807,
#151808,#151809,#151810,#151811,#151812,#151813,#151814,#151815,#151816,
#151817,#151818,#151819,#151820,#151821,#151822,#151823,#151824,#151825,
#151826,#151827,#151828,#151829,#151830,#151831,#151832,#151833,#151834,
#151835,#151836,#151837,#151838,#151839,#151840,#151841,#151842,#151843,
#151844,#151845,#151846,#151847,#151848,#151849,#151850,#151851,#151852,
#151853,#151854,#151855,#151856,#151857,#151858,#151859,#151860,#151861,
#151862,#151863,#151864,#151865,#151866,#151867,#151868,#151869,#151870,
#151871,#151872,#151873,#151874,#151875,#151876,#151877,#151878,#151879,
#151880,#151881,#151882,#151883,#151884,#151885,#151886,#151887,#151888,
#151889,#151890,#151891,#151892,#151893,#151894,#151895,#151896,#151897,
#151898,#151899,#151900,#151901,#151902,#151903,#151904,#151905,#151906,
#151907,#151908,#151909,#151910,#151911,#151912,#151913,#151914,#151915,
#151916,#151917,#151918,#151919,#151920,#151921,#151922,#151923,#151924,
#151925,#151926,#151927,#151928,#151929,#151930,#151931,#151932,#151933,
#151934,#151935,#151936,#151937,#151938,#151939,#151940,#151941,#151942,
#151943,#151944,#151945,#151946,#151947,#151948,#151949,#151950,#151951,
#151952,#151953,#151954,#151955,#151956,#151957,#151958,#151959,#151960,
#151961,#151962,#151963,#151964,#151965,#151966,#151967,#151968,#151969,
#151970,#151971,#151972,#151973,#151974,#151975,#151976,#151977,#151978,
#151979,#151980,#151981,#151982,#151983,#151984,#151985,#151986,#151987,
#151988,#151989,#151990,#151991,#151992,#151993,#151994,#151995,#151996,
#151997,#151998,#151999,#152000,#152001,#152002,#152003,#152004,#152005,
#152006,#152007,#152008,#152009,#152010,#152011,#152012,#152013,#152014,
#152015,#152016,#152017,#152018,#152019,#152020,#152021,#152022,#152023,
#152024,#152025,#152026,#152027,#152028,#152029,#152030,#152031,#152032,
#152033,#152034,#152035,#152036,#152037,#152038,#152039,#152040,#152041,
#152042,#152043,#152044,#152045,#152046,#152047,#152048,#152049,#152050,
#152051,#152052,#152053,#152054,#152055,#152056,#152057,#152058,#152059,
#152060,#152061,#152062,#152063,#152064,#152065,#152066,#152067,#152068,
#152069,#152070,#152071,#152072,#152073,#152074,#152075,#152076,#152077,
#152078,#152079,#152080,#152081,#152082,#152083,#152084,#152085,#152086,
#152087,#152088,#152089,#152090,#152091,#152092,#152093,#152094,#152095,
#152096,#152097,#152098,#152099,#152100,#152101,#152102,#152103,#152104,
#152105,#152106,#152107,#152108,#152109,#152110,#152111,#152112,#152113,
#152114,#152115,#152116,#152117,#152118,#152119,#152120,#152121,#152122,
#152123,#152124,#152125,#152126,#152127,#152128,#152129,#152130,#152131,
#152132,#152133,#152134,#152135,#152136,#152137,#152138,#152139,#152140,
#152141,#152142,#152143,#152144,#152145,#152146,#152147,#152148,#152149,
#152150,#152151,#152152,#152153,#152154,#152155,#152156,#152157,#152158,
#152159,#152160,#152161,#152162,#152163,#152164,#152165,#152166,#152167,
#152168,#152169,#152170,#152171,#152172,#152173,#152174,#152175,#152176,
#152177,#152178,#152179,#152180,#152181,#152182,#152183,#152184,#152185,
#152186,#152187,#152188,#152189,#152190,#152191,#152192,#152193,#152194,
#152195,#152196,#152197,#152198,#152199,#152200,#152201,#152202,#152203,
#152204,#152205,#152206,#152207,#152208,#152209,#152210,#152211,#152212,
#152213,#152214,#152215,#152216,#152217,#152218,#152219,#152220,#152221,
#152222,#152223,#152224,#152225,#152226,#152227,#152228,#152229,#152230,
#152231,#152232,#152233,#152234,#152235,#152236,#152237,#152238,#152239,
#152240,#152241,#152242,#152243,#152244,#152245,#152246,#152247,#152248,
#152249,#152250,#152251,#152252,#152253,#152254,#152255,#152256,#152257,
#152258,#152259,#152260,#152261,#152262,#152263,#152264,#152265,#152266,
#152267,#152268,#152269,#152270,#152271,#152272,#152273,#152274,#152275,
#152276,#152277,#152278,#152279,#152280,#152281,#152282,#152283,#152284,
#152285,#152286,#152287,#152288,#152289,#152290,#152291,#152292,#152293,
#152294,#152295,#152296,#152297,#152298,#152299,#152300,#152301,#152302,
#152303,#152304,#152305,#152306,#152307,#152308,#152309,#152310,#152311,
#152312,#152313,#152314,#152315,#152316,#152317,#152318,#152319,#152320,
#152321,#152322,#152323,#152324,#152325,#152326,#152327,#152328,#152329,
#152330,#152331,#152332,#152333,#152334,#152335,#152336,#152337,#152338,
#152339,#152340,#152341,#152342,#152343,#152344,#152345,#152346,#152347,
#152348,#152349,#152350,#152351,#152352,#152353,#152354,#152355,#152356,
#152357,#152358,#152359,#152360,#152361,#152362,#152363,#152364,#152365,
#152366,#152367,#152368,#152369,#152370,#152371,#152372,#152373,#152374,
#152375,#152376,#152377,#152378,#152379,#152380,#152381,#152382,#152383,
#152384,#152385,#152386,#152387,#152388,#152389,#152390,#152391,#152392,
#152393,#152394,#152395,#152396,#152397,#152398,#152399,#152400,#152401,
#152402,#152403,#152404,#152405,#152406,#152407,#152408,#152409,#152410,
#152411,#152412,#152413,#152414,#152415,#152416,#152417,#152418,#152419,
#152420,#152421,#152422,#152423,#152424,#152425,#152426,#152427,#152428,
#152429,#152430,#152431,#152432,#152433,#152434,#152435,#152436,#152437,
#152438,#152439,#152440,#152441,#152442,#152443,#152444,#152445,#152446,
#152447,#152448,#152449,#152450,#152451,#152452,#152453,#152454,#152455,
#152456,#152457,#152458,#152459,#152460,#152461,#152462,#152463,#152464,
#152465,#152466,#152467,#152468,#152469,#152470,#152471,#152472,#152473,
#152474,#152475,#152476,#152477,#152478,#152479,#152480,#152481,#152482,
#152483,#152484,#152485,#152486,#152487,#152488,#152489,#152490,#152491,
#152492,#152493,#152494,#152495,#152496,#152497,#152498,#152499,#152500,
#152501,#152502,#152503,#152504,#152505,#152506,#152507,#152508,#152509,
#152510,#152511,#152512,#152513,#152514,#152515,#152516,#152517,#152518,
#152519,#152520,#152521,#152522,#152523,#152524,#152525,#152526,#152527,
#152528,#152529,#152530,#152531,#152532,#152533,#152534,#152535,#152536,
#152537,#152538,#152539,#152540,#152541,#152542,#152543,#152544,#152545,
#152546,#152547,#152548,#152549,#152550,#152551,#152552,#152553,#152554,
#152555,#152556,#152557,#152558,#152559,#152560,#152561,#152562,#152563,
#152564,#152565,#152566,#152567,#152568,#152569,#152570,#152571,#152572,
#152573,#152574,#152575,#152576,#152577,#152578,#152579,#152580,#152581,
#152582,#152583,#152584,#152585,#152586,#152587,#152588,#152589,#152590,
#152591,#152592,#152593,#152594,#152595,#152596,#152597,#152598,#152599,
#152600,#152601,#152602,#152603,#152604,#152605,#152606,#152607,#152608,
#152609,#152610,#152611,#152612,#152613,#152614,#152615,#152616,#152617,
#152618,#152619,#152620,#152621,#152622,#152623,#152624,#152625,#152626,
#152627,#152628,#152629,#152630,#152631,#152632,#152633,#152634,#152635,
#152636,#152637,#152638,#152639,#152640,#152641,#152642,#152643,#152644,
#152645,#152646,#152647,#152648,#152649,#152650,#152651,#152652,#152653,
#152654,#152655,#152656,#152657,#152658,#152659,#152660,#152661,#152662,
#152663,#152664,#152665,#152666,#152667,#152668,#152669,#152670,#152671,
#152672,#152673,#152674,#152675,#152676,#152677,#152678,#152679,#152680,
#152681,#152682,#152683,#152684,#152685,#152686,#152687,#152688,#152689,
#152690,#152691,#152692,#152693,#152694,#152695,#152696,#152697,#152698,
#152699,#152700,#152701,#152702,#152703,#152704,#152705,#152706,#152707,
#152708,#152709,#152710,#152711,#152712,#152713,#152714,#152715,#152716,
#152717,#152718,#152719,#152720,#152721,#152722,#152723,#152724,#152725,
#152726,#152727,#152728,#152729,#152730,#152731,#152732,#152733,#152734,
#152735,#152736,#152737,#152738,#152739,#152740,#152741,#152742,#152743,
#152744,#152745,#152746,#152747,#152748,#152749,#152750,#152751,#152752,
#152753,#152754,#152755,#152756,#152757,#152758,#152759,#152760,#152761,
#152762,#152763,#152764,#152765,#152766,#152767,#152768,#152769,#152770,
#152771,#152772,#152773,#152774,#152775,#152776,#152777,#152778,#152779,
#152780,#152781,#152782,#152783,#152784,#152785,#152786,#152787,#152788,
#152789,#152790,#152791,#152792,#152793,#152794,#152795,#152796,#152797,
#152798,#152799,#152800,#152801,#152802,#152803,#152804,#152805,#152806,
#152807,#152808,#152809,#152810,#152811,#152812,#152813,#152814,#152815,
#152816,#152817,#152818,#152819,#152820,#152821,#152822,#152823,#152824,
#152825,#152826,#152827)),.UNSPECIFIED.,.T.,.F.,.F.)
B_SPLINE_SURFACE_WITH_KNOTS((3,2,2,2,3),(4,1,1,1,1,1,1,1,1,1,1,1,1,1,1,
1,1,1,1,1,1,1,1,1,1,1,1,1,1,1,1,1,1,1,1,1,1,1,1,1,1,1,1,1,1,1,1,1,1,1,1,
1,1,1,1,1,1,1,1,1,1,1,1,1,1,1,1,1,1,1,1,1,1,1,1,1,1,1,1,1,1,1,1,1,1,1,1,
1,1,1,1,1,1,1,1,1,1,1,1,1,1,1,1,1,1,1,1,1,1,1,1,1,1,1,1,1,1,1,1,1,1,1,1,
1,1,1,1,1,1,1,1,1,1,1,1,1,1,1,1,1,1,1,1,1,1,1,1,1,1,1,1,1,1,1,1,1,1,1,1,
1,1,1,1,1,1,1,1,1,1,1,1,1,1,1,1,1,1,1,1,1,1,1,1,1,1,1,1,1,1,1,1,1,1,1,1,
1,1,1,1,1,1,1,1,1,1,1,1,1,1,1,1,1,1,1,1,1,1,1,1,1,1,1,1,1,1,1,1,1,1,1,1,
1,1,1,1,1,1,1,1,1,1,1,1,1,1,1,1,1,1,1,1,1,1,1,1,1,1,1,1,1,1,1,1,1,1,1,1,
1,1,1,1,1,1,1,1,1,1,1,1,1,1,1,1,1,1,1,1,1,1,1,1,1,1,1,1,1,1,1,1,1,1,1,1,
1,1,1,1,1,1,1,1,1,1,1,1,1,1,1,1,1,1,1,1,1,1,1,1,1,1,1,1,1,1,1,1,1,1,1,1,
1,1,1,1,1,1,1,1,1,1,1,1,1,1,1,1,1,1,1,1,1,1,1,1,1,1,1,1,1,1,1,1,1,1,1,1,
1,1,1,1,1,1,1,1,1,1,1,1,1,1,1,1,1,1,1,1,1,1,1,1,1,1,1,1,1,1,1,1,1,1,1,1,
1,1,1,1,1,1,1,1,1,1,1,1,1,1,1,1,1,1,1,1,1,1,1,1,1,1,1,1,1,1,1,1,1,1,1,1,
1,1,1,1,1,1,1,1,1,1,1,1,1,1,1,1,1,1,1,1,1,1,1,1,1,1,1,1,1,1,1,1,1,1,1,1,
1,1,1,1,1,1,1,1,1,1,1,1,1,1,1,1,1,1,1,1,1,1,1,1,1,1,1,1,1,1,1,1,1,1,1,1,
1,1,1,1,1,1,1,1,1,1,1,1,1,1,1,1,1,1,1,1,1,1,1,1,1,1,1,1,1,1,1,1,1,1,1,1,
1,1,1,1,1,1,1,1,1,1,1,1,1,1,1,1,1,1,1,1,1,1,1,1,1,1,1,1,1,1,1,1,1,1,1,1,
1,1,1,1,1,1,1,1,1,1,1,1,1,1,1,1,1,1,1,1,1,1,1,1,1,1,1,1,1,1,1,1,1,1,1,1,
1,1,1,1,1,1,1,1,1,1,1,1,1,1,1,1,1,1,1,1,1,1,1,1,1,1,1,1,1,1,1,1,1,1,1,1,
1,1,1,1,1,1,1,1,1,1,1,1,1,1,1,1,1,1,1,1,1,1,1,1,1,1,1,1,1,1,1,1,1,1,1,1,
1,1,1,1,1,1,1,1,1,1,1,1,1,1,1,1,1,1,1,1,1,1,1,1,1,1,1,1,1,1,1,1,1,1,1,1,
1,1,1,1,1,1,1,1,1,1,1,1,1,1,1,1,1,1,1,1,1,1,1,1,1,1,1,1,1,1,1,1,1,1,1,1,
1,1,1,1,1,1,1,1,1,1,1,1,1,1,1,1,1,1,1,1,1,1,1,1,1,1,1,1,1,1,1,1,1,1,1,1,
1,1,1,1,1,1,1,1,1,1,1,1,1,1,1,1,1,1,1,1,1,1,1,1,1,1,1,1,1,1,1,1,1,1,1,1,
1,1,1,1,1,1,1,1,1,1,1,1,1,1,1,1,1,1,1,1,1,1,1,1,1,1,1,1,1,1,1,1,1,1,1,1,
1,1,1,1,1,1,1,1,1,1,1,1,1,1,1,1,1,1,1,1,1,1,1,1,1,1,1,1,1,1,1,1,1,1,1,1,
1,1,1,1,1,1,1,1,1,1,1,1,1,1,1,1,1,1,1,1,1,1,1,1,1,1,1,1,1,1,1,1,1,1,1,1,
1,1,1,1,1,1,1,1,1,1,1,1,1,1,1,1,1,1,1,1,1,1,1,1,1,1,1,1,1,1,1,1,1,1,1,1,
1,1,1,1,1,1,1,1,1,1,1,1,1,1,1,1,1,1,1,1,1,1,1,1,1,1,1,1,1,1,1,1,1,1,1,1,
1,1,1,1,1,1,1,1,1,1,1,1,1,1,1,1,1,1,1,1,1,1,1,1,1,1,1,1,1,1,1,1,1,1,1,1,
1,1,1,1,1,1,1,1,1,1,1,1,1,1,1,1,1,1,1,1,1,1,1,1,1,1,1,1,1,1,1,1,1,1,1,1,
1,1,1,1,1,1,1,1,1,1,1,1,1,1,1,1,1,1,1,1,1,1,1,1,1,1,1,1,1,1,1,1,1,1,1,1,
1,1,1,1,1,1,1,1,1,1,1,1,1,1,1,1,1,1,1,1,1,1,1,1,1,1,1,1,1,1,1,1,1,1,1,1,
1,1,1,1,1,1,1,1,1,1,1,1,1,1,1,1,1,1,1,1,1,1,1,1,1,1,1,1,1,1,1,1,1,1,1,1,
1,1,1,1,1,1,1,1,1,1,1,1,1,1,1,1,1,1,1,1,1,1,1,1,1,1,1,1,1,1,1,1,1,1,1,1,
1,1,1,1,1,1,1,1,1,1,1,1,1,1,1,1,1,1,1,1,1,1,1,1,1,1,1,1,1,1,1,1,1,1,1,1,
1,1,1,1,1,1,1,1,1,1,1,1,1,1,1,1,1,1,1,1,1,1,1,1,1,1,1,1,1,1,1,1,1,1,1,1,
1,1,1,1,1,1,1,1,1,1,1,1,1,1,1,1,1,1,1,1,1,1,1,1,1,1,1,1,1,1,1,1,1,1,1,1,
1,1,1,1,1,1,1,1,1,1,1,1,1,1,1,1,1,1,1,1,1,1,1,1,1,1,1,1,1,1,1,1,1,1,1,1,
1,1,1,1,1,1,1,1,1,1,1,1,1,1,1,1,1,1,1,1,1,1,1,1,1,1,1,1,1,1,1,1,1,1,1,1,
1,1,1,1,1,1,1,1,1,1,1,1,1,1,1,1,1,1,1,1,1,1,1,1,1,1,1,1,1,1,1,1,1,1,1,1,
1,1,1,1,1,1,1,1,1,1,1,1,1,1,1,1,1,1,1,1,1,1,1,1,1,1,1,1,1,1,1,1,1,1,1,1,
1,1,1,1,1,1,1,1,1,1,1,1,1,1,1,1,1,1,1,1,1,1,1,1,1,1,1,1,1,1,1,1,1,1,1,1,
1,1,1,1,1,1,1,1,1,1,1,1,1,1,1,1,1,1,1,1,1,1,1,1,1,1,1,1,1,1,1,1,1,1,1,1,
1,1,1,1,1,1,1,1,1,1,1,1,1,1,1,1,1,1,1,1,1,1,1,1,1,1,1,1,1,1,1,1,1,1,1,1,
1,1,1,1,1,1,1,1,1,1,1,1,1,1,1,1,1,1,1,1,1,1,1,1,1,1,1,1,1,1,1,1,1,1,1,1,
1,1,1,1,1,1,1,1,1,1,1,1,1,1,1,1,1,1,1,1,1,1,1,1,1,1,1,1,1,1,1,1,1,1,1,1,
1,1,1,1,1,1,1,1,1,1,1,1,1,1,1,1,1,1,1,1,1,1,1,1,1,1,1,1,1,1,1,1,1,1,1,1,
1,1,1,1,1,1,1,1,1,1,1,1,1,1,1,1,1,1,1,1,1,1,1,1,1,1,1,1,1,1,1,1,1,1,1,1,
1,1,1,1,1,1,1,1,1,1,1,1,1,1,1,1,1,1,1,1,1,1,1,1,1,1,1,1,1,1,1,1,1,1,1,1,
1,1,1,1,1,1,1,1,1,1,1,1,1,1,1,1,1,1,1,1,1,1,1,1,1,1,1,1,1,1,1,1,1,1,1,1,
1,1,1,1,1,1,1,1,1,1,1,1,1,1,1,1,1,1,1,1,1,1,1,1,1,1,1,1,1,1,1,1,1,1,1,1,
1,1,1,1,1,1,1,1,1,1,1,1,1,1,1,1,1,1,1,1,1,1,1,1,1,1,1,1,1,1,1,1,1,1,1,1,
1,1,1,1,1,1,1,1,1,1,1,1,1,1,1,1,1,1,1,1,1,1,1,1,1,1,1,1,1,1,1,1,1,1,1,1,
1,1,1,1,1,1,1,1,1,1,1,1,1,1,1,1,1,1,1,1,1,1,1,1,1,1,1,1,1,1,1,1,1,1,1,1,
1,1,1,1,1,1,1,1,1,1,1,1,1,1,1,1,1,1,1,1,1,1,1,1,1,1,1,1,1,1,1,1,1,1,1,1,
1,1,1,1,1,1,1,1,1,1,1,1,1,1,1,1,1,1,1,1,1,1,1,1,1,1,1,1,1,1,1,1,1,1,1,1,
1,1,1,1,1,1,1,1,1,1,1,1,1,1,1,1,1,4),(0.,0.117809724509617,0.235619449019234,
0.353429173528852,0.471238898038469),(0.,0.01797683372391,0.286633051710584,
0.555289278308216,0.823945516665782,1.09260176953922,1.36125803873948,1.62991432588463,
1.89857063164012,2.16722695661301,2.43588330050525,2.70453966304674,2.9731960431531,
3.24185243981471,3.51050885133453,3.77916527610465,4.04782171198515,4.31647815691489,
4.58513460847725,4.85379106430677,5.12244752187208,5.39110397865606,5.65976043217153,
5.92841687990537,6.19707331956994,6.46572974881596,6.73438616570634,7.00304256821933,
7.2716989549161,7.5403553242696,7.809011675483,8.07766800769526,8.34632432089157,
8.61498061505147,8.8836368910788,9.15229314997201,9.4209493936865,9.68960562442157,
9.95826184531348,10.226918059948,10.4955742727586,10.7642304884925,11.0328867113173,
11.3015429448574,11.5701991918227,11.8388554546081,12.1075117346518,12.3761680332469,
12.6448243507434,12.9134806874637,13.1821370428496,13.450793416388,13.7194498067883,
13.9881062128412,14.2567626326955,14.5254190645885,14.7940755062772,15.0627319555912,
15.3313884100611,15.6000448672586,15.8687013246492,16.1373577797,16.4060142299691,
16.6746706729765,16.9433271065265,17.2119835283531,17.4806399366567,17.7492963295502,
18.0179527057767,18.286609063996,18.555265403637,18.8239217240786,19.0925780255742,
19.3612343083975,19.6298905737625,19.898546823017,20.1672030584666,20.4358592827168,
20.7045154992928,20.973171712245,21.2418279262962,21.5104841459723,21.7791403749736,
22.0477966165324,22.316452872948,22.585109146262,22.8537654375589,23.1224217478187,
23.3910780770929,23.6597344254327,23.9283907920352,24.197047176159,24.4657035763222,
24.7343599911301,25.0030164185931,25.2716728568073,25.5403293034427,25.8089857562333,
26.0776422126729,26.3462986702843,26.6149551265448,26.8836115789212,27.1522680250308,
27.4209244624423,27.6895808890659,27.9582373027346,28.2268937018004,28.4955500845261,
28.7642064498512,29.0328627966379,29.3015191245544,29.5701754332357,29.838831723217,
30.1074879950829,30.3761442503694,30.6448004907916,30.9134567190168,31.1821129380756,
31.450769151893,31.7194253649682,31.9880815819663,32.2567378070174,32.5253940433706,
32.7940502938785,33.0627065604467,33.3313628447765,33.6000191476151,33.8686754696427,
34.1373318106287,34.405988170366,34.6746445478242,34.9433009420458,35.2119573513747,
35.480613774244,35.7492702085419,36.0179266522368,36.2865831029275,36.5552395582669,
36.8238960157264,37.0925524727952,37.3612089269773,37.6298653757534,37.8985218168153,
38.1671782477952,38.4358346667239,38.7044910715485,38.9731474607866,39.2418038328672,
39.5104601869391,39.7791165220837,40.0477728382212,40.3164291352602,40.5850854140292,
40.8537416754418,41.1223979213679,41.3910541539077,41.6597103761025,41.9283665914244,
42.1970228042084,42.4656790192,42.7343352406829,43.0029914723808,43.2716477171096,
43.540303977354,43.8089602546436,44.0776165503516,44.3462728649052,44.614929198697,
44.883585551232,45.1522419220568,45.4208983099307,45.6895547136931,45.9582111315299,
46.2268675617156,46.4955240020317,46.7641804503338,47.0328369041642,47.3014933611089,
47.5701498186329,47.8388062742058,48.107462725373,48.3761191696448,48.6447756048012,
48.9134320285537,49.1820884390673,49.4507448344197,49.7194012133072,49.9880575743413,
50.2567139168934,50.5253702402807,50.7940265446884,51.0626828303152,51.3313390982961,
51.5999953498901,51.8686515873141,52.1373078130706,52.4059640305862,52.6746202437936,
52.9432764573682,53.211932675918,53.480588903259,53.7492451427202,54.0179013967021,
54.2865576673334,54.5552139557853,54.823870263115,55.0925265894471,55.3611829348992,
55.6298392987282,55.8984956802486,56.1671520780245,56.4358084907065,56.7044649163381,
56.9731213530494,57.2417777985307,57.5104342505384,57.7790907065743,58.0477471641719,
58.3164036208043,58.5850600739368,58.8537165211707,59.1223729600609,59.39102938849,
59.6596858042645,59.9283422056975,60.1969985910129,60.4656549590995,60.7343113087676,
61.0029676396243,61.2716239512389,61.540280244075,61.808936518638,62.0775927763821,
62.3462490189291,62.6149052488546,62.8835614690812,63.1522176834332,63.4208738963055,
63.6895301124163,63.9581863359981,64.2268425704115,64.4954988186027,64.7641550825741,
65.0328113641112,65.3014676640435,65.5701239831253,65.8387803211949,66.1074366781083,
66.3760930528907,66.6447494446373,66.9134058517341,67.1820622726558,67.4507187053199,
67.7193751477252,67.988031597487,68.256688052277,68.5253445095709,68.7940009668648,
69.0626574216546,69.3313138714164,69.5999703138218,69.8686267464858,70.1372831674076,
70.4059395745042,70.6745959662509,70.9432523410334,71.2119086979469,71.4805650360164,
71.7492213550982,72.0178776550306,72.2865339365675,72.5551902005389,72.8238464487301,
73.0925026831433,73.3611589067251,73.6298151228357,73.8984713357081,74.1671275500599,
74.4357837702864,74.7044400002118,74.9730962427587,75.2417525005027,75.5104087750655,
75.7790650679015,76.047721379516,76.3163777103726,76.5850340600405,76.853690428127,
77.1223468134422,77.391003214875,77.6596596306495,77.9283160590784,78.1969724979684,
78.4656289452021,78.7342853983344,79.0029418549666,79.2715983125641,79.5402547685998,
79.8089112206075,80.0775676660886,80.3462241027997,80.6148805284312,80.8835369411131,
81.1521933388889,81.4208497204091,81.689506084238,81.9581624296899,82.2268187560219,
82.4954750633515,82.7641313518033,83.0327876224345,83.3014438764161,83.5701001158772,
83.838756343218,84.1074125617677,84.3760687753422,84.6447249885494,84.913381206065,
85.1820374318212,85.4506936692451,85.719349920839,85.9880061888197,86.2566624744465,
86.5253187788541,86.7939751022413,87.0626314447932,87.3312878058273,87.5999441847146,
87.8686005800667,88.1372569905802,88.4059134143327,88.6745698494889,88.9432262937606,
89.2118827449277,89.4805392005005,89.7491956580243,90.0178521149689,90.2865085687992,
90.5551650171012,90.8238214574172,91.0924778876028,91.3611343054394,91.6297907092016,
91.8984470970753,92.1671034679,92.4357598204347,92.7044161542264,92.9730724687798,
93.2417287644878,93.5103850417773,93.7790413020216,94.0476975467502,94.3163537784479,
94.5850099999307,94.8536662149221,95.1223224277061,95.390978643028,95.6596348652226,
95.9282910977624,96.1969473436883,96.4656036051009,96.7342598838697,97.0029161809086,
97.2715724970461,97.5402288321905,97.8088851862623,98.0775415583427,98.3461979475807,
98.6148543524051,98.8835107713336,99.1521672023136,99.4208236433754,99.6894800921513,
99.9581365463333,100.226793003402,100.495449460861,100.7641059162,101.032762366891,
101.301418810586,101.570075244884,101.838731667753,102.107388077082,102.376044471303,
102.644700848761,102.913357208498,103.182013549484,103.450669871511,103.71932617435,
103.98798245868,104.256638725248,104.525294975755,104.793951212108,105.062607437159,
105.331263654157,105.599919867233,105.86857608105,106.137232300108,106.405888528334,
106.674544768756,106.943201024042,107.211857295908,107.480513585889,107.74916989457,
108.017826222487,108.286482569273,108.555138934598,108.823795317324,109.09245171639,
109.361108130058,109.629764556682,109.898420994093,110.167077440202,110.435733892579,
110.704390348839,110.97304680645,111.24170326289,111.51035971568,111.779016162316,
112.04767260053,112.316329027993,112.5849854428,112.853641842963,113.122298227087,
113.39095459369,113.659610942029,113.928267271303,114.196923581563,114.46557987286,
114.734236146174,115.002892402589,115.271548644148,115.540204873149,115.808861092825,
116.077517306876,116.346173519828,116.614829736404,116.883485960654,117.152142196103,
117.420798445358,117.689454710722,117.958110993546,118.226767295041,118.495423615483,
118.764079955123,119.032736313343,119.301392689569,119.570049082462,119.838705490766,
120.107361912592,120.376018346142,120.644674789149,120.913331239418,121.181987694469,
121.45064415186,121.719300609057,121.987957063527,122.256613512841,122.525269954529,
122.793926386422,123.062582806276,123.331239212329,123.599895602729,123.868551976268,
124.137208331653,124.405864668374,124.67452098587,124.943177284465,125.211833564508,
125.480489827294,125.749146074259,126.017802307799,126.286458530624,126.555114746357,
126.823770959168,127.092427173802,127.361083394694,127.629739625429,127.898395869143,
128.167052128037,128.435708404064,128.704364698224,128.97302101142,129.241677343633,
129.510333694846,129.7789900642,130.047646450897,130.31630285341,130.5849592703,
130.853615699547,131.122272139211,131.390928586945,131.659585040461,131.928241497245,
132.19689795481,132.46555441064,132.734210862202,133.002867307132,133.271523743013,
133.540180167783,133.808836579303,134.077492975965,134.346149356071,134.614805718613,
134.883462062505,135.152118387478,135.420774693234,135.689430980379,135.958087249579,
136.226743502453,136.49539974081,136.76405596741,137.032712185392,137.301368398783,
137.570024612174,137.838680830155,138.107337056755,138.375993295112,138.644649547986,
138.913305817186,139.181962104332,139.450618410087,139.71927473506,139.987931078952,
140.256587441494,140.525243821601,140.793900218262,141.062556629782,141.331213054552,
141.599869490433,141.868525935363,142.137182386925,142.405838842755,142.67449530032,
142.943151757104,143.21180821062,143.480464658354,143.749121098019,144.017777527265,
144.286433944155,144.555090346668,144.823746733365,145.092403102719,145.361059453932,
145.629715786145,145.898372099341,146.167028393501,146.435684669529,146.704340928422,
146.972997172137,147.241653402872,147.510309623764,147.778965838398,148.047622051209,
148.316278266943,148.584934489768,148.853590723308,149.122246970274,149.390903233059,
149.659559513103,149.928215811698,150.196872129195,150.465528465915,150.734184821301,
151.00284119484,151.27149758524,151.540153991293,151.808810411148,152.077466843041,
152.34612328473,152.614779734044,152.883436188514,153.152092645711,153.420749103102,
153.689405558153,153.958062008422,154.22671845143,154.49537488498,154.764031306806,
155.03268771511,155.301344108004,155.57000048423,155.838656842449,156.107313182091,
156.375969502532,156.644625804028,156.913282086851,157.181938352216,157.450594601471,
157.719250836921,157.987907061171,158.256563277747,158.525219490699,158.793875704751,
159.062531924427,159.331188153428,159.599844394987,159.868500651403,160.137156924717,
160.405813216014,160.674469526274,160.943125855548,161.211782203888,161.480438570491,
161.749094954615,162.017751354778,162.286407769586,162.555064197049,162.823720635263,
163.092377081899,163.361033534689,163.629689991129,163.898346448741,164.167002905001,
164.435659357378,164.704315803488,164.972972240899,165.241628667523,165.510285081192,
165.778941480257,166.047597862983,166.316254228308,166.584910575095,166.853566903012,
167.122223211693,167.390879501675,167.659535773541,167.928192028827,168.19684826925,
168.465504497475,168.734160716534,169.002816930351,169.271473143427,169.540129360425,
169.808785585476,170.077441821829,170.346098072337,170.614754338905,170.883410623235,
171.152066926074,171.420723248102,171.689379589088,171.958035948825,172.226692326284,
172.495348720505,172.764005129834,173.032661552704,173.301317987002,173.569974430697,
173.838630881388,174.107287336727,174.375943794187,174.644600251255,174.913256705437,
175.181913154214,175.450569595276,175.719226026256,175.987882445184,176.256538850009,
176.525195239247,176.793851611328,177.0625079654,177.331164300545,177.599820616682,
177.868476913721,178.137133192491,178.405789453903,178.674445699829,178.943101932369,
179.211758154564,179.480414369886,179.74907058267,180.017726797662,180.286383019145,
180.555039250843,180.823695495572,181.092351755816,181.361008033106,181.629664328814,
181.898320643368,182.16697697716,182.435633329695,182.70428970052,182.972946088394,
183.241602492156,183.510258909993,183.778915340179,184.047571780495,184.316228228797,
184.584884682628,184.853541139572,185.122197597096,185.39085405267,185.659510503837,
185.928166948109,186.196823383265,186.465479807018,186.734136217531,187.002792612884,
187.271448991771,187.540105352806,187.808761695358,188.077418018745,188.346074323153,
188.61473060878,188.883386876761,189.152043128355,189.420699365779,189.689355591536,
189.958011809051,190.226668022259,190.495324235834,190.763980454383,191.032636681725,
191.301292921186,191.569949175168,191.838605445799,192.107261734251,192.375918041581,
192.644574367913,192.913230713365,193.181887077194,193.450543458715,193.719199856491,
193.987856269173,194.256512694805,194.525169131516,194.793825576997,195.062482029005,
195.331138485041,195.599794942639,195.868451399271,196.137107852404,196.405764299638,
196.674420738528,196.943077166957,197.211733582732,197.480389984165,197.749046369481,
198.017702737567,198.286359087236,198.555015418092,198.823671729707,199.092328022543,
199.360984297106,199.62964055485,199.898296797397,200.166953027323,200.43560924755,
200.704265461902,200.972921674774,201.241577890885,201.510234114467,201.77889034888,
202.047546597072,202.316202861043,202.584859142581,202.853515442513,203.122171761595,
203.390828099665,203.659484456579,203.928140831361,204.196797223108,204.465453630205,
204.734110051127,205.002766483791,205.271422926197,205.540079375959,205.808735830749,
206.077392288043,206.346048745337,206.614705200127,206.883361649889,207.152018092295,
207.420674524959,207.689330945881,207.957987352978,208.226643744725,208.495300119508,
208.763956476421,209.032612814491,209.301269133573,209.569925433505,209.838581715043,
210.107237979014,210.375894227206,210.644550461619,210.913206685201,211.181862901312,
211.450519114184,211.719175328536,211.987831548763,212.256487778689,212.525144021236,
212.79380027898,213.062456553543,213.331112846379,213.599769157994,213.868425488851,
214.137081838519,214.405738206606,214.674394591921,214.943050993354,215.211707409129,
215.480363837558,215.749020276448,216.017676723682,216.286333176815,216.554989633447,
216.823646091045,217.092302547081,217.360958999089,217.62961544457,217.898271881281,
218.166928306913,218.435584719595,218.704241117371,218.972897498892,219.241553862721,
219.510210208173,219.778866534505,220.047522841835,220.316179130287,220.584835400918,
220.8534916549,221.122147894361,221.390804121702,221.659460340252,221.928116553827,
222.196772767034,222.46542898455,222.734085210306,223.00274144773,223.271397699324,
223.540053967305,223.808710252932,224.07736655734,224.346022880728,224.61467922328,
224.883335584314,225.151991963201,225.420648358554,225.689304769068,225.95796119282,
226.226617627977,226.495274072249,226.763930523416,227.032586978989,227.301243436513,
227.569899893458,227.838556347288,228.10721279559,228.375869235907,228.644525666093,
228.913182083929,229.181838487692,229.450494875566,229.719151246391,229.987807598926,
230.256463932718,230.525120247271,230.79377654298,231.062432820269,231.331089080514,
231.599745325243,231.868401556941,232.137057778424,232.405713993415,232.674370206199,
232.943026421521,233.211682643716,233.480338876256,233.748995122182,234.017651383595,
234.286307662364,234.554963959403,234.823620275541,235.092276610685,235.360932964757,
235.629589336838,235.898245726076,236.166902130901,236.43555854983,236.70421498081,
236.972871421872,237.241527870648,237.51018432483,237.778840781899,238.047497239359,
238.316153694698,238.584810145389,238.853466589084,239.122123023382,239.390779446251,
239.65943585558,239.928092249802,240.19674862726,240.465404986998,240.734061327984,
241.002717650011,241.27137395285,241.54003023718,241.808686503748,242.077342754256,
242.345998990609,242.614655215661,242.883311432659,243.151967645734,243.420623859552,
243.68928007861,243.957936306836,244.226592547258,244.495248802545,244.763905074411,
245.032561364392,245.301217673074,245.56987400099,245.838530347777,246.107186713102,
246.375843095828,246.644499494894,246.913155908563,247.181812335186,247.450468772598,
247.719125218708,247.987781671084,248.256438127345,248.525094584956,248.793751041396,
249.062407494187,249.331063940822,249.599720379036,249.8683768065,250.137033221308,
250.405689621471,250.674346005595,250.943002372197,251.211658720537,251.480315049812,
251.748971360071,252.017627651368,252.286283924683,252.554940181098,252.823596422657,
253.092252651658,253.360908871335,253.629565085386,253.898221298338,254.166877514914,
254.435533739165,254.704189974614,254.972846223869,255.241502489234,255.510158772057,
255.778815073553,256.047471393995,256.316127733635,256.584784091854,256.85344046808,
257.122096860973,257.390753269276,257.659409691102,257.928066124652,258.196722567659,
258.465379017928,258.734035472978,259.002691930368,259.271348387566,259.540004842035,
259.808661291349,260.077317733037,260.345974164929,260.614630584783,260.883286990836,
261.151943381235,261.420599754774,261.689256110159,261.957912446879,262.226568764375,
262.49522506297,262.763881343014,263.032537605798,263.301193852763,263.569850086303,
263.838506309127,264.107162524861,264.375818737671,264.644474952305,264.913131173196,
265.181787403931,265.450443647645,265.719099906538,265.987756182565,266.256412476724,
266.52506878992,266.793725122132,267.062381473345,267.331037842698,267.599694229394,
267.868350631907,268.137007048797,268.405663478042,268.674319917706,268.94297636544,
269.211632818955,269.480289275739,269.748945733304,270.017602189133,270.286258640695,
270.554915085624,270.823571521504,271.092227946274,271.360884357793,271.629540754454,
271.89819713456,272.166853497101,272.435509840993,272.704166165965,272.97282247172,
273.241478758865,273.510135028065,273.778791280938,274.047447519295,274.316103745894,
274.584759963875,274.853416177266,275.122072390656,275.390728608637,275.659384835237,
275.928041073593,276.196697326466,276.465353595666,276.734009882811,277.002666188566,
277.271322513539,277.53997885743,277.808635219972,278.077291600077,278.345947996739,
278.614604408258,278.883260833028,279.151917268908,279.420573713837,279.689230165399,
279.957886621228,280.226543078793,280.495199535576,280.763855989092,281.032512436825,
281.301168876489,281.569825305735,281.838481722625,282.107138125138,282.375794511834,
282.644450881187,282.9131072324,283.181763564612,283.450419877808,283.719076171967,
283.987732447994,284.256388706887,284.525044950601,284.793701181336,285.062357402228,
285.331013616862,285.599669829672,285.868326045405,286.136982268229,286.405638501769,
286.674294748734,286.942951011519,287.211607291562,287.480263590157,287.748919907653,
288.017576244373,288.286232599758,288.554888973296,288.823545363696,289.092201769749,
289.360858189603,289.629514621495,289.898171063183,290.166827512497,290.435483966966,
290.704140424163,290.972796881554,291.241453336604,291.510109786873,291.77876622988,
292.047422663429,292.316079085255,292.584735493559,292.853391886452,293.122048262678,
293.390704620897,293.659360960537,293.928017280978,294.196673582474,294.465329865297,
294.733986130661,295.002642379915,295.271298615364,295.539954839614,295.808611056189,
296.077267269141,296.345923483192,296.614579702867,296.883235931868,297.151892173427,
297.420548429842,297.689204703155,297.957860994452,298.226517304711,298.495173633985,
298.763829982324,299.032486348927,299.30114273305,299.569799133212,299.83845554802,
300.107111975482,300.375768413696,300.644424860331,300.913081313121,301.181737769561,
301.450394227172,301.719050683432,301.987707135808,302.256363581917,302.525020019328,
302.793676445951,303.062332859619,303.330989258684,303.59964564141,303.868302006734,
304.136958353521,304.405614681437,304.674270990118,304.942927280098,305.211583551964,
305.48023980725,305.748896047671,306.017552275896,306.286208494954,306.554864708772,
306.823520921846,307.092177138844,307.360833363895,307.629489600247,307.898145850755,
308.166802117323,308.435458401652,308.70411470449,308.972771026517,309.241427367503,
309.51008372724,309.778740104698,310.047396498919,310.316052908247,310.584709331116,
310.853365765414,311.122022209108,311.390678659798,311.659335115137,311.927991572596,
312.196648029665,312.465304483846,312.733960932622,313.002617373684,313.271273804663,
313.539930223591,313.808586628416,314.077243017653,314.345899389733,314.614555743805,
314.883212078949,315.151868395086,315.420524692125,315.689180970894,315.957837232306,
316.226493478231,316.495149710771,316.763805932965,317.032462148286,317.30111836107,
317.569774576061,317.838430797543,318.107087029241,318.375743273969,318.644399534213,
318.913055811502,319.18171210721,319.450368421763,319.719024755555,319.987681108089,
320.256337478914,320.524993866787,320.793650270549,321.062306688385,321.33096311857,
321.599619558886,321.868276007188,322.136932461018,322.405588917962,322.674245375486,
322.942901831059,323.211558282225,323.480214726497,323.748871161653,324.017527585405,
324.286183995918,324.55484039127,324.823496770157,325.09215313119,325.360809473742,
325.629465797129,325.898122101536,326.166778387163,326.435434655143,326.704090906737,
326.97274714416,327.241403369916,327.510059587432,327.778715800638,328.047372014213,
328.316028232762,328.584684460102,328.853340699563,329.121996953545,329.390653224175,
329.659309512627,329.927965819956,330.196622146288,330.46527849174,330.733934855568,
331.002591237088,331.271247634863,331.539904047545,331.808560473176,332.077216909887,
332.345873355368,332.614529807375,332.883186263411,333.151842721008,333.42049917764,
333.689155630772,333.957812078005,334.226468516895,334.495124945324,334.763781361098,
335.03243776253,335.301094147845,335.569750515931,335.838406865599,336.107063196455,
336.375719508069,336.644375800905,336.913032075468,337.181688333211,337.450344575758,
337.719000805683,337.987657025909,338.256313240261,338.524969453133,338.793625669243,
339.062281892824,339.330938127237,339.599594375428,339.868250639399,340.136906920936,
340.405563220868,340.674219539949,340.942875878019,341.211532234932,341.480188609714,
341.74884500146,342.017501408557,342.286157829478,342.554814262142,342.823470704547,
343.092127154308,343.360783609098,343.629440066391,343.898096523685,344.166752978475,
344.435409428236,344.704065870641,344.972722303305,345.241378724226,345.510035131323,
345.778691523069,346.047347897851,346.316004254764,346.584660592834,346.853316911915,
347.121973211847,347.390629493384,347.659285757355,347.927942005546,348.196598239959,
348.46525446354,348.733910679651,349.002566892523,349.271223106874,349.5398793271,
349.808535557025,350.077191799572,350.345848057315,350.614504331878,350.883160624714,
351.151816936328,351.420473267184,351.689129616852,351.957785984938,352.226442370253,
352.495098771685,352.76375518746,353.032411615888,353.301068054778,353.569724502012,
353.838380955144,354.107037411776,354.375693869373,354.644350325408,354.913006777416,
355.181663222896,355.450319659607,355.718976085238,355.98763249792,356.256288895695,
356.524945277215,356.793601641044,357.062257986496,357.330914312827,357.599570620156,
357.868226908608,358.136883179239,358.40553943322,358.674195672681,358.942851900021,
359.211508118571,359.480164332145,359.748820545352,360.017476762867,360.286132988623,
360.554789226047,360.82344547764,361.09210174562,361.360758031247,361.629414335654,
361.898070659041,362.166727001593,362.435383362626,362.704039741513,362.972696136865,
363.241352547378,363.510008971131,363.778665406287,364.047321850558,364.315978301725,
364.584634757297,364.853291214821,365.121947671765,365.390604125595,365.659260573897,
365.927917014213,366.196573444398,366.465229862234,366.733886265996,367.002542653869,
367.271199024694,367.539855377228,367.808511711019,368.077168025573,368.34582432128,
368.614480598569,368.883136858813,369.151793103542,369.420449335239,369.689105556722,
369.957761771713,370.226417984496,370.495074199818,370.763730422012,371.032386654551,
371.301042900477,371.569699161889,371.838355440658,372.107011737697,372.375668053834,
372.644324388978,372.912980743049,373.18163711513,373.450293504367,373.718949909191,
373.98760632812,374.256262759099,374.524919200161,374.793575648936,375.062232103118,
375.330888560186,375.599545017646,375.868201472985,376.136857923675,376.40551436737,
376.674170801667,376.942827224536,377.211483633864,377.480140028085,377.748796405543,
378.01745276528,378.286109106266,378.554765428293,378.823421731131,379.092078015461,
379.360734282028,379.629390532536,379.898046768888,380.166702993939,380.435359210937,
380.704015424011,380.972671637828,381.241327856887,381.509984085112,381.778640325533,
382.047296580819,382.315952852685,382.584609142666,382.853265451347,383.121921779263,
383.390578126049,383.659234491374,383.927890874099,384.196547273165,384.465203686833,
384.733860113456,385.002516550867,385.271172996977,385.539829449352,385.808485905613,
386.077142363224,386.345798819663,386.614455272453,386.883111719088,387.151768157302,
387.420424584764,387.689080999572,387.957737399735,388.226393783858,388.49505015046,
388.7637064988,389.032362828074,389.301019138333,389.56967542963,389.838331702943,
390.106987959358,390.375644200917,390.644300429918,390.912956649593,391.181612863644,
391.450269076596,391.718925293171,391.987581517421,392.25623775287,392.524894002124,
392.793550267489,393.062206550312,393.330862851807,393.599519172248,393.868175511888,
394.136831870107,394.405488246334,394.674144639227,394.94280104753,395.211457469356,
395.480113902905,395.748770345913,396.017426796181,396.286083251232,396.554739708622,
396.823396165819,397.092052620289,397.360709069602,397.629365511291,397.898021943183,
398.166678363037,398.43533476909,398.703991159489,398.972647533028,399.241303888413,
399.509960225133,399.778616542629,400.047272841224,400.315929121267,400.584585384052,
400.853241631017,401.121897864557,401.390554087381,401.659210303115,401.927866515925,
402.196522730559,402.465178951451,402.733835182185,403.002491425899,403.271147684792,
403.539803960819,403.808460254978,404.077116568174,404.345772900386,404.614429251599,
404.883085620952,405.151742007649,405.420398410161,405.689054827051,405.957711256297,
406.226367695961,406.495024143695,406.76368059721,407.032337053993,407.300993511558,
407.569649967387,407.838306418949,408.106962863879,408.375619299759,408.644275724528,
408.912932136048,409.181588532709,409.450244912815,409.718901275356,409.987557619248,
410.25621394422,410.524870249975,410.79352653712,411.06218280632,411.330839059193,
411.599495297549,411.868151524149,412.13680774213,412.40546395552,412.674120168911,
412.942776386892,413.211432613491,413.480088851848,413.748745104721,414.017401373921,
414.286057661065,414.55471396682,414.823370291793,415.092026635685,415.360682998226,
415.629339378332,415.897995774993,416.166652186512,416.435308611282,416.703965047162,
416.972621492092,417.241277943654,417.509934399483,417.778590857048,418.047247313831,
418.315903767346,418.58456021508,418.853216654744,419.121873083989,419.390529500879,
419.659185903392,419.927842290088,420.196498659441,420.465155010654,420.733811342866,
421.002467656062,421.271123950222,421.539780226249,421.808436485141,422.077092728855,
422.34574895959,422.614405180482,422.883061395116,423.151717607926,423.42037382366,
423.689030046484,423.957686280024,424.226342526988,424.494998789773,424.763655069817,
425.032311368411,425.300967685907,425.569624022627,425.838280378013,426.106936751551,
426.375593141951,426.644249548003,426.912905967857,427.18156239975,427.450218841438,
427.718875290752,427.987531745221,428.256188202418,428.524844659809,428.793501114859,
429.062157565128,429.330814008135,429.599470441684,429.868126863511,430.136783271814,
430.405439664707,430.674096040933,430.942752399152,431.211408738792,431.480065059233,
431.748721360729,432.017377643552,432.286033908916,432.554690158171,432.823346393619,
433.092002617869,433.360658834445,433.629315047397,433.897971261447,434.166627481123,
434.435283710124,434.703939951682,434.972596208097,435.241252481411,435.509908772707,
435.778565082967,436.047221412241,436.31587776058,436.584534127182,436.853190511305,
437.121846911468,437.390503326275,437.659159753738,437.927816191952,438.196472638587,
438.465129091377,438.733785547816,439.002442005427,439.271098461688,439.539754914064,
439.808411360173,440.077067797584,440.345724224207,440.614380637875,440.883037036941,
441.151693419666,441.420349784991,441.689006131777,441.957662459693,442.226318768374,
442.494975058355,442.763631330221,443.032287585506,443.300943825928,443.569600054153,
443.838256273211,444.106912487028,444.375568700103,444.644224917101,444.912881142151,
445.181537378504,445.450193629011,445.718849895579,445.987506179909,446.256162482747,
446.524818804774,446.79347514576,447.062131505496,447.330787882954,447.599444277176,
447.868100686504,448.136757109373,448.40541354367,448.674069987365,448.942726438055,
449.211382893394,449.480039350853,449.748695807921,450.017352262103,450.286008710879,
450.55466515194,450.82332158292,451.091978001848,451.360634406672,451.62929079591,
451.89794716799,452.166603522061,452.435259857205,452.703916173343,452.972572470381,
453.24122874915,453.509885010562,453.778541256488,454.047197489028,454.315853711222,
454.584509926543,454.853166139327,455.121822354318,455.3904785758,455.659134807498,
455.927791052226,456.19644731247,456.465103589759,456.733759885467,457.00241620002,
457.271072533811,457.539728886346,457.80838525717,458.077041645044,458.345698048806,
458.614354466642,458.883010896827,459.151667337143,459.420323785445,459.688980239275,
459.957636696219,460.226293153743,460.494949609316,460.763606060482,461.032262504754,
461.300918939909,461.569575363662,461.838231774175,462.106888169527,462.375544548414,
462.644200909447,462.912857251999,463.181513575386,463.450169879794,463.71882616542,
463.987482433401,464.256138684994,464.524794922418,464.793451148174,465.062107365689,
465.330763578896,465.59941979247,465.86807601102,466.13673223836,466.405388477821,
466.674044731802,466.942701002433,467.211357290885,467.480013598214,467.748669924546,
468.017326269997,468.285982633826,468.554639015346,468.823295413121,469.091951825803,
469.360608251434,469.629264688145,469.897921133626,470.166577585633,470.435234041669,
470.703890499266,470.972546955898,471.24120340903,471.509859856263,471.778516295153,
472.047172723582,472.315829139356,472.584485540789,472.853141926103,473.12179829419,
473.390454643857,473.659110974714,473.927767286328,474.196423579164,474.465079853726,
474.73373611147,475.002392354016,475.271048583941,475.539704804167,475.808361018519,
476.077017231391,476.345673447501,476.614329671083,476.882985905496,477.151642153686,
477.420298417658,477.688954699194,477.957610999126,478.226267318208,478.494923656277,
478.76358001319,479.032236387973,479.300892779719,479.569549186815,479.838205607737,
480.106862040401,480.375518482806,480.644174932567,480.912831387357,481.18148784465,
481.450144301944,481.718800756733,481.987457206495,482.2561136489,482.524770081563,
482.793426502485,483.062082909582,483.330739301328,483.59939567611,483.868052033023,
484.136708371092,484.405364690174,484.674020990106,484.942677271643,485.211333535614,
485.479989783805,485.748646018218,486.017302241799,486.28595845791,486.554614670781,
486.823270885133,487.091927105359,487.360583335284,487.629239577831,487.897895835574,
488.166552110137,488.435208402973,488.703864714587,488.972521045443,489.241177395111,
489.509833763197,489.778490148512,490.047146549945,490.315802965719,490.584459394147,
490.853115833037,491.12177228027,491.390428733402,491.659085190034,491.927741647632,
492.196398103667,492.465054555674,492.733711001155,493.002367437866,493.271023863497,
493.539680276179,493.808336673954,494.076993055474,494.345649419303,494.614305764754,
494.882962091086,495.151618398416,495.420274686867,495.688930957498,495.95758721148,
496.22624345094,496.494899678281,496.76355589683,497.032212110404,497.300868323611,
497.569524541126,497.838180766882,498.106837004306,498.3754932559,498.64414952388,
498.912805809507,499.181462113914,499.450118437301,499.718774779852,499.987431140886,
500.256087519773,500.524743915125,500.793400325638,501.06205674939,501.330713184546,
501.599369628818,501.868026079984,502.136682535557,502.40533899308,502.673995450025,
502.942651903855,503.211308352156,503.479964792472,503.748621222657,504.017277640494,
504.285934044256,504.554590432129,504.823246802954,505.091903155488,505.360559489279,
505.629215803832,505.89787209954,506.166528376829,506.435184637073,506.703840881801,
506.972497113499,507.241153334981,507.509809549972,507.778465762756,508.047121978078,
508.315778200272,508.584434432811,508.853090678737,509.121746940149,509.390403218918,
509.659059515956,509.927715832093,510.196372167238,510.465028521309,510.733684893389,
511.002341282627,511.270997687451,511.53965410638,511.808310537359,512.076966978421,
512.345623427198,512.614279881382,512.882936338452,513.151592795914,513.420249251254,
513.688905701946,513.957562145643,514.226218579942,514.494875002812,514.763531412143,
515.032187806366,515.300844183826,515.569500543564,515.838156884552,516.106813206581,
516.375469509421,516.644125793752,516.912782060321,517.181438310831,517.450094547186,
517.718750772238,517.987406989238,518.256063202315,518.524719416134,518.793375635194,
519.062031863421,519.330688103845,519.599344359133,519.868000631,520.136656920983,
520.405313229665,520.673969557583,520.942625904371,521.211282269698,521.479938652425,
521.748595051492,522.017251465163,522.285907891788,522.554564329201,522.823220775312,
523.091877227689,523.360533683951,523.629190141564,523.897846598005,524.166503050797,
524.435159497434,524.70381593565,524.972472363114,525.241128777924,525.509785178088,
525.778441562214,526.047097928818,526.315754277159,526.584410606435,526.853066916696,
527.121723207994,527.390379481309,527.659035737726,527.927691979287,528.19634820829,
528.465004427967,528.73366064202,529.002316854973,529.270973071551,529.539629295803,
529.808285531254,530.07694178051,530.345598045876,530.614254328701,530.882910630198,
531.151566950641,531.420223290284,531.688879648504,531.957536024733,532.226192417628,
532.494848825933,532.76350524776,533.032161681312,533.30081812432,533.569474574591,
533.838131029643,534.106787487035,534.375443944235,534.644100398706,534.912756848021,
535.181413289711,535.450069721605,535.718726141461,535.987382547516,536.256038937917,
536.524695311458,536.793351666845,537.062008003567,537.330664321065,537.599320619661,
537.867976899706,538.136633162493,538.40528940946,538.673945643001,538.942601865828,
539.211258081563,539.479914294375,539.748570509011,540.017226729904,540.285882960641,
540.554539204357,540.823195463252,541.09185173928,541.360508033441,541.629164346639,
541.897820678853,542.166477030068,542.435133399423,542.703789786121,542.972446188636,
543.241102605527,543.509759034775,543.778415474441,544.047071922176,544.315728375693,
544.584384832479,544.853041290046,545.121697745877,545.390354197441,545.659010642372,
545.927667078254,546.196323503025,546.464979914547,546.733636311202,547.002292691334,
547.270949053789,547.539605397955,547.808261722147,548.076918029812,548.345574313508,
548.614230583738,548.882886864851,549.151542935882,549.420199787641,549.68885445376,
549.957511414581),.UNSPECIFIED.)
GEOMETRIC_REPRESENTATION_ITEM()
RATIONAL_B_SPLINE_SURFACE(((1.,1.,1.,1.,1.,1.,1.,1.,1.,1.,1.,1.,1.,1.,1.,
1.,1.,1.,1.,1.,1.,1.,1.,1.,1.,1.,1.,1.,1.,1.,1.,1.,1.,1.,1.,1.,1.,1.,1.,
1.,1.,1.,1.,1.,1.,1.,1.,1.,1.,1.,1.,1.,1.,1.,1.,1.,1.,1.,1.,1.,1.,1.,1.,
1.,1.,1.,1.,1.,1.,1.,1.,1.,1.,1.,1.,1.,1.,1.,1.,1.,1.,1.,1.,1.,1.,1.,1.,
1.,1.,1.,1.,1.,1.,1.,1.,1.,1.,1.,1.,1.,1.,1.,1.,1.,1.,1.,1.,1.,1.,1.,1.,
1.,1.,1.,1.,1.,1.,1.,1.,1.,1.,1.,1.,1.,1.,1.,1.,1.,1.,1.,1.,1.,1.,1.,1.,
1.,1.,1.,1.,1.,1.,1.,1.,1.,1.,1.,1.,1.,1.,1.,1.,1.,1.,1.,1.,1.,1.,1.,1.,
1.,1.,1.,1.,1.,1.,1.,1.,1.,1.,1.,1.,1.,1.,1.,1.,1.,1.,1.,1.,1.,1.,1.,1.,
1.,1.,1.,1.,1.,1.,1.,1.,1.,1.,1.,1.,1.,1.,1.,1.,1.,1.,1.,1.,1.,1.,1.,1.,
1.,1.,1.,1.,1.,1.,1.,1.,1.,1.,1.,1.,1.,1.,1.,1.,1.,1.,1.,1.,1.,1.,1.,1.,
1.,1.,1.,1.,1.,1.,1.,1.,1.,1.,1.,1.,1.,1.,1.,1.,1.,1.,1.,1.,1.,1.,1.,1.,
1.,1.,1.,1.,1.,1.,1.,1.,1.,1.,1.,1.,1.,1.,1.,1.,1.,1.,1.,1.,1.,1.,1.,1.,
1.,1.,1.,1.,1.,1.,1.,1.,1.,1.,1.,1.,1.,1.,1.,1.,1.,1.,1.,1.,1.,1.,1.,1.,
1.,1.,1.,1.,1.,1.,1.,1.,1.,1.,1.,1.,1.,1.,1.,1.,1.,1.,1.,1.,1.,1.,1.,1.,
1.,1.,1.,1.,1.,1.,1.,1.,1.,1.,1.,1.,1.,1.,1.,1.,1.,1.,1.,1.,1.,1.,1.,1.,
1.,1.,1.,1.,1.,1.,1.,1.,1.,1.,1.,1.,1.,1.,1.,1.,1.,1.,1.,1.,1.,1.,1.,1.,
1.,1.,1.,1.,1.,1.,1.,1.,1.,1.,1.,1.,1.,1.,1.,1.,1.,1.,1.,1.,1.,1.,1.,1.,
1.,1.,1.,1.,1.,1.,1.,1.,1.,1.,1.,1.,1.,1.,1.,1.,1.,1.,1.,1.,1.,1.,1.,1.,
1.,1.,1.,1.,1.,1.,1.,1.,1.,1.,1.,1.,1.,1.,1.,1.,1.,1.,1.,1.,1.,1.,1.,1.,
1.,1.,1.,1.,1.,1.,1.,1.,1.,1.,1.,1.,1.,1.,1.,1.,1.,1.,1.,1.,1.,1.,1.,1.,
1.,1.,1.,1.,1.,1.,1.,1.,1.,1.,1.,1.,1.,1.,1.,1.,1.,1.,1.,1.,1.,1.,1.,1.,
1.,1.,1.,1.,1.,1.,1.,1.,1.,1.,1.,1.,1.,1.,1.,1.,1.,1.,1.,1.,1.,1.,1.,1.,
1.,1.,1.,1.,1.,1.,1.,1.,1.,1.,1.,1.,1.,1.,1.,1.,1.,1.,1.,1.,1.,1.,1.,1.,
1.,1.,1.,1.,1.,1.,1.,1.,1.,1.,1.,1.,1.,1.,1.,1.,1.,1.,1.,1.,1.,1.,1.,1.,
1.,1.,1.,1.,1.,1.,1.,1.,1.,1.,1.,1.,1.,1.,1.,1.,1.,1.,1.,1.,1.,1.,1.,1.,
1.,1.,1.,1.,1.,1.,1.,1.,1.,1.,1.,1.,1.,1.,1.,1.,1.,1.,1.,1.,1.,1.,1.,1.,
1.,1.,1.,1.,1.,1.,1.,1.,1.,1.,1.,1.,1.,1.,1.,1.,1.,1.,1.,1.,1.,1.,1.,1.,
1.,1.,1.,1.,1.,1.,1.,1.,1.,1.,1.,1.,1.,1.,1.,1.,1.,1.,1.,1.,1.,1.,1.,1.,
1.,1.,1.,1.,1.,1.,1.,1.,1.,1.,1.,1.,1.,1.,1.,1.,1.,1.,1.,1.,1.,1.,1.,1.,
1.,1.,1.,1.,1.,1.,1.,1.,1.,1.,1.,1.,1.,1.,1.,1.,1.,1.,1.,1.,1.,1.,1.,1.,
1.,1.,1.,1.,1.,1.,1.,1.,1.,1.,1.,1.,1.,1.,1.,1.,1.,1.,1.,1.,1.,1.,1.,1.,
1.,1.,1.,1.,1.,1.,1.,1.,1.,1.,1.,1.,1.,1.,1.,1.,1.,1.,1.,1.,1.,1.,1.,1.,
1.,1.,1.,1.,1.,1.,1.,1.,1.,1.,1.,1.,1.,1.,1.,1.,1.,1.,1.,1.,1.,1.,1.,1.,
1.,1.,1.,1.,1.,1.,1.,1.,1.,1.,1.,1.,1.,1.,1.,1.,1.,1.,1.,1.,1.,1.,1.,1.,
1.,1.,1.,1.,1.,1.,1.,1.,1.,1.,1.,1.,1.,1.,1.,1.,1.,1.,1.,1.,1.,1.,1.,1.,
1.,1.,1.,1.,1.,1.,1.,1.,1.,1.,1.,1.,1.,1.,1.,1.,1.,1.,1.,1.,1.,1.,1.,1.,
1.,1.,1.,1.,1.,1.,1.,1.,1.,1.,1.,1.,1.,1.,1.,1.,1.,1.,1.,1.,1.,1.,1.,1.,
1.,1.,1.,1.,1.,1.,1.,1.,1.,1.,1.,1.,1.,1.,1.,1.,1.,1.,1.,1.,1.,1.,1.,1.,
1.,1.,1.,1.,1.,1.,1.,1.,1.,1.,1.,1.,1.,1.,1.,1.,1.,1.,1.,1.,1.,1.,1.,1.,
1.,1.,1.,1.,1.,1.,1.,1.,1.,1.,1.,1.,1.,1.,1.,1.,1.,1.,1.,1.,1.,1.,1.,1.,
1.,1.,1.,1.,1.,1.,1.,1.,1.,1.,1.,1.,1.,1.,1.,1.,1.,1.,1.,1.,1.,1.,1.,1.,
1.,1.,1.,1.,1.,1.,1.,1.,1.,1.,1.,1.,1.,1.,1.,1.,1.,1.,1.,1.,1.,1.,1.,1.,
1.,1.,1.,1.,1.,1.,1.,1.,1.,1.,1.,1.,1.,1.,1.,1.,1.,1.,1.,1.,1.,1.,1.,1.,
1.,1.,1.,1.,1.,1.,1.,1.,1.,1.,1.,1.,1.,1.,1.,1.,1.,1.,1.,1.,1.,1.,1.,1.,
1.,1.,1.,1.,1.,1.,1.,1.,1.,1.,1.,1.,1.,1.,1.,1.,1.,1.,1.,1.,1.,1.,1.,1.,
1.,1.,1.,1.,1.,1.,1.,1.,1.,1.,1.,1.,1.,1.,1.,1.,1.,1.,1.,1.,1.,1.,1.,1.,
1.,1.,1.,1.,1.,1.,1.,1.,1.,1.,1.,1.,1.,1.,1.,1.,1.,1.,1.,1.,1.,1.,1.,1.,
1.,1.,1.,1.,1.,1.,1.,1.,1.,1.,1.,1.,1.,1.,1.,1.,1.,1.,1.,1.,1.,1.,1.,1.,
1.,1.,1.,1.,1.,1.,1.,1.,1.,1.,1.,1.,1.,1.,1.,1.,1.,1.,1.,1.,1.,1.,1.,1.,
1.,1.,1.,1.,1.,1.,1.,1.,1.,1.,1.,1.,1.,1.,1.,1.,1.,1.,1.,1.,1.,1.,1.,1.,
1.,1.,1.,1.,1.,1.,1.,1.,1.,1.,1.,1.,1.,1.,1.,1.,1.,1.,1.,1.,1.,1.,1.,1.,
1.,1.,1.,1.,1.,1.,1.,1.,1.,1.,1.,1.,1.,1.,1.,1.,1.,1.,1.,1.,1.,1.,1.,1.,
1.,1.,1.,1.,1.,1.,1.,1.,1.,1.,1.,1.,1.,1.,1.,1.,1.,1.,1.,1.,1.,1.,1.,1.,
1.,1.,1.,1.,1.,1.,1.,1.,1.,1.,1.,1.,1.,1.,1.,1.,1.,1.,1.,1.,1.,1.,1.,1.,
1.,1.,1.,1.,1.,1.,1.,1.,1.,1.,1.,1.,1.,1.,1.,1.,1.,1.,1.,1.,1.,1.,1.,1.,
1.,1.,1.,1.,1.,1.,1.,1.,1.,1.,1.,1.,1.,1.,1.,1.,1.,1.,1.,1.,1.,1.,1.,1.,
1.,1.,1.,1.,1.,1.,1.,1.,1.,1.,1.,1.,1.,1.,1.,1.,1.,1.,1.,1.,1.,1.,1.,1.,
1.,1.,1.,1.,1.,1.,1.,1.,1.,1.,1.,1.,1.,1.,1.,1.,1.,1.,1.,1.,1.,1.,1.,1.,
1.,1.,1.,1.,1.,1.,1.,1.,1.,1.,1.,1.,1.,1.,1.,1.,1.,1.,1.,1.,1.,1.,1.,1.,
1.,1.,1.,1.,1.,1.,1.,1.,1.,1.,1.,1.,1.,1.,1.,1.,1.,1.,1.,1.,1.,1.,1.,1.,
1.,1.,1.,1.,1.,1.,1.,1.,1.,1.,1.,1.,1.,1.,1.,1.,1.,1.,1.,1.,1.,1.,1.,1.,
1.,1.,1.,1.,1.,1.,1.,1.,1.,1.,1.,1.,1.,1.,1.,1.,1.,1.,1.,1.,1.,1.,1.,1.,
1.,1.,1.,1.,1.,1.,1.,1.,1.,1.,1.,1.,1.,1.,1.,1.,1.,1.,1.,1.,1.,1.,1.,1.,
1.,1.,1.,1.,1.,1.,1.,1.,1.,1.,1.,1.,1.,1.,1.,1.,1.,1.,1.,1.,1.,1.,1.,1.,
1.,1.,1.,1.,1.,1.,1.,1.,1.,1.,1.,1.,1.,1.,1.,1.,1.,1.,1.,1.,1.,1.,1.,1.,
1.,1.,1.,1.,1.,1.,1.,1.,1.,1.,1.,1.,1.,1.,1.,1.,1.,1.,1.,1.,1.,1.,1.,1.,
1.,1.,1.,1.,1.,1.,1.,1.,1.,1.,1.,1.,1.,1.,1.,1.,1.,1.,1.,1.,1.,1.,1.,1.,
1.,1.,1.,1.,1.,1.,1.,1.,1.,1.,1.,1.,1.,1.,1.,1.,1.,1.,1.,1.,1.,1.,1.,1.,
1.,1.,1.,1.,1.,1.,1.,1.,1.,1.,1.,1.,1.,1.,1.,1.,1.,1.,1.,1.,1.,1.,1.,1.,
1.,1.,1.,1.,1.,1.,1.,1.,1.,1.,1.,1.,1.,1.,1.,1.,1.,1.,1.,1.,1.,1.,1.,1.,
1.,1.,1.,1.,1.,1.,1.,1.,1.,1.,1.,1.,1.,1.,1.,1.,1.,1.,1.,1.,1.,1.,1.,1.,
1.,1.,1.,1.,1.,1.,1.,1.,1.,1.,1.,1.,1.,1.,1.,1.,1.,1.,1.,1.,1.,1.,1.,1.,
1.,1.,1.,1.,1.,1.,1.,1.,1.,1.,1.,1.,1.,1.,1.,1.,1.,1.,1.,1.,1.,1.,1.,1.,
1.,1.,1.,1.,1.,1.,1.,1.,1.,1.,1.,1.,1.,1.,1.,1.,1.,1.,1.,1.,1.,1.,1.,1.,
1.,1.,1.,1.,1.,1.,1.,1.,1.,1.,1.,1.,1.,1.,1.,1.,1.,1.,1.,1.,1.,1.,1.,1.,
1.,1.,1.,1.,1.,1.,1.,1.,1.,1.,1.,1.,1.,1.,1.,1.,1.,1.,1.,1.,1.,1.,1.,1.,
1.,1.,1.,1.,1.,1.,1.,1.,1.,1.,1.,1.,1.,1.,1.,1.,1.,1.,1.,1.,1.,1.,1.,1.,
1.,1.,1.,1.,1.,1.,1.,1.,1.,1.,1.,1.,1.,1.,1.,1.,1.,1.,1.,1.,1.,1.,1.,1.,
1.,1.,1.,1.,1.,1.,1.,1.,1.,1.,1.,1.,1.,1.,1.,1.,1.,1.,1.,1.,1.,1.,1.,1.,
1.,1.,1.,1.,1.,1.,1.,1.,1.,1.,1.,1.,1.,1.,1.,1.,1.,1.,1.,1.,1.,1.,1.,1.,
1.,1.,1.,1.,1.,1.,1.,1.,1.,1.,1.,1.,1.,1.,1.,1.,1.,1.,1.,1.,1.,1.,1.,1.,
1.,1.,1.,1.,1.,1.,1.,1.,1.,1.,1.,1.,1.,1.,1.,1.,1.,1.,1.,1.,1.,1.,1.,1.,
1.,1.,1.,1.,1.,1.,1.,1.,1.,1.,1.,1.,1.,1.,1.,1.,1.,1.,1.,1.,1.,1.,1.,1.,
1.,1.,1.,1.,1.,1.,1.,1.,1.,1.,1.,1.,1.,1.,1.,1.,1.,1.,1.,1.,1.,1.,1.,1.,
1.,1.,1.,1.,1.,1.,1.,1.,1.,1.,1.,1.,1.,1.,1.,1.,1.,1.,1.,1.,1.,1.,1.,1.,
1.,1.,1.,1.,1.,1.,1.,1.,1.,1.,1.,1.,1.,1.,1.,1.,1.,1.,1.,1.),(0.707106781186548,
0.707106781186548,0.707106781186548,0.707106781186547,0.707106781186547,
0.707106781186548,0.707106781186547,0.707106781186547,0.707106781186547,
0.707106781186547,0.707106781186547,0.707106781186548,0.707106781186548,
0.707106781186548,0.707106781186547,0.707106781186548,0.707106781186547,
0.707106781186547,0.707106781186548,0.707106781186547,0.707106781186548,
0.707106781186547,0.707106781186548,0.707106781186547,0.707106781186548,
0.707106781186547,0.707106781186547,0.707106781186547,0.707106781186547,
0.707106781186547,0.707106781186548,0.707106781186547,0.707106781186547,
0.707106781186548,0.707106781186547,0.707106781186547,0.707106781186548,
0.707106781186547,0.707106781186547,0.707106781186548,0.707106781186548,
0.707106781186547,0.707106781186548,0.707106781186547,0.707106781186547,
0.707106781186547,0.707106781186548,0.707106781186548,0.707106781186547,
0.707106781186547,0.707106781186548,0.707106781186547,0.707106781186548,
0.707106781186547,0.707106781186547,0.707106781186547,0.707106781186547,
0.707106781186547,0.707106781186548,0.707106781186547,0.707106781186548,
0.707106781186547,0.707106781186548,0.707106781186547,0.707106781186548,
0.707106781186547,0.707106781186547,0.707106781186548,0.707106781186547,
0.707106781186547,0.707106781186548,0.707106781186547,0.707106781186548,
0.707106781186547,0.707106781186548,0.707106781186548,0.707106781186547,
0.707106781186548,0.707106781186547,0.707106781186547,0.707106781186548,
0.707106781186547,0.707106781186547,0.707106781186547,0.707106781186548,
0.707106781186547,0.707106781186547,0.707106781186547,0.707106781186547,
0.707106781186547,0.707106781186547,0.707106781186548,0.707106781186548,
0.707106781186547,0.707106781186548,0.707106781186547,0.707106781186548,
0.707106781186548,0.707106781186547,0.707106781186548,0.707106781186548,
0.707106781186548,0.707106781186547,0.707106781186548,0.707106781186547,
0.707106781186548,0.707106781186548,0.707106781186548,0.707106781186547,
0.707106781186547,0.707106781186547,0.707106781186548,0.707106781186548,
0.707106781186548,0.707106781186547,0.707106781186547,0.707106781186547,
0.707106781186548,0.707106781186548,0.707106781186547,0.707106781186547,
0.707106781186548,0.707106781186547,0.707106781186547,0.707106781186547,
0.707106781186547,0.707106781186548,0.707106781186547,0.707106781186548,
0.707106781186547,0.707106781186547,0.707106781186547,0.707106781186548,
0.707106781186548,0.707106781186547,0.707106781186548,0.707106781186548,
0.707106781186547,0.707106781186548,0.707106781186547,0.707106781186548,
0.707106781186547,0.707106781186548,0.707106781186547,0.707106781186547,
0.707106781186548,0.707106781186547,0.707106781186547,0.707106781186548,
0.707106781186547,0.707106781186547,0.707106781186548,0.707106781186547,
0.707106781186548,0.707106781186547,0.707106781186547,0.707106781186548,
0.707106781186548,0.707106781186547,0.707106781186548,0.707106781186547,
0.707106781186548,0.707106781186547,0.707106781186548,0.707106781186547,
0.707106781186548,0.707106781186547,0.707106781186548,0.707106781186547,
0.707106781186548,0.707106781186547,0.707106781186548,0.707106781186547,
0.707106781186547,0.707106781186548,0.707106781186547,0.707106781186548,
0.707106781186547,0.707106781186548,0.707106781186547,0.707106781186548,
0.707106781186547,0.707106781186547,0.707106781186548,0.707106781186547,
0.707106781186548,0.707106781186548,0.707106781186548,0.707106781186547,
0.707106781186547,0.707106781186547,0.707106781186547,0.707106781186548,
0.707106781186547,0.707106781186548,0.707106781186548,0.707106781186547,
0.707106781186547,0.707106781186548,0.707106781186548,0.707106781186547,
0.707106781186547,0.707106781186548,0.707106781186547,0.707106781186548,
0.707106781186547,0.707106781186547,0.707106781186547,0.707106781186547,
0.707106781186547,0.707106781186547,0.707106781186547,0.707106781186548,
0.707106781186547,0.707106781186548,0.707106781186547,0.707106781186548,
0.707106781186548,0.707106781186547,0.707106781186548,0.707106781186548,
0.707106781186548,0.707106781186548,0.707106781186547,0.707106781186548,
0.707106781186547,0.707106781186548,0.707106781186547,0.707106781186547,
0.707106781186548,0.707106781186548,0.707106781186547,0.707106781186547,
0.707106781186547,0.707106781186547,0.707106781186547,0.707106781186548,
0.707106781186548,0.707106781186547,0.707106781186547,0.707106781186548,
0.707106781186548,0.707106781186547,0.707106781186548,0.707106781186547,
0.707106781186548,0.707106781186548,0.707106781186547,0.707106781186547,
0.707106781186548,0.707106781186547,0.707106781186547,0.707106781186548,
0.707106781186547,0.707106781186548,0.707106781186547,0.707106781186548,
0.707106781186547,0.707106781186547,0.707106781186548,0.707106781186548,
0.707106781186547,0.707106781186547,0.707106781186548,0.707106781186547,
0.707106781186547,0.707106781186548,0.707106781186547,0.707106781186548,
0.707106781186547,0.707106781186548,0.707106781186547,0.707106781186548,
0.707106781186547,0.707106781186547,0.707106781186547,0.707106781186547,
0.707106781186547,0.707106781186547,0.707106781186548,0.707106781186547,
0.707106781186548,0.707106781186547,0.707106781186548,0.707106781186548,
0.707106781186547,0.707106781186548,0.707106781186548,0.707106781186547,
0.707106781186548,0.707106781186547,0.707106781186547,0.707106781186547,
0.707106781186548,0.707106781186547,0.707106781186547,0.707106781186548,
0.707106781186547,0.707106781186548,0.707106781186547,0.707106781186547,
0.707106781186547,0.707106781186548,0.707106781186548,0.707106781186547,
0.707106781186548,0.707106781186548,0.707106781186547,0.707106781186548,
0.707106781186547,0.707106781186548,0.707106781186548,0.707106781186547,
0.707106781186548,0.707106781186548,0.707106781186548,0.707106781186547,
0.707106781186547,0.707106781186548,0.707106781186547,0.707106781186548,
0.707106781186547,0.707106781186547,0.707106781186548,0.707106781186548,
0.707106781186548,0.707106781186547,0.707106781186547,0.707106781186548,
0.707106781186548,0.707106781186547,0.707106781186547,0.707106781186548,
0.707106781186547,0.707106781186547,0.707106781186548,0.707106781186548,
0.707106781186547,0.707106781186547,0.707106781186547,0.707106781186548,
0.707106781186547,0.707106781186547,0.707106781186547,0.707106781186548,
0.707106781186548,0.707106781186547,0.707106781186548,0.707106781186547,
0.707106781186548,0.707106781186547,0.707106781186548,0.707106781186548,
0.707106781186547,0.707106781186547,0.707106781186548,0.707106781186547,
0.707106781186547,0.707106781186548,0.707106781186547,0.707106781186548,
0.707106781186548,0.707106781186547,0.707106781186548,0.707106781186547,
0.707106781186547,0.707106781186547,0.707106781186548,0.707106781186548,
0.707106781186548,0.707106781186547,0.707106781186548,0.707106781186547,
0.707106781186548,0.707106781186547,0.707106781186547,0.707106781186547,
0.707106781186547,0.707106781186548,0.707106781186548,0.707106781186547,
0.707106781186547,0.707106781186548,0.707106781186547,0.707106781186548,
0.707106781186547,0.707106781186548,0.707106781186547,0.707106781186547,
0.707106781186548,0.707106781186547,0.707106781186548,0.707106781186547,
0.707106781186548,0.707106781186548,0.707106781186547,0.707106781186548,
0.707106781186547,0.707106781186548,0.707106781186548,0.707106781186547,
0.707106781186548,0.707106781186547,0.707106781186547,0.707106781186548,
0.707106781186547,0.707106781186548,0.707106781186547,0.707106781186548,
0.707106781186547,0.707106781186547,0.707106781186548,0.707106781186548,
0.707106781186548,0.707106781186548,0.707106781186547,0.707106781186548,
0.707106781186548,0.707106781186548,0.707106781186547,0.707106781186548,
0.707106781186548,0.707106781186548,0.707106781186547,0.707106781186547,
0.707106781186548,0.707106781186547,0.707106781186548,0.707106781186547,
0.707106781186548,0.707106781186548,0.707106781186547,0.707106781186547,
0.707106781186548,0.707106781186547,0.707106781186548,0.707106781186547,
0.707106781186548,0.707106781186548,0.707106781186547,0.707106781186547,
0.707106781186547,0.707106781186548,0.707106781186548,0.707106781186547,
0.707106781186547,0.707106781186548,0.707106781186548,0.707106781186548,
0.707106781186548,0.707106781186547,0.707106781186547,0.707106781186548,
0.707106781186548,0.707106781186547,0.707106781186548,0.707106781186547,
0.707106781186548,0.707106781186547,0.707106781186548,0.707106781186547,
0.707106781186547,0.707106781186548,0.707106781186547,0.707106781186547,
0.707106781186548,0.707106781186547,0.707106781186548,0.707106781186547,
0.707106781186548,0.707106781186547,0.707106781186548,0.707106781186547,
0.707106781186548,0.707106781186547,0.707106781186548,0.707106781186547,
0.707106781186547,0.707106781186548,0.707106781186548,0.707106781186547,
0.707106781186547,0.707106781186547,0.707106781186548,0.707106781186547,
0.707106781186548,0.707106781186547,0.707106781186548,0.707106781186547,
0.707106781186548,0.707106781186547,0.707106781186547,0.707106781186547,
0.707106781186548,0.707106781186547,0.707106781186548,0.707106781186548,
0.707106781186547,0.707106781186548,0.707106781186547,0.707106781186547,
0.707106781186548,0.707106781186547,0.707106781186547,0.707106781186548,
0.707106781186547,0.707106781186547,0.707106781186547,0.707106781186547,
0.707106781186548,0.707106781186547,0.707106781186547,0.707106781186547,
0.707106781186548,0.707106781186547,0.707106781186547,0.707106781186548,
0.707106781186548,0.707106781186547,0.707106781186548,0.707106781186548,
0.707106781186547,0.707106781186547,0.707106781186548,0.707106781186547,
0.707106781186547,0.707106781186548,0.707106781186547,0.707106781186547,
0.707106781186547,0.707106781186548,0.707106781186547,0.707106781186548,
0.707106781186547,0.707106781186548,0.707106781186547,0.707106781186548,
0.707106781186547,0.707106781186548,0.707106781186547,0.707106781186548,
0.707106781186548,0.707106781186547,0.707106781186547,0.707106781186548,
0.707106781186547,0.707106781186548,0.707106781186547,0.707106781186548,
0.707106781186548,0.707106781186547,0.707106781186548,0.707106781186547,
0.707106781186548,0.707106781186548,0.707106781186547,0.707106781186547,
0.707106781186548,0.707106781186547,0.707106781186548,0.707106781186547,
0.707106781186548,0.707106781186547,0.707106781186548,0.707106781186547,
0.707106781186547,0.707106781186547,0.707106781186547,0.707106781186547,
0.707106781186547,0.707106781186547,0.707106781186547,0.707106781186548,
0.707106781186547,0.707106781186548,0.707106781186547,0.707106781186547,
0.707106781186548,0.707106781186547,0.707106781186548,0.707106781186547,
0.707106781186547,0.707106781186548,0.707106781186547,0.707106781186548,
0.707106781186547,0.707106781186548,0.707106781186547,0.707106781186548,
0.707106781186547,0.707106781186548,0.707106781186547,0.707106781186548,
0.707106781186547,0.707106781186548,0.707106781186548,0.707106781186547,
0.707106781186548,0.707106781186547,0.707106781186547,0.707106781186547,
0.707106781186548,0.707106781186547,0.707106781186547,0.707106781186547,
0.707106781186548,0.707106781186547,0.707106781186547,0.707106781186548,
0.707106781186547,0.707106781186547,0.707106781186547,0.707106781186547,
0.707106781186548,0.707106781186547,0.707106781186547,0.707106781186547,
0.707106781186548,0.707106781186548,0.707106781186548,0.707106781186548,
0.707106781186547,0.707106781186548,0.707106781186547,0.707106781186547,
0.707106781186548,0.707106781186547,0.707106781186548,0.707106781186547,
0.707106781186547,0.707106781186548,0.707106781186547,0.707106781186547,
0.707106781186547,0.707106781186547,0.707106781186548,0.707106781186548,
0.707106781186547,0.707106781186547,0.707106781186548,0.707106781186547,
0.707106781186548,0.707106781186547,0.707106781186548,0.707106781186548,
0.707106781186547,0.707106781186547,0.707106781186548,0.707106781186548,
0.707106781186547,0.707106781186548,0.707106781186548,0.707106781186547,
0.707106781186548,0.707106781186548,0.707106781186548,0.707106781186547,
0.707106781186548,0.707106781186547,0.707106781186548,0.707106781186547,
0.707106781186548,0.707106781186547,0.707106781186548,0.707106781186547,
0.707106781186548,0.707106781186548,0.707106781186547,0.707106781186547,
0.707106781186548,0.707106781186547,0.707106781186548,0.707106781186547,
0.707106781186548,0.707106781186548,0.707106781186548,0.707106781186548,
0.707106781186548,0.707106781186547,0.707106781186547,0.707106781186547,
0.707106781186547,0.707106781186548,0.707106781186547,0.707106781186548,
0.707106781186547,0.707106781186547,0.707106781186548,0.707106781186548,
0.707106781186547,0.707106781186548,0.707106781186547,0.707106781186548,
0.707106781186548,0.707106781186547,0.707106781186547,0.707106781186548,
0.707106781186547,0.707106781186548,0.707106781186547,0.707106781186548,
0.707106781186547,0.707106781186548,0.707106781186547,0.707106781186548,
0.707106781186547,0.707106781186548,0.707106781186547,0.707106781186548,
0.707106781186548,0.707106781186547,0.707106781186548,0.707106781186547,
0.707106781186548,0.707106781186547,0.707106781186548,0.707106781186548,
0.707106781186548,0.707106781186547,0.707106781186547,0.707106781186548,
0.707106781186548,0.707106781186547,0.707106781186547,0.707106781186547,
0.707106781186548,0.707106781186547,0.707106781186548,0.707106781186547,
0.707106781186548,0.707106781186547,0.707106781186547,0.707106781186547,
0.707106781186548,0.707106781186547,0.707106781186548,0.707106781186547,
0.707106781186548,0.707106781186547,0.707106781186548,0.707106781186547,
0.707106781186547,0.707106781186548,0.707106781186547,0.707106781186547,
0.707106781186548,0.707106781186547,0.707106781186547,0.707106781186548,
0.707106781186547,0.707106781186547,0.707106781186547,0.707106781186548,
0.707106781186547,0.707106781186548,0.707106781186547,0.707106781186547,
0.707106781186547,0.707106781186548,0.707106781186548,0.707106781186547,
0.707106781186547,0.707106781186548,0.707106781186548,0.707106781186548,
0.707106781186547,0.707106781186548,0.707106781186547,0.707106781186548,
0.707106781186547,0.707106781186548,0.707106781186547,0.707106781186547,
0.707106781186547,0.707106781186547,0.707106781186548,0.707106781186547,
0.707106781186548,0.707106781186548,0.707106781186547,0.707106781186548,
0.707106781186547,0.707106781186547,0.707106781186547,0.707106781186547,
0.707106781186548,0.707106781186547,0.707106781186548,0.707106781186547,
0.707106781186548,0.707106781186548,0.707106781186547,0.707106781186548,
0.707106781186547,0.707106781186547,0.707106781186547,0.707106781186547,
0.707106781186548,0.707106781186547,0.707106781186548,0.707106781186548,
0.707106781186547,0.707106781186548,0.707106781186547,0.707106781186548,
0.707106781186547,0.707106781186547,0.707106781186548,0.707106781186547,
0.707106781186548,0.707106781186548,0.707106781186547,0.707106781186547,
0.707106781186548,0.707106781186548,0.707106781186547,0.707106781186547,
0.707106781186548,0.707106781186547,0.707106781186547,0.707106781186548,
0.707106781186547,0.707106781186547,0.707106781186548,0.707106781186547,
0.707106781186548,0.707106781186547,0.707106781186547,0.707106781186548,
0.707106781186547,0.707106781186548,0.707106781186547,0.707106781186548,
0.707106781186547,0.707106781186547,0.707106781186547,0.707106781186548,
0.707106781186547,0.707106781186548,0.707106781186547,0.707106781186548,
0.707106781186548,0.707106781186548,0.707106781186548,0.707106781186547,
0.707106781186547,0.707106781186547,0.707106781186548,0.707106781186547,
0.707106781186548,0.707106781186547,0.707106781186547,0.707106781186548,
0.707106781186547,0.707106781186547,0.707106781186548,0.707106781186547,
0.707106781186547,0.707106781186548,0.707106781186548,0.707106781186547,
0.707106781186548,0.707106781186547,0.707106781186547,0.707106781186548,
0.707106781186547,0.707106781186548,0.707106781186547,0.707106781186548,
0.707106781186547,0.707106781186547,0.707106781186547,0.707106781186548,
0.707106781186547,0.707106781186548,0.707106781186547,0.707106781186548,
0.707106781186547,0.707106781186547,0.707106781186548,0.707106781186548,
0.707106781186548,0.707106781186547,0.707106781186548,0.707106781186547,
0.707106781186548,0.707106781186547,0.707106781186548,0.707106781186547,
0.707106781186548,0.707106781186548,0.707106781186547,0.707106781186547,
0.707106781186547,0.707106781186548,0.707106781186547,0.707106781186547,
0.707106781186548,0.707106781186547,0.707106781186547,0.707106781186548,
0.707106781186547,0.707106781186548,0.707106781186548,0.707106781186548,
0.707106781186547,0.707106781186548,0.707106781186547,0.707106781186548,
0.707106781186547,0.707106781186548,0.707106781186547,0.707106781186548,
0.707106781186547,0.707106781186548,0.707106781186547,0.707106781186548,
0.707106781186548,0.707106781186547,0.707106781186548,0.707106781186547,
0.707106781186548,0.707106781186548,0.707106781186547,0.707106781186547,
0.707106781186548,0.707106781186547,0.707106781186547,0.707106781186548,
0.707106781186547,0.707106781186548,0.707106781186548,0.707106781186547,
0.707106781186548,0.707106781186548,0.707106781186548,0.707106781186548,
0.707106781186548,0.707106781186547,0.707106781186548,0.707106781186548,
0.707106781186548,0.707106781186547,0.707106781186548,0.707106781186547,
0.707106781186548,0.707106781186547,0.707106781186548,0.707106781186547,
0.707106781186548,0.707106781186547,0.707106781186548,0.707106781186547,
0.707106781186547,0.707106781186548,0.707106781186547,0.707106781186547,
0.707106781186548,0.707106781186547,0.707106781186548,0.707106781186547,
0.707106781186548,0.707106781186547,0.707106781186548,0.707106781186547,
0.707106781186547,0.707106781186548,0.707106781186547,0.707106781186547,
0.707106781186548,0.707106781186547,0.707106781186548,0.707106781186547,
0.707106781186547,0.707106781186548,0.707106781186548,0.707106781186547,
0.707106781186548,0.707106781186547,0.707106781186547,0.707106781186547,
0.707106781186548,0.707106781186547,0.707106781186547,0.707106781186548,
0.707106781186547,0.707106781186547,0.707106781186547,0.707106781186548,
0.707106781186548,0.707106781186547,0.707106781186548,0.707106781186547,
0.707106781186548,0.707106781186547,0.707106781186547,0.707106781186548,
0.707106781186547,0.707106781186548,0.707106781186547,0.707106781186547,
0.707106781186547,0.707106781186547,0.707106781186548,0.707106781186547,
0.707106781186547,0.707106781186547,0.707106781186547,0.707106781186547,
0.707106781186548,0.707106781186547,0.707106781186547,0.707106781186547,
0.707106781186547,0.707106781186548,0.707106781186547,0.707106781186548,
0.707106781186547,0.707106781186547,0.707106781186548,0.707106781186547,
0.707106781186548,0.707106781186547,0.707106781186547,0.707106781186548,
0.707106781186547,0.707106781186547,0.707106781186548,0.707106781186547,
0.707106781186547,0.707106781186547,0.707106781186547,0.707106781186548,
0.707106781186547,0.707106781186548,0.707106781186548,0.707106781186547,
0.707106781186548,0.707106781186548,0.707106781186547,0.707106781186547,
0.707106781186548,0.707106781186547,0.707106781186547,0.707106781186547,
0.707106781186548,0.707106781186547,0.707106781186547,0.707106781186548,
0.707106781186547,0.707106781186548,0.707106781186547,0.707106781186548,
0.707106781186547,0.707106781186547,0.707106781186548,0.707106781186547,
0.707106781186548,0.707106781186547,0.707106781186548,0.707106781186547,
0.707106781186548,0.707106781186547,0.707106781186548,0.707106781186547,
0.707106781186547,0.707106781186547,0.707106781186547,0.707106781186548,
0.707106781186548,0.707106781186547,0.707106781186548,0.707106781186548,
0.707106781186547,0.707106781186548,0.707106781186547,0.707106781186547,
0.707106781186548,0.707106781186547,0.707106781186547,0.707106781186547,
0.707106781186547,0.707106781186548,0.707106781186547,0.707106781186547,
0.707106781186547,0.707106781186548,0.707106781186547,0.707106781186547,
0.707106781186548,0.707106781186547,0.707106781186548,0.707106781186548,
0.707106781186547,0.707106781186548,0.707106781186547,0.707106781186548,
0.707106781186547,0.707106781186548,0.707106781186547,0.707106781186547,
0.707106781186548,0.707106781186547,0.707106781186548,0.707106781186548,
0.707106781186547,0.707106781186547,0.707106781186548,0.707106781186547,
0.707106781186548,0.707106781186547,0.707106781186548,0.707106781186547,
0.707106781186547,0.707106781186548,0.707106781186548,0.707106781186547,
0.707106781186548,0.707106781186548,0.707106781186547,0.707106781186548,
0.707106781186548,0.707106781186547,0.707106781186548,0.707106781186547,
0.707106781186548,0.707106781186547,0.707106781186548,0.707106781186547,
0.707106781186548,0.707106781186547,0.707106781186547,0.707106781186548,
0.707106781186547,0.707106781186547,0.707106781186548,0.707106781186547,
0.707106781186548,0.707106781186548,0.707106781186547,0.707106781186547,
0.707106781186547,0.707106781186548,0.707106781186547,0.707106781186548,
0.707106781186548,0.707106781186547,0.707106781186548,0.707106781186547,
0.707106781186548,0.707106781186547,0.707106781186548,0.707106781186547,
0.707106781186547,0.707106781186548,0.707106781186548,0.707106781186548,
0.707106781186547,0.707106781186548,0.707106781186548,0.707106781186547,
0.707106781186548,0.707106781186547,0.707106781186548,0.707106781186548,
0.707106781186548,0.707106781186548,0.707106781186548,0.707106781186548,
0.707106781186547,0.707106781186547,0.707106781186548,0.707106781186547,
0.707106781186547,0.707106781186548,0.707106781186547,0.707106781186547,
0.707106781186548,0.707106781186547,0.707106781186548,0.707106781186547,
0.707106781186548,0.707106781186547,0.707106781186547,0.707106781186547,
0.707106781186548,0.707106781186547,0.707106781186547,0.707106781186548,
0.707106781186547,0.707106781186548,0.707106781186547,0.707106781186548,
0.707106781186547,0.707106781186547,0.707106781186547,0.707106781186547,
0.707106781186548,0.707106781186547,0.707106781186547,0.707106781186548,
0.707106781186548,0.707106781186547,0.707106781186548,0.707106781186547,
0.707106781186548,0.707106781186547,0.707106781186547,0.707106781186548,
0.707106781186547,0.707106781186548,0.707106781186547,0.707106781186548,
0.707106781186547,0.707106781186548,0.707106781186548,0.707106781186547,
0.707106781186548,0.707106781186547,0.707106781186547,0.707106781186548,
0.707106781186547,0.707106781186547,0.707106781186548,0.707106781186548,
0.707106781186548,0.707106781186547,0.707106781186548,0.707106781186547,
0.707106781186547,0.707106781186547,0.707106781186548,0.707106781186547,
0.707106781186548,0.707106781186548,0.707106781186548,0.707106781186547,
0.707106781186547,0.707106781186547,0.707106781186547,0.707106781186548,
0.707106781186547,0.707106781186547,0.707106781186548,0.707106781186547,
0.707106781186548,0.707106781186547,0.707106781186547,0.707106781186548,
0.707106781186547,0.707106781186548,0.707106781186547,0.707106781186548,
0.707106781186547,0.707106781186547,0.707106781186547,0.707106781186547,
0.707106781186547,0.707106781186547,0.707106781186548,0.707106781186547,
0.707106781186547,0.707106781186548,0.707106781186548,0.707106781186547,
0.707106781186548,0.707106781186548,0.707106781186547,0.707106781186547,
0.707106781186548,0.707106781186547,0.707106781186547,0.707106781186548,
0.707106781186547,0.707106781186548,0.707106781186548,0.707106781186548,
0.707106781186547,0.707106781186547,0.707106781186547,0.707106781186547,
0.707106781186548,0.707106781186548,0.707106781186548,0.707106781186547,
0.707106781186548,0.707106781186547,0.707106781186548,0.707106781186548,
0.707106781186547,0.707106781186548,0.707106781186547,0.707106781186548,
0.707106781186548,0.707106781186547,0.707106781186547,0.707106781186548,
0.707106781186547,0.707106781186548,0.707106781186547,0.707106781186548,
0.707106781186548,0.707106781186548,0.707106781186547,0.707106781186548,
0.707106781186547,0.707106781186547,0.707106781186547,0.707106781186547,
0.707106781186548,0.707106781186548,0.707106781186547,0.707106781186547,
0.707106781186547,0.707106781186548,0.707106781186547,0.707106781186547,
0.707106781186548,0.707106781186547,0.707106781186548,0.707106781186548,
0.707106781186548,0.707106781186547,0.707106781186547,0.707106781186547,
0.707106781186547,0.707106781186548,0.707106781186548,0.707106781186547,
0.707106781186548,0.707106781186547,0.707106781186548,0.707106781186548,
0.707106781186547,0.707106781186548,0.707106781186547,0.707106781186548,
0.707106781186547,0.707106781186547,0.707106781186547,0.707106781186548,
0.707106781186547,0.707106781186548,0.707106781186547,0.707106781186548,
0.707106781186547,0.707106781186548,0.707106781186547,0.707106781186548,
0.707106781186547,0.707106781186547,0.707106781186548,0.707106781186547,
0.707106781186548,0.707106781186547,0.707106781186547,0.707106781186548,
0.707106781186548,0.707106781186547,0.707106781186548,0.707106781186548,
0.707106781186547,0.707106781186548,0.707106781186547,0.707106781186548,
0.707106781186547,0.707106781186547,0.707106781186547,0.707106781186548,
0.707106781186547,0.707106781186547,0.707106781186548,0.707106781186547,
0.707106781186548,0.707106781186547,0.707106781186548,0.707106781186548,
0.707106781186547,0.707106781186548,0.707106781186547,0.707106781186548,
0.707106781186548,0.707106781186548,0.707106781186548,0.707106781186547,
0.707106781186547,0.707106781186548,0.707106781186547,0.707106781186547,
0.707106781186548,0.707106781186548,0.707106781186547,0.707106781186547,
0.707106781186548,0.707106781186547,0.707106781186547,0.707106781186548,
0.707106781186547,0.707106781186548,0.707106781186547,0.707106781186548,
0.707106781186547,0.707106781186547,0.707106781186547,0.707106781186548,
0.707106781186547,0.707106781186547,0.707106781186548,0.707106781186547,
0.707106781186548,0.707106781186548,0.707106781186548,0.707106781186547,
0.707106781186547,0.707106781186547,0.707106781186548,0.707106781186548,
0.707106781186547,0.707106781186547,0.707106781186547,0.707106781186547,
0.707106781186548,0.707106781186548,0.707106781186547,0.707106781186547,
0.707106781186547,0.707106781186548,0.707106781186548,0.707106781186547,
0.707106781186548,0.707106781186547,0.707106781186548,0.707106781186547,
0.707106781186548,0.707106781186548,0.707106781186547,0.707106781186548,
0.707106781186548,0.707106781186548,0.707106781186547,0.707106781186547,
0.707106781186547,0.707106781186548,0.707106781186548,0.707106781186548,
0.707106781186547,0.707106781186547,0.707106781186548,0.707106781186548,
0.707106781186547,0.707106781186548,0.707106781186547,0.707106781186547,
0.707106781186548,0.707106781186547,0.707106781186548,0.707106781186547,
0.707106781186547,0.707106781186548,0.707106781186547,0.707106781186548,
0.707106781186548,0.707106781186547,0.707106781186547,0.707106781186548,
0.707106781186547,0.707106781186548,0.707106781186547,0.707106781186547,
0.707106781186548,0.707106781186547,0.707106781186548,0.707106781186547,
0.707106781186548,0.707106781186547,0.707106781186547,0.707106781186548,
0.707106781186547,0.707106781186547,0.707106781186547,0.707106781186547,
0.707106781186547,0.707106781186547,0.707106781186548,0.707106781186547,
0.707106781186548,0.707106781186548,0.707106781186548,0.707106781186547,
0.707106781186547,0.707106781186547,0.707106781186548,0.707106781186547,
0.707106781186548,0.707106781186547,0.707106781186547,0.707106781186548,
0.707106781186547,0.707106781186547,0.707106781186547,0.707106781186547,
0.707106781186547,0.707106781186548,0.707106781186547,0.707106781186548,
0.707106781186547,0.707106781186547,0.707106781186548,0.707106781186548,
0.707106781186547,0.707106781186547,0.707106781186547,0.707106781186548,
0.707106781186547,0.707106781186547,0.707106781186548,0.707106781186548,
0.707106781186547,0.707106781186548,0.707106781186547,0.707106781186548,
0.707106781186548,0.707106781186547,0.707106781186547,0.707106781186547,
0.707106781186548,0.707106781186548,0.707106781186547,0.707106781186548,
0.707106781186547,0.707106781186548,0.707106781186548,0.707106781186547,
0.707106781186548,0.707106781186547,0.707106781186547,0.707106781186547,
0.707106781186548,0.707106781186547,0.707106781186548,0.707106781186547,
0.707106781186548,0.707106781186547,0.707106781186547,0.707106781186547,
0.707106781186547,0.707106781186547,0.707106781186548,0.707106781186547,
0.707106781186548,0.707106781186547,0.707106781186548,0.707106781186547,
0.707106781186548,0.707106781186547,0.707106781186547,0.707106781186547,
0.707106781186547,0.707106781186547,0.707106781186548,0.707106781186548,
0.707106781186548,0.707106781186547,0.707106781186548,0.707106781186547,
0.707106781186548,0.707106781186547,0.707106781186547,0.707106781186548,
0.707106781186547,0.707106781186548,0.707106781186547,0.707106781186547,
0.707106781186547,0.707106781186548,0.707106781186548,0.707106781186547,
0.707106781186548,0.707106781186547,0.707106781186548,0.707106781186548,
0.707106781186547,0.707106781186548,0.707106781186547,0.707106781186548,
0.707106781186548,0.707106781186547,0.707106781186547,0.707106781186547,
0.707106781186547,0.707106781186547,0.707106781186547,0.707106781186548,
0.707106781186548,0.707106781186547,0.707106781186548,0.707106781186547,
0.707106781186547,0.707106781186548,0.707106781186547,0.707106781186547,
0.707106781186548,0.707106781186547,0.707106781186547,0.707106781186547,
0.707106781186548,0.707106781186547,0.707106781186547,0.707106781186548,
0.707106781186547,0.707106781186548,0.707106781186548,0.707106781186547,
0.707106781186547,0.707106781186547,0.707106781186548,0.707106781186547,
0.707106781186547,0.707106781186548,0.707106781186548,0.707106781186548,
0.707106781186548,0.707106781186547,0.707106781186548,0.707106781186548,
0.707106781186547,0.707106781186547,0.707106781186548,0.707106781186547,
0.707106781186548,0.707106781186547,0.707106781186547,0.707106781186548,
0.707106781186547,0.707106781186547,0.707106781186548,0.707106781186547,
0.707106781186548,0.707106781186547,0.707106781186548,0.707106781186547,
0.707106781186548,0.707106781186547,0.707106781186548,0.707106781186547,
0.707106781186548,0.707106781186548,0.707106781186547,0.707106781186547,
0.707106781186548,0.707106781186548,0.707106781186547,0.707106781186547,
0.707106781186547,0.707106781186547,0.707106781186547,0.707106781186548,
0.707106781186547,0.707106781186547,0.707106781186548,0.707106781186547,
0.707106781186548,0.707106781186548,0.707106781186547,0.707106781186548,
0.707106781186547,0.707106781186548,0.707106781186547,0.707106781186548,
0.707106781186547,0.707106781186547,0.707106781186547,0.707106781186547,
0.707106781186547,0.707106781186547,0.707106781186548,0.707106781186547,
0.707106781186548,0.707106781186547,0.707106781186547,0.707106781186547,
0.707106781186548,0.707106781186547,0.707106781186548,0.707106781186548,
0.707106781186547,0.707106781186547,0.707106781186548,0.707106781186547,
0.707106781186548,0.707106781186547,0.707106781186548,0.707106781186547,
0.707106781186548,0.707106781186547,0.707106781186547,0.707106781186548,
0.707106781186547,0.707106781186548,0.707106781186547,0.707106781186548,
0.707106781186548,0.707106781186548,0.707106781186548,0.707106781186547,
0.707106781186548,0.707106781186548,0.707106781186548,0.707106781186547,
0.707106781186548,0.707106781186548,0.707106781186547,0.707106781186548,
0.707106781186547,0.707106781186548,0.707106781186547,0.707106781186547,
0.707106781186547,0.707106781186548,0.707106781186548,0.707106781186547,
0.707106781186548,0.707106781186547,0.707106781186548,0.707106781186547,
0.707106781186548,0.707106781186548,0.707106781186547,0.707106781186548,
0.707106781186547,0.707106781186547,0.707106781186548,0.707106781186547,
0.707106781186547,0.707106781186547,0.707106781186548,0.707106781186547,
0.707106781186548,0.707106781186548,0.707106781186547,0.707106781186548,
0.707106781186547,0.707106781186548,0.707106781186548,0.707106781186548,
0.707106781186548,0.707106781186547,0.707106781186548,0.707106781186547,
0.707106781186548,0.707106781186547,0.707106781186548,0.707106781186547,
0.707106781186547,0.707106781186547,0.707106781186547,0.707106781186548,
0.707106781186547,0.707106781186548,0.707106781186547,0.707106781186547,
0.707106781186548,0.707106781186547,0.707106781186548,0.707106781186547,
0.707106781186548,0.707106781186547,0.707106781186548,0.707106781186548,
0.707106781186548,0.707106781186548,0.707106781186547,0.707106781186548,
0.707106781186548,0.707106781186547,0.707106781186548,0.707106781186547,
0.707106781186548,0.707106781186547,0.707106781186548,0.707106781186547,
0.707106781186547,0.707106781186548,0.707106781186547,0.707106781186548,
0.707106781186547,0.707106781186547,0.707106781186548,0.707106781186547,
0.707106781186548,0.707106781186547,0.707106781186547,0.707106781186548,
0.707106781186548,0.707106781186548,0.707106781186548,0.707106781186548,
0.707106781186548,0.707106781186548,0.707106781186548,0.707106781186548,
0.707106781186547,0.707106781186548,0.707106781186547,0.707106781186547,
0.707106781186548,0.707106781186547,0.707106781186548,0.707106781186548,
0.707106781186547,0.707106781186547,0.707106781186548,0.707106781186548,
0.707106781186547,0.707106781186547,0.707106781186547,0.707106781186547,
0.707106781186547,0.707106781186548,0.707106781186547,0.707106781186548,
0.707106781186548,0.707106781186548,0.707106781186547,0.707106781186548,
0.707106781186547,0.707106781186548,0.707106781186547,0.707106781186548,
0.707106781186547,0.707106781186548,0.707106781186548,0.707106781186547,
0.707106781186547,0.707106781186548,0.707106781186548,0.707106781186548,
0.707106781186547,0.707106781186547,0.707106781186548,0.707106781186547,
0.707106781186547,0.707106781186548,0.707106781186547,0.707106781186548,
0.707106781186547,0.707106781186547,0.707106781186548,0.707106781186548,
0.707106781186548,0.707106781186547,0.707106781186547,0.707106781186548,
0.707106781186547,0.707106781186548,0.707106781186547,0.707106781186548,
0.707106781186547,0.707106781186548,0.707106781186548,0.707106781186547,
0.707106781186548,0.707106781186547,0.707106781186548,0.707106781186547,
0.707106781186547,0.707106781186547,0.707106781186548,0.707106781186547,
0.707106781186548,0.707106781186547,0.707106781186547,0.707106781186547,
0.707106781186548,0.707106781186547,0.707106781186547,0.707106781186548,
0.707106781186548,0.707106781186547,0.707106781186548,0.707106781186547,
0.707106781186548,0.707106781186548,0.707106781186547,0.707106781186548,
0.707106781186547,0.707106781186547,0.707106781186548,0.707106781186547,
0.707106781186547,0.707106781186547,0.707106781186548,0.707106781186547,
0.707106781186548,0.707106781186547,0.707106781186548,0.707106781186548,
0.707106781186548,0.707106781186547,0.707106781186548,0.707106781186548,
0.707106781186548,0.707106781186547,0.707106781186548,0.707106781186547,
0.707106781186547,0.707106781186548,0.707106781186547,0.707106781186547,
0.707106781186548,0.707106781186548,0.707106781186547,0.707106781186548,
0.707106781186547,0.707106781186548,0.707106781186548,0.707106781186547,
0.707106781186548,0.707106781186547,0.707106781186548,0.707106781186547,
0.707106781186548,0.707106781186547,0.707106781186548,0.707106781186548,
0.707106781186548,0.707106781186547,0.707106781186548,0.707106781186548,
0.707106781186547,0.707106781186547,0.707106781186548,0.707106781186547,
0.707106781186548,0.707106781186548,0.707106781186547,0.707106781186548,
0.707106781186548,0.707106781186547,0.707106781186548,0.707106781186548,
0.707106781186547,0.707106781186547,0.707106781186548,0.707106781186547,
0.707106781186548,0.707106781186547,0.707106781186548,0.707106781186547,
0.707106781186548,0.707106781186548,0.707106781186548,0.707106781186547,
0.707106781186548,0.707106781186547,0.707106781186548,0.707106781186547,
0.707106781186548,0.707106781186547,0.707106781186548,0.707106781186547,
0.707106781186548,0.707106781186547,0.707106781186548,0.707106781186547,
0.707106781186547,0.707106781186547,0.707106781186548,0.707106781186547,
0.707106781186548,0.707106781186547,0.707106781186548,0.707106781186547,
0.707106781186548,0.707106781186547,0.707106781186548,0.707106781186548,
0.707106781186548,0.707106781186547,0.707106781186548,0.707106781186547,
0.707106781186548,0.707106781186548,0.707106781186547,0.707106781186548,
0.707106781186547,0.707106781186548,0.707106781186547,0.707106781186548,
0.707106781186547,0.707106781186548,0.707106781186547,0.707106781186547,
0.707106781186547,0.707106781186548,0.707106781186547,0.707106781186547,
0.707106781186548,0.707106781186547,0.707106781186548,0.707106781186547,
0.707106781186547,0.707106781186548,0.707106781186547,0.707106781186548,
0.707106781186547,0.707106781186548,0.707106781186548,0.707106781186548,
0.707106781186547,0.707106781186547,0.707106781186548,0.707106781186548,
0.707106781186547,0.707106781186548,0.707106781186547,0.707106781186547,
0.707106781186547,0.707106781186548,0.707106781186547,0.707106781186548,
0.707106781186547,0.707106781186548,0.707106781186548,0.707106781186548,
0.707106781186547,0.707106781186547,0.707106781186547,0.707106781186547,
0.707106781186547,0.707106781186547,0.707106781186548,0.707106781186547,
0.707106781186548,0.707106781186547,0.707106781186548,0.707106781186547,
0.707106781186547,0.707106781186548,0.707106781186547,0.707106781186547,
0.707106781186548,0.707106781186548,0.707106781186547,0.707106781186547,
0.707106781186547,0.707106781186548,0.707106781186547,0.707106781186547,
0.707106781186548,0.707106781186548),(1.,1.,1.,1.,1.,1.,1.,1.,1.,1.,1.,
1.,1.,1.,1.,1.,1.,1.,1.,1.,1.,1.,1.,1.,1.,1.,1.,1.,1.,1.,1.,1.,1.,1.,1.,
1.,1.,1.,1.,1.,1.,1.,1.,1.,1.,1.,1.,1.,1.,1.,1.,1.,1.,1.,1.,1.,1.,1.,1.,
1.,1.,1.,1.,1.,1.,1.,1.,1.,1.,1.,1.,1.,1.,1.,1.,1.,1.,1.,1.,1.,1.,1.,1.,
1.,1.,1.,1.,1.,1.,1.,1.,1.,1.,1.,1.,1.,1.,1.,1.,1.,1.,1.,1.,1.,1.,1.,1.,
1.,1.,1.,1.,1.,1.,1.,1.,1.,1.,1.,1.,1.,1.,1.,1.,1.,1.,1.,1.,1.,1.,1.,1.,
1.,1.,1.,1.,1.,1.,1.,1.,1.,1.,1.,1.,1.,1.,1.,1.,1.,1.,1.,1.,1.,1.,1.,1.,
1.,1.,1.,1.,1.,1.,1.,1.,1.,1.,1.,1.,1.,1.,1.,1.,1.,1.,1.,1.,1.,1.,1.,1.,
1.,1.,1.,1.,1.,1.,1.,1.,1.,1.,1.,1.,1.,1.,1.,1.,1.,1.,1.,1.,1.,1.,1.,1.,
1.,1.,1.,1.,1.,1.,1.,1.,1.,1.,1.,1.,1.,1.,1.,1.,1.,1.,1.,1.,1.,1.,1.,1.,
1.,1.,1.,1.,1.,1.,1.,1.,1.,1.,1.,1.,1.,1.,1.,1.,1.,1.,1.,1.,1.,1.,1.,1.,
1.,1.,1.,1.,1.,1.,1.,1.,1.,1.,1.,1.,1.,1.,1.,1.,1.,1.,1.,1.,1.,1.,1.,1.,
1.,1.,1.,1.,1.,1.,1.,1.,1.,1.,1.,1.,1.,1.,1.,1.,1.,1.,1.,1.,1.,1.,1.,1.,
1.,1.,1.,1.,1.,1.,1.,1.,1.,1.,1.,1.,1.,1.,1.,1.,1.,1.,1.,1.,1.,1.,1.,1.,
1.,1.,1.,1.,1.,1.,1.,1.,1.,1.,1.,1.,1.,1.,1.,1.,1.,1.,1.,1.,1.,1.,1.,1.,
1.,1.,1.,1.,1.,1.,1.,1.,1.,1.,1.,1.,1.,1.,1.,1.,1.,1.,1.,1.,1.,1.,1.,1.,
1.,1.,1.,1.,1.,1.,1.,1.,1.,1.,1.,1.,1.,1.,1.,1.,1.,1.,1.,1.,1.,1.,1.,1.,
1.,1.,1.,1.,1.,1.,1.,1.,1.,1.,1.,1.,1.,1.,1.,1.,1.,1.,1.,1.,1.,1.,1.,1.,
1.,1.,1.,1.,1.,1.,1.,1.,1.,1.,1.,1.,1.,1.,1.,1.,1.,1.,1.,1.,1.,1.,1.,1.,
1.,1.,1.,1.,1.,1.,1.,1.,1.,1.,1.,1.,1.,1.,1.,1.,1.,1.,1.,1.,1.,1.,1.,1.,
1.,1.,1.,1.,1.,1.,1.,1.,1.,1.,1.,1.,1.,1.,1.,1.,1.,1.,1.,1.,1.,1.,1.,1.,
1.,1.,1.,1.,1.,1.,1.,1.,1.,1.,1.,1.,1.,1.,1.,1.,1.,1.,1.,1.,1.,1.,1.,1.,
1.,1.,1.,1.,1.,1.,1.,1.,1.,1.,1.,1.,1.,1.,1.,1.,1.,1.,1.,1.,1.,1.,1.,1.,
1.,1.,1.,1.,1.,1.,1.,1.,1.,1.,1.,1.,1.,1.,1.,1.,1.,1.,1.,1.,1.,1.,1.,1.,
1.,1.,1.,1.,1.,1.,1.,1.,1.,1.,1.,1.,1.,1.,1.,1.,1.,1.,1.,1.,1.,1.,1.,1.,
1.,1.,1.,1.,1.,1.,1.,1.,1.,1.,1.,1.,1.,1.,1.,1.,1.,1.,1.,1.,1.,1.,1.,1.,
1.,1.,1.,1.,1.,1.,1.,1.,1.,1.,1.,1.,1.,1.,1.,1.,1.,1.,1.,1.,1.,1.,1.,1.,
1.,1.,1.,1.,1.,1.,1.,1.,1.,1.,1.,1.,1.,1.,1.,1.,1.,1.,1.,1.,1.,1.,1.,1.,
1.,1.,1.,1.,1.,1.,1.,1.,1.,1.,1.,1.,1.,1.,1.,1.,1.,1.,1.,1.,1.,1.,1.,1.,
1.,1.,1.,1.,1.,1.,1.,1.,1.,1.,1.,1.,1.,1.,1.,1.,1.,1.,1.,1.,1.,1.,1.,1.,
1.,1.,1.,1.,1.,1.,1.,1.,1.,1.,1.,1.,1.,1.,1.,1.,1.,1.,1.,1.,1.,1.,1.,1.,
1.,1.,1.,1.,1.,1.,1.,1.,1.,1.,1.,1.,1.,1.,1.,1.,1.,1.,1.,1.,1.,1.,1.,1.,
1.,1.,1.,1.,1.,1.,1.,1.,1.,1.,1.,1.,1.,1.,1.,1.,1.,1.,1.,1.,1.,1.,1.,1.,
1.,1.,1.,1.,1.,1.,1.,1.,1.,1.,1.,1.,1.,1.,1.,1.,1.,1.,1.,1.,1.,1.,1.,1.,
1.,1.,1.,1.,1.,1.,1.,1.,1.,1.,1.,1.,1.,1.,1.,1.,1.,1.,1.,1.,1.,1.,1.,1.,
1.,1.,1.,1.,1.,1.,1.,1.,1.,1.,1.,1.,1.,1.,1.,1.,1.,1.,1.,1.,1.,1.,1.,1.,
1.,1.,1.,1.,1.,1.,1.,1.,1.,1.,1.,1.,1.,1.,1.,1.,1.,1.,1.,1.,1.,1.,1.,1.,
1.,1.,1.,1.,1.,1.,1.,1.,1.,1.,1.,1.,1.,1.,1.,1.,1.,1.,1.,1.,1.,1.,1.,1.,
1.,1.,1.,1.,1.,1.,1.,1.,1.,1.,1.,1.,1.,1.,1.,1.,1.,1.,1.,1.,1.,1.,1.,1.,
1.,1.,1.,1.,1.,1.,1.,1.,1.,1.,1.,1.,1.,1.,1.,1.,1.,1.,1.,1.,1.,1.,1.,1.,
1.,1.,1.,1.,1.,1.,1.,1.,1.,1.,1.,1.,1.,1.,1.,1.,1.,1.,1.,1.,1.,1.,1.,1.,
1.,1.,1.,1.,1.,1.,1.,1.,1.,1.,1.,1.,1.,1.,1.,1.,1.,1.,1.,1.,1.,1.,1.,1.,
1.,1.,1.,1.,1.,1.,1.,1.,1.,1.,1.,1.,1.,1.,1.,1.,1.,1.,1.,1.,1.,1.,1.,1.,
1.,1.,1.,1.,1.,1.,1.,1.,1.,1.,1.,1.,1.,1.,1.,1.,1.,1.,1.,1.,1.,1.,1.,1.,
1.,1.,1.,1.,1.,1.,1.,1.,1.,1.,1.,1.,1.,1.,1.,1.,1.,1.,1.,1.,1.,1.,1.,1.,
1.,1.,1.,1.,1.,1.,1.,1.,1.,1.,1.,1.,1.,1.,1.,1.,1.,1.,1.,1.,1.,1.,1.,1.,
1.,1.,1.,1.,1.,1.,1.,1.,1.,1.,1.,1.,1.,1.,1.,1.,1.,1.,1.,1.,1.,1.,1.,1.,
1.,1.,1.,1.,1.,1.,1.,1.,1.,1.,1.,1.,1.,1.,1.,1.,1.,1.,1.,1.,1.,1.,1.,1.,
1.,1.,1.,1.,1.,1.,1.,1.,1.,1.,1.,1.,1.,1.,1.,1.,1.,1.,1.,1.,1.,1.,1.,1.,
1.,1.,1.,1.,1.,1.,1.,1.,1.,1.,1.,1.,1.,1.,1.,1.,1.,1.,1.,1.,1.,1.,1.,1.,
1.,1.,1.,1.,1.,1.,1.,1.,1.,1.,1.,1.,1.,1.,1.,1.,1.,1.,1.,1.,1.,1.,1.,1.,
1.,1.,1.,1.,1.,1.,1.,1.,1.,1.,1.,1.,1.,1.,1.,1.,1.,1.,1.,1.,1.,1.,1.,1.,
1.,1.,1.,1.,1.,1.,1.,1.,1.,1.,1.,1.,1.,1.,1.,1.,1.,1.,1.,1.,1.,1.,1.,1.,
1.,1.,1.,1.,1.,1.,1.,1.,1.,1.,1.,1.,1.,1.,1.,1.,1.,1.,1.,1.,1.,1.,1.,1.,
1.,1.,1.,1.,1.,1.,1.,1.,1.,1.,1.,1.,1.,1.,1.,1.,1.,1.,1.,1.,1.,1.,1.,1.,
1.,1.,1.,1.,1.,1.,1.,1.,1.,1.,1.,1.,1.,1.,1.,1.,1.,1.,1.,1.,1.,1.,1.,1.,
1.,1.,1.,1.,1.,1.,1.,1.,1.,1.,1.,1.,1.,1.,1.,1.,1.,1.,1.,1.,1.,1.,1.,1.,
1.,1.,1.,1.,1.,1.,1.,1.,1.,1.,1.,1.,1.,1.,1.,1.,1.,1.,1.,1.,1.,1.,1.,1.,
1.,1.,1.,1.,1.,1.,1.,1.,1.,1.,1.,1.,1.,1.,1.,1.,1.,1.,1.,1.,1.,1.,1.,1.,
1.,1.,1.,1.,1.,1.,1.,1.,1.,1.,1.,1.,1.,1.,1.,1.,1.,1.,1.,1.,1.,1.,1.,1.,
1.,1.,1.,1.,1.,1.,1.,1.,1.,1.,1.,1.,1.,1.,1.,1.,1.,1.,1.,1.,1.,1.,1.,1.,
1.,1.,1.,1.,1.,1.,1.,1.,1.,1.,1.,1.,1.,1.,1.,1.,1.,1.,1.,1.,1.,1.,1.,1.,
1.,1.,1.,1.,1.,1.,1.,1.,1.,1.,1.,1.,1.,1.,1.,1.,1.,1.,1.,1.,1.,1.,1.,1.,
1.,1.,1.,1.,1.,1.,1.,1.,1.,1.,1.,1.,1.,1.,1.,1.,1.,1.,1.,1.,1.,1.,1.,1.,
1.,1.,1.,1.,1.,1.,1.,1.,1.,1.,1.,1.,1.,1.,1.,1.,1.,1.,1.,1.,1.,1.,1.,1.,
1.,1.,1.,1.,1.,1.,1.,1.,1.,1.,1.,1.,1.,1.,1.,1.,1.,1.,1.,1.,1.,1.,1.,1.,
1.,1.,1.,1.,1.,1.,1.,1.,1.,1.,1.,1.,1.,1.,1.,1.,1.,1.,1.,1.,1.,1.,1.,1.,
1.,1.,1.,1.,1.,1.,1.,1.,1.,1.,1.,1.,1.,1.,1.,1.,1.,1.,1.,1.,1.,1.,1.,1.,
1.,1.,1.,1.,1.,1.,1.,1.,1.,1.,1.,1.,1.,1.,1.,1.,1.,1.,1.,1.,1.,1.,1.,1.,
1.,1.,1.,1.,1.,1.,1.,1.,1.,1.,1.,1.,1.,1.,1.,1.,1.,1.,1.,1.,1.,1.,1.,1.,
1.,1.,1.,1.,1.,1.,1.,1.,1.,1.,1.,1.,1.,1.,1.,1.,1.,1.,1.,1.,1.,1.,1.,1.,
1.,1.,1.,1.,1.,1.,1.,1.,1.,1.,1.,1.,1.,1.,1.,1.,1.,1.,1.,1.,1.,1.,1.,1.,
1.,1.,1.,1.,1.,1.,1.,1.,1.,1.,1.,1.,1.,1.,1.,1.,1.,1.,1.,1.,1.,1.,1.,1.,
1.,1.,1.,1.,1.,1.,1.,1.,1.,1.,1.,1.,1.,1.,1.,1.,1.,1.,1.,1.,1.,1.,1.,1.,
1.,1.,1.,1.,1.,1.,1.,1.,1.,1.,1.,1.,1.,1.,1.,1.,1.,1.,1.,1.,1.,1.,1.,1.,
1.,1.,1.,1.,1.,1.,1.,1.,1.,1.,1.,1.,1.,1.,1.,1.,1.,1.,1.,1.,1.,1.,1.,1.,
1.,1.,1.,1.,1.,1.,1.,1.,1.,1.,1.,1.,1.,1.,1.,1.,1.,1.,1.,1.,1.,1.,1.,1.,
1.,1.,1.,1.,1.,1.,1.,1.,1.,1.,1.,1.,1.,1.,1.,1.,1.,1.,1.,1.,1.,1.,1.,1.,
1.,1.,1.,1.,1.,1.,1.,1.,1.,1.,1.,1.,1.,1.,1.,1.,1.,1.,1.,1.,1.,1.,1.,1.,
1.,1.,1.,1.,1.,1.,1.,1.,1.,1.,1.,1.,1.,1.,1.,1.,1.,1.,1.,1.,1.,1.,1.,1.,
1.,1.,1.,1.,1.,1.,1.,1.,1.,1.,1.,1.,1.,1.,1.,1.,1.,1.,1.,1.,1.,1.,1.,1.,
1.,1.,1.,1.,1.,1.,1.,1.,1.,1.,1.,1.,1.,1.,1.,1.,1.,1.,1.,1.,1.,1.,1.,1.,
1.,1.,1.,1.,1.,1.,1.,1.,1.,1.,1.,1.,1.,1.,1.,1.,1.,1.,1.,1.,1.,1.,1.,1.,
1.,1.,1.,1.,1.,1.,1.,1.,1.,1.,1.,1.,1.,1.,1.,1.,1.,1.,1.,1.,1.,1.,1.,1.,
1.,1.,1.,1.,1.,1.,1.,1.,1.,1.,1.,1.,1.,1.,1.,1.,1.,1.,1.,1.,1.,1.,1.,1.,
1.,1.,1.,1.,1.,1.,1.,1.,1.,1.,1.,1.,1.,1.,1.,1.,1.,1.,1.,1.,1.,1.,1.,1.),
(0.707106781186548,0.707106781186548,0.707106781186548,0.707106781186547,
0.707106781186547,0.707106781186548,0.707106781186547,0.707106781186547,
0.707106781186547,0.707106781186547,0.707106781186547,0.707106781186548,
0.707106781186548,0.707106781186548,0.707106781186547,0.707106781186548,
0.707106781186547,0.707106781186547,0.707106781186548,0.707106781186547,
0.707106781186548,0.707106781186547,0.707106781186548,0.707106781186547,
0.707106781186548,0.707106781186547,0.707106781186547,0.707106781186547,
0.707106781186547,0.707106781186547,0.707106781186548,0.707106781186547,
0.707106781186547,0.707106781186548,0.707106781186547,0.707106781186547,
0.707106781186548,0.707106781186547,0.707106781186547,0.707106781186548,
0.707106781186548,0.707106781186547,0.707106781186548,0.707106781186547,
0.707106781186547,0.707106781186547,0.707106781186548,0.707106781186548,
0.707106781186547,0.707106781186547,0.707106781186548,0.707106781186547,
0.707106781186548,0.707106781186547,0.707106781186547,0.707106781186547,
0.707106781186547,0.707106781186547,0.707106781186548,0.707106781186547,
0.707106781186548,0.707106781186547,0.707106781186548,0.707106781186547,
0.707106781186548,0.707106781186547,0.707106781186547,0.707106781186548,
0.707106781186547,0.707106781186547,0.707106781186548,0.707106781186547,
0.707106781186548,0.707106781186547,0.707106781186548,0.707106781186548,
0.707106781186547,0.707106781186548,0.707106781186547,0.707106781186547,
0.707106781186548,0.707106781186547,0.707106781186547,0.707106781186547,
0.707106781186548,0.707106781186547,0.707106781186547,0.707106781186547,
0.707106781186547,0.707106781186547,0.707106781186547,0.707106781186548,
0.707106781186548,0.707106781186547,0.707106781186548,0.707106781186547,
0.707106781186548,0.707106781186548,0.707106781186547,0.707106781186548,
0.707106781186548,0.707106781186548,0.707106781186547,0.707106781186548,
0.707106781186547,0.707106781186548,0.707106781186548,0.707106781186548,
0.707106781186547,0.707106781186547,0.707106781186547,0.707106781186548,
0.707106781186548,0.707106781186548,0.707106781186547,0.707106781186547,
0.707106781186547,0.707106781186548,0.707106781186548,0.707106781186547,
0.707106781186547,0.707106781186548,0.707106781186547,0.707106781186547,
0.707106781186547,0.707106781186547,0.707106781186548,0.707106781186547,
0.707106781186548,0.707106781186547,0.707106781186547,0.707106781186547,
0.707106781186548,0.707106781186548,0.707106781186547,0.707106781186548,
0.707106781186548,0.707106781186547,0.707106781186548,0.707106781186547,
0.707106781186548,0.707106781186547,0.707106781186548,0.707106781186547,
0.707106781186547,0.707106781186548,0.707106781186547,0.707106781186547,
0.707106781186548,0.707106781186547,0.707106781186547,0.707106781186548,
0.707106781186547,0.707106781186548,0.707106781186547,0.707106781186547,
0.707106781186548,0.707106781186548,0.707106781186547,0.707106781186548,
0.707106781186547,0.707106781186548,0.707106781186547,0.707106781186548,
0.707106781186547,0.707106781186548,0.707106781186547,0.707106781186548,
0.707106781186547,0.707106781186548,0.707106781186547,0.707106781186548,
0.707106781186547,0.707106781186547,0.707106781186548,0.707106781186547,
0.707106781186548,0.707106781186547,0.707106781186548,0.707106781186547,
0.707106781186548,0.707106781186547,0.707106781186547,0.707106781186548,
0.707106781186547,0.707106781186548,0.707106781186548,0.707106781186548,
0.707106781186547,0.707106781186547,0.707106781186547,0.707106781186547,
0.707106781186548,0.707106781186547,0.707106781186548,0.707106781186548,
0.707106781186547,0.707106781186547,0.707106781186548,0.707106781186548,
0.707106781186547,0.707106781186547,0.707106781186548,0.707106781186547,
0.707106781186548,0.707106781186547,0.707106781186547,0.707106781186547,
0.707106781186547,0.707106781186547,0.707106781186547,0.707106781186547,
0.707106781186548,0.707106781186547,0.707106781186548,0.707106781186547,
0.707106781186548,0.707106781186548,0.707106781186547,0.707106781186548,
0.707106781186548,0.707106781186548,0.707106781186548,0.707106781186547,
0.707106781186548,0.707106781186547,0.707106781186548,0.707106781186547,
0.707106781186547,0.707106781186548,0.707106781186548,0.707106781186547,
0.707106781186547,0.707106781186547,0.707106781186547,0.707106781186547,
0.707106781186548,0.707106781186548,0.707106781186547,0.707106781186547,
0.707106781186548,0.707106781186548,0.707106781186547,0.707106781186548,
0.707106781186547,0.707106781186548,0.707106781186548,0.707106781186547,
0.707106781186547,0.707106781186548,0.707106781186547,0.707106781186547,
0.707106781186548,0.707106781186547,0.707106781186548,0.707106781186547,
0.707106781186548,0.707106781186547,0.707106781186547,0.707106781186548,
0.707106781186548,0.707106781186547,0.707106781186547,0.707106781186548,
0.707106781186547,0.707106781186547,0.707106781186548,0.707106781186547,
0.707106781186548,0.707106781186547,0.707106781186548,0.707106781186547,
0.707106781186548,0.707106781186547,0.707106781186547,0.707106781186547,
0.707106781186547,0.707106781186547,0.707106781186547,0.707106781186548,
0.707106781186547,0.707106781186548,0.707106781186547,0.707106781186548,
0.707106781186548,0.707106781186547,0.707106781186548,0.707106781186548,
0.707106781186547,0.707106781186548,0.707106781186547,0.707106781186547,
0.707106781186547,0.707106781186548,0.707106781186547,0.707106781186547,
0.707106781186548,0.707106781186547,0.707106781186548,0.707106781186547,
0.707106781186547,0.707106781186547,0.707106781186548,0.707106781186548,
0.707106781186547,0.707106781186548,0.707106781186548,0.707106781186547,
0.707106781186548,0.707106781186547,0.707106781186548,0.707106781186548,
0.707106781186547,0.707106781186548,0.707106781186548,0.707106781186548,
0.707106781186547,0.707106781186547,0.707106781186548,0.707106781186547,
0.707106781186548,0.707106781186547,0.707106781186547,0.707106781186548,
0.707106781186548,0.707106781186548,0.707106781186547,0.707106781186547,
0.707106781186548,0.707106781186548,0.707106781186547,0.707106781186547,
0.707106781186548,0.707106781186547,0.707106781186547,0.707106781186548,
0.707106781186548,0.707106781186547,0.707106781186547,0.707106781186547,
0.707106781186548,0.707106781186547,0.707106781186547,0.707106781186547,
0.707106781186548,0.707106781186548,0.707106781186547,0.707106781186548,
0.707106781186547,0.707106781186548,0.707106781186547,0.707106781186548,
0.707106781186548,0.707106781186547,0.707106781186547,0.707106781186548,
0.707106781186547,0.707106781186547,0.707106781186548,0.707106781186547,
0.707106781186548,0.707106781186548,0.707106781186547,0.707106781186548,
0.707106781186547,0.707106781186547,0.707106781186547,0.707106781186548,
0.707106781186548,0.707106781186548,0.707106781186547,0.707106781186548,
0.707106781186547,0.707106781186548,0.707106781186547,0.707106781186547,
0.707106781186547,0.707106781186547,0.707106781186548,0.707106781186548,
0.707106781186547,0.707106781186547,0.707106781186548,0.707106781186547,
0.707106781186548,0.707106781186547,0.707106781186548,0.707106781186547,
0.707106781186547,0.707106781186548,0.707106781186547,0.707106781186548,
0.707106781186547,0.707106781186548,0.707106781186548,0.707106781186547,
0.707106781186548,0.707106781186547,0.707106781186548,0.707106781186548,
0.707106781186547,0.707106781186548,0.707106781186547,0.707106781186547,
0.707106781186548,0.707106781186547,0.707106781186548,0.707106781186547,
0.707106781186548,0.707106781186547,0.707106781186547,0.707106781186548,
0.707106781186548,0.707106781186548,0.707106781186548,0.707106781186547,
0.707106781186548,0.707106781186548,0.707106781186548,0.707106781186547,
0.707106781186548,0.707106781186548,0.707106781186548,0.707106781186547,
0.707106781186547,0.707106781186548,0.707106781186547,0.707106781186548,
0.707106781186547,0.707106781186548,0.707106781186548,0.707106781186547,
0.707106781186547,0.707106781186548,0.707106781186547,0.707106781186548,
0.707106781186547,0.707106781186548,0.707106781186548,0.707106781186547,
0.707106781186547,0.707106781186547,0.707106781186548,0.707106781186548,
0.707106781186547,0.707106781186547,0.707106781186548,0.707106781186548,
0.707106781186548,0.707106781186548,0.707106781186547,0.707106781186547,
0.707106781186548,0.707106781186548,0.707106781186547,0.707106781186548,
0.707106781186547,0.707106781186548,0.707106781186547,0.707106781186548,
0.707106781186547,0.707106781186547,0.707106781186548,0.707106781186547,
0.707106781186547,0.707106781186548,0.707106781186547,0.707106781186548,
0.707106781186547,0.707106781186548,0.707106781186547,0.707106781186548,
0.707106781186547,0.707106781186548,0.707106781186547,0.707106781186548,
0.707106781186547,0.707106781186547,0.707106781186548,0.707106781186548,
0.707106781186547,0.707106781186547,0.707106781186547,0.707106781186548,
0.707106781186547,0.707106781186548,0.707106781186547,0.707106781186548,
0.707106781186547,0.707106781186548,0.707106781186547,0.707106781186547,
0.707106781186547,0.707106781186548,0.707106781186547,0.707106781186548,
0.707106781186548,0.707106781186547,0.707106781186548,0.707106781186547,
0.707106781186547,0.707106781186548,0.707106781186547,0.707106781186547,
0.707106781186548,0.707106781186547,0.707106781186547,0.707106781186547,
0.707106781186547,0.707106781186548,0.707106781186547,0.707106781186547,
0.707106781186547,0.707106781186548,0.707106781186547,0.707106781186547,
0.707106781186548,0.707106781186548,0.707106781186547,0.707106781186548,
0.707106781186548,0.707106781186547,0.707106781186547,0.707106781186548,
0.707106781186547,0.707106781186547,0.707106781186548,0.707106781186547,
0.707106781186547,0.707106781186547,0.707106781186548,0.707106781186547,
0.707106781186548,0.707106781186547,0.707106781186548,0.707106781186547,
0.707106781186548,0.707106781186547,0.707106781186548,0.707106781186547,
0.707106781186548,0.707106781186548,0.707106781186547,0.707106781186547,
0.707106781186548,0.707106781186547,0.707106781186548,0.707106781186547,
0.707106781186548,0.707106781186548,0.707106781186547,0.707106781186548,
0.707106781186547,0.707106781186548,0.707106781186548,0.707106781186547,
0.707106781186547,0.707106781186548,0.707106781186547,0.707106781186548,
0.707106781186547,0.707106781186548,0.707106781186547,0.707106781186548,
0.707106781186547,0.707106781186547,0.707106781186547,0.707106781186547,
0.707106781186547,0.707106781186547,0.707106781186547,0.707106781186547,
0.707106781186548,0.707106781186547,0.707106781186548,0.707106781186547,
0.707106781186547,0.707106781186548,0.707106781186547,0.707106781186548,
0.707106781186547,0.707106781186547,0.707106781186548,0.707106781186547,
0.707106781186548,0.707106781186547,0.707106781186548,0.707106781186547,
0.707106781186548,0.707106781186547,0.707106781186548,0.707106781186547,
0.707106781186548,0.707106781186547,0.707106781186548,0.707106781186548,
0.707106781186547,0.707106781186548,0.707106781186547,0.707106781186547,
0.707106781186547,0.707106781186548,0.707106781186547,0.707106781186547,
0.707106781186547,0.707106781186548,0.707106781186547,0.707106781186547,
0.707106781186548,0.707106781186547,0.707106781186547,0.707106781186547,
0.707106781186547,0.707106781186548,0.707106781186547,0.707106781186547,
0.707106781186547,0.707106781186548,0.707106781186548,0.707106781186548,
0.707106781186548,0.707106781186547,0.707106781186548,0.707106781186547,
0.707106781186547,0.707106781186548,0.707106781186547,0.707106781186548,
0.707106781186547,0.707106781186547,0.707106781186548,0.707106781186547,
0.707106781186547,0.707106781186547,0.707106781186547,0.707106781186548,
0.707106781186548,0.707106781186547,0.707106781186547,0.707106781186548,
0.707106781186547,0.707106781186548,0.707106781186547,0.707106781186548,
0.707106781186548,0.707106781186547,0.707106781186547,0.707106781186548,
0.707106781186548,0.707106781186547,0.707106781186548,0.707106781186548,
0.707106781186547,0.707106781186548,0.707106781186548,0.707106781186548,
0.707106781186547,0.707106781186548,0.707106781186547,0.707106781186548,
0.707106781186547,0.707106781186548,0.707106781186547,0.707106781186548,
0.707106781186547,0.707106781186548,0.707106781186548,0.707106781186547,
0.707106781186547,0.707106781186548,0.707106781186547,0.707106781186548,
0.707106781186547,0.707106781186548,0.707106781186548,0.707106781186548,
0.707106781186548,0.707106781186548,0.707106781186547,0.707106781186547,
0.707106781186547,0.707106781186547,0.707106781186548,0.707106781186547,
0.707106781186548,0.707106781186547,0.707106781186547,0.707106781186548,
0.707106781186548,0.707106781186547,0.707106781186548,0.707106781186547,
0.707106781186548,0.707106781186548,0.707106781186547,0.707106781186547,
0.707106781186548,0.707106781186547,0.707106781186548,0.707106781186547,
0.707106781186548,0.707106781186547,0.707106781186548,0.707106781186547,
0.707106781186548,0.707106781186547,0.707106781186548,0.707106781186547,
0.707106781186548,0.707106781186548,0.707106781186547,0.707106781186548,
0.707106781186547,0.707106781186548,0.707106781186547,0.707106781186548,
0.707106781186548,0.707106781186548,0.707106781186547,0.707106781186547,
0.707106781186548,0.707106781186548,0.707106781186547,0.707106781186547,
0.707106781186547,0.707106781186548,0.707106781186547,0.707106781186548,
0.707106781186547,0.707106781186548,0.707106781186547,0.707106781186547,
0.707106781186547,0.707106781186548,0.707106781186547,0.707106781186548,
0.707106781186547,0.707106781186548,0.707106781186547,0.707106781186548,
0.707106781186547,0.707106781186547,0.707106781186548,0.707106781186547,
0.707106781186547,0.707106781186548,0.707106781186547,0.707106781186547,
0.707106781186548,0.707106781186547,0.707106781186547,0.707106781186547,
0.707106781186548,0.707106781186547,0.707106781186548,0.707106781186547,
0.707106781186547,0.707106781186547,0.707106781186548,0.707106781186548,
0.707106781186547,0.707106781186547,0.707106781186548,0.707106781186548,
0.707106781186548,0.707106781186547,0.707106781186548,0.707106781186547,
0.707106781186548,0.707106781186547,0.707106781186548,0.707106781186547,
0.707106781186547,0.707106781186547,0.707106781186547,0.707106781186548,
0.707106781186547,0.707106781186548,0.707106781186548,0.707106781186547,
0.707106781186548,0.707106781186547,0.707106781186547,0.707106781186547,
0.707106781186547,0.707106781186548,0.707106781186547,0.707106781186548,
0.707106781186547,0.707106781186548,0.707106781186548,0.707106781186547,
0.707106781186548,0.707106781186547,0.707106781186547,0.707106781186547,
0.707106781186547,0.707106781186548,0.707106781186547,0.707106781186548,
0.707106781186548,0.707106781186547,0.707106781186548,0.707106781186547,
0.707106781186548,0.707106781186547,0.707106781186547,0.707106781186548,
0.707106781186547,0.707106781186548,0.707106781186548,0.707106781186547,
0.707106781186547,0.707106781186548,0.707106781186548,0.707106781186547,
0.707106781186547,0.707106781186548,0.707106781186547,0.707106781186547,
0.707106781186548,0.707106781186547,0.707106781186547,0.707106781186548,
0.707106781186547,0.707106781186548,0.707106781186547,0.707106781186547,
0.707106781186548,0.707106781186547,0.707106781186548,0.707106781186547,
0.707106781186548,0.707106781186547,0.707106781186547,0.707106781186547,
0.707106781186548,0.707106781186547,0.707106781186548,0.707106781186547,
0.707106781186548,0.707106781186548,0.707106781186548,0.707106781186548,
0.707106781186547,0.707106781186547,0.707106781186547,0.707106781186548,
0.707106781186547,0.707106781186548,0.707106781186547,0.707106781186547,
0.707106781186548,0.707106781186547,0.707106781186547,0.707106781186548,
0.707106781186547,0.707106781186547,0.707106781186548,0.707106781186548,
0.707106781186547,0.707106781186548,0.707106781186547,0.707106781186547,
0.707106781186548,0.707106781186547,0.707106781186548,0.707106781186547,
0.707106781186548,0.707106781186547,0.707106781186547,0.707106781186547,
0.707106781186548,0.707106781186547,0.707106781186548,0.707106781186547,
0.707106781186548,0.707106781186547,0.707106781186547,0.707106781186548,
0.707106781186548,0.707106781186548,0.707106781186547,0.707106781186548,
0.707106781186547,0.707106781186548,0.707106781186547,0.707106781186548,
0.707106781186547,0.707106781186548,0.707106781186548,0.707106781186547,
0.707106781186547,0.707106781186547,0.707106781186548,0.707106781186547,
0.707106781186547,0.707106781186548,0.707106781186547,0.707106781186547,
0.707106781186548,0.707106781186547,0.707106781186548,0.707106781186548,
0.707106781186548,0.707106781186547,0.707106781186548,0.707106781186547,
0.707106781186548,0.707106781186547,0.707106781186548,0.707106781186547,
0.707106781186548,0.707106781186547,0.707106781186548,0.707106781186547,
0.707106781186548,0.707106781186548,0.707106781186547,0.707106781186548,
0.707106781186547,0.707106781186548,0.707106781186548,0.707106781186547,
0.707106781186547,0.707106781186548,0.707106781186547,0.707106781186547,
0.707106781186548,0.707106781186547,0.707106781186548,0.707106781186548,
0.707106781186547,0.707106781186548,0.707106781186548,0.707106781186548,
0.707106781186548,0.707106781186548,0.707106781186547,0.707106781186548,
0.707106781186548,0.707106781186548,0.707106781186547,0.707106781186548,
0.707106781186547,0.707106781186548,0.707106781186547,0.707106781186548,
0.707106781186547,0.707106781186548,0.707106781186547,0.707106781186548,
0.707106781186547,0.707106781186547,0.707106781186548,0.707106781186547,
0.707106781186547,0.707106781186548,0.707106781186547,0.707106781186548,
0.707106781186547,0.707106781186548,0.707106781186547,0.707106781186548,
0.707106781186547,0.707106781186547,0.707106781186548,0.707106781186547,
0.707106781186547,0.707106781186548,0.707106781186547,0.707106781186548,
0.707106781186547,0.707106781186547,0.707106781186548,0.707106781186548,
0.707106781186547,0.707106781186548,0.707106781186547,0.707106781186547,
0.707106781186547,0.707106781186548,0.707106781186547,0.707106781186547,
0.707106781186548,0.707106781186547,0.707106781186547,0.707106781186547,
0.707106781186548,0.707106781186548,0.707106781186547,0.707106781186548,
0.707106781186547,0.707106781186548,0.707106781186547,0.707106781186547,
0.707106781186548,0.707106781186547,0.707106781186548,0.707106781186547,
0.707106781186547,0.707106781186547,0.707106781186547,0.707106781186548,
0.707106781186547,0.707106781186547,0.707106781186547,0.707106781186547,
0.707106781186547,0.707106781186548,0.707106781186547,0.707106781186547,
0.707106781186547,0.707106781186547,0.707106781186548,0.707106781186547,
0.707106781186548,0.707106781186547,0.707106781186547,0.707106781186548,
0.707106781186547,0.707106781186548,0.707106781186547,0.707106781186547,
0.707106781186548,0.707106781186547,0.707106781186547,0.707106781186548,
0.707106781186547,0.707106781186547,0.707106781186547,0.707106781186547,
0.707106781186548,0.707106781186547,0.707106781186548,0.707106781186548,
0.707106781186547,0.707106781186548,0.707106781186548,0.707106781186547,
0.707106781186547,0.707106781186548,0.707106781186547,0.707106781186547,
0.707106781186547,0.707106781186548,0.707106781186547,0.707106781186547,
0.707106781186548,0.707106781186547,0.707106781186548,0.707106781186547,
0.707106781186548,0.707106781186547,0.707106781186547,0.707106781186548,
0.707106781186547,0.707106781186548,0.707106781186547,0.707106781186548,
0.707106781186547,0.707106781186548,0.707106781186547,0.707106781186548,
0.707106781186547,0.707106781186547,0.707106781186547,0.707106781186547,
0.707106781186548,0.707106781186548,0.707106781186547,0.707106781186548,
0.707106781186548,0.707106781186547,0.707106781186548,0.707106781186547,
0.707106781186547,0.707106781186548,0.707106781186547,0.707106781186547,
0.707106781186547,0.707106781186547,0.707106781186548,0.707106781186547,
0.707106781186547,0.707106781186547,0.707106781186548,0.707106781186547,
0.707106781186547,0.707106781186548,0.707106781186547,0.707106781186548,
0.707106781186548,0.707106781186547,0.707106781186548,0.707106781186547,
0.707106781186548,0.707106781186547,0.707106781186548,0.707106781186547,
0.707106781186547,0.707106781186548,0.707106781186547,0.707106781186548,
0.707106781186548,0.707106781186547,0.707106781186547,0.707106781186548,
0.707106781186547,0.707106781186548,0.707106781186547,0.707106781186548,
0.707106781186547,0.707106781186547,0.707106781186548,0.707106781186548,
0.707106781186547,0.707106781186548,0.707106781186548,0.707106781186547,
0.707106781186548,0.707106781186548,0.707106781186547,0.707106781186548,
0.707106781186547,0.707106781186548,0.707106781186547,0.707106781186548,
0.707106781186547,0.707106781186548,0.707106781186547,0.707106781186547,
0.707106781186548,0.707106781186547,0.707106781186547,0.707106781186548,
0.707106781186547,0.707106781186548,0.707106781186548,0.707106781186547,
0.707106781186547,0.707106781186547,0.707106781186548,0.707106781186547,
0.707106781186548,0.707106781186548,0.707106781186547,0.707106781186548,
0.707106781186547,0.707106781186548,0.707106781186547,0.707106781186548,
0.707106781186547,0.707106781186547,0.707106781186548,0.707106781186548,
0.707106781186548,0.707106781186547,0.707106781186548,0.707106781186548,
0.707106781186547,0.707106781186548,0.707106781186547,0.707106781186548,
0.707106781186548,0.707106781186548,0.707106781186548,0.707106781186548,
0.707106781186548,0.707106781186547,0.707106781186547,0.707106781186548,
0.707106781186547,0.707106781186547,0.707106781186548,0.707106781186547,
0.707106781186547,0.707106781186548,0.707106781186547,0.707106781186548,
0.707106781186547,0.707106781186548,0.707106781186547,0.707106781186547,
0.707106781186547,0.707106781186548,0.707106781186547,0.707106781186547,
0.707106781186548,0.707106781186547,0.707106781186548,0.707106781186547,
0.707106781186548,0.707106781186547,0.707106781186547,0.707106781186547,
0.707106781186547,0.707106781186548,0.707106781186547,0.707106781186547,
0.707106781186548,0.707106781186548,0.707106781186547,0.707106781186548,
0.707106781186547,0.707106781186548,0.707106781186547,0.707106781186547,
0.707106781186548,0.707106781186547,0.707106781186548,0.707106781186547,
0.707106781186548,0.707106781186547,0.707106781186548,0.707106781186548,
0.707106781186547,0.707106781186548,0.707106781186547,0.707106781186547,
0.707106781186548,0.707106781186547,0.707106781186547,0.707106781186548,
0.707106781186548,0.707106781186548,0.707106781186547,0.707106781186548,
0.707106781186547,0.707106781186547,0.707106781186547,0.707106781186548,
0.707106781186547,0.707106781186548,0.707106781186548,0.707106781186548,
0.707106781186547,0.707106781186547,0.707106781186547,0.707106781186547,
0.707106781186548,0.707106781186547,0.707106781186547,0.707106781186548,
0.707106781186547,0.707106781186548,0.707106781186547,0.707106781186547,
0.707106781186548,0.707106781186547,0.707106781186548,0.707106781186547,
0.707106781186548,0.707106781186547,0.707106781186547,0.707106781186547,
0.707106781186547,0.707106781186547,0.707106781186547,0.707106781186548,
0.707106781186547,0.707106781186547,0.707106781186548,0.707106781186548,
0.707106781186547,0.707106781186548,0.707106781186548,0.707106781186547,
0.707106781186547,0.707106781186548,0.707106781186547,0.707106781186547,
0.707106781186548,0.707106781186547,0.707106781186548,0.707106781186548,
0.707106781186548,0.707106781186547,0.707106781186547,0.707106781186547,
0.707106781186547,0.707106781186548,0.707106781186548,0.707106781186548,
0.707106781186547,0.707106781186548,0.707106781186547,0.707106781186548,
0.707106781186548,0.707106781186547,0.707106781186548,0.707106781186547,
0.707106781186548,0.707106781186548,0.707106781186547,0.707106781186547,
0.707106781186548,0.707106781186547,0.707106781186548,0.707106781186547,
0.707106781186548,0.707106781186548,0.707106781186548,0.707106781186547,
0.707106781186548,0.707106781186547,0.707106781186547,0.707106781186547,
0.707106781186547,0.707106781186548,0.707106781186548,0.707106781186547,
0.707106781186547,0.707106781186547,0.707106781186548,0.707106781186547,
0.707106781186547,0.707106781186548,0.707106781186547,0.707106781186548,
0.707106781186548,0.707106781186548,0.707106781186547,0.707106781186547,
0.707106781186547,0.707106781186547,0.707106781186548,0.707106781186548,
0.707106781186547,0.707106781186548,0.707106781186547,0.707106781186548,
0.707106781186548,0.707106781186547,0.707106781186548,0.707106781186547,
0.707106781186548,0.707106781186547,0.707106781186547,0.707106781186547,
0.707106781186548,0.707106781186547,0.707106781186548,0.707106781186547,
0.707106781186548,0.707106781186547,0.707106781186548,0.707106781186547,
0.707106781186548,0.707106781186547,0.707106781186547,0.707106781186548,
0.707106781186547,0.707106781186548,0.707106781186547,0.707106781186547,
0.707106781186548,0.707106781186548,0.707106781186547,0.707106781186548,
0.707106781186548,0.707106781186547,0.707106781186548,0.707106781186547,
0.707106781186548,0.707106781186547,0.707106781186547,0.707106781186547,
0.707106781186548,0.707106781186547,0.707106781186547,0.707106781186548,
0.707106781186547,0.707106781186548,0.707106781186547,0.707106781186548,
0.707106781186548,0.707106781186547,0.707106781186548,0.707106781186547,
0.707106781186548,0.707106781186548,0.707106781186548,0.707106781186548,
0.707106781186547,0.707106781186547,0.707106781186548,0.707106781186547,
0.707106781186547,0.707106781186548,0.707106781186548,0.707106781186547,
0.707106781186547,0.707106781186548,0.707106781186547,0.707106781186547,
0.707106781186548,0.707106781186547,0.707106781186548,0.707106781186547,
0.707106781186548,0.707106781186547,0.707106781186547,0.707106781186547,
0.707106781186548,0.707106781186547,0.707106781186547,0.707106781186548,
0.707106781186547,0.707106781186548,0.707106781186548,0.707106781186548,
0.707106781186547,0.707106781186547,0.707106781186547,0.707106781186548,
0.707106781186548,0.707106781186547,0.707106781186547,0.707106781186547,
0.707106781186547,0.707106781186548,0.707106781186548,0.707106781186547,
0.707106781186547,0.707106781186547,0.707106781186548,0.707106781186548,
0.707106781186547,0.707106781186548,0.707106781186547,0.707106781186548,
0.707106781186547,0.707106781186548,0.707106781186548,0.707106781186547,
0.707106781186548,0.707106781186548,0.707106781186548,0.707106781186547,
0.707106781186547,0.707106781186547,0.707106781186548,0.707106781186548,
0.707106781186548,0.707106781186547,0.707106781186547,0.707106781186548,
0.707106781186548,0.707106781186547,0.707106781186548,0.707106781186547,
0.707106781186547,0.707106781186548,0.707106781186547,0.707106781186548,
0.707106781186547,0.707106781186547,0.707106781186548,0.707106781186547,
0.707106781186548,0.707106781186548,0.707106781186547,0.707106781186547,
0.707106781186548,0.707106781186547,0.707106781186548,0.707106781186547,
0.707106781186547,0.707106781186548,0.707106781186547,0.707106781186548,
0.707106781186547,0.707106781186548,0.707106781186547,0.707106781186547,
0.707106781186548,0.707106781186547,0.707106781186547,0.707106781186547,
0.707106781186547,0.707106781186547,0.707106781186547,0.707106781186548,
0.707106781186547,0.707106781186548,0.707106781186548,0.707106781186548,
0.707106781186547,0.707106781186547,0.707106781186547,0.707106781186548,
0.707106781186547,0.707106781186548,0.707106781186547,0.707106781186547,
0.707106781186548,0.707106781186547,0.707106781186547,0.707106781186547,
0.707106781186547,0.707106781186547,0.707106781186548,0.707106781186547,
0.707106781186548,0.707106781186547,0.707106781186547,0.707106781186548,
0.707106781186548,0.707106781186547,0.707106781186547,0.707106781186547,
0.707106781186548,0.707106781186547,0.707106781186547,0.707106781186548,
0.707106781186548,0.707106781186547,0.707106781186548,0.707106781186547,
0.707106781186548,0.707106781186548,0.707106781186547,0.707106781186547,
0.707106781186547,0.707106781186548,0.707106781186548,0.707106781186547,
0.707106781186548,0.707106781186547,0.707106781186548,0.707106781186548,
0.707106781186547,0.707106781186548,0.707106781186547,0.707106781186547,
0.707106781186547,0.707106781186548,0.707106781186547,0.707106781186548,
0.707106781186547,0.707106781186548,0.707106781186547,0.707106781186547,
0.707106781186547,0.707106781186547,0.707106781186547,0.707106781186548,
0.707106781186547,0.707106781186548,0.707106781186547,0.707106781186548,
0.707106781186547,0.707106781186548,0.707106781186547,0.707106781186547,
0.707106781186547,0.707106781186547,0.707106781186547,0.707106781186548,
0.707106781186548,0.707106781186548,0.707106781186547,0.707106781186548,
0.707106781186547,0.707106781186548,0.707106781186547,0.707106781186547,
0.707106781186548,0.707106781186547,0.707106781186548,0.707106781186547,
0.707106781186547,0.707106781186547,0.707106781186548,0.707106781186548,
0.707106781186547,0.707106781186548,0.707106781186547,0.707106781186548,
0.707106781186548,0.707106781186547,0.707106781186548,0.707106781186547,
0.707106781186548,0.707106781186548,0.707106781186547,0.707106781186547,
0.707106781186547,0.707106781186547,0.707106781186547,0.707106781186547,
0.707106781186548,0.707106781186548,0.707106781186547,0.707106781186548,
0.707106781186547,0.707106781186547,0.707106781186548,0.707106781186547,
0.707106781186547,0.707106781186548,0.707106781186547,0.707106781186547,
0.707106781186547,0.707106781186548,0.707106781186547,0.707106781186547,
0.707106781186548,0.707106781186547,0.707106781186548,0.707106781186548,
0.707106781186547,0.707106781186547,0.707106781186547,0.707106781186548,
0.707106781186547,0.707106781186547,0.707106781186548,0.707106781186548,
0.707106781186548,0.707106781186548,0.707106781186547,0.707106781186548,
0.707106781186548,0.707106781186547,0.707106781186547,0.707106781186548,
0.707106781186547,0.707106781186548,0.707106781186547,0.707106781186547,
0.707106781186548,0.707106781186547,0.707106781186547,0.707106781186548,
0.707106781186547,0.707106781186548,0.707106781186547,0.707106781186548,
0.707106781186547,0.707106781186548,0.707106781186547,0.707106781186548,
0.707106781186547,0.707106781186548,0.707106781186548,0.707106781186547,
0.707106781186547,0.707106781186548,0.707106781186548,0.707106781186547,
0.707106781186547,0.707106781186547,0.707106781186547,0.707106781186547,
0.707106781186548,0.707106781186547,0.707106781186547,0.707106781186548,
0.707106781186547,0.707106781186548,0.707106781186548,0.707106781186547,
0.707106781186548,0.707106781186547,0.707106781186548,0.707106781186547,
0.707106781186548,0.707106781186547,0.707106781186547,0.707106781186547,
0.707106781186547,0.707106781186547,0.707106781186547,0.707106781186548,
0.707106781186547,0.707106781186548,0.707106781186547,0.707106781186547,
0.707106781186547,0.707106781186548,0.707106781186547,0.707106781186548,
0.707106781186548,0.707106781186547,0.707106781186547,0.707106781186548,
0.707106781186547,0.707106781186548,0.707106781186547,0.707106781186548,
0.707106781186547,0.707106781186548,0.707106781186547,0.707106781186547,
0.707106781186548,0.707106781186547,0.707106781186548,0.707106781186547,
0.707106781186548,0.707106781186548,0.707106781186548,0.707106781186548,
0.707106781186547,0.707106781186548,0.707106781186548,0.707106781186548,
0.707106781186547,0.707106781186548,0.707106781186548,0.707106781186547,
0.707106781186548,0.707106781186547,0.707106781186548,0.707106781186547,
0.707106781186547,0.707106781186547,0.707106781186548,0.707106781186548,
0.707106781186547,0.707106781186548,0.707106781186547,0.707106781186548,
0.707106781186547,0.707106781186548,0.707106781186548,0.707106781186547,
0.707106781186548,0.707106781186547,0.707106781186547,0.707106781186548,
0.707106781186547,0.707106781186547,0.707106781186547,0.707106781186548,
0.707106781186547,0.707106781186548,0.707106781186548,0.707106781186547,
0.707106781186548,0.707106781186547,0.707106781186548,0.707106781186548,
0.707106781186548,0.707106781186548,0.707106781186547,0.707106781186548,
0.707106781186547,0.707106781186548,0.707106781186547,0.707106781186548,
0.707106781186547,0.707106781186547,0.707106781186547,0.707106781186547,
0.707106781186548,0.707106781186547,0.707106781186548,0.707106781186547,
0.707106781186547,0.707106781186548,0.707106781186547,0.707106781186548,
0.707106781186547,0.707106781186548,0.707106781186547,0.707106781186548,
0.707106781186548,0.707106781186548,0.707106781186548,0.707106781186547,
0.707106781186548,0.707106781186548,0.707106781186547,0.707106781186548,
0.707106781186547,0.707106781186548,0.707106781186547,0.707106781186548,
0.707106781186547,0.707106781186547,0.707106781186548,0.707106781186547,
0.707106781186548,0.707106781186547,0.707106781186547,0.707106781186548,
0.707106781186547,0.707106781186548,0.707106781186547,0.707106781186547,
0.707106781186548,0.707106781186548,0.707106781186548,0.707106781186548,
0.707106781186548,0.707106781186548,0.707106781186548,0.707106781186548,
0.707106781186548,0.707106781186547,0.707106781186548,0.707106781186547,
0.707106781186547,0.707106781186548,0.707106781186547,0.707106781186548,
0.707106781186548,0.707106781186547,0.707106781186547,0.707106781186548,
0.707106781186548,0.707106781186547,0.707106781186547,0.707106781186547,
0.707106781186547,0.707106781186547,0.707106781186548,0.707106781186547,
0.707106781186548,0.707106781186548,0.707106781186548,0.707106781186547,
0.707106781186548,0.707106781186547,0.707106781186548,0.707106781186547,
0.707106781186548,0.707106781186547,0.707106781186548,0.707106781186548,
0.707106781186547,0.707106781186547,0.707106781186548,0.707106781186548,
0.707106781186548,0.707106781186547,0.707106781186547,0.707106781186548,
0.707106781186547,0.707106781186547,0.707106781186548,0.707106781186547,
0.707106781186548,0.707106781186547,0.707106781186547,0.707106781186548,
0.707106781186548,0.707106781186548,0.707106781186547,0.707106781186547,
0.707106781186548,0.707106781186547,0.707106781186548,0.707106781186547,
0.707106781186548,0.707106781186547,0.707106781186548,0.707106781186548,
0.707106781186547,0.707106781186548,0.707106781186547,0.707106781186548,
0.707106781186547,0.707106781186547,0.707106781186547,0.707106781186548,
0.707106781186547,0.707106781186548,0.707106781186547,0.707106781186547,
0.707106781186547,0.707106781186548,0.707106781186547,0.707106781186547,
0.707106781186548,0.707106781186548,0.707106781186547,0.707106781186548,
0.707106781186547,0.707106781186548,0.707106781186548,0.707106781186547,
0.707106781186548,0.707106781186547,0.707106781186547,0.707106781186548,
0.707106781186547,0.707106781186547,0.707106781186547,0.707106781186548,
0.707106781186547,0.707106781186548,0.707106781186547,0.707106781186548,
0.707106781186548,0.707106781186548,0.707106781186547,0.707106781186548,
0.707106781186548,0.707106781186548,0.707106781186547,0.707106781186548,
0.707106781186547,0.707106781186547,0.707106781186548,0.707106781186547,
0.707106781186547,0.707106781186548,0.707106781186548,0.707106781186547,
0.707106781186548,0.707106781186547,0.707106781186548,0.707106781186548,
0.707106781186547,0.707106781186548,0.707106781186547,0.707106781186548,
0.707106781186547,0.707106781186548,0.707106781186547,0.707106781186548,
0.707106781186548,0.707106781186548,0.707106781186547,0.707106781186548,
0.707106781186548,0.707106781186547,0.707106781186547,0.707106781186548,
0.707106781186547,0.707106781186548,0.707106781186548,0.707106781186547,
0.707106781186548,0.707106781186548,0.707106781186547,0.707106781186548,
0.707106781186548,0.707106781186547,0.707106781186547,0.707106781186548,
0.707106781186547,0.707106781186548,0.707106781186547,0.707106781186548,
0.707106781186547,0.707106781186548,0.707106781186548,0.707106781186548,
0.707106781186547,0.707106781186548,0.707106781186547,0.707106781186548,
0.707106781186547,0.707106781186548,0.707106781186547,0.707106781186548,
0.707106781186547,0.707106781186548,0.707106781186547,0.707106781186548,
0.707106781186547,0.707106781186547,0.707106781186547,0.707106781186548,
0.707106781186547,0.707106781186548,0.707106781186547,0.707106781186548,
0.707106781186547,0.707106781186548,0.707106781186547,0.707106781186548,
0.707106781186548,0.707106781186548,0.707106781186547,0.707106781186548,
0.707106781186547,0.707106781186548,0.707106781186548,0.707106781186547,
0.707106781186548,0.707106781186547,0.707106781186548,0.707106781186547,
0.707106781186548,0.707106781186547,0.707106781186548,0.707106781186547,
0.707106781186547,0.707106781186547,0.707106781186548,0.707106781186547,
0.707106781186547,0.707106781186548,0.707106781186547,0.707106781186548,
0.707106781186547,0.707106781186547,0.707106781186548,0.707106781186547,
0.707106781186548,0.707106781186547,0.707106781186548,0.707106781186548,
0.707106781186548,0.707106781186547,0.707106781186547,0.707106781186548,
0.707106781186548,0.707106781186547,0.707106781186548,0.707106781186547,
0.707106781186547,0.707106781186547,0.707106781186548,0.707106781186547,
0.707106781186548,0.707106781186547,0.707106781186548,0.707106781186548,
0.707106781186548,0.707106781186547,0.707106781186547,0.707106781186547,
0.707106781186547,0.707106781186547,0.707106781186547,0.707106781186548,
0.707106781186547,0.707106781186548,0.707106781186547,0.707106781186548,
0.707106781186547,0.707106781186547,0.707106781186548,0.707106781186547,
0.707106781186547,0.707106781186548,0.707106781186548,0.707106781186547,
0.707106781186547,0.707106781186547,0.707106781186548,0.707106781186547,
0.707106781186547,0.707106781186548,0.707106781186548),(1.,1.,1.,1.,1.,
1.,1.,1.,1.,1.,1.,1.,1.,1.,1.,1.,1.,1.,1.,1.,1.,1.,1.,1.,1.,1.,1.,1.,1.,
1.,1.,1.,1.,1.,1.,1.,1.,1.,1.,1.,1.,1.,1.,1.,1.,1.,1.,1.,1.,1.,1.,1.,1.,
1.,1.,1.,1.,1.,1.,1.,1.,1.,1.,1.,1.,1.,1.,1.,1.,1.,1.,1.,1.,1.,1.,1.,1.,
1.,1.,1.,1.,1.,1.,1.,1.,1.,1.,1.,1.,1.,1.,1.,1.,1.,1.,1.,1.,1.,1.,1.,1.,
1.,1.,1.,1.,1.,1.,1.,1.,1.,1.,1.,1.,1.,1.,1.,1.,1.,1.,1.,1.,1.,1.,1.,1.,
1.,1.,1.,1.,1.,1.,1.,1.,1.,1.,1.,1.,1.,1.,1.,1.,1.,1.,1.,1.,1.,1.,1.,1.,
1.,1.,1.,1.,1.,1.,1.,1.,1.,1.,1.,1.,1.,1.,1.,1.,1.,1.,1.,1.,1.,1.,1.,1.,
1.,1.,1.,1.,1.,1.,1.,1.,1.,1.,1.,1.,1.,1.,1.,1.,1.,1.,1.,1.,1.,1.,1.,1.,
1.,1.,1.,1.,1.,1.,1.,1.,1.,1.,1.,1.,1.,1.,1.,1.,1.,1.,1.,1.,1.,1.,1.,1.,
1.,1.,1.,1.,1.,1.,1.,1.,1.,1.,1.,1.,1.,1.,1.,1.,1.,1.,1.,1.,1.,1.,1.,1.,
1.,1.,1.,1.,1.,1.,1.,1.,1.,1.,1.,1.,1.,1.,1.,1.,1.,1.,1.,1.,1.,1.,1.,1.,
1.,1.,1.,1.,1.,1.,1.,1.,1.,1.,1.,1.,1.,1.,1.,1.,1.,1.,1.,1.,1.,1.,1.,1.,
1.,1.,1.,1.,1.,1.,1.,1.,1.,1.,1.,1.,1.,1.,1.,1.,1.,1.,1.,1.,1.,1.,1.,1.,
1.,1.,1.,1.,1.,1.,1.,1.,1.,1.,1.,1.,1.,1.,1.,1.,1.,1.,1.,1.,1.,1.,1.,1.,
1.,1.,1.,1.,1.,1.,1.,1.,1.,1.,1.,1.,1.,1.,1.,1.,1.,1.,1.,1.,1.,1.,1.,1.,
1.,1.,1.,1.,1.,1.,1.,1.,1.,1.,1.,1.,1.,1.,1.,1.,1.,1.,1.,1.,1.,1.,1.,1.,
1.,1.,1.,1.,1.,1.,1.,1.,1.,1.,1.,1.,1.,1.,1.,1.,1.,1.,1.,1.,1.,1.,1.,1.,
1.,1.,1.,1.,1.,1.,1.,1.,1.,1.,1.,1.,1.,1.,1.,1.,1.,1.,1.,1.,1.,1.,1.,1.,
1.,1.,1.,1.,1.,1.,1.,1.,1.,1.,1.,1.,1.,1.,1.,1.,1.,1.,1.,1.,1.,1.,1.,1.,
1.,1.,1.,1.,1.,1.,1.,1.,1.,1.,1.,1.,1.,1.,1.,1.,1.,1.,1.,1.,1.,1.,1.,1.,
1.,1.,1.,1.,1.,1.,1.,1.,1.,1.,1.,1.,1.,1.,1.,1.,1.,1.,1.,1.,1.,1.,1.,1.,
1.,1.,1.,1.,1.,1.,1.,1.,1.,1.,1.,1.,1.,1.,1.,1.,1.,1.,1.,1.,1.,1.,1.,1.,
1.,1.,1.,1.,1.,1.,1.,1.,1.,1.,1.,1.,1.,1.,1.,1.,1.,1.,1.,1.,1.,1.,1.,1.,
1.,1.,1.,1.,1.,1.,1.,1.,1.,1.,1.,1.,1.,1.,1.,1.,1.,1.,1.,1.,1.,1.,1.,1.,
1.,1.,1.,1.,1.,1.,1.,1.,1.,1.,1.,1.,1.,1.,1.,1.,1.,1.,1.,1.,1.,1.,1.,1.,
1.,1.,1.,1.,1.,1.,1.,1.,1.,1.,1.,1.,1.,1.,1.,1.,1.,1.,1.,1.,1.,1.,1.,1.,
1.,1.,1.,1.,1.,1.,1.,1.,1.,1.,1.,1.,1.,1.,1.,1.,1.,1.,1.,1.,1.,1.,1.,1.,
1.,1.,1.,1.,1.,1.,1.,1.,1.,1.,1.,1.,1.,1.,1.,1.,1.,1.,1.,1.,1.,1.,1.,1.,
1.,1.,1.,1.,1.,1.,1.,1.,1.,1.,1.,1.,1.,1.,1.,1.,1.,1.,1.,1.,1.,1.,1.,1.,
1.,1.,1.,1.,1.,1.,1.,1.,1.,1.,1.,1.,1.,1.,1.,1.,1.,1.,1.,1.,1.,1.,1.,1.,
1.,1.,1.,1.,1.,1.,1.,1.,1.,1.,1.,1.,1.,1.,1.,1.,1.,1.,1.,1.,1.,1.,1.,1.,
1.,1.,1.,1.,1.,1.,1.,1.,1.,1.,1.,1.,1.,1.,1.,1.,1.,1.,1.,1.,1.,1.,1.,1.,
1.,1.,1.,1.,1.,1.,1.,1.,1.,1.,1.,1.,1.,1.,1.,1.,1.,1.,1.,1.,1.,1.,1.,1.,
1.,1.,1.,1.,1.,1.,1.,1.,1.,1.,1.,1.,1.,1.,1.,1.,1.,1.,1.,1.,1.,1.,1.,1.,
1.,1.,1.,1.,1.,1.,1.,1.,1.,1.,1.,1.,1.,1.,1.,1.,1.,1.,1.,1.,1.,1.,1.,1.,
1.,1.,1.,1.,1.,1.,1.,1.,1.,1.,1.,1.,1.,1.,1.,1.,1.,1.,1.,1.,1.,1.,1.,1.,
1.,1.,1.,1.,1.,1.,1.,1.,1.,1.,1.,1.,1.,1.,1.,1.,1.,1.,1.,1.,1.,1.,1.,1.,
1.,1.,1.,1.,1.,1.,1.,1.,1.,1.,1.,1.,1.,1.,1.,1.,1.,1.,1.,1.,1.,1.,1.,1.,
1.,1.,1.,1.,1.,1.,1.,1.,1.,1.,1.,1.,1.,1.,1.,1.,1.,1.,1.,1.,1.,1.,1.,1.,
1.,1.,1.,1.,1.,1.,1.,1.,1.,1.,1.,1.,1.,1.,1.,1.,1.,1.,1.,1.,1.,1.,1.,1.,
1.,1.,1.,1.,1.,1.,1.,1.,1.,1.,1.,1.,1.,1.,1.,1.,1.,1.,1.,1.,1.,1.,1.,1.,
1.,1.,1.,1.,1.,1.,1.,1.,1.,1.,1.,1.,1.,1.,1.,1.,1.,1.,1.,1.,1.,1.,1.,1.,
1.,1.,1.,1.,1.,1.,1.,1.,1.,1.,1.,1.,1.,1.,1.,1.,1.,1.,1.,1.,1.,1.,1.,1.,
1.,1.,1.,1.,1.,1.,1.,1.,1.,1.,1.,1.,1.,1.,1.,1.,1.,1.,1.,1.,1.,1.,1.,1.,
1.,1.,1.,1.,1.,1.,1.,1.,1.,1.,1.,1.,1.,1.,1.,1.,1.,1.,1.,1.,1.,1.,1.,1.,
1.,1.,1.,1.,1.,1.,1.,1.,1.,1.,1.,1.,1.,1.,1.,1.,1.,1.,1.,1.,1.,1.,1.,1.,
1.,1.,1.,1.,1.,1.,1.,1.,1.,1.,1.,1.,1.,1.,1.,1.,1.,1.,1.,1.,1.,1.,1.,1.,
1.,1.,1.,1.,1.,1.,1.,1.,1.,1.,1.,1.,1.,1.,1.,1.,1.,1.,1.,1.,1.,1.,1.,1.,
1.,1.,1.,1.,1.,1.,1.,1.,1.,1.,1.,1.,1.,1.,1.,1.,1.,1.,1.,1.,1.,1.,1.,1.,
1.,1.,1.,1.,1.,1.,1.,1.,1.,1.,1.,1.,1.,1.,1.,1.,1.,1.,1.,1.,1.,1.,1.,1.,
1.,1.,1.,1.,1.,1.,1.,1.,1.,1.,1.,1.,1.,1.,1.,1.,1.,1.,1.,1.,1.,1.,1.,1.,
1.,1.,1.,1.,1.,1.,1.,1.,1.,1.,1.,1.,1.,1.,1.,1.,1.,1.,1.,1.,1.,1.,1.,1.,
1.,1.,1.,1.,1.,1.,1.,1.,1.,1.,1.,1.,1.,1.,1.,1.,1.,1.,1.,1.,1.,1.,1.,1.,
1.,1.,1.,1.,1.,1.,1.,1.,1.,1.,1.,1.,1.,1.,1.,1.,1.,1.,1.,1.,1.,1.,1.,1.,
1.,1.,1.,1.,1.,1.,1.,1.,1.,1.,1.,1.,1.,1.,1.,1.,1.,1.,1.,1.,1.,1.,1.,1.,
1.,1.,1.,1.,1.,1.,1.,1.,1.,1.,1.,1.,1.,1.,1.,1.,1.,1.,1.,1.,1.,1.,1.,1.,
1.,1.,1.,1.,1.,1.,1.,1.,1.,1.,1.,1.,1.,1.,1.,1.,1.,1.,1.,1.,1.,1.,1.,1.,
1.,1.,1.,1.,1.,1.,1.,1.,1.,1.,1.,1.,1.,1.,1.,1.,1.,1.,1.,1.,1.,1.,1.,1.,
1.,1.,1.,1.,1.,1.,1.,1.,1.,1.,1.,1.,1.,1.,1.,1.,1.,1.,1.,1.,1.,1.,1.,1.,
1.,1.,1.,1.,1.,1.,1.,1.,1.,1.,1.,1.,1.,1.,1.,1.,1.,1.,1.,1.,1.,1.,1.,1.,
1.,1.,1.,1.,1.,1.,1.,1.,1.,1.,1.,1.,1.,1.,1.,1.,1.,1.,1.,1.,1.,1.,1.,1.,
1.,1.,1.,1.,1.,1.,1.,1.,1.,1.,1.,1.,1.,1.,1.,1.,1.,1.,1.,1.,1.,1.,1.,1.,
1.,1.,1.,1.,1.,1.,1.,1.,1.,1.,1.,1.,1.,1.,1.,1.,1.,1.,1.,1.,1.,1.,1.,1.,
1.,1.,1.,1.,1.,1.,1.,1.,1.,1.,1.,1.,1.,1.,1.,1.,1.,1.,1.,1.,1.,1.,1.,1.,
1.,1.,1.,1.,1.,1.,1.,1.,1.,1.,1.,1.,1.,1.,1.,1.,1.,1.,1.,1.,1.,1.,1.,1.,
1.,1.,1.,1.,1.,1.,1.,1.,1.,1.,1.,1.,1.,1.,1.,1.,1.,1.,1.,1.,1.,1.,1.,1.,
1.,1.,1.,1.,1.,1.,1.,1.,1.,1.,1.,1.,1.,1.,1.,1.,1.,1.,1.,1.,1.,1.,1.,1.,
1.,1.,1.,1.,1.,1.,1.,1.,1.,1.,1.,1.,1.,1.,1.,1.,1.,1.,1.,1.,1.,1.,1.,1.,
1.,1.,1.,1.,1.,1.,1.,1.,1.,1.,1.,1.,1.,1.,1.,1.,1.,1.,1.,1.,1.,1.,1.,1.,
1.,1.,1.,1.,1.,1.,1.,1.,1.,1.,1.,1.,1.,1.,1.,1.,1.,1.,1.,1.,1.,1.,1.,1.,
1.,1.,1.,1.,1.,1.,1.,1.,1.,1.,1.,1.,1.,1.,1.,1.,1.,1.,1.,1.,1.,1.,1.,1.,
1.,1.,1.,1.,1.,1.,1.,1.,1.,1.,1.,1.,1.,1.,1.,1.,1.,1.,1.,1.,1.,1.,1.,1.,
1.,1.,1.,1.,1.,1.,1.,1.,1.,1.,1.,1.,1.,1.,1.,1.,1.,1.,1.,1.,1.,1.,1.,1.,
1.,1.,1.,1.,1.,1.,1.,1.,1.,1.,1.,1.,1.,1.,1.,1.,1.,1.,1.,1.,1.,1.,1.,1.,
1.,1.,1.,1.,1.,1.,1.,1.,1.,1.,1.,1.,1.,1.,1.,1.,1.,1.,1.,1.,1.,1.,1.,1.,
1.,1.,1.,1.,1.,1.,1.,1.,1.,1.,1.,1.,1.,1.,1.,1.,1.,1.,1.,1.,1.,1.,1.,1.,
1.,1.,1.,1.,1.,1.,1.,1.,1.,1.,1.,1.,1.,1.,1.,1.,1.,1.,1.,1.,1.,1.,1.,1.,
1.,1.,1.,1.,1.,1.,1.,1.,1.,1.,1.,1.,1.,1.,1.,1.,1.,1.,1.,1.,1.,1.,1.,1.,
1.,1.,1.,1.,1.,1.,1.,1.,1.,1.,1.,1.,1.,1.,1.,1.,1.,1.,1.,1.,1.,1.,1.,1.,
1.,1.,1.,1.,1.,1.,1.,1.,1.,1.,1.,1.,1.,1.,1.,1.,1.,1.,1.,1.,1.,1.,1.,1.,
1.,1.,1.,1.,1.,1.,1.,1.,1.,1.,1.,1.,1.,1.,1.,1.,1.,1.,1.,1.,1.,1.,1.,1.,
1.,1.,1.,1.,1.,1.,1.,1.,1.,1.,1.,1.,1.,1.,1.,1.,1.,1.,1.,1.,1.,1.,1.,1.,
1.,1.,1.,1.,1.,1.,1.,1.,1.,1.,1.,1.,1.,1.,1.,1.,1.,1.,1.,1.,1.,1.,1.,1.,
1.,1.,1.,1.,1.,1.,1.,1.,1.,1.,1.,1.,1.,1.,1.,1.,1.,1.,1.,1.,1.,1.,1.,1.,
1.,1.,1.,1.,1.,1.,1.,1.,1.,1.,1.,1.,1.,1.,1.,1.,1.,1.,1.,1.,1.,1.,1.,1.,
1.,1.,1.,1.,1.,1.),(0.707106781186548,0.707106781186548,0.707106781186548,
0.707106781186547,0.707106781186547,0.707106781186548,0.707106781186547,
0.707106781186547,0.707106781186547,0.707106781186547,0.707106781186547,
0.707106781186548,0.707106781186548,0.707106781186548,0.707106781186547,
0.707106781186548,0.707106781186547,0.707106781186547,0.707106781186548,
0.707106781186547,0.707106781186548,0.707106781186547,0.707106781186548,
0.707106781186547,0.707106781186548,0.707106781186547,0.707106781186547,
0.707106781186547,0.707106781186547,0.707106781186547,0.707106781186548,
0.707106781186547,0.707106781186547,0.707106781186548,0.707106781186547,
0.707106781186547,0.707106781186548,0.707106781186547,0.707106781186547,
0.707106781186548,0.707106781186548,0.707106781186547,0.707106781186548,
0.707106781186547,0.707106781186547,0.707106781186547,0.707106781186548,
0.707106781186548,0.707106781186547,0.707106781186547,0.707106781186548,
0.707106781186547,0.707106781186548,0.707106781186547,0.707106781186547,
0.707106781186547,0.707106781186547,0.707106781186547,0.707106781186548,
0.707106781186547,0.707106781186548,0.707106781186547,0.707106781186548,
0.707106781186547,0.707106781186548,0.707106781186547,0.707106781186547,
0.707106781186548,0.707106781186547,0.707106781186547,0.707106781186548,
0.707106781186547,0.707106781186548,0.707106781186547,0.707106781186548,
0.707106781186548,0.707106781186547,0.707106781186548,0.707106781186547,
0.707106781186547,0.707106781186548,0.707106781186547,0.707106781186547,
0.707106781186547,0.707106781186548,0.707106781186547,0.707106781186547,
0.707106781186547,0.707106781186547,0.707106781186547,0.707106781186547,
0.707106781186548,0.707106781186548,0.707106781186547,0.707106781186548,
0.707106781186547,0.707106781186548,0.707106781186548,0.707106781186547,
0.707106781186548,0.707106781186548,0.707106781186548,0.707106781186547,
0.707106781186548,0.707106781186547,0.707106781186548,0.707106781186548,
0.707106781186548,0.707106781186547,0.707106781186547,0.707106781186547,
0.707106781186548,0.707106781186548,0.707106781186548,0.707106781186547,
0.707106781186547,0.707106781186547,0.707106781186548,0.707106781186548,
0.707106781186547,0.707106781186547,0.707106781186548,0.707106781186547,
0.707106781186547,0.707106781186547,0.707106781186547,0.707106781186548,
0.707106781186547,0.707106781186548,0.707106781186547,0.707106781186547,
0.707106781186547,0.707106781186548,0.707106781186548,0.707106781186547,
0.707106781186548,0.707106781186548,0.707106781186547,0.707106781186548,
0.707106781186547,0.707106781186548,0.707106781186547,0.707106781186548,
0.707106781186547,0.707106781186547,0.707106781186548,0.707106781186547,
0.707106781186547,0.707106781186548,0.707106781186547,0.707106781186547,
0.707106781186548,0.707106781186547,0.707106781186548,0.707106781186547,
0.707106781186547,0.707106781186548,0.707106781186548,0.707106781186547,
0.707106781186548,0.707106781186547,0.707106781186548,0.707106781186547,
0.707106781186548,0.707106781186547,0.707106781186548,0.707106781186547,
0.707106781186548,0.707106781186547,0.707106781186548,0.707106781186547,
0.707106781186548,0.707106781186547,0.707106781186547,0.707106781186548,
0.707106781186547,0.707106781186548,0.707106781186547,0.707106781186548,
0.707106781186547,0.707106781186548,0.707106781186547,0.707106781186547,
0.707106781186548,0.707106781186547,0.707106781186548,0.707106781186548,
0.707106781186548,0.707106781186547,0.707106781186547,0.707106781186547,
0.707106781186547,0.707106781186548,0.707106781186547,0.707106781186548,
0.707106781186548,0.707106781186547,0.707106781186547,0.707106781186548,
0.707106781186548,0.707106781186547,0.707106781186547,0.707106781186548,
0.707106781186547,0.707106781186548,0.707106781186547,0.707106781186547,
0.707106781186547,0.707106781186547,0.707106781186547,0.707106781186547,
0.707106781186547,0.707106781186548,0.707106781186547,0.707106781186548,
0.707106781186547,0.707106781186548,0.707106781186548,0.707106781186547,
0.707106781186548,0.707106781186548,0.707106781186548,0.707106781186548,
0.707106781186547,0.707106781186548,0.707106781186547,0.707106781186548,
0.707106781186547,0.707106781186547,0.707106781186548,0.707106781186548,
0.707106781186547,0.707106781186547,0.707106781186547,0.707106781186547,
0.707106781186547,0.707106781186548,0.707106781186548,0.707106781186547,
0.707106781186547,0.707106781186548,0.707106781186548,0.707106781186547,
0.707106781186548,0.707106781186547,0.707106781186548,0.707106781186548,
0.707106781186547,0.707106781186547,0.707106781186548,0.707106781186547,
0.707106781186547,0.707106781186548,0.707106781186547,0.707106781186548,
0.707106781186547,0.707106781186548,0.707106781186547,0.707106781186547,
0.707106781186548,0.707106781186548,0.707106781186547,0.707106781186547,
0.707106781186548,0.707106781186547,0.707106781186547,0.707106781186548,
0.707106781186547,0.707106781186548,0.707106781186547,0.707106781186548,
0.707106781186547,0.707106781186548,0.707106781186547,0.707106781186547,
0.707106781186547,0.707106781186547,0.707106781186547,0.707106781186547,
0.707106781186548,0.707106781186547,0.707106781186548,0.707106781186547,
0.707106781186548,0.707106781186548,0.707106781186547,0.707106781186548,
0.707106781186548,0.707106781186547,0.707106781186548,0.707106781186547,
0.707106781186547,0.707106781186547,0.707106781186548,0.707106781186547,
0.707106781186547,0.707106781186548,0.707106781186547,0.707106781186548,
0.707106781186547,0.707106781186547,0.707106781186547,0.707106781186548,
0.707106781186548,0.707106781186547,0.707106781186548,0.707106781186548,
0.707106781186547,0.707106781186548,0.707106781186547,0.707106781186548,
0.707106781186548,0.707106781186547,0.707106781186548,0.707106781186548,
0.707106781186548,0.707106781186547,0.707106781186547,0.707106781186548,
0.707106781186547,0.707106781186548,0.707106781186547,0.707106781186547,
0.707106781186548,0.707106781186548,0.707106781186548,0.707106781186547,
0.707106781186547,0.707106781186548,0.707106781186548,0.707106781186547,
0.707106781186547,0.707106781186548,0.707106781186547,0.707106781186547,
0.707106781186548,0.707106781186548,0.707106781186547,0.707106781186547,
0.707106781186547,0.707106781186548,0.707106781186547,0.707106781186547,
0.707106781186547,0.707106781186548,0.707106781186548,0.707106781186547,
0.707106781186548,0.707106781186547,0.707106781186548,0.707106781186547,
0.707106781186548,0.707106781186548,0.707106781186547,0.707106781186547,
0.707106781186548,0.707106781186547,0.707106781186547,0.707106781186548,
0.707106781186547,0.707106781186548,0.707106781186548,0.707106781186547,
0.707106781186548,0.707106781186547,0.707106781186547,0.707106781186547,
0.707106781186548,0.707106781186548,0.707106781186548,0.707106781186547,
0.707106781186548,0.707106781186547,0.707106781186548,0.707106781186547,
0.707106781186547,0.707106781186547,0.707106781186547,0.707106781186548,
0.707106781186548,0.707106781186547,0.707106781186547,0.707106781186548,
0.707106781186547,0.707106781186548,0.707106781186547,0.707106781186548,
0.707106781186547,0.707106781186547,0.707106781186548,0.707106781186547,
0.707106781186548,0.707106781186547,0.707106781186548,0.707106781186548,
0.707106781186547,0.707106781186548,0.707106781186547,0.707106781186548,
0.707106781186548,0.707106781186547,0.707106781186548,0.707106781186547,
0.707106781186547,0.707106781186548,0.707106781186547,0.707106781186548,
0.707106781186547,0.707106781186548,0.707106781186547,0.707106781186547,
0.707106781186548,0.707106781186548,0.707106781186548,0.707106781186548,
0.707106781186547,0.707106781186548,0.707106781186548,0.707106781186548,
0.707106781186547,0.707106781186548,0.707106781186548,0.707106781186548,
0.707106781186547,0.707106781186547,0.707106781186548,0.707106781186547,
0.707106781186548,0.707106781186547,0.707106781186548,0.707106781186548,
0.707106781186547,0.707106781186547,0.707106781186548,0.707106781186547,
0.707106781186548,0.707106781186547,0.707106781186548,0.707106781186548,
0.707106781186547,0.707106781186547,0.707106781186547,0.707106781186548,
0.707106781186548,0.707106781186547,0.707106781186547,0.707106781186548,
0.707106781186548,0.707106781186548,0.707106781186548,0.707106781186547,
0.707106781186547,0.707106781186548,0.707106781186548,0.707106781186547,
0.707106781186548,0.707106781186547,0.707106781186548,0.707106781186547,
0.707106781186548,0.707106781186547,0.707106781186547,0.707106781186548,
0.707106781186547,0.707106781186547,0.707106781186548,0.707106781186547,
0.707106781186548,0.707106781186547,0.707106781186548,0.707106781186547,
0.707106781186548,0.707106781186547,0.707106781186548,0.707106781186547,
0.707106781186548,0.707106781186547,0.707106781186547,0.707106781186548,
0.707106781186548,0.707106781186547,0.707106781186547,0.707106781186547,
0.707106781186548,0.707106781186547,0.707106781186548,0.707106781186547,
0.707106781186548,0.707106781186547,0.707106781186548,0.707106781186547,
0.707106781186547,0.707106781186547,0.707106781186548,0.707106781186547,
0.707106781186548,0.707106781186548,0.707106781186547,0.707106781186548,
0.707106781186547,0.707106781186547,0.707106781186548,0.707106781186547,
0.707106781186547,0.707106781186548,0.707106781186547,0.707106781186547,
0.707106781186547,0.707106781186547,0.707106781186548,0.707106781186547,
0.707106781186547,0.707106781186547,0.707106781186548,0.707106781186547,
0.707106781186547,0.707106781186548,0.707106781186548,0.707106781186547,
0.707106781186548,0.707106781186548,0.707106781186547,0.707106781186547,
0.707106781186548,0.707106781186547,0.707106781186547,0.707106781186548,
0.707106781186547,0.707106781186547,0.707106781186547,0.707106781186548,
0.707106781186547,0.707106781186548,0.707106781186547,0.707106781186548,
0.707106781186547,0.707106781186548,0.707106781186547,0.707106781186548,
0.707106781186547,0.707106781186548,0.707106781186548,0.707106781186547,
0.707106781186547,0.707106781186548,0.707106781186547,0.707106781186548,
0.707106781186547,0.707106781186548,0.707106781186548,0.707106781186547,
0.707106781186548,0.707106781186547,0.707106781186548,0.707106781186548,
0.707106781186547,0.707106781186547,0.707106781186548,0.707106781186547,
0.707106781186548,0.707106781186547,0.707106781186548,0.707106781186547,
0.707106781186548,0.707106781186547,0.707106781186547,0.707106781186547,
0.707106781186547,0.707106781186547,0.707106781186547,0.707106781186547,
0.707106781186547,0.707106781186548,0.707106781186547,0.707106781186548,
0.707106781186547,0.707106781186547,0.707106781186548,0.707106781186547,
0.707106781186548,0.707106781186547,0.707106781186547,0.707106781186548,
0.707106781186547,0.707106781186548,0.707106781186547,0.707106781186548,
0.707106781186547,0.707106781186548,0.707106781186547,0.707106781186548,
0.707106781186547,0.707106781186548,0.707106781186547,0.707106781186548,
0.707106781186548,0.707106781186547,0.707106781186548,0.707106781186547,
0.707106781186547,0.707106781186547,0.707106781186548,0.707106781186547,
0.707106781186547,0.707106781186547,0.707106781186548,0.707106781186547,
0.707106781186547,0.707106781186548,0.707106781186547,0.707106781186547,
0.707106781186547,0.707106781186547,0.707106781186548,0.707106781186547,
0.707106781186547,0.707106781186547,0.707106781186548,0.707106781186548,
0.707106781186548,0.707106781186548,0.707106781186547,0.707106781186548,
0.707106781186547,0.707106781186547,0.707106781186548,0.707106781186547,
0.707106781186548,0.707106781186547,0.707106781186547,0.707106781186548,
0.707106781186547,0.707106781186547,0.707106781186547,0.707106781186547,
0.707106781186548,0.707106781186548,0.707106781186547,0.707106781186547,
0.707106781186548,0.707106781186547,0.707106781186548,0.707106781186547,
0.707106781186548,0.707106781186548,0.707106781186547,0.707106781186547,
0.707106781186548,0.707106781186548,0.707106781186547,0.707106781186548,
0.707106781186548,0.707106781186547,0.707106781186548,0.707106781186548,
0.707106781186548,0.707106781186547,0.707106781186548,0.707106781186547,
0.707106781186548,0.707106781186547,0.707106781186548,0.707106781186547,
0.707106781186548,0.707106781186547,0.707106781186548,0.707106781186548,
0.707106781186547,0.707106781186547,0.707106781186548,0.707106781186547,
0.707106781186548,0.707106781186547,0.707106781186548,0.707106781186548,
0.707106781186548,0.707106781186548,0.707106781186548,0.707106781186547,
0.707106781186547,0.707106781186547,0.707106781186547,0.707106781186548,
0.707106781186547,0.707106781186548,0.707106781186547,0.707106781186547,
0.707106781186548,0.707106781186548,0.707106781186547,0.707106781186548,
0.707106781186547,0.707106781186548,0.707106781186548,0.707106781186547,
0.707106781186547,0.707106781186548,0.707106781186547,0.707106781186548,
0.707106781186547,0.707106781186548,0.707106781186547,0.707106781186548,
0.707106781186547,0.707106781186548,0.707106781186547,0.707106781186548,
0.707106781186547,0.707106781186548,0.707106781186548,0.707106781186547,
0.707106781186548,0.707106781186547,0.707106781186548,0.707106781186547,
0.707106781186548,0.707106781186548,0.707106781186548,0.707106781186547,
0.707106781186547,0.707106781186548,0.707106781186548,0.707106781186547,
0.707106781186547,0.707106781186547,0.707106781186548,0.707106781186547,
0.707106781186548,0.707106781186547,0.707106781186548,0.707106781186547,
0.707106781186547,0.707106781186547,0.707106781186548,0.707106781186547,
0.707106781186548,0.707106781186547,0.707106781186548,0.707106781186547,
0.707106781186548,0.707106781186547,0.707106781186547,0.707106781186548,
0.707106781186547,0.707106781186547,0.707106781186548,0.707106781186547,
0.707106781186547,0.707106781186548,0.707106781186547,0.707106781186547,
0.707106781186547,0.707106781186548,0.707106781186547,0.707106781186548,
0.707106781186547,0.707106781186547,0.707106781186547,0.707106781186548,
0.707106781186548,0.707106781186547,0.707106781186547,0.707106781186548,
0.707106781186548,0.707106781186548,0.707106781186547,0.707106781186548,
0.707106781186547,0.707106781186548,0.707106781186547,0.707106781186548,
0.707106781186547,0.707106781186547,0.707106781186547,0.707106781186547,
0.707106781186548,0.707106781186547,0.707106781186548,0.707106781186548,
0.707106781186547,0.707106781186548,0.707106781186547,0.707106781186547,
0.707106781186547,0.707106781186547,0.707106781186548,0.707106781186547,
0.707106781186548,0.707106781186547,0.707106781186548,0.707106781186548,
0.707106781186547,0.707106781186548,0.707106781186547,0.707106781186547,
0.707106781186547,0.707106781186547,0.707106781186548,0.707106781186547,
0.707106781186548,0.707106781186548,0.707106781186547,0.707106781186548,
0.707106781186547,0.707106781186548,0.707106781186547,0.707106781186547,
0.707106781186548,0.707106781186547,0.707106781186548,0.707106781186548,
0.707106781186547,0.707106781186547,0.707106781186548,0.707106781186548,
0.707106781186547,0.707106781186547,0.707106781186548,0.707106781186547,
0.707106781186547,0.707106781186548,0.707106781186547,0.707106781186547,
0.707106781186548,0.707106781186547,0.707106781186548,0.707106781186547,
0.707106781186547,0.707106781186548,0.707106781186547,0.707106781186548,
0.707106781186547,0.707106781186548,0.707106781186547,0.707106781186547,
0.707106781186547,0.707106781186548,0.707106781186547,0.707106781186548,
0.707106781186547,0.707106781186548,0.707106781186548,0.707106781186548,
0.707106781186548,0.707106781186547,0.707106781186547,0.707106781186547,
0.707106781186548,0.707106781186547,0.707106781186548,0.707106781186547,
0.707106781186547,0.707106781186548,0.707106781186547,0.707106781186547,
0.707106781186548,0.707106781186547,0.707106781186547,0.707106781186548,
0.707106781186548,0.707106781186547,0.707106781186548,0.707106781186547,
0.707106781186547,0.707106781186548,0.707106781186547,0.707106781186548,
0.707106781186547,0.707106781186548,0.707106781186547,0.707106781186547,
0.707106781186547,0.707106781186548,0.707106781186547,0.707106781186548,
0.707106781186547,0.707106781186548,0.707106781186547,0.707106781186547,
0.707106781186548,0.707106781186548,0.707106781186548,0.707106781186547,
0.707106781186548,0.707106781186547,0.707106781186548,0.707106781186547,
0.707106781186548,0.707106781186547,0.707106781186548,0.707106781186548,
0.707106781186547,0.707106781186547,0.707106781186547,0.707106781186548,
0.707106781186547,0.707106781186547,0.707106781186548,0.707106781186547,
0.707106781186547,0.707106781186548,0.707106781186547,0.707106781186548,
0.707106781186548,0.707106781186548,0.707106781186547,0.707106781186548,
0.707106781186547,0.707106781186548,0.707106781186547,0.707106781186548,
0.707106781186547,0.707106781186548,0.707106781186547,0.707106781186548,
0.707106781186547,0.707106781186548,0.707106781186548,0.707106781186547,
0.707106781186548,0.707106781186547,0.707106781186548,0.707106781186548,
0.707106781186547,0.707106781186547,0.707106781186548,0.707106781186547,
0.707106781186547,0.707106781186548,0.707106781186547,0.707106781186548,
0.707106781186548,0.707106781186547,0.707106781186548,0.707106781186548,
0.707106781186548,0.707106781186548,0.707106781186548,0.707106781186547,
0.707106781186548,0.707106781186548,0.707106781186548,0.707106781186547,
0.707106781186548,0.707106781186547,0.707106781186548,0.707106781186547,
0.707106781186548,0.707106781186547,0.707106781186548,0.707106781186547,
0.707106781186548,0.707106781186547,0.707106781186547,0.707106781186548,
0.707106781186547,0.707106781186547,0.707106781186548,0.707106781186547,
0.707106781186548,0.707106781186547,0.707106781186548,0.707106781186547,
0.707106781186548,0.707106781186547,0.707106781186547,0.707106781186548,
0.707106781186547,0.707106781186547,0.707106781186548,0.707106781186547,
0.707106781186548,0.707106781186547,0.707106781186547,0.707106781186548,
0.707106781186548,0.707106781186547,0.707106781186548,0.707106781186547,
0.707106781186547,0.707106781186547,0.707106781186548,0.707106781186547,
0.707106781186547,0.707106781186548,0.707106781186547,0.707106781186547,
0.707106781186547,0.707106781186548,0.707106781186548,0.707106781186547,
0.707106781186548,0.707106781186547,0.707106781186548,0.707106781186547,
0.707106781186547,0.707106781186548,0.707106781186547,0.707106781186548,
0.707106781186547,0.707106781186547,0.707106781186547,0.707106781186547,
0.707106781186548,0.707106781186547,0.707106781186547,0.707106781186547,
0.707106781186547,0.707106781186547,0.707106781186548,0.707106781186547,
0.707106781186547,0.707106781186547,0.707106781186547,0.707106781186548,
0.707106781186547,0.707106781186548,0.707106781186547,0.707106781186547,
0.707106781186548,0.707106781186547,0.707106781186548,0.707106781186547,
0.707106781186547,0.707106781186548,0.707106781186547,0.707106781186547,
0.707106781186548,0.707106781186547,0.707106781186547,0.707106781186547,
0.707106781186547,0.707106781186548,0.707106781186547,0.707106781186548,
0.707106781186548,0.707106781186547,0.707106781186548,0.707106781186548,
0.707106781186547,0.707106781186547,0.707106781186548,0.707106781186547,
0.707106781186547,0.707106781186547,0.707106781186548,0.707106781186547,
0.707106781186547,0.707106781186548,0.707106781186547,0.707106781186548,
0.707106781186547,0.707106781186548,0.707106781186547,0.707106781186547,
0.707106781186548,0.707106781186547,0.707106781186548,0.707106781186547,
0.707106781186548,0.707106781186547,0.707106781186548,0.707106781186547,
0.707106781186548,0.707106781186547,0.707106781186547,0.707106781186547,
0.707106781186547,0.707106781186548,0.707106781186548,0.707106781186547,
0.707106781186548,0.707106781186548,0.707106781186547,0.707106781186548,
0.707106781186547,0.707106781186547,0.707106781186548,0.707106781186547,
0.707106781186547,0.707106781186547,0.707106781186547,0.707106781186548,
0.707106781186547,0.707106781186547,0.707106781186547,0.707106781186548,
0.707106781186547,0.707106781186547,0.707106781186548,0.707106781186547,
0.707106781186548,0.707106781186548,0.707106781186547,0.707106781186548,
0.707106781186547,0.707106781186548,0.707106781186547,0.707106781186548,
0.707106781186547,0.707106781186547,0.707106781186548,0.707106781186547,
0.707106781186548,0.707106781186548,0.707106781186547,0.707106781186547,
0.707106781186548,0.707106781186547,0.707106781186548,0.707106781186547,
0.707106781186548,0.707106781186547,0.707106781186547,0.707106781186548,
0.707106781186548,0.707106781186547,0.707106781186548,0.707106781186548,
0.707106781186547,0.707106781186548,0.707106781186548,0.707106781186547,
0.707106781186548,0.707106781186547,0.707106781186548,0.707106781186547,
0.707106781186548,0.707106781186547,0.707106781186548,0.707106781186547,
0.707106781186547,0.707106781186548,0.707106781186547,0.707106781186547,
0.707106781186548,0.707106781186547,0.707106781186548,0.707106781186548,
0.707106781186547,0.707106781186547,0.707106781186547,0.707106781186548,
0.707106781186547,0.707106781186548,0.707106781186548,0.707106781186547,
0.707106781186548,0.707106781186547,0.707106781186548,0.707106781186547,
0.707106781186548,0.707106781186547,0.707106781186547,0.707106781186548,
0.707106781186548,0.707106781186548,0.707106781186547,0.707106781186548,
0.707106781186548,0.707106781186547,0.707106781186548,0.707106781186547,
0.707106781186548,0.707106781186548,0.707106781186548,0.707106781186548,
0.707106781186548,0.707106781186548,0.707106781186547,0.707106781186547,
0.707106781186548,0.707106781186547,0.707106781186547,0.707106781186548,
0.707106781186547,0.707106781186547,0.707106781186548,0.707106781186547,
0.707106781186548,0.707106781186547,0.707106781186548,0.707106781186547,
0.707106781186547,0.707106781186547,0.707106781186548,0.707106781186547,
0.707106781186547,0.707106781186548,0.707106781186547,0.707106781186548,
0.707106781186547,0.707106781186548,0.707106781186547,0.707106781186547,
0.707106781186547,0.707106781186547,0.707106781186548,0.707106781186547,
0.707106781186547,0.707106781186548,0.707106781186548,0.707106781186547,
0.707106781186548,0.707106781186547,0.707106781186548,0.707106781186547,
0.707106781186547,0.707106781186548,0.707106781186547,0.707106781186548,
0.707106781186547,0.707106781186548,0.707106781186547,0.707106781186548,
0.707106781186548,0.707106781186547,0.707106781186548,0.707106781186547,
0.707106781186547,0.707106781186548,0.707106781186547,0.707106781186547,
0.707106781186548,0.707106781186548,0.707106781186548,0.707106781186547,
0.707106781186548,0.707106781186547,0.707106781186547,0.707106781186547,
0.707106781186548,0.707106781186547,0.707106781186548,0.707106781186548,
0.707106781186548,0.707106781186547,0.707106781186547,0.707106781186547,
0.707106781186547,0.707106781186548,0.707106781186547,0.707106781186547,
0.707106781186548,0.707106781186547,0.707106781186548,0.707106781186547,
0.707106781186547,0.707106781186548,0.707106781186547,0.707106781186548,
0.707106781186547,0.707106781186548,0.707106781186547,0.707106781186547,
0.707106781186547,0.707106781186547,0.707106781186547,0.707106781186547,
0.707106781186548,0.707106781186547,0.707106781186547,0.707106781186548,
0.707106781186548,0.707106781186547,0.707106781186548,0.707106781186548,
0.707106781186547,0.707106781186547,0.707106781186548,0.707106781186547,
0.707106781186547,0.707106781186548,0.707106781186547,0.707106781186548,
0.707106781186548,0.707106781186548,0.707106781186547,0.707106781186547,
0.707106781186547,0.707106781186547,0.707106781186548,0.707106781186548,
0.707106781186548,0.707106781186547,0.707106781186548,0.707106781186547,
0.707106781186548,0.707106781186548,0.707106781186547,0.707106781186548,
0.707106781186547,0.707106781186548,0.707106781186548,0.707106781186547,
0.707106781186547,0.707106781186548,0.707106781186547,0.707106781186548,
0.707106781186547,0.707106781186548,0.707106781186548,0.707106781186548,
0.707106781186547,0.707106781186548,0.707106781186547,0.707106781186547,
0.707106781186547,0.707106781186547,0.707106781186548,0.707106781186548,
0.707106781186547,0.707106781186547,0.707106781186547,0.707106781186548,
0.707106781186547,0.707106781186547,0.707106781186548,0.707106781186547,
0.707106781186548,0.707106781186548,0.707106781186548,0.707106781186547,
0.707106781186547,0.707106781186547,0.707106781186547,0.707106781186548,
0.707106781186548,0.707106781186547,0.707106781186548,0.707106781186547,
0.707106781186548,0.707106781186548,0.707106781186547,0.707106781186548,
0.707106781186547,0.707106781186548,0.707106781186547,0.707106781186547,
0.707106781186547,0.707106781186548,0.707106781186547,0.707106781186548,
0.707106781186547,0.707106781186548,0.707106781186547,0.707106781186548,
0.707106781186547,0.707106781186548,0.707106781186547,0.707106781186547,
0.707106781186548,0.707106781186547,0.707106781186548,0.707106781186547,
0.707106781186547,0.707106781186548,0.707106781186548,0.707106781186547,
0.707106781186548,0.707106781186548,0.707106781186547,0.707106781186548,
0.707106781186547,0.707106781186548,0.707106781186547,0.707106781186547,
0.707106781186547,0.707106781186548,0.707106781186547,0.707106781186547,
0.707106781186548,0.707106781186547,0.707106781186548,0.707106781186547,
0.707106781186548,0.707106781186548,0.707106781186547,0.707106781186548,
0.707106781186547,0.707106781186548,0.707106781186548,0.707106781186548,
0.707106781186548,0.707106781186547,0.707106781186547,0.707106781186548,
0.707106781186547,0.707106781186547,0.707106781186548,0.707106781186548,
0.707106781186547,0.707106781186547,0.707106781186548,0.707106781186547,
0.707106781186547,0.707106781186548,0.707106781186547,0.707106781186548,
0.707106781186547,0.707106781186548,0.707106781186547,0.707106781186547,
0.707106781186547,0.707106781186548,0.707106781186547,0.707106781186547,
0.707106781186548,0.707106781186547,0.707106781186548,0.707106781186548,
0.707106781186548,0.707106781186547,0.707106781186547,0.707106781186547,
0.707106781186548,0.707106781186548,0.707106781186547,0.707106781186547,
0.707106781186547,0.707106781186547,0.707106781186548,0.707106781186548,
0.707106781186547,0.707106781186547,0.707106781186547,0.707106781186548,
0.707106781186548,0.707106781186547,0.707106781186548,0.707106781186547,
0.707106781186548,0.707106781186547,0.707106781186548,0.707106781186548,
0.707106781186547,0.707106781186548,0.707106781186548,0.707106781186548,
0.707106781186547,0.707106781186547,0.707106781186547,0.707106781186548,
0.707106781186548,0.707106781186548,0.707106781186547,0.707106781186547,
0.707106781186548,0.707106781186548,0.707106781186547,0.707106781186548,
0.707106781186547,0.707106781186547,0.707106781186548,0.707106781186547,
0.707106781186548,0.707106781186547,0.707106781186547,0.707106781186548,
0.707106781186547,0.707106781186548,0.707106781186548,0.707106781186547,
0.707106781186547,0.707106781186548,0.707106781186547,0.707106781186548,
0.707106781186547,0.707106781186547,0.707106781186548,0.707106781186547,
0.707106781186548,0.707106781186547,0.707106781186548,0.707106781186547,
0.707106781186547,0.707106781186548,0.707106781186547,0.707106781186547,
0.707106781186547,0.707106781186547,0.707106781186547,0.707106781186547,
0.707106781186548,0.707106781186547,0.707106781186548,0.707106781186548,
0.707106781186548,0.707106781186547,0.707106781186547,0.707106781186547,
0.707106781186548,0.707106781186547,0.707106781186548,0.707106781186547,
0.707106781186547,0.707106781186548,0.707106781186547,0.707106781186547,
0.707106781186547,0.707106781186547,0.707106781186547,0.707106781186548,
0.707106781186547,0.707106781186548,0.707106781186547,0.707106781186547,
0.707106781186548,0.707106781186548,0.707106781186547,0.707106781186547,
0.707106781186547,0.707106781186548,0.707106781186547,0.707106781186547,
0.707106781186548,0.707106781186548,0.707106781186547,0.707106781186548,
0.707106781186547,0.707106781186548,0.707106781186548,0.707106781186547,
0.707106781186547,0.707106781186547,0.707106781186548,0.707106781186548,
0.707106781186547,0.707106781186548,0.707106781186547,0.707106781186548,
0.707106781186548,0.707106781186547,0.707106781186548,0.707106781186547,
0.707106781186547,0.707106781186547,0.707106781186548,0.707106781186547,
0.707106781186548,0.707106781186547,0.707106781186548,0.707106781186547,
0.707106781186547,0.707106781186547,0.707106781186547,0.707106781186547,
0.707106781186548,0.707106781186547,0.707106781186548,0.707106781186547,
0.707106781186548,0.707106781186547,0.707106781186548,0.707106781186547,
0.707106781186547,0.707106781186547,0.707106781186547,0.707106781186547,
0.707106781186548,0.707106781186548,0.707106781186548,0.707106781186547,
0.707106781186548,0.707106781186547,0.707106781186548,0.707106781186547,
0.707106781186547,0.707106781186548,0.707106781186547,0.707106781186548,
0.707106781186547,0.707106781186547,0.707106781186547,0.707106781186548,
0.707106781186548,0.707106781186547,0.707106781186548,0.707106781186547,
0.707106781186548,0.707106781186548,0.707106781186547,0.707106781186548,
0.707106781186547,0.707106781186548,0.707106781186548,0.707106781186547,
0.707106781186547,0.707106781186547,0.707106781186547,0.707106781186547,
0.707106781186547,0.707106781186548,0.707106781186548,0.707106781186547,
0.707106781186548,0.707106781186547,0.707106781186547,0.707106781186548,
0.707106781186547,0.707106781186547,0.707106781186548,0.707106781186547,
0.707106781186547,0.707106781186547,0.707106781186548,0.707106781186547,
0.707106781186547,0.707106781186548,0.707106781186547,0.707106781186548,
0.707106781186548,0.707106781186547,0.707106781186547,0.707106781186547,
0.707106781186548,0.707106781186547,0.707106781186547,0.707106781186548,
0.707106781186548,0.707106781186548,0.707106781186548,0.707106781186547,
0.707106781186548,0.707106781186548,0.707106781186547,0.707106781186547,
0.707106781186548,0.707106781186547,0.707106781186548,0.707106781186547,
0.707106781186547,0.707106781186548,0.707106781186547,0.707106781186547,
0.707106781186548,0.707106781186547,0.707106781186548,0.707106781186547,
0.707106781186548,0.707106781186547,0.707106781186548,0.707106781186547,
0.707106781186548,0.707106781186547,0.707106781186548,0.707106781186548,
0.707106781186547,0.707106781186547,0.707106781186548,0.707106781186548,
0.707106781186547,0.707106781186547,0.707106781186547,0.707106781186547,
0.707106781186547,0.707106781186548,0.707106781186547,0.707106781186547,
0.707106781186548,0.707106781186547,0.707106781186548,0.707106781186548,
0.707106781186547,0.707106781186548,0.707106781186547,0.707106781186548,
0.707106781186547,0.707106781186548,0.707106781186547,0.707106781186547,
0.707106781186547,0.707106781186547,0.707106781186547,0.707106781186547,
0.707106781186548,0.707106781186547,0.707106781186548,0.707106781186547,
0.707106781186547,0.707106781186547,0.707106781186548,0.707106781186547,
0.707106781186548,0.707106781186548,0.707106781186547,0.707106781186547,
0.707106781186548,0.707106781186547,0.707106781186548,0.707106781186547,
0.707106781186548,0.707106781186547,0.707106781186548,0.707106781186547,
0.707106781186547,0.707106781186548,0.707106781186547,0.707106781186548,
0.707106781186547,0.707106781186548,0.707106781186548,0.707106781186548,
0.707106781186548,0.707106781186547,0.707106781186548,0.707106781186548,
0.707106781186548,0.707106781186547,0.707106781186548,0.707106781186548,
0.707106781186547,0.707106781186548,0.707106781186547,0.707106781186548,
0.707106781186547,0.707106781186547,0.707106781186547,0.707106781186548,
0.707106781186548,0.707106781186547,0.707106781186548,0.707106781186547,
0.707106781186548,0.707106781186547,0.707106781186548,0.707106781186548,
0.707106781186547,0.707106781186548,0.707106781186547,0.707106781186547,
0.707106781186548,0.707106781186547,0.707106781186547,0.707106781186547,
0.707106781186548,0.707106781186547,0.707106781186548,0.707106781186548,
0.707106781186547,0.707106781186548,0.707106781186547,0.707106781186548,
0.707106781186548,0.707106781186548,0.707106781186548,0.707106781186547,
0.707106781186548,0.707106781186547,0.707106781186548,0.707106781186547,
0.707106781186548,0.707106781186547,0.707106781186547,0.707106781186547,
0.707106781186547,0.707106781186548,0.707106781186547,0.707106781186548,
0.707106781186547,0.707106781186547,0.707106781186548,0.707106781186547,
0.707106781186548,0.707106781186547,0.707106781186548,0.707106781186547,
0.707106781186548,0.707106781186548,0.707106781186548,0.707106781186548,
0.707106781186547,0.707106781186548,0.707106781186548,0.707106781186547,
0.707106781186548,0.707106781186547,0.707106781186548,0.707106781186547,
0.707106781186548,0.707106781186547,0.707106781186547,0.707106781186548,
0.707106781186547,0.707106781186548,0.707106781186547,0.707106781186547,
0.707106781186548,0.707106781186547,0.707106781186548,0.707106781186547,
0.707106781186547,0.707106781186548,0.707106781186548,0.707106781186548,
0.707106781186548,0.707106781186548,0.707106781186548,0.707106781186548,
0.707106781186548,0.707106781186548,0.707106781186547,0.707106781186548,
0.707106781186547,0.707106781186547,0.707106781186548,0.707106781186547,
0.707106781186548,0.707106781186548,0.707106781186547,0.707106781186547,
0.707106781186548,0.707106781186548,0.707106781186547,0.707106781186547,
0.707106781186547,0.707106781186547,0.707106781186547,0.707106781186548,
0.707106781186547,0.707106781186548,0.707106781186548,0.707106781186548,
0.707106781186547,0.707106781186548,0.707106781186547,0.707106781186548,
0.707106781186547,0.707106781186548,0.707106781186547,0.707106781186548,
0.707106781186548,0.707106781186547,0.707106781186547,0.707106781186548,
0.707106781186548,0.707106781186548,0.707106781186547,0.707106781186547,
0.707106781186548,0.707106781186547,0.707106781186547,0.707106781186548,
0.707106781186547,0.707106781186548,0.707106781186547,0.707106781186547,
0.707106781186548,0.707106781186548,0.707106781186548,0.707106781186547,
0.707106781186547,0.707106781186548,0.707106781186547,0.707106781186548,
0.707106781186547,0.707106781186548,0.707106781186547,0.707106781186548,
0.707106781186548,0.707106781186547,0.707106781186548,0.707106781186547,
0.707106781186548,0.707106781186547,0.707106781186547,0.707106781186547,
0.707106781186548,0.707106781186547,0.707106781186548,0.707106781186547,
0.707106781186547,0.707106781186547,0.707106781186548,0.707106781186547,
0.707106781186547,0.707106781186548,0.707106781186548,0.707106781186547,
0.707106781186548,0.707106781186547,0.707106781186548,0.707106781186548,
0.707106781186547,0.707106781186548,0.707106781186547,0.707106781186547,
0.707106781186548,0.707106781186547,0.707106781186547,0.707106781186547,
0.707106781186548,0.707106781186547,0.707106781186548,0.707106781186547,
0.707106781186548,0.707106781186548,0.707106781186548,0.707106781186547,
0.707106781186548,0.707106781186548,0.707106781186548,0.707106781186547,
0.707106781186548,0.707106781186547,0.707106781186547,0.707106781186548,
0.707106781186547,0.707106781186547,0.707106781186548,0.707106781186548,
0.707106781186547,0.707106781186548,0.707106781186547,0.707106781186548,
0.707106781186548,0.707106781186547,0.707106781186548,0.707106781186547,
0.707106781186548,0.707106781186547,0.707106781186548,0.707106781186547,
0.707106781186548,0.707106781186548,0.707106781186548,0.707106781186547,
0.707106781186548,0.707106781186548,0.707106781186547,0.707106781186547,
0.707106781186548,0.707106781186547,0.707106781186548,0.707106781186548,
0.707106781186547,0.707106781186548,0.707106781186548,0.707106781186547,
0.707106781186548,0.707106781186548,0.707106781186547,0.707106781186547,
0.707106781186548,0.707106781186547,0.707106781186548,0.707106781186547,
0.707106781186548,0.707106781186547,0.707106781186548,0.707106781186548,
0.707106781186548,0.707106781186547,0.707106781186548,0.707106781186547,
0.707106781186548,0.707106781186547,0.707106781186548,0.707106781186547,
0.707106781186548,0.707106781186547,0.707106781186548,0.707106781186547,
0.707106781186548,0.707106781186547,0.707106781186547,0.707106781186547,
0.707106781186548,0.707106781186547,0.707106781186548,0.707106781186547,
0.707106781186548,0.707106781186547,0.707106781186548,0.707106781186547,
0.707106781186548,0.707106781186548,0.707106781186548,0.707106781186547,
0.707106781186548,0.707106781186547,0.707106781186548,0.707106781186548,
0.707106781186547,0.707106781186548,0.707106781186547,0.707106781186548,
0.707106781186547,0.707106781186548,0.707106781186547,0.707106781186548,
0.707106781186547,0.707106781186547,0.707106781186547,0.707106781186548,
0.707106781186547,0.707106781186547,0.707106781186548,0.707106781186547,
0.707106781186548,0.707106781186547,0.707106781186547,0.707106781186548,
0.707106781186547,0.707106781186548,0.707106781186547,0.707106781186548,
0.707106781186548,0.707106781186548,0.707106781186547,0.707106781186547,
0.707106781186548,0.707106781186548,0.707106781186547,0.707106781186548,
0.707106781186547,0.707106781186547,0.707106781186547,0.707106781186548,
0.707106781186547,0.707106781186548,0.707106781186547,0.707106781186548,
0.707106781186548,0.707106781186548,0.707106781186547,0.707106781186547,
0.707106781186547,0.707106781186547,0.707106781186547,0.707106781186547,
0.707106781186548,0.707106781186547,0.707106781186548,0.707106781186547,
0.707106781186548,0.707106781186547,0.707106781186547,0.707106781186548,
0.707106781186547,0.707106781186547,0.707106781186548,0.707106781186548,
0.707106781186547,0.707106781186547,0.707106781186547,0.707106781186548,
0.707106781186547,0.707106781186547,0.707106781186548,0.707106781186548),
(1.,1.,1.,1.,1.,1.,1.,1.,1.,1.,1.,1.,1.,1.,1.,1.,1.,1.,1.,1.,1.,1.,1.,1.,
1.,1.,1.,1.,1.,1.,1.,1.,1.,1.,1.,1.,1.,1.,1.,1.,1.,1.,1.,1.,1.,1.,1.,1.,
1.,1.,1.,1.,1.,1.,1.,1.,1.,1.,1.,1.,1.,1.,1.,1.,1.,1.,1.,1.,1.,1.,1.,1.,
1.,1.,1.,1.,1.,1.,1.,1.,1.,1.,1.,1.,1.,1.,1.,1.,1.,1.,1.,1.,1.,1.,1.,1.,
1.,1.,1.,1.,1.,1.,1.,1.,1.,1.,1.,1.,1.,1.,1.,1.,1.,1.,1.,1.,1.,1.,1.,1.,
1.,1.,1.,1.,1.,1.,1.,1.,1.,1.,1.,1.,1.,1.,1.,1.,1.,1.,1.,1.,1.,1.,1.,1.,
1.,1.,1.,1.,1.,1.,1.,1.,1.,1.,1.,1.,1.,1.,1.,1.,1.,1.,1.,1.,1.,1.,1.,1.,
1.,1.,1.,1.,1.,1.,1.,1.,1.,1.,1.,1.,1.,1.,1.,1.,1.,1.,1.,1.,1.,1.,1.,1.,
1.,1.,1.,1.,1.,1.,1.,1.,1.,1.,1.,1.,1.,1.,1.,1.,1.,1.,1.,1.,1.,1.,1.,1.,
1.,1.,1.,1.,1.,1.,1.,1.,1.,1.,1.,1.,1.,1.,1.,1.,1.,1.,1.,1.,1.,1.,1.,1.,
1.,1.,1.,1.,1.,1.,1.,1.,1.,1.,1.,1.,1.,1.,1.,1.,1.,1.,1.,1.,1.,1.,1.,1.,
1.,1.,1.,1.,1.,1.,1.,1.,1.,1.,1.,1.,1.,1.,1.,1.,1.,1.,1.,1.,1.,1.,1.,1.,
1.,1.,1.,1.,1.,1.,1.,1.,1.,1.,1.,1.,1.,1.,1.,1.,1.,1.,1.,1.,1.,1.,1.,1.,
1.,1.,1.,1.,1.,1.,1.,1.,1.,1.,1.,1.,1.,1.,1.,1.,1.,1.,1.,1.,1.,1.,1.,1.,
1.,1.,1.,1.,1.,1.,1.,1.,1.,1.,1.,1.,1.,1.,1.,1.,1.,1.,1.,1.,1.,1.,1.,1.,
1.,1.,1.,1.,1.,1.,1.,1.,1.,1.,1.,1.,1.,1.,1.,1.,1.,1.,1.,1.,1.,1.,1.,1.,
1.,1.,1.,1.,1.,1.,1.,1.,1.,1.,1.,1.,1.,1.,1.,1.,1.,1.,1.,1.,1.,1.,1.,1.,
1.,1.,1.,1.,1.,1.,1.,1.,1.,1.,1.,1.,1.,1.,1.,1.,1.,1.,1.,1.,1.,1.,1.,1.,
1.,1.,1.,1.,1.,1.,1.,1.,1.,1.,1.,1.,1.,1.,1.,1.,1.,1.,1.,1.,1.,1.,1.,1.,
1.,1.,1.,1.,1.,1.,1.,1.,1.,1.,1.,1.,1.,1.,1.,1.,1.,1.,1.,1.,1.,1.,1.,1.,
1.,1.,1.,1.,1.,1.,1.,1.,1.,1.,1.,1.,1.,1.,1.,1.,1.,1.,1.,1.,1.,1.,1.,1.,
1.,1.,1.,1.,1.,1.,1.,1.,1.,1.,1.,1.,1.,1.,1.,1.,1.,1.,1.,1.,1.,1.,1.,1.,
1.,1.,1.,1.,1.,1.,1.,1.,1.,1.,1.,1.,1.,1.,1.,1.,1.,1.,1.,1.,1.,1.,1.,1.,
1.,1.,1.,1.,1.,1.,1.,1.,1.,1.,1.,1.,1.,1.,1.,1.,1.,1.,1.,1.,1.,1.,1.,1.,
1.,1.,1.,1.,1.,1.,1.,1.,1.,1.,1.,1.,1.,1.,1.,1.,1.,1.,1.,1.,1.,1.,1.,1.,
1.,1.,1.,1.,1.,1.,1.,1.,1.,1.,1.,1.,1.,1.,1.,1.,1.,1.,1.,1.,1.,1.,1.,1.,
1.,1.,1.,1.,1.,1.,1.,1.,1.,1.,1.,1.,1.,1.,1.,1.,1.,1.,1.,1.,1.,1.,1.,1.,
1.,1.,1.,1.,1.,1.,1.,1.,1.,1.,1.,1.,1.,1.,1.,1.,1.,1.,1.,1.,1.,1.,1.,1.,
1.,1.,1.,1.,1.,1.,1.,1.,1.,1.,1.,1.,1.,1.,1.,1.,1.,1.,1.,1.,1.,1.,1.,1.,
1.,1.,1.,1.,1.,1.,1.,1.,1.,1.,1.,1.,1.,1.,1.,1.,1.,1.,1.,1.,1.,1.,1.,1.,
1.,1.,1.,1.,1.,1.,1.,1.,1.,1.,1.,1.,1.,1.,1.,1.,1.,1.,1.,1.,1.,1.,1.,1.,
1.,1.,1.,1.,1.,1.,1.,1.,1.,1.,1.,1.,1.,1.,1.,1.,1.,1.,1.,1.,1.,1.,1.,1.,
1.,1.,1.,1.,1.,1.,1.,1.,1.,1.,1.,1.,1.,1.,1.,1.,1.,1.,1.,1.,1.,1.,1.,1.,
1.,1.,1.,1.,1.,1.,1.,1.,1.,1.,1.,1.,1.,1.,1.,1.,1.,1.,1.,1.,1.,1.,1.,1.,
1.,1.,1.,1.,1.,1.,1.,1.,1.,1.,1.,1.,1.,1.,1.,1.,1.,1.,1.,1.,1.,1.,1.,1.,
1.,1.,1.,1.,1.,1.,1.,1.,1.,1.,1.,1.,1.,1.,1.,1.,1.,1.,1.,1.,1.,1.,1.,1.,
1.,1.,1.,1.,1.,1.,1.,1.,1.,1.,1.,1.,1.,1.,1.,1.,1.,1.,1.,1.,1.,1.,1.,1.,
1.,1.,1.,1.,1.,1.,1.,1.,1.,1.,1.,1.,1.,1.,1.,1.,1.,1.,1.,1.,1.,1.,1.,1.,
1.,1.,1.,1.,1.,1.,1.,1.,1.,1.,1.,1.,1.,1.,1.,1.,1.,1.,1.,1.,1.,1.,1.,1.,
1.,1.,1.,1.,1.,1.,1.,1.,1.,1.,1.,1.,1.,1.,1.,1.,1.,1.,1.,1.,1.,1.,1.,1.,
1.,1.,1.,1.,1.,1.,1.,1.,1.,1.,1.,1.,1.,1.,1.,1.,1.,1.,1.,1.,1.,1.,1.,1.,
1.,1.,1.,1.,1.,1.,1.,1.,1.,1.,1.,1.,1.,1.,1.,1.,1.,1.,1.,1.,1.,1.,1.,1.,
1.,1.,1.,1.,1.,1.,1.,1.,1.,1.,1.,1.,1.,1.,1.,1.,1.,1.,1.,1.,1.,1.,1.,1.,
1.,1.,1.,1.,1.,1.,1.,1.,1.,1.,1.,1.,1.,1.,1.,1.,1.,1.,1.,1.,1.,1.,1.,1.,
1.,1.,1.,1.,1.,1.,1.,1.,1.,1.,1.,1.,1.,1.,1.,1.,1.,1.,1.,1.,1.,1.,1.,1.,
1.,1.,1.,1.,1.,1.,1.,1.,1.,1.,1.,1.,1.,1.,1.,1.,1.,1.,1.,1.,1.,1.,1.,1.,
1.,1.,1.,1.,1.,1.,1.,1.,1.,1.,1.,1.,1.,1.,1.,1.,1.,1.,1.,1.,1.,1.,1.,1.,
1.,1.,1.,1.,1.,1.,1.,1.,1.,1.,1.,1.,1.,1.,1.,1.,1.,1.,1.,1.,1.,1.,1.,1.,
1.,1.,1.,1.,1.,1.,1.,1.,1.,1.,1.,1.,1.,1.,1.,1.,1.,1.,1.,1.,1.,1.,1.,1.,
1.,1.,1.,1.,1.,1.,1.,1.,1.,1.,1.,1.,1.,1.,1.,1.,1.,1.,1.,1.,1.,1.,1.,1.,
1.,1.,1.,1.,1.,1.,1.,1.,1.,1.,1.,1.,1.,1.,1.,1.,1.,1.,1.,1.,1.,1.,1.,1.,
1.,1.,1.,1.,1.,1.,1.,1.,1.,1.,1.,1.,1.,1.,1.,1.,1.,1.,1.,1.,1.,1.,1.,1.,
1.,1.,1.,1.,1.,1.,1.,1.,1.,1.,1.,1.,1.,1.,1.,1.,1.,1.,1.,1.,1.,1.,1.,1.,
1.,1.,1.,1.,1.,1.,1.,1.,1.,1.,1.,1.,1.,1.,1.,1.,1.,1.,1.,1.,1.,1.,1.,1.,
1.,1.,1.,1.,1.,1.,1.,1.,1.,1.,1.,1.,1.,1.,1.,1.,1.,1.,1.,1.,1.,1.,1.,1.,
1.,1.,1.,1.,1.,1.,1.,1.,1.,1.,1.,1.,1.,1.,1.,1.,1.,1.,1.,1.,1.,1.,1.,1.,
1.,1.,1.,1.,1.,1.,1.,1.,1.,1.,1.,1.,1.,1.,1.,1.,1.,1.,1.,1.,1.,1.,1.,1.,
1.,1.,1.,1.,1.,1.,1.,1.,1.,1.,1.,1.,1.,1.,1.,1.,1.,1.,1.,1.,1.,1.,1.,1.,
1.,1.,1.,1.,1.,1.,1.,1.,1.,1.,1.,1.,1.,1.,1.,1.,1.,1.,1.,1.,1.,1.,1.,1.,
1.,1.,1.,1.,1.,1.,1.,1.,1.,1.,1.,1.,1.,1.,1.,1.,1.,1.,1.,1.,1.,1.,1.,1.,
1.,1.,1.,1.,1.,1.,1.,1.,1.,1.,1.,1.,1.,1.,1.,1.,1.,1.,1.,1.,1.,1.,1.,1.,
1.,1.,1.,1.,1.,1.,1.,1.,1.,1.,1.,1.,1.,1.,1.,1.,1.,1.,1.,1.,1.,1.,1.,1.,
1.,1.,1.,1.,1.,1.,1.,1.,1.,1.,1.,1.,1.,1.,1.,1.,1.,1.,1.,1.,1.,1.,1.,1.,
1.,1.,1.,1.,1.,1.,1.,1.,1.,1.,1.,1.,1.,1.,1.,1.,1.,1.,1.,1.,1.,1.,1.,1.,
1.,1.,1.,1.,1.,1.,1.,1.,1.,1.,1.,1.,1.,1.,1.,1.,1.,1.,1.,1.,1.,1.,1.,1.,
1.,1.,1.,1.,1.,1.,1.,1.,1.,1.,1.,1.,1.,1.,1.,1.,1.,1.,1.,1.,1.,1.,1.,1.,
1.,1.,1.,1.,1.,1.,1.,1.,1.,1.,1.,1.,1.,1.,1.,1.,1.,1.,1.,1.,1.,1.,1.,1.,
1.,1.,1.,1.,1.,1.,1.,1.,1.,1.,1.,1.,1.,1.,1.,1.,1.,1.,1.,1.,1.,1.,1.,1.,
1.,1.,1.,1.,1.,1.,1.,1.,1.,1.,1.,1.,1.,1.,1.,1.,1.,1.,1.,1.,1.,1.,1.,1.,
1.,1.,1.,1.,1.,1.,1.,1.,1.,1.,1.,1.,1.,1.,1.,1.,1.,1.,1.,1.,1.,1.,1.,1.,
1.,1.,1.,1.,1.,1.,1.,1.,1.,1.,1.,1.,1.,1.,1.,1.,1.,1.,1.,1.,1.,1.,1.,1.,
1.,1.,1.,1.,1.,1.,1.,1.,1.,1.,1.,1.,1.,1.,1.,1.,1.,1.,1.,1.,1.,1.,1.,1.,
1.,1.,1.,1.,1.,1.,1.,1.,1.,1.,1.,1.,1.,1.,1.,1.,1.,1.,1.,1.,1.,1.,1.,1.,
1.,1.,1.,1.,1.,1.,1.,1.,1.,1.,1.,1.,1.,1.,1.,1.,1.,1.,1.,1.,1.,1.,1.,1.,
1.,1.,1.,1.,1.,1.,1.,1.,1.,1.,1.,1.,1.,1.,1.,1.,1.,1.,1.,1.,1.,1.,1.,1.,
1.,1.,1.,1.,1.,1.,1.,1.,1.,1.,1.,1.,1.,1.,1.,1.,1.,1.,1.,1.,1.,1.,1.,1.,
1.,1.,1.,1.,1.,1.,1.,1.,1.,1.,1.,1.,1.,1.,1.,1.,1.,1.,1.,1.,1.,1.,1.,1.,
1.,1.,1.,1.,1.,1.,1.,1.,1.,1.,1.,1.,1.,1.,1.,1.,1.,1.,1.,1.,1.,1.,1.,1.,
1.,1.,1.,1.,1.,1.,1.,1.,1.,1.,1.,1.,1.,1.,1.,1.,1.,1.,1.,1.,1.,1.,1.,1.,
1.,1.,1.,1.,1.,1.,1.,1.,1.,1.,1.,1.,1.,1.,1.,1.,1.,1.,1.,1.,1.,1.,1.,1.,
1.,1.,1.,1.,1.,1.,1.,1.,1.,1.,1.,1.,1.,1.,1.,1.,1.,1.,1.,1.,1.,1.,1.,1.,
1.,1.,1.,1.,1.,1.,1.,1.,1.,1.,1.,1.,1.,1.,1.,1.,1.,1.,1.,1.,1.,1.,1.,1.,
1.,1.,1.,1.,1.,1.,1.,1.,1.,1.,1.,1.,1.,1.,1.,1.,1.,1.,1.,1.,1.,1.,1.,1.,
1.,1.,1.,1.,1.,1.,1.,1.,1.,1.,1.,1.,1.,1.,1.,1.,1.,1.,1.,1.,1.,1.,1.,1.,
1.,1.,1.,1.,1.,1.,1.,1.,1.,1.,1.,1.,1.,1.,1.,1.,1.,1.,1.,1.,1.,1.,1.,1.,
1.,1.,1.,1.,1.,1.,1.,1.,1.,1.,1.),(0.707106781186548,0.707106781186548,
0.707106781186548,0.707106781186547,0.707106781186547,0.707106781186548,
0.707106781186547,0.707106781186547,0.707106781186547,0.707106781186547,
0.707106781186547,0.707106781186548,0.707106781186548,0.707106781186548,
0.707106781186547,0.707106781186548,0.707106781186547,0.707106781186547,
0.707106781186548,0.707106781186547,0.707106781186548,0.707106781186547,
0.707106781186548,0.707106781186547,0.707106781186548,0.707106781186547,
0.707106781186547,0.707106781186547,0.707106781186547,0.707106781186547,
0.707106781186548,0.707106781186547,0.707106781186547,0.707106781186548,
0.707106781186547,0.707106781186547,0.707106781186548,0.707106781186547,
0.707106781186547,0.707106781186548,0.707106781186548,0.707106781186547,
0.707106781186548,0.707106781186547,0.707106781186547,0.707106781186547,
0.707106781186548,0.707106781186548,0.707106781186547,0.707106781186547,
0.707106781186548,0.707106781186547,0.707106781186548,0.707106781186547,
0.707106781186547,0.707106781186547,0.707106781186547,0.707106781186547,
0.707106781186548,0.707106781186547,0.707106781186548,0.707106781186547,
0.707106781186548,0.707106781186547,0.707106781186548,0.707106781186547,
0.707106781186547,0.707106781186548,0.707106781186547,0.707106781186547,
0.707106781186548,0.707106781186547,0.707106781186548,0.707106781186547,
0.707106781186548,0.707106781186548,0.707106781186547,0.707106781186548,
0.707106781186547,0.707106781186547,0.707106781186548,0.707106781186547,
0.707106781186547,0.707106781186547,0.707106781186548,0.707106781186547,
0.707106781186547,0.707106781186547,0.707106781186547,0.707106781186547,
0.707106781186547,0.707106781186548,0.707106781186548,0.707106781186547,
0.707106781186548,0.707106781186547,0.707106781186548,0.707106781186548,
0.707106781186547,0.707106781186548,0.707106781186548,0.707106781186548,
0.707106781186547,0.707106781186548,0.707106781186547,0.707106781186548,
0.707106781186548,0.707106781186548,0.707106781186547,0.707106781186547,
0.707106781186547,0.707106781186548,0.707106781186548,0.707106781186548,
0.707106781186547,0.707106781186547,0.707106781186547,0.707106781186548,
0.707106781186548,0.707106781186547,0.707106781186547,0.707106781186548,
0.707106781186547,0.707106781186547,0.707106781186547,0.707106781186547,
0.707106781186548,0.707106781186547,0.707106781186548,0.707106781186547,
0.707106781186547,0.707106781186547,0.707106781186548,0.707106781186548,
0.707106781186547,0.707106781186548,0.707106781186548,0.707106781186547,
0.707106781186548,0.707106781186547,0.707106781186548,0.707106781186547,
0.707106781186548,0.707106781186547,0.707106781186547,0.707106781186548,
0.707106781186547,0.707106781186547,0.707106781186548,0.707106781186547,
0.707106781186547,0.707106781186548,0.707106781186547,0.707106781186548,
0.707106781186547,0.707106781186547,0.707106781186548,0.707106781186548,
0.707106781186547,0.707106781186548,0.707106781186547,0.707106781186548,
0.707106781186547,0.707106781186548,0.707106781186547,0.707106781186548,
0.707106781186547,0.707106781186548,0.707106781186547,0.707106781186548,
0.707106781186547,0.707106781186548,0.707106781186547,0.707106781186547,
0.707106781186548,0.707106781186547,0.707106781186548,0.707106781186547,
0.707106781186548,0.707106781186547,0.707106781186548,0.707106781186547,
0.707106781186547,0.707106781186548,0.707106781186547,0.707106781186548,
0.707106781186548,0.707106781186548,0.707106781186547,0.707106781186547,
0.707106781186547,0.707106781186547,0.707106781186548,0.707106781186547,
0.707106781186548,0.707106781186548,0.707106781186547,0.707106781186547,
0.707106781186548,0.707106781186548,0.707106781186547,0.707106781186547,
0.707106781186548,0.707106781186547,0.707106781186548,0.707106781186547,
0.707106781186547,0.707106781186547,0.707106781186547,0.707106781186547,
0.707106781186547,0.707106781186547,0.707106781186548,0.707106781186547,
0.707106781186548,0.707106781186547,0.707106781186548,0.707106781186548,
0.707106781186547,0.707106781186548,0.707106781186548,0.707106781186548,
0.707106781186548,0.707106781186547,0.707106781186548,0.707106781186547,
0.707106781186548,0.707106781186547,0.707106781186547,0.707106781186548,
0.707106781186548,0.707106781186547,0.707106781186547,0.707106781186547,
0.707106781186547,0.707106781186547,0.707106781186548,0.707106781186548,
0.707106781186547,0.707106781186547,0.707106781186548,0.707106781186548,
0.707106781186547,0.707106781186548,0.707106781186547,0.707106781186548,
0.707106781186548,0.707106781186547,0.707106781186547,0.707106781186548,
0.707106781186547,0.707106781186547,0.707106781186548,0.707106781186547,
0.707106781186548,0.707106781186547,0.707106781186548,0.707106781186547,
0.707106781186547,0.707106781186548,0.707106781186548,0.707106781186547,
0.707106781186547,0.707106781186548,0.707106781186547,0.707106781186547,
0.707106781186548,0.707106781186547,0.707106781186548,0.707106781186547,
0.707106781186548,0.707106781186547,0.707106781186548,0.707106781186547,
0.707106781186547,0.707106781186547,0.707106781186547,0.707106781186547,
0.707106781186547,0.707106781186548,0.707106781186547,0.707106781186548,
0.707106781186547,0.707106781186548,0.707106781186548,0.707106781186547,
0.707106781186548,0.707106781186548,0.707106781186547,0.707106781186548,
0.707106781186547,0.707106781186547,0.707106781186547,0.707106781186548,
0.707106781186547,0.707106781186547,0.707106781186548,0.707106781186547,
0.707106781186548,0.707106781186547,0.707106781186547,0.707106781186547,
0.707106781186548,0.707106781186548,0.707106781186547,0.707106781186548,
0.707106781186548,0.707106781186547,0.707106781186548,0.707106781186547,
0.707106781186548,0.707106781186548,0.707106781186547,0.707106781186548,
0.707106781186548,0.707106781186548,0.707106781186547,0.707106781186547,
0.707106781186548,0.707106781186547,0.707106781186548,0.707106781186547,
0.707106781186547,0.707106781186548,0.707106781186548,0.707106781186548,
0.707106781186547,0.707106781186547,0.707106781186548,0.707106781186548,
0.707106781186547,0.707106781186547,0.707106781186548,0.707106781186547,
0.707106781186547,0.707106781186548,0.707106781186548,0.707106781186547,
0.707106781186547,0.707106781186547,0.707106781186548,0.707106781186547,
0.707106781186547,0.707106781186547,0.707106781186548,0.707106781186548,
0.707106781186547,0.707106781186548,0.707106781186547,0.707106781186548,
0.707106781186547,0.707106781186548,0.707106781186548,0.707106781186547,
0.707106781186547,0.707106781186548,0.707106781186547,0.707106781186547,
0.707106781186548,0.707106781186547,0.707106781186548,0.707106781186548,
0.707106781186547,0.707106781186548,0.707106781186547,0.707106781186547,
0.707106781186547,0.707106781186548,0.707106781186548,0.707106781186548,
0.707106781186547,0.707106781186548,0.707106781186547,0.707106781186548,
0.707106781186547,0.707106781186547,0.707106781186547,0.707106781186547,
0.707106781186548,0.707106781186548,0.707106781186547,0.707106781186547,
0.707106781186548,0.707106781186547,0.707106781186548,0.707106781186547,
0.707106781186548,0.707106781186547,0.707106781186547,0.707106781186548,
0.707106781186547,0.707106781186548,0.707106781186547,0.707106781186548,
0.707106781186548,0.707106781186547,0.707106781186548,0.707106781186547,
0.707106781186548,0.707106781186548,0.707106781186547,0.707106781186548,
0.707106781186547,0.707106781186547,0.707106781186548,0.707106781186547,
0.707106781186548,0.707106781186547,0.707106781186548,0.707106781186547,
0.707106781186547,0.707106781186548,0.707106781186548,0.707106781186548,
0.707106781186548,0.707106781186547,0.707106781186548,0.707106781186548,
0.707106781186548,0.707106781186547,0.707106781186548,0.707106781186548,
0.707106781186548,0.707106781186547,0.707106781186547,0.707106781186548,
0.707106781186547,0.707106781186548,0.707106781186547,0.707106781186548,
0.707106781186548,0.707106781186547,0.707106781186547,0.707106781186548,
0.707106781186547,0.707106781186548,0.707106781186547,0.707106781186548,
0.707106781186548,0.707106781186547,0.707106781186547,0.707106781186547,
0.707106781186548,0.707106781186548,0.707106781186547,0.707106781186547,
0.707106781186548,0.707106781186548,0.707106781186548,0.707106781186548,
0.707106781186547,0.707106781186547,0.707106781186548,0.707106781186548,
0.707106781186547,0.707106781186548,0.707106781186547,0.707106781186548,
0.707106781186547,0.707106781186548,0.707106781186547,0.707106781186547,
0.707106781186548,0.707106781186547,0.707106781186547,0.707106781186548,
0.707106781186547,0.707106781186548,0.707106781186547,0.707106781186548,
0.707106781186547,0.707106781186548,0.707106781186547,0.707106781186548,
0.707106781186547,0.707106781186548,0.707106781186547,0.707106781186547,
0.707106781186548,0.707106781186548,0.707106781186547,0.707106781186547,
0.707106781186547,0.707106781186548,0.707106781186547,0.707106781186548,
0.707106781186547,0.707106781186548,0.707106781186547,0.707106781186548,
0.707106781186547,0.707106781186547,0.707106781186547,0.707106781186548,
0.707106781186547,0.707106781186548,0.707106781186548,0.707106781186547,
0.707106781186548,0.707106781186547,0.707106781186547,0.707106781186548,
0.707106781186547,0.707106781186547,0.707106781186548,0.707106781186547,
0.707106781186547,0.707106781186547,0.707106781186547,0.707106781186548,
0.707106781186547,0.707106781186547,0.707106781186547,0.707106781186548,
0.707106781186547,0.707106781186547,0.707106781186548,0.707106781186548,
0.707106781186547,0.707106781186548,0.707106781186548,0.707106781186547,
0.707106781186547,0.707106781186548,0.707106781186547,0.707106781186547,
0.707106781186548,0.707106781186547,0.707106781186547,0.707106781186547,
0.707106781186548,0.707106781186547,0.707106781186548,0.707106781186547,
0.707106781186548,0.707106781186547,0.707106781186548,0.707106781186547,
0.707106781186548,0.707106781186547,0.707106781186548,0.707106781186548,
0.707106781186547,0.707106781186547,0.707106781186548,0.707106781186547,
0.707106781186548,0.707106781186547,0.707106781186548,0.707106781186548,
0.707106781186547,0.707106781186548,0.707106781186547,0.707106781186548,
0.707106781186548,0.707106781186547,0.707106781186547,0.707106781186548,
0.707106781186547,0.707106781186548,0.707106781186547,0.707106781186548,
0.707106781186547,0.707106781186548,0.707106781186547,0.707106781186547,
0.707106781186547,0.707106781186547,0.707106781186547,0.707106781186547,
0.707106781186547,0.707106781186547,0.707106781186548,0.707106781186547,
0.707106781186548,0.707106781186547,0.707106781186547,0.707106781186548,
0.707106781186547,0.707106781186548,0.707106781186547,0.707106781186547,
0.707106781186548,0.707106781186547,0.707106781186548,0.707106781186547,
0.707106781186548,0.707106781186547,0.707106781186548,0.707106781186547,
0.707106781186548,0.707106781186547,0.707106781186548,0.707106781186547,
0.707106781186548,0.707106781186548,0.707106781186547,0.707106781186548,
0.707106781186547,0.707106781186547,0.707106781186547,0.707106781186548,
0.707106781186547,0.707106781186547,0.707106781186547,0.707106781186548,
0.707106781186547,0.707106781186547,0.707106781186548,0.707106781186547,
0.707106781186547,0.707106781186547,0.707106781186547,0.707106781186548,
0.707106781186547,0.707106781186547,0.707106781186547,0.707106781186548,
0.707106781186548,0.707106781186548,0.707106781186548,0.707106781186547,
0.707106781186548,0.707106781186547,0.707106781186547,0.707106781186548,
0.707106781186547,0.707106781186548,0.707106781186547,0.707106781186547,
0.707106781186548,0.707106781186547,0.707106781186547,0.707106781186547,
0.707106781186547,0.707106781186548,0.707106781186548,0.707106781186547,
0.707106781186547,0.707106781186548,0.707106781186547,0.707106781186548,
0.707106781186547,0.707106781186548,0.707106781186548,0.707106781186547,
0.707106781186547,0.707106781186548,0.707106781186548,0.707106781186547,
0.707106781186548,0.707106781186548,0.707106781186547,0.707106781186548,
0.707106781186548,0.707106781186548,0.707106781186547,0.707106781186548,
0.707106781186547,0.707106781186548,0.707106781186547,0.707106781186548,
0.707106781186547,0.707106781186548,0.707106781186547,0.707106781186548,
0.707106781186548,0.707106781186547,0.707106781186547,0.707106781186548,
0.707106781186547,0.707106781186548,0.707106781186547,0.707106781186548,
0.707106781186548,0.707106781186548,0.707106781186548,0.707106781186548,
0.707106781186547,0.707106781186547,0.707106781186547,0.707106781186547,
0.707106781186548,0.707106781186547,0.707106781186548,0.707106781186547,
0.707106781186547,0.707106781186548,0.707106781186548,0.707106781186547,
0.707106781186548,0.707106781186547,0.707106781186548,0.707106781186548,
0.707106781186547,0.707106781186547,0.707106781186548,0.707106781186547,
0.707106781186548,0.707106781186547,0.707106781186548,0.707106781186547,
0.707106781186548,0.707106781186547,0.707106781186548,0.707106781186547,
0.707106781186548,0.707106781186547,0.707106781186548,0.707106781186548,
0.707106781186547,0.707106781186548,0.707106781186547,0.707106781186548,
0.707106781186547,0.707106781186548,0.707106781186548,0.707106781186548,
0.707106781186547,0.707106781186547,0.707106781186548,0.707106781186548,
0.707106781186547,0.707106781186547,0.707106781186547,0.707106781186548,
0.707106781186547,0.707106781186548,0.707106781186547,0.707106781186548,
0.707106781186547,0.707106781186547,0.707106781186547,0.707106781186548,
0.707106781186547,0.707106781186548,0.707106781186547,0.707106781186548,
0.707106781186547,0.707106781186548,0.707106781186547,0.707106781186547,
0.707106781186548,0.707106781186547,0.707106781186547,0.707106781186548,
0.707106781186547,0.707106781186547,0.707106781186548,0.707106781186547,
0.707106781186547,0.707106781186547,0.707106781186548,0.707106781186547,
0.707106781186548,0.707106781186547,0.707106781186547,0.707106781186547,
0.707106781186548,0.707106781186548,0.707106781186547,0.707106781186547,
0.707106781186548,0.707106781186548,0.707106781186548,0.707106781186547,
0.707106781186548,0.707106781186547,0.707106781186548,0.707106781186547,
0.707106781186548,0.707106781186547,0.707106781186547,0.707106781186547,
0.707106781186547,0.707106781186548,0.707106781186547,0.707106781186548,
0.707106781186548,0.707106781186547,0.707106781186548,0.707106781186547,
0.707106781186547,0.707106781186547,0.707106781186547,0.707106781186548,
0.707106781186547,0.707106781186548,0.707106781186547,0.707106781186548,
0.707106781186548,0.707106781186547,0.707106781186548,0.707106781186547,
0.707106781186547,0.707106781186547,0.707106781186547,0.707106781186548,
0.707106781186547,0.707106781186548,0.707106781186548,0.707106781186547,
0.707106781186548,0.707106781186547,0.707106781186548,0.707106781186547,
0.707106781186547,0.707106781186548,0.707106781186547,0.707106781186548,
0.707106781186548,0.707106781186547,0.707106781186547,0.707106781186548,
0.707106781186548,0.707106781186547,0.707106781186547,0.707106781186548,
0.707106781186547,0.707106781186547,0.707106781186548,0.707106781186547,
0.707106781186547,0.707106781186548,0.707106781186547,0.707106781186548,
0.707106781186547,0.707106781186547,0.707106781186548,0.707106781186547,
0.707106781186548,0.707106781186547,0.707106781186548,0.707106781186547,
0.707106781186547,0.707106781186547,0.707106781186548,0.707106781186547,
0.707106781186548,0.707106781186547,0.707106781186548,0.707106781186548,
0.707106781186548,0.707106781186548,0.707106781186547,0.707106781186547,
0.707106781186547,0.707106781186548,0.707106781186547,0.707106781186548,
0.707106781186547,0.707106781186547,0.707106781186548,0.707106781186547,
0.707106781186547,0.707106781186548,0.707106781186547,0.707106781186547,
0.707106781186548,0.707106781186548,0.707106781186547,0.707106781186548,
0.707106781186547,0.707106781186547,0.707106781186548,0.707106781186547,
0.707106781186548,0.707106781186547,0.707106781186548,0.707106781186547,
0.707106781186547,0.707106781186547,0.707106781186548,0.707106781186547,
0.707106781186548,0.707106781186547,0.707106781186548,0.707106781186547,
0.707106781186547,0.707106781186548,0.707106781186548,0.707106781186548,
0.707106781186547,0.707106781186548,0.707106781186547,0.707106781186548,
0.707106781186547,0.707106781186548,0.707106781186547,0.707106781186548,
0.707106781186548,0.707106781186547,0.707106781186547,0.707106781186547,
0.707106781186548,0.707106781186547,0.707106781186547,0.707106781186548,
0.707106781186547,0.707106781186547,0.707106781186548,0.707106781186547,
0.707106781186548,0.707106781186548,0.707106781186548,0.707106781186547,
0.707106781186548,0.707106781186547,0.707106781186548,0.707106781186547,
0.707106781186548,0.707106781186547,0.707106781186548,0.707106781186547,
0.707106781186548,0.707106781186547,0.707106781186548,0.707106781186548,
0.707106781186547,0.707106781186548,0.707106781186547,0.707106781186548,
0.707106781186548,0.707106781186547,0.707106781186547,0.707106781186548,
0.707106781186547,0.707106781186547,0.707106781186548,0.707106781186547,
0.707106781186548,0.707106781186548,0.707106781186547,0.707106781186548,
0.707106781186548,0.707106781186548,0.707106781186548,0.707106781186548,
0.707106781186547,0.707106781186548,0.707106781186548,0.707106781186548,
0.707106781186547,0.707106781186548,0.707106781186547,0.707106781186548,
0.707106781186547,0.707106781186548,0.707106781186547,0.707106781186548,
0.707106781186547,0.707106781186548,0.707106781186547,0.707106781186547,
0.707106781186548,0.707106781186547,0.707106781186547,0.707106781186548,
0.707106781186547,0.707106781186548,0.707106781186547,0.707106781186548,
0.707106781186547,0.707106781186548,0.707106781186547,0.707106781186547,
0.707106781186548,0.707106781186547,0.707106781186547,0.707106781186548,
0.707106781186547,0.707106781186548,0.707106781186547,0.707106781186547,
0.707106781186548,0.707106781186548,0.707106781186547,0.707106781186548,
0.707106781186547,0.707106781186547,0.707106781186547,0.707106781186548,
0.707106781186547,0.707106781186547,0.707106781186548,0.707106781186547,
0.707106781186547,0.707106781186547,0.707106781186548,0.707106781186548,
0.707106781186547,0.707106781186548,0.707106781186547,0.707106781186548,
0.707106781186547,0.707106781186547,0.707106781186548,0.707106781186547,
0.707106781186548,0.707106781186547,0.707106781186547,0.707106781186547,
0.707106781186547,0.707106781186548,0.707106781186547,0.707106781186547,
0.707106781186547,0.707106781186547,0.707106781186547,0.707106781186548,
0.707106781186547,0.707106781186547,0.707106781186547,0.707106781186547,
0.707106781186548,0.707106781186547,0.707106781186548,0.707106781186547,
0.707106781186547,0.707106781186548,0.707106781186547,0.707106781186548,
0.707106781186547,0.707106781186547,0.707106781186548,0.707106781186547,
0.707106781186547,0.707106781186548,0.707106781186547,0.707106781186547,
0.707106781186547,0.707106781186547,0.707106781186548,0.707106781186547,
0.707106781186548,0.707106781186548,0.707106781186547,0.707106781186548,
0.707106781186548,0.707106781186547,0.707106781186547,0.707106781186548,
0.707106781186547,0.707106781186547,0.707106781186547,0.707106781186548,
0.707106781186547,0.707106781186547,0.707106781186548,0.707106781186547,
0.707106781186548,0.707106781186547,0.707106781186548,0.707106781186547,
0.707106781186547,0.707106781186548,0.707106781186547,0.707106781186548,
0.707106781186547,0.707106781186548,0.707106781186547,0.707106781186548,
0.707106781186547,0.707106781186548,0.707106781186547,0.707106781186547,
0.707106781186547,0.707106781186547,0.707106781186548,0.707106781186548,
0.707106781186547,0.707106781186548,0.707106781186548,0.707106781186547,
0.707106781186548,0.707106781186547,0.707106781186547,0.707106781186548,
0.707106781186547,0.707106781186547,0.707106781186547,0.707106781186547,
0.707106781186548,0.707106781186547,0.707106781186547,0.707106781186547,
0.707106781186548,0.707106781186547,0.707106781186547,0.707106781186548,
0.707106781186547,0.707106781186548,0.707106781186548,0.707106781186547,
0.707106781186548,0.707106781186547,0.707106781186548,0.707106781186547,
0.707106781186548,0.707106781186547,0.707106781186547,0.707106781186548,
0.707106781186547,0.707106781186548,0.707106781186548,0.707106781186547,
0.707106781186547,0.707106781186548,0.707106781186547,0.707106781186548,
0.707106781186547,0.707106781186548,0.707106781186547,0.707106781186547,
0.707106781186548,0.707106781186548,0.707106781186547,0.707106781186548,
0.707106781186548,0.707106781186547,0.707106781186548,0.707106781186548,
0.707106781186547,0.707106781186548,0.707106781186547,0.707106781186548,
0.707106781186547,0.707106781186548,0.707106781186547,0.707106781186548,
0.707106781186547,0.707106781186547,0.707106781186548,0.707106781186547,
0.707106781186547,0.707106781186548,0.707106781186547,0.707106781186548,
0.707106781186548,0.707106781186547,0.707106781186547,0.707106781186547,
0.707106781186548,0.707106781186547,0.707106781186548,0.707106781186548,
0.707106781186547,0.707106781186548,0.707106781186547,0.707106781186548,
0.707106781186547,0.707106781186548,0.707106781186547,0.707106781186547,
0.707106781186548,0.707106781186548,0.707106781186548,0.707106781186547,
0.707106781186548,0.707106781186548,0.707106781186547,0.707106781186548,
0.707106781186547,0.707106781186548,0.707106781186548,0.707106781186548,
0.707106781186548,0.707106781186548,0.707106781186548,0.707106781186547,
0.707106781186547,0.707106781186548,0.707106781186547,0.707106781186547,
0.707106781186548,0.707106781186547,0.707106781186547,0.707106781186548,
0.707106781186547,0.707106781186548,0.707106781186547,0.707106781186548,
0.707106781186547,0.707106781186547,0.707106781186547,0.707106781186548,
0.707106781186547,0.707106781186547,0.707106781186548,0.707106781186547,
0.707106781186548,0.707106781186547,0.707106781186548,0.707106781186547,
0.707106781186547,0.707106781186547,0.707106781186547,0.707106781186548,
0.707106781186547,0.707106781186547,0.707106781186548,0.707106781186548,
0.707106781186547,0.707106781186548,0.707106781186547,0.707106781186548,
0.707106781186547,0.707106781186547,0.707106781186548,0.707106781186547,
0.707106781186548,0.707106781186547,0.707106781186548,0.707106781186547,
0.707106781186548,0.707106781186548,0.707106781186547,0.707106781186548,
0.707106781186547,0.707106781186547,0.707106781186548,0.707106781186547,
0.707106781186547,0.707106781186548,0.707106781186548,0.707106781186548,
0.707106781186547,0.707106781186548,0.707106781186547,0.707106781186547,
0.707106781186547,0.707106781186548,0.707106781186547,0.707106781186548,
0.707106781186548,0.707106781186548,0.707106781186547,0.707106781186547,
0.707106781186547,0.707106781186547,0.707106781186548,0.707106781186547,
0.707106781186547,0.707106781186548,0.707106781186547,0.707106781186548,
0.707106781186547,0.707106781186547,0.707106781186548,0.707106781186547,
0.707106781186548,0.707106781186547,0.707106781186548,0.707106781186547,
0.707106781186547,0.707106781186547,0.707106781186547,0.707106781186547,
0.707106781186547,0.707106781186548,0.707106781186547,0.707106781186547,
0.707106781186548,0.707106781186548,0.707106781186547,0.707106781186548,
0.707106781186548,0.707106781186547,0.707106781186547,0.707106781186548,
0.707106781186547,0.707106781186547,0.707106781186548,0.707106781186547,
0.707106781186548,0.707106781186548,0.707106781186548,0.707106781186547,
0.707106781186547,0.707106781186547,0.707106781186547,0.707106781186548,
0.707106781186548,0.707106781186548,0.707106781186547,0.707106781186548,
0.707106781186547,0.707106781186548,0.707106781186548,0.707106781186547,
0.707106781186548,0.707106781186547,0.707106781186548,0.707106781186548,
0.707106781186547,0.707106781186547,0.707106781186548,0.707106781186547,
0.707106781186548,0.707106781186547,0.707106781186548,0.707106781186548,
0.707106781186548,0.707106781186547,0.707106781186548,0.707106781186547,
0.707106781186547,0.707106781186547,0.707106781186547,0.707106781186548,
0.707106781186548,0.707106781186547,0.707106781186547,0.707106781186547,
0.707106781186548,0.707106781186547,0.707106781186547,0.707106781186548,
0.707106781186547,0.707106781186548,0.707106781186548,0.707106781186548,
0.707106781186547,0.707106781186547,0.707106781186547,0.707106781186547,
0.707106781186548,0.707106781186548,0.707106781186547,0.707106781186548,
0.707106781186547,0.707106781186548,0.707106781186548,0.707106781186547,
0.707106781186548,0.707106781186547,0.707106781186548,0.707106781186547,
0.707106781186547,0.707106781186547,0.707106781186548,0.707106781186547,
0.707106781186548,0.707106781186547,0.707106781186548,0.707106781186547,
0.707106781186548,0.707106781186547,0.707106781186548,0.707106781186547,
0.707106781186547,0.707106781186548,0.707106781186547,0.707106781186548,
0.707106781186547,0.707106781186547,0.707106781186548,0.707106781186548,
0.707106781186547,0.707106781186548,0.707106781186548,0.707106781186547,
0.707106781186548,0.707106781186547,0.707106781186548,0.707106781186547,
0.707106781186547,0.707106781186547,0.707106781186548,0.707106781186547,
0.707106781186547,0.707106781186548,0.707106781186547,0.707106781186548,
0.707106781186547,0.707106781186548,0.707106781186548,0.707106781186547,
0.707106781186548,0.707106781186547,0.707106781186548,0.707106781186548,
0.707106781186548,0.707106781186548,0.707106781186547,0.707106781186547,
0.707106781186548,0.707106781186547,0.707106781186547,0.707106781186548,
0.707106781186548,0.707106781186547,0.707106781186547,0.707106781186548,
0.707106781186547,0.707106781186547,0.707106781186548,0.707106781186547,
0.707106781186548,0.707106781186547,0.707106781186548,0.707106781186547,
0.707106781186547,0.707106781186547,0.707106781186548,0.707106781186547,
0.707106781186547,0.707106781186548,0.707106781186547,0.707106781186548,
0.707106781186548,0.707106781186548,0.707106781186547,0.707106781186547,
0.707106781186547,0.707106781186548,0.707106781186548,0.707106781186547,
0.707106781186547,0.707106781186547,0.707106781186547,0.707106781186548,
0.707106781186548,0.707106781186547,0.707106781186547,0.707106781186547,
0.707106781186548,0.707106781186548,0.707106781186547,0.707106781186548,
0.707106781186547,0.707106781186548,0.707106781186547,0.707106781186548,
0.707106781186548,0.707106781186547,0.707106781186548,0.707106781186548,
0.707106781186548,0.707106781186547,0.707106781186547,0.707106781186547,
0.707106781186548,0.707106781186548,0.707106781186548,0.707106781186547,
0.707106781186547,0.707106781186548,0.707106781186548,0.707106781186547,
0.707106781186548,0.707106781186547,0.707106781186547,0.707106781186548,
0.707106781186547,0.707106781186548,0.707106781186547,0.707106781186547,
0.707106781186548,0.707106781186547,0.707106781186548,0.707106781186548,
0.707106781186547,0.707106781186547,0.707106781186548,0.707106781186547,
0.707106781186548,0.707106781186547,0.707106781186547,0.707106781186548,
0.707106781186547,0.707106781186548,0.707106781186547,0.707106781186548,
0.707106781186547,0.707106781186547,0.707106781186548,0.707106781186547,
0.707106781186547,0.707106781186547,0.707106781186547,0.707106781186547,
0.707106781186547,0.707106781186548,0.707106781186547,0.707106781186548,
0.707106781186548,0.707106781186548,0.707106781186547,0.707106781186547,
0.707106781186547,0.707106781186548,0.707106781186547,0.707106781186548,
0.707106781186547,0.707106781186547,0.707106781186548,0.707106781186547,
0.707106781186547,0.707106781186547,0.707106781186547,0.707106781186547,
0.707106781186548,0.707106781186547,0.707106781186548,0.707106781186547,
0.707106781186547,0.707106781186548,0.707106781186548,0.707106781186547,
0.707106781186547,0.707106781186547,0.707106781186548,0.707106781186547,
0.707106781186547,0.707106781186548,0.707106781186548,0.707106781186547,
0.707106781186548,0.707106781186547,0.707106781186548,0.707106781186548,
0.707106781186547,0.707106781186547,0.707106781186547,0.707106781186548,
0.707106781186548,0.707106781186547,0.707106781186548,0.707106781186547,
0.707106781186548,0.707106781186548,0.707106781186547,0.707106781186548,
0.707106781186547,0.707106781186547,0.707106781186547,0.707106781186548,
0.707106781186547,0.707106781186548,0.707106781186547,0.707106781186548,
0.707106781186547,0.707106781186547,0.707106781186547,0.707106781186547,
0.707106781186547,0.707106781186548,0.707106781186547,0.707106781186548,
0.707106781186547,0.707106781186548,0.707106781186547,0.707106781186548,
0.707106781186547,0.707106781186547,0.707106781186547,0.707106781186547,
0.707106781186547,0.707106781186548,0.707106781186548,0.707106781186548,
0.707106781186547,0.707106781186548,0.707106781186547,0.707106781186548,
0.707106781186547,0.707106781186547,0.707106781186548,0.707106781186547,
0.707106781186548,0.707106781186547,0.707106781186547,0.707106781186547,
0.707106781186548,0.707106781186548,0.707106781186547,0.707106781186548,
0.707106781186547,0.707106781186548,0.707106781186548,0.707106781186547,
0.707106781186548,0.707106781186547,0.707106781186548,0.707106781186548,
0.707106781186547,0.707106781186547,0.707106781186547,0.707106781186547,
0.707106781186547,0.707106781186547,0.707106781186548,0.707106781186548,
0.707106781186547,0.707106781186548,0.707106781186547,0.707106781186547,
0.707106781186548,0.707106781186547,0.707106781186547,0.707106781186548,
0.707106781186547,0.707106781186547,0.707106781186547,0.707106781186548,
0.707106781186547,0.707106781186547,0.707106781186548,0.707106781186547,
0.707106781186548,0.707106781186548,0.707106781186547,0.707106781186547,
0.707106781186547,0.707106781186548,0.707106781186547,0.707106781186547,
0.707106781186548,0.707106781186548,0.707106781186548,0.707106781186548,
0.707106781186547,0.707106781186548,0.707106781186548,0.707106781186547,
0.707106781186547,0.707106781186548,0.707106781186547,0.707106781186548,
0.707106781186547,0.707106781186547,0.707106781186548,0.707106781186547,
0.707106781186547,0.707106781186548,0.707106781186547,0.707106781186548,
0.707106781186547,0.707106781186548,0.707106781186547,0.707106781186548,
0.707106781186547,0.707106781186548,0.707106781186547,0.707106781186548,
0.707106781186548,0.707106781186547,0.707106781186547,0.707106781186548,
0.707106781186548,0.707106781186547,0.707106781186547,0.707106781186547,
0.707106781186547,0.707106781186547,0.707106781186548,0.707106781186547,
0.707106781186547,0.707106781186548,0.707106781186547,0.707106781186548,
0.707106781186548,0.707106781186547,0.707106781186548,0.707106781186547,
0.707106781186548,0.707106781186547,0.707106781186548,0.707106781186547,
0.707106781186547,0.707106781186547,0.707106781186547,0.707106781186547,
0.707106781186547,0.707106781186548,0.707106781186547,0.707106781186548,
0.707106781186547,0.707106781186547,0.707106781186547,0.707106781186548,
0.707106781186547,0.707106781186548,0.707106781186548,0.707106781186547,
0.707106781186547,0.707106781186548,0.707106781186547,0.707106781186548,
0.707106781186547,0.707106781186548,0.707106781186547,0.707106781186548,
0.707106781186547,0.707106781186547,0.707106781186548,0.707106781186547,
0.707106781186548,0.707106781186547,0.707106781186548,0.707106781186548,
0.707106781186548,0.707106781186548,0.707106781186547,0.707106781186548,
0.707106781186548,0.707106781186548,0.707106781186547,0.707106781186548,
0.707106781186548,0.707106781186547,0.707106781186548,0.707106781186547,
0.707106781186548,0.707106781186547,0.707106781186547,0.707106781186547,
0.707106781186548,0.707106781186548,0.707106781186547,0.707106781186548,
0.707106781186547,0.707106781186548,0.707106781186547,0.707106781186548,
0.707106781186548,0.707106781186547,0.707106781186548,0.707106781186547,
0.707106781186547,0.707106781186548,0.707106781186547,0.707106781186547,
0.707106781186547,0.707106781186548,0.707106781186547,0.707106781186548,
0.707106781186548,0.707106781186547,0.707106781186548,0.707106781186547,
0.707106781186548,0.707106781186548,0.707106781186548,0.707106781186548,
0.707106781186547,0.707106781186548,0.707106781186547,0.707106781186548,
0.707106781186547,0.707106781186548,0.707106781186547,0.707106781186547,
0.707106781186547,0.707106781186547,0.707106781186548,0.707106781186547,
0.707106781186548,0.707106781186547,0.707106781186547,0.707106781186548,
0.707106781186547,0.707106781186548,0.707106781186547,0.707106781186548,
0.707106781186547,0.707106781186548,0.707106781186548,0.707106781186548,
0.707106781186548,0.707106781186547,0.707106781186548,0.707106781186548,
0.707106781186547,0.707106781186548,0.707106781186547,0.707106781186548,
0.707106781186547,0.707106781186548,0.707106781186547,0.707106781186547,
0.707106781186548,0.707106781186547,0.707106781186548,0.707106781186547,
0.707106781186547,0.707106781186548,0.707106781186547,0.707106781186548,
0.707106781186547,0.707106781186547,0.707106781186548,0.707106781186548,
0.707106781186548,0.707106781186548,0.707106781186548,0.707106781186548,
0.707106781186548,0.707106781186548,0.707106781186548,0.707106781186547,
0.707106781186548,0.707106781186547,0.707106781186547,0.707106781186548,
0.707106781186547,0.707106781186548,0.707106781186548,0.707106781186547,
0.707106781186547,0.707106781186548,0.707106781186548,0.707106781186547,
0.707106781186547,0.707106781186547,0.707106781186547,0.707106781186547,
0.707106781186548,0.707106781186547,0.707106781186548,0.707106781186548,
0.707106781186548,0.707106781186547,0.707106781186548,0.707106781186547,
0.707106781186548,0.707106781186547,0.707106781186548,0.707106781186547,
0.707106781186548,0.707106781186548,0.707106781186547,0.707106781186547,
0.707106781186548,0.707106781186548,0.707106781186548,0.707106781186547,
0.707106781186547,0.707106781186548,0.707106781186547,0.707106781186547,
0.707106781186548,0.707106781186547,0.707106781186548,0.707106781186547,
0.707106781186547,0.707106781186548,0.707106781186548,0.707106781186548,
0.707106781186547,0.707106781186547,0.707106781186548,0.707106781186547,
0.707106781186548,0.707106781186547,0.707106781186548,0.707106781186547,
0.707106781186548,0.707106781186548,0.707106781186547,0.707106781186548,
0.707106781186547,0.707106781186548,0.707106781186547,0.707106781186547,
0.707106781186547,0.707106781186548,0.707106781186547,0.707106781186548,
0.707106781186547,0.707106781186547,0.707106781186547,0.707106781186548,
0.707106781186547,0.707106781186547,0.707106781186548,0.707106781186548,
0.707106781186547,0.707106781186548,0.707106781186547,0.707106781186548,
0.707106781186548,0.707106781186547,0.707106781186548,0.707106781186547,
0.707106781186547,0.707106781186548,0.707106781186547,0.707106781186547,
0.707106781186547,0.707106781186548,0.707106781186547,0.707106781186548,
0.707106781186547,0.707106781186548,0.707106781186548,0.707106781186548,
0.707106781186547,0.707106781186548,0.707106781186548,0.707106781186548,
0.707106781186547,0.707106781186548,0.707106781186547,0.707106781186547,
0.707106781186548,0.707106781186547,0.707106781186547,0.707106781186548,
0.707106781186548,0.707106781186547,0.707106781186548,0.707106781186547,
0.707106781186548,0.707106781186548,0.707106781186547,0.707106781186548,
0.707106781186547,0.707106781186548,0.707106781186547,0.707106781186548,
0.707106781186547,0.707106781186548,0.707106781186548,0.707106781186548,
0.707106781186547,0.707106781186548,0.707106781186548,0.707106781186547,
0.707106781186547,0.707106781186548,0.707106781186547,0.707106781186548,
0.707106781186548,0.707106781186547,0.707106781186548,0.707106781186548,
0.707106781186547,0.707106781186548,0.707106781186548,0.707106781186547,
0.707106781186547,0.707106781186548,0.707106781186547,0.707106781186548,
0.707106781186547,0.707106781186548,0.707106781186547,0.707106781186548,
0.707106781186548,0.707106781186548,0.707106781186547,0.707106781186548,
0.707106781186547,0.707106781186548,0.707106781186547,0.707106781186548,
0.707106781186547,0.707106781186548,0.707106781186547,0.707106781186548,
0.707106781186547,0.707106781186548,0.707106781186547,0.707106781186547,
0.707106781186547,0.707106781186548,0.707106781186547,0.707106781186548,
0.707106781186547,0.707106781186548,0.707106781186547,0.707106781186548,
0.707106781186547,0.707106781186548,0.707106781186548,0.707106781186548,
0.707106781186547,0.707106781186548,0.707106781186547,0.707106781186548,
0.707106781186548,0.707106781186547,0.707106781186548,0.707106781186547,
0.707106781186548,0.707106781186547,0.707106781186548,0.707106781186547,
0.707106781186548,0.707106781186547,0.707106781186547,0.707106781186547,
0.707106781186548,0.707106781186547,0.707106781186547,0.707106781186548,
0.707106781186547,0.707106781186548,0.707106781186547,0.707106781186547,
0.707106781186548,0.707106781186547,0.707106781186548,0.707106781186547,
0.707106781186548,0.707106781186548,0.707106781186548,0.707106781186547,
0.707106781186547,0.707106781186548,0.707106781186548,0.707106781186547,
0.707106781186548,0.707106781186547,0.707106781186547,0.707106781186547,
0.707106781186548,0.707106781186547,0.707106781186548,0.707106781186547,
0.707106781186548,0.707106781186548,0.707106781186548,0.707106781186547,
0.707106781186547,0.707106781186547,0.707106781186547,0.707106781186547,
0.707106781186547,0.707106781186548,0.707106781186547,0.707106781186548,
0.707106781186547,0.707106781186548,0.707106781186547,0.707106781186547,
0.707106781186548,0.707106781186547,0.707106781186547,0.707106781186548,
0.707106781186548,0.707106781186547,0.707106781186547,0.707106781186547,
0.707106781186548,0.707106781186547,0.707106781186547,0.707106781186548,
0.707106781186548),(1.,1.,1.,1.,1.,1.,1.,1.,1.,1.,1.,1.,1.,1.,1.,1.,1.,
1.,1.,1.,1.,1.,1.,1.,1.,1.,1.,1.,1.,1.,1.,1.,1.,1.,1.,1.,1.,1.,1.,1.,1.,
1.,1.,1.,1.,1.,1.,1.,1.,1.,1.,1.,1.,1.,1.,1.,1.,1.,1.,1.,1.,1.,1.,1.,1.,
1.,1.,1.,1.,1.,1.,1.,1.,1.,1.,1.,1.,1.,1.,1.,1.,1.,1.,1.,1.,1.,1.,1.,1.,
1.,1.,1.,1.,1.,1.,1.,1.,1.,1.,1.,1.,1.,1.,1.,1.,1.,1.,1.,1.,1.,1.,1.,1.,
1.,1.,1.,1.,1.,1.,1.,1.,1.,1.,1.,1.,1.,1.,1.,1.,1.,1.,1.,1.,1.,1.,1.,1.,
1.,1.,1.,1.,1.,1.,1.,1.,1.,1.,1.,1.,1.,1.,1.,1.,1.,1.,1.,1.,1.,1.,1.,1.,
1.,1.,1.,1.,1.,1.,1.,1.,1.,1.,1.,1.,1.,1.,1.,1.,1.,1.,1.,1.,1.,1.,1.,1.,
1.,1.,1.,1.,1.,1.,1.,1.,1.,1.,1.,1.,1.,1.,1.,1.,1.,1.,1.,1.,1.,1.,1.,1.,
1.,1.,1.,1.,1.,1.,1.,1.,1.,1.,1.,1.,1.,1.,1.,1.,1.,1.,1.,1.,1.,1.,1.,1.,
1.,1.,1.,1.,1.,1.,1.,1.,1.,1.,1.,1.,1.,1.,1.,1.,1.,1.,1.,1.,1.,1.,1.,1.,
1.,1.,1.,1.,1.,1.,1.,1.,1.,1.,1.,1.,1.,1.,1.,1.,1.,1.,1.,1.,1.,1.,1.,1.,
1.,1.,1.,1.,1.,1.,1.,1.,1.,1.,1.,1.,1.,1.,1.,1.,1.,1.,1.,1.,1.,1.,1.,1.,
1.,1.,1.,1.,1.,1.,1.,1.,1.,1.,1.,1.,1.,1.,1.,1.,1.,1.,1.,1.,1.,1.,1.,1.,
1.,1.,1.,1.,1.,1.,1.,1.,1.,1.,1.,1.,1.,1.,1.,1.,1.,1.,1.,1.,1.,1.,1.,1.,
1.,1.,1.,1.,1.,1.,1.,1.,1.,1.,1.,1.,1.,1.,1.,1.,1.,1.,1.,1.,1.,1.,1.,1.,
1.,1.,1.,1.,1.,1.,1.,1.,1.,1.,1.,1.,1.,1.,1.,1.,1.,1.,1.,1.,1.,1.,1.,1.,
1.,1.,1.,1.,1.,1.,1.,1.,1.,1.,1.,1.,1.,1.,1.,1.,1.,1.,1.,1.,1.,1.,1.,1.,
1.,1.,1.,1.,1.,1.,1.,1.,1.,1.,1.,1.,1.,1.,1.,1.,1.,1.,1.,1.,1.,1.,1.,1.,
1.,1.,1.,1.,1.,1.,1.,1.,1.,1.,1.,1.,1.,1.,1.,1.,1.,1.,1.,1.,1.,1.,1.,1.,
1.,1.,1.,1.,1.,1.,1.,1.,1.,1.,1.,1.,1.,1.,1.,1.,1.,1.,1.,1.,1.,1.,1.,1.,
1.,1.,1.,1.,1.,1.,1.,1.,1.,1.,1.,1.,1.,1.,1.,1.,1.,1.,1.,1.,1.,1.,1.,1.,
1.,1.,1.,1.,1.,1.,1.,1.,1.,1.,1.,1.,1.,1.,1.,1.,1.,1.,1.,1.,1.,1.,1.,1.,
1.,1.,1.,1.,1.,1.,1.,1.,1.,1.,1.,1.,1.,1.,1.,1.,1.,1.,1.,1.,1.,1.,1.,1.,
1.,1.,1.,1.,1.,1.,1.,1.,1.,1.,1.,1.,1.,1.,1.,1.,1.,1.,1.,1.,1.,1.,1.,1.,
1.,1.,1.,1.,1.,1.,1.,1.,1.,1.,1.,1.,1.,1.,1.,1.,1.,1.,1.,1.,1.,1.,1.,1.,
1.,1.,1.,1.,1.,1.,1.,1.,1.,1.,1.,1.,1.,1.,1.,1.,1.,1.,1.,1.,1.,1.,1.,1.,
1.,1.,1.,1.,1.,1.,1.,1.,1.,1.,1.,1.,1.,1.,1.,1.,1.,1.,1.,1.,1.,1.,1.,1.,
1.,1.,1.,1.,1.,1.,1.,1.,1.,1.,1.,1.,1.,1.,1.,1.,1.,1.,1.,1.,1.,1.,1.,1.,
1.,1.,1.,1.,1.,1.,1.,1.,1.,1.,1.,1.,1.,1.,1.,1.,1.,1.,1.,1.,1.,1.,1.,1.,
1.,1.,1.,1.,1.,1.,1.,1.,1.,1.,1.,1.,1.,1.,1.,1.,1.,1.,1.,1.,1.,1.,1.,1.,
1.,1.,1.,1.,1.,1.,1.,1.,1.,1.,1.,1.,1.,1.,1.,1.,1.,1.,1.,1.,1.,1.,1.,1.,
1.,1.,1.,1.,1.,1.,1.,1.,1.,1.,1.,1.,1.,1.,1.,1.,1.,1.,1.,1.,1.,1.,1.,1.,
1.,1.,1.,1.,1.,1.,1.,1.,1.,1.,1.,1.,1.,1.,1.,1.,1.,1.,1.,1.,1.,1.,1.,1.,
1.,1.,1.,1.,1.,1.,1.,1.,1.,1.,1.,1.,1.,1.,1.,1.,1.,1.,1.,1.,1.,1.,1.,1.,
1.,1.,1.,1.,1.,1.,1.,1.,1.,1.,1.,1.,1.,1.,1.,1.,1.,1.,1.,1.,1.,1.,1.,1.,
1.,1.,1.,1.,1.,1.,1.,1.,1.,1.,1.,1.,1.,1.,1.,1.,1.,1.,1.,1.,1.,1.,1.,1.,
1.,1.,1.,1.,1.,1.,1.,1.,1.,1.,1.,1.,1.,1.,1.,1.,1.,1.,1.,1.,1.,1.,1.,1.,
1.,1.,1.,1.,1.,1.,1.,1.,1.,1.,1.,1.,1.,1.,1.,1.,1.,1.,1.,1.,1.,1.,1.,1.,
1.,1.,1.,1.,1.,1.,1.,1.,1.,1.,1.,1.,1.,1.,1.,1.,1.,1.,1.,1.,1.,1.,1.,1.,
1.,1.,1.,1.,1.,1.,1.,1.,1.,1.,1.,1.,1.,1.,1.,1.,1.,1.,1.,1.,1.,1.,1.,1.,
1.,1.,1.,1.,1.,1.,1.,1.,1.,1.,1.,1.,1.,1.,1.,1.,1.,1.,1.,1.,1.,1.,1.,1.,
1.,1.,1.,1.,1.,1.,1.,1.,1.,1.,1.,1.,1.,1.,1.,1.,1.,1.,1.,1.,1.,1.,1.,1.,
1.,1.,1.,1.,1.,1.,1.,1.,1.,1.,1.,1.,1.,1.,1.,1.,1.,1.,1.,1.,1.,1.,1.,1.,
1.,1.,1.,1.,1.,1.,1.,1.,1.,1.,1.,1.,1.,1.,1.,1.,1.,1.,1.,1.,1.,1.,1.,1.,
1.,1.,1.,1.,1.,1.,1.,1.,1.,1.,1.,1.,1.,1.,1.,1.,1.,1.,1.,1.,1.,1.,1.,1.,
1.,1.,1.,1.,1.,1.,1.,1.,1.,1.,1.,1.,1.,1.,1.,1.,1.,1.,1.,1.,1.,1.,1.,1.,
1.,1.,1.,1.,1.,1.,1.,1.,1.,1.,1.,1.,1.,1.,1.,1.,1.,1.,1.,1.,1.,1.,1.,1.,
1.,1.,1.,1.,1.,1.,1.,1.,1.,1.,1.,1.,1.,1.,1.,1.,1.,1.,1.,1.,1.,1.,1.,1.,
1.,1.,1.,1.,1.,1.,1.,1.,1.,1.,1.,1.,1.,1.,1.,1.,1.,1.,1.,1.,1.,1.,1.,1.,
1.,1.,1.,1.,1.,1.,1.,1.,1.,1.,1.,1.,1.,1.,1.,1.,1.,1.,1.,1.,1.,1.,1.,1.,
1.,1.,1.,1.,1.,1.,1.,1.,1.,1.,1.,1.,1.,1.,1.,1.,1.,1.,1.,1.,1.,1.,1.,1.,
1.,1.,1.,1.,1.,1.,1.,1.,1.,1.,1.,1.,1.,1.,1.,1.,1.,1.,1.,1.,1.,1.,1.,1.,
1.,1.,1.,1.,1.,1.,1.,1.,1.,1.,1.,1.,1.,1.,1.,1.,1.,1.,1.,1.,1.,1.,1.,1.,
1.,1.,1.,1.,1.,1.,1.,1.,1.,1.,1.,1.,1.,1.,1.,1.,1.,1.,1.,1.,1.,1.,1.,1.,
1.,1.,1.,1.,1.,1.,1.,1.,1.,1.,1.,1.,1.,1.,1.,1.,1.,1.,1.,1.,1.,1.,1.,1.,
1.,1.,1.,1.,1.,1.,1.,1.,1.,1.,1.,1.,1.,1.,1.,1.,1.,1.,1.,1.,1.,1.,1.,1.,
1.,1.,1.,1.,1.,1.,1.,1.,1.,1.,1.,1.,1.,1.,1.,1.,1.,1.,1.,1.,1.,1.,1.,1.,
1.,1.,1.,1.,1.,1.,1.,1.,1.,1.,1.,1.,1.,1.,1.,1.,1.,1.,1.,1.,1.,1.,1.,1.,
1.,1.,1.,1.,1.,1.,1.,1.,1.,1.,1.,1.,1.,1.,1.,1.,1.,1.,1.,1.,1.,1.,1.,1.,
1.,1.,1.,1.,1.,1.,1.,1.,1.,1.,1.,1.,1.,1.,1.,1.,1.,1.,1.,1.,1.,1.,1.,1.,
1.,1.,1.,1.,1.,1.,1.,1.,1.,1.,1.,1.,1.,1.,1.,1.,1.,1.,1.,1.,1.,1.,1.,1.,
1.,1.,1.,1.,1.,1.,1.,1.,1.,1.,1.,1.,1.,1.,1.,1.,1.,1.,1.,1.,1.,1.,1.,1.,
1.,1.,1.,1.,1.,1.,1.,1.,1.,1.,1.,1.,1.,1.,1.,1.,1.,1.,1.,1.,1.,1.,1.,1.,
1.,1.,1.,1.,1.,1.,1.,1.,1.,1.,1.,1.,1.,1.,1.,1.,1.,1.,1.,1.,1.,1.,1.,1.,
1.,1.,1.,1.,1.,1.,1.,1.,1.,1.,1.,1.,1.,1.,1.,1.,1.,1.,1.,1.,1.,1.,1.,1.,
1.,1.,1.,1.,1.,1.,1.,1.,1.,1.,1.,1.,1.,1.,1.,1.,1.,1.,1.,1.,1.,1.,1.,1.,
1.,1.,1.,1.,1.,1.,1.,1.,1.,1.,1.,1.,1.,1.,1.,1.,1.,1.,1.,1.,1.,1.,1.,1.,
1.,1.,1.,1.,1.,1.,1.,1.,1.,1.,1.,1.,1.,1.,1.,1.,1.,1.,1.,1.,1.,1.,1.,1.,
1.,1.,1.,1.,1.,1.,1.,1.,1.,1.,1.,1.,1.,1.,1.,1.,1.,1.,1.,1.,1.,1.,1.,1.,
1.,1.,1.,1.,1.,1.,1.,1.,1.,1.,1.,1.,1.,1.,1.,1.,1.,1.,1.,1.,1.,1.,1.,1.,
1.,1.,1.,1.,1.,1.,1.,1.,1.,1.,1.,1.,1.,1.,1.,1.,1.,1.,1.,1.,1.,1.,1.,1.,
1.,1.,1.,1.,1.,1.,1.,1.,1.,1.,1.,1.,1.,1.,1.,1.,1.,1.,1.,1.,1.,1.,1.,1.,
1.,1.,1.,1.,1.,1.,1.,1.,1.,1.,1.,1.,1.,1.,1.,1.,1.,1.,1.,1.,1.,1.,1.,1.,
1.,1.,1.,1.,1.,1.,1.,1.,1.,1.,1.,1.,1.,1.,1.,1.,1.,1.,1.,1.,1.,1.,1.,1.,
1.,1.,1.,1.,1.,1.,1.,1.,1.,1.,1.,1.,1.,1.,1.,1.,1.,1.,1.,1.,1.,1.,1.,1.,
1.,1.,1.,1.,1.,1.,1.,1.,1.,1.,1.,1.,1.,1.,1.,1.,1.,1.,1.,1.,1.,1.,1.,1.,
1.,1.,1.,1.,1.,1.,1.,1.,1.,1.,1.,1.,1.,1.,1.,1.,1.,1.,1.,1.,1.,1.,1.,1.,
1.,1.,1.,1.,1.,1.,1.,1.,1.,1.,1.,1.,1.,1.,1.,1.,1.,1.,1.,1.,1.,1.,1.,1.,
1.,1.,1.,1.,1.,1.,1.,1.,1.,1.,1.,1.,1.,1.,1.,1.,1.,1.,1.,1.,1.,1.,1.,1.,
1.,1.,1.,1.,1.,1.,1.,1.,1.,1.,1.,1.,1.,1.,1.,1.,1.,1.,1.,1.,1.,1.,1.,1.,
1.,1.,1.,1.,1.,1.,1.,1.,1.,1.,1.,1.,1.,1.,1.,1.,1.,1.,1.,1.,1.,1.,1.,1.,
1.,1.,1.,1.,1.,1.,1.,1.,1.,1.,1.,1.,1.,1.,1.,1.,1.,1.,1.,1.,1.,1.,1.,1.,
1.,1.,1.,1.,1.,1.,1.,1.,1.,1.,1.,1.,1.,1.,1.,1.,1.,1.,1.,1.,1.,1.,1.,1.,
1.,1.,1.,1.,1.,1.,1.,1.,1.,1.,1.,1.,1.,1.,1.,1.,1.,1.,1.,1.,1.,1.,1.,1.,
1.,1.,1.,1.,1.,1.,1.,1.,1.,1.,1.,1.,1.,1.,1.,1.,1.,1.)))
REPRESENTATION_ITEM('')
SURFACE()
) ;
#48 = (
BOUNDED_SURFACE()
B_SPLINE_SURFACE(3,2,((#154048,#154049,#154050,#154051,#154052,#154053,
#154054,#154055,#154056),(#154057,#154058,#154059,#154060,#154061,#154062,
#154063,#154064,#154065),(#154066,#154067,#154068,#154069,#154070,#154071,
#154072,#154073,#154074),(#154075,#154076,#154077,#154078,#154079,#154080,
#154081,#154082,#154083),(#154084,#154085,#154086,#154087,#154088,#154089,
#154090,#154091,#154092),(#154093,#154094,#154095,#154096,#154097,#154098,
#154099,#154100,#154101),(#154102,#154103,#154104,#154105,#154106,#154107,
#154108,#154109,#154110)),.UNSPECIFIED.,.F.,.T.,.F.)
B_SPLINE_SURFACE_WITH_KNOTS((4,1,1,1,4),(3,2,2,2,3),(0.,0.0911446219616379,
0.182289243923276,0.273433865884915,0.364578487846551),(0.,0.117809724509617,
0.235619449019234,0.353429173528852,0.471238898038469),.UNSPECIFIED.)
GEOMETRIC_REPRESENTATION_ITEM()
RATIONAL_B_SPLINE_SURFACE(((1.,0.707106781186548,1.,0.707106781186548,1.,
0.707106781186548,1.,0.707106781186548,1.),(1.,0.707106781186548,1.,0.707106781186548,
1.,0.707106781186548,1.,0.707106781186548,1.),(1.,0.707106781186547,1.,
0.707106781186547,1.,0.707106781186547,1.,0.707106781186547,1.),(1.,0.707106781186548,
1.,0.707106781186548,1.,0.707106781186548,1.,0.707106781186548,1.),(1.,
0.707106781186547,1.,0.707106781186547,1.,0.707106781186547,1.,0.707106781186547,
1.),(1.,0.707106781186548,1.,0.707106781186548,1.,0.707106781186548,1.,
0.707106781186548,1.),(1.,0.707106781186548,1.,0.707106781186548,1.,0.707106781186548,
1.,0.707106781186548,1.)))
REPRESENTATION_ITEM('')
SURFACE()
) ;
#49 = (
BOUNDED_SURFACE()
B_SPLINE_SURFACE(3,2,((#154120,#154121,#154122,#154123,#154124,#154125,
#154126,#154127,#154128),(#154129,#154130,#154131,#154132,#154133,#154134,
#154135,#154136,#154137),(#154138,#154139,#154140,#154141,#154142,#154143,
#154144,#154145,#154146),(#154147,#154148,#154149,#154150,#154151,#154152,
#154153,#154154,#154155)),.UNSPECIFIED.,.F.,.T.,.F.)
B_SPLINE_SURFACE_WITH_KNOTS((4,4),(3,2,2,2,3),(0.,1.1454147408364),(0.,
0.117809724509617,0.235619449019234,0.353429173528852,0.471238898038469),
 .UNSPECIFIED.)
GEOMETRIC_REPRESENTATION_ITEM()
RATIONAL_B_SPLINE_SURFACE(((1.,0.707106781186548,1.,0.707106781186548,1.,
0.707106781186548,1.,0.707106781186548,1.),(1.,0.707106781186548,1.,0.707106781186548,
1.,0.707106781186548,1.,0.707106781186548,1.),(1.,0.707106781186547,1.,
0.707106781186547,1.,0.707106781186547,1.,0.707106781186547,1.),(1.,0.707106781186548,
1.,0.707106781186548,1.,0.707106781186548,1.,0.707106781186548,1.)))
REPRESENTATION_ITEM('')
SURFACE()
) ;
#50 = (
BOUNDED_SURFACE()
B_SPLINE_SURFACE(3,2,((#154163,#154164,#154165,#154166,#154167,#154168,
#154169,#154170,#154171),(#154172,#154173,#154174,#154175,#154176,#154177,
#154178,#154179,#154180),(#154181,#154182,#154183,#154184,#154185,#154186,
#154187,#154188,#154189),(#154190,#154191,#154192,#154193,#154194,#154195,
#154196,#154197,#154198),(#154199,#154200,#154201,#154202,#154203,#154204,
#154205,#154206,#154207),(#154208,#154209,#154210,#154211,#154212,#154213,
#154214,#154215,#154216),(#154217,#154218,#154219,#154220,#154221,#154222,
#154223,#154224,#154225),(#154226,#154227,#154228,#154229,#154230,#154231,
#154232,#154233,#154234),(#154235,#154236,#154237,#154238,#154239,#154240,
#154241,#154242,#154243),(#154244,#154245,#154246,#154247,#154248,#154249,
#154250,#154251,#154252),(#154253,#154254,#154255,#154256,#154257,#154258,
#154259,#154260,#154261),(#154262,#154263,#154264,#154265,#154266,#154267,
#154268,#154269,#154270),(#154271,#154272,#154273,#154274,#154275,#154276,
#154277,#154278,#154279),(#154280,#154281,#154282,#154283,#154284,#154285,
#154286,#154287,#154288),(#154289,#154290,#154291,#154292,#154293,#154294,
#154295,#154296,#154297),(#154298,#154299,#154300,#154301,#154302,#154303,
#154304,#154305,#154306),(#154307,#154308,#154309,#154310,#154311,#154312,
#154313,#154314,#154315),(#154316,#154317,#154318,#154319,#154320,#154321,
#154322,#154323,#154324),(#154325,#154326,#154327,#154328,#154329,#154330,
#154331,#154332,#154333)),.UNSPECIFIED.,.F.,.T.,.F.)
B_SPLINE_SURFACE_WITH_KNOTS((4,1,1,1,1,1,1,1,1,1,1,1,1,1,1,1,4),(3,2,2,
2,3),(0.,0.226732296973331,0.464902013928651,0.70307173088397,0.9298040278573,
1.15653632483063,1.39470604178595,1.63287575874127,1.8596080557146,2.08634035268793,
2.32451006964325,2.56267978659857,2.7894120835719,3.01614438054523,3.25431409750055,
3.49248381445586,3.7192161114292),(0.,0.117809724509617,0.235619449019234,
0.353429173528852,0.471238898038469),.UNSPECIFIED.)
GEOMETRIC_REPRESENTATION_ITEM()
RATIONAL_B_SPLINE_SURFACE(((1.,0.707106781186548,1.,0.707106781186548,1.,
0.707106781186548,1.,0.707106781186548,1.),(1.,0.707106781186547,1.,0.707106781186547,
1.,0.707106781186547,1.,0.707106781186547,1.),(1.,0.707106781186548,1.,
0.707106781186548,1.,0.707106781186548,1.,0.707106781186548,1.),(1.,0.707106781186547,
1.,0.707106781186547,1.,0.707106781186547,1.,0.707106781186547,1.),(1.,
0.707106781186548,1.,0.707106781186548,1.,0.707106781186548,1.,0.707106781186548,
1.),(1.,0.707106781186547,1.,0.707106781186547,1.,0.707106781186547,1.,
0.707106781186547,1.),(1.,0.707106781186548,1.,0.707106781186548,1.,0.707106781186548,
1.,0.707106781186548,1.),(1.,0.707106781186547,1.,0.707106781186547,1.,
0.707106781186547,1.,0.707106781186547,1.),(1.,0.707106781186547,1.,0.707106781186547,
1.,0.707106781186547,1.,0.707106781186547,1.),(1.,0.707106781186547,1.,
0.707106781186547,1.,0.707106781186547,1.,0.707106781186547,1.),(1.,0.707106781186548,
1.,0.707106781186548,1.,0.707106781186548,1.,0.707106781186548,1.),(1.,
0.707106781186547,1.,0.707106781186547,1.,0.707106781186547,1.,0.707106781186547,
1.),(1.,0.707106781186547,1.,0.707106781186547,1.,0.707106781186547,1.,
0.707106781186547,1.),(1.,0.707106781186547,1.,0.707106781186547,1.,0.707106781186547,
1.,0.707106781186547,1.),(1.,0.707106781186547,1.,0.707106781186547,1.,
0.707106781186547,1.,0.707106781186547,1.),(1.,0.707106781186547,1.,0.707106781186547,
1.,0.707106781186547,1.,0.707106781186547,1.),(1.,0.707106781186548,1.,
0.707106781186548,1.,0.707106781186548,1.,0.707106781186548,1.),(1.,0.707106781186547,
1.,0.707106781186547,1.,0.707106781186547,1.,0.707106781186547,1.),(1.,
0.707106781186548,1.,0.707106781186548,1.,0.707106781186548,1.,0.707106781186548,
1.)))
REPRESENTATION_ITEM('')
SURFACE()
) ;
#51 = (
BOUNDED_SURFACE()
B_SPLINE_SURFACE(2,2,((#154360,#154361,#154362),(#154363,#154364,#154365),
(#154366,#154367,#154368),(#154369,#154370,#154371),(#154372,#154373,#154374),
(#154375,#154376,#154377),(#154378,#154379,#154380),(#154381,#154382,#154383),
(#154384,#154385,#154386)),.UNSPECIFIED.,.T.,.F.,.F.)
B_SPLINE_SURFACE_WITH_KNOTS((3,2,2,2,3),(3,3),(0.,1.5707963267949,3.1415926535898,
4.71238898038469,6.28318530717959),(0.,1.05013832301181),.UNSPECIFIED.)
GEOMETRIC_REPRESENTATION_ITEM()
RATIONAL_B_SPLINE_SURFACE(((1.,0.963886720506905,1.),(0.707106781186548,
0.681570836366095,0.707106781186548),(1.,0.963886720506905,1.),(0.707106781186548,
0.681570836366095,0.707106781186548),(1.,0.963886720506905,1.),(0.707106781186548,
0.681570836366095,0.707106781186548),(1.,0.963886720506905,1.),(0.707106781186548,
0.681570836366095,0.707106781186548),(1.,0.963886720506905,1.)))
REPRESENTATION_ITEM('')
SURFACE()
) ;
#52 = (
BOUNDED_SURFACE()
B_SPLINE_SURFACE(2,1,((#154391,#154392),(#154393,#154394),(#154395,#154396),
(#154397,#154398),(#154399,#154400),(#154401,#154402),(#154403,#154404),
(#154405,#154406),(#154407,#154408)),.UNSPECIFIED.,.T.,.F.,.F.)
B_SPLINE_SURFACE_WITH_KNOTS((3,2,2,2,3),(2,2),(0.,1.5707963267949,3.1415926535898,
4.71238898038469,6.28318530717959),(0.,0.0454859585810007),
 .UNSPECIFIED.)
GEOMETRIC_REPRESENTATION_ITEM()
RATIONAL_B_SPLINE_SURFACE(((1.,1.),(0.707106781186548,0.707106781186548),
(1.,1.),(0.707106781186548,0.707106781186548),(1.,1.),(0.707106781186548,
0.707106781186548),(1.,1.),(0.707106781186548,0.707106781186548),(1.,1.)))
REPRESENTATION_ITEM('')
SURFACE()
) ;
#53 = (
BOUNDED_SURFACE()
B_SPLINE_SURFACE(2,2,((#154412,#154413,#154414,#154415,#154416,#154417,
#154418,#154419,#154420),(#154421,#154422,#154423,#154424,#154425,#154426,
#154427,#154428,#154429),(#154430,#154431,#154432,#154433,#154434,#154435,
#154436,#154437,#154438),(#154439,#154440,#154441,#154442,#154443,#154444,
#154445,#154446,#154447),(#154448,#154449,#154450,#154451,#154452,#154453,
#154454,#154455,#154456),(#154457,#154458,#154459,#154460,#154461,#154462,
#154463,#154464,#154465),(#154466,#154467,#154468,#154469,#154470,#154471,
#154472,#154473,#154474),(#154475,#154476,#154477,#154478,#154479,#154480,
#154481,#154482,#154483),(#154484,#154485,#154486,#154487,#154488,#154489,
#154490,#154491,#154492)),.UNSPECIFIED.,.T.,.F.,.F.)
B_SPLINE_SURFACE_WITH_KNOTS((3,2,2,2,3),(3,2,2,2,3),(0.,1.5707963267949,
3.1415926535898,4.71238898038469,6.28318530717959),(1.42918797785348,1.62618617063892,
1.86180561965816,2.09742506867739,2.29442326146283),.UNSPECIFIED.)
GEOMETRIC_REPRESENTATION_ITEM()
RATIONAL_B_SPLINE_SURFACE(((1.,1.,1.,0.707106781186548,1.,0.707106781186548,
1.,1.,1.),(0.707106781186548,0.707106781186548,0.707106781186548,0.5,0.707106781186548,
0.5,0.707106781186548,0.707106781186548,0.707106781186548),(1.,1.,1.,0.707106781186548,
1.,0.707106781186548,1.,1.,1.),(0.707106781186548,0.707106781186548,0.707106781186548,
0.5,0.707106781186548,0.5,0.707106781186548,0.707106781186548,0.707106781186548),
(1.,1.,1.,0.707106781186548,1.,0.707106781186548,1.,1.,1.),(0.707106781186548,
0.707106781186548,0.707106781186548,0.5,0.707106781186548,0.5,0.707106781186548,
0.707106781186548,0.707106781186548),(1.,1.,1.,0.707106781186548,1.,0.707106781186548,
1.,1.,1.),(0.707106781186548,0.707106781186548,0.707106781186548,0.5,0.707106781186548,
0.5,0.707106781186548,0.707106781186548,0.707106781186548),(1.,1.,1.,0.707106781186548,
1.,0.707106781186548,1.,1.,1.)))
REPRESENTATION_ITEM('')
SURFACE()
) ;
#54 = (
BOUNDED_SURFACE()
B_SPLINE_SURFACE(2,1,((#154504,#154505),(#154506,#154507),(#154508,#154509),
(#154510,#154511),(#154512,#154513),(#154514,#154515),(#154516,#154517),
(#154518,#154519),(#154520,#154521)),.UNSPECIFIED.,.T.,.F.,.F.)
B_SPLINE_SURFACE_WITH_KNOTS((3,2,2,2,3),(2,2),(0.,1.5707963267949,3.1415926535898,
4.71238898038469,6.28318530717959),(0.,1.586514041419),.UNSPECIFIED.)
GEOMETRIC_REPRESENTATION_ITEM()
RATIONAL_B_SPLINE_SURFACE(((1.,1.),(0.707106781186548,0.707106781186548),
(1.,1.),(0.707106781186548,0.707106781186548),(1.,1.),(0.707106781186548,
0.707106781186548),(1.,1.),(0.707106781186548,0.707106781186548),(1.,1.)))
REPRESENTATION_ITEM('')
SURFACE()
) ;
#55 = (
BOUNDED_SURFACE()
B_SPLINE_SURFACE(2,1,((#154525,#154526),(#154527,#154528),(#154529,#154530),
(#154531,#154532),(#154533,#154534),(#154535,#154536),(#154537,#154538),
(#154539,#154540),(#154541,#154542)),.UNSPECIFIED.,.T.,.F.,.F.)
B_SPLINE_SURFACE_WITH_KNOTS((3,2,2,2,3),(2,2),(0.,1.5707963267949,3.1415926535898,
4.71238898038469,6.28318530717959),(15.5153736066212,15.6567949628585),
 .UNSPECIFIED.)
GEOMETRIC_REPRESENTATION_ITEM()
RATIONAL_B_SPLINE_SURFACE(((1.,1.),(0.707106781186548,0.707106781186548),
(1.,1.),(0.707106781186548,0.707106781186548),(1.,1.),(0.707106781186548,
0.707106781186548),(1.,1.),(0.707106781186548,0.707106781186548),(1.,1.)))
REPRESENTATION_ITEM('')
SURFACE()
) ;
#56 = (
BOUNDED_SURFACE()
B_SPLINE_SURFACE(2,2,((#154549,#154550,#154551,#154552,#154553,#154554,
#154555,#154556,#154557),(#154558,#154559,#154560,#154561,#154562,#154563,
#154564,#154565,#154566),(#154567,#154568,#154569,#154570,#154571,#154572,
#154573,#154574,#154575)),.UNSPECIFIED.,.F.,.T.,.F.)
B_SPLINE_SURFACE_WITH_KNOTS((3,3),(3,2,2,2,3),(0.,1.05013832301181),(0.,
1.5707963267949,3.1415926535898,4.71238898038469,6.28318530717959),
 .UNSPECIFIED.)
GEOMETRIC_REPRESENTATION_ITEM()
RATIONAL_B_SPLINE_SURFACE(((1.,0.707106781186548,1.,0.707106781186548,1.,
0.707106781186548,1.,0.707106781186548,1.),(0.963886720506905,0.681570836366095,
0.963886720506905,0.681570836366095,0.963886720506905,0.681570836366095,
0.963886720506905,0.681570836366095,0.963886720506905),(1.,0.707106781186548,
1.,0.707106781186548,1.,0.707106781186548,1.,0.707106781186548,1.)))
REPRESENTATION_ITEM('')
SURFACE()
) ;
#57 = (
BOUNDED_SURFACE()
B_SPLINE_SURFACE(2,1,((#154580,#154581),(#154582,#154583),(#154584,#154585),
(#154586,#154587),(#154588,#154589),(#154590,#154591),(#154592,#154593),
(#154594,#154595),(#154596,#154597)),.UNSPECIFIED.,.T.,.F.,.F.)
B_SPLINE_SURFACE_WITH_KNOTS((3,2,2,2,3),(2,2),(0.,1.5707963267949,3.1415926535898,
4.71238898038469,6.28318530717959),(0.,0.0454859585810007),
 .UNSPECIFIED.)
GEOMETRIC_REPRESENTATION_ITEM()
RATIONAL_B_SPLINE_SURFACE(((1.,1.),(0.707106781186548,0.707106781186548),
(1.,1.),(0.707106781186548,0.707106781186548),(1.,1.),(0.707106781186548,
0.707106781186548),(1.,1.),(0.707106781186548,0.707106781186548),(1.,1.)))
REPRESENTATION_ITEM('')
SURFACE()
) ;
#58 = (
BOUNDED_SURFACE()
B_SPLINE_SURFACE(2,2,((#154601,#154602,#154603,#154604,#154605,#154606,
#154607,#154608,#154609),(#154610,#154611,#154612,#154613,#154614,#154615,
#154616,#154617,#154618),(#154619,#154620,#154621,#154622,#154623,#154624,
#154625,#154626,#154627),(#154628,#154629,#154630,#154631,#154632,#154633,
#154634,#154635,#154636),(#154637,#154638,#154639,#154640,#154641,#154642,
#154643,#154644,#154645),(#154646,#154647,#154648,#154649,#154650,#154651,
#154652,#154653,#154654),(#154655,#154656,#154657,#154658,#154659,#154660,
#154661,#154662,#154663),(#154664,#154665,#154666,#154667,#154668,#154669,
#154670,#154671,#154672),(#154673,#154674,#154675,#154676,#154677,#154678,
#154679,#154680,#154681)),.UNSPECIFIED.,.F.,.T.,.F.)
B_SPLINE_SURFACE_WITH_KNOTS((3,2,2,2,3),(3,2,2,2,3),(1.42918797785348,1.62618617063892,
1.86180561965816,2.09742506867739,2.29442326146283),(0.,1.5707963267949,
3.1415926535898,4.71238898038469,6.28318530717959),.UNSPECIFIED.)
GEOMETRIC_REPRESENTATION_ITEM()
RATIONAL_B_SPLINE_SURFACE(((1.,0.707106781186548,1.,0.707106781186548,1.,
0.707106781186548,1.,0.707106781186548,1.),(1.,0.707106781186548,1.,0.707106781186548,
1.,0.707106781186548,1.,0.707106781186548,1.),(1.,0.707106781186548,1.,
0.707106781186548,1.,0.707106781186548,1.,0.707106781186548,1.),(0.707106781186548,
0.5,0.707106781186548,0.5,0.707106781186548,0.5,0.707106781186548,0.5,0.707106781186548),
(1.,0.707106781186548,1.,0.707106781186548,1.,0.707106781186548,1.,0.707106781186548,
1.),(0.707106781186548,0.5,0.707106781186548,0.5,0.707106781186548,0.5,
0.707106781186548,0.5,0.707106781186548),(1.,0.707106781186548,1.,0.707106781186548,
1.,0.707106781186548,1.,0.707106781186548,1.),(1.,0.707106781186548,1.,
0.707106781186548,1.,0.707106781186548,1.,0.707106781186548,1.),(1.,0.707106781186548,
1.,0.707106781186548,1.,0.707106781186548,1.,0.707106781186548,1.)))
REPRESENTATION_ITEM('')
SURFACE()
) ;
#59 = (
BOUNDED_SURFACE()
B_SPLINE_SURFACE(2,1,((#154693,#154694),(#154695,#154696),(#154697,#154698),
(#154699,#154700),(#154701,#154702),(#154703,#154704),(#154705,#154706),
(#154707,#154708),(#154709,#154710)),.UNSPECIFIED.,.T.,.F.,.F.)
B_SPLINE_SURFACE_WITH_KNOTS((3,2,2,2,3),(2,2),(0.,1.5707963267949,3.1415926535898,
4.71238898038469,6.28318530717959),(0.,1.586514041419),.UNSPECIFIED.)
GEOMETRIC_REPRESENTATION_ITEM()
RATIONAL_B_SPLINE_SURFACE(((1.,1.),(0.707106781186548,0.707106781186548),
(1.,1.),(0.707106781186548,0.707106781186548),(1.,1.),(0.707106781186548,
0.707106781186548),(1.,1.),(0.707106781186548,0.707106781186548),(1.,1.)))
REPRESENTATION_ITEM('')
SURFACE()
) ;
#60 = (
BOUNDED_SURFACE()
B_SPLINE_SURFACE(1,2,((#154714,#154715,#154716,#154717,#154718,#154719,
#154720,#154721,#154722),(#154723,#154724,#154725,#154726,#154727,#154728,
#154729,#154730,#154731)),.UNSPECIFIED.,.F.,.T.,.F.)
B_SPLINE_SURFACE_WITH_KNOTS((2,2),(3,2,2,2,3),(15.5153736066212,15.6567949628585),
(0.,1.5707963267949,3.1415926535898,4.71238898038469,6.28318530717959),
 .UNSPECIFIED.)
GEOMETRIC_REPRESENTATION_ITEM()
RATIONAL_B_SPLINE_SURFACE(((1.,0.707106781186548,1.,0.707106781186548,1.,
0.707106781186548,1.,0.707106781186548,1.),(1.,0.707106781186548,1.,0.707106781186548,
1.,0.707106781186548,1.,0.707106781186548,1.)))
REPRESENTATION_ITEM('')
SURFACE()
) ;
#61 = (
BOUNDED_SURFACE()
B_SPLINE_SURFACE(3,2,((#154736,#154737,#154738,#154739,#154740,#154741,
#154742,#154743,#154744),(#154745,#154746,#154747,#154748,#154749,#154750,
#154751,#154752,#154753),(#154754,#154755,#154756,#154757,#154758,#154759,
#154760,#154761,#154762),(#154763,#154764,#154765,#154766,#154767,#154768,
#154769,#154770,#154771),(#154772,#154773,#154774,#154775,#154776,#154777,
#154778,#154779,#154780),(#154781,#154782,#154783,#154784,#154785,#154786,
#154787,#154788,#154789),(#154790,#154791,#154792,#154793,#154794,#154795,
#154796,#154797,#154798),(#154799,#154800,#154801,#154802,#154803,#154804,
#154805,#154806,#154807),(#154808,#154809,#154810,#154811,#154812,#154813,
#154814,#154815,#154816),(#154817,#154818,#154819,#154820,#154821,#154822,
#154823,#154824,#154825),(#154826,#154827,#154828,#154829,#154830,#154831,
#154832,#154833,#154834),(#154835,#154836,#154837,#154838,#154839,#154840,
#154841,#154842,#154843),(#154844,#154845,#154846,#154847,#154848,#154849,
#154850,#154851,#154852),(#154853,#154854,#154855,#154856,#154857,#154858,
#154859,#154860,#154861),(#154862,#154863,#154864,#154865,#154866,#154867,
#154868,#154869,#154870),(#154871,#154872,#154873,#154874,#154875,#154876,
#154877,#154878,#154879),(#154880,#154881,#154882,#154883,#154884,#154885,
#154886,#154887,#154888),(#154889,#154890,#154891,#154892,#154893,#154894,
#154895,#154896,#154897),(#154898,#154899,#154900,#154901,#154902,#154903,
#154904,#154905,#154906),(#154907,#154908,#154909,#154910,#154911,#154912,
#154913,#154914,#154915),(#154916,#154917,#154918,#154919,#154920,#154921,
#154922,#154923,#154924),(#154925,#154926,#154927,#154928,#154929,#154930,
#154931,#154932,#154933),(#154934,#154935,#154936,#154937,#154938,#154939,
#154940,#154941,#154942),(#154943,#154944,#154945,#154946,#154947,#154948,
#154949,#154950,#154951),(#154952,#154953,#154954,#154955,#154956,#154957,
#154958,#154959,#154960),(#154961,#154962,#154963,#154964,#154965,#154966,
#154967,#154968,#154969),(#154970,#154971,#154972,#154973,#154974,#154975,
#154976,#154977,#154978),(#154979,#154980,#154981,#154982,#154983,#154984,
#154985,#154986,#154987),(#154988,#154989,#154990,#154991,#154992,#154993,
#154994,#154995,#154996),(#154997,#154998,#154999,#155000,#155001,#155002,
#155003,#155004,#155005),(#155006,#155007,#155008,#155009,#155010,#155011,
#155012,#155013,#155014),(#155015,#155016,#155017,#155018,#155019,#155020,
#155021,#155022,#155023),(#155024,#155025,#155026,#155027,#155028,#155029,
#155030,#155031,#155032),(#155033,#155034,#155035,#155036,#155037,#155038,
#155039,#155040,#155041),(#155042,#155043,#155044,#155045,#155046,#155047,
#155048,#155049,#155050),(#155051,#155052,#155053,#155054,#155055,#155056,
#155057,#155058,#155059),(#155060,#155061,#155062,#155063,#155064,#155065,
#155066,#155067,#155068),(#155069,#155070,#155071,#155072,#155073,#155074,
#155075,#155076,#155077),(#155078,#155079,#155080,#155081,#155082,#155083,
#155084,#155085,#155086),(#155087,#155088,#155089,#155090,#155091,#155092,
#155093,#155094,#155095),(#155096,#155097,#155098,#155099,#155100,#155101,
#155102,#155103,#155104),(#155105,#155106,#155107,#155108,#155109,#155110,
#155111,#155112,#155113),(#155114,#155115,#155116,#155117,#155118,#155119,
#155120,#155121,#155122),(#155123,#155124,#155125,#155126,#155127,#155128,
#155129,#155130,#155131),(#155132,#155133,#155134,#155135,#155136,#155137,
#155138,#155139,#155140),(#155141,#155142,#155143,#155144,#155145,#155146,
#155147,#155148,#155149),(#155150,#155151,#155152,#155153,#155154,#155155,
#155156,#155157,#155158),(#155159,#155160,#155161,#155162,#155163,#155164,
#155165,#155166,#155167),(#155168,#155169,#155170,#155171,#155172,#155173,
#155174,#155175,#155176),(#155177,#155178,#155179,#155180,#155181,#155182,
#155183,#155184,#155185),(#155186,#155187,#155188,#155189,#155190,#155191,
#155192,#155193,#155194),(#155195,#155196,#155197,#155198,#155199,#155200,
#155201,#155202,#155203),(#155204,#155205,#155206,#155207,#155208,#155209,
#155210,#155211,#155212),(#155213,#155214,#155215,#155216,#155217,#155218,
#155219,#155220,#155221),(#155222,#155223,#155224,#155225,#155226,#155227,
#155228,#155229,#155230),(#155231,#155232,#155233,#155234,#155235,#155236,
#155237,#155238,#155239),(#155240,#155241,#155242,#155243,#155244,#155245,
#155246,#155247,#155248),(#155249,#155250,#155251,#155252,#155253,#155254,
#155255,#155256,#155257),(#155258,#155259,#155260,#155261,#155262,#155263,
#155264,#155265,#155266),(#155267,#155268,#155269,#155270,#155271,#155272,
#155273,#155274,#155275),(#155276,#155277,#155278,#155279,#155280,#155281,
#155282,#155283,#155284),(#155285,#155286,#155287,#155288,#155289,#155290,
#155291,#155292,#155293),(#155294,#155295,#155296,#155297,#155298,#155299,
#155300,#155301,#155302),(#155303,#155304,#155305,#155306,#155307,#155308,
#155309,#155310,#155311),(#155312,#155313,#155314,#155315,#155316,#155317,
#155318,#155319,#155320),(#155321,#155322,#155323,#155324,#155325,#155326,
#155327,#155328,#155329),(#155330,#155331,#155332,#155333,#155334,#155335,
#155336,#155337,#155338),(#155339,#155340,#155341,#155342,#155343,#155344,
#155345,#155346,#155347),(#155348,#155349,#155350,#155351,#155352,#155353,
#155354,#155355,#155356),(#155357,#155358,#155359,#155360,#155361,#155362,
#155363,#155364,#155365),(#155366,#155367,#155368,#155369,#155370,#155371,
#155372,#155373,#155374),(#155375,#155376,#155377,#155378,#155379,#155380,
#155381,#155382,#155383),(#155384,#155385,#155386,#155387,#155388,#155389,
#155390,#155391,#155392),(#155393,#155394,#155395,#155396,#155397,#155398,
#155399,#155400,#155401),(#155402,#155403,#155404,#155405,#155406,#155407,
#155408,#155409,#155410),(#155411,#155412,#155413,#155414,#155415,#155416,
#155417,#155418,#155419),(#155420,#155421,#155422,#155423,#155424,#155425,
#155426,#155427,#155428),(#155429,#155430,#155431,#155432,#155433,#155434,
#155435,#155436,#155437),(#155438,#155439,#155440,#155441,#155442,#155443,
#155444,#155445,#155446),(#155447,#155448,#155449,#155450,#155451,#155452,
#155453,#155454,#155455),(#155456,#155457,#155458,#155459,#155460,#155461,
#155462,#155463,#155464),(#155465,#155466,#155467,#155468,#155469,#155470,
#155471,#155472,#155473),(#155474,#155475,#155476,#155477,#155478,#155479,
#155480,#155481,#155482),(#155483,#155484,#155485,#155486,#155487,#155488,
#155489,#155490,#155491),(#155492,#155493,#155494,#155495,#155496,#155497,
#155498,#155499,#155500),(#155501,#155502,#155503,#155504,#155505,#155506,
#155507,#155508,#155509),(#155510,#155511,#155512,#155513,#155514,#155515,
#155516,#155517,#155518),(#155519,#155520,#155521,#155522,#155523,#155524,
#155525,#155526,#155527),(#155528,#155529,#155530,#155531,#155532,#155533,
#155534,#155535,#155536),(#155537,#155538,#155539,#155540,#155541,#155542,
#155543,#155544,#155545),(#155546,#155547,#155548,#155549,#155550,#155551,
#155552,#155553,#155554),(#155555,#155556,#155557,#155558,#155559,#155560,
#155561,#155562,#155563),(#155564,#155565,#155566,#155567,#155568,#155569,
#155570,#155571,#155572),(#155573,#155574,#155575,#155576,#155577,#155578,
#155579,#155580,#155581),(#155582,#155583,#155584,#155585,#155586,#155587,
#155588,#155589,#155590),(#155591,#155592,#155593,#155594,#155595,#155596,
#155597,#155598,#155599),(#155600,#155601,#155602,#155603,#155604,#155605,
#155606,#155607,#155608),(#155609,#155610,#155611,#155612,#155613,#155614,
#155615,#155616,#155617),(#155618,#155619,#155620,#155621,#155622,#155623,
#155624,#155625,#155626),(#155627,#155628,#155629,#155630,#155631,#155632,
#155633,#155634,#155635),(#155636,#155637,#155638,#155639,#155640,#155641,
#155642,#155643,#155644),(#155645,#155646,#155647,#155648,#155649,#155650,
#155651,#155652,#155653),(#155654,#155655,#155656,#155657,#155658,#155659,
#155660,#155661,#155662),(#155663,#155664,#155665,#155666,#155667,#155668,
#155669,#155670,#155671),(#155672,#155673,#155674,#155675,#155676,#155677,
#155678,#155679,#155680),(#155681,#155682,#155683,#155684,#155685,#155686,
#155687,#155688,#155689),(#155690,#155691,#155692,#155693,#155694,#155695,
#155696,#155697,#155698),(#155699,#155700,#155701,#155702,#155703,#155704,
#155705,#155706,#155707),(#155708,#155709,#155710,#155711,#155712,#155713,
#155714,#155715,#155716),(#155717,#155718,#155719,#155720,#155721,#155722,
#155723,#155724,#155725),(#155726,#155727,#155728,#155729,#155730,#155731,
#155732,#155733,#155734),(#155735,#155736,#155737,#155738,#155739,#155740,
#155741,#155742,#155743),(#155744,#155745,#155746,#155747,#155748,#155749,
#155750,#155751,#155752),(#155753,#155754,#155755,#155756,#155757,#155758,
#155759,#155760,#155761),(#155762,#155763,#155764,#155765,#155766,#155767,
#155768,#155769,#155770),(#155771,#155772,#155773,#155774,#155775,#155776,
#155777,#155778,#155779),(#155780,#155781,#155782,#155783,#155784,#155785,
#155786,#155787,#155788),(#155789,#155790,#155791,#155792,#155793,#155794,
#155795,#155796,#155797),(#155798,#155799,#155800,#155801,#155802,#155803,
#155804,#155805,#155806),(#155807,#155808,#155809,#155810,#155811,#155812,
#155813,#155814,#155815),(#155816,#155817,#155818,#155819,#155820,#155821,
#155822,#155823,#155824),(#155825,#155826,#155827,#155828,#155829,#155830,
#155831,#155832,#155833),(#155834,#155835,#155836,#155837,#155838,#155839,
#155840,#155841,#155842),(#155843,#155844,#155845,#155846,#155847,#155848,
#155849,#155850,#155851),(#155852,#155853,#155854,#155855,#155856,#155857,
#155858,#155859,#155860),(#155861,#155862,#155863,#155864,#155865,#155866,
#155867,#155868,#155869),(#155870,#155871,#155872,#155873,#155874,#155875,
#155876,#155877,#155878),(#155879,#155880,#155881,#155882,#155883,#155884,
#155885,#155886,#155887),(#155888,#155889,#155890,#155891,#155892,#155893,
#155894,#155895,#155896),(#155897,#155898,#155899,#155900,#155901,#155902,
#155903,#155904,#155905),(#155906,#155907,#155908,#155909,#155910,#155911,
#155912,#155913,#155914),(#155915,#155916,#155917,#155918,#155919,#155920,
#155921,#155922,#155923),(#155924,#155925,#155926,#155927,#155928,#155929,
#155930,#155931,#155932),(#155933,#155934,#155935,#155936,#155937,#155938,
#155939,#155940,#155941),(#155942,#155943,#155944,#155945,#155946,#155947,
#155948,#155949,#155950),(#155951,#155952,#155953,#155954,#155955,#155956,
#155957,#155958,#155959),(#155960,#155961,#155962,#155963,#155964,#155965,
#155966,#155967,#155968),(#155969,#155970,#155971,#155972,#155973,#155974,
#155975,#155976,#155977),(#155978,#155979,#155980,#155981,#155982,#155983,
#155984,#155985,#155986),(#155987,#155988,#155989,#155990,#155991,#155992,
#155993,#155994,#155995),(#155996,#155997,#155998,#155999,#156000,#156001,
#156002,#156003,#156004),(#156005,#156006,#156007,#156008,#156009,#156010,
#156011,#156012,#156013),(#156014,#156015,#156016,#156017,#156018,#156019,
#156020,#156021,#156022),(#156023,#156024,#156025,#156026,#156027,#156028,
#156029,#156030,#156031),(#156032,#156033,#156034,#156035,#156036,#156037,
#156038,#156039,#156040),(#156041,#156042,#156043,#156044,#156045,#156046,
#156047,#156048,#156049),(#156050,#156051,#156052,#156053,#156054,#156055,
#156056,#156057,#156058),(#156059,#156060,#156061,#156062,#156063,#156064,
#156065,#156066,#156067),(#156068,#156069,#156070,#156071,#156072,#156073,
#156074,#156075,#156076),(#156077,#156078,#156079,#156080,#156081,#156082,
#156083,#156084,#156085),(#156086,#156087,#156088,#156089,#156090,#156091,
#156092,#156093,#156094),(#156095,#156096,#156097,#156098,#156099,#156100,
#156101,#156102,#156103),(#156104,#156105,#156106,#156107,#156108,#156109,
#156110,#156111,#156112),(#156113,#156114,#156115,#156116,#156117,#156118,
#156119,#156120,#156121),(#156122,#156123,#156124,#156125,#156126,#156127,
#156128,#156129,#156130),(#156131,#156132,#156133,#156134,#156135,#156136,
#156137,#156138,#156139),(#156140,#156141,#156142,#156143,#156144,#156145,
#156146,#156147,#156148),(#156149,#156150,#156151,#156152,#156153,#156154,
#156155,#156156,#156157),(#156158,#156159,#156160,#156161,#156162,#156163,
#156164,#156165,#156166),(#156167,#156168,#156169,#156170,#156171,#156172,
#156173,#156174,#156175),(#156176,#156177,#156178,#156179,#156180,#156181,
#156182,#156183,#156184),(#156185,#156186,#156187,#156188,#156189,#156190,
#156191,#156192,#156193),(#156194,#156195,#156196,#156197,#156198,#156199,
#156200,#156201,#156202),(#156203,#156204,#156205,#156206,#156207,#156208,
#156209,#156210,#156211),(#156212,#156213,#156214,#156215,#156216,#156217,
#156218,#156219,#156220),(#156221,#156222,#156223,#156224,#156225,#156226,
#156227,#156228,#156229),(#156230,#156231,#156232,#156233,#156234,#156235,
#156236,#156237,#156238),(#156239,#156240,#156241,#156242,#156243,#156244,
#156245,#156246,#156247),(#156248,#156249,#156250,#156251,#156252,#156253,
#156254,#156255,#156256),(#156257,#156258,#156259,#156260,#156261,#156262,
#156263,#156264,#156265),(#156266,#156267,#156268,#156269,#156270,#156271,
#156272,#156273,#156274),(#156275,#156276,#156277,#156278,#156279,#156280,
#156281,#156282,#156283),(#156284,#156285,#156286,#156287,#156288,#156289,
#156290,#156291,#156292),(#156293,#156294,#156295,#156296,#156297,#156298,
#156299,#156300,#156301),(#156302,#156303,#156304,#156305,#156306,#156307,
#156308,#156309,#156310),(#156311,#156312,#156313,#156314,#156315,#156316,
#156317,#156318,#156319),(#156320,#156321,#156322,#156323,#156324,#156325,
#156326,#156327,#156328),(#156329,#156330,#156331,#156332,#156333,#156334,
#156335,#156336,#156337),(#156338,#156339,#156340,#156341,#156342,#156343,
#156344,#156345,#156346),(#156347,#156348,#156349,#156350,#156351,#156352,
#156353,#156354,#156355),(#156356,#156357,#156358,#156359,#156360,#156361,
#156362,#156363,#156364),(#156365,#156366,#156367,#156368,#156369,#156370,
#156371,#156372,#156373),(#156374,#156375,#156376,#156377,#156378,#156379,
#156380,#156381,#156382),(#156383,#156384,#156385,#156386,#156387,#156388,
#156389,#156390,#156391),(#156392,#156393,#156394,#156395,#156396,#156397,
#156398,#156399,#156400),(#156401,#156402,#156403,#156404,#156405,#156406,
#156407,#156408,#156409),(#156410,#156411,#156412,#156413,#156414,#156415,
#156416,#156417,#156418),(#156419,#156420,#156421,#156422,#156423,#156424,
#156425,#156426,#156427),(#156428,#156429,#156430,#156431,#156432,#156433,
#156434,#156435,#156436),(#156437,#156438,#156439,#156440,#156441,#156442,
#156443,#156444,#156445),(#156446,#156447,#156448,#156449,#156450,#156451,
#156452,#156453,#156454),(#156455,#156456,#156457,#156458,#156459,#156460,
#156461,#156462,#156463),(#156464,#156465,#156466,#156467,#156468,#156469,
#156470,#156471,#156472),(#156473,#156474,#156475,#156476,#156477,#156478,
#156479,#156480,#156481),(#156482,#156483,#156484,#156485,#156486,#156487,
#156488,#156489,#156490),(#156491,#156492,#156493,#156494,#156495,#156496,
#156497,#156498,#156499),(#156500,#156501,#156502,#156503,#156504,#156505,
#156506,#156507,#156508),(#156509,#156510,#156511,#156512,#156513,#156514,
#156515,#156516,#156517),(#156518,#156519,#156520,#156521,#156522,#156523,
#156524,#156525,#156526),(#156527,#156528,#156529,#156530,#156531,#156532,
#156533,#156534,#156535),(#156536,#156537,#156538,#156539,#156540,#156541,
#156542,#156543,#156544),(#156545,#156546,#156547,#156548,#156549,#156550,
#156551,#156552,#156553),(#156554,#156555,#156556,#156557,#156558,#156559,
#156560,#156561,#156562),(#156563,#156564,#156565,#156566,#156567,#156568,
#156569,#156570,#156571),(#156572,#156573,#156574,#156575,#156576,#156577,
#156578,#156579,#156580),(#156581,#156582,#156583,#156584,#156585,#156586,
#156587,#156588,#156589),(#156590,#156591,#156592,#156593,#156594,#156595,
#156596,#156597,#156598),(#156599,#156600,#156601,#156602,#156603,#156604,
#156605,#156606,#156607),(#156608,#156609,#156610,#156611,#156612,#156613,
#156614,#156615,#156616),(#156617,#156618,#156619,#156620,#156621,#156622,
#156623,#156624,#156625),(#156626,#156627,#156628,#156629,#156630,#156631,
#156632,#156633,#156634),(#156635,#156636,#156637,#156638,#156639,#156640,
#156641,#156642,#156643),(#156644,#156645,#156646,#156647,#156648,#156649,
#156650,#156651,#156652),(#156653,#156654,#156655,#156656,#156657,#156658,
#156659,#156660,#156661),(#156662,#156663,#156664,#156665,#156666,#156667,
#156668,#156669,#156670),(#156671,#156672,#156673,#156674,#156675,#156676,
#156677,#156678,#156679),(#156680,#156681,#156682,#156683,#156684,#156685,
#156686,#156687,#156688),(#156689,#156690,#156691,#156692,#156693,#156694,
#156695,#156696,#156697),(#156698,#156699,#156700,#156701,#156702,#156703,
#156704,#156705,#156706),(#156707,#156708,#156709,#156710,#156711,#156712,
#156713,#156714,#156715),(#156716,#156717,#156718,#156719,#156720,#156721,
#156722,#156723,#156724),(#156725,#156726,#156727,#156728,#156729,#156730,
#156731,#156732,#156733),(#156734,#156735,#156736,#156737,#156738,#156739,
#156740,#156741,#156742),(#156743,#156744,#156745,#156746,#156747,#156748,
#156749,#156750,#156751),(#156752,#156753,#156754,#156755,#156756,#156757,
#156758,#156759,#156760),(#156761,#156762,#156763,#156764,#156765,#156766,
#156767,#156768,#156769),(#156770,#156771,#156772,#156773,#156774,#156775,
#156776,#156777,#156778),(#156779,#156780,#156781,#156782,#156783,#156784,
#156785,#156786,#156787),(#156788,#156789,#156790,#156791,#156792,#156793,
#156794,#156795,#156796),(#156797,#156798,#156799,#156800,#156801,#156802,
#156803,#156804,#156805),(#156806,#156807,#156808,#156809,#156810,#156811,
#156812,#156813,#156814),(#156815,#156816,#156817,#156818,#156819,#156820,
#156821,#156822,#156823),(#156824,#156825,#156826,#156827,#156828,#156829,
#156830,#156831,#156832),(#156833,#156834,#156835,#156836,#156837,#156838,
#156839,#156840,#156841),(#156842,#156843,#156844,#156845,#156846,#156847,
#156848,#156849,#156850),(#156851,#156852,#156853,#156854,#156855,#156856,
#156857,#156858,#156859),(#156860,#156861,#156862,#156863,#156864,#156865,
#156866,#156867,#156868),(#156869,#156870,#156871,#156872,#156873,#156874,
#156875,#156876,#156877),(#156878,#156879,#156880,#156881,#156882,#156883,
#156884,#156885,#156886),(#156887,#156888,#156889,#156890,#156891,#156892,
#156893,#156894,#156895),(#156896,#156897,#156898,#156899,#156900,#156901,
#156902,#156903,#156904),(#156905,#156906,#156907,#156908,#156909,#156910,
#156911,#156912,#156913),(#156914,#156915,#156916,#156917,#156918,#156919,
#156920,#156921,#156922),(#156923,#156924,#156925,#156926,#156927,#156928,
#156929,#156930,#156931),(#156932,#156933,#156934,#156935,#156936,#156937,
#156938,#156939,#156940),(#156941,#156942,#156943,#156944,#156945,#156946,
#156947,#156948,#156949),(#156950,#156951,#156952,#156953,#156954,#156955,
#156956,#156957,#156958),(#156959,#156960,#156961,#156962,#156963,#156964,
#156965,#156966,#156967),(#156968,#156969,#156970,#156971,#156972,#156973,
#156974,#156975,#156976),(#156977,#156978,#156979,#156980,#156981,#156982,
#156983,#156984,#156985),(#156986,#156987,#156988,#156989,#156990,#156991,
#156992,#156993,#156994),(#156995,#156996,#156997,#156998,#156999,#157000,
#157001,#157002,#157003),(#157004,#157005,#157006,#157007,#157008,#157009,
#157010,#157011,#157012),(#157013,#157014,#157015,#157016,#157017,#157018,
#157019,#157020,#157021),(#157022,#157023,#157024,#157025,#157026,#157027,
#157028,#157029,#157030),(#157031,#157032,#157033,#157034,#157035,#157036,
#157037,#157038,#157039),(#157040,#157041,#157042,#157043,#157044,#157045,
#157046,#157047,#157048),(#157049,#157050,#157051,#157052,#157053,#157054,
#157055,#157056,#157057),(#157058,#157059,#157060,#157061,#157062,#157063,
#157064,#157065,#157066),(#157067,#157068,#157069,#157070,#157071,#157072,
#157073,#157074,#157075),(#157076,#157077,#157078,#157079,#157080,#157081,
#157082,#157083,#157084),(#157085,#157086,#157087,#157088,#157089,#157090,
#157091,#157092,#157093),(#157094,#157095,#157096,#157097,#157098,#157099,
#157100,#157101,#157102),(#157103,#157104,#157105,#157106,#157107,#157108,
#157109,#157110,#157111),(#157112,#157113,#157114,#157115,#157116,#157117,
#157118,#157119,#157120),(#157121,#157122,#157123,#157124,#157125,#157126,
#157127,#157128,#157129),(#157130,#157131,#157132,#157133,#157134,#157135,
#157136,#157137,#157138),(#157139,#157140,#157141,#157142,#157143,#157144,
#157145,#157146,#157147),(#157148,#157149,#157150,#157151,#157152,#157153,
#157154,#157155,#157156),(#157157,#157158,#157159,#157160,#157161,#157162,
#157163,#157164,#157165),(#157166,#157167,#157168,#157169,#157170,#157171,
#157172,#157173,#157174),(#157175,#157176,#157177,#157178,#157179,#157180,
#157181,#157182,#157183),(#157184,#157185,#157186,#157187,#157188,#157189,
#157190,#157191,#157192),(#157193,#157194,#157195,#157196,#157197,#157198,
#157199,#157200,#157201),(#157202,#157203,#157204,#157205,#157206,#157207,
#157208,#157209,#157210),(#157211,#157212,#157213,#157214,#157215,#157216,
#157217,#157218,#157219),(#157220,#157221,#157222,#157223,#157224,#157225,
#157226,#157227,#157228),(#157229,#157230,#157231,#157232,#157233,#157234,
#157235,#157236,#157237),(#157238,#157239,#157240,#157241,#157242,#157243,
#157244,#157245,#157246),(#157247,#157248,#157249,#157250,#157251,#157252,
#157253,#157254,#157255),(#157256,#157257,#157258,#157259,#157260,#157261,
#157262,#157263,#157264),(#157265,#157266,#157267,#157268,#157269,#157270,
#157271,#157272,#157273),(#157274,#157275,#157276,#157277,#157278,#157279,
#157280,#157281,#157282),(#157283,#157284,#157285,#157286,#157287,#157288,
#157289,#157290,#157291),(#157292,#157293,#157294,#157295,#157296,#157297,
#157298,#157299,#157300),(#157301,#157302,#157303,#157304,#157305,#157306,
#157307,#157308,#157309),(#157310,#157311,#157312,#157313,#157314,#157315,
#157316,#157317,#157318),(#157319,#157320,#157321,#157322,#157323,#157324,
#157325,#157326,#157327),(#157328,#157329,#157330,#157331,#157332,#157333,
#157334,#157335,#157336),(#157337,#157338,#157339,#157340,#157341,#157342,
#157343,#157344,#157345),(#157346,#157347,#157348,#157349,#157350,#157351,
#157352,#157353,#157354),(#157355,#157356,#157357,#157358,#157359,#157360,
#157361,#157362,#157363),(#157364,#157365,#157366,#157367,#157368,#157369,
#157370,#157371,#157372),(#157373,#157374,#157375,#157376,#157377,#157378,
#157379,#157380,#157381),(#157382,#157383,#157384,#157385,#157386,#157387,
#157388,#157389,#157390),(#157391,#157392,#157393,#157394,#157395,#157396,
#157397,#157398,#157399),(#157400,#157401,#157402,#157403,#157404,#157405,
#157406,#157407,#157408),(#157409,#157410,#157411,#157412,#157413,#157414,
#157415,#157416,#157417),(#157418,#157419,#157420,#157421,#157422,#157423,
#157424,#157425,#157426),(#157427,#157428,#157429,#157430,#157431,#157432,
#157433,#157434,#157435),(#157436,#157437,#157438,#157439,#157440,#157441,
#157442,#157443,#157444),(#157445,#157446,#157447,#157448,#157449,#157450,
#157451,#157452,#157453),(#157454,#157455,#157456,#157457,#157458,#157459,
#157460,#157461,#157462),(#157463,#157464,#157465,#157466,#157467,#157468,
#157469,#157470,#157471),(#157472,#157473,#157474,#157475,#157476,#157477,
#157478,#157479,#157480),(#157481,#157482,#157483,#157484,#157485,#157486,
#157487,#157488,#157489),(#157490,#157491,#157492,#157493,#157494,#157495,
#157496,#157497,#157498),(#157499,#157500,#157501,#157502,#157503,#157504,
#157505,#157506,#157507),(#157508,#157509,#157510,#157511,#157512,#157513,
#157514,#157515,#157516),(#157517,#157518,#157519,#157520,#157521,#157522,
#157523,#157524,#157525),(#157526,#157527,#157528,#157529,#157530,#157531,
#157532,#157533,#157534),(#157535,#157536,#157537,#157538,#157539,#157540,
#157541,#157542,#157543),(#157544,#157545,#157546,#157547,#157548,#157549,
#157550,#157551,#157552),(#157553,#157554,#157555,#157556,#157557,#157558,
#157559,#157560,#157561),(#157562,#157563,#157564,#157565,#157566,#157567,
#157568,#157569,#157570),(#157571,#157572,#157573,#157574,#157575,#157576,
#157577,#157578,#157579),(#157580,#157581,#157582,#157583,#157584,#157585,
#157586,#157587,#157588),(#157589,#157590,#157591,#157592,#157593,#157594,
#157595,#157596,#157597),(#157598,#157599,#157600,#157601,#157602,#157603,
#157604,#157605,#157606),(#157607,#157608,#157609,#157610,#157611,#157612,
#157613,#157614,#157615),(#157616,#157617,#157618,#157619,#157620,#157621,
#157622,#157623,#157624),(#157625,#157626,#157627,#157628,#157629,#157630,
#157631,#157632,#157633),(#157634,#157635,#157636,#157637,#157638,#157639,
#157640,#157641,#157642),(#157643,#157644,#157645,#157646,#157647,#157648,
#157649,#157650,#157651),(#157652,#157653,#157654,#157655,#157656,#157657,
#157658,#157659,#157660),(#157661,#157662,#157663,#157664,#157665,#157666,
#157667,#157668,#157669),(#157670,#157671,#157672,#157673,#157674,#157675,
#157676,#157677,#157678),(#157679,#157680,#157681,#157682,#157683,#157684,
#157685,#157686,#157687),(#157688,#157689,#157690,#157691,#157692,#157693,
#157694,#157695,#157696),(#157697,#157698,#157699,#157700,#157701,#157702,
#157703,#157704,#157705),(#157706,#157707,#157708,#157709,#157710,#157711,
#157712,#157713,#157714),(#157715,#157716,#157717,#157718,#157719,#157720,
#157721,#157722,#157723),(#157724,#157725,#157726,#157727,#157728,#157729,
#157730,#157731,#157732),(#157733,#157734,#157735,#157736,#157737,#157738,
#157739,#157740,#157741),(#157742,#157743,#157744,#157745,#157746,#157747,
#157748,#157749,#157750),(#157751,#157752,#157753,#157754,#157755,#157756,
#157757,#157758,#157759),(#157760,#157761,#157762,#157763,#157764,#157765,
#157766,#157767,#157768),(#157769,#157770,#157771,#157772,#157773,#157774,
#157775,#157776,#157777),(#157778,#157779,#157780,#157781,#157782,#157783,
#157784,#157785,#157786),(#157787,#157788,#157789,#157790,#157791,#157792,
#157793,#157794,#157795),(#157796,#157797,#157798,#157799,#157800,#157801,
#157802,#157803,#157804),(#157805,#157806,#157807,#157808,#157809,#157810,
#157811,#157812,#157813),(#157814,#157815,#157816,#157817,#157818,#157819,
#157820,#157821,#157822),(#157823,#157824,#157825,#157826,#157827,#157828,
#157829,#157830,#157831),(#157832,#157833,#157834,#157835,#157836,#157837,
#157838,#157839,#157840),(#157841,#157842,#157843,#157844,#157845,#157846,
#157847,#157848,#157849),(#157850,#157851,#157852,#157853,#157854,#157855,
#157856,#157857,#157858),(#157859,#157860,#157861,#157862,#157863,#157864,
#157865,#157866,#157867),(#157868,#157869,#157870,#157871,#157872,#157873,
#157874,#157875,#157876),(#157877,#157878,#157879,#157880,#157881,#157882,
#157883,#157884,#157885),(#157886,#157887,#157888,#157889,#157890,#157891,
#157892,#157893,#157894),(#157895,#157896,#157897,#157898,#157899,#157900,
#157901,#157902,#157903),(#157904,#157905,#157906,#157907,#157908,#157909,
#157910,#157911,#157912),(#157913,#157914,#157915,#157916,#157917,#157918,
#157919,#157920,#157921),(#157922,#157923,#157924,#157925,#157926,#157927,
#157928,#157929,#157930),(#157931,#157932,#157933,#157934,#157935,#157936,
#157937,#157938,#157939),(#157940,#157941,#157942,#157943,#157944,#157945,
#157946,#157947,#157948),(#157949,#157950,#157951,#157952,#157953,#157954,
#157955,#157956,#157957),(#157958,#157959,#157960,#157961,#157962,#157963,
#157964,#157965,#157966),(#157967,#157968,#157969,#157970,#157971,#157972,
#157973,#157974,#157975),(#157976,#157977,#157978,#157979,#157980,#157981,
#157982,#157983,#157984),(#157985,#157986,#157987,#157988,#157989,#157990,
#157991,#157992,#157993),(#157994,#157995,#157996,#157997,#157998,#157999,
#158000,#158001,#158002),(#158003,#158004,#158005,#158006,#158007,#158008,
#158009,#158010,#158011),(#158012,#158013,#158014,#158015,#158016,#158017,
#158018,#158019,#158020),(#158021,#158022,#158023,#158024,#158025,#158026,
#158027,#158028,#158029),(#158030,#158031,#158032,#158033,#158034,#158035,
#158036,#158037,#158038),(#158039,#158040,#158041,#158042,#158043,#158044,
#158045,#158046,#158047),(#158048,#158049,#158050,#158051,#158052,#158053,
#158054,#158055,#158056),(#158057,#158058,#158059,#158060,#158061,#158062,
#158063,#158064,#158065),(#158066,#158067,#158068,#158069,#158070,#158071,
#158072,#158073,#158074),(#158075,#158076,#158077,#158078,#158079,#158080,
#158081,#158082,#158083),(#158084,#158085,#158086,#158087,#158088,#158089,
#158090,#158091,#158092),(#158093,#158094,#158095,#158096,#158097,#158098,
#158099,#158100,#158101),(#158102,#158103,#158104,#158105,#158106,#158107,
#158108,#158109,#158110),(#158111,#158112,#158113,#158114,#158115,#158116,
#158117,#158118,#158119),(#158120,#158121,#158122,#158123,#158124,#158125,
#158126,#158127,#158128),(#158129,#158130,#158131,#158132,#158133,#158134,
#158135,#158136,#158137),(#158138,#158139,#158140,#158141,#158142,#158143,
#158144,#158145,#158146),(#158147,#158148,#158149,#158150,#158151,#158152,
#158153,#158154,#158155),(#158156,#158157,#158158,#158159,#158160,#158161,
#158162,#158163,#158164),(#158165,#158166,#158167,#158168,#158169,#158170,
#158171,#158172,#158173),(#158174,#158175,#158176,#158177,#158178,#158179,
#158180,#158181,#158182),(#158183,#158184,#158185,#158186,#158187,#158188,
#158189,#158190,#158191),(#158192,#158193,#158194,#158195,#158196,#158197,
#158198,#158199,#158200),(#158201,#158202,#158203,#158204,#158205,#158206,
#158207,#158208,#158209),(#158210,#158211,#158212,#158213,#158214,#158215,
#158216,#158217,#158218),(#158219,#158220,#158221,#158222,#158223,#158224,
#158225,#158226,#158227),(#158228,#158229,#158230,#158231,#158232,#158233,
#158234,#158235,#158236),(#158237,#158238,#158239,#158240,#158241,#158242,
#158243,#158244,#158245),(#158246,#158247,#158248,#158249,#158250,#158251,
#158252,#158253,#158254),(#158255,#158256,#158257,#158258,#158259,#158260,
#158261,#158262,#158263),(#158264,#158265,#158266,#158267,#158268,#158269,
#158270,#158271,#158272),(#158273,#158274,#158275,#158276,#158277,#158278,
#158279,#158280,#158281),(#158282,#158283,#158284,#158285,#158286,#158287,
#158288,#158289,#158290),(#158291,#158292,#158293,#158294,#158295,#158296,
#158297,#158298,#158299),(#158300,#158301,#158302,#158303,#158304,#158305,
#158306,#158307,#158308),(#158309,#158310,#158311,#158312,#158313,#158314,
#158315,#158316,#158317),(#158318,#158319,#158320,#158321,#158322,#158323,
#158324,#158325,#158326),(#158327,#158328,#158329,#158330,#158331,#158332,
#158333,#158334,#158335),(#158336,#158337,#158338,#158339,#158340,#158341,
#158342,#158343,#158344),(#158345,#158346,#158347,#158348,#158349,#158350,
#158351,#158352,#158353),(#158354,#158355,#158356,#158357,#158358,#158359,
#158360,#158361,#158362),(#158363,#158364,#158365,#158366,#158367,#158368,
#158369,#158370,#158371),(#158372,#158373,#158374,#158375,#158376,#158377,
#158378,#158379,#158380),(#158381,#158382,#158383,#158384,#158385,#158386,
#158387,#158388,#158389),(#158390,#158391,#158392,#158393,#158394,#158395,
#158396,#158397,#158398),(#158399,#158400,#158401,#158402,#158403,#158404,
#158405,#158406,#158407),(#158408,#158409,#158410,#158411,#158412,#158413,
#158414,#158415,#158416),(#158417,#158418,#158419,#158420,#158421,#158422,
#158423,#158424,#158425),(#158426,#158427,#158428,#158429,#158430,#158431,
#158432,#158433,#158434),(#158435,#158436,#158437,#158438,#158439,#158440,
#158441,#158442,#158443),(#158444,#158445,#158446,#158447,#158448,#158449,
#158450,#158451,#158452),(#158453,#158454,#158455,#158456,#158457,#158458,
#158459,#158460,#158461),(#158462,#158463,#158464,#158465,#158466,#158467,
#158468,#158469,#158470),(#158471,#158472,#158473,#158474,#158475,#158476,
#158477,#158478,#158479),(#158480,#158481,#158482,#158483,#158484,#158485,
#158486,#158487,#158488),(#158489,#158490,#158491,#158492,#158493,#158494,
#158495,#158496,#158497),(#158498,#158499,#158500,#158501,#158502,#158503,
#158504,#158505,#158506),(#158507,#158508,#158509,#158510,#158511,#158512,
#158513,#158514,#158515),(#158516,#158517,#158518,#158519,#158520,#158521,
#158522,#158523,#158524),(#158525,#158526,#158527,#158528,#158529,#158530,
#158531,#158532,#158533),(#158534,#158535,#158536,#158537,#158538,#158539,
#158540,#158541,#158542),(#158543,#158544,#158545,#158546,#158547,#158548,
#158549,#158550,#158551),(#158552,#158553,#158554,#158555,#158556,#158557,
#158558,#158559,#158560),(#158561,#158562,#158563,#158564,#158565,#158566,
#158567,#158568,#158569),(#158570,#158571,#158572,#158573,#158574,#158575,
#158576,#158577,#158578),(#158579,#158580,#158581,#158582,#158583,#158584,
#158585,#158586,#158587),(#158588,#158589,#158590,#158591,#158592,#158593,
#158594,#158595,#158596),(#158597,#158598,#158599,#158600,#158601,#158602,
#158603,#158604,#158605),(#158606,#158607,#158608,#158609,#158610,#158611,
#158612,#158613,#158614),(#158615,#158616,#158617,#158618,#158619,#158620,
#158621,#158622,#158623),(#158624,#158625,#158626,#158627,#158628,#158629,
#158630,#158631,#158632),(#158633,#158634,#158635,#158636,#158637,#158638,
#158639,#158640,#158641),(#158642,#158643,#158644,#158645,#158646,#158647,
#158648,#158649,#158650),(#158651,#158652,#158653,#158654,#158655,#158656,
#158657,#158658,#158659),(#158660,#158661,#158662,#158663,#158664,#158665,
#158666,#158667,#158668),(#158669,#158670,#158671,#158672,#158673,#158674,
#158675,#158676,#158677),(#158678,#158679,#158680,#158681,#158682,#158683,
#158684,#158685,#158686),(#158687,#158688,#158689,#158690,#158691,#158692,
#158693,#158694,#158695),(#158696,#158697,#158698,#158699,#158700,#158701,
#158702,#158703,#158704),(#158705,#158706,#158707,#158708,#158709,#158710,
#158711,#158712,#158713),(#158714,#158715,#158716,#158717,#158718,#158719,
#158720,#158721,#158722),(#158723,#158724,#158725,#158726,#158727,#158728,
#158729,#158730,#158731),(#158732,#158733,#158734,#158735,#158736,#158737,
#158738,#158739,#158740),(#158741,#158742,#158743,#158744,#158745,#158746,
#158747,#158748,#158749),(#158750,#158751,#158752,#158753,#158754,#158755,
#158756,#158757,#158758),(#158759,#158760,#158761,#158762,#158763,#158764,
#158765,#158766,#158767),(#158768,#158769,#158770,#158771,#158772,#158773,
#158774,#158775,#158776),(#158777,#158778,#158779,#158780,#158781,#158782,
#158783,#158784,#158785),(#158786,#158787,#158788,#158789,#158790,#158791,
#158792,#158793,#158794),(#158795,#158796,#158797,#158798,#158799,#158800,
#158801,#158802,#158803),(#158804,#158805,#158806,#158807,#158808,#158809,
#158810,#158811,#158812),(#158813,#158814,#158815,#158816,#158817,#158818,
#158819,#158820,#158821),(#158822,#158823,#158824,#158825,#158826,#158827,
#158828,#158829,#158830),(#158831,#158832,#158833,#158834,#158835,#158836,
#158837,#158838,#158839),(#158840,#158841,#158842,#158843,#158844,#158845,
#158846,#158847,#158848),(#158849,#158850,#158851,#158852,#158853,#158854,
#158855,#158856,#158857),(#158858,#158859,#158860,#158861,#158862,#158863,
#158864,#158865,#158866),(#158867,#158868,#158869,#158870,#158871,#158872,
#158873,#158874,#158875),(#158876,#158877,#158878,#158879,#158880,#158881,
#158882,#158883,#158884),(#158885,#158886,#158887,#158888,#158889,#158890,
#158891,#158892,#158893),(#158894,#158895,#158896,#158897,#158898,#158899,
#158900,#158901,#158902),(#158903,#158904,#158905,#158906,#158907,#158908,
#158909,#158910,#158911),(#158912,#158913,#158914,#158915,#158916,#158917,
#158918,#158919,#158920),(#158921,#158922,#158923,#158924,#158925,#158926,
#158927,#158928,#158929),(#158930,#158931,#158932,#158933,#158934,#158935,
#158936,#158937,#158938),(#158939,#158940,#158941,#158942,#158943,#158944,
#158945,#158946,#158947),(#158948,#158949,#158950,#158951,#158952,#158953,
#158954,#158955,#158956),(#158957,#158958,#158959,#158960,#158961,#158962,
#158963,#158964,#158965),(#158966,#158967,#158968,#158969,#158970,#158971,
#158972,#158973,#158974),(#158975,#158976,#158977,#158978,#158979,#158980,
#158981,#158982,#158983),(#158984,#158985,#158986,#158987,#158988,#158989,
#158990,#158991,#158992),(#158993,#158994,#158995,#158996,#158997,#158998,
#158999,#159000,#159001),(#159002,#159003,#159004,#159005,#159006,#159007,
#159008,#159009,#159010),(#159011,#159012,#159013,#159014,#159015,#159016,
#159017,#159018,#159019),(#159020,#159021,#159022,#159023,#159024,#159025,
#159026,#159027,#159028),(#159029,#159030,#159031,#159032,#159033,#159034,
#159035,#159036,#159037),(#159038,#159039,#159040,#159041,#159042,#159043,
#159044,#159045,#159046),(#159047,#159048,#159049,#159050,#159051,#159052,
#159053,#159054,#159055),(#159056,#159057,#159058,#159059,#159060,#159061,
#159062,#159063,#159064),(#159065,#159066,#159067,#159068,#159069,#159070,
#159071,#159072,#159073),(#159074,#159075,#159076,#159077,#159078,#159079,
#159080,#159081,#159082),(#159083,#159084,#159085,#159086,#159087,#159088,
#159089,#159090,#159091),(#159092,#159093,#159094,#159095,#159096,#159097,
#159098,#159099,#159100),(#159101,#159102,#159103,#159104,#159105,#159106,
#159107,#159108,#159109),(#159110,#159111,#159112,#159113,#159114,#159115,
#159116,#159117,#159118),(#159119,#159120,#159121,#159122,#159123,#159124,
#159125,#159126,#159127),(#159128,#159129,#159130,#159131,#159132,#159133,
#159134,#159135,#159136),(#159137,#159138,#159139,#159140,#159141,#159142,
#159143,#159144,#159145),(#159146,#159147,#159148,#159149,#159150,#159151,
#159152,#159153,#159154),(#159155,#159156,#159157,#159158,#159159,#159160,
#159161,#159162,#159163),(#159164,#159165,#159166,#159167,#159168,#159169,
#159170,#159171,#159172),(#159173,#159174,#159175,#159176,#159177,#159178,
#159179,#159180,#159181),(#159182,#159183,#159184,#159185,#159186,#159187,
#159188,#159189,#159190),(#159191,#159192,#159193,#159194,#159195,#159196,
#159197,#159198,#159199),(#159200,#159201,#159202,#159203,#159204,#159205,
#159206,#159207,#159208),(#159209,#159210,#159211,#159212,#159213,#159214,
#159215,#159216,#159217),(#159218,#159219,#159220,#159221,#159222,#159223,
#159224,#159225,#159226),(#159227,#159228,#159229,#159230,#159231,#159232,
#159233,#159234,#159235),(#159236,#159237,#159238,#159239,#159240,#159241,
#159242,#159243,#159244),(#159245,#159246,#159247,#159248,#159249,#159250,
#159251,#159252,#159253),(#159254,#159255,#159256,#159257,#159258,#159259,
#159260,#159261,#159262),(#159263,#159264,#159265,#159266,#159267,#159268,
#159269,#159270,#159271),(#159272,#159273,#159274,#159275,#159276,#159277,
#159278,#159279,#159280),(#159281,#159282,#159283,#159284,#159285,#159286,
#159287,#159288,#159289),(#159290,#159291,#159292,#159293,#159294,#159295,
#159296,#159297,#159298),(#159299,#159300,#159301,#159302,#159303,#159304,
#159305,#159306,#159307),(#159308,#159309,#159310,#159311,#159312,#159313,
#159314,#159315,#159316),(#159317,#159318,#159319,#159320,#159321,#159322,
#159323,#159324,#159325),(#159326,#159327,#159328,#159329,#159330,#159331,
#159332,#159333,#159334),(#159335,#159336,#159337,#159338,#159339,#159340,
#159341,#159342,#159343),(#159344,#159345,#159346,#159347,#159348,#159349,
#159350,#159351,#159352),(#159353,#159354,#159355,#159356,#159357,#159358,
#159359,#159360,#159361),(#159362,#159363,#159364,#159365,#159366,#159367,
#159368,#159369,#159370),(#159371,#159372,#159373,#159374,#159375,#159376,
#159377,#159378,#159379),(#159380,#159381,#159382,#159383,#159384,#159385,
#159386,#159387,#159388),(#159389,#159390,#159391,#159392,#159393,#159394,
#159395,#159396,#159397),(#159398,#159399,#159400,#159401,#159402,#159403,
#159404,#159405,#159406),(#159407,#159408,#159409,#159410,#159411,#159412,
#159413,#159414,#159415),(#159416,#159417,#159418,#159419,#159420,#159421,
#159422,#159423,#159424),(#159425,#159426,#159427,#159428,#159429,#159430,
#159431,#159432,#159433),(#159434,#159435,#159436,#159437,#159438,#159439,
#159440,#159441,#159442),(#159443,#159444,#159445,#159446,#159447,#159448,
#159449,#159450,#159451),(#159452,#159453,#159454,#159455,#159456,#159457,
#159458,#159459,#159460),(#159461,#159462,#159463,#159464,#159465,#159466,
#159467,#159468,#159469),(#159470,#159471,#159472,#159473,#159474,#159475,
#159476,#159477,#159478),(#159479,#159480,#159481,#159482,#159483,#159484,
#159485,#159486,#159487),(#159488,#159489,#159490,#159491,#159492,#159493,
#159494,#159495,#159496),(#159497,#159498,#159499,#159500,#159501,#159502,
#159503,#159504,#159505),(#159506,#159507,#159508,#159509,#159510,#159511,
#159512,#159513,#159514),(#159515,#159516,#159517,#159518,#159519,#159520,
#159521,#159522,#159523),(#159524,#159525,#159526,#159527,#159528,#159529,
#159530,#159531,#159532),(#159533,#159534,#159535,#159536,#159537,#159538,
#159539,#159540,#159541),(#159542,#159543,#159544,#159545,#159546,#159547,
#159548,#159549,#159550),(#159551,#159552,#159553,#159554,#159555,#159556,
#159557,#159558,#159559),(#159560,#159561,#159562,#159563,#159564,#159565,
#159566,#159567,#159568),(#159569,#159570,#159571,#159572,#159573,#159574,
#159575,#159576,#159577),(#159578,#159579,#159580,#159581,#159582,#159583,
#159584,#159585,#159586),(#159587,#159588,#159589,#159590,#159591,#159592,
#159593,#159594,#159595),(#159596,#159597,#159598,#159599,#159600,#159601,
#159602,#159603,#159604),(#159605,#159606,#159607,#159608,#159609,#159610,
#159611,#159612,#159613),(#159614,#159615,#159616,#159617,#159618,#159619,
#159620,#159621,#159622),(#159623,#159624,#159625,#159626,#159627,#159628,
#159629,#159630,#159631),(#159632,#159633,#159634,#159635,#159636,#159637,
#159638,#159639,#159640),(#159641,#159642,#159643,#159644,#159645,#159646,
#159647,#159648,#159649),(#159650,#159651,#159652,#159653,#159654,#159655,
#159656,#159657,#159658),(#159659,#159660,#159661,#159662,#159663,#159664,
#159665,#159666,#159667),(#159668,#159669,#159670,#159671,#159672,#159673,
#159674,#159675,#159676),(#159677,#159678,#159679,#159680,#159681,#159682,
#159683,#159684,#159685),(#159686,#159687,#159688,#159689,#159690,#159691,
#159692,#159693,#159694),(#159695,#159696,#159697,#159698,#159699,#159700,
#159701,#159702,#159703),(#159704,#159705,#159706,#159707,#159708,#159709,
#159710,#159711,#159712),(#159713,#159714,#159715,#159716,#159717,#159718,
#159719,#159720,#159721),(#159722,#159723,#159724,#159725,#159726,#159727,
#159728,#159729,#159730),(#159731,#159732,#159733,#159734,#159735,#159736,
#159737,#159738,#159739),(#159740,#159741,#159742,#159743,#159744,#159745,
#159746,#159747,#159748),(#159749,#159750,#159751,#159752,#159753,#159754,
#159755,#159756,#159757),(#159758,#159759,#159760,#159761,#159762,#159763,
#159764,#159765,#159766),(#159767,#159768,#159769,#159770,#159771,#159772,
#159773,#159774,#159775),(#159776,#159777,#159778,#159779,#159780,#159781,
#159782,#159783,#159784),(#159785,#159786,#159787,#159788,#159789,#159790,
#159791,#159792,#159793),(#159794,#159795,#159796,#159797,#159798,#159799,
#159800,#159801,#159802),(#159803,#159804,#159805,#159806,#159807,#159808,
#159809,#159810,#159811),(#159812,#159813,#159814,#159815,#159816,#159817,
#159818,#159819,#159820),(#159821,#159822,#159823,#159824,#159825,#159826,
#159827,#159828,#159829),(#159830,#159831,#159832,#159833,#159834,#159835,
#159836,#159837,#159838),(#159839,#159840,#159841,#159842,#159843,#159844,
#159845,#159846,#159847),(#159848,#159849,#159850,#159851,#159852,#159853,
#159854,#159855,#159856),(#159857,#159858,#159859,#159860,#159861,#159862,
#159863,#159864,#159865),(#159866,#159867,#159868,#159869,#159870,#159871,
#159872,#159873,#159874),(#159875,#159876,#159877,#159878,#159879,#159880,
#159881,#159882,#159883),(#159884,#159885,#159886,#159887,#159888,#159889,
#159890,#159891,#159892),(#159893,#159894,#159895,#159896,#159897,#159898,
#159899,#159900,#159901),(#159902,#159903,#159904,#159905,#159906,#159907,
#159908,#159909,#159910),(#159911,#159912,#159913,#159914,#159915,#159916,
#159917,#159918,#159919),(#159920,#159921,#159922,#159923,#159924,#159925,
#159926,#159927,#159928),(#159929,#159930,#159931,#159932,#159933,#159934,
#159935,#159936,#159937),(#159938,#159939,#159940,#159941,#159942,#159943,
#159944,#159945,#159946),(#159947,#159948,#159949,#159950,#159951,#159952,
#159953,#159954,#159955),(#159956,#159957,#159958,#159959,#159960,#159961,
#159962,#159963,#159964),(#159965,#159966,#159967,#159968,#159969,#159970,
#159971,#159972,#159973),(#159974,#159975,#159976,#159977,#159978,#159979,
#159980,#159981,#159982),(#159983,#159984,#159985,#159986,#159987,#159988,
#159989,#159990,#159991),(#159992,#159993,#159994,#159995,#159996,#159997,
#159998,#159999,#160000),(#160001,#160002,#160003,#160004,#160005,#160006,
#160007,#160008,#160009),(#160010,#160011,#160012,#160013,#160014,#160015,
#160016,#160017,#160018),(#160019,#160020,#160021,#160022,#160023,#160024,
#160025,#160026,#160027),(#160028,#160029,#160030,#160031,#160032,#160033,
#160034,#160035,#160036),(#160037,#160038,#160039,#160040,#160041,#160042,
#160043,#160044,#160045),(#160046,#160047,#160048,#160049,#160050,#160051,
#160052,#160053,#160054),(#160055,#160056,#160057,#160058,#160059,#160060,
#160061,#160062,#160063),(#160064,#160065,#160066,#160067,#160068,#160069,
#160070,#160071,#160072),(#160073,#160074,#160075,#160076,#160077,#160078,
#160079,#160080,#160081),(#160082,#160083,#160084,#160085,#160086,#160087,
#160088,#160089,#160090),(#160091,#160092,#160093,#160094,#160095,#160096,
#160097,#160098,#160099),(#160100,#160101,#160102,#160103,#160104,#160105,
#160106,#160107,#160108),(#160109,#160110,#160111,#160112,#160113,#160114,
#160115,#160116,#160117),(#160118,#160119,#160120,#160121,#160122,#160123,
#160124,#160125,#160126),(#160127,#160128,#160129,#160130,#160131,#160132,
#160133,#160134,#160135),(#160136,#160137,#160138,#160139,#160140,#160141,
#160142,#160143,#160144),(#160145,#160146,#160147,#160148,#160149,#160150,
#160151,#160152,#160153),(#160154,#160155,#160156,#160157,#160158,#160159,
#160160,#160161,#160162),(#160163,#160164,#160165,#160166,#160167,#160168,
#160169,#160170,#160171),(#160172,#160173,#160174,#160175,#160176,#160177,
#160178,#160179,#160180),(#160181,#160182,#160183,#160184,#160185,#160186,
#160187,#160188,#160189),(#160190,#160191,#160192,#160193,#160194,#160195,
#160196,#160197,#160198),(#160199,#160200,#160201,#160202,#160203,#160204,
#160205,#160206,#160207),(#160208,#160209,#160210,#160211,#160212,#160213,
#160214,#160215,#160216),(#160217,#160218,#160219,#160220,#160221,#160222,
#160223,#160224,#160225),(#160226,#160227,#160228,#160229,#160230,#160231,
#160232,#160233,#160234),(#160235,#160236,#160237,#160238,#160239,#160240,
#160241,#160242,#160243),(#160244,#160245,#160246,#160247,#160248,#160249,
#160250,#160251,#160252),(#160253,#160254,#160255,#160256,#160257,#160258,
#160259,#160260,#160261),(#160262,#160263,#160264,#160265,#160266,#160267,
#160268,#160269,#160270),(#160271,#160272,#160273,#160274,#160275,#160276,
#160277,#160278,#160279),(#160280,#160281,#160282,#160283,#160284,#160285,
#160286,#160287,#160288),(#160289,#160290,#160291,#160292,#160293,#160294,
#160295,#160296,#160297),(#160298,#160299,#160300,#160301,#160302,#160303,
#160304,#160305,#160306),(#160307,#160308,#160309,#160310,#160311,#160312,
#160313,#160314,#160315),(#160316,#160317,#160318,#160319,#160320,#160321,
#160322,#160323,#160324),(#160325,#160326,#160327,#160328,#160329,#160330,
#160331,#160332,#160333),(#160334,#160335,#160336,#160337,#160338,#160339,
#160340,#160341,#160342),(#160343,#160344,#160345,#160346,#160347,#160348,
#160349,#160350,#160351),(#160352,#160353,#160354,#160355,#160356,#160357,
#160358,#160359,#160360),(#160361,#160362,#160363,#160364,#160365,#160366,
#160367,#160368,#160369),(#160370,#160371,#160372,#160373,#160374,#160375,
#160376,#160377,#160378),(#160379,#160380,#160381,#160382,#160383,#160384,
#160385,#160386,#160387),(#160388,#160389,#160390,#160391,#160392,#160393,
#160394,#160395,#160396),(#160397,#160398,#160399,#160400,#160401,#160402,
#160403,#160404,#160405),(#160406,#160407,#160408,#160409,#160410,#160411,
#160412,#160413,#160414),(#160415,#160416,#160417,#160418,#160419,#160420,
#160421,#160422,#160423),(#160424,#160425,#160426,#160427,#160428,#160429,
#160430,#160431,#160432),(#160433,#160434,#160435,#160436,#160437,#160438,
#160439,#160440,#160441),(#160442,#160443,#160444,#160445,#160446,#160447,
#160448,#160449,#160450),(#160451,#160452,#160453,#160454,#160455,#160456,
#160457,#160458,#160459),(#160460,#160461,#160462,#160463,#160464,#160465,
#160466,#160467,#160468),(#160469,#160470,#160471,#160472,#160473,#160474,
#160475,#160476,#160477),(#160478,#160479,#160480,#160481,#160482,#160483,
#160484,#160485,#160486),(#160487,#160488,#160489,#160490,#160491,#160492,
#160493,#160494,#160495),(#160496,#160497,#160498,#160499,#160500,#160501,
#160502,#160503,#160504),(#160505,#160506,#160507,#160508,#160509,#160510,
#160511,#160512,#160513),(#160514,#160515,#160516,#160517,#160518,#160519,
#160520,#160521,#160522),(#160523,#160524,#160525,#160526,#160527,#160528,
#160529,#160530,#160531),(#160532,#160533,#160534,#160535,#160536,#160537,
#160538,#160539,#160540),(#160541,#160542,#160543,#160544,#160545,#160546,
#160547,#160548,#160549),(#160550,#160551,#160552,#160553,#160554,#160555,
#160556,#160557,#160558),(#160559,#160560,#160561,#160562,#160563,#160564,
#160565,#160566,#160567),(#160568,#160569,#160570,#160571,#160572,#160573,
#160574,#160575,#160576),(#160577,#160578,#160579,#160580,#160581,#160582,
#160583,#160584,#160585),(#160586,#160587,#160588,#160589,#160590,#160591,
#160592,#160593,#160594),(#160595,#160596,#160597,#160598,#160599,#160600,
#160601,#160602,#160603),(#160604,#160605,#160606,#160607,#160608,#160609,
#160610,#160611,#160612),(#160613,#160614,#160615,#160616,#160617,#160618,
#160619,#160620,#160621),(#160622,#160623,#160624,#160625,#160626,#160627,
#160628,#160629,#160630),(#160631,#160632,#160633,#160634,#160635,#160636,
#160637,#160638,#160639),(#160640,#160641,#160642,#160643,#160644,#160645,
#160646,#160647,#160648),(#160649,#160650,#160651,#160652,#160653,#160654,
#160655,#160656,#160657),(#160658,#160659,#160660,#160661,#160662,#160663,
#160664,#160665,#160666),(#160667,#160668,#160669,#160670,#160671,#160672,
#160673,#160674,#160675),(#160676,#160677,#160678,#160679,#160680,#160681,
#160682,#160683,#160684),(#160685,#160686,#160687,#160688,#160689,#160690,
#160691,#160692,#160693),(#160694,#160695,#160696,#160697,#160698,#160699,
#160700,#160701,#160702),(#160703,#160704,#160705,#160706,#160707,#160708,
#160709,#160710,#160711),(#160712,#160713,#160714,#160715,#160716,#160717,
#160718,#160719,#160720),(#160721,#160722,#160723,#160724,#160725,#160726,
#160727,#160728,#160729),(#160730,#160731,#160732,#160733,#160734,#160735,
#160736,#160737,#160738),(#160739,#160740,#160741,#160742,#160743,#160744,
#160745,#160746,#160747),(#160748,#160749,#160750,#160751,#160752,#160753,
#160754,#160755,#160756),(#160757,#160758,#160759,#160760,#160761,#160762,
#160763,#160764,#160765),(#160766,#160767,#160768,#160769,#160770,#160771,
#160772,#160773,#160774),(#160775,#160776,#160777,#160778,#160779,#160780,
#160781,#160782,#160783),(#160784,#160785,#160786,#160787,#160788,#160789,
#160790,#160791,#160792),(#160793,#160794,#160795,#160796,#160797,#160798,
#160799,#160800,#160801),(#160802,#160803,#160804,#160805,#160806,#160807,
#160808,#160809,#160810),(#160811,#160812,#160813,#160814,#160815,#160816,
#160817,#160818,#160819),(#160820,#160821,#160822,#160823,#160824,#160825,
#160826,#160827,#160828),(#160829,#160830,#160831,#160832,#160833,#160834,
#160835,#160836,#160837),(#160838,#160839,#160840,#160841,#160842,#160843,
#160844,#160845,#160846),(#160847,#160848,#160849,#160850,#160851,#160852,
#160853,#160854,#160855),(#160856,#160857,#160858,#160859,#160860,#160861,
#160862,#160863,#160864),(#160865,#160866,#160867,#160868,#160869,#160870,
#160871,#160872,#160873),(#160874,#160875,#160876,#160877,#160878,#160879,
#160880,#160881,#160882),(#160883,#160884,#160885,#160886,#160887,#160888,
#160889,#160890,#160891),(#160892,#160893,#160894,#160895,#160896,#160897,
#160898,#160899,#160900),(#160901,#160902,#160903,#160904,#160905,#160906,
#160907,#160908,#160909),(#160910,#160911,#160912,#160913,#160914,#160915,
#160916,#160917,#160918),(#160919,#160920,#160921,#160922,#160923,#160924,
#160925,#160926,#160927),(#160928,#160929,#160930,#160931,#160932,#160933,
#160934,#160935,#160936),(#160937,#160938,#160939,#160940,#160941,#160942,
#160943,#160944,#160945),(#160946,#160947,#160948,#160949,#160950,#160951,
#160952,#160953,#160954),(#160955,#160956,#160957,#160958,#160959,#160960,
#160961,#160962,#160963),(#160964,#160965,#160966,#160967,#160968,#160969,
#160970,#160971,#160972),(#160973,#160974,#160975,#160976,#160977,#160978,
#160979,#160980,#160981),(#160982,#160983,#160984,#160985,#160986,#160987,
#160988,#160989,#160990),(#160991,#160992,#160993,#160994,#160995,#160996,
#160997,#160998,#160999),(#161000,#161001,#161002,#161003,#161004,#161005,
#161006,#161007,#161008),(#161009,#161010,#161011,#161012,#161013,#161014,
#161015,#161016,#161017),(#161018,#161019,#161020,#161021,#161022,#161023,
#161024,#161025,#161026),(#161027,#161028,#161029,#161030,#161031,#161032,
#161033,#161034,#161035),(#161036,#161037,#161038,#161039,#161040,#161041,
#161042,#161043,#161044),(#161045,#161046,#161047,#161048,#161049,#161050,
#161051,#161052,#161053),(#161054,#161055,#161056,#161057,#161058,#161059,
#161060,#161061,#161062),(#161063,#161064,#161065,#161066,#161067,#161068,
#161069,#161070,#161071),(#161072,#161073,#161074,#161075,#161076,#161077,
#161078,#161079,#161080),(#161081,#161082,#161083,#161084,#161085,#161086,
#161087,#161088,#161089),(#161090,#161091,#161092,#161093,#161094,#161095,
#161096,#161097,#161098),(#161099,#161100,#161101,#161102,#161103,#161104,
#161105,#161106,#161107),(#161108,#161109,#161110,#161111,#161112,#161113,
#161114,#161115,#161116),(#161117,#161118,#161119,#161120,#161121,#161122,
#161123,#161124,#161125),(#161126,#161127,#161128,#161129,#161130,#161131,
#161132,#161133,#161134),(#161135,#161136,#161137,#161138,#161139,#161140,
#161141,#161142,#161143),(#161144,#161145,#161146,#161147,#161148,#161149,
#161150,#161151,#161152),(#161153,#161154,#161155,#161156,#161157,#161158,
#161159,#161160,#161161),(#161162,#161163,#161164,#161165,#161166,#161167,
#161168,#161169,#161170),(#161171,#161172,#161173,#161174,#161175,#161176,
#161177,#161178,#161179),(#161180,#161181,#161182,#161183,#161184,#161185,
#161186,#161187,#161188),(#161189,#161190,#161191,#161192,#161193,#161194,
#161195,#161196,#161197),(#161198,#161199,#161200,#161201,#161202,#161203,
#161204,#161205,#161206),(#161207,#161208,#161209,#161210,#161211,#161212,
#161213,#161214,#161215),(#161216,#161217,#161218,#161219,#161220,#161221,
#161222,#161223,#161224),(#161225,#161226,#161227,#161228,#161229,#161230,
#161231,#161232,#161233),(#161234,#161235,#161236,#161237,#161238,#161239,
#161240,#161241,#161242),(#161243,#161244,#161245,#161246,#161247,#161248,
#161249,#161250,#161251),(#161252,#161253,#161254,#161255,#161256,#161257,
#161258,#161259,#161260),(#161261,#161262,#161263,#161264,#161265,#161266,
#161267,#161268,#161269),(#161270,#161271,#161272,#161273,#161274,#161275,
#161276,#161277,#161278),(#161279,#161280,#161281,#161282,#161283,#161284,
#161285,#161286,#161287),(#161288,#161289,#161290,#161291,#161292,#161293,
#161294,#161295,#161296),(#161297,#161298,#161299,#161300,#161301,#161302,
#161303,#161304,#161305),(#161306,#161307,#161308,#161309,#161310,#161311,
#161312,#161313,#161314),(#161315,#161316,#161317,#161318,#161319,#161320,
#161321,#161322,#161323),(#161324,#161325,#161326,#161327,#161328,#161329,
#161330,#161331,#161332),(#161333,#161334,#161335,#161336,#161337,#161338,
#161339,#161340,#161341),(#161342,#161343,#161344,#161345,#161346,#161347,
#161348,#161349,#161350),(#161351,#161352,#161353,#161354,#161355,#161356,
#161357,#161358,#161359),(#161360,#161361,#161362,#161363,#161364,#161365,
#161366,#161367,#161368),(#161369,#161370,#161371,#161372,#161373,#161374,
#161375,#161376,#161377),(#161378,#161379,#161380,#161381,#161382,#161383,
#161384,#161385,#161386),(#161387,#161388,#161389,#161390,#161391,#161392,
#161393,#161394,#161395),(#161396,#161397,#161398,#161399,#161400,#161401,
#161402,#161403,#161404),(#161405,#161406,#161407,#161408,#161409,#161410,
#161411,#161412,#161413),(#161414,#161415,#161416,#161417,#161418,#161419,
#161420,#161421,#161422),(#161423,#161424,#161425,#161426,#161427,#161428,
#161429,#161430,#161431),(#161432,#161433,#161434,#161435,#161436,#161437,
#161438,#161439,#161440),(#161441,#161442,#161443,#161444,#161445,#161446,
#161447,#161448,#161449),(#161450,#161451,#161452,#161453,#161454,#161455,
#161456,#161457,#161458),(#161459,#161460,#161461,#161462,#161463,#161464,
#161465,#161466,#161467),(#161468,#161469,#161470,#161471,#161472,#161473,
#161474,#161475,#161476),(#161477,#161478,#161479,#161480,#161481,#161482,
#161483,#161484,#161485),(#161486,#161487,#161488,#161489,#161490,#161491,
#161492,#161493,#161494),(#161495,#161496,#161497,#161498,#161499,#161500,
#161501,#161502,#161503),(#161504,#161505,#161506,#161507,#161508,#161509,
#161510,#161511,#161512),(#161513,#161514,#161515,#161516,#161517,#161518,
#161519,#161520,#161521),(#161522,#161523,#161524,#161525,#161526,#161527,
#161528,#161529,#161530),(#161531,#161532,#161533,#161534,#161535,#161536,
#161537,#161538,#161539),(#161540,#161541,#161542,#161543,#161544,#161545,
#161546,#161547,#161548),(#161549,#161550,#161551,#161552,#161553,#161554,
#161555,#161556,#161557),(#161558,#161559,#161560,#161561,#161562,#161563,
#161564,#161565,#161566),(#161567,#161568,#161569,#161570,#161571,#161572,
#161573,#161574,#161575),(#161576,#161577,#161578,#161579,#161580,#161581,
#161582,#161583,#161584),(#161585,#161586,#161587,#161588,#161589,#161590,
#161591,#161592,#161593),(#161594,#161595,#161596,#161597,#161598,#161599,
#161600,#161601,#161602),(#161603,#161604,#161605,#161606,#161607,#161608,
#161609,#161610,#161611),(#161612,#161613,#161614,#161615,#161616,#161617,
#161618,#161619,#161620),(#161621,#161622,#161623,#161624,#161625,#161626,
#161627,#161628,#161629),(#161630,#161631,#161632,#161633,#161634,#161635,
#161636,#161637,#161638),(#161639,#161640,#161641,#161642,#161643,#161644,
#161645,#161646,#161647),(#161648,#161649,#161650,#161651,#161652,#161653,
#161654,#161655,#161656),(#161657,#161658,#161659,#161660,#161661,#161662,
#161663,#161664,#161665),(#161666,#161667,#161668,#161669,#161670,#161671,
#161672,#161673,#161674),(#161675,#161676,#161677,#161678,#161679,#161680,
#161681,#161682,#161683),(#161684,#161685,#161686,#161687,#161688,#161689,
#161690,#161691,#161692),(#161693,#161694,#161695,#161696,#161697,#161698,
#161699,#161700,#161701),(#161702,#161703,#161704,#161705,#161706,#161707,
#161708,#161709,#161710),(#161711,#161712,#161713,#161714,#161715,#161716,
#161717,#161718,#161719),(#161720,#161721,#161722,#161723,#161724,#161725,
#161726,#161727,#161728),(#161729,#161730,#161731,#161732,#161733,#161734,
#161735,#161736,#161737),(#161738,#161739,#161740,#161741,#161742,#161743,
#161744,#161745,#161746),(#161747,#161748,#161749,#161750,#161751,#161752,
#161753,#161754,#161755),(#161756,#161757,#161758,#161759,#161760,#161761,
#161762,#161763,#161764),(#161765,#161766,#161767,#161768,#161769,#161770,
#161771,#161772,#161773),(#161774,#161775,#161776,#161777,#161778,#161779,
#161780,#161781,#161782),(#161783,#161784,#161785,#161786,#161787,#161788,
#161789,#161790,#161791),(#161792,#161793,#161794,#161795,#161796,#161797,
#161798,#161799,#161800),(#161801,#161802,#161803,#161804,#161805,#161806,
#161807,#161808,#161809),(#161810,#161811,#161812,#161813,#161814,#161815,
#161816,#161817,#161818),(#161819,#161820,#161821,#161822,#161823,#161824,
#161825,#161826,#161827),(#161828,#161829,#161830,#161831,#161832,#161833,
#161834,#161835,#161836),(#161837,#161838,#161839,#161840,#161841,#161842,
#161843,#161844,#161845),(#161846,#161847,#161848,#161849,#161850,#161851,
#161852,#161853,#161854),(#161855,#161856,#161857,#161858,#161859,#161860,
#161861,#161862,#161863),(#161864,#161865,#161866,#161867,#161868,#161869,
#161870,#161871,#161872),(#161873,#161874,#161875,#161876,#161877,#161878,
#161879,#161880,#161881),(#161882,#161883,#161884,#161885,#161886,#161887,
#161888,#161889,#161890),(#161891,#161892,#161893,#161894,#161895,#161896,
#161897,#161898,#161899),(#161900,#161901,#161902,#161903,#161904,#161905,
#161906,#161907,#161908),(#161909,#161910,#161911,#161912,#161913,#161914,
#161915,#161916,#161917),(#161918,#161919,#161920,#161921,#161922,#161923,
#161924,#161925,#161926),(#161927,#161928,#161929,#161930,#161931,#161932,
#161933,#161934,#161935),(#161936,#161937,#161938,#161939,#161940,#161941,
#161942,#161943,#161944),(#161945,#161946,#161947,#161948,#161949,#161950,
#161951,#161952,#161953),(#161954,#161955,#161956,#161957,#161958,#161959,
#161960,#161961,#161962),(#161963,#161964,#161965,#161966,#161967,#161968,
#161969,#161970,#161971),(#161972,#161973,#161974,#161975,#161976,#161977,
#161978,#161979,#161980),(#161981,#161982,#161983,#161984,#161985,#161986,
#161987,#161988,#161989),(#161990,#161991,#161992,#161993,#161994,#161995,
#161996,#161997,#161998),(#161999,#162000,#162001,#162002,#162003,#162004,
#162005,#162006,#162007),(#162008,#162009,#162010,#162011,#162012,#162013,
#162014,#162015,#162016),(#162017,#162018,#162019,#162020,#162021,#162022,
#162023,#162024,#162025),(#162026,#162027,#162028,#162029,#162030,#162031,
#162032,#162033,#162034),(#162035,#162036,#162037,#162038,#162039,#162040,
#162041,#162042,#162043),(#162044,#162045,#162046,#162047,#162048,#162049,
#162050,#162051,#162052),(#162053,#162054,#162055,#162056,#162057,#162058,
#162059,#162060,#162061),(#162062,#162063,#162064,#162065,#162066,#162067,
#162068,#162069,#162070),(#162071,#162072,#162073,#162074,#162075,#162076,
#162077,#162078,#162079),(#162080,#162081,#162082,#162083,#162084,#162085,
#162086,#162087,#162088),(#162089,#162090,#162091,#162092,#162093,#162094,
#162095,#162096,#162097),(#162098,#162099,#162100,#162101,#162102,#162103,
#162104,#162105,#162106),(#162107,#162108,#162109,#162110,#162111,#162112,
#162113,#162114,#162115),(#162116,#162117,#162118,#162119,#162120,#162121,
#162122,#162123,#162124),(#162125,#162126,#162127,#162128,#162129,#162130,
#162131,#162132,#162133),(#162134,#162135,#162136,#162137,#162138,#162139,
#162140,#162141,#162142),(#162143,#162144,#162145,#162146,#162147,#162148,
#162149,#162150,#162151),(#162152,#162153,#162154,#162155,#162156,#162157,
#162158,#162159,#162160),(#162161,#162162,#162163,#162164,#162165,#162166,
#162167,#162168,#162169),(#162170,#162171,#162172,#162173,#162174,#162175,
#162176,#162177,#162178),(#162179,#162180,#162181,#162182,#162183,#162184,
#162185,#162186,#162187),(#162188,#162189,#162190,#162191,#162192,#162193,
#162194,#162195,#162196),(#162197,#162198,#162199,#162200,#162201,#162202,
#162203,#162204,#162205),(#162206,#162207,#162208,#162209,#162210,#162211,
#162212,#162213,#162214),(#162215,#162216,#162217,#162218,#162219,#162220,
#162221,#162222,#162223),(#162224,#162225,#162226,#162227,#162228,#162229,
#162230,#162231,#162232),(#162233,#162234,#162235,#162236,#162237,#162238,
#162239,#162240,#162241),(#162242,#162243,#162244,#162245,#162246,#162247,
#162248,#162249,#162250),(#162251,#162252,#162253,#162254,#162255,#162256,
#162257,#162258,#162259),(#162260,#162261,#162262,#162263,#162264,#162265,
#162266,#162267,#162268),(#162269,#162270,#162271,#162272,#162273,#162274,
#162275,#162276,#162277),(#162278,#162279,#162280,#162281,#162282,#162283,
#162284,#162285,#162286),(#162287,#162288,#162289,#162290,#162291,#162292,
#162293,#162294,#162295),(#162296,#162297,#162298,#162299,#162300,#162301,
#162302,#162303,#162304),(#162305,#162306,#162307,#162308,#162309,#162310,
#162311,#162312,#162313),(#162314,#162315,#162316,#162317,#162318,#162319,
#162320,#162321,#162322),(#162323,#162324,#162325,#162326,#162327,#162328,
#162329,#162330,#162331),(#162332,#162333,#162334,#162335,#162336,#162337,
#162338,#162339,#162340),(#162341,#162342,#162343,#162344,#162345,#162346,
#162347,#162348,#162349),(#162350,#162351,#162352,#162353,#162354,#162355,
#162356,#162357,#162358),(#162359,#162360,#162361,#162362,#162363,#162364,
#162365,#162366,#162367),(#162368,#162369,#162370,#162371,#162372,#162373,
#162374,#162375,#162376),(#162377,#162378,#162379,#162380,#162381,#162382,
#162383,#162384,#162385),(#162386,#162387,#162388,#162389,#162390,#162391,
#162392,#162393,#162394),(#162395,#162396,#162397,#162398,#162399,#162400,
#162401,#162402,#162403),(#162404,#162405,#162406,#162407,#162408,#162409,
#162410,#162411,#162412),(#162413,#162414,#162415,#162416,#162417,#162418,
#162419,#162420,#162421),(#162422,#162423,#162424,#162425,#162426,#162427,
#162428,#162429,#162430),(#162431,#162432,#162433,#162434,#162435,#162436,
#162437,#162438,#162439),(#162440,#162441,#162442,#162443,#162444,#162445,
#162446,#162447,#162448),(#162449,#162450,#162451,#162452,#162453,#162454,
#162455,#162456,#162457),(#162458,#162459,#162460,#162461,#162462,#162463,
#162464,#162465,#162466),(#162467,#162468,#162469,#162470,#162471,#162472,
#162473,#162474,#162475),(#162476,#162477,#162478,#162479,#162480,#162481,
#162482,#162483,#162484),(#162485,#162486,#162487,#162488,#162489,#162490,
#162491,#162492,#162493),(#162494,#162495,#162496,#162497,#162498,#162499,
#162500,#162501,#162502),(#162503,#162504,#162505,#162506,#162507,#162508,
#162509,#162510,#162511),(#162512,#162513,#162514,#162515,#162516,#162517,
#162518,#162519,#162520),(#162521,#162522,#162523,#162524,#162525,#162526,
#162527,#162528,#162529),(#162530,#162531,#162532,#162533,#162534,#162535,
#162536,#162537,#162538),(#162539,#162540,#162541,#162542,#162543,#162544,
#162545,#162546,#162547),(#162548,#162549,#162550,#162551,#162552,#162553,
#162554,#162555,#162556),(#162557,#162558,#162559,#162560,#162561,#162562,
#162563,#162564,#162565),(#162566,#162567,#162568,#162569,#162570,#162571,
#162572,#162573,#162574),(#162575,#162576,#162577,#162578,#162579,#162580,
#162581,#162582,#162583),(#162584,#162585,#162586,#162587,#162588,#162589,
#162590,#162591,#162592),(#162593,#162594,#162595,#162596,#162597,#162598,
#162599,#162600,#162601),(#162602,#162603,#162604,#162605,#162606,#162607,
#162608,#162609,#162610),(#162611,#162612,#162613,#162614,#162615,#162616,
#162617,#162618,#162619),(#162620,#162621,#162622,#162623,#162624,#162625,
#162626,#162627,#162628),(#162629,#162630,#162631,#162632,#162633,#162634,
#162635,#162636,#162637),(#162638,#162639,#162640,#162641,#162642,#162643,
#162644,#162645,#162646),(#162647,#162648,#162649,#162650,#162651,#162652,
#162653,#162654,#162655),(#162656,#162657,#162658,#162659,#162660,#162661,
#162662,#162663,#162664),(#162665,#162666,#162667,#162668,#162669,#162670,
#162671,#162672,#162673),(#162674,#162675,#162676,#162677,#162678,#162679,
#162680,#162681,#162682),(#162683,#162684,#162685,#162686,#162687,#162688,
#162689,#162690,#162691),(#162692,#162693,#162694,#162695,#162696,#162697,
#162698,#162699,#162700),(#162701,#162702,#162703,#162704,#162705,#162706,
#162707,#162708,#162709),(#162710,#162711,#162712,#162713,#162714,#162715,
#162716,#162717,#162718),(#162719,#162720,#162721,#162722,#162723,#162724,
#162725,#162726,#162727),(#162728,#162729,#162730,#162731,#162732,#162733,
#162734,#162735,#162736),(#162737,#162738,#162739,#162740,#162741,#162742,
#162743,#162744,#162745),(#162746,#162747,#162748,#162749,#162750,#162751,
#162752,#162753,#162754),(#162755,#162756,#162757,#162758,#162759,#162760,
#162761,#162762,#162763),(#162764,#162765,#162766,#162767,#162768,#162769,
#162770,#162771,#162772),(#162773,#162774,#162775,#162776,#162777,#162778,
#162779,#162780,#162781),(#162782,#162783,#162784,#162785,#162786,#162787,
#162788,#162789,#162790),(#162791,#162792,#162793,#162794,#162795,#162796,
#162797,#162798,#162799),(#162800,#162801,#162802,#162803,#162804,#162805,
#162806,#162807,#162808),(#162809,#162810,#162811,#162812,#162813,#162814,
#162815,#162816,#162817),(#162818,#162819,#162820,#162821,#162822,#162823,
#162824,#162825,#162826),(#162827,#162828,#162829,#162830,#162831,#162832,
#162833,#162834,#162835),(#162836,#162837,#162838,#162839,#162840,#162841,
#162842,#162843,#162844),(#162845,#162846,#162847,#162848,#162849,#162850,
#162851,#162852,#162853),(#162854,#162855,#162856,#162857,#162858,#162859,
#162860,#162861,#162862),(#162863,#162864,#162865,#162866,#162867,#162868,
#162869,#162870,#162871),(#162872,#162873,#162874,#162875,#162876,#162877,
#162878,#162879,#162880),(#162881,#162882,#162883,#162884,#162885,#162886,
#162887,#162888,#162889),(#162890,#162891,#162892,#162893,#162894,#162895,
#162896,#162897,#162898),(#162899,#162900,#162901,#162902,#162903,#162904,
#162905,#162906,#162907),(#162908,#162909,#162910,#162911,#162912,#162913,
#162914,#162915,#162916),(#162917,#162918,#162919,#162920,#162921,#162922,
#162923,#162924,#162925),(#162926,#162927,#162928,#162929,#162930,#162931,
#162932,#162933,#162934),(#162935,#162936,#162937,#162938,#162939,#162940,
#162941,#162942,#162943),(#162944,#162945,#162946,#162947,#162948,#162949,
#162950,#162951,#162952),(#162953,#162954,#162955,#162956,#162957,#162958,
#162959,#162960,#162961),(#162962,#162963,#162964,#162965,#162966,#162967,
#162968,#162969,#162970),(#162971,#162972,#162973,#162974,#162975,#162976,
#162977,#162978,#162979),(#162980,#162981,#162982,#162983,#162984,#162985,
#162986,#162987,#162988),(#162989,#162990,#162991,#162992,#162993,#162994,
#162995,#162996,#162997),(#162998,#162999,#163000,#163001,#163002,#163003,
#163004,#163005,#163006),(#163007,#163008,#163009,#163010,#163011,#163012,
#163013,#163014,#163015),(#163016,#163017,#163018,#163019,#163020,#163021,
#163022,#163023,#163024),(#163025,#163026,#163027,#163028,#163029,#163030,
#163031,#163032,#163033),(#163034,#163035,#163036,#163037,#163038,#163039,
#163040,#163041,#163042),(#163043,#163044,#163045,#163046,#163047,#163048,
#163049,#163050,#163051),(#163052,#163053,#163054,#163055,#163056,#163057,
#163058,#163059,#163060),(#163061,#163062,#163063,#163064,#163065,#163066,
#163067,#163068,#163069),(#163070,#163071,#163072,#163073,#163074,#163075,
#163076,#163077,#163078),(#163079,#163080,#163081,#163082,#163083,#163084,
#163085,#163086,#163087),(#163088,#163089,#163090,#163091,#163092,#163093,
#163094,#163095,#163096),(#163097,#163098,#163099,#163100,#163101,#163102,
#163103,#163104,#163105),(#163106,#163107,#163108,#163109,#163110,#163111,
#163112,#163113,#163114),(#163115,#163116,#163117,#163118,#163119,#163120,
#163121,#163122,#163123),(#163124,#163125,#163126,#163127,#163128,#163129,
#163130,#163131,#163132),(#163133,#163134,#163135,#163136,#163137,#163138,
#163139,#163140,#163141),(#163142,#163143,#163144,#163145,#163146,#163147,
#163148,#163149,#163150),(#163151,#163152,#163153,#163154,#163155,#163156,
#163157,#163158,#163159),(#163160,#163161,#163162,#163163,#163164,#163165,
#163166,#163167,#163168),(#163169,#163170,#163171,#163172,#163173,#163174,
#163175,#163176,#163177),(#163178,#163179,#163180,#163181,#163182,#163183,
#163184,#163185,#163186),(#163187,#163188,#163189,#163190,#163191,#163192,
#163193,#163194,#163195),(#163196,#163197,#163198,#163199,#163200,#163201,
#163202,#163203,#163204),(#163205,#163206,#163207,#163208,#163209,#163210,
#163211,#163212,#163213),(#163214,#163215,#163216,#163217,#163218,#163219,
#163220,#163221,#163222),(#163223,#163224,#163225,#163226,#163227,#163228,
#163229,#163230,#163231),(#163232,#163233,#163234,#163235,#163236,#163237,
#163238,#163239,#163240),(#163241,#163242,#163243,#163244,#163245,#163246,
#163247,#163248,#163249),(#163250,#163251,#163252,#163253,#163254,#163255,
#163256,#163257,#163258),(#163259,#163260,#163261,#163262,#163263,#163264,
#163265,#163266,#163267),(#163268,#163269,#163270,#163271,#163272,#163273,
#163274,#163275,#163276),(#163277,#163278,#163279,#163280,#163281,#163282,
#163283,#163284,#163285),(#163286,#163287,#163288,#163289,#163290,#163291,
#163292,#163293,#163294),(#163295,#163296,#163297,#163298,#163299,#163300,
#163301,#163302,#163303),(#163304,#163305,#163306,#163307,#163308,#163309,
#163310,#163311,#163312),(#163313,#163314,#163315,#163316,#163317,#163318,
#163319,#163320,#163321),(#163322,#163323,#163324,#163325,#163326,#163327,
#163328,#163329,#163330),(#163331,#163332,#163333,#163334,#163335,#163336,
#163337,#163338,#163339),(#163340,#163341,#163342,#163343,#163344,#163345,
#163346,#163347,#163348),(#163349,#163350,#163351,#163352,#163353,#163354,
#163355,#163356,#163357),(#163358,#163359,#163360,#163361,#163362,#163363,
#163364,#163365,#163366),(#163367,#163368,#163369,#163370,#163371,#163372,
#163373,#163374,#163375),(#163376,#163377,#163378,#163379,#163380,#163381,
#163382,#163383,#163384),(#163385,#163386,#163387,#163388,#163389,#163390,
#163391,#163392,#163393),(#163394,#163395,#163396,#163397,#163398,#163399,
#163400,#163401,#163402),(#163403,#163404,#163405,#163406,#163407,#163408,
#163409,#163410,#163411),(#163412,#163413,#163414,#163415,#163416,#163417,
#163418,#163419,#163420),(#163421,#163422,#163423,#163424,#163425,#163426,
#163427,#163428,#163429),(#163430,#163431,#163432,#163433,#163434,#163435,
#163436,#163437,#163438),(#163439,#163440,#163441,#163442,#163443,#163444,
#163445,#163446,#163447),(#163448,#163449,#163450,#163451,#163452,#163453,
#163454,#163455,#163456),(#163457,#163458,#163459,#163460,#163461,#163462,
#163463,#163464,#163465),(#163466,#163467,#163468,#163469,#163470,#163471,
#163472,#163473,#163474),(#163475,#163476,#163477,#163478,#163479,#163480,
#163481,#163482,#163483),(#163484,#163485,#163486,#163487,#163488,#163489,
#163490,#163491,#163492),(#163493,#163494,#163495,#163496,#163497,#163498,
#163499,#163500,#163501),(#163502,#163503,#163504,#163505,#163506,#163507,
#163508,#163509,#163510),(#163511,#163512,#163513,#163514,#163515,#163516,
#163517,#163518,#163519),(#163520,#163521,#163522,#163523,#163524,#163525,
#163526,#163527,#163528),(#163529,#163530,#163531,#163532,#163533,#163534,
#163535,#163536,#163537),(#163538,#163539,#163540,#163541,#163542,#163543,
#163544,#163545,#163546),(#163547,#163548,#163549,#163550,#163551,#163552,
#163553,#163554,#163555),(#163556,#163557,#163558,#163559,#163560,#163561,
#163562,#163563,#163564),(#163565,#163566,#163567,#163568,#163569,#163570,
#163571,#163572,#163573),(#163574,#163575,#163576,#163577,#163578,#163579,
#163580,#163581,#163582),(#163583,#163584,#163585,#163586,#163587,#163588,
#163589,#163590,#163591),(#163592,#163593,#163594,#163595,#163596,#163597,
#163598,#163599,#163600),(#163601,#163602,#163603,#163604,#163605,#163606,
#163607,#163608,#163609),(#163610,#163611,#163612,#163613,#163614,#163615,
#163616,#163617,#163618),(#163619,#163620,#163621,#163622,#163623,#163624,
#163625,#163626,#163627),(#163628,#163629,#163630,#163631,#163632,#163633,
#163634,#163635,#163636),(#163637,#163638,#163639,#163640,#163641,#163642,
#163643,#163644,#163645),(#163646,#163647,#163648,#163649,#163650,#163651,
#163652,#163653,#163654),(#163655,#163656,#163657,#163658,#163659,#163660,
#163661,#163662,#163663),(#163664,#163665,#163666,#163667,#163668,#163669,
#163670,#163671,#163672),(#163673,#163674,#163675,#163676,#163677,#163678,
#163679,#163680,#163681),(#163682,#163683,#163684,#163685,#163686,#163687,
#163688,#163689,#163690),(#163691,#163692,#163693,#163694,#163695,#163696,
#163697,#163698,#163699),(#163700,#163701,#163702,#163703,#163704,#163705,
#163706,#163707,#163708),(#163709,#163710,#163711,#163712,#163713,#163714,
#163715,#163716,#163717),(#163718,#163719,#163720,#163721,#163722,#163723,
#163724,#163725,#163726),(#163727,#163728,#163729,#163730,#163731,#163732,
#163733,#163734,#163735),(#163736,#163737,#163738,#163739,#163740,#163741,
#163742,#163743,#163744),(#163745,#163746,#163747,#163748,#163749,#163750,
#163751,#163752,#163753),(#163754,#163755,#163756,#163757,#163758,#163759,
#163760,#163761,#163762),(#163763,#163764,#163765,#163766,#163767,#163768,
#163769,#163770,#163771),(#163772,#163773,#163774,#163775,#163776,#163777,
#163778,#163779,#163780),(#163781,#163782,#163783,#163784,#163785,#163786,
#163787,#163788,#163789),(#163790,#163791,#163792,#163793,#163794,#163795,
#163796,#163797,#163798),(#163799,#163800,#163801,#163802,#163803,#163804,
#163805,#163806,#163807),(#163808,#163809,#163810,#163811,#163812,#163813,
#163814,#163815,#163816),(#163817,#163818,#163819,#163820,#163821,#163822,
#163823,#163824,#163825),(#163826,#163827,#163828,#163829,#163830,#163831,
#163832,#163833,#163834),(#163835,#163836,#163837,#163838,#163839,#163840,
#163841,#163842,#163843),(#163844,#163845,#163846,#163847,#163848,#163849,
#163850,#163851,#163852),(#163853,#163854,#163855,#163856,#163857,#163858,
#163859,#163860,#163861),(#163862,#163863,#163864,#163865,#163866,#163867,
#163868,#163869,#163870),(#163871,#163872,#163873,#163874,#163875,#163876,
#163877,#163878,#163879),(#163880,#163881,#163882,#163883,#163884,#163885,
#163886,#163887,#163888),(#163889,#163890,#163891,#163892,#163893,#163894,
#163895,#163896,#163897),(#163898,#163899,#163900,#163901,#163902,#163903,
#163904,#163905,#163906),(#163907,#163908,#163909,#163910,#163911,#163912,
#163913,#163914,#163915),(#163916,#163917,#163918,#163919,#163920,#163921,
#163922,#163923,#163924),(#163925,#163926,#163927,#163928,#163929,#163930,
#163931,#163932,#163933),(#163934,#163935,#163936,#163937,#163938,#163939,
#163940,#163941,#163942),(#163943,#163944,#163945,#163946,#163947,#163948,
#163949,#163950,#163951),(#163952,#163953,#163954,#163955,#163956,#163957,
#163958,#163959,#163960),(#163961,#163962,#163963,#163964,#163965,#163966,
#163967,#163968,#163969),(#163970,#163971,#163972,#163973,#163974,#163975,
#163976,#163977,#163978),(#163979,#163980,#163981,#163982,#163983,#163984,
#163985,#163986,#163987),(#163988,#163989,#163990,#163991,#163992,#163993,
#163994,#163995,#163996),(#163997,#163998,#163999,#164000,#164001,#164002,
#164003,#164004,#164005),(#164006,#164007,#164008,#164009,#164010,#164011,
#164012,#164013,#164014),(#164015,#164016,#164017,#164018,#164019,#164020,
#164021,#164022,#164023),(#164024,#164025,#164026,#164027,#164028,#164029,
#164030,#164031,#164032),(#164033,#164034,#164035,#164036,#164037,#164038,
#164039,#164040,#164041),(#164042,#164043,#164044,#164045,#164046,#164047,
#164048,#164049,#164050),(#164051,#164052,#164053,#164054,#164055,#164056,
#164057,#164058,#164059),(#164060,#164061,#164062,#164063,#164064,#164065,
#164066,#164067,#164068),(#164069,#164070,#164071,#164072,#164073,#164074,
#164075,#164076,#164077),(#164078,#164079,#164080,#164081,#164082,#164083,
#164084,#164085,#164086),(#164087,#164088,#164089,#164090,#164091,#164092,
#164093,#164094,#164095),(#164096,#164097,#164098,#164099,#164100,#164101,
#164102,#164103,#164104),(#164105,#164106,#164107,#164108,#164109,#164110,
#164111,#164112,#164113),(#164114,#164115,#164116,#164117,#164118,#164119,
#164120,#164121,#164122),(#164123,#164124,#164125,#164126,#164127,#164128,
#164129,#164130,#164131),(#164132,#164133,#164134,#164135,#164136,#164137,
#164138,#164139,#164140),(#164141,#164142,#164143,#164144,#164145,#164146,
#164147,#164148,#164149),(#164150,#164151,#164152,#164153,#164154,#164155,
#164156,#164157,#164158),(#164159,#164160,#164161,#164162,#164163,#164164,
#164165,#164166,#164167),(#164168,#164169,#164170,#164171,#164172,#164173,
#164174,#164175,#164176),(#164177,#164178,#164179,#164180,#164181,#164182,
#164183,#164184,#164185),(#164186,#164187,#164188,#164189,#164190,#164191,
#164192,#164193,#164194),(#164195,#164196,#164197,#164198,#164199,#164200,
#164201,#164202,#164203),(#164204,#164205,#164206,#164207,#164208,#164209,
#164210,#164211,#164212),(#164213,#164214,#164215,#164216,#164217,#164218,
#164219,#164220,#164221),(#164222,#164223,#164224,#164225,#164226,#164227,
#164228,#164229,#164230),(#164231,#164232,#164233,#164234,#164235,#164236,
#164237,#164238,#164239),(#164240,#164241,#164242,#164243,#164244,#164245,
#164246,#164247,#164248),(#164249,#164250,#164251,#164252,#164253,#164254,
#164255,#164256,#164257),(#164258,#164259,#164260,#164261,#164262,#164263,
#164264,#164265,#164266),(#164267,#164268,#164269,#164270,#164271,#164272,
#164273,#164274,#164275),(#164276,#164277,#164278,#164279,#164280,#164281,
#164282,#164283,#164284),(#164285,#164286,#164287,#164288,#164289,#164290,
#164291,#164292,#164293),(#164294,#164295,#164296,#164297,#164298,#164299,
#164300,#164301,#164302),(#164303,#164304,#164305,#164306,#164307,#164308,
#164309,#164310,#164311),(#164312,#164313,#164314,#164315,#164316,#164317,
#164318,#164319,#164320),(#164321,#164322,#164323,#164324,#164325,#164326,
#164327,#164328,#164329),(#164330,#164331,#164332,#164333,#164334,#164335,
#164336,#164337,#164338),(#164339,#164340,#164341,#164342,#164343,#164344,
#164345,#164346,#164347),(#164348,#164349,#164350,#164351,#164352,#164353,
#164354,#164355,#164356),(#164357,#164358,#164359,#164360,#164361,#164362,
#164363,#164364,#164365),(#164366,#164367,#164368,#164369,#164370,#164371,
#164372,#164373,#164374),(#164375,#164376,#164377,#164378,#164379,#164380,
#164381,#164382,#164383),(#164384,#164385,#164386,#164387,#164388,#164389,
#164390,#164391,#164392),(#164393,#164394,#164395,#164396,#164397,#164398,
#164399,#164400,#164401),(#164402,#164403,#164404,#164405,#164406,#164407,
#164408,#164409,#164410),(#164411,#164412,#164413,#164414,#164415,#164416,
#164417,#164418,#164419),(#164420,#164421,#164422,#164423,#164424,#164425,
#164426,#164427,#164428),(#164429,#164430,#164431,#164432,#164433,#164434,
#164435,#164436,#164437),(#164438,#164439,#164440,#164441,#164442,#164443,
#164444,#164445,#164446),(#164447,#164448,#164449,#164450,#164451,#164452,
#164453,#164454,#164455),(#164456,#164457,#164458,#164459,#164460,#164461,
#164462,#164463,#164464),(#164465,#164466,#164467,#164468,#164469,#164470,
#164471,#164472,#164473),(#164474,#164475,#164476,#164477,#164478,#164479,
#164480,#164481,#164482),(#164483,#164484,#164485,#164486,#164487,#164488,
#164489,#164490,#164491),(#164492,#164493,#164494,#164495,#164496,#164497,
#164498,#164499,#164500),(#164501,#164502,#164503,#164504,#164505,#164506,
#164507,#164508,#164509),(#164510,#164511,#164512,#164513,#164514,#164515,
#164516,#164517,#164518),(#164519,#164520,#164521,#164522,#164523,#164524,
#164525,#164526,#164527),(#164528,#164529,#164530,#164531,#164532,#164533,
#164534,#164535,#164536),(#164537,#164538,#164539,#164540,#164541,#164542,
#164543,#164544,#164545),(#164546,#164547,#164548,#164549,#164550,#164551,
#164552,#164553,#164554),(#164555,#164556,#164557,#164558,#164559,#164560,
#164561,#164562,#164563),(#164564,#164565,#164566,#164567,#164568,#164569,
#164570,#164571,#164572),(#164573,#164574,#164575,#164576,#164577,#164578,
#164579,#164580,#164581),(#164582,#164583,#164584,#164585,#164586,#164587,
#164588,#164589,#164590),(#164591,#164592,#164593,#164594,#164595,#164596,
#164597,#164598,#164599),(#164600,#164601,#164602,#164603,#164604,#164605,
#164606,#164607,#164608),(#164609,#164610,#164611,#164612,#164613,#164614,
#164615,#164616,#164617),(#164618,#164619,#164620,#164621,#164622,#164623,
#164624,#164625,#164626),(#164627,#164628,#164629,#164630,#164631,#164632,
#164633,#164634,#164635),(#164636,#164637,#164638,#164639,#164640,#164641,
#164642,#164643,#164644),(#164645,#164646,#164647,#164648,#164649,#164650,
#164651,#164652,#164653),(#164654,#164655,#164656,#164657,#164658,#164659,
#164660,#164661,#164662),(#164663,#164664,#164665,#164666,#164667,#164668,
#164669,#164670,#164671),(#164672,#164673,#164674,#164675,#164676,#164677,
#164678,#164679,#164680),(#164681,#164682,#164683,#164684,#164685,#164686,
#164687,#164688,#164689),(#164690,#164691,#164692,#164693,#164694,#164695,
#164696,#164697,#164698),(#164699,#164700,#164701,#164702,#164703,#164704,
#164705,#164706,#164707),(#164708,#164709,#164710,#164711,#164712,#164713,
#164714,#164715,#164716),(#164717,#164718,#164719,#164720,#164721,#164722,
#164723,#164724,#164725),(#164726,#164727,#164728,#164729,#164730,#164731,
#164732,#164733,#164734),(#164735,#164736,#164737,#164738,#164739,#164740,
#164741,#164742,#164743),(#164744,#164745,#164746,#164747,#164748,#164749,
#164750,#164751,#164752),(#164753,#164754,#164755,#164756,#164757,#164758,
#164759,#164760,#164761),(#164762,#164763,#164764,#164765,#164766,#164767,
#164768,#164769,#164770),(#164771,#164772,#164773,#164774,#164775,#164776,
#164777,#164778,#164779),(#164780,#164781,#164782,#164783,#164784,#164785,
#164786,#164787,#164788),(#164789,#164790,#164791,#164792,#164793,#164794,
#164795,#164796,#164797),(#164798,#164799,#164800,#164801,#164802,#164803,
#164804,#164805,#164806),(#164807,#164808,#164809,#164810,#164811,#164812,
#164813,#164814,#164815),(#164816,#164817,#164818,#164819,#164820,#164821,
#164822,#164823,#164824),(#164825,#164826,#164827,#164828,#164829,#164830,
#164831,#164832,#164833),(#164834,#164835,#164836,#164837,#164838,#164839,
#164840,#164841,#164842),(#164843,#164844,#164845,#164846,#164847,#164848,
#164849,#164850,#164851),(#164852,#164853,#164854,#164855,#164856,#164857,
#164858,#164859,#164860),(#164861,#164862,#164863,#164864,#164865,#164866,
#164867,#164868,#164869),(#164870,#164871,#164872,#164873,#164874,#164875,
#164876,#164877,#164878),(#164879,#164880,#164881,#164882,#164883,#164884,
#164885,#164886,#164887),(#164888,#164889,#164890,#164891,#164892,#164893,
#164894,#164895,#164896),(#164897,#164898,#164899,#164900,#164901,#164902,
#164903,#164904,#164905),(#164906,#164907,#164908,#164909,#164910,#164911,
#164912,#164913,#164914),(#164915,#164916,#164917,#164918,#164919,#164920,
#164921,#164922,#164923),(#164924,#164925,#164926,#164927,#164928,#164929,
#164930,#164931,#164932),(#164933,#164934,#164935,#164936,#164937,#164938,
#164939,#164940,#164941),(#164942,#164943,#164944,#164945,#164946,#164947,
#164948,#164949,#164950),(#164951,#164952,#164953,#164954,#164955,#164956,
#164957,#164958,#164959),(#164960,#164961,#164962,#164963,#164964,#164965,
#164966,#164967,#164968),(#164969,#164970,#164971,#164972,#164973,#164974,
#164975,#164976,#164977),(#164978,#164979,#164980,#164981,#164982,#164983,
#164984,#164985,#164986),(#164987,#164988,#164989,#164990,#164991,#164992,
#164993,#164994,#164995),(#164996,#164997,#164998,#164999,#165000,#165001,
#165002,#165003,#165004),(#165005,#165006,#165007,#165008,#165009,#165010,
#165011,#165012,#165013),(#165014,#165015,#165016,#165017,#165018,#165019,
#165020,#165021,#165022),(#165023,#165024,#165025,#165026,#165027,#165028,
#165029,#165030,#165031),(#165032,#165033,#165034,#165035,#165036,#165037,
#165038,#165039,#165040),(#165041,#165042,#165043,#165044,#165045,#165046,
#165047,#165048,#165049),(#165050,#165051,#165052,#165053,#165054,#165055,
#165056,#165057,#165058),(#165059,#165060,#165061,#165062,#165063,#165064,
#165065,#165066,#165067),(#165068,#165069,#165070,#165071,#165072,#165073,
#165074,#165075,#165076),(#165077,#165078,#165079,#165080,#165081,#165082,
#165083,#165084,#165085),(#165086,#165087,#165088,#165089,#165090,#165091,
#165092,#165093,#165094),(#165095,#165096,#165097,#165098,#165099,#165100,
#165101,#165102,#165103),(#165104,#165105,#165106,#165107,#165108,#165109,
#165110,#165111,#165112),(#165113,#165114,#165115,#165116,#165117,#165118,
#165119,#165120,#165121),(#165122,#165123,#165124,#165125,#165126,#165127,
#165128,#165129,#165130),(#165131,#165132,#165133,#165134,#165135,#165136,
#165137,#165138,#165139),(#165140,#165141,#165142,#165143,#165144,#165145,
#165146,#165147,#165148),(#165149,#165150,#165151,#165152,#165153,#165154,
#165155,#165156,#165157),(#165158,#165159,#165160,#165161,#165162,#165163,
#165164,#165165,#165166),(#165167,#165168,#165169,#165170,#165171,#165172,
#165173,#165174,#165175),(#165176,#165177,#165178,#165179,#165180,#165181,
#165182,#165183,#165184),(#165185,#165186,#165187,#165188,#165189,#165190,
#165191,#165192,#165193),(#165194,#165195,#165196,#165197,#165198,#165199,
#165200,#165201,#165202),(#165203,#165204,#165205,#165206,#165207,#165208,
#165209,#165210,#165211),(#165212,#165213,#165214,#165215,#165216,#165217,
#165218,#165219,#165220),(#165221,#165222,#165223,#165224,#165225,#165226,
#165227,#165228,#165229),(#165230,#165231,#165232,#165233,#165234,#165235,
#165236,#165237,#165238),(#165239,#165240,#165241,#165242,#165243,#165244,
#165245,#165246,#165247),(#165248,#165249,#165250,#165251,#165252,#165253,
#165254,#165255,#165256),(#165257,#165258,#165259,#165260,#165261,#165262,
#165263,#165264,#165265),(#165266,#165267,#165268,#165269,#165270,#165271,
#165272,#165273,#165274),(#165275,#165276,#165277,#165278,#165279,#165280,
#165281,#165282,#165283),(#165284,#165285,#165286,#165287,#165288,#165289,
#165290,#165291,#165292),(#165293,#165294,#165295,#165296,#165297,#165298,
#165299,#165300,#165301),(#165302,#165303,#165304,#165305,#165306,#165307,
#165308,#165309,#165310),(#165311,#165312,#165313,#165314,#165315,#165316,
#165317,#165318,#165319),(#165320,#165321,#165322,#165323,#165324,#165325,
#165326,#165327,#165328),(#165329,#165330,#165331,#165332,#165333,#165334,
#165335,#165336,#165337),(#165338,#165339,#165340,#165341,#165342,#165343,
#165344,#165345,#165346),(#165347,#165348,#165349,#165350,#165351,#165352,
#165353,#165354,#165355),(#165356,#165357,#165358,#165359,#165360,#165361,
#165362,#165363,#165364),(#165365,#165366,#165367,#165368,#165369,#165370,
#165371,#165372,#165373),(#165374,#165375,#165376,#165377,#165378,#165379,
#165380,#165381,#165382),(#165383,#165384,#165385,#165386,#165387,#165388,
#165389,#165390,#165391),(#165392,#165393,#165394,#165395,#165396,#165397,
#165398,#165399,#165400),(#165401,#165402,#165403,#165404,#165405,#165406,
#165407,#165408,#165409),(#165410,#165411,#165412,#165413,#165414,#165415,
#165416,#165417,#165418),(#165419,#165420,#165421,#165422,#165423,#165424,
#165425,#165426,#165427),(#165428,#165429,#165430,#165431,#165432,#165433,
#165434,#165435,#165436),(#165437,#165438,#165439,#165440,#165441,#165442,
#165443,#165444,#165445),(#165446,#165447,#165448,#165449,#165450,#165451,
#165452,#165453,#165454),(#165455,#165456,#165457,#165458,#165459,#165460,
#165461,#165462,#165463),(#165464,#165465,#165466,#165467,#165468,#165469,
#165470,#165471,#165472),(#165473,#165474,#165475,#165476,#165477,#165478,
#165479,#165480,#165481),(#165482,#165483,#165484,#165485,#165486,#165487,
#165488,#165489,#165490),(#165491,#165492,#165493,#165494,#165495,#165496,
#165497,#165498,#165499),(#165500,#165501,#165502,#165503,#165504,#165505,
#165506,#165507,#165508),(#165509,#165510,#165511,#165512,#165513,#165514,
#165515,#165516,#165517),(#165518,#165519,#165520,#165521,#165522,#165523,
#165524,#165525,#165526),(#165527,#165528,#165529,#165530,#165531,#165532,
#165533,#165534,#165535),(#165536,#165537,#165538,#165539,#165540,#165541,
#165542,#165543,#165544),(#165545,#165546,#165547,#165548,#165549,#165550,
#165551,#165552,#165553),(#165554,#165555,#165556,#165557,#165558,#165559,
#165560,#165561,#165562),(#165563,#165564,#165565,#165566,#165567,#165568,
#165569,#165570,#165571),(#165572,#165573,#165574,#165575,#165576,#165577,
#165578,#165579,#165580),(#165581,#165582,#165583,#165584,#165585,#165586,
#165587,#165588,#165589),(#165590,#165591,#165592,#165593,#165594,#165595,
#165596,#165597,#165598),(#165599,#165600,#165601,#165602,#165603,#165604,
#165605,#165606,#165607),(#165608,#165609,#165610,#165611,#165612,#165613,
#165614,#165615,#165616),(#165617,#165618,#165619,#165620,#165621,#165622,
#165623,#165624,#165625),(#165626,#165627,#165628,#165629,#165630,#165631,
#165632,#165633,#165634),(#165635,#165636,#165637,#165638,#165639,#165640,
#165641,#165642,#165643),(#165644,#165645,#165646,#165647,#165648,#165649,
#165650,#165651,#165652),(#165653,#165654,#165655,#165656,#165657,#165658,
#165659,#165660,#165661),(#165662,#165663,#165664,#165665,#165666,#165667,
#165668,#165669,#165670),(#165671,#165672,#165673,#165674,#165675,#165676,
#165677,#165678,#165679),(#165680,#165681,#165682,#165683,#165684,#165685,
#165686,#165687,#165688),(#165689,#165690,#165691,#165692,#165693,#165694,
#165695,#165696,#165697),(#165698,#165699,#165700,#165701,#165702,#165703,
#165704,#165705,#165706),(#165707,#165708,#165709,#165710,#165711,#165712,
#165713,#165714,#165715),(#165716,#165717,#165718,#165719,#165720,#165721,
#165722,#165723,#165724),(#165725,#165726,#165727,#165728,#165729,#165730,
#165731,#165732,#165733),(#165734,#165735,#165736,#165737,#165738,#165739,
#165740,#165741,#165742),(#165743,#165744,#165745,#165746,#165747,#165748,
#165749,#165750,#165751),(#165752,#165753,#165754,#165755,#165756,#165757,
#165758,#165759,#165760),(#165761,#165762,#165763,#165764,#165765,#165766,
#165767,#165768,#165769),(#165770,#165771,#165772,#165773,#165774,#165775,
#165776,#165777,#165778),(#165779,#165780,#165781,#165782,#165783,#165784,
#165785,#165786,#165787),(#165788,#165789,#165790,#165791,#165792,#165793,
#165794,#165795,#165796),(#165797,#165798,#165799,#165800,#165801,#165802,
#165803,#165804,#165805),(#165806,#165807,#165808,#165809,#165810,#165811,
#165812,#165813,#165814),(#165815,#165816,#165817,#165818,#165819,#165820,
#165821,#165822,#165823),(#165824,#165825,#165826,#165827,#165828,#165829,
#165830,#165831,#165832),(#165833,#165834,#165835,#165836,#165837,#165838,
#165839,#165840,#165841),(#165842,#165843,#165844,#165845,#165846,#165847,
#165848,#165849,#165850),(#165851,#165852,#165853,#165854,#165855,#165856,
#165857,#165858,#165859),(#165860,#165861,#165862,#165863,#165864,#165865,
#165866,#165867,#165868),(#165869,#165870,#165871,#165872,#165873,#165874,
#165875,#165876,#165877),(#165878,#165879,#165880,#165881,#165882,#165883,
#165884,#165885,#165886),(#165887,#165888,#165889,#165890,#165891,#165892,
#165893,#165894,#165895),(#165896,#165897,#165898,#165899,#165900,#165901,
#165902,#165903,#165904),(#165905,#165906,#165907,#165908,#165909,#165910,
#165911,#165912,#165913),(#165914,#165915,#165916,#165917,#165918,#165919,
#165920,#165921,#165922),(#165923,#165924,#165925,#165926,#165927,#165928,
#165929,#165930,#165931),(#165932,#165933,#165934,#165935,#165936,#165937,
#165938,#165939,#165940),(#165941,#165942,#165943,#165944,#165945,#165946,
#165947,#165948,#165949),(#165950,#165951,#165952,#165953,#165954,#165955,
#165956,#165957,#165958),(#165959,#165960,#165961,#165962,#165963,#165964,
#165965,#165966,#165967),(#165968,#165969,#165970,#165971,#165972,#165973,
#165974,#165975,#165976),(#165977,#165978,#165979,#165980,#165981,#165982,
#165983,#165984,#165985),(#165986,#165987,#165988,#165989,#165990,#165991,
#165992,#165993,#165994),(#165995,#165996,#165997,#165998,#165999,#166000,
#166001,#166002,#166003),(#166004,#166005,#166006,#166007,#166008,#166009,
#166010,#166011,#166012),(#166013,#166014,#166015,#166016,#166017,#166018,
#166019,#166020,#166021),(#166022,#166023,#166024,#166025,#166026,#166027,
#166028,#166029,#166030),(#166031,#166032,#166033,#166034,#166035,#166036,
#166037,#166038,#166039),(#166040,#166041,#166042,#166043,#166044,#166045,
#166046,#166047,#166048),(#166049,#166050,#166051,#166052,#166053,#166054,
#166055,#166056,#166057),(#166058,#166059,#166060,#166061,#166062,#166063,
#166064,#166065,#166066),(#166067,#166068,#166069,#166070,#166071,#166072,
#166073,#166074,#166075),(#166076,#166077,#166078,#166079,#166080,#166081,
#166082,#166083,#166084),(#166085,#166086,#166087,#166088,#166089,#166090,
#166091,#166092,#166093),(#166094,#166095,#166096,#166097,#166098,#166099,
#166100,#166101,#166102),(#166103,#166104,#166105,#166106,#166107,#166108,
#166109,#166110,#166111),(#166112,#166113,#166114,#166115,#166116,#166117,
#166118,#166119,#166120),(#166121,#166122,#166123,#166124,#166125,#166126,
#166127,#166128,#166129),(#166130,#166131,#166132,#166133,#166134,#166135,
#166136,#166137,#166138),(#166139,#166140,#166141,#166142,#166143,#166144,
#166145,#166146,#166147),(#166148,#166149,#166150,#166151,#166152,#166153,
#166154,#166155,#166156),(#166157,#166158,#166159,#166160,#166161,#166162,
#166163,#166164,#166165),(#166166,#166167,#166168,#166169,#166170,#166171,
#166172,#166173,#166174),(#166175,#166176,#166177,#166178,#166179,#166180,
#166181,#166182,#166183),(#166184,#166185,#166186,#166187,#166188,#166189,
#166190,#166191,#166192),(#166193,#166194,#166195,#166196,#166197,#166198,
#166199,#166200,#166201),(#166202,#166203,#166204,#166205,#166206,#166207,
#166208,#166209,#166210),(#166211,#166212,#166213,#166214,#166215,#166216,
#166217,#166218,#166219),(#166220,#166221,#166222,#166223,#166224,#166225,
#166226,#166227,#166228),(#166229,#166230,#166231,#166232,#166233,#166234,
#166235,#166236,#166237),(#166238,#166239,#166240,#166241,#166242,#166243,
#166244,#166245,#166246),(#166247,#166248,#166249,#166250,#166251,#166252,
#166253,#166254,#166255),(#166256,#166257,#166258,#166259,#166260,#166261,
#166262,#166263,#166264),(#166265,#166266,#166267,#166268,#166269,#166270,
#166271,#166272,#166273),(#166274,#166275,#166276,#166277,#166278,#166279,
#166280,#166281,#166282),(#166283,#166284,#166285,#166286,#166287,#166288,
#166289,#166290,#166291),(#166292,#166293,#166294,#166295,#166296,#166297,
#166298,#166299,#166300),(#166301,#166302,#166303,#166304,#166305,#166306,
#166307,#166308,#166309),(#166310,#166311,#166312,#166313,#166314,#166315,
#166316,#166317,#166318),(#166319,#166320,#166321,#166322,#166323,#166324,
#166325,#166326,#166327),(#166328,#166329,#166330,#166331,#166332,#166333,
#166334,#166335,#166336),(#166337,#166338,#166339,#166340,#166341,#166342,
#166343,#166344,#166345),(#166346,#166347,#166348,#166349,#166350,#166351,
#166352,#166353,#166354),(#166355,#166356,#166357,#166358,#166359,#166360,
#166361,#166362,#166363),(#166364,#166365,#166366,#166367,#166368,#166369,
#166370,#166371,#166372),(#166373,#166374,#166375,#166376,#166377,#166378,
#166379,#166380,#166381),(#166382,#166383,#166384,#166385,#166386,#166387,
#166388,#166389,#166390),(#166391,#166392,#166393,#166394,#166395,#166396,
#166397,#166398,#166399),(#166400,#166401,#166402,#166403,#166404,#166405,
#166406,#166407,#166408),(#166409,#166410,#166411,#166412,#166413,#166414,
#166415,#166416,#166417),(#166418,#166419,#166420,#166421,#166422,#166423,
#166424,#166425,#166426),(#166427,#166428,#166429,#166430,#166431,#166432,
#166433,#166434,#166435),(#166436,#166437,#166438,#166439,#166440,#166441,
#166442,#166443,#166444),(#166445,#166446,#166447,#166448,#166449,#166450,
#166451,#166452,#166453),(#166454,#166455,#166456,#166457,#166458,#166459,
#166460,#166461,#166462),(#166463,#166464,#166465,#166466,#166467,#166468,
#166469,#166470,#166471),(#166472,#166473,#166474,#166475,#166476,#166477,
#166478,#166479,#166480),(#166481,#166482,#166483,#166484,#166485,#166486,
#166487,#166488,#166489),(#166490,#166491,#166492,#166493,#166494,#166495,
#166496,#166497,#166498),(#166499,#166500,#166501,#166502,#166503,#166504,
#166505,#166506,#166507),(#166508,#166509,#166510,#166511,#166512,#166513,
#166514,#166515,#166516),(#166517,#166518,#166519,#166520,#166521,#166522,
#166523,#166524,#166525),(#166526,#166527,#166528,#166529,#166530,#166531,
#166532,#166533,#166534),(#166535,#166536,#166537,#166538,#166539,#166540,
#166541,#166542,#166543),(#166544,#166545,#166546,#166547,#166548,#166549,
#166550,#166551,#166552),(#166553,#166554,#166555,#166556,#166557,#166558,
#166559,#166560,#166561),(#166562,#166563,#166564,#166565,#166566,#166567,
#166568,#166569,#166570),(#166571,#166572,#166573,#166574,#166575,#166576,
#166577,#166578,#166579),(#166580,#166581,#166582,#166583,#166584,#166585,
#166586,#166587,#166588),(#166589,#166590,#166591,#166592,#166593,#166594,
#166595,#166596,#166597),(#166598,#166599,#166600,#166601,#166602,#166603,
#166604,#166605,#166606),(#166607,#166608,#166609,#166610,#166611,#166612,
#166613,#166614,#166615),(#166616,#166617,#166618,#166619,#166620,#166621,
#166622,#166623,#166624),(#166625,#166626,#166627,#166628,#166629,#166630,
#166631,#166632,#166633),(#166634,#166635,#166636,#166637,#166638,#166639,
#166640,#166641,#166642),(#166643,#166644,#166645,#166646,#166647,#166648,
#166649,#166650,#166651),(#166652,#166653,#166654,#166655,#166656,#166657,
#166658,#166659,#166660),(#166661,#166662,#166663,#166664,#166665,#166666,
#166667,#166668,#166669),(#166670,#166671,#166672,#166673,#166674,#166675,
#166676,#166677,#166678),(#166679,#166680,#166681,#166682,#166683,#166684,
#166685,#166686,#166687),(#166688,#166689,#166690,#166691,#166692,#166693,
#166694,#166695,#166696),(#166697,#166698,#166699,#166700,#166701,#166702,
#166703,#166704,#166705),(#166706,#166707,#166708,#166709,#166710,#166711,
#166712,#166713,#166714),(#166715,#166716,#166717,#166718,#166719,#166720,
#166721,#166722,#166723),(#166724,#166725,#166726,#166727,#166728,#166729,
#166730,#166731,#166732),(#166733,#166734,#166735,#166736,#166737,#166738,
#166739,#166740,#166741),(#166742,#166743,#166744,#166745,#166746,#166747,
#166748,#166749,#166750),(#166751,#166752,#166753,#166754,#166755,#166756,
#166757,#166758,#166759),(#166760,#166761,#166762,#166763,#166764,#166765,
#166766,#166767,#166768),(#166769,#166770,#166771,#166772,#166773,#166774,
#166775,#166776,#166777),(#166778,#166779,#166780,#166781,#166782,#166783,
#166784,#166785,#166786),(#166787,#166788,#166789,#166790,#166791,#166792,
#166793,#166794,#166795),(#166796,#166797,#166798,#166799,#166800,#166801,
#166802,#166803,#166804),(#166805,#166806,#166807,#166808,#166809,#166810,
#166811,#166812,#166813),(#166814,#166815,#166816,#166817,#166818,#166819,
#166820,#166821,#166822),(#166823,#166824,#166825,#166826,#166827,#166828,
#166829,#166830,#166831),(#166832,#166833,#166834,#166835,#166836,#166837,
#166838,#166839,#166840),(#166841,#166842,#166843,#166844,#166845,#166846,
#166847,#166848,#166849),(#166850,#166851,#166852,#166853,#166854,#166855,
#166856,#166857,#166858),(#166859,#166860,#166861,#166862,#166863,#166864,
#166865,#166866,#166867),(#166868,#166869,#166870,#166871,#166872,#166873,
#166874,#166875,#166876),(#166877,#166878,#166879,#166880,#166881,#166882,
#166883,#166884,#166885),(#166886,#166887,#166888,#166889,#166890,#166891,
#166892,#166893,#166894),(#166895,#166896,#166897,#166898,#166899,#166900,
#166901,#166902,#166903),(#166904,#166905,#166906,#166907,#166908,#166909,
#166910,#166911,#166912),(#166913,#166914,#166915,#166916,#166917,#166918,
#166919,#166920,#166921),(#166922,#166923,#166924,#166925,#166926,#166927,
#166928,#166929,#166930),(#166931,#166932,#166933,#166934,#166935,#166936,
#166937,#166938,#166939),(#166940,#166941,#166942,#166943,#166944,#166945,
#166946,#166947,#166948),(#166949,#166950,#166951,#166952,#166953,#166954,
#166955,#166956,#166957),(#166958,#166959,#166960,#166961,#166962,#166963,
#166964,#166965,#166966),(#166967,#166968,#166969,#166970,#166971,#166972,
#166973,#166974,#166975),(#166976,#166977,#166978,#166979,#166980,#166981,
#166982,#166983,#166984),(#166985,#166986,#166987,#166988,#166989,#166990,
#166991,#166992,#166993),(#166994,#166995,#166996,#166997,#166998,#166999,
#167000,#167001,#167002),(#167003,#167004,#167005,#167006,#167007,#167008,
#167009,#167010,#167011),(#167012,#167013,#167014,#167015,#167016,#167017,
#167018,#167019,#167020),(#167021,#167022,#167023,#167024,#167025,#167026,
#167027,#167028,#167029),(#167030,#167031,#167032,#167033,#167034,#167035,
#167036,#167037,#167038),(#167039,#167040,#167041,#167042,#167043,#167044,
#167045,#167046,#167047),(#167048,#167049,#167050,#167051,#167052,#167053,
#167054,#167055,#167056),(#167057,#167058,#167059,#167060,#167061,#167062,
#167063,#167064,#167065),(#167066,#167067,#167068,#167069,#167070,#167071,
#167072,#167073,#167074),(#167075,#167076,#167077,#167078,#167079,#167080,
#167081,#167082,#167083),(#167084,#167085,#167086,#167087,#167088,#167089,
#167090,#167091,#167092),(#167093,#167094,#167095,#167096,#167097,#167098,
#167099,#167100,#167101),(#167102,#167103,#167104,#167105,#167106,#167107,
#167108,#167109,#167110),(#167111,#167112,#167113,#167114,#167115,#167116,
#167117,#167118,#167119),(#167120,#167121,#167122,#167123,#167124,#167125,
#167126,#167127,#167128),(#167129,#167130,#167131,#167132,#167133,#167134,
#167135,#167136,#167137),(#167138,#167139,#167140,#167141,#167142,#167143,
#167144,#167145,#167146),(#167147,#167148,#167149,#167150,#167151,#167152,
#167153,#167154,#167155),(#167156,#167157,#167158,#167159,#167160,#167161,
#167162,#167163,#167164),(#167165,#167166,#167167,#167168,#167169,#167170,
#167171,#167172,#167173),(#167174,#167175,#167176,#167177,#167178,#167179,
#167180,#167181,#167182),(#167183,#167184,#167185,#167186,#167187,#167188,
#167189,#167190,#167191),(#167192,#167193,#167194,#167195,#167196,#167197,
#167198,#167199,#167200),(#167201,#167202,#167203,#167204,#167205,#167206,
#167207,#167208,#167209),(#167210,#167211,#167212,#167213,#167214,#167215,
#167216,#167217,#167218),(#167219,#167220,#167221,#167222,#167223,#167224,
#167225,#167226,#167227),(#167228,#167229,#167230,#167231,#167232,#167233,
#167234,#167235,#167236),(#167237,#167238,#167239,#167240,#167241,#167242,
#167243,#167244,#167245),(#167246,#167247,#167248,#167249,#167250,#167251,
#167252,#167253,#167254),(#167255,#167256,#167257,#167258,#167259,#167260,
#167261,#167262,#167263),(#167264,#167265,#167266,#167267,#167268,#167269,
#167270,#167271,#167272),(#167273,#167274,#167275,#167276,#167277,#167278,
#167279,#167280,#167281),(#167282,#167283,#167284,#167285,#167286,#167287,
#167288,#167289,#167290),(#167291,#167292,#167293,#167294,#167295,#167296,
#167297,#167298,#167299),(#167300,#167301,#167302,#167303,#167304,#167305,
#167306,#167307,#167308),(#167309,#167310,#167311,#167312,#167313,#167314,
#167315,#167316,#167317),(#167318,#167319,#167320,#167321,#167322,#167323,
#167324,#167325,#167326),(#167327,#167328,#167329,#167330,#167331,#167332,
#167333,#167334,#167335),(#167336,#167337,#167338,#167339,#167340,#167341,
#167342,#167343,#167344),(#167345,#167346,#167347,#167348,#167349,#167350,
#167351,#167352,#167353),(#167354,#167355,#167356,#167357,#167358,#167359,
#167360,#167361,#167362),(#167363,#167364,#167365,#167366,#167367,#167368,
#167369,#167370,#167371),(#167372,#167373,#167374,#167375,#167376,#167377,
#167378,#167379,#167380),(#167381,#167382,#167383,#167384,#167385,#167386,
#167387,#167388,#167389),(#167390,#167391,#167392,#167393,#167394,#167395,
#167396,#167397,#167398),(#167399,#167400,#167401,#167402,#167403,#167404,
#167405,#167406,#167407),(#167408,#167409,#167410,#167411,#167412,#167413,
#167414,#167415,#167416),(#167417,#167418,#167419,#167420,#167421,#167422,
#167423,#167424,#167425),(#167426,#167427,#167428,#167429,#167430,#167431,
#167432,#167433,#167434),(#167435,#167436,#167437,#167438,#167439,#167440,
#167441,#167442,#167443),(#167444,#167445,#167446,#167447,#167448,#167449,
#167450,#167451,#167452),(#167453,#167454,#167455,#167456,#167457,#167458,
#167459,#167460,#167461),(#167462,#167463,#167464,#167465,#167466,#167467,
#167468,#167469,#167470),(#167471,#167472,#167473,#167474,#167475,#167476,
#167477,#167478,#167479),(#167480,#167481,#167482,#167483,#167484,#167485,
#167486,#167487,#167488),(#167489,#167490,#167491,#167492,#167493,#167494,
#167495,#167496,#167497),(#167498,#167499,#167500,#167501,#167502,#167503,
#167504,#167505,#167506),(#167507,#167508,#167509,#167510,#167511,#167512,
#167513,#167514,#167515),(#167516,#167517,#167518,#167519,#167520,#167521,
#167522,#167523,#167524),(#167525,#167526,#167527,#167528,#167529,#167530,
#167531,#167532,#167533),(#167534,#167535,#167536,#167537,#167538,#167539,
#167540,#167541,#167542),(#167543,#167544,#167545,#167546,#167547,#167548,
#167549,#167550,#167551),(#167552,#167553,#167554,#167555,#167556,#167557,
#167558,#167559,#167560),(#167561,#167562,#167563,#167564,#167565,#167566,
#167567,#167568,#167569),(#167570,#167571,#167572,#167573,#167574,#167575,
#167576,#167577,#167578),(#167579,#167580,#167581,#167582,#167583,#167584,
#167585,#167586,#167587),(#167588,#167589,#167590,#167591,#167592,#167593,
#167594,#167595,#167596),(#167597,#167598,#167599,#167600,#167601,#167602,
#167603,#167604,#167605),(#167606,#167607,#167608,#167609,#167610,#167611,
#167612,#167613,#167614),(#167615,#167616,#167617,#167618,#167619,#167620,
#167621,#167622,#167623),(#167624,#167625,#167626,#167627,#167628,#167629,
#167630,#167631,#167632),(#167633,#167634,#167635,#167636,#167637,#167638,
#167639,#167640,#167641),(#167642,#167643,#167644,#167645,#167646,#167647,
#167648,#167649,#167650),(#167651,#167652,#167653,#167654,#167655,#167656,
#167657,#167658,#167659),(#167660,#167661,#167662,#167663,#167664,#167665,
#167666,#167667,#167668),(#167669,#167670,#167671,#167672,#167673,#167674,
#167675,#167676,#167677),(#167678,#167679,#167680,#167681,#167682,#167683,
#167684,#167685,#167686),(#167687,#167688,#167689,#167690,#167691,#167692,
#167693,#167694,#167695),(#167696,#167697,#167698,#167699,#167700,#167701,
#167702,#167703,#167704),(#167705,#167706,#167707,#167708,#167709,#167710,
#167711,#167712,#167713),(#167714,#167715,#167716,#167717,#167718,#167719,
#167720,#167721,#167722),(#167723,#167724,#167725,#167726,#167727,#167728,
#167729,#167730,#167731),(#167732,#167733,#167734,#167735,#167736,#167737,
#167738,#167739,#167740),(#167741,#167742,#167743,#167744,#167745,#167746,
#167747,#167748,#167749),(#167750,#167751,#167752,#167753,#167754,#167755,
#167756,#167757,#167758),(#167759,#167760,#167761,#167762,#167763,#167764,
#167765,#167766,#167767),(#167768,#167769,#167770,#167771,#167772,#167773,
#167774,#167775,#167776),(#167777,#167778,#167779,#167780,#167781,#167782,
#167783,#167784,#167785),(#167786,#167787,#167788,#167789,#167790,#167791,
#167792,#167793,#167794),(#167795,#167796,#167797,#167798,#167799,#167800,
#167801,#167802,#167803),(#167804,#167805,#167806,#167807,#167808,#167809,
#167810,#167811,#167812),(#167813,#167814,#167815,#167816,#167817,#167818,
#167819,#167820,#167821),(#167822,#167823,#167824,#167825,#167826,#167827,
#167828,#167829,#167830),(#167831,#167832,#167833,#167834,#167835,#167836,
#167837,#167838,#167839),(#167840,#167841,#167842,#167843,#167844,#167845,
#167846,#167847,#167848),(#167849,#167850,#167851,#167852,#167853,#167854,
#167855,#167856,#167857),(#167858,#167859,#167860,#167861,#167862,#167863,
#167864,#167865,#167866),(#167867,#167868,#167869,#167870,#167871,#167872,
#167873,#167874,#167875),(#167876,#167877,#167878,#167879,#167880,#167881,
#167882,#167883,#167884),(#167885,#167886,#167887,#167888,#167889,#167890,
#167891,#167892,#167893),(#167894,#167895,#167896,#167897,#167898,#167899,
#167900,#167901,#167902),(#167903,#167904,#167905,#167906,#167907,#167908,
#167909,#167910,#167911),(#167912,#167913,#167914,#167915,#167916,#167917,
#167918,#167919,#167920),(#167921,#167922,#167923,#167924,#167925,#167926,
#167927,#167928,#167929),(#167930,#167931,#167932,#167933,#167934,#167935,
#167936,#167937,#167938),(#167939,#167940,#167941,#167942,#167943,#167944,
#167945,#167946,#167947),(#167948,#167949,#167950,#167951,#167952,#167953,
#167954,#167955,#167956),(#167957,#167958,#167959,#167960,#167961,#167962,
#167963,#167964,#167965),(#167966,#167967,#167968,#167969,#167970,#167971,
#167972,#167973,#167974),(#167975,#167976,#167977,#167978,#167979,#167980,
#167981,#167982,#167983),(#167984,#167985,#167986,#167987,#167988,#167989,
#167990,#167991,#167992),(#167993,#167994,#167995,#167996,#167997,#167998,
#167999,#168000,#168001),(#168002,#168003,#168004,#168005,#168006,#168007,
#168008,#168009,#168010),(#168011,#168012,#168013,#168014,#168015,#168016,
#168017,#168018,#168019),(#168020,#168021,#168022,#168023,#168024,#168025,
#168026,#168027,#168028),(#168029,#168030,#168031,#168032,#168033,#168034,
#168035,#168036,#168037),(#168038,#168039,#168040,#168041,#168042,#168043,
#168044,#168045,#168046),(#168047,#168048,#168049,#168050,#168051,#168052,
#168053,#168054,#168055),(#168056,#168057,#168058,#168059,#168060,#168061,
#168062,#168063,#168064),(#168065,#168066,#168067,#168068,#168069,#168070,
#168071,#168072,#168073),(#168074,#168075,#168076,#168077,#168078,#168079,
#168080,#168081,#168082),(#168083,#168084,#168085,#168086,#168087,#168088,
#168089,#168090,#168091),(#168092,#168093,#168094,#168095,#168096,#168097,
#168098,#168099,#168100),(#168101,#168102,#168103,#168104,#168105,#168106,
#168107,#168108,#168109),(#168110,#168111,#168112,#168113,#168114,#168115,
#168116,#168117,#168118),(#168119,#168120,#168121,#168122,#168123,#168124,
#168125,#168126,#168127),(#168128,#168129,#168130,#168131,#168132,#168133,
#168134,#168135,#168136),(#168137,#168138,#168139,#168140,#168141,#168142,
#168143,#168144,#168145),(#168146,#168147,#168148,#168149,#168150,#168151,
#168152,#168153,#168154),(#168155,#168156,#168157,#168158,#168159,#168160,
#168161,#168162,#168163),(#168164,#168165,#168166,#168167,#168168,#168169,
#168170,#168171,#168172),(#168173,#168174,#168175,#168176,#168177,#168178,
#168179,#168180,#168181),(#168182,#168183,#168184,#168185,#168186,#168187,
#168188,#168189,#168190),(#168191,#168192,#168193,#168194,#168195,#168196,
#168197,#168198,#168199),(#168200,#168201,#168202,#168203,#168204,#168205,
#168206,#168207,#168208),(#168209,#168210,#168211,#168212,#168213,#168214,
#168215,#168216,#168217),(#168218,#168219,#168220,#168221,#168222,#168223,
#168224,#168225,#168226),(#168227,#168228,#168229,#168230,#168231,#168232,
#168233,#168234,#168235),(#168236,#168237,#168238,#168239,#168240,#168241,
#168242,#168243,#168244),(#168245,#168246,#168247,#168248,#168249,#168250,
#168251,#168252,#168253),(#168254,#168255,#168256,#168257,#168258,#168259,
#168260,#168261,#168262),(#168263,#168264,#168265,#168266,#168267,#168268,
#168269,#168270,#168271),(#168272,#168273,#168274,#168275,#168276,#168277,
#168278,#168279,#168280),(#168281,#168282,#168283,#168284,#168285,#168286,
#168287,#168288,#168289),(#168290,#168291,#168292,#168293,#168294,#168295,
#168296,#168297,#168298),(#168299,#168300,#168301,#168302,#168303,#168304,
#168305,#168306,#168307),(#168308,#168309,#168310,#168311,#168312,#168313,
#168314,#168315,#168316),(#168317,#168318,#168319,#168320,#168321,#168322,
#168323,#168324,#168325),(#168326,#168327,#168328,#168329,#168330,#168331,
#168332,#168333,#168334),(#168335,#168336,#168337,#168338,#168339,#168340,
#168341,#168342,#168343),(#168344,#168345,#168346,#168347,#168348,#168349,
#168350,#168351,#168352),(#168353,#168354,#168355,#168356,#168357,#168358,
#168359,#168360,#168361),(#168362,#168363,#168364,#168365,#168366,#168367,
#168368,#168369,#168370),(#168371,#168372,#168373,#168374,#168375,#168376,
#168377,#168378,#168379),(#168380,#168381,#168382,#168383,#168384,#168385,
#168386,#168387,#168388),(#168389,#168390,#168391,#168392,#168393,#168394,
#168395,#168396,#168397),(#168398,#168399,#168400,#168401,#168402,#168403,
#168404,#168405,#168406),(#168407,#168408,#168409,#168410,#168411,#168412,
#168413,#168414,#168415),(#168416,#168417,#168418,#168419,#168420,#168421,
#168422,#168423,#168424),(#168425,#168426,#168427,#168428,#168429,#168430,
#168431,#168432,#168433),(#168434,#168435,#168436,#168437,#168438,#168439,
#168440,#168441,#168442),(#168443,#168444,#168445,#168446,#168447,#168448,
#168449,#168450,#168451),(#168452,#168453,#168454,#168455,#168456,#168457,
#168458,#168459,#168460),(#168461,#168462,#168463,#168464,#168465,#168466,
#168467,#168468,#168469),(#168470,#168471,#168472,#168473,#168474,#168475,
#168476,#168477,#168478),(#168479,#168480,#168481,#168482,#168483,#168484,
#168485,#168486,#168487),(#168488,#168489,#168490,#168491,#168492,#168493,
#168494,#168495,#168496),(#168497,#168498,#168499,#168500,#168501,#168502,
#168503,#168504,#168505),(#168506,#168507,#168508,#168509,#168510,#168511,
#168512,#168513,#168514),(#168515,#168516,#168517,#168518,#168519,#168520,
#168521,#168522,#168523),(#168524,#168525,#168526,#168527,#168528,#168529,
#168530,#168531,#168532),(#168533,#168534,#168535,#168536,#168537,#168538,
#168539,#168540,#168541),(#168542,#168543,#168544,#168545,#168546,#168547,
#168548,#168549,#168550),(#168551,#168552,#168553,#168554,#168555,#168556,
#168557,#168558,#168559),(#168560,#168561,#168562,#168563,#168564,#168565,
#168566,#168567,#168568),(#168569,#168570,#168571,#168572,#168573,#168574,
#168575,#168576,#168577),(#168578,#168579,#168580,#168581,#168582,#168583,
#168584,#168585,#168586),(#168587,#168588,#168589,#168590,#168591,#168592,
#168593,#168594,#168595),(#168596,#168597,#168598,#168599,#168600,#168601,
#168602,#168603,#168604),(#168605,#168606,#168607,#168608,#168609,#168610,
#168611,#168612,#168613),(#168614,#168615,#168616,#168617,#168618,#168619,
#168620,#168621,#168622),(#168623,#168624,#168625,#168626,#168627,#168628,
#168629,#168630,#168631),(#168632,#168633,#168634,#168635,#168636,#168637,
#168638,#168639,#168640),(#168641,#168642,#168643,#168644,#168645,#168646,
#168647,#168648,#168649),(#168650,#168651,#168652,#168653,#168654,#168655,
#168656,#168657,#168658),(#168659,#168660,#168661,#168662,#168663,#168664,
#168665,#168666,#168667),(#168668,#168669,#168670,#168671,#168672,#168673,
#168674,#168675,#168676),(#168677,#168678,#168679,#168680,#168681,#168682,
#168683,#168684,#168685),(#168686,#168687,#168688,#168689,#168690,#168691,
#168692,#168693,#168694),(#168695,#168696,#168697,#168698,#168699,#168700,
#168701,#168702,#168703),(#168704,#168705,#168706,#168707,#168708,#168709,
#168710,#168711,#168712),(#168713,#168714,#168715,#168716,#168717,#168718,
#168719,#168720,#168721),(#168722,#168723,#168724,#168725,#168726,#168727,
#168728,#168729,#168730),(#168731,#168732,#168733,#168734,#168735,#168736,
#168737,#168738,#168739),(#168740,#168741,#168742,#168743,#168744,#168745,
#168746,#168747,#168748),(#168749,#168750,#168751,#168752,#168753,#168754,
#168755,#168756,#168757),(#168758,#168759,#168760,#168761,#168762,#168763,
#168764,#168765,#168766),(#168767,#168768,#168769,#168770,#168771,#168772,
#168773,#168774,#168775),(#168776,#168777,#168778,#168779,#168780,#168781,
#168782,#168783,#168784),(#168785,#168786,#168787,#168788,#168789,#168790,
#168791,#168792,#168793),(#168794,#168795,#168796,#168797,#168798,#168799,
#168800,#168801,#168802),(#168803,#168804,#168805,#168806,#168807,#168808,
#168809,#168810,#168811),(#168812,#168813,#168814,#168815,#168816,#168817,
#168818,#168819,#168820),(#168821,#168822,#168823,#168824,#168825,#168826,
#168827,#168828,#168829),(#168830,#168831,#168832,#168833,#168834,#168835,
#168836,#168837,#168838),(#168839,#168840,#168841,#168842,#168843,#168844,
#168845,#168846,#168847),(#168848,#168849,#168850,#168851,#168852,#168853,
#168854,#168855,#168856),(#168857,#168858,#168859,#168860,#168861,#168862,
#168863,#168864,#168865),(#168866,#168867,#168868,#168869,#168870,#168871,
#168872,#168873,#168874),(#168875,#168876,#168877,#168878,#168879,#168880,
#168881,#168882,#168883),(#168884,#168885,#168886,#168887,#168888,#168889,
#168890,#168891,#168892),(#168893,#168894,#168895,#168896,#168897,#168898,
#168899,#168900,#168901),(#168902,#168903,#168904,#168905,#168906,#168907,
#168908,#168909,#168910),(#168911,#168912,#168913,#168914,#168915,#168916,
#168917,#168918,#168919),(#168920,#168921,#168922,#168923,#168924,#168925,
#168926,#168927,#168928),(#168929,#168930,#168931,#168932,#168933,#168934,
#168935,#168936,#168937),(#168938,#168939,#168940,#168941,#168942,#168943,
#168944,#168945,#168946),(#168947,#168948,#168949,#168950,#168951,#168952,
#168953,#168954,#168955),(#168956,#168957,#168958,#168959,#168960,#168961,
#168962,#168963,#168964),(#168965,#168966,#168967,#168968,#168969,#168970,
#168971,#168972,#168973),(#168974,#168975,#168976,#168977,#168978,#168979,
#168980,#168981,#168982),(#168983,#168984,#168985,#168986,#168987,#168988,
#168989,#168990,#168991),(#168992,#168993,#168994,#168995,#168996,#168997,
#168998,#168999,#169000),(#169001,#169002,#169003,#169004,#169005,#169006,
#169007,#169008,#169009),(#169010,#169011,#169012,#169013,#169014,#169015,
#169016,#169017,#169018),(#169019,#169020,#169021,#169022,#169023,#169024,
#169025,#169026,#169027),(#169028,#169029,#169030,#169031,#169032,#169033,
#169034,#169035,#169036),(#169037,#169038,#169039,#169040,#169041,#169042,
#169043,#169044,#169045),(#169046,#169047,#169048,#169049,#169050,#169051,
#169052,#169053,#169054),(#169055,#169056,#169057,#169058,#169059,#169060,
#169061,#169062,#169063),(#169064,#169065,#169066,#169067,#169068,#169069,
#169070,#169071,#169072),(#169073,#169074,#169075,#169076,#169077,#169078,
#169079,#169080,#169081),(#169082,#169083,#169084,#169085,#169086,#169087,
#169088,#169089,#169090),(#169091,#169092,#169093,#169094,#169095,#169096,
#169097,#169098,#169099),(#169100,#169101,#169102,#169103,#169104,#169105,
#169106,#169107,#169108),(#169109,#169110,#169111,#169112,#169113,#169114,
#169115,#169116,#169117),(#169118,#169119,#169120,#169121,#169122,#169123,
#169124,#169125,#169126),(#169127,#169128,#169129,#169130,#169131,#169132,
#169133,#169134,#169135),(#169136,#169137,#169138,#169139,#169140,#169141,
#169142,#169143,#169144),(#169145,#169146,#169147,#169148,#169149,#169150,
#169151,#169152,#169153),(#169154,#169155,#169156,#169157,#169158,#169159,
#169160,#169161,#169162),(#169163,#169164,#169165,#169166,#169167,#169168,
#169169,#169170,#169171),(#169172,#169173,#169174,#169175,#169176,#169177,
#169178,#169179,#169180),(#169181,#169182,#169183,#169184,#169185,#169186,
#169187,#169188,#169189),(#169190,#169191,#169192,#169193,#169194,#169195,
#169196,#169197,#169198),(#169199,#169200,#169201,#169202,#169203,#169204,
#169205,#169206,#169207),(#169208,#169209,#169210,#169211,#169212,#169213,
#169214,#169215,#169216),(#169217,#169218,#169219,#169220,#169221,#169222,
#169223,#169224,#169225),(#169226,#169227,#169228,#169229,#169230,#169231,
#169232,#169233,#169234),(#169235,#169236,#169237,#169238,#169239,#169240,
#169241,#169242,#169243),(#169244,#169245,#169246,#169247,#169248,#169249,
#169250,#169251,#169252),(#169253,#169254,#169255,#169256,#169257,#169258,
#169259,#169260,#169261),(#169262,#169263,#169264,#169265,#169266,#169267,
#169268,#169269,#169270),(#169271,#169272,#169273,#169274,#169275,#169276,
#169277,#169278,#169279),(#169280,#169281,#169282,#169283,#169284,#169285,
#169286,#169287,#169288),(#169289,#169290,#169291,#169292,#169293,#169294,
#169295,#169296,#169297),(#169298,#169299,#169300,#169301,#169302,#169303,
#169304,#169305,#169306),(#169307,#169308,#169309,#169310,#169311,#169312,
#169313,#169314,#169315),(#169316,#169317,#169318,#169319,#169320,#169321,
#169322,#169323,#169324),(#169325,#169326,#169327,#169328,#169329,#169330,
#169331,#169332,#169333),(#169334,#169335,#169336,#169337,#169338,#169339,
#169340,#169341,#169342),(#169343,#169344,#169345,#169346,#169347,#169348,
#169349,#169350,#169351),(#169352,#169353,#169354,#169355,#169356,#169357,
#169358,#169359,#169360),(#169361,#169362,#169363,#169364,#169365,#169366,
#169367,#169368,#169369),(#169370,#169371,#169372,#169373,#169374,#169375,
#169376,#169377,#169378),(#169379,#169380,#169381,#169382,#169383,#169384,
#169385,#169386,#169387),(#169388,#169389,#169390,#169391,#169392,#169393,
#169394,#169395,#169396),(#169397,#169398,#169399,#169400,#169401,#169402,
#169403,#169404,#169405),(#169406,#169407,#169408,#169409,#169410,#169411,
#169412,#169413,#169414),(#169415,#169416,#169417,#169418,#169419,#169420,
#169421,#169422,#169423),(#169424,#169425,#169426,#169427,#169428,#169429,
#169430,#169431,#169432),(#169433,#169434,#169435,#169436,#169437,#169438,
#169439,#169440,#169441),(#169442,#169443,#169444,#169445,#169446,#169447,
#169448,#169449,#169450),(#169451,#169452,#169453,#169454,#169455,#169456,
#169457,#169458,#169459),(#169460,#169461,#169462,#169463,#169464,#169465,
#169466,#169467,#169468),(#169469,#169470,#169471,#169472,#169473,#169474,
#169475,#169476,#169477),(#169478,#169479,#169480,#169481,#169482,#169483,
#169484,#169485,#169486),(#169487,#169488,#169489,#169490,#169491,#169492,
#169493,#169494,#169495),(#169496,#169497,#169498,#169499,#169500,#169501,
#169502,#169503,#169504),(#169505,#169506,#169507,#169508,#169509,#169510,
#169511,#169512,#169513),(#169514,#169515,#169516,#169517,#169518,#169519,
#169520,#169521,#169522),(#169523,#169524,#169525,#169526,#169527,#169528,
#169529,#169530,#169531),(#169532,#169533,#169534,#169535,#169536,#169537,
#169538,#169539,#169540),(#169541,#169542,#169543,#169544,#169545,#169546,
#169547,#169548,#169549),(#169550,#169551,#169552,#169553,#169554,#169555,
#169556,#169557,#169558),(#169559,#169560,#169561,#169562,#169563,#169564,
#169565,#169566,#169567),(#169568,#169569,#169570,#169571,#169572,#169573,
#169574,#169575,#169576),(#169577,#169578,#169579,#169580,#169581,#169582,
#169583,#169584,#169585),(#169586,#169587,#169588,#169589,#169590,#169591,
#169592,#169593,#169594),(#169595,#169596,#169597,#169598,#169599,#169600,
#169601,#169602,#169603),(#169604,#169605,#169606,#169607,#169608,#169609,
#169610,#169611,#169612),(#169613,#169614,#169615,#169616,#169617,#169618,
#169619,#169620,#169621),(#169622,#169623,#169624,#169625,#169626,#169627,
#169628,#169629,#169630),(#169631,#169632,#169633,#169634,#169635,#169636,
#169637,#169638,#169639),(#169640,#169641,#169642,#169643,#169644,#169645,
#169646,#169647,#169648),(#169649,#169650,#169651,#169652,#169653,#169654,
#169655,#169656,#169657),(#169658,#169659,#169660,#169661,#169662,#169663,
#169664,#169665,#169666),(#169667,#169668,#169669,#169670,#169671,#169672,
#169673,#169674,#169675),(#169676,#169677,#169678,#169679,#169680,#169681,
#169682,#169683,#169684),(#169685,#169686,#169687,#169688,#169689,#169690,
#169691,#169692,#169693),(#169694,#169695,#169696,#169697,#169698,#169699,
#169700,#169701,#169702),(#169703,#169704,#169705,#169706,#169707,#169708,
#169709,#169710,#169711),(#169712,#169713,#169714,#169715,#169716,#169717,
#169718,#169719,#169720),(#169721,#169722,#169723,#169724,#169725,#169726,
#169727,#169728,#169729),(#169730,#169731,#169732,#169733,#169734,#169735,
#169736,#169737,#169738),(#169739,#169740,#169741,#169742,#169743,#169744,
#169745,#169746,#169747),(#169748,#169749,#169750,#169751,#169752,#169753,
#169754,#169755,#169756),(#169757,#169758,#169759,#169760,#169761,#169762,
#169763,#169764,#169765),(#169766,#169767,#169768,#169769,#169770,#169771,
#169772,#169773,#169774),(#169775,#169776,#169777,#169778,#169779,#169780,
#169781,#169782,#169783),(#169784,#169785,#169786,#169787,#169788,#169789,
#169790,#169791,#169792),(#169793,#169794,#169795,#169796,#169797,#169798,
#169799,#169800,#169801),(#169802,#169803,#169804,#169805,#169806,#169807,
#169808,#169809,#169810),(#169811,#169812,#169813,#169814,#169815,#169816,
#169817,#169818,#169819),(#169820,#169821,#169822,#169823,#169824,#169825,
#169826,#169827,#169828),(#169829,#169830,#169831,#169832,#169833,#169834,
#169835,#169836,#169837),(#169838,#169839,#169840,#169841,#169842,#169843,
#169844,#169845,#169846),(#169847,#169848,#169849,#169850,#169851,#169852,
#169853,#169854,#169855),(#169856,#169857,#169858,#169859,#169860,#169861,
#169862,#169863,#169864),(#169865,#169866,#169867,#169868,#169869,#169870,
#169871,#169872,#169873),(#169874,#169875,#169876,#169877,#169878,#169879,
#169880,#169881,#169882),(#169883,#169884,#169885,#169886,#169887,#169888,
#169889,#169890,#169891),(#169892,#169893,#169894,#169895,#169896,#169897,
#169898,#169899,#169900),(#169901,#169902,#169903,#169904,#169905,#169906,
#169907,#169908,#169909),(#169910,#169911,#169912,#169913,#169914,#169915,
#169916,#169917,#169918),(#169919,#169920,#169921,#169922,#169923,#169924,
#169925,#169926,#169927),(#169928,#169929,#169930,#169931,#169932,#169933,
#169934,#169935,#169936),(#169937,#169938,#169939,#169940,#169941,#169942,
#169943,#169944,#169945),(#169946,#169947,#169948,#169949,#169950,#169951,
#169952,#169953,#169954),(#169955,#169956,#169957,#169958,#169959,#169960,
#169961,#169962,#169963),(#169964,#169965,#169966,#169967,#169968,#169969,
#169970,#169971,#169972),(#169973,#169974,#169975,#169976,#169977,#169978,
#169979,#169980,#169981),(#169982,#169983,#169984,#169985,#169986,#169987,
#169988,#169989,#169990),(#169991,#169992,#169993,#169994,#169995,#169996,
#169997,#169998,#169999),(#170000,#170001,#170002,#170003,#170004,#170005,
#170006,#170007,#170008),(#170009,#170010,#170011,#170012,#170013,#170014,
#170015,#170016,#170017),(#170018,#170019,#170020,#170021,#170022,#170023,
#170024,#170025,#170026),(#170027,#170028,#170029,#170030,#170031,#170032,
#170033,#170034,#170035),(#170036,#170037,#170038,#170039,#170040,#170041,
#170042,#170043,#170044),(#170045,#170046,#170047,#170048,#170049,#170050,
#170051,#170052,#170053),(#170054,#170055,#170056,#170057,#170058,#170059,
#170060,#170061,#170062),(#170063,#170064,#170065,#170066,#170067,#170068,
#170069,#170070,#170071),(#170072,#170073,#170074,#170075,#170076,#170077,
#170078,#170079,#170080),(#170081,#170082,#170083,#170084,#170085,#170086,
#170087,#170088,#170089),(#170090,#170091,#170092,#170093,#170094,#170095,
#170096,#170097,#170098),(#170099,#170100,#170101,#170102,#170103,#170104,
#170105,#170106,#170107),(#170108,#170109,#170110,#170111,#170112,#170113,
#170114,#170115,#170116),(#170117,#170118,#170119,#170120,#170121,#170122,
#170123,#170124,#170125),(#170126,#170127,#170128,#170129,#170130,#170131,
#170132,#170133,#170134),(#170135,#170136,#170137,#170138,#170139,#170140,
#170141,#170142,#170143),(#170144,#170145,#170146,#170147,#170148,#170149,
#170150,#170151,#170152),(#170153,#170154,#170155,#170156,#170157,#170158,
#170159,#170160,#170161),(#170162,#170163,#170164,#170165,#170166,#170167,
#170168,#170169,#170170),(#170171,#170172,#170173,#170174,#170175,#170176,
#170177,#170178,#170179),(#170180,#170181,#170182,#170183,#170184,#170185,
#170186,#170187,#170188),(#170189,#170190,#170191,#170192,#170193,#170194,
#170195,#170196,#170197),(#170198,#170199,#170200,#170201,#170202,#170203,
#170204,#170205,#170206),(#170207,#170208,#170209,#170210,#170211,#170212,
#170213,#170214,#170215),(#170216,#170217,#170218,#170219,#170220,#170221,
#170222,#170223,#170224),(#170225,#170226,#170227,#170228,#170229,#170230,
#170231,#170232,#170233),(#170234,#170235,#170236,#170237,#170238,#170239,
#170240,#170241,#170242),(#170243,#170244,#170245,#170246,#170247,#170248,
#170249,#170250,#170251),(#170252,#170253,#170254,#170255,#170256,#170257,
#170258,#170259,#170260),(#170261,#170262,#170263,#170264,#170265,#170266,
#170267,#170268,#170269),(#170270,#170271,#170272,#170273,#170274,#170275,
#170276,#170277,#170278),(#170279,#170280,#170281,#170282,#170283,#170284,
#170285,#170286,#170287),(#170288,#170289,#170290,#170291,#170292,#170293,
#170294,#170295,#170296),(#170297,#170298,#170299,#170300,#170301,#170302,
#170303,#170304,#170305),(#170306,#170307,#170308,#170309,#170310,#170311,
#170312,#170313,#170314),(#170315,#170316,#170317,#170318,#170319,#170320,
#170321,#170322,#170323),(#170324,#170325,#170326,#170327,#170328,#170329,
#170330,#170331,#170332),(#170333,#170334,#170335,#170336,#170337,#170338,
#170339,#170340,#170341),(#170342,#170343,#170344,#170345,#170346,#170347,
#170348,#170349,#170350),(#170351,#170352,#170353,#170354,#170355,#170356,
#170357,#170358,#170359),(#170360,#170361,#170362,#170363,#170364,#170365,
#170366,#170367,#170368),(#170369,#170370,#170371,#170372,#170373,#170374,
#170375,#170376,#170377),(#170378,#170379,#170380,#170381,#170382,#170383,
#170384,#170385,#170386),(#170387,#170388,#170389,#170390,#170391,#170392,
#170393,#170394,#170395),(#170396,#170397,#170398,#170399,#170400,#170401,
#170402,#170403,#170404),(#170405,#170406,#170407,#170408,#170409,#170410,
#170411,#170412,#170413),(#170414,#170415,#170416,#170417,#170418,#170419,
#170420,#170421,#170422),(#170423,#170424,#170425,#170426,#170427,#170428,
#170429,#170430,#170431),(#170432,#170433,#170434,#170435,#170436,#170437,
#170438,#170439,#170440),(#170441,#170442,#170443,#170444,#170445,#170446,
#170447,#170448,#170449),(#170450,#170451,#170452,#170453,#170454,#170455,
#170456,#170457,#170458),(#170459,#170460,#170461,#170462,#170463,#170464,
#170465,#170466,#170467),(#170468,#170469,#170470,#170471,#170472,#170473,
#170474,#170475,#170476),(#170477,#170478,#170479,#170480,#170481,#170482,
#170483,#170484,#170485),(#170486,#170487,#170488,#170489,#170490,#170491,
#170492,#170493,#170494),(#170495,#170496,#170497,#170498,#170499,#170500,
#170501,#170502,#170503),(#170504,#170505,#170506,#170507,#170508,#170509,
#170510,#170511,#170512),(#170513,#170514,#170515,#170516,#170517,#170518,
#170519,#170520,#170521),(#170522,#170523,#170524,#170525,#170526,#170527,
#170528,#170529,#170530),(#170531,#170532,#170533,#170534,#170535,#170536,
#170537,#170538,#170539),(#170540,#170541,#170542,#170543,#170544,#170545,
#170546,#170547,#170548),(#170549,#170550,#170551,#170552,#170553,#170554,
#170555,#170556,#170557),(#170558,#170559,#170560,#170561,#170562,#170563,
#170564,#170565,#170566),(#170567,#170568,#170569,#170570,#170571,#170572,
#170573,#170574,#170575),(#170576,#170577,#170578,#170579,#170580,#170581,
#170582,#170583,#170584),(#170585,#170586,#170587,#170588,#170589,#170590,
#170591,#170592,#170593),(#170594,#170595,#170596,#170597,#170598,#170599,
#170600,#170601,#170602),(#170603,#170604,#170605,#170606,#170607,#170608,
#170609,#170610,#170611),(#170612,#170613,#170614,#170615,#170616,#170617,
#170618,#170619,#170620),(#170621,#170622,#170623,#170624,#170625,#170626,
#170627,#170628,#170629),(#170630,#170631,#170632,#170633,#170634,#170635,
#170636,#170637,#170638),(#170639,#170640,#170641,#170642,#170643,#170644,
#170645,#170646,#170647),(#170648,#170649,#170650,#170651,#170652,#170653,
#170654,#170655,#170656),(#170657,#170658,#170659,#170660,#170661,#170662,
#170663,#170664,#170665),(#170666,#170667,#170668,#170669,#170670,#170671,
#170672,#170673,#170674),(#170675,#170676,#170677,#170678,#170679,#170680,
#170681,#170682,#170683),(#170684,#170685,#170686,#170687,#170688,#170689,
#170690,#170691,#170692),(#170693,#170694,#170695,#170696,#170697,#170698,
#170699,#170700,#170701),(#170702,#170703,#170704,#170705,#170706,#170707,
#170708,#170709,#170710),(#170711,#170712,#170713,#170714,#170715,#170716,
#170717,#170718,#170719),(#170720,#170721,#170722,#170723,#170724,#170725,
#170726,#170727,#170728),(#170729,#170730,#170731,#170732,#170733,#170734,
#170735,#170736,#170737),(#170738,#170739,#170740,#170741,#170742,#170743,
#170744,#170745,#170746),(#170747,#170748,#170749,#170750,#170751,#170752,
#170753,#170754,#170755),(#170756,#170757,#170758,#170759,#170760,#170761,
#170762,#170763,#170764),(#170765,#170766,#170767,#170768,#170769,#170770,
#170771,#170772,#170773),(#170774,#170775,#170776,#170777,#170778,#170779,
#170780,#170781,#170782),(#170783,#170784,#170785,#170786,#170787,#170788,
#170789,#170790,#170791),(#170792,#170793,#170794,#170795,#170796,#170797,
#170798,#170799,#170800),(#170801,#170802,#170803,#170804,#170805,#170806,
#170807,#170808,#170809),(#170810,#170811,#170812,#170813,#170814,#170815,
#170816,#170817,#170818),(#170819,#170820,#170821,#170822,#170823,#170824,
#170825,#170826,#170827),(#170828,#170829,#170830,#170831,#170832,#170833,
#170834,#170835,#170836),(#170837,#170838,#170839,#170840,#170841,#170842,
#170843,#170844,#170845),(#170846,#170847,#170848,#170849,#170850,#170851,
#170852,#170853,#170854),(#170855,#170856,#170857,#170858,#170859,#170860,
#170861,#170862,#170863),(#170864,#170865,#170866,#170867,#170868,#170869,
#170870,#170871,#170872),(#170873,#170874,#170875,#170876,#170877,#170878,
#170879,#170880,#170881),(#170882,#170883,#170884,#170885,#170886,#170887,
#170888,#170889,#170890),(#170891,#170892,#170893,#170894,#170895,#170896,
#170897,#170898,#170899),(#170900,#170901,#170902,#170903,#170904,#170905,
#170906,#170907,#170908),(#170909,#170910,#170911,#170912,#170913,#170914,
#170915,#170916,#170917),(#170918,#170919,#170920,#170921,#170922,#170923,
#170924,#170925,#170926),(#170927,#170928,#170929,#170930,#170931,#170932,
#170933,#170934,#170935),(#170936,#170937,#170938,#170939,#170940,#170941,
#170942,#170943,#170944),(#170945,#170946,#170947,#170948,#170949,#170950,
#170951,#170952,#170953),(#170954,#170955,#170956,#170957,#170958,#170959,
#170960,#170961,#170962),(#170963,#170964,#170965,#170966,#170967,#170968,
#170969,#170970,#170971),(#170972,#170973,#170974,#170975,#170976,#170977,
#170978,#170979,#170980),(#170981,#170982,#170983,#170984,#170985,#170986,
#170987,#170988,#170989),(#170990,#170991,#170992,#170993,#170994,#170995,
#170996,#170997,#170998),(#170999,#171000,#171001,#171002,#171003,#171004,
#171005,#171006,#171007),(#171008,#171009,#171010,#171011,#171012,#171013,
#171014,#171015,#171016),(#171017,#171018,#171019,#171020,#171021,#171022,
#171023,#171024,#171025),(#171026,#171027,#171028,#171029,#171030,#171031,
#171032,#171033,#171034),(#171035,#171036,#171037,#171038,#171039,#171040,
#171041,#171042,#171043),(#171044,#171045,#171046,#171047,#171048,#171049,
#171050,#171051,#171052),(#171053,#171054,#171055,#171056,#171057,#171058,
#171059,#171060,#171061),(#171062,#171063,#171064,#171065,#171066,#171067,
#171068,#171069,#171070),(#171071,#171072,#171073,#171074,#171075,#171076,
#171077,#171078,#171079),(#171080,#171081,#171082,#171083,#171084,#171085,
#171086,#171087,#171088),(#171089,#171090,#171091,#171092,#171093,#171094,
#171095,#171096,#171097),(#171098,#171099,#171100,#171101,#171102,#171103,
#171104,#171105,#171106),(#171107,#171108,#171109,#171110,#171111,#171112,
#171113,#171114,#171115),(#171116,#171117,#171118,#171119,#171120,#171121,
#171122,#171123,#171124),(#171125,#171126,#171127,#171128,#171129,#171130,
#171131,#171132,#171133),(#171134,#171135,#171136,#171137,#171138,#171139,
#171140,#171141,#171142),(#171143,#171144,#171145,#171146,#171147,#171148,
#171149,#171150,#171151),(#171152,#171153,#171154,#171155,#171156,#171157,
#171158,#171159,#171160),(#171161,#171162,#171163,#171164,#171165,#171166,
#171167,#171168,#171169),(#171170,#171171,#171172,#171173,#171174,#171175,
#171176,#171177,#171178),(#171179,#171180,#171181,#171182,#171183,#171184,
#171185,#171186,#171187),(#171188,#171189,#171190,#171191,#171192,#171193,
#171194,#171195,#171196),(#171197,#171198,#171199,#171200,#171201,#171202,
#171203,#171204,#171205),(#171206,#171207,#171208,#171209,#171210,#171211,
#171212,#171213,#171214),(#171215,#171216,#171217,#171218,#171219,#171220,
#171221,#171222,#171223),(#171224,#171225,#171226,#171227,#171228,#171229,
#171230,#171231,#171232),(#171233,#171234,#171235,#171236,#171237,#171238,
#171239,#171240,#171241),(#171242,#171243,#171244,#171245,#171246,#171247,
#171248,#171249,#171250),(#171251,#171252,#171253,#171254,#171255,#171256,
#171257,#171258,#171259),(#171260,#171261,#171262,#171263,#171264,#171265,
#171266,#171267,#171268),(#171269,#171270,#171271,#171272,#171273,#171274,
#171275,#171276,#171277),(#171278,#171279,#171280,#171281,#171282,#171283,
#171284,#171285,#171286),(#171287,#171288,#171289,#171290,#171291,#171292,
#171293,#171294,#171295),(#171296,#171297,#171298,#171299,#171300,#171301,
#171302,#171303,#171304),(#171305,#171306,#171307,#171308,#171309,#171310,
#171311,#171312,#171313),(#171314,#171315,#171316,#171317,#171318,#171319,
#171320,#171321,#171322),(#171323,#171324,#171325,#171326,#171327,#171328,
#171329,#171330,#171331),(#171332,#171333,#171334,#171335,#171336,#171337,
#171338,#171339,#171340),(#171341,#171342,#171343,#171344,#171345,#171346,
#171347,#171348,#171349),(#171350,#171351,#171352,#171353,#171354,#171355,
#171356,#171357,#171358),(#171359,#171360,#171361,#171362,#171363,#171364,
#171365,#171366,#171367),(#171368,#171369,#171370,#171371,#171372,#171373,
#171374,#171375,#171376),(#171377,#171378,#171379,#171380,#171381,#171382,
#171383,#171384,#171385),(#171386,#171387,#171388,#171389,#171390,#171391,
#171392,#171393,#171394),(#171395,#171396,#171397,#171398,#171399,#171400,
#171401,#171402,#171403),(#171404,#171405,#171406,#171407,#171408,#171409,
#171410,#171411,#171412),(#171413,#171414,#171415,#171416,#171417,#171418,
#171419,#171420,#171421),(#171422,#171423,#171424,#171425,#171426,#171427,
#171428,#171429,#171430),(#171431,#171432,#171433,#171434,#171435,#171436,
#171437,#171438,#171439),(#171440,#171441,#171442,#171443,#171444,#171445,
#171446,#171447,#171448),(#171449,#171450,#171451,#171452,#171453,#171454,
#171455,#171456,#171457),(#171458,#171459,#171460,#171461,#171462,#171463,
#171464,#171465,#171466),(#171467,#171468,#171469,#171470,#171471,#171472,
#171473,#171474,#171475),(#171476,#171477,#171478,#171479,#171480,#171481,
#171482,#171483,#171484),(#171485,#171486,#171487,#171488,#171489,#171490,
#171491,#171492,#171493),(#171494,#171495,#171496,#171497,#171498,#171499,
#171500,#171501,#171502),(#171503,#171504,#171505,#171506,#171507,#171508,
#171509,#171510,#171511),(#171512,#171513,#171514,#171515,#171516,#171517,
#171518,#171519,#171520),(#171521,#171522,#171523,#171524,#171525,#171526,
#171527,#171528,#171529),(#171530,#171531,#171532,#171533,#171534,#171535,
#171536,#171537,#171538),(#171539,#171540,#171541,#171542,#171543,#171544,
#171545,#171546,#171547),(#171548,#171549,#171550,#171551,#171552,#171553,
#171554,#171555,#171556),(#171557,#171558,#171559,#171560,#171561,#171562,
#171563,#171564,#171565),(#171566,#171567,#171568,#171569,#171570,#171571,
#171572,#171573,#171574),(#171575,#171576,#171577,#171578,#171579,#171580,
#171581,#171582,#171583),(#171584,#171585,#171586,#171587,#171588,#171589,
#171590,#171591,#171592),(#171593,#171594,#171595,#171596,#171597,#171598,
#171599,#171600,#171601),(#171602,#171603,#171604,#171605,#171606,#171607,
#171608,#171609,#171610),(#171611,#171612,#171613,#171614,#171615,#171616,
#171617,#171618,#171619),(#171620,#171621,#171622,#171623,#171624,#171625,
#171626,#171627,#171628),(#171629,#171630,#171631,#171632,#171633,#171634,
#171635,#171636,#171637),(#171638,#171639,#171640,#171641,#171642,#171643,
#171644,#171645,#171646),(#171647,#171648,#171649,#171650,#171651,#171652,
#171653,#171654,#171655),(#171656,#171657,#171658,#171659,#171660,#171661,
#171662,#171663,#171664),(#171665,#171666,#171667,#171668,#171669,#171670,
#171671,#171672,#171673),(#171674,#171675,#171676,#171677,#171678,#171679,
#171680,#171681,#171682),(#171683,#171684,#171685,#171686,#171687,#171688,
#171689,#171690,#171691),(#171692,#171693,#171694,#171695,#171696,#171697,
#171698,#171699,#171700),(#171701,#171702,#171703,#171704,#171705,#171706,
#171707,#171708,#171709),(#171710,#171711,#171712,#171713,#171714,#171715,
#171716,#171717,#171718),(#171719,#171720,#171721,#171722,#171723,#171724,
#171725,#171726,#171727),(#171728,#171729,#171730,#171731,#171732,#171733,
#171734,#171735,#171736),(#171737,#171738,#171739,#171740,#171741,#171742,
#171743,#171744,#171745),(#171746,#171747,#171748,#171749,#171750,#171751,
#171752,#171753,#171754),(#171755,#171756,#171757,#171758,#171759,#171760,
#171761,#171762,#171763),(#171764,#171765,#171766,#171767,#171768,#171769,
#171770,#171771,#171772),(#171773,#171774,#171775,#171776,#171777,#171778,
#171779,#171780,#171781),(#171782,#171783,#171784,#171785,#171786,#171787,
#171788,#171789,#171790),(#171791,#171792,#171793,#171794,#171795,#171796,
#171797,#171798,#171799),(#171800,#171801,#171802,#171803,#171804,#171805,
#171806,#171807,#171808),(#171809,#171810,#171811,#171812,#171813,#171814,
#171815,#171816,#171817),(#171818,#171819,#171820,#171821,#171822,#171823,
#171824,#171825,#171826),(#171827,#171828,#171829,#171830,#171831,#171832,
#171833,#171834,#171835),(#171836,#171837,#171838,#171839,#171840,#171841,
#171842,#171843,#171844),(#171845,#171846,#171847,#171848,#171849,#171850,
#171851,#171852,#171853),(#171854,#171855,#171856,#171857,#171858,#171859,
#171860,#171861,#171862),(#171863,#171864,#171865,#171866,#171867,#171868,
#171869,#171870,#171871),(#171872,#171873,#171874,#171875,#171876,#171877,
#171878,#171879,#171880),(#171881,#171882,#171883,#171884,#171885,#171886,
#171887,#171888,#171889),(#171890,#171891,#171892,#171893,#171894,#171895,
#171896,#171897,#171898),(#171899,#171900,#171901,#171902,#171903,#171904,
#171905,#171906,#171907),(#171908,#171909,#171910,#171911,#171912,#171913,
#171914,#171915,#171916),(#171917,#171918,#171919,#171920,#171921,#171922,
#171923,#171924,#171925),(#171926,#171927,#171928,#171929,#171930,#171931,
#171932,#171933,#171934),(#171935,#171936,#171937,#171938,#171939,#171940,
#171941,#171942,#171943),(#171944,#171945,#171946,#171947,#171948,#171949,
#171950,#171951,#171952),(#171953,#171954,#171955,#171956,#171957,#171958,
#171959,#171960,#171961),(#171962,#171963,#171964,#171965,#171966,#171967,
#171968,#171969,#171970),(#171971,#171972,#171973,#171974,#171975,#171976,
#171977,#171978,#171979),(#171980,#171981,#171982,#171983,#171984,#171985,
#171986,#171987,#171988),(#171989,#171990,#171991,#171992,#171993,#171994,
#171995,#171996,#171997),(#171998,#171999,#172000,#172001,#172002,#172003,
#172004,#172005,#172006),(#172007,#172008,#172009,#172010,#172011,#172012,
#172013,#172014,#172015),(#172016,#172017,#172018,#172019,#172020,#172021,
#172022,#172023,#172024),(#172025,#172026,#172027,#172028,#172029,#172030,
#172031,#172032,#172033),(#172034,#172035,#172036,#172037,#172038,#172039,
#172040,#172041,#172042),(#172043,#172044,#172045,#172046,#172047,#172048,
#172049,#172050,#172051),(#172052,#172053,#172054,#172055,#172056,#172057,
#172058,#172059,#172060),(#172061,#172062,#172063,#172064,#172065,#172066,
#172067,#172068,#172069),(#172070,#172071,#172072,#172073,#172074,#172075,
#172076,#172077,#172078),(#172079,#172080,#172081,#172082,#172083,#172084,
#172085,#172086,#172087),(#172088,#172089,#172090,#172091,#172092,#172093,
#172094,#172095,#172096),(#172097,#172098,#172099,#172100,#172101,#172102,
#172103,#172104,#172105),(#172106,#172107,#172108,#172109,#172110,#172111,
#172112,#172113,#172114),(#172115,#172116,#172117,#172118,#172119,#172120,
#172121,#172122,#172123),(#172124,#172125,#172126,#172127,#172128,#172129,
#172130,#172131,#172132),(#172133,#172134,#172135,#172136,#172137,#172138,
#172139,#172140,#172141),(#172142,#172143,#172144,#172145,#172146,#172147,
#172148,#172149,#172150),(#172151,#172152,#172153,#172154,#172155,#172156,
#172157,#172158,#172159),(#172160,#172161,#172162,#172163,#172164,#172165,
#172166,#172167,#172168),(#172169,#172170,#172171,#172172,#172173,#172174,
#172175,#172176,#172177),(#172178,#172179,#172180,#172181,#172182,#172183,
#172184,#172185,#172186),(#172187,#172188,#172189,#172190,#172191,#172192,
#172193,#172194,#172195),(#172196,#172197,#172198,#172199,#172200,#172201,
#172202,#172203,#172204),(#172205,#172206,#172207,#172208,#172209,#172210,
#172211,#172212,#172213),(#172214,#172215,#172216,#172217,#172218,#172219,
#172220,#172221,#172222),(#172223,#172224,#172225,#172226,#172227,#172228,
#172229,#172230,#172231),(#172232,#172233,#172234,#172235,#172236,#172237,
#172238,#172239,#172240),(#172241,#172242,#172243,#172244,#172245,#172246,
#172247,#172248,#172249),(#172250,#172251,#172252,#172253,#172254,#172255,
#172256,#172257,#172258),(#172259,#172260,#172261,#172262,#172263,#172264,
#172265,#172266,#172267),(#172268,#172269,#172270,#172271,#172272,#172273,
#172274,#172275,#172276),(#172277,#172278,#172279,#172280,#172281,#172282,
#172283,#172284,#172285),(#172286,#172287,#172288,#172289,#172290,#172291,
#172292,#172293,#172294),(#172295,#172296,#172297,#172298,#172299,#172300,
#172301,#172302,#172303),(#172304,#172305,#172306,#172307,#172308,#172309,
#172310,#172311,#172312),(#172313,#172314,#172315,#172316,#172317,#172318,
#172319,#172320,#172321),(#172322,#172323,#172324,#172325,#172326,#172327,
#172328,#172329,#172330),(#172331,#172332,#172333,#172334,#172335,#172336,
#172337,#172338,#172339),(#172340,#172341,#172342,#172343,#172344,#172345,
#172346,#172347,#172348),(#172349,#172350,#172351,#172352,#172353,#172354,
#172355,#172356,#172357),(#172358,#172359,#172360,#172361,#172362,#172363,
#172364,#172365,#172366),(#172367,#172368,#172369,#172370,#172371,#172372,
#172373,#172374,#172375),(#172376,#172377,#172378,#172379,#172380,#172381,
#172382,#172383,#172384),(#172385,#172386,#172387,#172388,#172389,#172390,
#172391,#172392,#172393),(#172394,#172395,#172396,#172397,#172398,#172399,
#172400,#172401,#172402),(#172403,#172404,#172405,#172406,#172407,#172408,
#172409,#172410,#172411),(#172412,#172413,#172414,#172415,#172416,#172417,
#172418,#172419,#172420),(#172421,#172422,#172423,#172424,#172425,#172426,
#172427,#172428,#172429),(#172430,#172431,#172432,#172433,#172434,#172435,
#172436,#172437,#172438),(#172439,#172440,#172441,#172442,#172443,#172444,
#172445,#172446,#172447),(#172448,#172449,#172450,#172451,#172452,#172453,
#172454,#172455,#172456),(#172457,#172458,#172459,#172460,#172461,#172462,
#172463,#172464,#172465),(#172466,#172467,#172468,#172469,#172470,#172471,
#172472,#172473,#172474),(#172475,#172476,#172477,#172478,#172479,#172480,
#172481,#172482,#172483),(#172484,#172485,#172486,#172487,#172488,#172489,
#172490,#172491,#172492),(#172493,#172494,#172495,#172496,#172497,#172498,
#172499,#172500,#172501),(#172502,#172503,#172504,#172505,#172506,#172507,
#172508,#172509,#172510),(#172511,#172512,#172513,#172514,#172515,#172516,
#172517,#172518,#172519),(#172520,#172521,#172522,#172523,#172524,#172525,
#172526,#172527,#172528),(#172529,#172530,#172531,#172532,#172533,#172534,
#172535,#172536,#172537),(#172538,#172539,#172540,#172541,#172542,#172543,
#172544,#172545,#172546),(#172547,#172548,#172549,#172550,#172551,#172552,
#172553,#172554,#172555),(#172556,#172557,#172558,#172559,#172560,#172561,
#172562,#172563,#172564),(#172565,#172566,#172567,#172568,#172569,#172570,
#172571,#172572,#172573),(#172574,#172575,#172576,#172577,#172578,#172579,
#172580,#172581,#172582),(#172583,#172584,#172585,#172586,#172587,#172588,
#172589,#172590,#172591),(#172592,#172593,#172594,#172595,#172596,#172597,
#172598,#172599,#172600),(#172601,#172602,#172603,#172604,#172605,#172606,
#172607,#172608,#172609),(#172610,#172611,#172612,#172613,#172614,#172615,
#172616,#172617,#172618),(#172619,#172620,#172621,#172622,#172623,#172624,
#172625,#172626,#172627),(#172628,#172629,#172630,#172631,#172632,#172633,
#172634,#172635,#172636),(#172637,#172638,#172639,#172640,#172641,#172642,
#172643,#172644,#172645),(#172646,#172647,#172648,#172649,#172650,#172651,
#172652,#172653,#172654),(#172655,#172656,#172657,#172658,#172659,#172660,
#172661,#172662,#172663),(#172664,#172665,#172666,#172667,#172668,#172669,
#172670,#172671,#172672),(#172673,#172674,#172675,#172676,#172677,#172678,
#172679,#172680,#172681),(#172682,#172683,#172684,#172685,#172686,#172687,
#172688,#172689,#172690),(#172691,#172692,#172693,#172694,#172695,#172696,
#172697,#172698,#172699),(#172700,#172701,#172702,#172703,#172704,#172705,
#172706,#172707,#172708),(#172709,#172710,#172711,#172712,#172713,#172714,
#172715,#172716,#172717),(#172718,#172719,#172720,#172721,#172722,#172723,
#172724,#172725,#172726),(#172727,#172728,#172729,#172730,#172731,#172732,
#172733,#172734,#172735),(#172736,#172737,#172738,#172739,#172740,#172741,
#172742,#172743,#172744),(#172745,#172746,#172747,#172748,#172749,#172750,
#172751,#172752,#172753),(#172754,#172755,#172756,#172757,#172758,#172759,
#172760,#172761,#172762),(#172763,#172764,#172765,#172766,#172767,#172768,
#172769,#172770,#172771),(#172772,#172773,#172774,#172775,#172776,#172777,
#172778,#172779,#172780),(#172781,#172782,#172783,#172784,#172785,#172786,
#172787,#172788,#172789),(#172790,#172791,#172792,#172793,#172794,#172795,
#172796,#172797,#172798),(#172799,#172800,#172801,#172802,#172803,#172804,
#172805,#172806,#172807),(#172808,#172809,#172810,#172811,#172812,#172813,
#172814,#172815,#172816),(#172817,#172818,#172819,#172820,#172821,#172822,
#172823,#172824,#172825),(#172826,#172827,#172828,#172829,#172830,#172831,
#172832,#172833,#172834),(#172835,#172836,#172837,#172838,#172839,#172840,
#172841,#172842,#172843),(#172844,#172845,#172846,#172847,#172848,#172849,
#172850,#172851,#172852),(#172853,#172854,#172855,#172856,#172857,#172858,
#172859,#172860,#172861),(#172862,#172863,#172864,#172865,#172866,#172867,
#172868,#172869,#172870),(#172871,#172872,#172873,#172874,#172875,#172876,
#172877,#172878,#172879),(#172880,#172881,#172882,#172883,#172884,#172885,
#172886,#172887,#172888),(#172889,#172890,#172891,#172892,#172893,#172894,
#172895,#172896,#172897),(#172898,#172899,#172900,#172901,#172902,#172903,
#172904,#172905,#172906),(#172907,#172908,#172909,#172910,#172911,#172912,
#172913,#172914,#172915),(#172916,#172917,#172918,#172919,#172920,#172921,
#172922,#172923,#172924),(#172925,#172926,#172927,#172928,#172929,#172930,
#172931,#172932,#172933),(#172934,#172935,#172936,#172937,#172938,#172939,
#172940,#172941,#172942),(#172943,#172944,#172945,#172946,#172947,#172948,
#172949,#172950,#172951),(#172952,#172953,#172954,#172955,#172956,#172957,
#172958,#172959,#172960),(#172961,#172962,#172963,#172964,#172965,#172966,
#172967,#172968,#172969),(#172970,#172971,#172972,#172973,#172974,#172975,
#172976,#172977,#172978),(#172979,#172980,#172981,#172982,#172983,#172984,
#172985,#172986,#172987),(#172988,#172989,#172990,#172991,#172992,#172993,
#172994,#172995,#172996),(#172997,#172998,#172999,#173000,#173001,#173002,
#173003,#173004,#173005),(#173006,#173007,#173008,#173009,#173010,#173011,
#173012,#173013,#173014),(#173015,#173016,#173017,#173018,#173019,#173020,
#173021,#173022,#173023),(#173024,#173025,#173026,#173027,#173028,#173029,
#173030,#173031,#173032),(#173033,#173034,#173035,#173036,#173037,#173038,
#173039,#173040,#173041),(#173042,#173043,#173044,#173045,#173046,#173047,
#173048,#173049,#173050),(#173051,#173052,#173053,#173054,#173055,#173056,
#173057,#173058,#173059),(#173060,#173061,#173062,#173063,#173064,#173065,
#173066,#173067,#173068),(#173069,#173070,#173071,#173072,#173073,#173074,
#173075,#173076,#173077),(#173078,#173079,#173080,#173081,#173082,#173083,
#173084,#173085,#173086),(#173087,#173088,#173089,#173090,#173091,#173092,
#173093,#173094,#173095),(#173096,#173097,#173098,#173099,#173100,#173101,
#173102,#173103,#173104),(#173105,#173106,#173107,#173108,#173109,#173110,
#173111,#173112,#173113),(#173114,#173115,#173116,#173117,#173118,#173119,
#173120,#173121,#173122),(#173123,#173124,#173125,#173126,#173127,#173128,
#173129,#173130,#173131),(#173132,#173133,#173134,#173135,#173136,#173137,
#173138,#173139,#173140),(#173141,#173142,#173143,#173144,#173145,#173146,
#173147,#173148,#173149),(#173150,#173151,#173152,#173153,#173154,#173155,
#173156,#173157,#173158),(#173159,#173160,#173161,#173162,#173163,#173164,
#173165,#173166,#173167),(#173168,#173169,#173170,#173171,#173172,#173173,
#173174,#173175,#173176),(#173177,#173178,#173179,#173180,#173181,#173182,
#173183,#173184,#173185),(#173186,#173187,#173188,#173189,#173190,#173191,
#173192,#173193,#173194)),.UNSPECIFIED.,.F.,.T.,.F.)
B_SPLINE_SURFACE_WITH_KNOTS((4,1,1,1,1,1,1,1,1,1,1,1,1,1,1,1,1,1,1,1,1,
1,1,1,1,1,1,1,1,1,1,1,1,1,1,1,1,1,1,1,1,1,1,1,1,1,1,1,1,1,1,1,1,1,1,1,1,
1,1,1,1,1,1,1,1,1,1,1,1,1,1,1,1,1,1,1,1,1,1,1,1,1,1,1,1,1,1,1,1,1,1,1,1,
1,1,1,1,1,1,1,1,1,1,1,1,1,1,1,1,1,1,1,1,1,1,1,1,1,1,1,1,1,1,1,1,1,1,1,1,
1,1,1,1,1,1,1,1,1,1,1,1,1,1,1,1,1,1,1,1,1,1,1,1,1,1,1,1,1,1,1,1,1,1,1,1,
1,1,1,1,1,1,1,1,1,1,1,1,1,1,1,1,1,1,1,1,1,1,1,1,1,1,1,1,1,1,1,1,1,1,1,1,
1,1,1,1,1,1,1,1,1,1,1,1,1,1,1,1,1,1,1,1,1,1,1,1,1,1,1,1,1,1,1,1,1,1,1,1,
1,1,1,1,1,1,1,1,1,1,1,1,1,1,1,1,1,1,1,1,1,1,1,1,1,1,1,1,1,1,1,1,1,1,1,1,
1,1,1,1,1,1,1,1,1,1,1,1,1,1,1,1,1,1,1,1,1,1,1,1,1,1,1,1,1,1,1,1,1,1,1,1,
1,1,1,1,1,1,1,1,1,1,1,1,1,1,1,1,1,1,1,1,1,1,1,1,1,1,1,1,1,1,1,1,1,1,1,1,
1,1,1,1,1,1,1,1,1,1,1,1,1,1,1,1,1,1,1,1,1,1,1,1,1,1,1,1,1,1,1,1,1,1,1,1,
1,1,1,1,1,1,1,1,1,1,1,1,1,1,1,1,1,1,1,1,1,1,1,1,1,1,1,1,1,1,1,1,1,1,1,1,
1,1,1,1,1,1,1,1,1,1,1,1,1,1,1,1,1,1,1,1,1,1,1,1,1,1,1,1,1,1,1,1,1,1,1,1,
1,1,1,1,1,1,1,1,1,1,1,1,1,1,1,1,1,1,1,1,1,1,1,1,1,1,1,1,1,1,1,1,1,1,1,1,
1,1,1,1,1,1,1,1,1,1,1,1,1,1,1,1,1,1,1,1,1,1,1,1,1,1,1,1,1,1,1,1,1,1,1,1,
1,1,1,1,1,1,1,1,1,1,1,1,1,1,1,1,1,1,1,1,1,1,1,1,1,1,1,1,1,1,1,1,1,1,1,1,
1,1,1,1,1,1,1,1,1,1,1,1,1,1,1,1,1,1,1,1,1,1,1,1,1,1,1,1,1,1,1,1,1,1,1,1,
1,1,1,1,1,1,1,1,1,1,1,1,1,1,1,1,1,1,1,1,1,1,1,1,1,1,1,1,1,1,1,1,1,1,1,1,
1,1,1,1,1,1,1,1,1,1,1,1,1,1,1,1,1,1,1,1,1,1,1,1,1,1,1,1,1,1,1,1,1,1,1,1,
1,1,1,1,1,1,1,1,1,1,1,1,1,1,1,1,1,1,1,1,1,1,1,1,1,1,1,1,1,1,1,1,1,1,1,1,
1,1,1,1,1,1,1,1,1,1,1,1,1,1,1,1,1,1,1,1,1,1,1,1,1,1,1,1,1,1,1,1,1,1,1,1,
1,1,1,1,1,1,1,1,1,1,1,1,1,1,1,1,1,1,1,1,1,1,1,1,1,1,1,1,1,1,1,1,1,1,1,1,
1,1,1,1,1,1,1,1,1,1,1,1,1,1,1,1,1,1,1,1,1,1,1,1,1,1,1,1,1,1,1,1,1,1,1,1,
1,1,1,1,1,1,1,1,1,1,1,1,1,1,1,1,1,1,1,1,1,1,1,1,1,1,1,1,1,1,1,1,1,1,1,1,
1,1,1,1,1,1,1,1,1,1,1,1,1,1,1,1,1,1,1,1,1,1,1,1,1,1,1,1,1,1,1,1,1,1,1,1,
1,1,1,1,1,1,1,1,1,1,1,1,1,1,1,1,1,1,1,1,1,1,1,1,1,1,1,1,1,1,1,1,1,1,1,1,
1,1,1,1,1,1,1,1,1,1,1,1,1,1,1,1,1,1,1,1,1,1,1,1,1,1,1,1,1,1,1,1,1,1,1,1,
1,1,1,1,1,1,1,1,1,1,1,1,1,1,1,1,1,1,1,1,1,1,1,1,1,1,1,1,1,1,1,1,1,1,1,1,
1,1,1,1,1,1,1,1,1,1,1,1,1,1,1,1,1,1,1,1,1,1,1,1,1,1,1,1,1,1,1,1,1,1,1,1,
1,1,1,1,1,1,1,1,1,1,1,1,1,1,1,1,1,1,1,1,1,1,1,1,1,1,1,1,1,1,1,1,1,1,1,1,
1,1,1,1,1,1,1,1,1,1,1,1,1,1,1,1,1,1,1,1,1,1,1,1,1,1,1,1,1,1,1,1,1,1,1,1,
1,1,1,1,1,1,1,1,1,1,1,1,1,1,1,1,1,1,1,1,1,1,1,1,1,1,1,1,1,1,1,1,1,1,1,1,
1,1,1,1,1,1,1,1,1,1,1,1,1,1,1,1,1,1,1,1,1,1,1,1,1,1,1,1,1,1,1,1,1,1,1,1,
1,1,1,1,1,1,1,1,1,1,1,1,1,1,1,1,1,1,1,1,1,1,1,1,1,1,1,1,1,1,1,1,1,1,1,1,
1,1,1,1,1,1,1,1,1,1,1,1,1,1,1,1,1,1,1,1,1,1,1,1,1,1,1,1,1,1,1,1,1,1,1,1,
1,1,1,1,1,1,1,1,1,1,1,1,1,1,1,1,1,1,1,1,1,1,1,1,1,1,1,1,1,1,1,1,1,1,1,1,
1,1,1,1,1,1,1,1,1,1,1,1,1,1,1,1,1,1,1,1,1,1,1,1,1,1,1,1,1,1,1,1,1,1,1,1,
1,1,1,1,1,1,1,1,1,1,1,1,1,1,1,1,1,1,1,1,1,1,1,1,1,1,1,1,1,1,1,1,1,1,1,1,
1,1,1,1,1,1,1,1,1,1,1,1,1,1,1,1,1,1,1,1,1,1,1,1,1,1,1,1,1,1,1,1,1,1,1,1,
1,1,1,1,1,1,1,1,1,1,1,1,1,1,1,1,1,1,1,1,1,1,1,1,1,1,1,1,1,1,1,1,1,1,1,1,
1,1,1,1,1,1,1,1,1,1,1,1,1,1,1,1,1,1,1,1,1,1,1,1,1,1,1,1,1,1,1,1,1,1,1,1,
1,1,1,1,1,1,1,1,1,1,1,1,1,1,1,1,1,1,1,1,1,1,1,1,1,1,1,1,1,1,1,1,1,1,1,1,
1,1,1,1,1,1,1,1,1,1,1,1,1,1,1,1,1,1,1,1,1,1,1,1,1,1,1,1,1,1,1,1,1,1,1,1,
1,1,1,1,1,1,1,1,1,1,1,1,1,1,1,1,1,1,1,1,1,1,1,1,1,1,1,1,1,1,1,1,1,1,1,1,
1,1,1,1,1,1,1,1,1,1,1,1,1,1,1,1,1,1,1,1,1,1,1,1,1,1,1,1,1,1,1,1,1,1,1,1,
1,1,1,1,1,1,1,1,1,1,1,1,1,1,1,1,1,1,1,1,1,1,1,1,1,1,1,1,1,1,1,1,1,1,1,1,
1,1,1,1,1,1,1,1,1,1,1,1,1,1,1,1,1,1,1,1,1,1,1,1,1,1,1,1,1,1,1,1,1,1,1,1,
1,1,1,1,1,1,1,1,1,1,1,1,1,1,1,1,1,1,1,1,1,1,1,1,1,1,1,1,1,1,1,1,1,1,1,1,
1,1,1,1,1,1,1,1,1,1,1,1,1,1,1,1,1,1,1,1,1,1,1,1,1,1,1,1,1,1,1,1,1,1,1,1,
1,1,1,1,1,1,1,1,1,1,1,1,1,1,1,1,1,1,1,1,1,1,1,1,1,1,1,1,1,1,1,1,1,1,1,1,
1,1,1,1,1,1,1,1,1,1,1,1,1,1,1,1,1,1,1,1,1,1,1,1,1,1,1,1,1,1,1,1,1,1,1,1,
1,1,1,1,1,1,1,1,1,1,1,1,1,1,1,1,1,1,1,1,1,1,1,1,1,1,1,1,1,1,1,1,1,1,1,1,
1,1,1,1,1,1,1,1,1,1,1,1,1,1,1,1,1,1,1,1,1,1,1,1,1,1,1,1,1,1,1,1,1,1,1,1,
1,1,1,1,1,1,1,1,1,1,1,1,1,1,1,1,1,1,1,1,1,1,1,1,1,1,1,1,1,1,1,1,1,1,1,1,
1,1,1,1,1,1,1,1,1,1,1,1,1,1,1,1,1,1,1,1,1,1,1,1,1,1,1,1,1,1,1,1,1,1,1,1,
1,1,1,1,1,1,1,1,1,1,1,1,1,1,1,1,1,1,1,1,1,1,1,1,1,1,1,1,1,1,1,1,1,1,1,1,
1,1,1,1,1,1,1,1,1,1,1,1,1,1,1,1,1,1,1,1,1,1,1,1,1,1,1,1,1,1,1,1,1,1,1,1,
1,1,1,1,1,1,1,1,1,1,1,4),(3,2,2,2,3),(0.,0.01797683372391,0.286633051710584,
0.555289278308216,0.823945516665782,1.09260176953922,1.36125803873948,1.62991432588463,
1.89857063164012,2.16722695661301,2.43588330050525,2.70453966304674,2.9731960431531,
3.24185243981471,3.51050885133453,3.77916527610465,4.04782171198515,4.31647815691489,
4.58513460847725,4.85379106430677,5.12244752187208,5.39110397865606,5.65976043217153,
5.92841687990537,6.19707331956994,6.46572974881596,6.73438616570634,7.00304256821933,
7.2716989549161,7.5403553242696,7.809011675483,8.07766800769526,8.34632432089157,
8.61498061505147,8.8836368910788,9.15229314997201,9.4209493936865,9.68960562442157,
9.95826184531348,10.226918059948,10.4955742727586,10.7642304884925,11.0328867113173,
11.3015429448574,11.5701991918227,11.8388554546081,12.1075117346518,12.3761680332469,
12.6448243507434,12.9134806874637,13.1821370428496,13.450793416388,13.7194498067883,
13.9881062128412,14.2567626326955,14.5254190645885,14.7940755062772,15.0627319555912,
15.3313884100611,15.6000448672586,15.8687013246492,16.1373577797,16.4060142299691,
16.6746706729765,16.9433271065265,17.2119835283531,17.4806399366567,17.7492963295502,
18.0179527057767,18.286609063996,18.555265403637,18.8239217240786,19.0925780255742,
19.3612343083975,19.6298905737625,19.898546823017,20.1672030584666,20.4358592827168,
20.7045154992928,20.973171712245,21.2418279262962,21.5104841459723,21.7791403749736,
22.0477966165324,22.316452872948,22.585109146262,22.8537654375589,23.1224217478187,
23.3910780770929,23.6597344254327,23.9283907920352,24.197047176159,24.4657035763222,
24.7343599911301,25.0030164185931,25.2716728568073,25.5403293034427,25.8089857562333,
26.0776422126729,26.3462986702843,26.6149551265448,26.8836115789212,27.1522680250308,
27.4209244624423,27.6895808890659,27.9582373027346,28.2268937018004,28.4955500845261,
28.7642064498512,29.0328627966379,29.3015191245544,29.5701754332357,29.838831723217,
30.1074879950829,30.3761442503694,30.6448004907916,30.9134567190168,31.1821129380756,
31.450769151893,31.7194253649682,31.9880815819663,32.2567378070174,32.5253940433706,
32.7940502938785,33.0627065604467,33.3313628447765,33.6000191476151,33.8686754696427,
34.1373318106287,34.405988170366,34.6746445478242,34.9433009420458,35.2119573513747,
35.480613774244,35.7492702085419,36.0179266522368,36.2865831029275,36.5552395582669,
36.8238960157264,37.0925524727952,37.3612089269773,37.6298653757534,37.8985218168153,
38.1671782477952,38.4358346667239,38.7044910715485,38.9731474607866,39.2418038328672,
39.5104601869391,39.7791165220837,40.0477728382212,40.3164291352602,40.5850854140292,
40.8537416754418,41.1223979213679,41.3910541539077,41.6597103761025,41.9283665914244,
42.1970228042084,42.4656790192,42.7343352406829,43.0029914723808,43.2716477171096,
43.540303977354,43.8089602546436,44.0776165503516,44.3462728649052,44.614929198697,
44.883585551232,45.1522419220568,45.4208983099307,45.6895547136931,45.9582111315299,
46.2268675617156,46.4955240020317,46.7641804503338,47.0328369041642,47.3014933611089,
47.5701498186329,47.8388062742058,48.107462725373,48.3761191696448,48.6447756048012,
48.9134320285537,49.1820884390673,49.4507448344197,49.7194012133072,49.9880575743413,
50.2567139168934,50.5253702402807,50.7940265446884,51.0626828303152,51.3313390982961,
51.5999953498901,51.8686515873141,52.1373078130706,52.4059640305862,52.6746202437936,
52.9432764573682,53.211932675918,53.480588903259,53.7492451427202,54.0179013967021,
54.2865576673334,54.5552139557853,54.823870263115,55.0925265894471,55.3611829348992,
55.6298392987282,55.8984956802486,56.1671520780245,56.4358084907065,56.7044649163381,
56.9731213530494,57.2417777985307,57.5104342505384,57.7790907065743,58.0477471641719,
58.3164036208043,58.5850600739368,58.8537165211707,59.1223729600609,59.39102938849,
59.6596858042645,59.9283422056975,60.1969985910129,60.4656549590995,60.7343113087676,
61.0029676396243,61.2716239512389,61.540280244075,61.808936518638,62.0775927763821,
62.3462490189291,62.6149052488546,62.8835614690812,63.1522176834332,63.4208738963055,
63.6895301124163,63.9581863359981,64.2268425704115,64.4954988186027,64.7641550825741,
65.0328113641112,65.3014676640435,65.5701239831253,65.8387803211949,66.1074366781083,
66.3760930528907,66.6447494446373,66.9134058517341,67.1820622726558,67.4507187053199,
67.7193751477252,67.988031597487,68.256688052277,68.5253445095709,68.7940009668648,
69.0626574216546,69.3313138714164,69.5999703138218,69.8686267464858,70.1372831674076,
70.4059395745042,70.6745959662509,70.9432523410334,71.2119086979469,71.4805650360164,
71.7492213550982,72.0178776550306,72.2865339365675,72.5551902005389,72.8238464487301,
73.0925026831433,73.3611589067251,73.6298151228357,73.8984713357081,74.1671275500599,
74.4357837702864,74.7044400002118,74.9730962427587,75.2417525005027,75.5104087750655,
75.7790650679015,76.047721379516,76.3163777103726,76.5850340600405,76.853690428127,
77.1223468134422,77.391003214875,77.6596596306495,77.9283160590784,78.1969724979684,
78.4656289452021,78.7342853983344,79.0029418549666,79.2715983125641,79.5402547685998,
79.8089112206075,80.0775676660886,80.3462241027997,80.6148805284312,80.8835369411131,
81.1521933388889,81.4208497204091,81.689506084238,81.9581624296899,82.2268187560219,
82.4954750633515,82.7641313518033,83.0327876224345,83.3014438764161,83.5701001158772,
83.838756343218,84.1074125617677,84.3760687753422,84.6447249885494,84.913381206065,
85.1820374318212,85.4506936692451,85.719349920839,85.9880061888197,86.2566624744465,
86.5253187788541,86.7939751022413,87.0626314447932,87.3312878058273,87.5999441847146,
87.8686005800667,88.1372569905802,88.4059134143327,88.6745698494889,88.9432262937606,
89.2118827449277,89.4805392005005,89.7491956580243,90.0178521149689,90.2865085687992,
90.5551650171012,90.8238214574172,91.0924778876028,91.3611343054394,91.6297907092016,
91.8984470970753,92.1671034679,92.4357598204347,92.7044161542264,92.9730724687798,
93.2417287644878,93.5103850417773,93.7790413020216,94.0476975467502,94.3163537784479,
94.5850099999307,94.8536662149221,95.1223224277061,95.390978643028,95.6596348652226,
95.9282910977624,96.1969473436883,96.4656036051009,96.7342598838697,97.0029161809086,
97.2715724970461,97.5402288321905,97.8088851862623,98.0775415583427,98.3461979475807,
98.6148543524051,98.8835107713336,99.1521672023136,99.4208236433754,99.6894800921513,
99.9581365463333,100.226793003402,100.495449460861,100.7641059162,101.032762366891,
101.301418810586,101.570075244884,101.838731667753,102.107388077082,102.376044471303,
102.644700848761,102.913357208498,103.182013549484,103.450669871511,103.71932617435,
103.98798245868,104.256638725248,104.525294975755,104.793951212108,105.062607437159,
105.331263654157,105.599919867233,105.86857608105,106.137232300108,106.405888528334,
106.674544768756,106.943201024042,107.211857295908,107.480513585889,107.74916989457,
108.017826222487,108.286482569273,108.555138934598,108.823795317324,109.09245171639,
109.361108130058,109.629764556682,109.898420994093,110.167077440202,110.435733892579,
110.704390348839,110.97304680645,111.24170326289,111.51035971568,111.779016162316,
112.04767260053,112.316329027993,112.5849854428,112.853641842963,113.122298227087,
113.39095459369,113.659610942029,113.928267271303,114.196923581563,114.46557987286,
114.734236146174,115.002892402589,115.271548644148,115.540204873149,115.808861092825,
116.077517306876,116.346173519828,116.614829736404,116.883485960654,117.152142196103,
117.420798445358,117.689454710722,117.958110993546,118.226767295041,118.495423615483,
118.764079955123,119.032736313343,119.301392689569,119.570049082462,119.838705490766,
120.107361912592,120.376018346142,120.644674789149,120.913331239418,121.181987694469,
121.45064415186,121.719300609057,121.987957063527,122.256613512841,122.525269954529,
122.793926386422,123.062582806276,123.331239212329,123.599895602729,123.868551976268,
124.137208331653,124.405864668374,124.67452098587,124.943177284465,125.211833564508,
125.480489827294,125.749146074259,126.017802307799,126.286458530624,126.555114746357,
126.823770959168,127.092427173802,127.361083394694,127.629739625429,127.898395869143,
128.167052128037,128.435708404064,128.704364698224,128.97302101142,129.241677343633,
129.510333694846,129.7789900642,130.047646450897,130.31630285341,130.5849592703,
130.853615699547,131.122272139211,131.390928586945,131.659585040461,131.928241497245,
132.19689795481,132.46555441064,132.734210862202,133.002867307132,133.271523743013,
133.540180167783,133.808836579303,134.077492975965,134.346149356071,134.614805718613,
134.883462062505,135.152118387478,135.420774693234,135.689430980379,135.958087249579,
136.226743502453,136.49539974081,136.76405596741,137.032712185392,137.301368398783,
137.570024612174,137.838680830155,138.107337056755,138.375993295112,138.644649547986,
138.913305817186,139.181962104332,139.450618410087,139.71927473506,139.987931078952,
140.256587441494,140.525243821601,140.793900218262,141.062556629782,141.331213054552,
141.599869490433,141.868525935363,142.137182386925,142.405838842755,142.67449530032,
142.943151757104,143.21180821062,143.480464658354,143.749121098019,144.017777527265,
144.286433944155,144.555090346668,144.823746733365,145.092403102719,145.361059453932,
145.629715786145,145.898372099341,146.167028393501,146.435684669529,146.704340928422,
146.972997172137,147.241653402872,147.510309623764,147.778965838398,148.047622051209,
148.316278266943,148.584934489768,148.853590723308,149.122246970274,149.390903233059,
149.659559513103,149.928215811698,150.196872129195,150.465528465915,150.734184821301,
151.00284119484,151.27149758524,151.540153991293,151.808810411148,152.077466843041,
152.34612328473,152.614779734044,152.883436188514,153.152092645711,153.420749103102,
153.689405558153,153.958062008422,154.22671845143,154.49537488498,154.764031306806,
155.03268771511,155.301344108004,155.57000048423,155.838656842449,156.107313182091,
156.375969502532,156.644625804028,156.913282086851,157.181938352216,157.450594601471,
157.719250836921,157.987907061171,158.256563277747,158.525219490699,158.793875704751,
159.062531924427,159.331188153428,159.599844394987,159.868500651403,160.137156924717,
160.405813216014,160.674469526274,160.943125855548,161.211782203888,161.480438570491,
161.749094954615,162.017751354778,162.286407769586,162.555064197049,162.823720635263,
163.092377081899,163.361033534689,163.629689991129,163.898346448741,164.167002905001,
164.435659357378,164.704315803488,164.972972240899,165.241628667523,165.510285081192,
165.778941480257,166.047597862983,166.316254228308,166.584910575095,166.853566903012,
167.122223211693,167.390879501675,167.659535773541,167.928192028827,168.19684826925,
168.465504497475,168.734160716534,169.002816930351,169.271473143427,169.540129360425,
169.808785585476,170.077441821829,170.346098072337,170.614754338905,170.883410623235,
171.152066926074,171.420723248102,171.689379589088,171.958035948825,172.226692326284,
172.495348720505,172.764005129834,173.032661552704,173.301317987002,173.569974430697,
173.838630881388,174.107287336727,174.375943794187,174.644600251255,174.913256705437,
175.181913154214,175.450569595276,175.719226026256,175.987882445184,176.256538850009,
176.525195239247,176.793851611328,177.0625079654,177.331164300545,177.599820616682,
177.868476913721,178.137133192491,178.405789453903,178.674445699829,178.943101932369,
179.211758154564,179.480414369886,179.74907058267,180.017726797662,180.286383019145,
180.555039250843,180.823695495572,181.092351755816,181.361008033106,181.629664328814,
181.898320643368,182.16697697716,182.435633329695,182.70428970052,182.972946088394,
183.241602492156,183.510258909993,183.778915340179,184.047571780495,184.316228228797,
184.584884682628,184.853541139572,185.122197597096,185.39085405267,185.659510503837,
185.928166948109,186.196823383265,186.465479807018,186.734136217531,187.002792612884,
187.271448991771,187.540105352806,187.808761695358,188.077418018745,188.346074323153,
188.61473060878,188.883386876761,189.152043128355,189.420699365779,189.689355591536,
189.958011809051,190.226668022259,190.495324235834,190.763980454383,191.032636681725,
191.301292921186,191.569949175168,191.838605445799,192.107261734251,192.375918041581,
192.644574367913,192.913230713365,193.181887077194,193.450543458715,193.719199856491,
193.987856269173,194.256512694805,194.525169131516,194.793825576997,195.062482029005,
195.331138485041,195.599794942639,195.868451399271,196.137107852404,196.405764299638,
196.674420738528,196.943077166957,197.211733582732,197.480389984165,197.749046369481,
198.017702737567,198.286359087236,198.555015418092,198.823671729707,199.092328022543,
199.360984297106,199.62964055485,199.898296797397,200.166953027323,200.43560924755,
200.704265461902,200.972921674774,201.241577890885,201.510234114467,201.77889034888,
202.047546597072,202.316202861043,202.584859142581,202.853515442513,203.122171761595,
203.390828099665,203.659484456579,203.928140831361,204.196797223108,204.465453630205,
204.734110051127,205.002766483791,205.271422926197,205.540079375959,205.808735830749,
206.077392288043,206.346048745337,206.614705200127,206.883361649889,207.152018092295,
207.420674524959,207.689330945881,207.957987352978,208.226643744725,208.495300119508,
208.763956476421,209.032612814491,209.301269133573,209.569925433505,209.838581715043,
210.107237979014,210.375894227206,210.644550461619,210.913206685201,211.181862901312,
211.450519114184,211.719175328536,211.987831548763,212.256487778689,212.525144021236,
212.79380027898,213.062456553543,213.331112846379,213.599769157994,213.868425488851,
214.137081838519,214.405738206606,214.674394591921,214.943050993354,215.211707409129,
215.480363837558,215.749020276448,216.017676723682,216.286333176815,216.554989633447,
216.823646091045,217.092302547081,217.360958999089,217.62961544457,217.898271881281,
218.166928306913,218.435584719595,218.704241117371,218.972897498892,219.241553862721,
219.510210208173,219.778866534505,220.047522841835,220.316179130287,220.584835400918,
220.8534916549,221.122147894361,221.390804121702,221.659460340252,221.928116553827,
222.196772767034,222.46542898455,222.734085210306,223.00274144773,223.271397699324,
223.540053967305,223.808710252932,224.07736655734,224.346022880728,224.61467922328,
224.883335584314,225.151991963201,225.420648358554,225.689304769068,225.95796119282,
226.226617627977,226.495274072249,226.763930523416,227.032586978989,227.301243436513,
227.569899893458,227.838556347288,228.10721279559,228.375869235907,228.644525666093,
228.913182083929,229.181838487692,229.450494875566,229.719151246391,229.987807598926,
230.256463932718,230.525120247271,230.79377654298,231.062432820269,231.331089080514,
231.599745325243,231.868401556941,232.137057778424,232.405713993415,232.674370206199,
232.943026421521,233.211682643716,233.480338876256,233.748995122182,234.017651383595,
234.286307662364,234.554963959403,234.823620275541,235.092276610685,235.360932964757,
235.629589336838,235.898245726076,236.166902130901,236.43555854983,236.70421498081,
236.972871421872,237.241527870648,237.51018432483,237.778840781899,238.047497239359,
238.316153694698,238.584810145389,238.853466589084,239.122123023382,239.390779446251,
239.65943585558,239.928092249802,240.19674862726,240.465404986998,240.734061327984,
241.002717650011,241.27137395285,241.54003023718,241.808686503748,242.077342754256,
242.345998990609,242.614655215661,242.883311432659,243.151967645734,243.420623859552,
243.68928007861,243.957936306836,244.226592547258,244.495248802545,244.763905074411,
245.032561364392,245.301217673074,245.56987400099,245.838530347777,246.107186713102,
246.375843095828,246.644499494894,246.913155908563,247.181812335186,247.450468772598,
247.719125218708,247.987781671084,248.256438127345,248.525094584956,248.793751041396,
249.062407494187,249.331063940822,249.599720379036,249.8683768065,250.137033221308,
250.405689621471,250.674346005595,250.943002372197,251.211658720537,251.480315049812,
251.748971360071,252.017627651368,252.286283924683,252.554940181098,252.823596422657,
253.092252651658,253.360908871335,253.629565085386,253.898221298338,254.166877514914,
254.435533739165,254.704189974614,254.972846223869,255.241502489234,255.510158772057,
255.778815073553,256.047471393995,256.316127733635,256.584784091854,256.85344046808,
257.122096860973,257.390753269276,257.659409691102,257.928066124652,258.196722567659,
258.465379017928,258.734035472978,259.002691930368,259.271348387566,259.540004842035,
259.808661291349,260.077317733037,260.345974164929,260.614630584783,260.883286990836,
261.151943381235,261.420599754774,261.689256110159,261.957912446879,262.226568764375,
262.49522506297,262.763881343014,263.032537605798,263.301193852763,263.569850086303,
263.838506309127,264.107162524861,264.375818737671,264.644474952305,264.913131173196,
265.181787403931,265.450443647645,265.719099906538,265.987756182565,266.256412476724,
266.52506878992,266.793725122132,267.062381473345,267.331037842698,267.599694229394,
267.868350631907,268.137007048797,268.405663478042,268.674319917706,268.94297636544,
269.211632818955,269.480289275739,269.748945733304,270.017602189133,270.286258640695,
270.554915085624,270.823571521504,271.092227946274,271.360884357793,271.629540754454,
271.89819713456,272.166853497101,272.435509840993,272.704166165965,272.97282247172,
273.241478758865,273.510135028065,273.778791280938,274.047447519295,274.316103745894,
274.584759963875,274.853416177266,275.122072390656,275.390728608637,275.659384835237,
275.928041073593,276.196697326466,276.465353595666,276.734009882811,277.002666188566,
277.271322513539,277.53997885743,277.808635219972,278.077291600077,278.345947996739,
278.614604408258,278.883260833028,279.151917268908,279.420573713837,279.689230165399,
279.957886621228,280.226543078793,280.495199535576,280.763855989092,281.032512436825,
281.301168876489,281.569825305735,281.838481722625,282.107138125138,282.375794511834,
282.644450881187,282.9131072324,283.181763564612,283.450419877808,283.719076171967,
283.987732447994,284.256388706887,284.525044950601,284.793701181336,285.062357402228,
285.331013616862,285.599669829672,285.868326045405,286.136982268229,286.405638501769,
286.674294748734,286.942951011519,287.211607291562,287.480263590157,287.748919907653,
288.017576244373,288.286232599758,288.554888973296,288.823545363696,289.092201769749,
289.360858189603,289.629514621495,289.898171063183,290.166827512497,290.435483966966,
290.704140424163,290.972796881554,291.241453336604,291.510109786873,291.77876622988,
292.047422663429,292.316079085255,292.584735493559,292.853391886452,293.122048262678,
293.390704620897,293.659360960537,293.928017280978,294.196673582474,294.465329865297,
294.733986130661,295.002642379915,295.271298615364,295.539954839614,295.808611056189,
296.077267269141,296.345923483192,296.614579702867,296.883235931868,297.151892173427,
297.420548429842,297.689204703155,297.957860994452,298.226517304711,298.495173633985,
298.763829982324,299.032486348927,299.30114273305,299.569799133212,299.83845554802,
300.107111975482,300.375768413696,300.644424860331,300.913081313121,301.181737769561,
301.450394227172,301.719050683432,301.987707135808,302.256363581917,302.525020019328,
302.793676445951,303.062332859619,303.330989258684,303.59964564141,303.868302006734,
304.136958353521,304.405614681437,304.674270990118,304.942927280098,305.211583551964,
305.48023980725,305.748896047671,306.017552275896,306.286208494954,306.554864708772,
306.823520921846,307.092177138844,307.360833363895,307.629489600247,307.898145850755,
308.166802117323,308.435458401652,308.70411470449,308.972771026517,309.241427367503,
309.51008372724,309.778740104698,310.047396498919,310.316052908247,310.584709331116,
310.853365765414,311.122022209108,311.390678659798,311.659335115137,311.927991572596,
312.196648029665,312.465304483846,312.733960932622,313.002617373684,313.271273804663,
313.539930223591,313.808586628416,314.077243017653,314.345899389733,314.614555743805,
314.883212078949,315.151868395086,315.420524692125,315.689180970894,315.957837232306,
316.226493478231,316.495149710771,316.763805932965,317.032462148286,317.30111836107,
317.569774576061,317.838430797543,318.107087029241,318.375743273969,318.644399534213,
318.913055811502,319.18171210721,319.450368421763,319.719024755555,319.987681108089,
320.256337478914,320.524993866787,320.793650270549,321.062306688385,321.33096311857,
321.599619558886,321.868276007188,322.136932461018,322.405588917962,322.674245375486,
322.942901831059,323.211558282225,323.480214726497,323.748871161653,324.017527585405,
324.286183995918,324.55484039127,324.823496770157,325.09215313119,325.360809473742,
325.629465797129,325.898122101536,326.166778387163,326.435434655143,326.704090906737,
326.97274714416,327.241403369916,327.510059587432,327.778715800638,328.047372014213,
328.316028232762,328.584684460102,328.853340699563,329.121996953545,329.390653224175,
329.659309512627,329.927965819956,330.196622146288,330.46527849174,330.733934855568,
331.002591237088,331.271247634863,331.539904047545,331.808560473176,332.077216909887,
332.345873355368,332.614529807375,332.883186263411,333.151842721008,333.42049917764,
333.689155630772,333.957812078005,334.226468516895,334.495124945324,334.763781361098,
335.03243776253,335.301094147845,335.569750515931,335.838406865599,336.107063196455,
336.375719508069,336.644375800905,336.913032075468,337.181688333211,337.450344575758,
337.719000805683,337.987657025909,338.256313240261,338.524969453133,338.793625669243,
339.062281892824,339.330938127237,339.599594375428,339.868250639399,340.136906920936,
340.405563220868,340.674219539949,340.942875878019,341.211532234932,341.480188609714,
341.74884500146,342.017501408557,342.286157829478,342.554814262142,342.823470704547,
343.092127154308,343.360783609098,343.629440066391,343.898096523685,344.166752978475,
344.435409428236,344.704065870641,344.972722303305,345.241378724226,345.510035131323,
345.778691523069,346.047347897851,346.316004254764,346.584660592834,346.853316911915,
347.121973211847,347.390629493384,347.659285757355,347.927942005546,348.196598239959,
348.46525446354,348.733910679651,349.002566892523,349.271223106874,349.5398793271,
349.808535557025,350.077191799572,350.345848057315,350.614504331878,350.883160624714,
351.151816936328,351.420473267184,351.689129616852,351.957785984938,352.226442370253,
352.495098771685,352.76375518746,353.032411615888,353.301068054778,353.569724502012,
353.838380955144,354.107037411776,354.375693869373,354.644350325408,354.913006777416,
355.181663222896,355.450319659607,355.718976085238,355.98763249792,356.256288895695,
356.524945277215,356.793601641044,357.062257986496,357.330914312827,357.599570620156,
357.868226908608,358.136883179239,358.40553943322,358.674195672681,358.942851900021,
359.211508118571,359.480164332145,359.748820545352,360.017476762867,360.286132988623,
360.554789226047,360.82344547764,361.09210174562,361.360758031247,361.629414335654,
361.898070659041,362.166727001593,362.435383362626,362.704039741513,362.972696136865,
363.241352547378,363.510008971131,363.778665406287,364.047321850558,364.315978301725,
364.584634757297,364.853291214821,365.121947671765,365.390604125595,365.659260573897,
365.927917014213,366.196573444398,366.465229862234,366.733886265996,367.002542653869,
367.271199024694,367.539855377228,367.808511711019,368.077168025573,368.34582432128,
368.614480598569,368.883136858813,369.151793103542,369.420449335239,369.689105556722,
369.957761771713,370.226417984496,370.495074199818,370.763730422012,371.032386654551,
371.301042900477,371.569699161889,371.838355440658,372.107011737697,372.375668053834,
372.644324388978,372.912980743049,373.18163711513,373.450293504367,373.718949909191,
373.98760632812,374.256262759099,374.524919200161,374.793575648936,375.062232103118,
375.330888560186,375.599545017646,375.868201472985,376.136857923675,376.40551436737,
376.674170801667,376.942827224536,377.211483633864,377.480140028085,377.748796405543,
378.01745276528,378.286109106266,378.554765428293,378.823421731131,379.092078015461,
379.360734282028,379.629390532536,379.898046768888,380.166702993939,380.435359210937,
380.704015424011,380.972671637828,381.241327856887,381.509984085112,381.778640325533,
382.047296580819,382.315952852685,382.584609142666,382.853265451347,383.121921779263,
383.390578126049,383.659234491374,383.927890874099,384.196547273165,384.465203686833,
384.733860113456,385.002516550867,385.271172996977,385.539829449352,385.808485905613,
386.077142363224,386.345798819663,386.614455272453,386.883111719088,387.151768157302,
387.420424584764,387.689080999572,387.957737399735,388.226393783858,388.49505015046,
388.7637064988,389.032362828074,389.301019138333,389.56967542963,389.838331702943,
390.106987959358,390.375644200917,390.644300429918,390.912956649593,391.181612863644,
391.450269076596,391.718925293171,391.987581517421,392.25623775287,392.524894002124,
392.793550267489,393.062206550312,393.330862851807,393.599519172248,393.868175511888,
394.136831870107,394.405488246334,394.674144639227,394.94280104753,395.211457469356,
395.480113902905,395.748770345913,396.017426796181,396.286083251232,396.554739708622,
396.823396165819,397.092052620289,397.360709069602,397.629365511291,397.898021943183,
398.166678363037,398.43533476909,398.703991159489,398.972647533028,399.241303888413,
399.509960225133,399.778616542629,400.047272841224,400.315929121267,400.584585384052,
400.853241631017,401.121897864557,401.390554087381,401.659210303115,401.927866515925,
402.196522730559,402.465178951451,402.733835182185,403.002491425899,403.271147684792,
403.539803960819,403.808460254978,404.077116568174,404.345772900386,404.614429251599,
404.883085620952,405.151742007649,405.420398410161,405.689054827051,405.957711256297,
406.226367695961,406.495024143695,406.76368059721,407.032337053993,407.300993511558,
407.569649967387,407.838306418949,408.106962863879,408.375619299759,408.644275724528,
408.912932136048,409.181588532709,409.450244912815,409.718901275356,409.987557619248,
410.25621394422,410.524870249975,410.79352653712,411.06218280632,411.330839059193,
411.599495297549,411.868151524149,412.13680774213,412.40546395552,412.674120168911,
412.942776386892,413.211432613491,413.480088851848,413.748745104721,414.017401373921,
414.286057661065,414.55471396682,414.823370291793,415.092026635685,415.360682998226,
415.629339378332,415.897995774993,416.166652186512,416.435308611282,416.703965047162,
416.972621492092,417.241277943654,417.509934399483,417.778590857048,418.047247313831,
418.315903767346,418.58456021508,418.853216654744,419.121873083989,419.390529500879,
419.659185903392,419.927842290088,420.196498659441,420.465155010654,420.733811342866,
421.002467656062,421.271123950222,421.539780226249,421.808436485141,422.077092728855,
422.34574895959,422.614405180482,422.883061395116,423.151717607926,423.42037382366,
423.689030046484,423.957686280024,424.226342526988,424.494998789773,424.763655069817,
425.032311368411,425.300967685907,425.569624022627,425.838280378013,426.106936751551,
426.375593141951,426.644249548003,426.912905967857,427.18156239975,427.450218841438,
427.718875290752,427.987531745221,428.256188202418,428.524844659809,428.793501114859,
429.062157565128,429.330814008135,429.599470441684,429.868126863511,430.136783271814,
430.405439664707,430.674096040933,430.942752399152,431.211408738792,431.480065059233,
431.748721360729,432.017377643552,432.286033908916,432.554690158171,432.823346393619,
433.092002617869,433.360658834445,433.629315047397,433.897971261447,434.166627481123,
434.435283710124,434.703939951682,434.972596208097,435.241252481411,435.509908772707,
435.778565082967,436.047221412241,436.31587776058,436.584534127182,436.853190511305,
437.121846911468,437.390503326275,437.659159753738,437.927816191952,438.196472638587,
438.465129091377,438.733785547816,439.002442005427,439.271098461688,439.539754914064,
439.808411360173,440.077067797584,440.345724224207,440.614380637875,440.883037036941,
441.151693419666,441.420349784991,441.689006131777,441.957662459693,442.226318768374,
442.494975058355,442.763631330221,443.032287585506,443.300943825928,443.569600054153,
443.838256273211,444.106912487028,444.375568700103,444.644224917101,444.912881142151,
445.181537378504,445.450193629011,445.718849895579,445.987506179909,446.256162482747,
446.524818804774,446.79347514576,447.062131505496,447.330787882954,447.599444277176,
447.868100686504,448.136757109373,448.40541354367,448.674069987365,448.942726438055,
449.211382893394,449.480039350853,449.748695807921,450.017352262103,450.286008710879,
450.55466515194,450.82332158292,451.091978001848,451.360634406672,451.62929079591,
451.89794716799,452.166603522061,452.435259857205,452.703916173343,452.972572470381,
453.24122874915,453.509885010562,453.778541256488,454.047197489028,454.315853711222,
454.584509926543,454.853166139327,455.121822354318,455.3904785758,455.659134807498,
455.927791052226,456.19644731247,456.465103589759,456.733759885467,457.00241620002,
457.271072533811,457.539728886346,457.80838525717,458.077041645044,458.345698048806,
458.614354466642,458.883010896827,459.151667337143,459.420323785445,459.688980239275,
459.957636696219,460.226293153743,460.494949609316,460.763606060482,461.032262504754,
461.300918939909,461.569575363662,461.838231774175,462.106888169527,462.375544548414,
462.644200909447,462.912857251999,463.181513575386,463.450169879794,463.71882616542,
463.987482433401,464.256138684994,464.524794922418,464.793451148174,465.062107365689,
465.330763578896,465.59941979247,465.86807601102,466.13673223836,466.405388477821,
466.674044731802,466.942701002433,467.211357290885,467.480013598214,467.748669924546,
468.017326269997,468.285982633826,468.554639015346,468.823295413121,469.091951825803,
469.360608251434,469.629264688145,469.897921133626,470.166577585633,470.435234041669,
470.703890499266,470.972546955898,471.24120340903,471.509859856263,471.778516295153,
472.047172723582,472.315829139356,472.584485540789,472.853141926103,473.12179829419,
473.390454643857,473.659110974714,473.927767286328,474.196423579164,474.465079853726,
474.73373611147,475.002392354016,475.271048583941,475.539704804167,475.808361018519,
476.077017231391,476.345673447501,476.614329671083,476.882985905496,477.151642153686,
477.420298417658,477.688954699194,477.957610999126,478.226267318208,478.494923656277,
478.76358001319,479.032236387973,479.300892779719,479.569549186815,479.838205607737,
480.106862040401,480.375518482806,480.644174932567,480.912831387357,481.18148784465,
481.450144301944,481.718800756733,481.987457206495,482.2561136489,482.524770081563,
482.793426502485,483.062082909582,483.330739301328,483.59939567611,483.868052033023,
484.136708371092,484.405364690174,484.674020990106,484.942677271643,485.211333535614,
485.479989783805,485.748646018218,486.017302241799,486.28595845791,486.554614670781,
486.823270885133,487.091927105359,487.360583335284,487.629239577831,487.897895835574,
488.166552110137,488.435208402973,488.703864714587,488.972521045443,489.241177395111,
489.509833763197,489.778490148512,490.047146549945,490.315802965719,490.584459394147,
490.853115833037,491.12177228027,491.390428733402,491.659085190034,491.927741647632,
492.196398103667,492.465054555674,492.733711001155,493.002367437866,493.271023863497,
493.539680276179,493.808336673954,494.076993055474,494.345649419303,494.614305764754,
494.882962091086,495.151618398416,495.420274686867,495.688930957498,495.95758721148,
496.22624345094,496.494899678281,496.76355589683,497.032212110404,497.300868323611,
497.569524541126,497.838180766882,498.106837004306,498.3754932559,498.64414952388,
498.912805809507,499.181462113914,499.450118437301,499.718774779852,499.987431140886,
500.256087519773,500.524743915125,500.793400325638,501.06205674939,501.330713184546,
501.599369628818,501.868026079984,502.136682535557,502.40533899308,502.673995450025,
502.942651903855,503.211308352156,503.479964792472,503.748621222657,504.017277640494,
504.285934044256,504.554590432129,504.823246802954,505.091903155488,505.360559489279,
505.629215803832,505.89787209954,506.166528376829,506.435184637073,506.703840881801,
506.972497113499,507.241153334981,507.509809549972,507.778465762756,508.047121978078,
508.315778200272,508.584434432811,508.853090678737,509.121746940149,509.390403218918,
509.659059515956,509.927715832093,510.196372167238,510.465028521309,510.733684893389,
511.002341282627,511.270997687451,511.53965410638,511.808310537359,512.076966978421,
512.345623427198,512.614279881382,512.882936338452,513.151592795914,513.420249251254,
513.688905701946,513.957562145643,514.226218579942,514.494875002812,514.763531412143,
515.032187806366,515.300844183826,515.569500543564,515.838156884552,516.106813206581,
516.375469509421,516.644125793752,516.912782060321,517.181438310831,517.450094547186,
517.718750772238,517.987406989238,518.256063202315,518.524719416134,518.793375635194,
519.062031863421,519.330688103845,519.599344359133,519.868000631,520.136656920983,
520.405313229665,520.673969557583,520.942625904371,521.211282269698,521.479938652425,
521.748595051492,522.017251465163,522.285907891788,522.554564329201,522.823220775312,
523.091877227689,523.360533683951,523.629190141564,523.897846598005,524.166503050797,
524.435159497434,524.70381593565,524.972472363114,525.241128777924,525.509785178088,
525.778441562214,526.047097928818,526.315754277159,526.584410606435,526.853066916696,
527.121723207994,527.390379481309,527.659035737726,527.927691979287,528.19634820829,
528.465004427967,528.73366064202,529.002316854973,529.270973071551,529.539629295803,
529.808285531254,530.07694178051,530.345598045876,530.614254328701,530.882910630198,
531.151566950641,531.420223290284,531.688879648504,531.957536024733,532.226192417628,
532.494848825933,532.76350524776,533.032161681312,533.30081812432,533.569474574591,
533.838131029643,534.106787487035,534.375443944235,534.644100398706,534.912756848021,
535.181413289711,535.450069721605,535.718726141461,535.987382547516,536.256038937917,
536.524695311458,536.793351666845,537.062008003567,537.330664321065,537.599320619661,
537.867976899706,538.136633162493,538.40528940946,538.673945643001,538.942601865828,
539.211258081563,539.479914294375,539.748570509011,540.017226729904,540.285882960641,
540.554539204357,540.823195463252,541.09185173928,541.360508033441,541.629164346639,
541.897820678853,542.166477030068,542.435133399423,542.703789786121,542.972446188636,
543.241102605527,543.509759034775,543.778415474441,544.047071922176,544.315728375693,
544.584384832479,544.853041290046,545.121697745877,545.390354197441,545.659010642372,
545.927667078254,546.196323503025,546.464979914547,546.733636311202,547.002292691334,
547.270949053789,547.539605397955,547.808261722147,548.076918029812,548.345574313508,
548.614230583738,548.882886864851,549.151542935882,549.420199787641,549.68885445376,
549.957511414581),(0.,0.117809724509617,0.235619449019234,0.353429173528852,
0.471238898038469),.UNSPECIFIED.)
GEOMETRIC_REPRESENTATION_ITEM()
RATIONAL_B_SPLINE_SURFACE(((1.,0.707106781186548,1.,0.707106781186548,1.,
0.707106781186548,1.,0.707106781186548,1.),(1.,0.707106781186548,1.,0.707106781186548,
1.,0.707106781186548,1.,0.707106781186548,1.),(1.,0.707106781186548,1.,
0.707106781186548,1.,0.707106781186548,1.,0.707106781186548,1.),(1.,0.707106781186547,
1.,0.707106781186547,1.,0.707106781186547,1.,0.707106781186547,1.),(1.,
0.707106781186547,1.,0.707106781186547,1.,0.707106781186547,1.,0.707106781186547,
1.),(1.,0.707106781186548,1.,0.707106781186548,1.,0.707106781186548,1.,
0.707106781186548,1.),(1.,0.707106781186547,1.,0.707106781186547,1.,0.707106781186547,
1.,0.707106781186547,1.),(1.,0.707106781186547,1.,0.707106781186547,1.,
0.707106781186547,1.,0.707106781186547,1.),(1.,0.707106781186547,1.,0.707106781186547,
1.,0.707106781186547,1.,0.707106781186547,1.),(1.,0.707106781186547,1.,
0.707106781186547,1.,0.707106781186547,1.,0.707106781186547,1.),(1.,0.707106781186547,
1.,0.707106781186547,1.,0.707106781186547,1.,0.707106781186547,1.),(1.,
0.707106781186548,1.,0.707106781186548,1.,0.707106781186548,1.,0.707106781186548,
1.),(1.,0.707106781186548,1.,0.707106781186548,1.,0.707106781186548,1.,
0.707106781186548,1.),(1.,0.707106781186548,1.,0.707106781186548,1.,0.707106781186548,
1.,0.707106781186548,1.),(1.,0.707106781186547,1.,0.707106781186547,1.,
0.707106781186547,1.,0.707106781186547,1.),(1.,0.707106781186548,1.,0.707106781186548,
1.,0.707106781186548,1.,0.707106781186548,1.),(1.,0.707106781186547,1.,
0.707106781186547,1.,0.707106781186547,1.,0.707106781186547,1.),(1.,0.707106781186547,
1.,0.707106781186547,1.,0.707106781186547,1.,0.707106781186547,1.),(1.,
0.707106781186548,1.,0.707106781186548,1.,0.707106781186548,1.,0.707106781186548,
1.),(1.,0.707106781186547,1.,0.707106781186547,1.,0.707106781186547,1.,
0.707106781186547,1.),(1.,0.707106781186548,1.,0.707106781186548,1.,0.707106781186548,
1.,0.707106781186548,1.),(1.,0.707106781186547,1.,0.707106781186547,1.,
0.707106781186547,1.,0.707106781186547,1.),(1.,0.707106781186548,1.,0.707106781186548,
1.,0.707106781186548,1.,0.707106781186548,1.),(1.,0.707106781186547,1.,
0.707106781186547,1.,0.707106781186547,1.,0.707106781186547,1.),(1.,0.707106781186548,
1.,0.707106781186548,1.,0.707106781186548,1.,0.707106781186548,1.),(1.,
0.707106781186547,1.,0.707106781186547,1.,0.707106781186547,1.,0.707106781186547,
1.),(1.,0.707106781186547,1.,0.707106781186547,1.,0.707106781186547,1.,
0.707106781186547,1.),(1.,0.707106781186547,1.,0.707106781186547,1.,0.707106781186547,
1.,0.707106781186547,1.),(1.,0.707106781186547,1.,0.707106781186547,1.,
0.707106781186547,1.,0.707106781186547,1.),(1.,0.707106781186547,1.,0.707106781186547,
1.,0.707106781186547,1.,0.707106781186547,1.),(1.,0.707106781186548,1.,
0.707106781186548,1.,0.707106781186548,1.,0.707106781186548,1.),(1.,0.707106781186547,
1.,0.707106781186547,1.,0.707106781186547,1.,0.707106781186547,1.),(1.,
0.707106781186547,1.,0.707106781186547,1.,0.707106781186547,1.,0.707106781186547,
1.),(1.,0.707106781186548,1.,0.707106781186548,1.,0.707106781186548,1.,
0.707106781186548,1.),(1.,0.707106781186547,1.,0.707106781186547,1.,0.707106781186547,
1.,0.707106781186547,1.),(1.,0.707106781186547,1.,0.707106781186547,1.,
0.707106781186547,1.,0.707106781186547,1.),(1.,0.707106781186548,1.,0.707106781186548,
1.,0.707106781186548,1.,0.707106781186548,1.),(1.,0.707106781186547,1.,
0.707106781186547,1.,0.707106781186547,1.,0.707106781186547,1.),(1.,0.707106781186547,
1.,0.707106781186547,1.,0.707106781186547,1.,0.707106781186547,1.),(1.,
0.707106781186548,1.,0.707106781186548,1.,0.707106781186548,1.,0.707106781186548,
1.),(1.,0.707106781186548,1.,0.707106781186548,1.,0.707106781186548,1.,
0.707106781186548,1.),(1.,0.707106781186547,1.,0.707106781186547,1.,0.707106781186547,
1.,0.707106781186547,1.),(1.,0.707106781186548,1.,0.707106781186548,1.,
0.707106781186548,1.,0.707106781186548,1.),(1.,0.707106781186547,1.,0.707106781186547,
1.,0.707106781186547,1.,0.707106781186547,1.),(1.,0.707106781186547,1.,
0.707106781186547,1.,0.707106781186547,1.,0.707106781186547,1.),(1.,0.707106781186547,
1.,0.707106781186547,1.,0.707106781186547,1.,0.707106781186547,1.),(1.,
0.707106781186548,1.,0.707106781186548,1.,0.707106781186548,1.,0.707106781186548,
1.),(1.,0.707106781186548,1.,0.707106781186548,1.,0.707106781186548,1.,
0.707106781186548,1.),(1.,0.707106781186547,1.,0.707106781186547,1.,0.707106781186547,
1.,0.707106781186547,1.),(1.,0.707106781186547,1.,0.707106781186547,1.,
0.707106781186547,1.,0.707106781186547,1.),(1.,0.707106781186548,1.,0.707106781186548,
1.,0.707106781186548,1.,0.707106781186548,1.),(1.,0.707106781186547,1.,
0.707106781186547,1.,0.707106781186547,1.,0.707106781186547,1.),(1.,0.707106781186548,
1.,0.707106781186548,1.,0.707106781186548,1.,0.707106781186548,1.),(1.,
0.707106781186547,1.,0.707106781186547,1.,0.707106781186547,1.,0.707106781186547,
1.),(1.,0.707106781186547,1.,0.707106781186547,1.,0.707106781186547,1.,
0.707106781186547,1.),(1.,0.707106781186547,1.,0.707106781186547,1.,0.707106781186547,
1.,0.707106781186547,1.),(1.,0.707106781186547,1.,0.707106781186547,1.,
0.707106781186547,1.,0.707106781186547,1.),(1.,0.707106781186547,1.,0.707106781186547,
1.,0.707106781186547,1.,0.707106781186547,1.),(1.,0.707106781186548,1.,
0.707106781186548,1.,0.707106781186548,1.,0.707106781186548,1.),(1.,0.707106781186547,
1.,0.707106781186547,1.,0.707106781186547,1.,0.707106781186547,1.),(1.,
0.707106781186548,1.,0.707106781186548,1.,0.707106781186548,1.,0.707106781186548,
1.),(1.,0.707106781186547,1.,0.707106781186547,1.,0.707106781186547,1.,
0.707106781186547,1.),(1.,0.707106781186548,1.,0.707106781186548,1.,0.707106781186548,
1.,0.707106781186548,1.),(1.,0.707106781186547,1.,0.707106781186547,1.,
0.707106781186547,1.,0.707106781186547,1.),(1.,0.707106781186548,1.,0.707106781186548,
1.,0.707106781186548,1.,0.707106781186548,1.),(1.,0.707106781186547,1.,
0.707106781186547,1.,0.707106781186547,1.,0.707106781186547,1.),(1.,0.707106781186547,
1.,0.707106781186547,1.,0.707106781186547,1.,0.707106781186547,1.),(1.,
0.707106781186548,1.,0.707106781186548,1.,0.707106781186548,1.,0.707106781186548,
1.),(1.,0.707106781186547,1.,0.707106781186547,1.,0.707106781186547,1.,
0.707106781186547,1.),(1.,0.707106781186547,1.,0.707106781186547,1.,0.707106781186547,
1.,0.707106781186547,1.),(1.,0.707106781186548,1.,0.707106781186548,1.,
0.707106781186548,1.,0.707106781186548,1.),(1.,0.707106781186547,1.,0.707106781186547,
1.,0.707106781186547,1.,0.707106781186547,1.),(1.,0.707106781186548,1.,
0.707106781186548,1.,0.707106781186548,1.,0.707106781186548,1.),(1.,0.707106781186547,
1.,0.707106781186547,1.,0.707106781186547,1.,0.707106781186547,1.),(1.,
0.707106781186548,1.,0.707106781186548,1.,0.707106781186548,1.,0.707106781186548,
1.),(1.,0.707106781186548,1.,0.707106781186548,1.,0.707106781186548,1.,
0.707106781186548,1.),(1.,0.707106781186547,1.,0.707106781186547,1.,0.707106781186547,
1.,0.707106781186547,1.),(1.,0.707106781186548,1.,0.707106781186548,1.,
0.707106781186548,1.,0.707106781186548,1.),(1.,0.707106781186547,1.,0.707106781186547,
1.,0.707106781186547,1.,0.707106781186547,1.),(1.,0.707106781186547,1.,
0.707106781186547,1.,0.707106781186547,1.,0.707106781186547,1.),(1.,0.707106781186548,
1.,0.707106781186548,1.,0.707106781186548,1.,0.707106781186548,1.),(1.,
0.707106781186547,1.,0.707106781186547,1.,0.707106781186547,1.,0.707106781186547,
1.),(1.,0.707106781186547,1.,0.707106781186547,1.,0.707106781186547,1.,
0.707106781186547,1.),(1.,0.707106781186547,1.,0.707106781186547,1.,0.707106781186547,
1.,0.707106781186547,1.),(1.,0.707106781186548,1.,0.707106781186548,1.,
0.707106781186548,1.,0.707106781186548,1.),(1.,0.707106781186547,1.,0.707106781186547,
1.,0.707106781186547,1.,0.707106781186547,1.),(1.,0.707106781186547,1.,
0.707106781186547,1.,0.707106781186547,1.,0.707106781186547,1.),(1.,0.707106781186547,
1.,0.707106781186547,1.,0.707106781186547,1.,0.707106781186547,1.),(1.,
0.707106781186547,1.,0.707106781186547,1.,0.707106781186547,1.,0.707106781186547,
1.),(1.,0.707106781186547,1.,0.707106781186547,1.,0.707106781186547,1.,
0.707106781186547,1.),(1.,0.707106781186547,1.,0.707106781186547,1.,0.707106781186547,
1.,0.707106781186547,1.),(1.,0.707106781186548,1.,0.707106781186548,1.,
0.707106781186548,1.,0.707106781186548,1.),(1.,0.707106781186548,1.,0.707106781186548,
1.,0.707106781186548,1.,0.707106781186548,1.),(1.,0.707106781186547,1.,
0.707106781186547,1.,0.707106781186547,1.,0.707106781186547,1.),(1.,0.707106781186548,
1.,0.707106781186548,1.,0.707106781186548,1.,0.707106781186548,1.),(1.,
0.707106781186547,1.,0.707106781186547,1.,0.707106781186547,1.,0.707106781186547,
1.),(1.,0.707106781186548,1.,0.707106781186548,1.,0.707106781186548,1.,
0.707106781186548,1.),(1.,0.707106781186548,1.,0.707106781186548,1.,0.707106781186548,
1.,0.707106781186548,1.),(1.,0.707106781186547,1.,0.707106781186547,1.,
0.707106781186547,1.,0.707106781186547,1.),(1.,0.707106781186548,1.,0.707106781186548,
1.,0.707106781186548,1.,0.707106781186548,1.),(1.,0.707106781186548,1.,
0.707106781186548,1.,0.707106781186548,1.,0.707106781186548,1.),(1.,0.707106781186548,
1.,0.707106781186548,1.,0.707106781186548,1.,0.707106781186548,1.),(1.,
0.707106781186547,1.,0.707106781186547,1.,0.707106781186547,1.,0.707106781186547,
1.),(1.,0.707106781186548,1.,0.707106781186548,1.,0.707106781186548,1.,
0.707106781186548,1.),(1.,0.707106781186547,1.,0.707106781186547,1.,0.707106781186547,
1.,0.707106781186547,1.),(1.,0.707106781186548,1.,0.707106781186548,1.,
0.707106781186548,1.,0.707106781186548,1.),(1.,0.707106781186548,1.,0.707106781186548,
1.,0.707106781186548,1.,0.707106781186548,1.),(1.,0.707106781186548,1.,
0.707106781186548,1.,0.707106781186548,1.,0.707106781186548,1.),(1.,0.707106781186547,
1.,0.707106781186547,1.,0.707106781186547,1.,0.707106781186547,1.),(1.,
0.707106781186547,1.,0.707106781186547,1.,0.707106781186547,1.,0.707106781186547,
1.),(1.,0.707106781186547,1.,0.707106781186547,1.,0.707106781186547,1.,
0.707106781186547,1.),(1.,0.707106781186548,1.,0.707106781186548,1.,0.707106781186548,
1.,0.707106781186548,1.),(1.,0.707106781186548,1.,0.707106781186548,1.,
0.707106781186548,1.,0.707106781186548,1.),(1.,0.707106781186548,1.,0.707106781186548,
1.,0.707106781186548,1.,0.707106781186548,1.),(1.,0.707106781186547,1.,
0.707106781186547,1.,0.707106781186547,1.,0.707106781186547,1.),(1.,0.707106781186547,
1.,0.707106781186547,1.,0.707106781186547,1.,0.707106781186547,1.),(1.,
0.707106781186547,1.,0.707106781186547,1.,0.707106781186547,1.,0.707106781186547,
1.),(1.,0.707106781186548,1.,0.707106781186548,1.,0.707106781186548,1.,
0.707106781186548,1.),(1.,0.707106781186548,1.,0.707106781186548,1.,0.707106781186548,
1.,0.707106781186548,1.),(1.,0.707106781186547,1.,0.707106781186547,1.,
0.707106781186547,1.,0.707106781186547,1.),(1.,0.707106781186547,1.,0.707106781186547,
1.,0.707106781186547,1.,0.707106781186547,1.),(1.,0.707106781186548,1.,
0.707106781186548,1.,0.707106781186548,1.,0.707106781186548,1.),(1.,0.707106781186547,
1.,0.707106781186547,1.,0.707106781186547,1.,0.707106781186547,1.),(1.,
0.707106781186547,1.,0.707106781186547,1.,0.707106781186547,1.,0.707106781186547,
1.),(1.,0.707106781186547,1.,0.707106781186547,1.,0.707106781186547,1.,
0.707106781186547,1.),(1.,0.707106781186547,1.,0.707106781186547,1.,0.707106781186547,
1.,0.707106781186547,1.),(1.,0.707106781186548,1.,0.707106781186548,1.,
0.707106781186548,1.,0.707106781186548,1.),(1.,0.707106781186547,1.,0.707106781186547,
1.,0.707106781186547,1.,0.707106781186547,1.),(1.,0.707106781186548,1.,
0.707106781186548,1.,0.707106781186548,1.,0.707106781186548,1.),(1.,0.707106781186547,
1.,0.707106781186547,1.,0.707106781186547,1.,0.707106781186547,1.),(1.,
0.707106781186547,1.,0.707106781186547,1.,0.707106781186547,1.,0.707106781186547,
1.),(1.,0.707106781186547,1.,0.707106781186547,1.,0.707106781186547,1.,
0.707106781186547,1.),(1.,0.707106781186548,1.,0.707106781186548,1.,0.707106781186548,
1.,0.707106781186548,1.),(1.,0.707106781186548,1.,0.707106781186548,1.,
0.707106781186548,1.,0.707106781186548,1.),(1.,0.707106781186547,1.,0.707106781186547,
1.,0.707106781186547,1.,0.707106781186547,1.),(1.,0.707106781186548,1.,
0.707106781186548,1.,0.707106781186548,1.,0.707106781186548,1.),(1.,0.707106781186548,
1.,0.707106781186548,1.,0.707106781186548,1.,0.707106781186548,1.),(1.,
0.707106781186547,1.,0.707106781186547,1.,0.707106781186547,1.,0.707106781186547,
1.),(1.,0.707106781186548,1.,0.707106781186548,1.,0.707106781186548,1.,
0.707106781186548,1.),(1.,0.707106781186547,1.,0.707106781186547,1.,0.707106781186547,
1.,0.707106781186547,1.),(1.,0.707106781186548,1.,0.707106781186548,1.,
0.707106781186548,1.,0.707106781186548,1.),(1.,0.707106781186547,1.,0.707106781186547,
1.,0.707106781186547,1.,0.707106781186547,1.),(1.,0.707106781186548,1.,
0.707106781186548,1.,0.707106781186548,1.,0.707106781186548,1.),(1.,0.707106781186547,
1.,0.707106781186547,1.,0.707106781186547,1.,0.707106781186547,1.),(1.,
0.707106781186547,1.,0.707106781186547,1.,0.707106781186547,1.,0.707106781186547,
1.),(1.,0.707106781186548,1.,0.707106781186548,1.,0.707106781186548,1.,
0.707106781186548,1.),(1.,0.707106781186547,1.,0.707106781186547,1.,0.707106781186547,
1.,0.707106781186547,1.),(1.,0.707106781186547,1.,0.707106781186547,1.,
0.707106781186547,1.,0.707106781186547,1.),(1.,0.707106781186548,1.,0.707106781186548,
1.,0.707106781186548,1.,0.707106781186548,1.),(1.,0.707106781186547,1.,
0.707106781186547,1.,0.707106781186547,1.,0.707106781186547,1.),(1.,0.707106781186547,
1.,0.707106781186547,1.,0.707106781186547,1.,0.707106781186547,1.),(1.,
0.707106781186548,1.,0.707106781186548,1.,0.707106781186548,1.,0.707106781186548,
1.),(1.,0.707106781186547,1.,0.707106781186547,1.,0.707106781186547,1.,
0.707106781186547,1.),(1.,0.707106781186548,1.,0.707106781186548,1.,0.707106781186548,
1.,0.707106781186548,1.),(1.,0.707106781186547,1.,0.707106781186547,1.,
0.707106781186547,1.,0.707106781186547,1.),(1.,0.707106781186547,1.,0.707106781186547,
1.,0.707106781186547,1.,0.707106781186547,1.),(1.,0.707106781186548,1.,
0.707106781186548,1.,0.707106781186548,1.,0.707106781186548,1.),(1.,0.707106781186548,
1.,0.707106781186548,1.,0.707106781186548,1.,0.707106781186548,1.),(1.,
0.707106781186547,1.,0.707106781186547,1.,0.707106781186547,1.,0.707106781186547,
1.),(1.,0.707106781186548,1.,0.707106781186548,1.,0.707106781186548,1.,
0.707106781186548,1.),(1.,0.707106781186547,1.,0.707106781186547,1.,0.707106781186547,
1.,0.707106781186547,1.),(1.,0.707106781186548,1.,0.707106781186548,1.,
0.707106781186548,1.,0.707106781186548,1.),(1.,0.707106781186547,1.,0.707106781186547,
1.,0.707106781186547,1.,0.707106781186547,1.),(1.,0.707106781186548,1.,
0.707106781186548,1.,0.707106781186548,1.,0.707106781186548,1.),(1.,0.707106781186547,
1.,0.707106781186547,1.,0.707106781186547,1.,0.707106781186547,1.),(1.,
0.707106781186548,1.,0.707106781186548,1.,0.707106781186548,1.,0.707106781186548,
1.),(1.,0.707106781186547,1.,0.707106781186547,1.,0.707106781186547,1.,
0.707106781186547,1.),(1.,0.707106781186548,1.,0.707106781186548,1.,0.707106781186548,
1.,0.707106781186548,1.),(1.,0.707106781186547,1.,0.707106781186547,1.,
0.707106781186547,1.,0.707106781186547,1.),(1.,0.707106781186548,1.,0.707106781186548,
1.,0.707106781186548,1.,0.707106781186548,1.),(1.,0.707106781186547,1.,
0.707106781186547,1.,0.707106781186547,1.,0.707106781186547,1.),(1.,0.707106781186548,
1.,0.707106781186548,1.,0.707106781186548,1.,0.707106781186548,1.),(1.,
0.707106781186547,1.,0.707106781186547,1.,0.707106781186547,1.,0.707106781186547,
1.),(1.,0.707106781186547,1.,0.707106781186547,1.,0.707106781186547,1.,
0.707106781186547,1.),(1.,0.707106781186548,1.,0.707106781186548,1.,0.707106781186548,
1.,0.707106781186548,1.),(1.,0.707106781186547,1.,0.707106781186547,1.,
0.707106781186547,1.,0.707106781186547,1.),(1.,0.707106781186548,1.,0.707106781186548,
1.,0.707106781186548,1.,0.707106781186548,1.),(1.,0.707106781186547,1.,
0.707106781186547,1.,0.707106781186547,1.,0.707106781186547,1.),(1.,0.707106781186548,
1.,0.707106781186548,1.,0.707106781186548,1.,0.707106781186548,1.),(1.,
0.707106781186547,1.,0.707106781186547,1.,0.707106781186547,1.,0.707106781186547,
1.),(1.,0.707106781186548,1.,0.707106781186548,1.,0.707106781186548,1.,
0.707106781186548,1.),(1.,0.707106781186547,1.,0.707106781186547,1.,0.707106781186547,
1.,0.707106781186547,1.),(1.,0.707106781186547,1.,0.707106781186547,1.,
0.707106781186547,1.,0.707106781186547,1.),(1.,0.707106781186548,1.,0.707106781186548,
1.,0.707106781186548,1.,0.707106781186548,1.),(1.,0.707106781186547,1.,
0.707106781186547,1.,0.707106781186547,1.,0.707106781186547,1.),(1.,0.707106781186548,
1.,0.707106781186548,1.,0.707106781186548,1.,0.707106781186548,1.),(1.,
0.707106781186548,1.,0.707106781186548,1.,0.707106781186548,1.,0.707106781186548,
1.),(1.,0.707106781186548,1.,0.707106781186548,1.,0.707106781186548,1.,
0.707106781186548,1.),(1.,0.707106781186547,1.,0.707106781186547,1.,0.707106781186547,
1.,0.707106781186547,1.),(1.,0.707106781186547,1.,0.707106781186547,1.,
0.707106781186547,1.,0.707106781186547,1.),(1.,0.707106781186547,1.,0.707106781186547,
1.,0.707106781186547,1.,0.707106781186547,1.),(1.,0.707106781186547,1.,
0.707106781186547,1.,0.707106781186547,1.,0.707106781186547,1.),(1.,0.707106781186548,
1.,0.707106781186548,1.,0.707106781186548,1.,0.707106781186548,1.),(1.,
0.707106781186547,1.,0.707106781186547,1.,0.707106781186547,1.,0.707106781186547,
1.),(1.,0.707106781186548,1.,0.707106781186548,1.,0.707106781186548,1.,
0.707106781186548,1.),(1.,0.707106781186548,1.,0.707106781186548,1.,0.707106781186548,
1.,0.707106781186548,1.),(1.,0.707106781186547,1.,0.707106781186547,1.,
0.707106781186547,1.,0.707106781186547,1.),(1.,0.707106781186547,1.,0.707106781186547,
1.,0.707106781186547,1.,0.707106781186547,1.),(1.,0.707106781186548,1.,
0.707106781186548,1.,0.707106781186548,1.,0.707106781186548,1.),(1.,0.707106781186548,
1.,0.707106781186548,1.,0.707106781186548,1.,0.707106781186548,1.),(1.,
0.707106781186547,1.,0.707106781186547,1.,0.707106781186547,1.,0.707106781186547,
1.),(1.,0.707106781186547,1.,0.707106781186547,1.,0.707106781186547,1.,
0.707106781186547,1.),(1.,0.707106781186548,1.,0.707106781186548,1.,0.707106781186548,
1.,0.707106781186548,1.),(1.,0.707106781186547,1.,0.707106781186547,1.,
0.707106781186547,1.,0.707106781186547,1.),(1.,0.707106781186548,1.,0.707106781186548,
1.,0.707106781186548,1.,0.707106781186548,1.),(1.,0.707106781186547,1.,
0.707106781186547,1.,0.707106781186547,1.,0.707106781186547,1.),(1.,0.707106781186547,
1.,0.707106781186547,1.,0.707106781186547,1.,0.707106781186547,1.),(1.,
0.707106781186547,1.,0.707106781186547,1.,0.707106781186547,1.,0.707106781186547,
1.),(1.,0.707106781186547,1.,0.707106781186547,1.,0.707106781186547,1.,
0.707106781186547,1.),(1.,0.707106781186547,1.,0.707106781186547,1.,0.707106781186547,
1.,0.707106781186547,1.),(1.,0.707106781186547,1.,0.707106781186547,1.,
0.707106781186547,1.,0.707106781186547,1.),(1.,0.707106781186547,1.,0.707106781186547,
1.,0.707106781186547,1.,0.707106781186547,1.),(1.,0.707106781186548,1.,
0.707106781186548,1.,0.707106781186548,1.,0.707106781186548,1.),(1.,0.707106781186547,
1.,0.707106781186547,1.,0.707106781186547,1.,0.707106781186547,1.),(1.,
0.707106781186548,1.,0.707106781186548,1.,0.707106781186548,1.,0.707106781186548,
1.),(1.,0.707106781186547,1.,0.707106781186547,1.,0.707106781186547,1.,
0.707106781186547,1.),(1.,0.707106781186548,1.,0.707106781186548,1.,0.707106781186548,
1.,0.707106781186548,1.),(1.,0.707106781186548,1.,0.707106781186548,1.,
0.707106781186548,1.,0.707106781186548,1.),(1.,0.707106781186547,1.,0.707106781186547,
1.,0.707106781186547,1.,0.707106781186547,1.),(1.,0.707106781186548,1.,
0.707106781186548,1.,0.707106781186548,1.,0.707106781186548,1.),(1.,0.707106781186548,
1.,0.707106781186548,1.,0.707106781186548,1.,0.707106781186548,1.),(1.,
0.707106781186548,1.,0.707106781186548,1.,0.707106781186548,1.,0.707106781186548,
1.),(1.,0.707106781186548,1.,0.707106781186548,1.,0.707106781186548,1.,
0.707106781186548,1.),(1.,0.707106781186547,1.,0.707106781186547,1.,0.707106781186547,
1.,0.707106781186547,1.),(1.,0.707106781186548,1.,0.707106781186548,1.,
0.707106781186548,1.,0.707106781186548,1.),(1.,0.707106781186547,1.,0.707106781186547,
1.,0.707106781186547,1.,0.707106781186547,1.),(1.,0.707106781186548,1.,
0.707106781186548,1.,0.707106781186548,1.,0.707106781186548,1.),(1.,0.707106781186547,
1.,0.707106781186547,1.,0.707106781186547,1.,0.707106781186547,1.),(1.,
0.707106781186547,1.,0.707106781186547,1.,0.707106781186547,1.,0.707106781186547,
1.),(1.,0.707106781186548,1.,0.707106781186548,1.,0.707106781186548,1.,
0.707106781186548,1.),(1.,0.707106781186548,1.,0.707106781186548,1.,0.707106781186548,
1.,0.707106781186548,1.),(1.,0.707106781186547,1.,0.707106781186547,1.,
0.707106781186547,1.,0.707106781186547,1.),(1.,0.707106781186547,1.,0.707106781186547,
1.,0.707106781186547,1.,0.707106781186547,1.),(1.,0.707106781186547,1.,
0.707106781186547,1.,0.707106781186547,1.,0.707106781186547,1.),(1.,0.707106781186547,
1.,0.707106781186547,1.,0.707106781186547,1.,0.707106781186547,1.),(1.,
0.707106781186547,1.,0.707106781186547,1.,0.707106781186547,1.,0.707106781186547,
1.),(1.,0.707106781186548,1.,0.707106781186548,1.,0.707106781186548,1.,
0.707106781186548,1.),(1.,0.707106781186548,1.,0.707106781186548,1.,0.707106781186548,
1.,0.707106781186548,1.),(1.,0.707106781186547,1.,0.707106781186547,1.,
0.707106781186547,1.,0.707106781186547,1.),(1.,0.707106781186547,1.,0.707106781186547,
1.,0.707106781186547,1.,0.707106781186547,1.),(1.,0.707106781186548,1.,
0.707106781186548,1.,0.707106781186548,1.,0.707106781186548,1.),(1.,0.707106781186548,
1.,0.707106781186548,1.,0.707106781186548,1.,0.707106781186548,1.),(1.,
0.707106781186547,1.,0.707106781186547,1.,0.707106781186547,1.,0.707106781186547,
1.),(1.,0.707106781186548,1.,0.707106781186548,1.,0.707106781186548,1.,
0.707106781186548,1.),(1.,0.707106781186547,1.,0.707106781186547,1.,0.707106781186547,
1.,0.707106781186547,1.),(1.,0.707106781186548,1.,0.707106781186548,1.,
0.707106781186548,1.,0.707106781186548,1.),(1.,0.707106781186548,1.,0.707106781186548,
1.,0.707106781186548,1.,0.707106781186548,1.),(1.,0.707106781186547,1.,
0.707106781186547,1.,0.707106781186547,1.,0.707106781186547,1.),(1.,0.707106781186547,
1.,0.707106781186547,1.,0.707106781186547,1.,0.707106781186547,1.),(1.,
0.707106781186548,1.,0.707106781186548,1.,0.707106781186548,1.,0.707106781186548,
1.),(1.,0.707106781186547,1.,0.707106781186547,1.,0.707106781186547,1.,
0.707106781186547,1.),(1.,0.707106781186547,1.,0.707106781186547,1.,0.707106781186547,
1.,0.707106781186547,1.),(1.,0.707106781186548,1.,0.707106781186548,1.,
0.707106781186548,1.,0.707106781186548,1.),(1.,0.707106781186547,1.,0.707106781186547,
1.,0.707106781186547,1.,0.707106781186547,1.),(1.,0.707106781186548,1.,
0.707106781186548,1.,0.707106781186548,1.,0.707106781186548,1.),(1.,0.707106781186547,
1.,0.707106781186547,1.,0.707106781186547,1.,0.707106781186547,1.),(1.,
0.707106781186548,1.,0.707106781186548,1.,0.707106781186548,1.,0.707106781186548,
1.),(1.,0.707106781186547,1.,0.707106781186547,1.,0.707106781186547,1.,
0.707106781186547,1.),(1.,0.707106781186547,1.,0.707106781186547,1.,0.707106781186547,
1.,0.707106781186547,1.),(1.,0.707106781186548,1.,0.707106781186548,1.,
0.707106781186548,1.,0.707106781186548,1.),(1.,0.707106781186548,1.,0.707106781186548,
1.,0.707106781186548,1.,0.707106781186548,1.),(1.,0.707106781186547,1.,
0.707106781186547,1.,0.707106781186547,1.,0.707106781186547,1.),(1.,0.707106781186547,
1.,0.707106781186547,1.,0.707106781186547,1.,0.707106781186547,1.),(1.,
0.707106781186548,1.,0.707106781186548,1.,0.707106781186548,1.,0.707106781186548,
1.),(1.,0.707106781186547,1.,0.707106781186547,1.,0.707106781186547,1.,
0.707106781186547,1.),(1.,0.707106781186547,1.,0.707106781186547,1.,0.707106781186547,
1.,0.707106781186547,1.),(1.,0.707106781186548,1.,0.707106781186548,1.,
0.707106781186548,1.,0.707106781186548,1.),(1.,0.707106781186547,1.,0.707106781186547,
1.,0.707106781186547,1.,0.707106781186547,1.),(1.,0.707106781186548,1.,
0.707106781186548,1.,0.707106781186548,1.,0.707106781186548,1.),(1.,0.707106781186547,
1.,0.707106781186547,1.,0.707106781186547,1.,0.707106781186547,1.),(1.,
0.707106781186548,1.,0.707106781186548,1.,0.707106781186548,1.,0.707106781186548,
1.),(1.,0.707106781186547,1.,0.707106781186547,1.,0.707106781186547,1.,
0.707106781186547,1.),(1.,0.707106781186548,1.,0.707106781186548,1.,0.707106781186548,
1.,0.707106781186548,1.),(1.,0.707106781186547,1.,0.707106781186547,1.,
0.707106781186547,1.,0.707106781186547,1.),(1.,0.707106781186547,1.,0.707106781186547,
1.,0.707106781186547,1.,0.707106781186547,1.),(1.,0.707106781186547,1.,
0.707106781186547,1.,0.707106781186547,1.,0.707106781186547,1.),(1.,0.707106781186547,
1.,0.707106781186547,1.,0.707106781186547,1.,0.707106781186547,1.),(1.,
0.707106781186547,1.,0.707106781186547,1.,0.707106781186547,1.,0.707106781186547,
1.),(1.,0.707106781186547,1.,0.707106781186547,1.,0.707106781186547,1.,
0.707106781186547,1.),(1.,0.707106781186548,1.,0.707106781186548,1.,0.707106781186548,
1.,0.707106781186548,1.),(1.,0.707106781186547,1.,0.707106781186547,1.,
0.707106781186547,1.,0.707106781186547,1.),(1.,0.707106781186548,1.,0.707106781186548,
1.,0.707106781186548,1.,0.707106781186548,1.),(1.,0.707106781186547,1.,
0.707106781186547,1.,0.707106781186547,1.,0.707106781186547,1.),(1.,0.707106781186548,
1.,0.707106781186548,1.,0.707106781186548,1.,0.707106781186548,1.),(1.,
0.707106781186548,1.,0.707106781186548,1.,0.707106781186548,1.,0.707106781186548,
1.),(1.,0.707106781186547,1.,0.707106781186547,1.,0.707106781186547,1.,
0.707106781186547,1.),(1.,0.707106781186548,1.,0.707106781186548,1.,0.707106781186548,
1.,0.707106781186548,1.),(1.,0.707106781186548,1.,0.707106781186548,1.,
0.707106781186548,1.,0.707106781186548,1.),(1.,0.707106781186547,1.,0.707106781186547,
1.,0.707106781186547,1.,0.707106781186547,1.),(1.,0.707106781186548,1.,
0.707106781186548,1.,0.707106781186548,1.,0.707106781186548,1.),(1.,0.707106781186547,
1.,0.707106781186547,1.,0.707106781186547,1.,0.707106781186547,1.),(1.,
0.707106781186547,1.,0.707106781186547,1.,0.707106781186547,1.,0.707106781186547,
1.),(1.,0.707106781186547,1.,0.707106781186547,1.,0.707106781186547,1.,
0.707106781186547,1.),(1.,0.707106781186548,1.,0.707106781186548,1.,0.707106781186548,
1.,0.707106781186548,1.),(1.,0.707106781186547,1.,0.707106781186547,1.,
0.707106781186547,1.,0.707106781186547,1.),(1.,0.707106781186547,1.,0.707106781186547,
1.,0.707106781186547,1.,0.707106781186547,1.),(1.,0.707106781186548,1.,
0.707106781186548,1.,0.707106781186548,1.,0.707106781186548,1.),(1.,0.707106781186547,
1.,0.707106781186547,1.,0.707106781186547,1.,0.707106781186547,1.),(1.,
0.707106781186548,1.,0.707106781186548,1.,0.707106781186548,1.,0.707106781186548,
1.),(1.,0.707106781186547,1.,0.707106781186547,1.,0.707106781186547,1.,
0.707106781186547,1.),(1.,0.707106781186547,1.,0.707106781186547,1.,0.707106781186547,
1.,0.707106781186547,1.),(1.,0.707106781186547,1.,0.707106781186547,1.,
0.707106781186547,1.,0.707106781186547,1.),(1.,0.707106781186548,1.,0.707106781186548,
1.,0.707106781186548,1.,0.707106781186548,1.),(1.,0.707106781186548,1.,
0.707106781186548,1.,0.707106781186548,1.,0.707106781186548,1.),(1.,0.707106781186547,
1.,0.707106781186547,1.,0.707106781186547,1.,0.707106781186547,1.),(1.,
0.707106781186548,1.,0.707106781186548,1.,0.707106781186548,1.,0.707106781186548,
1.),(1.,0.707106781186548,1.,0.707106781186548,1.,0.707106781186548,1.,
0.707106781186548,1.),(1.,0.707106781186547,1.,0.707106781186547,1.,0.707106781186547,
1.,0.707106781186547,1.),(1.,0.707106781186548,1.,0.707106781186548,1.,
0.707106781186548,1.,0.707106781186548,1.),(1.,0.707106781186547,1.,0.707106781186547,
1.,0.707106781186547,1.,0.707106781186547,1.),(1.,0.707106781186548,1.,
0.707106781186548,1.,0.707106781186548,1.,0.707106781186548,1.),(1.,0.707106781186548,
1.,0.707106781186548,1.,0.707106781186548,1.,0.707106781186548,1.),(1.,
0.707106781186547,1.,0.707106781186547,1.,0.707106781186547,1.,0.707106781186547,
1.),(1.,0.707106781186548,1.,0.707106781186548,1.,0.707106781186548,1.,
0.707106781186548,1.),(1.,0.707106781186548,1.,0.707106781186548,1.,0.707106781186548,
1.,0.707106781186548,1.),(1.,0.707106781186548,1.,0.707106781186548,1.,
0.707106781186548,1.,0.707106781186548,1.),(1.,0.707106781186547,1.,0.707106781186547,
1.,0.707106781186547,1.,0.707106781186547,1.),(1.,0.707106781186547,1.,
0.707106781186547,1.,0.707106781186547,1.,0.707106781186547,1.),(1.,0.707106781186548,
1.,0.707106781186548,1.,0.707106781186548,1.,0.707106781186548,1.),(1.,
0.707106781186547,1.,0.707106781186547,1.,0.707106781186547,1.,0.707106781186547,
1.),(1.,0.707106781186548,1.,0.707106781186548,1.,0.707106781186548,1.,
0.707106781186548,1.),(1.,0.707106781186547,1.,0.707106781186547,1.,0.707106781186547,
1.,0.707106781186547,1.),(1.,0.707106781186547,1.,0.707106781186547,1.,
0.707106781186547,1.,0.707106781186547,1.),(1.,0.707106781186548,1.,0.707106781186548,
1.,0.707106781186548,1.,0.707106781186548,1.),(1.,0.707106781186548,1.,
0.707106781186548,1.,0.707106781186548,1.,0.707106781186548,1.),(1.,0.707106781186548,
1.,0.707106781186548,1.,0.707106781186548,1.,0.707106781186548,1.),(1.,
0.707106781186547,1.,0.707106781186547,1.,0.707106781186547,1.,0.707106781186547,
1.),(1.,0.707106781186547,1.,0.707106781186547,1.,0.707106781186547,1.,
0.707106781186547,1.),(1.,0.707106781186548,1.,0.707106781186548,1.,0.707106781186548,
1.,0.707106781186548,1.),(1.,0.707106781186548,1.,0.707106781186548,1.,
0.707106781186548,1.,0.707106781186548,1.),(1.,0.707106781186547,1.,0.707106781186547,
1.,0.707106781186547,1.,0.707106781186547,1.),(1.,0.707106781186547,1.,
0.707106781186547,1.,0.707106781186547,1.,0.707106781186547,1.),(1.,0.707106781186548,
1.,0.707106781186548,1.,0.707106781186548,1.,0.707106781186548,1.),(1.,
0.707106781186547,1.,0.707106781186547,1.,0.707106781186547,1.,0.707106781186547,
1.),(1.,0.707106781186547,1.,0.707106781186547,1.,0.707106781186547,1.,
0.707106781186547,1.),(1.,0.707106781186548,1.,0.707106781186548,1.,0.707106781186548,
1.,0.707106781186548,1.),(1.,0.707106781186548,1.,0.707106781186548,1.,
0.707106781186548,1.,0.707106781186548,1.),(1.,0.707106781186547,1.,0.707106781186547,
1.,0.707106781186547,1.,0.707106781186547,1.),(1.,0.707106781186547,1.,
0.707106781186547,1.,0.707106781186547,1.,0.707106781186547,1.),(1.,0.707106781186547,
1.,0.707106781186547,1.,0.707106781186547,1.,0.707106781186547,1.),(1.,
0.707106781186548,1.,0.707106781186548,1.,0.707106781186548,1.,0.707106781186548,
1.),(1.,0.707106781186547,1.,0.707106781186547,1.,0.707106781186547,1.,
0.707106781186547,1.),(1.,0.707106781186547,1.,0.707106781186547,1.,0.707106781186547,
1.,0.707106781186547,1.),(1.,0.707106781186547,1.,0.707106781186547,1.,
0.707106781186547,1.,0.707106781186547,1.),(1.,0.707106781186548,1.,0.707106781186548,
1.,0.707106781186548,1.,0.707106781186548,1.),(1.,0.707106781186548,1.,
0.707106781186548,1.,0.707106781186548,1.,0.707106781186548,1.),(1.,0.707106781186547,
1.,0.707106781186547,1.,0.707106781186547,1.,0.707106781186547,1.),(1.,
0.707106781186548,1.,0.707106781186548,1.,0.707106781186548,1.,0.707106781186548,
1.),(1.,0.707106781186547,1.,0.707106781186547,1.,0.707106781186547,1.,
0.707106781186547,1.),(1.,0.707106781186548,1.,0.707106781186548,1.,0.707106781186548,
1.,0.707106781186548,1.),(1.,0.707106781186547,1.,0.707106781186547,1.,
0.707106781186547,1.,0.707106781186547,1.),(1.,0.707106781186548,1.,0.707106781186548,
1.,0.707106781186548,1.,0.707106781186548,1.),(1.,0.707106781186548,1.,
0.707106781186548,1.,0.707106781186548,1.,0.707106781186548,1.),(1.,0.707106781186547,
1.,0.707106781186547,1.,0.707106781186547,1.,0.707106781186547,1.),(1.,
0.707106781186547,1.,0.707106781186547,1.,0.707106781186547,1.,0.707106781186547,
1.),(1.,0.707106781186548,1.,0.707106781186548,1.,0.707106781186548,1.,
0.707106781186548,1.),(1.,0.707106781186547,1.,0.707106781186547,1.,0.707106781186547,
1.,0.707106781186547,1.),(1.,0.707106781186547,1.,0.707106781186547,1.,
0.707106781186547,1.,0.707106781186547,1.),(1.,0.707106781186548,1.,0.707106781186548,
1.,0.707106781186548,1.,0.707106781186548,1.),(1.,0.707106781186547,1.,
0.707106781186547,1.,0.707106781186547,1.,0.707106781186547,1.),(1.,0.707106781186548,
1.,0.707106781186548,1.,0.707106781186548,1.,0.707106781186548,1.),(1.,
0.707106781186548,1.,0.707106781186548,1.,0.707106781186548,1.,0.707106781186548,
1.),(1.,0.707106781186547,1.,0.707106781186547,1.,0.707106781186547,1.,
0.707106781186547,1.),(1.,0.707106781186548,1.,0.707106781186548,1.,0.707106781186548,
1.,0.707106781186548,1.),(1.,0.707106781186547,1.,0.707106781186547,1.,
0.707106781186547,1.,0.707106781186547,1.),(1.,0.707106781186547,1.,0.707106781186547,
1.,0.707106781186547,1.,0.707106781186547,1.),(1.,0.707106781186547,1.,
0.707106781186547,1.,0.707106781186547,1.,0.707106781186547,1.),(1.,0.707106781186548,
1.,0.707106781186548,1.,0.707106781186548,1.,0.707106781186548,1.),(1.,
0.707106781186548,1.,0.707106781186548,1.,0.707106781186548,1.,0.707106781186548,
1.),(1.,0.707106781186548,1.,0.707106781186548,1.,0.707106781186548,1.,
0.707106781186548,1.),(1.,0.707106781186547,1.,0.707106781186547,1.,0.707106781186547,
1.,0.707106781186547,1.),(1.,0.707106781186548,1.,0.707106781186548,1.,
0.707106781186548,1.,0.707106781186548,1.),(1.,0.707106781186547,1.,0.707106781186547,
1.,0.707106781186547,1.,0.707106781186547,1.),(1.,0.707106781186548,1.,
0.707106781186548,1.,0.707106781186548,1.,0.707106781186548,1.),(1.,0.707106781186547,
1.,0.707106781186547,1.,0.707106781186547,1.,0.707106781186547,1.),(1.,
0.707106781186547,1.,0.707106781186547,1.,0.707106781186547,1.,0.707106781186547,
1.),(1.,0.707106781186547,1.,0.707106781186547,1.,0.707106781186547,1.,
0.707106781186547,1.),(1.,0.707106781186547,1.,0.707106781186547,1.,0.707106781186547,
1.,0.707106781186547,1.),(1.,0.707106781186548,1.,0.707106781186548,1.,
0.707106781186548,1.,0.707106781186548,1.),(1.,0.707106781186548,1.,0.707106781186548,
1.,0.707106781186548,1.,0.707106781186548,1.),(1.,0.707106781186547,1.,
0.707106781186547,1.,0.707106781186547,1.,0.707106781186547,1.),(1.,0.707106781186547,
1.,0.707106781186547,1.,0.707106781186547,1.,0.707106781186547,1.),(1.,
0.707106781186548,1.,0.707106781186548,1.,0.707106781186548,1.,0.707106781186548,
1.),(1.,0.707106781186547,1.,0.707106781186547,1.,0.707106781186547,1.,
0.707106781186547,1.),(1.,0.707106781186548,1.,0.707106781186548,1.,0.707106781186548,
1.,0.707106781186548,1.),(1.,0.707106781186547,1.,0.707106781186547,1.,
0.707106781186547,1.,0.707106781186547,1.),(1.,0.707106781186548,1.,0.707106781186548,
1.,0.707106781186548,1.,0.707106781186548,1.),(1.,0.707106781186547,1.,
0.707106781186547,1.,0.707106781186547,1.,0.707106781186547,1.),(1.,0.707106781186547,
1.,0.707106781186547,1.,0.707106781186547,1.,0.707106781186547,1.),(1.,
0.707106781186548,1.,0.707106781186548,1.,0.707106781186548,1.,0.707106781186548,
1.),(1.,0.707106781186547,1.,0.707106781186547,1.,0.707106781186547,1.,
0.707106781186547,1.),(1.,0.707106781186548,1.,0.707106781186548,1.,0.707106781186548,
1.,0.707106781186548,1.),(1.,0.707106781186547,1.,0.707106781186547,1.,
0.707106781186547,1.,0.707106781186547,1.),(1.,0.707106781186548,1.,0.707106781186548,
1.,0.707106781186548,1.,0.707106781186548,1.),(1.,0.707106781186548,1.,
0.707106781186548,1.,0.707106781186548,1.,0.707106781186548,1.),(1.,0.707106781186547,
1.,0.707106781186547,1.,0.707106781186547,1.,0.707106781186547,1.),(1.,
0.707106781186548,1.,0.707106781186548,1.,0.707106781186548,1.,0.707106781186548,
1.),(1.,0.707106781186547,1.,0.707106781186547,1.,0.707106781186547,1.,
0.707106781186547,1.),(1.,0.707106781186548,1.,0.707106781186548,1.,0.707106781186548,
1.,0.707106781186548,1.),(1.,0.707106781186548,1.,0.707106781186548,1.,
0.707106781186548,1.,0.707106781186548,1.),(1.,0.707106781186547,1.,0.707106781186547,
1.,0.707106781186547,1.,0.707106781186547,1.),(1.,0.707106781186548,1.,
0.707106781186548,1.,0.707106781186548,1.,0.707106781186548,1.),(1.,0.707106781186547,
1.,0.707106781186547,1.,0.707106781186547,1.,0.707106781186547,1.),(1.,
0.707106781186547,1.,0.707106781186547,1.,0.707106781186547,1.,0.707106781186547,
1.),(1.,0.707106781186548,1.,0.707106781186548,1.,0.707106781186548,1.,
0.707106781186548,1.),(1.,0.707106781186547,1.,0.707106781186547,1.,0.707106781186547,
1.,0.707106781186547,1.),(1.,0.707106781186548,1.,0.707106781186548,1.,
0.707106781186548,1.,0.707106781186548,1.),(1.,0.707106781186547,1.,0.707106781186547,
1.,0.707106781186547,1.,0.707106781186547,1.),(1.,0.707106781186548,1.,
0.707106781186548,1.,0.707106781186548,1.,0.707106781186548,1.),(1.,0.707106781186547,
1.,0.707106781186547,1.,0.707106781186547,1.,0.707106781186547,1.),(1.,
0.707106781186547,1.,0.707106781186547,1.,0.707106781186547,1.,0.707106781186547,
1.),(1.,0.707106781186548,1.,0.707106781186548,1.,0.707106781186548,1.,
0.707106781186548,1.),(1.,0.707106781186548,1.,0.707106781186548,1.,0.707106781186548,
1.,0.707106781186548,1.),(1.,0.707106781186548,1.,0.707106781186548,1.,
0.707106781186548,1.,0.707106781186548,1.),(1.,0.707106781186548,1.,0.707106781186548,
1.,0.707106781186548,1.,0.707106781186548,1.),(1.,0.707106781186547,1.,
0.707106781186547,1.,0.707106781186547,1.,0.707106781186547,1.),(1.,0.707106781186548,
1.,0.707106781186548,1.,0.707106781186548,1.,0.707106781186548,1.),(1.,
0.707106781186548,1.,0.707106781186548,1.,0.707106781186548,1.,0.707106781186548,
1.),(1.,0.707106781186548,1.,0.707106781186548,1.,0.707106781186548,1.,
0.707106781186548,1.),(1.,0.707106781186547,1.,0.707106781186547,1.,0.707106781186547,
1.,0.707106781186547,1.),(1.,0.707106781186548,1.,0.707106781186548,1.,
0.707106781186548,1.,0.707106781186548,1.),(1.,0.707106781186548,1.,0.707106781186548,
1.,0.707106781186548,1.,0.707106781186548,1.),(1.,0.707106781186548,1.,
0.707106781186548,1.,0.707106781186548,1.,0.707106781186548,1.),(1.,0.707106781186547,
1.,0.707106781186547,1.,0.707106781186547,1.,0.707106781186547,1.),(1.,
0.707106781186547,1.,0.707106781186547,1.,0.707106781186547,1.,0.707106781186547,
1.),(1.,0.707106781186548,1.,0.707106781186548,1.,0.707106781186548,1.,
0.707106781186548,1.),(1.,0.707106781186547,1.,0.707106781186547,1.,0.707106781186547,
1.,0.707106781186547,1.),(1.,0.707106781186548,1.,0.707106781186548,1.,
0.707106781186548,1.,0.707106781186548,1.),(1.,0.707106781186547,1.,0.707106781186547,
1.,0.707106781186547,1.,0.707106781186547,1.),(1.,0.707106781186548,1.,
0.707106781186548,1.,0.707106781186548,1.,0.707106781186548,1.),(1.,0.707106781186548,
1.,0.707106781186548,1.,0.707106781186548,1.,0.707106781186548,1.),(1.,
0.707106781186547,1.,0.707106781186547,1.,0.707106781186547,1.,0.707106781186547,
1.),(1.,0.707106781186547,1.,0.707106781186547,1.,0.707106781186547,1.,
0.707106781186547,1.),(1.,0.707106781186548,1.,0.707106781186548,1.,0.707106781186548,
1.,0.707106781186548,1.),(1.,0.707106781186547,1.,0.707106781186547,1.,
0.707106781186547,1.,0.707106781186547,1.),(1.,0.707106781186548,1.,0.707106781186548,
1.,0.707106781186548,1.,0.707106781186548,1.),(1.,0.707106781186547,1.,
0.707106781186547,1.,0.707106781186547,1.,0.707106781186547,1.),(1.,0.707106781186548,
1.,0.707106781186548,1.,0.707106781186548,1.,0.707106781186548,1.),(1.,
0.707106781186548,1.,0.707106781186548,1.,0.707106781186548,1.,0.707106781186548,
1.),(1.,0.707106781186547,1.,0.707106781186547,1.,0.707106781186547,1.,
0.707106781186547,1.),(1.,0.707106781186547,1.,0.707106781186547,1.,0.707106781186547,
1.,0.707106781186547,1.),(1.,0.707106781186547,1.,0.707106781186547,1.,
0.707106781186547,1.,0.707106781186547,1.),(1.,0.707106781186548,1.,0.707106781186548,
1.,0.707106781186548,1.,0.707106781186548,1.),(1.,0.707106781186548,1.,
0.707106781186548,1.,0.707106781186548,1.,0.707106781186548,1.),(1.,0.707106781186547,
1.,0.707106781186547,1.,0.707106781186547,1.,0.707106781186547,1.),(1.,
0.707106781186547,1.,0.707106781186547,1.,0.707106781186547,1.,0.707106781186547,
1.),(1.,0.707106781186548,1.,0.707106781186548,1.,0.707106781186548,1.,
0.707106781186548,1.),(1.,0.707106781186548,1.,0.707106781186548,1.,0.707106781186548,
1.,0.707106781186548,1.),(1.,0.707106781186548,1.,0.707106781186548,1.,
0.707106781186548,1.,0.707106781186548,1.),(1.,0.707106781186548,1.,0.707106781186548,
1.,0.707106781186548,1.,0.707106781186548,1.),(1.,0.707106781186547,1.,
0.707106781186547,1.,0.707106781186547,1.,0.707106781186547,1.),(1.,0.707106781186547,
1.,0.707106781186547,1.,0.707106781186547,1.,0.707106781186547,1.),(1.,
0.707106781186548,1.,0.707106781186548,1.,0.707106781186548,1.,0.707106781186548,
1.),(1.,0.707106781186548,1.,0.707106781186548,1.,0.707106781186548,1.,
0.707106781186548,1.),(1.,0.707106781186547,1.,0.707106781186547,1.,0.707106781186547,
1.,0.707106781186547,1.),(1.,0.707106781186548,1.,0.707106781186548,1.,
0.707106781186548,1.,0.707106781186548,1.),(1.,0.707106781186547,1.,0.707106781186547,
1.,0.707106781186547,1.,0.707106781186547,1.),(1.,0.707106781186548,1.,
0.707106781186548,1.,0.707106781186548,1.,0.707106781186548,1.),(1.,0.707106781186547,
1.,0.707106781186547,1.,0.707106781186547,1.,0.707106781186547,1.),(1.,
0.707106781186548,1.,0.707106781186548,1.,0.707106781186548,1.,0.707106781186548,
1.),(1.,0.707106781186547,1.,0.707106781186547,1.,0.707106781186547,1.,
0.707106781186547,1.),(1.,0.707106781186547,1.,0.707106781186547,1.,0.707106781186547,
1.,0.707106781186547,1.),(1.,0.707106781186548,1.,0.707106781186548,1.,
0.707106781186548,1.,0.707106781186548,1.),(1.,0.707106781186547,1.,0.707106781186547,
1.,0.707106781186547,1.,0.707106781186547,1.),(1.,0.707106781186547,1.,
0.707106781186547,1.,0.707106781186547,1.,0.707106781186547,1.),(1.,0.707106781186548,
1.,0.707106781186548,1.,0.707106781186548,1.,0.707106781186548,1.),(1.,
0.707106781186547,1.,0.707106781186547,1.,0.707106781186547,1.,0.707106781186547,
1.),(1.,0.707106781186548,1.,0.707106781186548,1.,0.707106781186548,1.,
0.707106781186548,1.),(1.,0.707106781186547,1.,0.707106781186547,1.,0.707106781186547,
1.,0.707106781186547,1.),(1.,0.707106781186548,1.,0.707106781186548,1.,
0.707106781186548,1.,0.707106781186548,1.),(1.,0.707106781186547,1.,0.707106781186547,
1.,0.707106781186547,1.,0.707106781186547,1.),(1.,0.707106781186548,1.,
0.707106781186548,1.,0.707106781186548,1.,0.707106781186548,1.),(1.,0.707106781186547,
1.,0.707106781186547,1.,0.707106781186547,1.,0.707106781186547,1.),(1.,
0.707106781186548,1.,0.707106781186548,1.,0.707106781186548,1.,0.707106781186548,
1.),(1.,0.707106781186547,1.,0.707106781186547,1.,0.707106781186547,1.,
0.707106781186547,1.),(1.,0.707106781186548,1.,0.707106781186548,1.,0.707106781186548,
1.,0.707106781186548,1.),(1.,0.707106781186547,1.,0.707106781186547,1.,
0.707106781186547,1.,0.707106781186547,1.),(1.,0.707106781186547,1.,0.707106781186547,
1.,0.707106781186547,1.,0.707106781186547,1.),(1.,0.707106781186548,1.,
0.707106781186548,1.,0.707106781186548,1.,0.707106781186548,1.),(1.,0.707106781186548,
1.,0.707106781186548,1.,0.707106781186548,1.,0.707106781186548,1.),(1.,
0.707106781186547,1.,0.707106781186547,1.,0.707106781186547,1.,0.707106781186547,
1.),(1.,0.707106781186547,1.,0.707106781186547,1.,0.707106781186547,1.,
0.707106781186547,1.),(1.,0.707106781186547,1.,0.707106781186547,1.,0.707106781186547,
1.,0.707106781186547,1.),(1.,0.707106781186548,1.,0.707106781186548,1.,
0.707106781186548,1.,0.707106781186548,1.),(1.,0.707106781186547,1.,0.707106781186547,
1.,0.707106781186547,1.,0.707106781186547,1.),(1.,0.707106781186548,1.,
0.707106781186548,1.,0.707106781186548,1.,0.707106781186548,1.),(1.,0.707106781186547,
1.,0.707106781186547,1.,0.707106781186547,1.,0.707106781186547,1.),(1.,
0.707106781186548,1.,0.707106781186548,1.,0.707106781186548,1.,0.707106781186548,
1.),(1.,0.707106781186547,1.,0.707106781186547,1.,0.707106781186547,1.,
0.707106781186547,1.),(1.,0.707106781186548,1.,0.707106781186548,1.,0.707106781186548,
1.,0.707106781186548,1.),(1.,0.707106781186547,1.,0.707106781186547,1.,
0.707106781186547,1.,0.707106781186547,1.),(1.,0.707106781186547,1.,0.707106781186547,
1.,0.707106781186547,1.,0.707106781186547,1.),(1.,0.707106781186547,1.,
0.707106781186547,1.,0.707106781186547,1.,0.707106781186547,1.),(1.,0.707106781186548,
1.,0.707106781186548,1.,0.707106781186548,1.,0.707106781186548,1.),(1.,
0.707106781186547,1.,0.707106781186547,1.,0.707106781186547,1.,0.707106781186547,
1.),(1.,0.707106781186548,1.,0.707106781186548,1.,0.707106781186548,1.,
0.707106781186548,1.),(1.,0.707106781186548,1.,0.707106781186548,1.,0.707106781186548,
1.,0.707106781186548,1.),(1.,0.707106781186547,1.,0.707106781186547,1.,
0.707106781186547,1.,0.707106781186547,1.),(1.,0.707106781186548,1.,0.707106781186548,
1.,0.707106781186548,1.,0.707106781186548,1.),(1.,0.707106781186547,1.,
0.707106781186547,1.,0.707106781186547,1.,0.707106781186547,1.),(1.,0.707106781186547,
1.,0.707106781186547,1.,0.707106781186547,1.,0.707106781186547,1.),(1.,
0.707106781186548,1.,0.707106781186548,1.,0.707106781186548,1.,0.707106781186548,
1.),(1.,0.707106781186547,1.,0.707106781186547,1.,0.707106781186547,1.,
0.707106781186547,1.),(1.,0.707106781186547,1.,0.707106781186547,1.,0.707106781186547,
1.,0.707106781186547,1.),(1.,0.707106781186548,1.,0.707106781186548,1.,
0.707106781186548,1.,0.707106781186548,1.),(1.,0.707106781186547,1.,0.707106781186547,
1.,0.707106781186547,1.,0.707106781186547,1.),(1.,0.707106781186547,1.,
0.707106781186547,1.,0.707106781186547,1.,0.707106781186547,1.),(1.,0.707106781186547,
1.,0.707106781186547,1.,0.707106781186547,1.,0.707106781186547,1.),(1.,
0.707106781186547,1.,0.707106781186547,1.,0.707106781186547,1.,0.707106781186547,
1.),(1.,0.707106781186548,1.,0.707106781186548,1.,0.707106781186548,1.,
0.707106781186548,1.),(1.,0.707106781186547,1.,0.707106781186547,1.,0.707106781186547,
1.,0.707106781186547,1.),(1.,0.707106781186547,1.,0.707106781186547,1.,
0.707106781186547,1.,0.707106781186547,1.),(1.,0.707106781186547,1.,0.707106781186547,
1.,0.707106781186547,1.,0.707106781186547,1.),(1.,0.707106781186548,1.,
0.707106781186548,1.,0.707106781186548,1.,0.707106781186548,1.),(1.,0.707106781186547,
1.,0.707106781186547,1.,0.707106781186547,1.,0.707106781186547,1.),(1.,
0.707106781186547,1.,0.707106781186547,1.,0.707106781186547,1.,0.707106781186547,
1.),(1.,0.707106781186548,1.,0.707106781186548,1.,0.707106781186548,1.,
0.707106781186548,1.),(1.,0.707106781186548,1.,0.707106781186548,1.,0.707106781186548,
1.,0.707106781186548,1.),(1.,0.707106781186547,1.,0.707106781186547,1.,
0.707106781186547,1.,0.707106781186547,1.),(1.,0.707106781186548,1.,0.707106781186548,
1.,0.707106781186548,1.,0.707106781186548,1.),(1.,0.707106781186548,1.,
0.707106781186548,1.,0.707106781186548,1.,0.707106781186548,1.),(1.,0.707106781186547,
1.,0.707106781186547,1.,0.707106781186547,1.,0.707106781186547,1.),(1.,
0.707106781186547,1.,0.707106781186547,1.,0.707106781186547,1.,0.707106781186547,
1.),(1.,0.707106781186548,1.,0.707106781186548,1.,0.707106781186548,1.,
0.707106781186548,1.),(1.,0.707106781186547,1.,0.707106781186547,1.,0.707106781186547,
1.,0.707106781186547,1.),(1.,0.707106781186547,1.,0.707106781186547,1.,
0.707106781186547,1.,0.707106781186547,1.),(1.,0.707106781186548,1.,0.707106781186548,
1.,0.707106781186548,1.,0.707106781186548,1.),(1.,0.707106781186547,1.,
0.707106781186547,1.,0.707106781186547,1.,0.707106781186547,1.),(1.,0.707106781186547,
1.,0.707106781186547,1.,0.707106781186547,1.,0.707106781186547,1.),(1.,
0.707106781186547,1.,0.707106781186547,1.,0.707106781186547,1.,0.707106781186547,
1.),(1.,0.707106781186548,1.,0.707106781186548,1.,0.707106781186548,1.,
0.707106781186548,1.),(1.,0.707106781186547,1.,0.707106781186547,1.,0.707106781186547,
1.,0.707106781186547,1.),(1.,0.707106781186548,1.,0.707106781186548,1.,
0.707106781186548,1.,0.707106781186548,1.),(1.,0.707106781186547,1.,0.707106781186547,
1.,0.707106781186547,1.,0.707106781186547,1.),(1.,0.707106781186548,1.,
0.707106781186548,1.,0.707106781186548,1.,0.707106781186548,1.),(1.,0.707106781186547,
1.,0.707106781186547,1.,0.707106781186547,1.,0.707106781186547,1.),(1.,
0.707106781186548,1.,0.707106781186548,1.,0.707106781186548,1.,0.707106781186548,
1.),(1.,0.707106781186547,1.,0.707106781186547,1.,0.707106781186547,1.,
0.707106781186547,1.),(1.,0.707106781186548,1.,0.707106781186548,1.,0.707106781186548,
1.,0.707106781186548,1.),(1.,0.707106781186547,1.,0.707106781186547,1.,
0.707106781186547,1.,0.707106781186547,1.),(1.,0.707106781186548,1.,0.707106781186548,
1.,0.707106781186548,1.,0.707106781186548,1.),(1.,0.707106781186548,1.,
0.707106781186548,1.,0.707106781186548,1.,0.707106781186548,1.),(1.,0.707106781186547,
1.,0.707106781186547,1.,0.707106781186547,1.,0.707106781186547,1.),(1.,
0.707106781186547,1.,0.707106781186547,1.,0.707106781186547,1.,0.707106781186547,
1.),(1.,0.707106781186548,1.,0.707106781186548,1.,0.707106781186548,1.,
0.707106781186548,1.),(1.,0.707106781186547,1.,0.707106781186547,1.,0.707106781186547,
1.,0.707106781186547,1.),(1.,0.707106781186548,1.,0.707106781186548,1.,
0.707106781186548,1.,0.707106781186548,1.),(1.,0.707106781186547,1.,0.707106781186547,
1.,0.707106781186547,1.,0.707106781186547,1.),(1.,0.707106781186548,1.,
0.707106781186548,1.,0.707106781186548,1.,0.707106781186548,1.),(1.,0.707106781186548,
1.,0.707106781186548,1.,0.707106781186548,1.,0.707106781186548,1.),(1.,
0.707106781186547,1.,0.707106781186547,1.,0.707106781186547,1.,0.707106781186547,
1.),(1.,0.707106781186548,1.,0.707106781186548,1.,0.707106781186548,1.,
0.707106781186548,1.),(1.,0.707106781186547,1.,0.707106781186547,1.,0.707106781186547,
1.,0.707106781186547,1.),(1.,0.707106781186548,1.,0.707106781186548,1.,
0.707106781186548,1.,0.707106781186548,1.),(1.,0.707106781186548,1.,0.707106781186548,
1.,0.707106781186548,1.,0.707106781186548,1.),(1.,0.707106781186547,1.,
0.707106781186547,1.,0.707106781186547,1.,0.707106781186547,1.),(1.,0.707106781186547,
1.,0.707106781186547,1.,0.707106781186547,1.,0.707106781186547,1.),(1.,
0.707106781186548,1.,0.707106781186548,1.,0.707106781186548,1.,0.707106781186548,
1.),(1.,0.707106781186547,1.,0.707106781186547,1.,0.707106781186547,1.,
0.707106781186547,1.),(1.,0.707106781186548,1.,0.707106781186548,1.,0.707106781186548,
1.,0.707106781186548,1.),(1.,0.707106781186547,1.,0.707106781186547,1.,
0.707106781186547,1.,0.707106781186547,1.),(1.,0.707106781186548,1.,0.707106781186548,
1.,0.707106781186548,1.,0.707106781186548,1.),(1.,0.707106781186547,1.,
0.707106781186547,1.,0.707106781186547,1.,0.707106781186547,1.),(1.,0.707106781186548,
1.,0.707106781186548,1.,0.707106781186548,1.,0.707106781186548,1.),(1.,
0.707106781186547,1.,0.707106781186547,1.,0.707106781186547,1.,0.707106781186547,
1.),(1.,0.707106781186547,1.,0.707106781186547,1.,0.707106781186547,1.,
0.707106781186547,1.),(1.,0.707106781186547,1.,0.707106781186547,1.,0.707106781186547,
1.,0.707106781186547,1.),(1.,0.707106781186547,1.,0.707106781186547,1.,
0.707106781186547,1.,0.707106781186547,1.),(1.,0.707106781186547,1.,0.707106781186547,
1.,0.707106781186547,1.,0.707106781186547,1.),(1.,0.707106781186547,1.,
0.707106781186547,1.,0.707106781186547,1.,0.707106781186547,1.),(1.,0.707106781186547,
1.,0.707106781186547,1.,0.707106781186547,1.,0.707106781186547,1.),(1.,
0.707106781186547,1.,0.707106781186547,1.,0.707106781186547,1.,0.707106781186547,
1.),(1.,0.707106781186548,1.,0.707106781186548,1.,0.707106781186548,1.,
0.707106781186548,1.),(1.,0.707106781186547,1.,0.707106781186547,1.,0.707106781186547,
1.,0.707106781186547,1.),(1.,0.707106781186548,1.,0.707106781186548,1.,
0.707106781186548,1.,0.707106781186548,1.),(1.,0.707106781186547,1.,0.707106781186547,
1.,0.707106781186547,1.,0.707106781186547,1.),(1.,0.707106781186547,1.,
0.707106781186547,1.,0.707106781186547,1.,0.707106781186547,1.),(1.,0.707106781186548,
1.,0.707106781186548,1.,0.707106781186548,1.,0.707106781186548,1.),(1.,
0.707106781186547,1.,0.707106781186547,1.,0.707106781186547,1.,0.707106781186547,
1.),(1.,0.707106781186548,1.,0.707106781186548,1.,0.707106781186548,1.,
0.707106781186548,1.),(1.,0.707106781186547,1.,0.707106781186547,1.,0.707106781186547,
1.,0.707106781186547,1.),(1.,0.707106781186547,1.,0.707106781186547,1.,
0.707106781186547,1.,0.707106781186547,1.),(1.,0.707106781186548,1.,0.707106781186548,
1.,0.707106781186548,1.,0.707106781186548,1.),(1.,0.707106781186547,1.,
0.707106781186547,1.,0.707106781186547,1.,0.707106781186547,1.),(1.,0.707106781186548,
1.,0.707106781186548,1.,0.707106781186548,1.,0.707106781186548,1.),(1.,
0.707106781186547,1.,0.707106781186547,1.,0.707106781186547,1.,0.707106781186547,
1.),(1.,0.707106781186548,1.,0.707106781186548,1.,0.707106781186548,1.,
0.707106781186548,1.),(1.,0.707106781186547,1.,0.707106781186547,1.,0.707106781186547,
1.,0.707106781186547,1.),(1.,0.707106781186548,1.,0.707106781186548,1.,
0.707106781186548,1.,0.707106781186548,1.),(1.,0.707106781186547,1.,0.707106781186547,
1.,0.707106781186547,1.,0.707106781186547,1.),(1.,0.707106781186548,1.,
0.707106781186548,1.,0.707106781186548,1.,0.707106781186548,1.),(1.,0.707106781186547,
1.,0.707106781186547,1.,0.707106781186547,1.,0.707106781186547,1.),(1.,
0.707106781186548,1.,0.707106781186548,1.,0.707106781186548,1.,0.707106781186548,
1.),(1.,0.707106781186547,1.,0.707106781186547,1.,0.707106781186547,1.,
0.707106781186547,1.),(1.,0.707106781186548,1.,0.707106781186548,1.,0.707106781186548,
1.,0.707106781186548,1.),(1.,0.707106781186548,1.,0.707106781186548,1.,
0.707106781186548,1.,0.707106781186548,1.),(1.,0.707106781186547,1.,0.707106781186547,
1.,0.707106781186547,1.,0.707106781186547,1.),(1.,0.707106781186548,1.,
0.707106781186548,1.,0.707106781186548,1.,0.707106781186548,1.),(1.,0.707106781186547,
1.,0.707106781186547,1.,0.707106781186547,1.,0.707106781186547,1.),(1.,
0.707106781186547,1.,0.707106781186547,1.,0.707106781186547,1.,0.707106781186547,
1.),(1.,0.707106781186547,1.,0.707106781186547,1.,0.707106781186547,1.,
0.707106781186547,1.),(1.,0.707106781186548,1.,0.707106781186548,1.,0.707106781186548,
1.,0.707106781186548,1.),(1.,0.707106781186547,1.,0.707106781186547,1.,
0.707106781186547,1.,0.707106781186547,1.),(1.,0.707106781186547,1.,0.707106781186547,
1.,0.707106781186547,1.,0.707106781186547,1.),(1.,0.707106781186547,1.,
0.707106781186547,1.,0.707106781186547,1.,0.707106781186547,1.),(1.,0.707106781186548,
1.,0.707106781186548,1.,0.707106781186548,1.,0.707106781186548,1.),(1.,
0.707106781186547,1.,0.707106781186547,1.,0.707106781186547,1.,0.707106781186547,
1.),(1.,0.707106781186547,1.,0.707106781186547,1.,0.707106781186547,1.,
0.707106781186547,1.),(1.,0.707106781186548,1.,0.707106781186548,1.,0.707106781186548,
1.,0.707106781186548,1.),(1.,0.707106781186547,1.,0.707106781186547,1.,
0.707106781186547,1.,0.707106781186547,1.),(1.,0.707106781186547,1.,0.707106781186547,
1.,0.707106781186547,1.,0.707106781186547,1.),(1.,0.707106781186547,1.,
0.707106781186547,1.,0.707106781186547,1.,0.707106781186547,1.),(1.,0.707106781186547,
1.,0.707106781186547,1.,0.707106781186547,1.,0.707106781186547,1.),(1.,
0.707106781186548,1.,0.707106781186548,1.,0.707106781186548,1.,0.707106781186548,
1.),(1.,0.707106781186547,1.,0.707106781186547,1.,0.707106781186547,1.,
0.707106781186547,1.),(1.,0.707106781186547,1.,0.707106781186547,1.,0.707106781186547,
1.,0.707106781186547,1.),(1.,0.707106781186547,1.,0.707106781186547,1.,
0.707106781186547,1.,0.707106781186547,1.),(1.,0.707106781186548,1.,0.707106781186548,
1.,0.707106781186548,1.,0.707106781186548,1.),(1.,0.707106781186548,1.,
0.707106781186548,1.,0.707106781186548,1.,0.707106781186548,1.),(1.,0.707106781186548,
1.,0.707106781186548,1.,0.707106781186548,1.,0.707106781186548,1.),(1.,
0.707106781186548,1.,0.707106781186548,1.,0.707106781186548,1.,0.707106781186548,
1.),(1.,0.707106781186547,1.,0.707106781186547,1.,0.707106781186547,1.,
0.707106781186547,1.),(1.,0.707106781186548,1.,0.707106781186548,1.,0.707106781186548,
1.,0.707106781186548,1.),(1.,0.707106781186547,1.,0.707106781186547,1.,
0.707106781186547,1.,0.707106781186547,1.),(1.,0.707106781186547,1.,0.707106781186547,
1.,0.707106781186547,1.,0.707106781186547,1.),(1.,0.707106781186548,1.,
0.707106781186548,1.,0.707106781186548,1.,0.707106781186548,1.),(1.,0.707106781186547,
1.,0.707106781186547,1.,0.707106781186547,1.,0.707106781186547,1.),(1.,
0.707106781186548,1.,0.707106781186548,1.,0.707106781186548,1.,0.707106781186548,
1.),(1.,0.707106781186547,1.,0.707106781186547,1.,0.707106781186547,1.,
0.707106781186547,1.),(1.,0.707106781186547,1.,0.707106781186547,1.,0.707106781186547,
1.,0.707106781186547,1.),(1.,0.707106781186548,1.,0.707106781186548,1.,
0.707106781186548,1.,0.707106781186548,1.),(1.,0.707106781186547,1.,0.707106781186547,
1.,0.707106781186547,1.,0.707106781186547,1.),(1.,0.707106781186547,1.,
0.707106781186547,1.,0.707106781186547,1.,0.707106781186547,1.),(1.,0.707106781186547,
1.,0.707106781186547,1.,0.707106781186547,1.,0.707106781186547,1.),(1.,
0.707106781186547,1.,0.707106781186547,1.,0.707106781186547,1.,0.707106781186547,
1.),(1.,0.707106781186548,1.,0.707106781186548,1.,0.707106781186548,1.,
0.707106781186548,1.),(1.,0.707106781186548,1.,0.707106781186548,1.,0.707106781186548,
1.,0.707106781186548,1.),(1.,0.707106781186547,1.,0.707106781186547,1.,
0.707106781186547,1.,0.707106781186547,1.),(1.,0.707106781186547,1.,0.707106781186547,
1.,0.707106781186547,1.,0.707106781186547,1.),(1.,0.707106781186548,1.,
0.707106781186548,1.,0.707106781186548,1.,0.707106781186548,1.),(1.,0.707106781186547,
1.,0.707106781186547,1.,0.707106781186547,1.,0.707106781186547,1.),(1.,
0.707106781186548,1.,0.707106781186548,1.,0.707106781186548,1.,0.707106781186548,
1.),(1.,0.707106781186547,1.,0.707106781186547,1.,0.707106781186547,1.,
0.707106781186547,1.),(1.,0.707106781186548,1.,0.707106781186548,1.,0.707106781186548,
1.,0.707106781186548,1.),(1.,0.707106781186548,1.,0.707106781186548,1.,
0.707106781186548,1.,0.707106781186548,1.),(1.,0.707106781186547,1.,0.707106781186547,
1.,0.707106781186547,1.,0.707106781186547,1.),(1.,0.707106781186547,1.,
0.707106781186547,1.,0.707106781186547,1.,0.707106781186547,1.),(1.,0.707106781186548,
1.,0.707106781186548,1.,0.707106781186548,1.,0.707106781186548,1.),(1.,
0.707106781186548,1.,0.707106781186548,1.,0.707106781186548,1.,0.707106781186548,
1.),(1.,0.707106781186547,1.,0.707106781186547,1.,0.707106781186547,1.,
0.707106781186547,1.),(1.,0.707106781186548,1.,0.707106781186548,1.,0.707106781186548,
1.,0.707106781186548,1.),(1.,0.707106781186548,1.,0.707106781186548,1.,
0.707106781186548,1.,0.707106781186548,1.),(1.,0.707106781186547,1.,0.707106781186547,
1.,0.707106781186547,1.,0.707106781186547,1.),(1.,0.707106781186548,1.,
0.707106781186548,1.,0.707106781186548,1.,0.707106781186548,1.),(1.,0.707106781186548,
1.,0.707106781186548,1.,0.707106781186548,1.,0.707106781186548,1.),(1.,
0.707106781186548,1.,0.707106781186548,1.,0.707106781186548,1.,0.707106781186548,
1.),(1.,0.707106781186547,1.,0.707106781186547,1.,0.707106781186547,1.,
0.707106781186547,1.),(1.,0.707106781186548,1.,0.707106781186548,1.,0.707106781186548,
1.,0.707106781186548,1.),(1.,0.707106781186547,1.,0.707106781186547,1.,
0.707106781186547,1.,0.707106781186547,1.),(1.,0.707106781186548,1.,0.707106781186548,
1.,0.707106781186548,1.,0.707106781186548,1.),(1.,0.707106781186547,1.,
0.707106781186547,1.,0.707106781186547,1.,0.707106781186547,1.),(1.,0.707106781186548,
1.,0.707106781186548,1.,0.707106781186548,1.,0.707106781186548,1.),(1.,
0.707106781186547,1.,0.707106781186547,1.,0.707106781186547,1.,0.707106781186547,
1.),(1.,0.707106781186548,1.,0.707106781186548,1.,0.707106781186548,1.,
0.707106781186548,1.),(1.,0.707106781186547,1.,0.707106781186547,1.,0.707106781186547,
1.,0.707106781186547,1.),(1.,0.707106781186548,1.,0.707106781186548,1.,
0.707106781186548,1.,0.707106781186548,1.),(1.,0.707106781186548,1.,0.707106781186548,
1.,0.707106781186548,1.,0.707106781186548,1.),(1.,0.707106781186547,1.,
0.707106781186547,1.,0.707106781186547,1.,0.707106781186547,1.),(1.,0.707106781186547,
1.,0.707106781186547,1.,0.707106781186547,1.,0.707106781186547,1.),(1.,
0.707106781186548,1.,0.707106781186548,1.,0.707106781186548,1.,0.707106781186548,
1.),(1.,0.707106781186547,1.,0.707106781186547,1.,0.707106781186547,1.,
0.707106781186547,1.),(1.,0.707106781186548,1.,0.707106781186548,1.,0.707106781186548,
1.,0.707106781186548,1.),(1.,0.707106781186547,1.,0.707106781186547,1.,
0.707106781186547,1.,0.707106781186547,1.),(1.,0.707106781186548,1.,0.707106781186548,
1.,0.707106781186548,1.,0.707106781186548,1.),(1.,0.707106781186548,1.,
0.707106781186548,1.,0.707106781186548,1.,0.707106781186548,1.),(1.,0.707106781186548,
1.,0.707106781186548,1.,0.707106781186548,1.,0.707106781186548,1.),(1.,
0.707106781186548,1.,0.707106781186548,1.,0.707106781186548,1.,0.707106781186548,
1.),(1.,0.707106781186548,1.,0.707106781186548,1.,0.707106781186548,1.,
0.707106781186548,1.),(1.,0.707106781186547,1.,0.707106781186547,1.,0.707106781186547,
1.,0.707106781186547,1.),(1.,0.707106781186547,1.,0.707106781186547,1.,
0.707106781186547,1.,0.707106781186547,1.),(1.,0.707106781186547,1.,0.707106781186547,
1.,0.707106781186547,1.,0.707106781186547,1.),(1.,0.707106781186547,1.,
0.707106781186547,1.,0.707106781186547,1.,0.707106781186547,1.),(1.,0.707106781186548,
1.,0.707106781186548,1.,0.707106781186548,1.,0.707106781186548,1.),(1.,
0.707106781186547,1.,0.707106781186547,1.,0.707106781186547,1.,0.707106781186547,
1.),(1.,0.707106781186548,1.,0.707106781186548,1.,0.707106781186548,1.,
0.707106781186548,1.),(1.,0.707106781186547,1.,0.707106781186547,1.,0.707106781186547,
1.,0.707106781186547,1.),(1.,0.707106781186547,1.,0.707106781186547,1.,
0.707106781186547,1.,0.707106781186547,1.),(1.,0.707106781186548,1.,0.707106781186548,
1.,0.707106781186548,1.,0.707106781186548,1.),(1.,0.707106781186548,1.,
0.707106781186548,1.,0.707106781186548,1.,0.707106781186548,1.),(1.,0.707106781186547,
1.,0.707106781186547,1.,0.707106781186547,1.,0.707106781186547,1.),(1.,
0.707106781186548,1.,0.707106781186548,1.,0.707106781186548,1.,0.707106781186548,
1.),(1.,0.707106781186547,1.,0.707106781186547,1.,0.707106781186547,1.,
0.707106781186547,1.),(1.,0.707106781186548,1.,0.707106781186548,1.,0.707106781186548,
1.,0.707106781186548,1.),(1.,0.707106781186548,1.,0.707106781186548,1.,
0.707106781186548,1.,0.707106781186548,1.),(1.,0.707106781186547,1.,0.707106781186547,
1.,0.707106781186547,1.,0.707106781186547,1.),(1.,0.707106781186547,1.,
0.707106781186547,1.,0.707106781186547,1.,0.707106781186547,1.),(1.,0.707106781186548,
1.,0.707106781186548,1.,0.707106781186548,1.,0.707106781186548,1.),(1.,
0.707106781186547,1.,0.707106781186547,1.,0.707106781186547,1.,0.707106781186547,
1.),(1.,0.707106781186548,1.,0.707106781186548,1.,0.707106781186548,1.,
0.707106781186548,1.),(1.,0.707106781186547,1.,0.707106781186547,1.,0.707106781186547,
1.,0.707106781186547,1.),(1.,0.707106781186548,1.,0.707106781186548,1.,
0.707106781186548,1.,0.707106781186548,1.),(1.,0.707106781186547,1.,0.707106781186547,
1.,0.707106781186547,1.,0.707106781186547,1.),(1.,0.707106781186548,1.,
0.707106781186548,1.,0.707106781186548,1.,0.707106781186548,1.),(1.,0.707106781186547,
1.,0.707106781186547,1.,0.707106781186547,1.,0.707106781186547,1.),(1.,
0.707106781186548,1.,0.707106781186548,1.,0.707106781186548,1.,0.707106781186548,
1.),(1.,0.707106781186547,1.,0.707106781186547,1.,0.707106781186547,1.,
0.707106781186547,1.),(1.,0.707106781186548,1.,0.707106781186548,1.,0.707106781186548,
1.,0.707106781186548,1.),(1.,0.707106781186547,1.,0.707106781186547,1.,
0.707106781186547,1.,0.707106781186547,1.),(1.,0.707106781186548,1.,0.707106781186548,
1.,0.707106781186548,1.,0.707106781186548,1.),(1.,0.707106781186548,1.,
0.707106781186548,1.,0.707106781186548,1.,0.707106781186548,1.),(1.,0.707106781186547,
1.,0.707106781186547,1.,0.707106781186547,1.,0.707106781186547,1.),(1.,
0.707106781186548,1.,0.707106781186548,1.,0.707106781186548,1.,0.707106781186548,
1.),(1.,0.707106781186547,1.,0.707106781186547,1.,0.707106781186547,1.,
0.707106781186547,1.),(1.,0.707106781186548,1.,0.707106781186548,1.,0.707106781186548,
1.,0.707106781186548,1.),(1.,0.707106781186547,1.,0.707106781186547,1.,
0.707106781186547,1.,0.707106781186547,1.),(1.,0.707106781186548,1.,0.707106781186548,
1.,0.707106781186548,1.,0.707106781186548,1.),(1.,0.707106781186548,1.,
0.707106781186548,1.,0.707106781186548,1.,0.707106781186548,1.),(1.,0.707106781186548,
1.,0.707106781186548,1.,0.707106781186548,1.,0.707106781186548,1.),(1.,
0.707106781186547,1.,0.707106781186547,1.,0.707106781186547,1.,0.707106781186547,
1.),(1.,0.707106781186547,1.,0.707106781186547,1.,0.707106781186547,1.,
0.707106781186547,1.),(1.,0.707106781186548,1.,0.707106781186548,1.,0.707106781186548,
1.,0.707106781186548,1.),(1.,0.707106781186548,1.,0.707106781186548,1.,
0.707106781186548,1.,0.707106781186548,1.),(1.,0.707106781186547,1.,0.707106781186547,
1.,0.707106781186547,1.,0.707106781186547,1.),(1.,0.707106781186547,1.,
0.707106781186547,1.,0.707106781186547,1.,0.707106781186547,1.),(1.,0.707106781186547,
1.,0.707106781186547,1.,0.707106781186547,1.,0.707106781186547,1.),(1.,
0.707106781186548,1.,0.707106781186548,1.,0.707106781186548,1.,0.707106781186548,
1.),(1.,0.707106781186547,1.,0.707106781186547,1.,0.707106781186547,1.,
0.707106781186547,1.),(1.,0.707106781186548,1.,0.707106781186548,1.,0.707106781186548,
1.,0.707106781186548,1.),(1.,0.707106781186547,1.,0.707106781186547,1.,
0.707106781186547,1.,0.707106781186547,1.),(1.,0.707106781186548,1.,0.707106781186548,
1.,0.707106781186548,1.,0.707106781186548,1.),(1.,0.707106781186547,1.,
0.707106781186547,1.,0.707106781186547,1.,0.707106781186547,1.),(1.,0.707106781186547,
1.,0.707106781186547,1.,0.707106781186547,1.,0.707106781186547,1.),(1.,
0.707106781186547,1.,0.707106781186547,1.,0.707106781186547,1.,0.707106781186547,
1.),(1.,0.707106781186548,1.,0.707106781186548,1.,0.707106781186548,1.,
0.707106781186548,1.),(1.,0.707106781186547,1.,0.707106781186547,1.,0.707106781186547,
1.,0.707106781186547,1.),(1.,0.707106781186548,1.,0.707106781186548,1.,
0.707106781186548,1.,0.707106781186548,1.),(1.,0.707106781186547,1.,0.707106781186547,
1.,0.707106781186547,1.,0.707106781186547,1.),(1.,0.707106781186548,1.,
0.707106781186548,1.,0.707106781186548,1.,0.707106781186548,1.),(1.,0.707106781186547,
1.,0.707106781186547,1.,0.707106781186547,1.,0.707106781186547,1.),(1.,
0.707106781186548,1.,0.707106781186548,1.,0.707106781186548,1.,0.707106781186548,
1.),(1.,0.707106781186547,1.,0.707106781186547,1.,0.707106781186547,1.,
0.707106781186547,1.),(1.,0.707106781186547,1.,0.707106781186547,1.,0.707106781186547,
1.,0.707106781186547,1.),(1.,0.707106781186548,1.,0.707106781186548,1.,
0.707106781186548,1.,0.707106781186548,1.),(1.,0.707106781186547,1.,0.707106781186547,
1.,0.707106781186547,1.,0.707106781186547,1.),(1.,0.707106781186547,1.,
0.707106781186547,1.,0.707106781186547,1.,0.707106781186547,1.),(1.,0.707106781186548,
1.,0.707106781186548,1.,0.707106781186548,1.,0.707106781186548,1.),(1.,
0.707106781186547,1.,0.707106781186547,1.,0.707106781186547,1.,0.707106781186547,
1.),(1.,0.707106781186547,1.,0.707106781186547,1.,0.707106781186547,1.,
0.707106781186547,1.),(1.,0.707106781186548,1.,0.707106781186548,1.,0.707106781186548,
1.,0.707106781186548,1.),(1.,0.707106781186547,1.,0.707106781186547,1.,
0.707106781186547,1.,0.707106781186547,1.),(1.,0.707106781186547,1.,0.707106781186547,
1.,0.707106781186547,1.,0.707106781186547,1.),(1.,0.707106781186547,1.,
0.707106781186547,1.,0.707106781186547,1.,0.707106781186547,1.),(1.,0.707106781186548,
1.,0.707106781186548,1.,0.707106781186548,1.,0.707106781186548,1.),(1.,
0.707106781186547,1.,0.707106781186547,1.,0.707106781186547,1.,0.707106781186547,
1.),(1.,0.707106781186548,1.,0.707106781186548,1.,0.707106781186548,1.,
0.707106781186548,1.),(1.,0.707106781186547,1.,0.707106781186547,1.,0.707106781186547,
1.,0.707106781186547,1.),(1.,0.707106781186547,1.,0.707106781186547,1.,
0.707106781186547,1.,0.707106781186547,1.),(1.,0.707106781186547,1.,0.707106781186547,
1.,0.707106781186547,1.,0.707106781186547,1.),(1.,0.707106781186548,1.,
0.707106781186548,1.,0.707106781186548,1.,0.707106781186548,1.),(1.,0.707106781186548,
1.,0.707106781186548,1.,0.707106781186548,1.,0.707106781186548,1.),(1.,
0.707106781186547,1.,0.707106781186547,1.,0.707106781186547,1.,0.707106781186547,
1.),(1.,0.707106781186547,1.,0.707106781186547,1.,0.707106781186547,1.,
0.707106781186547,1.),(1.,0.707106781186548,1.,0.707106781186548,1.,0.707106781186548,
1.,0.707106781186548,1.),(1.,0.707106781186548,1.,0.707106781186548,1.,
0.707106781186548,1.,0.707106781186548,1.),(1.,0.707106781186548,1.,0.707106781186548,
1.,0.707106781186548,1.,0.707106781186548,1.),(1.,0.707106781186547,1.,
0.707106781186547,1.,0.707106781186547,1.,0.707106781186547,1.),(1.,0.707106781186548,
1.,0.707106781186548,1.,0.707106781186548,1.,0.707106781186548,1.),(1.,
0.707106781186547,1.,0.707106781186547,1.,0.707106781186547,1.,0.707106781186547,
1.),(1.,0.707106781186548,1.,0.707106781186548,1.,0.707106781186548,1.,
0.707106781186548,1.),(1.,0.707106781186547,1.,0.707106781186547,1.,0.707106781186547,
1.,0.707106781186547,1.),(1.,0.707106781186548,1.,0.707106781186548,1.,
0.707106781186548,1.,0.707106781186548,1.),(1.,0.707106781186547,1.,0.707106781186547,
1.,0.707106781186547,1.,0.707106781186547,1.),(1.,0.707106781186547,1.,
0.707106781186547,1.,0.707106781186547,1.,0.707106781186547,1.),(1.,0.707106781186547,
1.,0.707106781186547,1.,0.707106781186547,1.,0.707106781186547,1.),(1.,
0.707106781186547,1.,0.707106781186547,1.,0.707106781186547,1.,0.707106781186547,
1.),(1.,0.707106781186548,1.,0.707106781186548,1.,0.707106781186548,1.,
0.707106781186548,1.),(1.,0.707106781186547,1.,0.707106781186547,1.,0.707106781186547,
1.,0.707106781186547,1.),(1.,0.707106781186548,1.,0.707106781186548,1.,
0.707106781186548,1.,0.707106781186548,1.),(1.,0.707106781186548,1.,0.707106781186548,
1.,0.707106781186548,1.,0.707106781186548,1.),(1.,0.707106781186547,1.,
0.707106781186547,1.,0.707106781186547,1.,0.707106781186547,1.),(1.,0.707106781186548,
1.,0.707106781186548,1.,0.707106781186548,1.,0.707106781186548,1.),(1.,
0.707106781186547,1.,0.707106781186547,1.,0.707106781186547,1.,0.707106781186547,
1.),(1.,0.707106781186547,1.,0.707106781186547,1.,0.707106781186547,1.,
0.707106781186547,1.),(1.,0.707106781186547,1.,0.707106781186547,1.,0.707106781186547,
1.,0.707106781186547,1.),(1.,0.707106781186547,1.,0.707106781186547,1.,
0.707106781186547,1.,0.707106781186547,1.),(1.,0.707106781186548,1.,0.707106781186548,
1.,0.707106781186548,1.,0.707106781186548,1.),(1.,0.707106781186547,1.,
0.707106781186547,1.,0.707106781186547,1.,0.707106781186547,1.),(1.,0.707106781186548,
1.,0.707106781186548,1.,0.707106781186548,1.,0.707106781186548,1.),(1.,
0.707106781186547,1.,0.707106781186547,1.,0.707106781186547,1.,0.707106781186547,
1.),(1.,0.707106781186548,1.,0.707106781186548,1.,0.707106781186548,1.,
0.707106781186548,1.),(1.,0.707106781186548,1.,0.707106781186548,1.,0.707106781186548,
1.,0.707106781186548,1.),(1.,0.707106781186547,1.,0.707106781186547,1.,
0.707106781186547,1.,0.707106781186547,1.),(1.,0.707106781186548,1.,0.707106781186548,
1.,0.707106781186548,1.,0.707106781186548,1.),(1.,0.707106781186547,1.,
0.707106781186547,1.,0.707106781186547,1.,0.707106781186547,1.),(1.,0.707106781186547,
1.,0.707106781186547,1.,0.707106781186547,1.,0.707106781186547,1.),(1.,
0.707106781186547,1.,0.707106781186547,1.,0.707106781186547,1.,0.707106781186547,
1.),(1.,0.707106781186547,1.,0.707106781186547,1.,0.707106781186547,1.,
0.707106781186547,1.),(1.,0.707106781186548,1.,0.707106781186548,1.,0.707106781186548,
1.,0.707106781186548,1.),(1.,0.707106781186547,1.,0.707106781186547,1.,
0.707106781186547,1.,0.707106781186547,1.),(1.,0.707106781186548,1.,0.707106781186548,
1.,0.707106781186548,1.,0.707106781186548,1.),(1.,0.707106781186548,1.,
0.707106781186548,1.,0.707106781186548,1.,0.707106781186548,1.),(1.,0.707106781186547,
1.,0.707106781186547,1.,0.707106781186547,1.,0.707106781186547,1.),(1.,
0.707106781186548,1.,0.707106781186548,1.,0.707106781186548,1.,0.707106781186548,
1.),(1.,0.707106781186547,1.,0.707106781186547,1.,0.707106781186547,1.,
0.707106781186547,1.),(1.,0.707106781186548,1.,0.707106781186548,1.,0.707106781186548,
1.,0.707106781186548,1.),(1.,0.707106781186547,1.,0.707106781186547,1.,
0.707106781186547,1.,0.707106781186547,1.),(1.,0.707106781186547,1.,0.707106781186547,
1.,0.707106781186547,1.,0.707106781186547,1.),(1.,0.707106781186548,1.,
0.707106781186548,1.,0.707106781186548,1.,0.707106781186548,1.),(1.,0.707106781186547,
1.,0.707106781186547,1.,0.707106781186547,1.,0.707106781186547,1.),(1.,
0.707106781186548,1.,0.707106781186548,1.,0.707106781186548,1.,0.707106781186548,
1.),(1.,0.707106781186548,1.,0.707106781186548,1.,0.707106781186548,1.,
0.707106781186548,1.),(1.,0.707106781186547,1.,0.707106781186547,1.,0.707106781186547,
1.,0.707106781186547,1.),(1.,0.707106781186547,1.,0.707106781186547,1.,
0.707106781186547,1.,0.707106781186547,1.),(1.,0.707106781186548,1.,0.707106781186548,
1.,0.707106781186548,1.,0.707106781186548,1.),(1.,0.707106781186548,1.,
0.707106781186548,1.,0.707106781186548,1.,0.707106781186548,1.),(1.,0.707106781186547,
1.,0.707106781186547,1.,0.707106781186547,1.,0.707106781186547,1.),(1.,
0.707106781186547,1.,0.707106781186547,1.,0.707106781186547,1.,0.707106781186547,
1.),(1.,0.707106781186548,1.,0.707106781186548,1.,0.707106781186548,1.,
0.707106781186548,1.),(1.,0.707106781186547,1.,0.707106781186547,1.,0.707106781186547,
1.,0.707106781186547,1.),(1.,0.707106781186547,1.,0.707106781186547,1.,
0.707106781186547,1.,0.707106781186547,1.),(1.,0.707106781186548,1.,0.707106781186548,
1.,0.707106781186548,1.,0.707106781186548,1.),(1.,0.707106781186547,1.,
0.707106781186547,1.,0.707106781186547,1.,0.707106781186547,1.),(1.,0.707106781186547,
1.,0.707106781186547,1.,0.707106781186547,1.,0.707106781186547,1.),(1.,
0.707106781186548,1.,0.707106781186548,1.,0.707106781186548,1.,0.707106781186548,
1.),(1.,0.707106781186547,1.,0.707106781186547,1.,0.707106781186547,1.,
0.707106781186547,1.),(1.,0.707106781186548,1.,0.707106781186548,1.,0.707106781186548,
1.,0.707106781186548,1.),(1.,0.707106781186547,1.,0.707106781186547,1.,
0.707106781186547,1.,0.707106781186547,1.),(1.,0.707106781186547,1.,0.707106781186547,
1.,0.707106781186547,1.,0.707106781186547,1.),(1.,0.707106781186548,1.,
0.707106781186548,1.,0.707106781186548,1.,0.707106781186548,1.),(1.,0.707106781186547,
1.,0.707106781186547,1.,0.707106781186547,1.,0.707106781186547,1.),(1.,
0.707106781186548,1.,0.707106781186548,1.,0.707106781186548,1.,0.707106781186548,
1.),(1.,0.707106781186547,1.,0.707106781186547,1.,0.707106781186547,1.,
0.707106781186547,1.),(1.,0.707106781186548,1.,0.707106781186548,1.,0.707106781186548,
1.,0.707106781186548,1.),(1.,0.707106781186547,1.,0.707106781186547,1.,
0.707106781186547,1.,0.707106781186547,1.),(1.,0.707106781186547,1.,0.707106781186547,
1.,0.707106781186547,1.,0.707106781186547,1.),(1.,0.707106781186547,1.,
0.707106781186547,1.,0.707106781186547,1.,0.707106781186547,1.),(1.,0.707106781186548,
1.,0.707106781186548,1.,0.707106781186548,1.,0.707106781186548,1.),(1.,
0.707106781186547,1.,0.707106781186547,1.,0.707106781186547,1.,0.707106781186547,
1.),(1.,0.707106781186548,1.,0.707106781186548,1.,0.707106781186548,1.,
0.707106781186548,1.),(1.,0.707106781186547,1.,0.707106781186547,1.,0.707106781186547,
1.,0.707106781186547,1.),(1.,0.707106781186548,1.,0.707106781186548,1.,
0.707106781186548,1.,0.707106781186548,1.),(1.,0.707106781186548,1.,0.707106781186548,
1.,0.707106781186548,1.,0.707106781186548,1.),(1.,0.707106781186548,1.,
0.707106781186548,1.,0.707106781186548,1.,0.707106781186548,1.),(1.,0.707106781186548,
1.,0.707106781186548,1.,0.707106781186548,1.,0.707106781186548,1.),(1.,
0.707106781186547,1.,0.707106781186547,1.,0.707106781186547,1.,0.707106781186547,
1.),(1.,0.707106781186547,1.,0.707106781186547,1.,0.707106781186547,1.,
0.707106781186547,1.),(1.,0.707106781186547,1.,0.707106781186547,1.,0.707106781186547,
1.,0.707106781186547,1.),(1.,0.707106781186548,1.,0.707106781186548,1.,
0.707106781186548,1.,0.707106781186548,1.),(1.,0.707106781186547,1.,0.707106781186547,
1.,0.707106781186547,1.,0.707106781186547,1.),(1.,0.707106781186548,1.,
0.707106781186548,1.,0.707106781186548,1.,0.707106781186548,1.),(1.,0.707106781186547,
1.,0.707106781186547,1.,0.707106781186547,1.,0.707106781186547,1.),(1.,
0.707106781186547,1.,0.707106781186547,1.,0.707106781186547,1.,0.707106781186547,
1.),(1.,0.707106781186548,1.,0.707106781186548,1.,0.707106781186548,1.,
0.707106781186548,1.),(1.,0.707106781186547,1.,0.707106781186547,1.,0.707106781186547,
1.,0.707106781186547,1.),(1.,0.707106781186547,1.,0.707106781186547,1.,
0.707106781186547,1.,0.707106781186547,1.),(1.,0.707106781186548,1.,0.707106781186548,
1.,0.707106781186548,1.,0.707106781186548,1.),(1.,0.707106781186547,1.,
0.707106781186547,1.,0.707106781186547,1.,0.707106781186547,1.),(1.,0.707106781186547,
1.,0.707106781186547,1.,0.707106781186547,1.,0.707106781186547,1.),(1.,
0.707106781186548,1.,0.707106781186548,1.,0.707106781186548,1.,0.707106781186548,
1.),(1.,0.707106781186548,1.,0.707106781186548,1.,0.707106781186548,1.,
0.707106781186548,1.),(1.,0.707106781186547,1.,0.707106781186547,1.,0.707106781186547,
1.,0.707106781186547,1.),(1.,0.707106781186548,1.,0.707106781186548,1.,
0.707106781186548,1.,0.707106781186548,1.),(1.,0.707106781186547,1.,0.707106781186547,
1.,0.707106781186547,1.,0.707106781186547,1.),(1.,0.707106781186547,1.,
0.707106781186547,1.,0.707106781186547,1.,0.707106781186547,1.),(1.,0.707106781186548,
1.,0.707106781186548,1.,0.707106781186548,1.,0.707106781186548,1.),(1.,
0.707106781186547,1.,0.707106781186547,1.,0.707106781186547,1.,0.707106781186547,
1.),(1.,0.707106781186548,1.,0.707106781186548,1.,0.707106781186548,1.,
0.707106781186548,1.),(1.,0.707106781186547,1.,0.707106781186547,1.,0.707106781186547,
1.,0.707106781186547,1.),(1.,0.707106781186548,1.,0.707106781186548,1.,
0.707106781186548,1.,0.707106781186548,1.),(1.,0.707106781186547,1.,0.707106781186547,
1.,0.707106781186547,1.,0.707106781186547,1.),(1.,0.707106781186547,1.,
0.707106781186547,1.,0.707106781186547,1.,0.707106781186547,1.),(1.,0.707106781186547,
1.,0.707106781186547,1.,0.707106781186547,1.,0.707106781186547,1.),(1.,
0.707106781186548,1.,0.707106781186548,1.,0.707106781186548,1.,0.707106781186548,
1.),(1.,0.707106781186547,1.,0.707106781186547,1.,0.707106781186547,1.,
0.707106781186547,1.),(1.,0.707106781186548,1.,0.707106781186548,1.,0.707106781186548,
1.,0.707106781186548,1.),(1.,0.707106781186547,1.,0.707106781186547,1.,
0.707106781186547,1.,0.707106781186547,1.),(1.,0.707106781186548,1.,0.707106781186548,
1.,0.707106781186548,1.,0.707106781186548,1.),(1.,0.707106781186547,1.,
0.707106781186547,1.,0.707106781186547,1.,0.707106781186547,1.),(1.,0.707106781186547,
1.,0.707106781186547,1.,0.707106781186547,1.,0.707106781186547,1.),(1.,
0.707106781186548,1.,0.707106781186548,1.,0.707106781186548,1.,0.707106781186548,
1.),(1.,0.707106781186548,1.,0.707106781186548,1.,0.707106781186548,1.,
0.707106781186548,1.),(1.,0.707106781186548,1.,0.707106781186548,1.,0.707106781186548,
1.,0.707106781186548,1.),(1.,0.707106781186547,1.,0.707106781186547,1.,
0.707106781186547,1.,0.707106781186547,1.),(1.,0.707106781186548,1.,0.707106781186548,
1.,0.707106781186548,1.,0.707106781186548,1.),(1.,0.707106781186547,1.,
0.707106781186547,1.,0.707106781186547,1.,0.707106781186547,1.),(1.,0.707106781186548,
1.,0.707106781186548,1.,0.707106781186548,1.,0.707106781186548,1.),(1.,
0.707106781186547,1.,0.707106781186547,1.,0.707106781186547,1.,0.707106781186547,
1.),(1.,0.707106781186548,1.,0.707106781186548,1.,0.707106781186548,1.,
0.707106781186548,1.),(1.,0.707106781186547,1.,0.707106781186547,1.,0.707106781186547,
1.,0.707106781186547,1.),(1.,0.707106781186548,1.,0.707106781186548,1.,
0.707106781186548,1.,0.707106781186548,1.),(1.,0.707106781186548,1.,0.707106781186548,
1.,0.707106781186548,1.,0.707106781186548,1.),(1.,0.707106781186547,1.,
0.707106781186547,1.,0.707106781186547,1.,0.707106781186547,1.),(1.,0.707106781186547,
1.,0.707106781186547,1.,0.707106781186547,1.,0.707106781186547,1.),(1.,
0.707106781186547,1.,0.707106781186547,1.,0.707106781186547,1.,0.707106781186547,
1.),(1.,0.707106781186548,1.,0.707106781186548,1.,0.707106781186548,1.,
0.707106781186548,1.),(1.,0.707106781186547,1.,0.707106781186547,1.,0.707106781186547,
1.,0.707106781186547,1.),(1.,0.707106781186547,1.,0.707106781186547,1.,
0.707106781186547,1.,0.707106781186547,1.),(1.,0.707106781186548,1.,0.707106781186548,
1.,0.707106781186548,1.,0.707106781186548,1.),(1.,0.707106781186547,1.,
0.707106781186547,1.,0.707106781186547,1.,0.707106781186547,1.),(1.,0.707106781186547,
1.,0.707106781186547,1.,0.707106781186547,1.,0.707106781186547,1.),(1.,
0.707106781186548,1.,0.707106781186548,1.,0.707106781186548,1.,0.707106781186548,
1.),(1.,0.707106781186547,1.,0.707106781186547,1.,0.707106781186547,1.,
0.707106781186547,1.),(1.,0.707106781186548,1.,0.707106781186548,1.,0.707106781186548,
1.,0.707106781186548,1.),(1.,0.707106781186548,1.,0.707106781186548,1.,
0.707106781186548,1.,0.707106781186548,1.),(1.,0.707106781186548,1.,0.707106781186548,
1.,0.707106781186548,1.,0.707106781186548,1.),(1.,0.707106781186547,1.,
0.707106781186547,1.,0.707106781186547,1.,0.707106781186547,1.),(1.,0.707106781186548,
1.,0.707106781186548,1.,0.707106781186548,1.,0.707106781186548,1.),(1.,
0.707106781186547,1.,0.707106781186547,1.,0.707106781186547,1.,0.707106781186547,
1.),(1.,0.707106781186548,1.,0.707106781186548,1.,0.707106781186548,1.,
0.707106781186548,1.),(1.,0.707106781186547,1.,0.707106781186547,1.,0.707106781186547,
1.,0.707106781186547,1.),(1.,0.707106781186548,1.,0.707106781186548,1.,
0.707106781186548,1.,0.707106781186548,1.),(1.,0.707106781186547,1.,0.707106781186547,
1.,0.707106781186547,1.,0.707106781186547,1.),(1.,0.707106781186548,1.,
0.707106781186548,1.,0.707106781186548,1.,0.707106781186548,1.),(1.,0.707106781186547,
1.,0.707106781186547,1.,0.707106781186547,1.,0.707106781186547,1.),(1.,
0.707106781186548,1.,0.707106781186548,1.,0.707106781186548,1.,0.707106781186548,
1.),(1.,0.707106781186547,1.,0.707106781186547,1.,0.707106781186547,1.,
0.707106781186547,1.),(1.,0.707106781186548,1.,0.707106781186548,1.,0.707106781186548,
1.,0.707106781186548,1.),(1.,0.707106781186548,1.,0.707106781186548,1.,
0.707106781186548,1.,0.707106781186548,1.),(1.,0.707106781186547,1.,0.707106781186547,
1.,0.707106781186547,1.,0.707106781186547,1.),(1.,0.707106781186548,1.,
0.707106781186548,1.,0.707106781186548,1.,0.707106781186548,1.),(1.,0.707106781186547,
1.,0.707106781186547,1.,0.707106781186547,1.,0.707106781186547,1.),(1.,
0.707106781186548,1.,0.707106781186548,1.,0.707106781186548,1.,0.707106781186548,
1.),(1.,0.707106781186548,1.,0.707106781186548,1.,0.707106781186548,1.,
0.707106781186548,1.),(1.,0.707106781186547,1.,0.707106781186547,1.,0.707106781186547,
1.,0.707106781186547,1.),(1.,0.707106781186547,1.,0.707106781186547,1.,
0.707106781186547,1.,0.707106781186547,1.),(1.,0.707106781186548,1.,0.707106781186548,
1.,0.707106781186548,1.,0.707106781186548,1.),(1.,0.707106781186547,1.,
0.707106781186547,1.,0.707106781186547,1.,0.707106781186547,1.),(1.,0.707106781186547,
1.,0.707106781186547,1.,0.707106781186547,1.,0.707106781186547,1.),(1.,
0.707106781186548,1.,0.707106781186548,1.,0.707106781186548,1.,0.707106781186548,
1.),(1.,0.707106781186547,1.,0.707106781186547,1.,0.707106781186547,1.,
0.707106781186547,1.),(1.,0.707106781186548,1.,0.707106781186548,1.,0.707106781186548,
1.,0.707106781186548,1.),(1.,0.707106781186548,1.,0.707106781186548,1.,
0.707106781186548,1.,0.707106781186548,1.),(1.,0.707106781186547,1.,0.707106781186547,
1.,0.707106781186547,1.,0.707106781186547,1.),(1.,0.707106781186548,1.,
0.707106781186548,1.,0.707106781186548,1.,0.707106781186548,1.),(1.,0.707106781186548,
1.,0.707106781186548,1.,0.707106781186548,1.,0.707106781186548,1.),(1.,
0.707106781186548,1.,0.707106781186548,1.,0.707106781186548,1.,0.707106781186548,
1.),(1.,0.707106781186548,1.,0.707106781186548,1.,0.707106781186548,1.,
0.707106781186548,1.),(1.,0.707106781186548,1.,0.707106781186548,1.,0.707106781186548,
1.,0.707106781186548,1.),(1.,0.707106781186547,1.,0.707106781186547,1.,
0.707106781186547,1.,0.707106781186547,1.),(1.,0.707106781186548,1.,0.707106781186548,
1.,0.707106781186548,1.,0.707106781186548,1.),(1.,0.707106781186548,1.,
0.707106781186548,1.,0.707106781186548,1.,0.707106781186548,1.),(1.,0.707106781186548,
1.,0.707106781186548,1.,0.707106781186548,1.,0.707106781186548,1.),(1.,
0.707106781186547,1.,0.707106781186547,1.,0.707106781186547,1.,0.707106781186547,
1.),(1.,0.707106781186548,1.,0.707106781186548,1.,0.707106781186548,1.,
0.707106781186548,1.),(1.,0.707106781186547,1.,0.707106781186547,1.,0.707106781186547,
1.,0.707106781186547,1.),(1.,0.707106781186548,1.,0.707106781186548,1.,
0.707106781186548,1.,0.707106781186548,1.),(1.,0.707106781186547,1.,0.707106781186547,
1.,0.707106781186547,1.,0.707106781186547,1.),(1.,0.707106781186548,1.,
0.707106781186548,1.,0.707106781186548,1.,0.707106781186548,1.),(1.,0.707106781186547,
1.,0.707106781186547,1.,0.707106781186547,1.,0.707106781186547,1.),(1.,
0.707106781186548,1.,0.707106781186548,1.,0.707106781186548,1.,0.707106781186548,
1.),(1.,0.707106781186547,1.,0.707106781186547,1.,0.707106781186547,1.,
0.707106781186547,1.),(1.,0.707106781186548,1.,0.707106781186548,1.,0.707106781186548,
1.,0.707106781186548,1.),(1.,0.707106781186547,1.,0.707106781186547,1.,
0.707106781186547,1.,0.707106781186547,1.),(1.,0.707106781186547,1.,0.707106781186547,
1.,0.707106781186547,1.,0.707106781186547,1.),(1.,0.707106781186548,1.,
0.707106781186548,1.,0.707106781186548,1.,0.707106781186548,1.),(1.,0.707106781186547,
1.,0.707106781186547,1.,0.707106781186547,1.,0.707106781186547,1.),(1.,
0.707106781186547,1.,0.707106781186547,1.,0.707106781186547,1.,0.707106781186547,
1.),(1.,0.707106781186548,1.,0.707106781186548,1.,0.707106781186548,1.,
0.707106781186548,1.),(1.,0.707106781186547,1.,0.707106781186547,1.,0.707106781186547,
1.,0.707106781186547,1.),(1.,0.707106781186548,1.,0.707106781186548,1.,
0.707106781186548,1.,0.707106781186548,1.),(1.,0.707106781186547,1.,0.707106781186547,
1.,0.707106781186547,1.,0.707106781186547,1.),(1.,0.707106781186548,1.,
0.707106781186548,1.,0.707106781186548,1.,0.707106781186548,1.),(1.,0.707106781186547,
1.,0.707106781186547,1.,0.707106781186547,1.,0.707106781186547,1.),(1.,
0.707106781186548,1.,0.707106781186548,1.,0.707106781186548,1.,0.707106781186548,
1.),(1.,0.707106781186547,1.,0.707106781186547,1.,0.707106781186547,1.,
0.707106781186547,1.),(1.,0.707106781186547,1.,0.707106781186547,1.,0.707106781186547,
1.,0.707106781186547,1.),(1.,0.707106781186548,1.,0.707106781186548,1.,
0.707106781186548,1.,0.707106781186548,1.),(1.,0.707106781186547,1.,0.707106781186547,
1.,0.707106781186547,1.,0.707106781186547,1.),(1.,0.707106781186547,1.,
0.707106781186547,1.,0.707106781186547,1.,0.707106781186547,1.),(1.,0.707106781186548,
1.,0.707106781186548,1.,0.707106781186548,1.,0.707106781186548,1.),(1.,
0.707106781186547,1.,0.707106781186547,1.,0.707106781186547,1.,0.707106781186547,
1.),(1.,0.707106781186548,1.,0.707106781186548,1.,0.707106781186548,1.,
0.707106781186548,1.),(1.,0.707106781186547,1.,0.707106781186547,1.,0.707106781186547,
1.,0.707106781186547,1.),(1.,0.707106781186547,1.,0.707106781186547,1.,
0.707106781186547,1.,0.707106781186547,1.),(1.,0.707106781186548,1.,0.707106781186548,
1.,0.707106781186548,1.,0.707106781186548,1.),(1.,0.707106781186548,1.,
0.707106781186548,1.,0.707106781186548,1.,0.707106781186548,1.),(1.,0.707106781186547,
1.,0.707106781186547,1.,0.707106781186547,1.,0.707106781186547,1.),(1.,
0.707106781186548,1.,0.707106781186548,1.,0.707106781186548,1.,0.707106781186548,
1.),(1.,0.707106781186547,1.,0.707106781186547,1.,0.707106781186547,1.,
0.707106781186547,1.),(1.,0.707106781186547,1.,0.707106781186547,1.,0.707106781186547,
1.,0.707106781186547,1.),(1.,0.707106781186547,1.,0.707106781186547,1.,
0.707106781186547,1.,0.707106781186547,1.),(1.,0.707106781186548,1.,0.707106781186548,
1.,0.707106781186548,1.,0.707106781186548,1.),(1.,0.707106781186547,1.,
0.707106781186547,1.,0.707106781186547,1.,0.707106781186547,1.),(1.,0.707106781186547,
1.,0.707106781186547,1.,0.707106781186547,1.,0.707106781186547,1.),(1.,
0.707106781186548,1.,0.707106781186548,1.,0.707106781186548,1.,0.707106781186548,
1.),(1.,0.707106781186547,1.,0.707106781186547,1.,0.707106781186547,1.,
0.707106781186547,1.),(1.,0.707106781186547,1.,0.707106781186547,1.,0.707106781186547,
1.,0.707106781186547,1.),(1.,0.707106781186547,1.,0.707106781186547,1.,
0.707106781186547,1.,0.707106781186547,1.),(1.,0.707106781186548,1.,0.707106781186548,
1.,0.707106781186548,1.,0.707106781186548,1.),(1.,0.707106781186548,1.,
0.707106781186548,1.,0.707106781186548,1.,0.707106781186548,1.),(1.,0.707106781186547,
1.,0.707106781186547,1.,0.707106781186547,1.,0.707106781186547,1.),(1.,
0.707106781186548,1.,0.707106781186548,1.,0.707106781186548,1.,0.707106781186548,
1.),(1.,0.707106781186547,1.,0.707106781186547,1.,0.707106781186547,1.,
0.707106781186547,1.),(1.,0.707106781186548,1.,0.707106781186548,1.,0.707106781186548,
1.,0.707106781186548,1.),(1.,0.707106781186547,1.,0.707106781186547,1.,
0.707106781186547,1.,0.707106781186547,1.),(1.,0.707106781186547,1.,0.707106781186547,
1.,0.707106781186547,1.,0.707106781186547,1.),(1.,0.707106781186548,1.,
0.707106781186548,1.,0.707106781186548,1.,0.707106781186548,1.),(1.,0.707106781186547,
1.,0.707106781186547,1.,0.707106781186547,1.,0.707106781186547,1.),(1.,
0.707106781186548,1.,0.707106781186548,1.,0.707106781186548,1.,0.707106781186548,
1.),(1.,0.707106781186547,1.,0.707106781186547,1.,0.707106781186547,1.,
0.707106781186547,1.),(1.,0.707106781186547,1.,0.707106781186547,1.,0.707106781186547,
1.,0.707106781186547,1.),(1.,0.707106781186547,1.,0.707106781186547,1.,
0.707106781186547,1.,0.707106781186547,1.),(1.,0.707106781186547,1.,0.707106781186547,
1.,0.707106781186547,1.,0.707106781186547,1.),(1.,0.707106781186548,1.,
0.707106781186548,1.,0.707106781186548,1.,0.707106781186548,1.),(1.,0.707106781186547,
1.,0.707106781186547,1.,0.707106781186547,1.,0.707106781186547,1.),(1.,
0.707106781186547,1.,0.707106781186547,1.,0.707106781186547,1.,0.707106781186547,
1.),(1.,0.707106781186547,1.,0.707106781186547,1.,0.707106781186547,1.,
0.707106781186547,1.),(1.,0.707106781186547,1.,0.707106781186547,1.,0.707106781186547,
1.,0.707106781186547,1.),(1.,0.707106781186547,1.,0.707106781186547,1.,
0.707106781186547,1.,0.707106781186547,1.),(1.,0.707106781186548,1.,0.707106781186548,
1.,0.707106781186548,1.,0.707106781186548,1.),(1.,0.707106781186547,1.,
0.707106781186547,1.,0.707106781186547,1.,0.707106781186547,1.),(1.,0.707106781186547,
1.,0.707106781186547,1.,0.707106781186547,1.,0.707106781186547,1.),(1.,
0.707106781186547,1.,0.707106781186547,1.,0.707106781186547,1.,0.707106781186547,
1.),(1.,0.707106781186547,1.,0.707106781186547,1.,0.707106781186547,1.,
0.707106781186547,1.),(1.,0.707106781186548,1.,0.707106781186548,1.,0.707106781186548,
1.,0.707106781186548,1.),(1.,0.707106781186547,1.,0.707106781186547,1.,
0.707106781186547,1.,0.707106781186547,1.),(1.,0.707106781186548,1.,0.707106781186548,
1.,0.707106781186548,1.,0.707106781186548,1.),(1.,0.707106781186547,1.,
0.707106781186547,1.,0.707106781186547,1.,0.707106781186547,1.),(1.,0.707106781186547,
1.,0.707106781186547,1.,0.707106781186547,1.,0.707106781186547,1.),(1.,
0.707106781186548,1.,0.707106781186548,1.,0.707106781186548,1.,0.707106781186548,
1.),(1.,0.707106781186547,1.,0.707106781186547,1.,0.707106781186547,1.,
0.707106781186547,1.),(1.,0.707106781186548,1.,0.707106781186548,1.,0.707106781186548,
1.,0.707106781186548,1.),(1.,0.707106781186547,1.,0.707106781186547,1.,
0.707106781186547,1.,0.707106781186547,1.),(1.,0.707106781186547,1.,0.707106781186547,
1.,0.707106781186547,1.,0.707106781186547,1.),(1.,0.707106781186548,1.,
0.707106781186548,1.,0.707106781186548,1.,0.707106781186548,1.),(1.,0.707106781186547,
1.,0.707106781186547,1.,0.707106781186547,1.,0.707106781186547,1.),(1.,
0.707106781186547,1.,0.707106781186547,1.,0.707106781186547,1.,0.707106781186547,
1.),(1.,0.707106781186548,1.,0.707106781186548,1.,0.707106781186548,1.,
0.707106781186548,1.),(1.,0.707106781186547,1.,0.707106781186547,1.,0.707106781186547,
1.,0.707106781186547,1.),(1.,0.707106781186547,1.,0.707106781186547,1.,
0.707106781186547,1.,0.707106781186547,1.),(1.,0.707106781186547,1.,0.707106781186547,
1.,0.707106781186547,1.,0.707106781186547,1.),(1.,0.707106781186547,1.,
0.707106781186547,1.,0.707106781186547,1.,0.707106781186547,1.),(1.,0.707106781186548,
1.,0.707106781186548,1.,0.707106781186548,1.,0.707106781186548,1.),(1.,
0.707106781186547,1.,0.707106781186547,1.,0.707106781186547,1.,0.707106781186547,
1.),(1.,0.707106781186548,1.,0.707106781186548,1.,0.707106781186548,1.,
0.707106781186548,1.),(1.,0.707106781186548,1.,0.707106781186548,1.,0.707106781186548,
1.,0.707106781186548,1.),(1.,0.707106781186547,1.,0.707106781186547,1.,
0.707106781186547,1.,0.707106781186547,1.),(1.,0.707106781186548,1.,0.707106781186548,
1.,0.707106781186548,1.,0.707106781186548,1.),(1.,0.707106781186548,1.,
0.707106781186548,1.,0.707106781186548,1.,0.707106781186548,1.),(1.,0.707106781186547,
1.,0.707106781186547,1.,0.707106781186547,1.,0.707106781186547,1.),(1.,
0.707106781186547,1.,0.707106781186547,1.,0.707106781186547,1.,0.707106781186547,
1.),(1.,0.707106781186548,1.,0.707106781186548,1.,0.707106781186548,1.,
0.707106781186548,1.),(1.,0.707106781186547,1.,0.707106781186547,1.,0.707106781186547,
1.,0.707106781186547,1.),(1.,0.707106781186547,1.,0.707106781186547,1.,
0.707106781186547,1.,0.707106781186547,1.),(1.,0.707106781186547,1.,0.707106781186547,
1.,0.707106781186547,1.,0.707106781186547,1.),(1.,0.707106781186548,1.,
0.707106781186548,1.,0.707106781186548,1.,0.707106781186548,1.),(1.,0.707106781186547,
1.,0.707106781186547,1.,0.707106781186547,1.,0.707106781186547,1.),(1.,
0.707106781186547,1.,0.707106781186547,1.,0.707106781186547,1.,0.707106781186547,
1.),(1.,0.707106781186548,1.,0.707106781186548,1.,0.707106781186548,1.,
0.707106781186548,1.),(1.,0.707106781186547,1.,0.707106781186547,1.,0.707106781186547,
1.,0.707106781186547,1.),(1.,0.707106781186548,1.,0.707106781186548,1.,
0.707106781186548,1.,0.707106781186548,1.),(1.,0.707106781186547,1.,0.707106781186547,
1.,0.707106781186547,1.,0.707106781186547,1.),(1.,0.707106781186548,1.,
0.707106781186548,1.,0.707106781186548,1.,0.707106781186548,1.),(1.,0.707106781186547,
1.,0.707106781186547,1.,0.707106781186547,1.,0.707106781186547,1.),(1.,
0.707106781186547,1.,0.707106781186547,1.,0.707106781186547,1.,0.707106781186547,
1.),(1.,0.707106781186548,1.,0.707106781186548,1.,0.707106781186548,1.,
0.707106781186548,1.),(1.,0.707106781186547,1.,0.707106781186547,1.,0.707106781186547,
1.,0.707106781186547,1.),(1.,0.707106781186548,1.,0.707106781186548,1.,
0.707106781186548,1.,0.707106781186548,1.),(1.,0.707106781186547,1.,0.707106781186547,
1.,0.707106781186547,1.,0.707106781186547,1.),(1.,0.707106781186548,1.,
0.707106781186548,1.,0.707106781186548,1.,0.707106781186548,1.),(1.,0.707106781186547,
1.,0.707106781186547,1.,0.707106781186547,1.,0.707106781186547,1.),(1.,
0.707106781186548,1.,0.707106781186548,1.,0.707106781186548,1.,0.707106781186548,
1.),(1.,0.707106781186547,1.,0.707106781186547,1.,0.707106781186547,1.,
0.707106781186547,1.),(1.,0.707106781186548,1.,0.707106781186548,1.,0.707106781186548,
1.,0.707106781186548,1.),(1.,0.707106781186547,1.,0.707106781186547,1.,
0.707106781186547,1.,0.707106781186547,1.),(1.,0.707106781186547,1.,0.707106781186547,
1.,0.707106781186547,1.,0.707106781186547,1.),(1.,0.707106781186547,1.,
0.707106781186547,1.,0.707106781186547,1.,0.707106781186547,1.),(1.,0.707106781186547,
1.,0.707106781186547,1.,0.707106781186547,1.,0.707106781186547,1.),(1.,
0.707106781186548,1.,0.707106781186548,1.,0.707106781186548,1.,0.707106781186548,
1.),(1.,0.707106781186548,1.,0.707106781186548,1.,0.707106781186548,1.,
0.707106781186548,1.),(1.,0.707106781186547,1.,0.707106781186547,1.,0.707106781186547,
1.,0.707106781186547,1.),(1.,0.707106781186548,1.,0.707106781186548,1.,
0.707106781186548,1.,0.707106781186548,1.),(1.,0.707106781186548,1.,0.707106781186548,
1.,0.707106781186548,1.,0.707106781186548,1.),(1.,0.707106781186547,1.,
0.707106781186547,1.,0.707106781186547,1.,0.707106781186547,1.),(1.,0.707106781186548,
1.,0.707106781186548,1.,0.707106781186548,1.,0.707106781186548,1.),(1.,
0.707106781186547,1.,0.707106781186547,1.,0.707106781186547,1.,0.707106781186547,
1.),(1.,0.707106781186547,1.,0.707106781186547,1.,0.707106781186547,1.,
0.707106781186547,1.),(1.,0.707106781186548,1.,0.707106781186548,1.,0.707106781186548,
1.,0.707106781186548,1.),(1.,0.707106781186547,1.,0.707106781186547,1.,
0.707106781186547,1.,0.707106781186547,1.),(1.,0.707106781186547,1.,0.707106781186547,
1.,0.707106781186547,1.,0.707106781186547,1.),(1.,0.707106781186547,1.,
0.707106781186547,1.,0.707106781186547,1.,0.707106781186547,1.),(1.,0.707106781186547,
1.,0.707106781186547,1.,0.707106781186547,1.,0.707106781186547,1.),(1.,
0.707106781186548,1.,0.707106781186548,1.,0.707106781186548,1.,0.707106781186548,
1.),(1.,0.707106781186547,1.,0.707106781186547,1.,0.707106781186547,1.,
0.707106781186547,1.),(1.,0.707106781186547,1.,0.707106781186547,1.,0.707106781186547,
1.,0.707106781186547,1.),(1.,0.707106781186547,1.,0.707106781186547,1.,
0.707106781186547,1.,0.707106781186547,1.),(1.,0.707106781186548,1.,0.707106781186548,
1.,0.707106781186548,1.,0.707106781186548,1.),(1.,0.707106781186547,1.,
0.707106781186547,1.,0.707106781186547,1.,0.707106781186547,1.),(1.,0.707106781186547,
1.,0.707106781186547,1.,0.707106781186547,1.,0.707106781186547,1.),(1.,
0.707106781186548,1.,0.707106781186548,1.,0.707106781186548,1.,0.707106781186548,
1.),(1.,0.707106781186547,1.,0.707106781186547,1.,0.707106781186547,1.,
0.707106781186547,1.),(1.,0.707106781186548,1.,0.707106781186548,1.,0.707106781186548,
1.,0.707106781186548,1.),(1.,0.707106781186548,1.,0.707106781186548,1.,
0.707106781186548,1.,0.707106781186548,1.),(1.,0.707106781186547,1.,0.707106781186547,
1.,0.707106781186547,1.,0.707106781186547,1.),(1.,0.707106781186548,1.,
0.707106781186548,1.,0.707106781186548,1.,0.707106781186548,1.),(1.,0.707106781186547,
1.,0.707106781186547,1.,0.707106781186547,1.,0.707106781186547,1.),(1.,
0.707106781186548,1.,0.707106781186548,1.,0.707106781186548,1.,0.707106781186548,
1.),(1.,0.707106781186547,1.,0.707106781186547,1.,0.707106781186547,1.,
0.707106781186547,1.),(1.,0.707106781186548,1.,0.707106781186548,1.,0.707106781186548,
1.,0.707106781186548,1.),(1.,0.707106781186547,1.,0.707106781186547,1.,
0.707106781186547,1.,0.707106781186547,1.),(1.,0.707106781186547,1.,0.707106781186547,
1.,0.707106781186547,1.,0.707106781186547,1.),(1.,0.707106781186548,1.,
0.707106781186548,1.,0.707106781186548,1.,0.707106781186548,1.),(1.,0.707106781186547,
1.,0.707106781186547,1.,0.707106781186547,1.,0.707106781186547,1.),(1.,
0.707106781186548,1.,0.707106781186548,1.,0.707106781186548,1.,0.707106781186548,
1.),(1.,0.707106781186548,1.,0.707106781186548,1.,0.707106781186548,1.,
0.707106781186548,1.),(1.,0.707106781186547,1.,0.707106781186547,1.,0.707106781186547,
1.,0.707106781186547,1.),(1.,0.707106781186547,1.,0.707106781186547,1.,
0.707106781186547,1.,0.707106781186547,1.),(1.,0.707106781186548,1.,0.707106781186548,
1.,0.707106781186548,1.,0.707106781186548,1.),(1.,0.707106781186547,1.,
0.707106781186547,1.,0.707106781186547,1.,0.707106781186547,1.),(1.,0.707106781186548,
1.,0.707106781186548,1.,0.707106781186548,1.,0.707106781186548,1.),(1.,
0.707106781186547,1.,0.707106781186547,1.,0.707106781186547,1.,0.707106781186547,
1.),(1.,0.707106781186548,1.,0.707106781186548,1.,0.707106781186548,1.,
0.707106781186548,1.),(1.,0.707106781186547,1.,0.707106781186547,1.,0.707106781186547,
1.,0.707106781186547,1.),(1.,0.707106781186547,1.,0.707106781186547,1.,
0.707106781186547,1.,0.707106781186547,1.),(1.,0.707106781186548,1.,0.707106781186548,
1.,0.707106781186548,1.,0.707106781186548,1.),(1.,0.707106781186548,1.,
0.707106781186548,1.,0.707106781186548,1.,0.707106781186548,1.),(1.,0.707106781186547,
1.,0.707106781186547,1.,0.707106781186547,1.,0.707106781186547,1.),(1.,
0.707106781186548,1.,0.707106781186548,1.,0.707106781186548,1.,0.707106781186548,
1.),(1.,0.707106781186548,1.,0.707106781186548,1.,0.707106781186548,1.,
0.707106781186548,1.),(1.,0.707106781186547,1.,0.707106781186547,1.,0.707106781186547,
1.,0.707106781186547,1.),(1.,0.707106781186548,1.,0.707106781186548,1.,
0.707106781186548,1.,0.707106781186548,1.),(1.,0.707106781186548,1.,0.707106781186548,
1.,0.707106781186548,1.,0.707106781186548,1.),(1.,0.707106781186547,1.,
0.707106781186547,1.,0.707106781186547,1.,0.707106781186547,1.),(1.,0.707106781186548,
1.,0.707106781186548,1.,0.707106781186548,1.,0.707106781186548,1.),(1.,
0.707106781186547,1.,0.707106781186547,1.,0.707106781186547,1.,0.707106781186547,
1.),(1.,0.707106781186548,1.,0.707106781186548,1.,0.707106781186548,1.,
0.707106781186548,1.),(1.,0.707106781186547,1.,0.707106781186547,1.,0.707106781186547,
1.,0.707106781186547,1.),(1.,0.707106781186548,1.,0.707106781186548,1.,
0.707106781186548,1.,0.707106781186548,1.),(1.,0.707106781186547,1.,0.707106781186547,
1.,0.707106781186547,1.,0.707106781186547,1.),(1.,0.707106781186548,1.,
0.707106781186548,1.,0.707106781186548,1.,0.707106781186548,1.),(1.,0.707106781186547,
1.,0.707106781186547,1.,0.707106781186547,1.,0.707106781186547,1.),(1.,
0.707106781186547,1.,0.707106781186547,1.,0.707106781186547,1.,0.707106781186547,
1.),(1.,0.707106781186548,1.,0.707106781186548,1.,0.707106781186548,1.,
0.707106781186548,1.),(1.,0.707106781186547,1.,0.707106781186547,1.,0.707106781186547,
1.,0.707106781186547,1.),(1.,0.707106781186547,1.,0.707106781186547,1.,
0.707106781186547,1.,0.707106781186547,1.),(1.,0.707106781186548,1.,0.707106781186548,
1.,0.707106781186548,1.,0.707106781186548,1.),(1.,0.707106781186547,1.,
0.707106781186547,1.,0.707106781186547,1.,0.707106781186547,1.),(1.,0.707106781186548,
1.,0.707106781186548,1.,0.707106781186548,1.,0.707106781186548,1.),(1.,
0.707106781186548,1.,0.707106781186548,1.,0.707106781186548,1.,0.707106781186548,
1.),(1.,0.707106781186547,1.,0.707106781186547,1.,0.707106781186547,1.,
0.707106781186547,1.),(1.,0.707106781186547,1.,0.707106781186547,1.,0.707106781186547,
1.,0.707106781186547,1.),(1.,0.707106781186547,1.,0.707106781186547,1.,
0.707106781186547,1.,0.707106781186547,1.),(1.,0.707106781186548,1.,0.707106781186548,
1.,0.707106781186548,1.,0.707106781186548,1.),(1.,0.707106781186547,1.,
0.707106781186547,1.,0.707106781186547,1.,0.707106781186547,1.),(1.,0.707106781186548,
1.,0.707106781186548,1.,0.707106781186548,1.,0.707106781186548,1.),(1.,
0.707106781186548,1.,0.707106781186548,1.,0.707106781186548,1.,0.707106781186548,
1.),(1.,0.707106781186547,1.,0.707106781186547,1.,0.707106781186547,1.,
0.707106781186547,1.),(1.,0.707106781186548,1.,0.707106781186548,1.,0.707106781186548,
1.,0.707106781186548,1.),(1.,0.707106781186547,1.,0.707106781186547,1.,
0.707106781186547,1.,0.707106781186547,1.),(1.,0.707106781186548,1.,0.707106781186548,
1.,0.707106781186548,1.,0.707106781186548,1.),(1.,0.707106781186547,1.,
0.707106781186547,1.,0.707106781186547,1.,0.707106781186547,1.),(1.,0.707106781186548,
1.,0.707106781186548,1.,0.707106781186548,1.,0.707106781186548,1.),(1.,
0.707106781186547,1.,0.707106781186547,1.,0.707106781186547,1.,0.707106781186547,
1.),(1.,0.707106781186547,1.,0.707106781186547,1.,0.707106781186547,1.,
0.707106781186547,1.),(1.,0.707106781186548,1.,0.707106781186548,1.,0.707106781186548,
1.,0.707106781186548,1.),(1.,0.707106781186548,1.,0.707106781186548,1.,
0.707106781186548,1.,0.707106781186548,1.),(1.,0.707106781186548,1.,0.707106781186548,
1.,0.707106781186548,1.,0.707106781186548,1.),(1.,0.707106781186547,1.,
0.707106781186547,1.,0.707106781186547,1.,0.707106781186547,1.),(1.,0.707106781186548,
1.,0.707106781186548,1.,0.707106781186548,1.,0.707106781186548,1.),(1.,
0.707106781186548,1.,0.707106781186548,1.,0.707106781186548,1.,0.707106781186548,
1.),(1.,0.707106781186547,1.,0.707106781186547,1.,0.707106781186547,1.,
0.707106781186547,1.),(1.,0.707106781186548,1.,0.707106781186548,1.,0.707106781186548,
1.,0.707106781186548,1.),(1.,0.707106781186547,1.,0.707106781186547,1.,
0.707106781186547,1.,0.707106781186547,1.),(1.,0.707106781186548,1.,0.707106781186548,
1.,0.707106781186548,1.,0.707106781186548,1.),(1.,0.707106781186548,1.,
0.707106781186548,1.,0.707106781186548,1.,0.707106781186548,1.),(1.,0.707106781186548,
1.,0.707106781186548,1.,0.707106781186548,1.,0.707106781186548,1.),(1.,
0.707106781186548,1.,0.707106781186548,1.,0.707106781186548,1.,0.707106781186548,
1.),(1.,0.707106781186548,1.,0.707106781186548,1.,0.707106781186548,1.,
0.707106781186548,1.),(1.,0.707106781186548,1.,0.707106781186548,1.,0.707106781186548,
1.,0.707106781186548,1.),(1.,0.707106781186547,1.,0.707106781186547,1.,
0.707106781186547,1.,0.707106781186547,1.),(1.,0.707106781186547,1.,0.707106781186547,
1.,0.707106781186547,1.,0.707106781186547,1.),(1.,0.707106781186548,1.,
0.707106781186548,1.,0.707106781186548,1.,0.707106781186548,1.),(1.,0.707106781186547,
1.,0.707106781186547,1.,0.707106781186547,1.,0.707106781186547,1.),(1.,
0.707106781186547,1.,0.707106781186547,1.,0.707106781186547,1.,0.707106781186547,
1.),(1.,0.707106781186548,1.,0.707106781186548,1.,0.707106781186548,1.,
0.707106781186548,1.),(1.,0.707106781186547,1.,0.707106781186547,1.,0.707106781186547,
1.,0.707106781186547,1.),(1.,0.707106781186547,1.,0.707106781186547,1.,
0.707106781186547,1.,0.707106781186547,1.),(1.,0.707106781186548,1.,0.707106781186548,
1.,0.707106781186548,1.,0.707106781186548,1.),(1.,0.707106781186547,1.,
0.707106781186547,1.,0.707106781186547,1.,0.707106781186547,1.),(1.,0.707106781186548,
1.,0.707106781186548,1.,0.707106781186548,1.,0.707106781186548,1.),(1.,
0.707106781186547,1.,0.707106781186547,1.,0.707106781186547,1.,0.707106781186547,
1.),(1.,0.707106781186548,1.,0.707106781186548,1.,0.707106781186548,1.,
0.707106781186548,1.),(1.,0.707106781186547,1.,0.707106781186547,1.,0.707106781186547,
1.,0.707106781186547,1.),(1.,0.707106781186547,1.,0.707106781186547,1.,
0.707106781186547,1.,0.707106781186547,1.),(1.,0.707106781186547,1.,0.707106781186547,
1.,0.707106781186547,1.,0.707106781186547,1.),(1.,0.707106781186548,1.,
0.707106781186548,1.,0.707106781186548,1.,0.707106781186548,1.),(1.,0.707106781186547,
1.,0.707106781186547,1.,0.707106781186547,1.,0.707106781186547,1.),(1.,
0.707106781186547,1.,0.707106781186547,1.,0.707106781186547,1.,0.707106781186547,
1.),(1.,0.707106781186548,1.,0.707106781186548,1.,0.707106781186548,1.,
0.707106781186548,1.),(1.,0.707106781186547,1.,0.707106781186547,1.,0.707106781186547,
1.,0.707106781186547,1.),(1.,0.707106781186548,1.,0.707106781186548,1.,
0.707106781186548,1.,0.707106781186548,1.),(1.,0.707106781186547,1.,0.707106781186547,
1.,0.707106781186547,1.,0.707106781186547,1.),(1.,0.707106781186548,1.,
0.707106781186548,1.,0.707106781186548,1.,0.707106781186548,1.),(1.,0.707106781186547,
1.,0.707106781186547,1.,0.707106781186547,1.,0.707106781186547,1.),(1.,
0.707106781186547,1.,0.707106781186547,1.,0.707106781186547,1.,0.707106781186547,
1.),(1.,0.707106781186547,1.,0.707106781186547,1.,0.707106781186547,1.,
0.707106781186547,1.),(1.,0.707106781186547,1.,0.707106781186547,1.,0.707106781186547,
1.,0.707106781186547,1.),(1.,0.707106781186548,1.,0.707106781186548,1.,
0.707106781186548,1.,0.707106781186548,1.),(1.,0.707106781186547,1.,0.707106781186547,
1.,0.707106781186547,1.,0.707106781186547,1.),(1.,0.707106781186547,1.,
0.707106781186547,1.,0.707106781186547,1.,0.707106781186547,1.),(1.,0.707106781186548,
1.,0.707106781186548,1.,0.707106781186548,1.,0.707106781186548,1.),(1.,
0.707106781186548,1.,0.707106781186548,1.,0.707106781186548,1.,0.707106781186548,
1.),(1.,0.707106781186547,1.,0.707106781186547,1.,0.707106781186547,1.,
0.707106781186547,1.),(1.,0.707106781186548,1.,0.707106781186548,1.,0.707106781186548,
1.,0.707106781186548,1.),(1.,0.707106781186547,1.,0.707106781186547,1.,
0.707106781186547,1.,0.707106781186547,1.),(1.,0.707106781186548,1.,0.707106781186548,
1.,0.707106781186548,1.,0.707106781186548,1.),(1.,0.707106781186547,1.,
0.707106781186547,1.,0.707106781186547,1.,0.707106781186547,1.),(1.,0.707106781186547,
1.,0.707106781186547,1.,0.707106781186547,1.,0.707106781186547,1.),(1.,
0.707106781186548,1.,0.707106781186548,1.,0.707106781186548,1.,0.707106781186548,
1.),(1.,0.707106781186547,1.,0.707106781186547,1.,0.707106781186547,1.,
0.707106781186547,1.),(1.,0.707106781186548,1.,0.707106781186548,1.,0.707106781186548,
1.,0.707106781186548,1.),(1.,0.707106781186547,1.,0.707106781186547,1.,
0.707106781186547,1.,0.707106781186547,1.),(1.,0.707106781186548,1.,0.707106781186548,
1.,0.707106781186548,1.,0.707106781186548,1.),(1.,0.707106781186547,1.,
0.707106781186547,1.,0.707106781186547,1.,0.707106781186547,1.),(1.,0.707106781186548,
1.,0.707106781186548,1.,0.707106781186548,1.,0.707106781186548,1.),(1.,
0.707106781186548,1.,0.707106781186548,1.,0.707106781186548,1.,0.707106781186548,
1.),(1.,0.707106781186547,1.,0.707106781186547,1.,0.707106781186547,1.,
0.707106781186547,1.),(1.,0.707106781186548,1.,0.707106781186548,1.,0.707106781186548,
1.,0.707106781186548,1.),(1.,0.707106781186547,1.,0.707106781186547,1.,
0.707106781186547,1.,0.707106781186547,1.),(1.,0.707106781186547,1.,0.707106781186547,
1.,0.707106781186547,1.,0.707106781186547,1.),(1.,0.707106781186548,1.,
0.707106781186548,1.,0.707106781186548,1.,0.707106781186548,1.),(1.,0.707106781186547,
1.,0.707106781186547,1.,0.707106781186547,1.,0.707106781186547,1.),(1.,
0.707106781186547,1.,0.707106781186547,1.,0.707106781186547,1.,0.707106781186547,
1.),(1.,0.707106781186548,1.,0.707106781186548,1.,0.707106781186548,1.,
0.707106781186548,1.),(1.,0.707106781186548,1.,0.707106781186548,1.,0.707106781186548,
1.,0.707106781186548,1.),(1.,0.707106781186548,1.,0.707106781186548,1.,
0.707106781186548,1.,0.707106781186548,1.),(1.,0.707106781186547,1.,0.707106781186547,
1.,0.707106781186547,1.,0.707106781186547,1.),(1.,0.707106781186548,1.,
0.707106781186548,1.,0.707106781186548,1.,0.707106781186548,1.),(1.,0.707106781186547,
1.,0.707106781186547,1.,0.707106781186547,1.,0.707106781186547,1.),(1.,
0.707106781186547,1.,0.707106781186547,1.,0.707106781186547,1.,0.707106781186547,
1.),(1.,0.707106781186547,1.,0.707106781186547,1.,0.707106781186547,1.,
0.707106781186547,1.),(1.,0.707106781186548,1.,0.707106781186548,1.,0.707106781186548,
1.,0.707106781186548,1.),(1.,0.707106781186547,1.,0.707106781186547,1.,
0.707106781186547,1.,0.707106781186547,1.),(1.,0.707106781186548,1.,0.707106781186548,
1.,0.707106781186548,1.,0.707106781186548,1.),(1.,0.707106781186548,1.,
0.707106781186548,1.,0.707106781186548,1.,0.707106781186548,1.),(1.,0.707106781186548,
1.,0.707106781186548,1.,0.707106781186548,1.,0.707106781186548,1.),(1.,
0.707106781186547,1.,0.707106781186547,1.,0.707106781186547,1.,0.707106781186547,
1.),(1.,0.707106781186547,1.,0.707106781186547,1.,0.707106781186547,1.,
0.707106781186547,1.),(1.,0.707106781186547,1.,0.707106781186547,1.,0.707106781186547,
1.,0.707106781186547,1.),(1.,0.707106781186547,1.,0.707106781186547,1.,
0.707106781186547,1.,0.707106781186547,1.),(1.,0.707106781186548,1.,0.707106781186548,
1.,0.707106781186548,1.,0.707106781186548,1.),(1.,0.707106781186547,1.,
0.707106781186547,1.,0.707106781186547,1.,0.707106781186547,1.),(1.,0.707106781186547,
1.,0.707106781186547,1.,0.707106781186547,1.,0.707106781186547,1.),(1.,
0.707106781186548,1.,0.707106781186548,1.,0.707106781186548,1.,0.707106781186548,
1.),(1.,0.707106781186547,1.,0.707106781186547,1.,0.707106781186547,1.,
0.707106781186547,1.),(1.,0.707106781186548,1.,0.707106781186548,1.,0.707106781186548,
1.,0.707106781186548,1.),(1.,0.707106781186547,1.,0.707106781186547,1.,
0.707106781186547,1.,0.707106781186547,1.),(1.,0.707106781186547,1.,0.707106781186547,
1.,0.707106781186547,1.,0.707106781186547,1.),(1.,0.707106781186548,1.,
0.707106781186548,1.,0.707106781186548,1.,0.707106781186548,1.),(1.,0.707106781186547,
1.,0.707106781186547,1.,0.707106781186547,1.,0.707106781186547,1.),(1.,
0.707106781186548,1.,0.707106781186548,1.,0.707106781186548,1.,0.707106781186548,
1.),(1.,0.707106781186547,1.,0.707106781186547,1.,0.707106781186547,1.,
0.707106781186547,1.),(1.,0.707106781186548,1.,0.707106781186548,1.,0.707106781186548,
1.,0.707106781186548,1.),(1.,0.707106781186547,1.,0.707106781186547,1.,
0.707106781186547,1.,0.707106781186547,1.),(1.,0.707106781186547,1.,0.707106781186547,
1.,0.707106781186547,1.,0.707106781186547,1.),(1.,0.707106781186547,1.,
0.707106781186547,1.,0.707106781186547,1.,0.707106781186547,1.),(1.,0.707106781186547,
1.,0.707106781186547,1.,0.707106781186547,1.,0.707106781186547,1.),(1.,
0.707106781186547,1.,0.707106781186547,1.,0.707106781186547,1.,0.707106781186547,
1.),(1.,0.707106781186547,1.,0.707106781186547,1.,0.707106781186547,1.,
0.707106781186547,1.),(1.,0.707106781186548,1.,0.707106781186548,1.,0.707106781186548,
1.,0.707106781186548,1.),(1.,0.707106781186547,1.,0.707106781186547,1.,
0.707106781186547,1.,0.707106781186547,1.),(1.,0.707106781186547,1.,0.707106781186547,
1.,0.707106781186547,1.,0.707106781186547,1.),(1.,0.707106781186548,1.,
0.707106781186548,1.,0.707106781186548,1.,0.707106781186548,1.),(1.,0.707106781186548,
1.,0.707106781186548,1.,0.707106781186548,1.,0.707106781186548,1.),(1.,
0.707106781186547,1.,0.707106781186547,1.,0.707106781186547,1.,0.707106781186547,
1.),(1.,0.707106781186548,1.,0.707106781186548,1.,0.707106781186548,1.,
0.707106781186548,1.),(1.,0.707106781186548,1.,0.707106781186548,1.,0.707106781186548,
1.,0.707106781186548,1.),(1.,0.707106781186547,1.,0.707106781186547,1.,
0.707106781186547,1.,0.707106781186547,1.),(1.,0.707106781186547,1.,0.707106781186547,
1.,0.707106781186547,1.,0.707106781186547,1.),(1.,0.707106781186548,1.,
0.707106781186548,1.,0.707106781186548,1.,0.707106781186548,1.),(1.,0.707106781186547,
1.,0.707106781186547,1.,0.707106781186547,1.,0.707106781186547,1.),(1.,
0.707106781186547,1.,0.707106781186547,1.,0.707106781186547,1.,0.707106781186547,
1.),(1.,0.707106781186548,1.,0.707106781186548,1.,0.707106781186548,1.,
0.707106781186548,1.),(1.,0.707106781186547,1.,0.707106781186547,1.,0.707106781186547,
1.,0.707106781186547,1.),(1.,0.707106781186548,1.,0.707106781186548,1.,
0.707106781186548,1.,0.707106781186548,1.),(1.,0.707106781186548,1.,0.707106781186548,
1.,0.707106781186548,1.,0.707106781186548,1.),(1.,0.707106781186548,1.,
0.707106781186548,1.,0.707106781186548,1.,0.707106781186548,1.),(1.,0.707106781186547,
1.,0.707106781186547,1.,0.707106781186547,1.,0.707106781186547,1.),(1.,
0.707106781186547,1.,0.707106781186547,1.,0.707106781186547,1.,0.707106781186547,
1.),(1.,0.707106781186547,1.,0.707106781186547,1.,0.707106781186547,1.,
0.707106781186547,1.),(1.,0.707106781186547,1.,0.707106781186547,1.,0.707106781186547,
1.,0.707106781186547,1.),(1.,0.707106781186548,1.,0.707106781186548,1.,
0.707106781186548,1.,0.707106781186548,1.),(1.,0.707106781186548,1.,0.707106781186548,
1.,0.707106781186548,1.,0.707106781186548,1.),(1.,0.707106781186548,1.,
0.707106781186548,1.,0.707106781186548,1.,0.707106781186548,1.),(1.,0.707106781186547,
1.,0.707106781186547,1.,0.707106781186547,1.,0.707106781186547,1.),(1.,
0.707106781186548,1.,0.707106781186548,1.,0.707106781186548,1.,0.707106781186548,
1.),(1.,0.707106781186547,1.,0.707106781186547,1.,0.707106781186547,1.,
0.707106781186547,1.),(1.,0.707106781186548,1.,0.707106781186548,1.,0.707106781186548,
1.,0.707106781186548,1.),(1.,0.707106781186548,1.,0.707106781186548,1.,
0.707106781186548,1.,0.707106781186548,1.),(1.,0.707106781186547,1.,0.707106781186547,
1.,0.707106781186547,1.,0.707106781186547,1.),(1.,0.707106781186548,1.,
0.707106781186548,1.,0.707106781186548,1.,0.707106781186548,1.),(1.,0.707106781186547,
1.,0.707106781186547,1.,0.707106781186547,1.,0.707106781186547,1.),(1.,
0.707106781186548,1.,0.707106781186548,1.,0.707106781186548,1.,0.707106781186548,
1.),(1.,0.707106781186548,1.,0.707106781186548,1.,0.707106781186548,1.,
0.707106781186548,1.),(1.,0.707106781186547,1.,0.707106781186547,1.,0.707106781186547,
1.,0.707106781186547,1.),(1.,0.707106781186547,1.,0.707106781186547,1.,
0.707106781186547,1.,0.707106781186547,1.),(1.,0.707106781186548,1.,0.707106781186548,
1.,0.707106781186548,1.,0.707106781186548,1.),(1.,0.707106781186547,1.,
0.707106781186547,1.,0.707106781186547,1.,0.707106781186547,1.),(1.,0.707106781186548,
1.,0.707106781186548,1.,0.707106781186548,1.,0.707106781186548,1.),(1.,
0.707106781186547,1.,0.707106781186547,1.,0.707106781186547,1.,0.707106781186547,
1.),(1.,0.707106781186548,1.,0.707106781186548,1.,0.707106781186548,1.,
0.707106781186548,1.),(1.,0.707106781186548,1.,0.707106781186548,1.,0.707106781186548,
1.,0.707106781186548,1.),(1.,0.707106781186548,1.,0.707106781186548,1.,
0.707106781186548,1.,0.707106781186548,1.),(1.,0.707106781186547,1.,0.707106781186547,
1.,0.707106781186547,1.,0.707106781186547,1.),(1.,0.707106781186548,1.,
0.707106781186548,1.,0.707106781186548,1.,0.707106781186548,1.),(1.,0.707106781186547,
1.,0.707106781186547,1.,0.707106781186547,1.,0.707106781186547,1.),(1.,
0.707106781186547,1.,0.707106781186547,1.,0.707106781186547,1.,0.707106781186547,
1.),(1.,0.707106781186547,1.,0.707106781186547,1.,0.707106781186547,1.,
0.707106781186547,1.),(1.,0.707106781186547,1.,0.707106781186547,1.,0.707106781186547,
1.,0.707106781186547,1.),(1.,0.707106781186548,1.,0.707106781186548,1.,
0.707106781186548,1.,0.707106781186548,1.),(1.,0.707106781186548,1.,0.707106781186548,
1.,0.707106781186548,1.,0.707106781186548,1.),(1.,0.707106781186547,1.,
0.707106781186547,1.,0.707106781186547,1.,0.707106781186547,1.),(1.,0.707106781186547,
1.,0.707106781186547,1.,0.707106781186547,1.,0.707106781186547,1.),(1.,
0.707106781186547,1.,0.707106781186547,1.,0.707106781186547,1.,0.707106781186547,
1.),(1.,0.707106781186548,1.,0.707106781186548,1.,0.707106781186548,1.,
0.707106781186548,1.),(1.,0.707106781186547,1.,0.707106781186547,1.,0.707106781186547,
1.,0.707106781186547,1.),(1.,0.707106781186547,1.,0.707106781186547,1.,
0.707106781186547,1.,0.707106781186547,1.),(1.,0.707106781186548,1.,0.707106781186548,
1.,0.707106781186548,1.,0.707106781186548,1.),(1.,0.707106781186547,1.,
0.707106781186547,1.,0.707106781186547,1.,0.707106781186547,1.),(1.,0.707106781186548,
1.,0.707106781186548,1.,0.707106781186548,1.,0.707106781186548,1.),(1.,
0.707106781186548,1.,0.707106781186548,1.,0.707106781186548,1.,0.707106781186548,
1.),(1.,0.707106781186548,1.,0.707106781186548,1.,0.707106781186548,1.,
0.707106781186548,1.),(1.,0.707106781186547,1.,0.707106781186547,1.,0.707106781186547,
1.,0.707106781186547,1.),(1.,0.707106781186547,1.,0.707106781186547,1.,
0.707106781186547,1.,0.707106781186547,1.),(1.,0.707106781186547,1.,0.707106781186547,
1.,0.707106781186547,1.,0.707106781186547,1.),(1.,0.707106781186547,1.,
0.707106781186547,1.,0.707106781186547,1.,0.707106781186547,1.),(1.,0.707106781186548,
1.,0.707106781186548,1.,0.707106781186548,1.,0.707106781186548,1.),(1.,
0.707106781186548,1.,0.707106781186548,1.,0.707106781186548,1.,0.707106781186548,
1.),(1.,0.707106781186547,1.,0.707106781186547,1.,0.707106781186547,1.,
0.707106781186547,1.),(1.,0.707106781186548,1.,0.707106781186548,1.,0.707106781186548,
1.,0.707106781186548,1.),(1.,0.707106781186547,1.,0.707106781186547,1.,
0.707106781186547,1.,0.707106781186547,1.),(1.,0.707106781186548,1.,0.707106781186548,
1.,0.707106781186548,1.,0.707106781186548,1.),(1.,0.707106781186548,1.,
0.707106781186548,1.,0.707106781186548,1.,0.707106781186548,1.),(1.,0.707106781186547,
1.,0.707106781186547,1.,0.707106781186547,1.,0.707106781186547,1.),(1.,
0.707106781186548,1.,0.707106781186548,1.,0.707106781186548,1.,0.707106781186548,
1.),(1.,0.707106781186547,1.,0.707106781186547,1.,0.707106781186547,1.,
0.707106781186547,1.),(1.,0.707106781186548,1.,0.707106781186548,1.,0.707106781186548,
1.,0.707106781186548,1.),(1.,0.707106781186547,1.,0.707106781186547,1.,
0.707106781186547,1.,0.707106781186547,1.),(1.,0.707106781186547,1.,0.707106781186547,
1.,0.707106781186547,1.,0.707106781186547,1.),(1.,0.707106781186547,1.,
0.707106781186547,1.,0.707106781186547,1.,0.707106781186547,1.),(1.,0.707106781186548,
1.,0.707106781186548,1.,0.707106781186548,1.,0.707106781186548,1.),(1.,
0.707106781186547,1.,0.707106781186547,1.,0.707106781186547,1.,0.707106781186547,
1.),(1.,0.707106781186548,1.,0.707106781186548,1.,0.707106781186548,1.,
0.707106781186548,1.),(1.,0.707106781186547,1.,0.707106781186547,1.,0.707106781186547,
1.,0.707106781186547,1.),(1.,0.707106781186548,1.,0.707106781186548,1.,
0.707106781186548,1.,0.707106781186548,1.),(1.,0.707106781186547,1.,0.707106781186547,
1.,0.707106781186547,1.,0.707106781186547,1.),(1.,0.707106781186548,1.,
0.707106781186548,1.,0.707106781186548,1.,0.707106781186548,1.),(1.,0.707106781186547,
1.,0.707106781186547,1.,0.707106781186547,1.,0.707106781186547,1.),(1.,
0.707106781186548,1.,0.707106781186548,1.,0.707106781186548,1.,0.707106781186548,
1.),(1.,0.707106781186547,1.,0.707106781186547,1.,0.707106781186547,1.,
0.707106781186547,1.),(1.,0.707106781186547,1.,0.707106781186547,1.,0.707106781186547,
1.,0.707106781186547,1.),(1.,0.707106781186548,1.,0.707106781186548,1.,
0.707106781186548,1.,0.707106781186548,1.),(1.,0.707106781186547,1.,0.707106781186547,
1.,0.707106781186547,1.,0.707106781186547,1.),(1.,0.707106781186548,1.,
0.707106781186548,1.,0.707106781186548,1.,0.707106781186548,1.),(1.,0.707106781186547,
1.,0.707106781186547,1.,0.707106781186547,1.,0.707106781186547,1.),(1.,
0.707106781186547,1.,0.707106781186547,1.,0.707106781186547,1.,0.707106781186547,
1.),(1.,0.707106781186548,1.,0.707106781186548,1.,0.707106781186548,1.,
0.707106781186548,1.),(1.,0.707106781186548,1.,0.707106781186548,1.,0.707106781186548,
1.,0.707106781186548,1.),(1.,0.707106781186547,1.,0.707106781186547,1.,
0.707106781186547,1.,0.707106781186547,1.),(1.,0.707106781186548,1.,0.707106781186548,
1.,0.707106781186548,1.,0.707106781186548,1.),(1.,0.707106781186548,1.,
0.707106781186548,1.,0.707106781186548,1.,0.707106781186548,1.),(1.,0.707106781186547,
1.,0.707106781186547,1.,0.707106781186547,1.,0.707106781186547,1.),(1.,
0.707106781186548,1.,0.707106781186548,1.,0.707106781186548,1.,0.707106781186548,
1.),(1.,0.707106781186547,1.,0.707106781186547,1.,0.707106781186547,1.,
0.707106781186547,1.),(1.,0.707106781186548,1.,0.707106781186548,1.,0.707106781186548,
1.,0.707106781186548,1.),(1.,0.707106781186547,1.,0.707106781186547,1.,
0.707106781186547,1.,0.707106781186547,1.),(1.,0.707106781186547,1.,0.707106781186547,
1.,0.707106781186547,1.,0.707106781186547,1.),(1.,0.707106781186547,1.,
0.707106781186547,1.,0.707106781186547,1.,0.707106781186547,1.),(1.,0.707106781186548,
1.,0.707106781186548,1.,0.707106781186548,1.,0.707106781186548,1.),(1.,
0.707106781186547,1.,0.707106781186547,1.,0.707106781186547,1.,0.707106781186547,
1.),(1.,0.707106781186547,1.,0.707106781186547,1.,0.707106781186547,1.,
0.707106781186547,1.),(1.,0.707106781186548,1.,0.707106781186548,1.,0.707106781186548,
1.,0.707106781186548,1.),(1.,0.707106781186547,1.,0.707106781186547,1.,
0.707106781186547,1.,0.707106781186547,1.),(1.,0.707106781186548,1.,0.707106781186548,
1.,0.707106781186548,1.,0.707106781186548,1.),(1.,0.707106781186547,1.,
0.707106781186547,1.,0.707106781186547,1.,0.707106781186547,1.),(1.,0.707106781186548,
1.,0.707106781186548,1.,0.707106781186548,1.,0.707106781186548,1.),(1.,
0.707106781186548,1.,0.707106781186548,1.,0.707106781186548,1.,0.707106781186548,
1.),(1.,0.707106781186547,1.,0.707106781186547,1.,0.707106781186547,1.,
0.707106781186547,1.),(1.,0.707106781186548,1.,0.707106781186548,1.,0.707106781186548,
1.,0.707106781186548,1.),(1.,0.707106781186547,1.,0.707106781186547,1.,
0.707106781186547,1.,0.707106781186547,1.),(1.,0.707106781186548,1.,0.707106781186548,
1.,0.707106781186548,1.,0.707106781186548,1.),(1.,0.707106781186548,1.,
0.707106781186548,1.,0.707106781186548,1.,0.707106781186548,1.),(1.,0.707106781186548,
1.,0.707106781186548,1.,0.707106781186548,1.,0.707106781186548,1.),(1.,
0.707106781186548,1.,0.707106781186548,1.,0.707106781186548,1.,0.707106781186548,
1.),(1.,0.707106781186547,1.,0.707106781186547,1.,0.707106781186547,1.,
0.707106781186547,1.),(1.,0.707106781186547,1.,0.707106781186547,1.,0.707106781186547,
1.,0.707106781186547,1.),(1.,0.707106781186548,1.,0.707106781186548,1.,
0.707106781186548,1.,0.707106781186548,1.),(1.,0.707106781186547,1.,0.707106781186547,
1.,0.707106781186547,1.,0.707106781186547,1.),(1.,0.707106781186547,1.,
0.707106781186547,1.,0.707106781186547,1.,0.707106781186547,1.),(1.,0.707106781186548,
1.,0.707106781186548,1.,0.707106781186548,1.,0.707106781186548,1.),(1.,
0.707106781186548,1.,0.707106781186548,1.,0.707106781186548,1.,0.707106781186548,
1.),(1.,0.707106781186547,1.,0.707106781186547,1.,0.707106781186547,1.,
0.707106781186547,1.),(1.,0.707106781186547,1.,0.707106781186547,1.,0.707106781186547,
1.,0.707106781186547,1.),(1.,0.707106781186548,1.,0.707106781186548,1.,
0.707106781186548,1.,0.707106781186548,1.),(1.,0.707106781186547,1.,0.707106781186547,
1.,0.707106781186547,1.,0.707106781186547,1.),(1.,0.707106781186547,1.,
0.707106781186547,1.,0.707106781186547,1.,0.707106781186547,1.),(1.,0.707106781186548,
1.,0.707106781186548,1.,0.707106781186548,1.,0.707106781186548,1.),(1.,
0.707106781186547,1.,0.707106781186547,1.,0.707106781186547,1.,0.707106781186547,
1.),(1.,0.707106781186548,1.,0.707106781186548,1.,0.707106781186548,1.,
0.707106781186548,1.),(1.,0.707106781186547,1.,0.707106781186547,1.,0.707106781186547,
1.,0.707106781186547,1.),(1.,0.707106781186548,1.,0.707106781186548,1.,
0.707106781186548,1.,0.707106781186548,1.),(1.,0.707106781186547,1.,0.707106781186547,
1.,0.707106781186547,1.,0.707106781186547,1.),(1.,0.707106781186547,1.,
0.707106781186547,1.,0.707106781186547,1.,0.707106781186547,1.),(1.,0.707106781186547,
1.,0.707106781186547,1.,0.707106781186547,1.,0.707106781186547,1.),(1.,
0.707106781186548,1.,0.707106781186548,1.,0.707106781186548,1.,0.707106781186548,
1.),(1.,0.707106781186547,1.,0.707106781186547,1.,0.707106781186547,1.,
0.707106781186547,1.),(1.,0.707106781186547,1.,0.707106781186547,1.,0.707106781186547,
1.,0.707106781186547,1.),(1.,0.707106781186548,1.,0.707106781186548,1.,
0.707106781186548,1.,0.707106781186548,1.),(1.,0.707106781186547,1.,0.707106781186547,
1.,0.707106781186547,1.,0.707106781186547,1.),(1.,0.707106781186548,1.,
0.707106781186548,1.,0.707106781186548,1.,0.707106781186548,1.),(1.,0.707106781186548,
1.,0.707106781186548,1.,0.707106781186548,1.,0.707106781186548,1.),(1.,
0.707106781186548,1.,0.707106781186548,1.,0.707106781186548,1.,0.707106781186548,
1.),(1.,0.707106781186547,1.,0.707106781186547,1.,0.707106781186547,1.,
0.707106781186547,1.),(1.,0.707106781186547,1.,0.707106781186547,1.,0.707106781186547,
1.,0.707106781186547,1.),(1.,0.707106781186547,1.,0.707106781186547,1.,
0.707106781186547,1.,0.707106781186547,1.),(1.,0.707106781186548,1.,0.707106781186548,
1.,0.707106781186548,1.,0.707106781186548,1.),(1.,0.707106781186548,1.,
0.707106781186548,1.,0.707106781186548,1.,0.707106781186548,1.),(1.,0.707106781186547,
1.,0.707106781186547,1.,0.707106781186547,1.,0.707106781186547,1.),(1.,
0.707106781186547,1.,0.707106781186547,1.,0.707106781186547,1.,0.707106781186547,
1.),(1.,0.707106781186547,1.,0.707106781186547,1.,0.707106781186547,1.,
0.707106781186547,1.),(1.,0.707106781186547,1.,0.707106781186547,1.,0.707106781186547,
1.,0.707106781186547,1.),(1.,0.707106781186548,1.,0.707106781186548,1.,
0.707106781186548,1.,0.707106781186548,1.),(1.,0.707106781186548,1.,0.707106781186548,
1.,0.707106781186548,1.,0.707106781186548,1.),(1.,0.707106781186547,1.,
0.707106781186547,1.,0.707106781186547,1.,0.707106781186547,1.),(1.,0.707106781186547,
1.,0.707106781186547,1.,0.707106781186547,1.,0.707106781186547,1.),(1.,
0.707106781186547,1.,0.707106781186547,1.,0.707106781186547,1.,0.707106781186547,
1.),(1.,0.707106781186548,1.,0.707106781186548,1.,0.707106781186548,1.,
0.707106781186548,1.),(1.,0.707106781186548,1.,0.707106781186548,1.,0.707106781186548,
1.,0.707106781186548,1.),(1.,0.707106781186547,1.,0.707106781186547,1.,
0.707106781186547,1.,0.707106781186547,1.),(1.,0.707106781186548,1.,0.707106781186548,
1.,0.707106781186548,1.,0.707106781186548,1.),(1.,0.707106781186547,1.,
0.707106781186547,1.,0.707106781186547,1.,0.707106781186547,1.),(1.,0.707106781186548,
1.,0.707106781186548,1.,0.707106781186548,1.,0.707106781186548,1.),(1.,
0.707106781186547,1.,0.707106781186547,1.,0.707106781186547,1.,0.707106781186547,
1.),(1.,0.707106781186548,1.,0.707106781186548,1.,0.707106781186548,1.,
0.707106781186548,1.),(1.,0.707106781186548,1.,0.707106781186548,1.,0.707106781186548,
1.,0.707106781186548,1.),(1.,0.707106781186547,1.,0.707106781186547,1.,
0.707106781186547,1.,0.707106781186547,1.),(1.,0.707106781186548,1.,0.707106781186548,
1.,0.707106781186548,1.,0.707106781186548,1.),(1.,0.707106781186548,1.,
0.707106781186548,1.,0.707106781186548,1.,0.707106781186548,1.),(1.,0.707106781186548,
1.,0.707106781186548,1.,0.707106781186548,1.,0.707106781186548,1.),(1.,
0.707106781186547,1.,0.707106781186547,1.,0.707106781186547,1.,0.707106781186547,
1.),(1.,0.707106781186547,1.,0.707106781186547,1.,0.707106781186547,1.,
0.707106781186547,1.),(1.,0.707106781186547,1.,0.707106781186547,1.,0.707106781186547,
1.,0.707106781186547,1.),(1.,0.707106781186548,1.,0.707106781186548,1.,
0.707106781186548,1.,0.707106781186548,1.),(1.,0.707106781186548,1.,0.707106781186548,
1.,0.707106781186548,1.,0.707106781186548,1.),(1.,0.707106781186548,1.,
0.707106781186548,1.,0.707106781186548,1.,0.707106781186548,1.),(1.,0.707106781186547,
1.,0.707106781186547,1.,0.707106781186547,1.,0.707106781186547,1.),(1.,
0.707106781186547,1.,0.707106781186547,1.,0.707106781186547,1.,0.707106781186547,
1.),(1.,0.707106781186548,1.,0.707106781186548,1.,0.707106781186548,1.,
0.707106781186548,1.),(1.,0.707106781186548,1.,0.707106781186548,1.,0.707106781186548,
1.,0.707106781186548,1.),(1.,0.707106781186547,1.,0.707106781186547,1.,
0.707106781186547,1.,0.707106781186547,1.),(1.,0.707106781186548,1.,0.707106781186548,
1.,0.707106781186548,1.,0.707106781186548,1.),(1.,0.707106781186547,1.,
0.707106781186547,1.,0.707106781186547,1.,0.707106781186547,1.),(1.,0.707106781186547,
1.,0.707106781186547,1.,0.707106781186547,1.,0.707106781186547,1.),(1.,
0.707106781186548,1.,0.707106781186548,1.,0.707106781186548,1.,0.707106781186548,
1.),(1.,0.707106781186547,1.,0.707106781186547,1.,0.707106781186547,1.,
0.707106781186547,1.),(1.,0.707106781186548,1.,0.707106781186548,1.,0.707106781186548,
1.,0.707106781186548,1.),(1.,0.707106781186547,1.,0.707106781186547,1.,
0.707106781186547,1.,0.707106781186547,1.),(1.,0.707106781186547,1.,0.707106781186547,
1.,0.707106781186547,1.,0.707106781186547,1.),(1.,0.707106781186548,1.,
0.707106781186548,1.,0.707106781186548,1.,0.707106781186548,1.),(1.,0.707106781186547,
1.,0.707106781186547,1.,0.707106781186547,1.,0.707106781186547,1.),(1.,
0.707106781186548,1.,0.707106781186548,1.,0.707106781186548,1.,0.707106781186548,
1.),(1.,0.707106781186548,1.,0.707106781186548,1.,0.707106781186548,1.,
0.707106781186548,1.),(1.,0.707106781186547,1.,0.707106781186547,1.,0.707106781186547,
1.,0.707106781186547,1.),(1.,0.707106781186547,1.,0.707106781186547,1.,
0.707106781186547,1.,0.707106781186547,1.),(1.,0.707106781186548,1.,0.707106781186548,
1.,0.707106781186548,1.,0.707106781186548,1.),(1.,0.707106781186547,1.,
0.707106781186547,1.,0.707106781186547,1.,0.707106781186547,1.),(1.,0.707106781186548,
1.,0.707106781186548,1.,0.707106781186548,1.,0.707106781186548,1.),(1.,
0.707106781186547,1.,0.707106781186547,1.,0.707106781186547,1.,0.707106781186547,
1.),(1.,0.707106781186547,1.,0.707106781186547,1.,0.707106781186547,1.,
0.707106781186547,1.),(1.,0.707106781186548,1.,0.707106781186548,1.,0.707106781186548,
1.,0.707106781186548,1.),(1.,0.707106781186547,1.,0.707106781186547,1.,
0.707106781186547,1.,0.707106781186547,1.),(1.,0.707106781186548,1.,0.707106781186548,
1.,0.707106781186548,1.,0.707106781186548,1.),(1.,0.707106781186547,1.,
0.707106781186547,1.,0.707106781186547,1.,0.707106781186547,1.),(1.,0.707106781186548,
1.,0.707106781186548,1.,0.707106781186548,1.,0.707106781186548,1.),(1.,
0.707106781186547,1.,0.707106781186547,1.,0.707106781186547,1.,0.707106781186547,
1.),(1.,0.707106781186547,1.,0.707106781186547,1.,0.707106781186547,1.,
0.707106781186547,1.),(1.,0.707106781186548,1.,0.707106781186548,1.,0.707106781186548,
1.,0.707106781186548,1.),(1.,0.707106781186547,1.,0.707106781186547,1.,
0.707106781186547,1.,0.707106781186547,1.),(1.,0.707106781186547,1.,0.707106781186547,
1.,0.707106781186547,1.,0.707106781186547,1.),(1.,0.707106781186547,1.,
0.707106781186547,1.,0.707106781186547,1.,0.707106781186547,1.),(1.,0.707106781186547,
1.,0.707106781186547,1.,0.707106781186547,1.,0.707106781186547,1.),(1.,
0.707106781186547,1.,0.707106781186547,1.,0.707106781186547,1.,0.707106781186547,
1.),(1.,0.707106781186547,1.,0.707106781186547,1.,0.707106781186547,1.,
0.707106781186547,1.),(1.,0.707106781186548,1.,0.707106781186548,1.,0.707106781186548,
1.,0.707106781186548,1.),(1.,0.707106781186547,1.,0.707106781186547,1.,
0.707106781186547,1.,0.707106781186547,1.),(1.,0.707106781186548,1.,0.707106781186548,
1.,0.707106781186548,1.,0.707106781186548,1.),(1.,0.707106781186548,1.,
0.707106781186548,1.,0.707106781186548,1.,0.707106781186548,1.),(1.,0.707106781186548,
1.,0.707106781186548,1.,0.707106781186548,1.,0.707106781186548,1.),(1.,
0.707106781186547,1.,0.707106781186547,1.,0.707106781186547,1.,0.707106781186547,
1.),(1.,0.707106781186547,1.,0.707106781186547,1.,0.707106781186547,1.,
0.707106781186547,1.),(1.,0.707106781186547,1.,0.707106781186547,1.,0.707106781186547,
1.,0.707106781186547,1.),(1.,0.707106781186548,1.,0.707106781186548,1.,
0.707106781186548,1.,0.707106781186548,1.),(1.,0.707106781186547,1.,0.707106781186547,
1.,0.707106781186547,1.,0.707106781186547,1.),(1.,0.707106781186548,1.,
0.707106781186548,1.,0.707106781186548,1.,0.707106781186548,1.),(1.,0.707106781186547,
1.,0.707106781186547,1.,0.707106781186547,1.,0.707106781186547,1.),(1.,
0.707106781186547,1.,0.707106781186547,1.,0.707106781186547,1.,0.707106781186547,
1.),(1.,0.707106781186548,1.,0.707106781186548,1.,0.707106781186548,1.,
0.707106781186548,1.),(1.,0.707106781186547,1.,0.707106781186547,1.,0.707106781186547,
1.,0.707106781186547,1.),(1.,0.707106781186547,1.,0.707106781186547,1.,
0.707106781186547,1.,0.707106781186547,1.),(1.,0.707106781186547,1.,0.707106781186547,
1.,0.707106781186547,1.,0.707106781186547,1.),(1.,0.707106781186547,1.,
0.707106781186547,1.,0.707106781186547,1.,0.707106781186547,1.),(1.,0.707106781186547,
1.,0.707106781186547,1.,0.707106781186547,1.,0.707106781186547,1.),(1.,
0.707106781186548,1.,0.707106781186548,1.,0.707106781186548,1.,0.707106781186548,
1.),(1.,0.707106781186547,1.,0.707106781186547,1.,0.707106781186547,1.,
0.707106781186547,1.),(1.,0.707106781186548,1.,0.707106781186548,1.,0.707106781186548,
1.,0.707106781186548,1.),(1.,0.707106781186547,1.,0.707106781186547,1.,
0.707106781186547,1.,0.707106781186547,1.),(1.,0.707106781186547,1.,0.707106781186547,
1.,0.707106781186547,1.,0.707106781186547,1.),(1.,0.707106781186548,1.,
0.707106781186548,1.,0.707106781186548,1.,0.707106781186548,1.),(1.,0.707106781186548,
1.,0.707106781186548,1.,0.707106781186548,1.,0.707106781186548,1.),(1.,
0.707106781186547,1.,0.707106781186547,1.,0.707106781186547,1.,0.707106781186547,
1.),(1.,0.707106781186547,1.,0.707106781186547,1.,0.707106781186547,1.,
0.707106781186547,1.),(1.,0.707106781186547,1.,0.707106781186547,1.,0.707106781186547,
1.,0.707106781186547,1.),(1.,0.707106781186548,1.,0.707106781186548,1.,
0.707106781186548,1.,0.707106781186548,1.),(1.,0.707106781186547,1.,0.707106781186547,
1.,0.707106781186547,1.,0.707106781186547,1.),(1.,0.707106781186547,1.,
0.707106781186547,1.,0.707106781186547,1.,0.707106781186547,1.),(1.,0.707106781186548,
1.,0.707106781186548,1.,0.707106781186548,1.,0.707106781186548,1.),(1.,
0.707106781186548,1.,0.707106781186548,1.,0.707106781186548,1.,0.707106781186548,
1.),(1.,0.707106781186547,1.,0.707106781186547,1.,0.707106781186547,1.,
0.707106781186547,1.),(1.,0.707106781186548,1.,0.707106781186548,1.,0.707106781186548,
1.,0.707106781186548,1.),(1.,0.707106781186547,1.,0.707106781186547,1.,
0.707106781186547,1.,0.707106781186547,1.),(1.,0.707106781186548,1.,0.707106781186548,
1.,0.707106781186548,1.,0.707106781186548,1.),(1.,0.707106781186548,1.,
0.707106781186548,1.,0.707106781186548,1.,0.707106781186548,1.),(1.,0.707106781186547,
1.,0.707106781186547,1.,0.707106781186547,1.,0.707106781186547,1.),(1.,
0.707106781186547,1.,0.707106781186547,1.,0.707106781186547,1.,0.707106781186547,
1.),(1.,0.707106781186547,1.,0.707106781186547,1.,0.707106781186547,1.,
0.707106781186547,1.),(1.,0.707106781186548,1.,0.707106781186548,1.,0.707106781186548,
1.,0.707106781186548,1.),(1.,0.707106781186548,1.,0.707106781186548,1.,
0.707106781186548,1.,0.707106781186548,1.),(1.,0.707106781186547,1.,0.707106781186547,
1.,0.707106781186547,1.,0.707106781186547,1.),(1.,0.707106781186548,1.,
0.707106781186548,1.,0.707106781186548,1.,0.707106781186548,1.),(1.,0.707106781186547,
1.,0.707106781186547,1.,0.707106781186547,1.,0.707106781186547,1.),(1.,
0.707106781186548,1.,0.707106781186548,1.,0.707106781186548,1.,0.707106781186548,
1.),(1.,0.707106781186548,1.,0.707106781186548,1.,0.707106781186548,1.,
0.707106781186548,1.),(1.,0.707106781186547,1.,0.707106781186547,1.,0.707106781186547,
1.,0.707106781186547,1.),(1.,0.707106781186548,1.,0.707106781186548,1.,
0.707106781186548,1.,0.707106781186548,1.),(1.,0.707106781186547,1.,0.707106781186547,
1.,0.707106781186547,1.,0.707106781186547,1.),(1.,0.707106781186547,1.,
0.707106781186547,1.,0.707106781186547,1.,0.707106781186547,1.),(1.,0.707106781186547,
1.,0.707106781186547,1.,0.707106781186547,1.,0.707106781186547,1.),(1.,
0.707106781186548,1.,0.707106781186548,1.,0.707106781186548,1.,0.707106781186548,
1.),(1.,0.707106781186547,1.,0.707106781186547,1.,0.707106781186547,1.,
0.707106781186547,1.),(1.,0.707106781186548,1.,0.707106781186548,1.,0.707106781186548,
1.,0.707106781186548,1.),(1.,0.707106781186547,1.,0.707106781186547,1.,
0.707106781186547,1.,0.707106781186547,1.),(1.,0.707106781186548,1.,0.707106781186548,
1.,0.707106781186548,1.,0.707106781186548,1.),(1.,0.707106781186547,1.,
0.707106781186547,1.,0.707106781186547,1.,0.707106781186547,1.),(1.,0.707106781186547,
1.,0.707106781186547,1.,0.707106781186547,1.,0.707106781186547,1.),(1.,
0.707106781186547,1.,0.707106781186547,1.,0.707106781186547,1.,0.707106781186547,
1.),(1.,0.707106781186547,1.,0.707106781186547,1.,0.707106781186547,1.,
0.707106781186547,1.),(1.,0.707106781186547,1.,0.707106781186547,1.,0.707106781186547,
1.,0.707106781186547,1.),(1.,0.707106781186548,1.,0.707106781186548,1.,
0.707106781186548,1.,0.707106781186548,1.),(1.,0.707106781186547,1.,0.707106781186547,
1.,0.707106781186547,1.,0.707106781186547,1.),(1.,0.707106781186548,1.,
0.707106781186548,1.,0.707106781186548,1.,0.707106781186548,1.),(1.,0.707106781186547,
1.,0.707106781186547,1.,0.707106781186547,1.,0.707106781186547,1.),(1.,
0.707106781186548,1.,0.707106781186548,1.,0.707106781186548,1.,0.707106781186548,
1.),(1.,0.707106781186547,1.,0.707106781186547,1.,0.707106781186547,1.,
0.707106781186547,1.),(1.,0.707106781186548,1.,0.707106781186548,1.,0.707106781186548,
1.,0.707106781186548,1.),(1.,0.707106781186547,1.,0.707106781186547,1.,
0.707106781186547,1.,0.707106781186547,1.),(1.,0.707106781186547,1.,0.707106781186547,
1.,0.707106781186547,1.,0.707106781186547,1.),(1.,0.707106781186547,1.,
0.707106781186547,1.,0.707106781186547,1.,0.707106781186547,1.),(1.,0.707106781186547,
1.,0.707106781186547,1.,0.707106781186547,1.,0.707106781186547,1.),(1.,
0.707106781186547,1.,0.707106781186547,1.,0.707106781186547,1.,0.707106781186547,
1.),(1.,0.707106781186548,1.,0.707106781186548,1.,0.707106781186548,1.,
0.707106781186548,1.),(1.,0.707106781186548,1.,0.707106781186548,1.,0.707106781186548,
1.,0.707106781186548,1.),(1.,0.707106781186548,1.,0.707106781186548,1.,
0.707106781186548,1.,0.707106781186548,1.),(1.,0.707106781186547,1.,0.707106781186547,
1.,0.707106781186547,1.,0.707106781186547,1.),(1.,0.707106781186548,1.,
0.707106781186548,1.,0.707106781186548,1.,0.707106781186548,1.),(1.,0.707106781186547,
1.,0.707106781186547,1.,0.707106781186547,1.,0.707106781186547,1.),(1.,
0.707106781186548,1.,0.707106781186548,1.,0.707106781186548,1.,0.707106781186548,
1.),(1.,0.707106781186547,1.,0.707106781186547,1.,0.707106781186547,1.,
0.707106781186547,1.),(1.,0.707106781186547,1.,0.707106781186547,1.,0.707106781186547,
1.,0.707106781186547,1.),(1.,0.707106781186548,1.,0.707106781186548,1.,
0.707106781186548,1.,0.707106781186548,1.),(1.,0.707106781186547,1.,0.707106781186547,
1.,0.707106781186547,1.,0.707106781186547,1.),(1.,0.707106781186548,1.,
0.707106781186548,1.,0.707106781186548,1.,0.707106781186548,1.),(1.,0.707106781186547,
1.,0.707106781186547,1.,0.707106781186547,1.,0.707106781186547,1.),(1.,
0.707106781186547,1.,0.707106781186547,1.,0.707106781186547,1.,0.707106781186547,
1.),(1.,0.707106781186547,1.,0.707106781186547,1.,0.707106781186547,1.,
0.707106781186547,1.),(1.,0.707106781186548,1.,0.707106781186548,1.,0.707106781186548,
1.,0.707106781186548,1.),(1.,0.707106781186548,1.,0.707106781186548,1.,
0.707106781186548,1.,0.707106781186548,1.),(1.,0.707106781186547,1.,0.707106781186547,
1.,0.707106781186547,1.,0.707106781186547,1.),(1.,0.707106781186548,1.,
0.707106781186548,1.,0.707106781186548,1.,0.707106781186548,1.),(1.,0.707106781186547,
1.,0.707106781186547,1.,0.707106781186547,1.,0.707106781186547,1.),(1.,
0.707106781186548,1.,0.707106781186548,1.,0.707106781186548,1.,0.707106781186548,
1.),(1.,0.707106781186548,1.,0.707106781186548,1.,0.707106781186548,1.,
0.707106781186548,1.),(1.,0.707106781186547,1.,0.707106781186547,1.,0.707106781186547,
1.,0.707106781186547,1.),(1.,0.707106781186548,1.,0.707106781186548,1.,
0.707106781186548,1.,0.707106781186548,1.),(1.,0.707106781186547,1.,0.707106781186547,
1.,0.707106781186547,1.,0.707106781186547,1.),(1.,0.707106781186548,1.,
0.707106781186548,1.,0.707106781186548,1.,0.707106781186548,1.),(1.,0.707106781186548,
1.,0.707106781186548,1.,0.707106781186548,1.,0.707106781186548,1.),(1.,
0.707106781186547,1.,0.707106781186547,1.,0.707106781186547,1.,0.707106781186547,
1.),(1.,0.707106781186547,1.,0.707106781186547,1.,0.707106781186547,1.,
0.707106781186547,1.),(1.,0.707106781186547,1.,0.707106781186547,1.,0.707106781186547,
1.,0.707106781186547,1.),(1.,0.707106781186547,1.,0.707106781186547,1.,
0.707106781186547,1.,0.707106781186547,1.),(1.,0.707106781186547,1.,0.707106781186547,
1.,0.707106781186547,1.,0.707106781186547,1.),(1.,0.707106781186547,1.,
0.707106781186547,1.,0.707106781186547,1.,0.707106781186547,1.),(1.,0.707106781186548,
1.,0.707106781186548,1.,0.707106781186548,1.,0.707106781186548,1.),(1.,
0.707106781186548,1.,0.707106781186548,1.,0.707106781186548,1.,0.707106781186548,
1.),(1.,0.707106781186547,1.,0.707106781186547,1.,0.707106781186547,1.,
0.707106781186547,1.),(1.,0.707106781186548,1.,0.707106781186548,1.,0.707106781186548,
1.,0.707106781186548,1.),(1.,0.707106781186547,1.,0.707106781186547,1.,
0.707106781186547,1.,0.707106781186547,1.),(1.,0.707106781186547,1.,0.707106781186547,
1.,0.707106781186547,1.,0.707106781186547,1.),(1.,0.707106781186548,1.,
0.707106781186548,1.,0.707106781186548,1.,0.707106781186548,1.),(1.,0.707106781186547,
1.,0.707106781186547,1.,0.707106781186547,1.,0.707106781186547,1.),(1.,
0.707106781186547,1.,0.707106781186547,1.,0.707106781186547,1.,0.707106781186547,
1.),(1.,0.707106781186548,1.,0.707106781186548,1.,0.707106781186548,1.,
0.707106781186548,1.),(1.,0.707106781186547,1.,0.707106781186547,1.,0.707106781186547,
1.,0.707106781186547,1.),(1.,0.707106781186547,1.,0.707106781186547,1.,
0.707106781186547,1.,0.707106781186547,1.),(1.,0.707106781186547,1.,0.707106781186547,
1.,0.707106781186547,1.,0.707106781186547,1.),(1.,0.707106781186548,1.,
0.707106781186548,1.,0.707106781186548,1.,0.707106781186548,1.),(1.,0.707106781186547,
1.,0.707106781186547,1.,0.707106781186547,1.,0.707106781186547,1.),(1.,
0.707106781186547,1.,0.707106781186547,1.,0.707106781186547,1.,0.707106781186547,
1.),(1.,0.707106781186548,1.,0.707106781186548,1.,0.707106781186548,1.,
0.707106781186548,1.),(1.,0.707106781186547,1.,0.707106781186547,1.,0.707106781186547,
1.,0.707106781186547,1.),(1.,0.707106781186548,1.,0.707106781186548,1.,
0.707106781186548,1.,0.707106781186548,1.),(1.,0.707106781186548,1.,0.707106781186548,
1.,0.707106781186548,1.,0.707106781186548,1.),(1.,0.707106781186547,1.,
0.707106781186547,1.,0.707106781186547,1.,0.707106781186547,1.),(1.,0.707106781186547,
1.,0.707106781186547,1.,0.707106781186547,1.,0.707106781186547,1.),(1.,
0.707106781186547,1.,0.707106781186547,1.,0.707106781186547,1.,0.707106781186547,
1.),(1.,0.707106781186548,1.,0.707106781186548,1.,0.707106781186548,1.,
0.707106781186548,1.),(1.,0.707106781186547,1.,0.707106781186547,1.,0.707106781186547,
1.,0.707106781186547,1.),(1.,0.707106781186547,1.,0.707106781186547,1.,
0.707106781186547,1.,0.707106781186547,1.),(1.,0.707106781186548,1.,0.707106781186548,
1.,0.707106781186548,1.,0.707106781186548,1.),(1.,0.707106781186548,1.,
0.707106781186548,1.,0.707106781186548,1.,0.707106781186548,1.),(1.,0.707106781186548,
1.,0.707106781186548,1.,0.707106781186548,1.,0.707106781186548,1.),(1.,
0.707106781186548,1.,0.707106781186548,1.,0.707106781186548,1.,0.707106781186548,
1.),(1.,0.707106781186547,1.,0.707106781186547,1.,0.707106781186547,1.,
0.707106781186547,1.),(1.,0.707106781186548,1.,0.707106781186548,1.,0.707106781186548,
1.,0.707106781186548,1.),(1.,0.707106781186548,1.,0.707106781186548,1.,
0.707106781186548,1.,0.707106781186548,1.),(1.,0.707106781186547,1.,0.707106781186547,
1.,0.707106781186547,1.,0.707106781186547,1.),(1.,0.707106781186547,1.,
0.707106781186547,1.,0.707106781186547,1.,0.707106781186547,1.),(1.,0.707106781186548,
1.,0.707106781186548,1.,0.707106781186548,1.,0.707106781186548,1.),(1.,
0.707106781186547,1.,0.707106781186547,1.,0.707106781186547,1.,0.707106781186547,
1.),(1.,0.707106781186548,1.,0.707106781186548,1.,0.707106781186548,1.,
0.707106781186548,1.),(1.,0.707106781186547,1.,0.707106781186547,1.,0.707106781186547,
1.,0.707106781186547,1.),(1.,0.707106781186547,1.,0.707106781186547,1.,
0.707106781186547,1.,0.707106781186547,1.),(1.,0.707106781186548,1.,0.707106781186548,
1.,0.707106781186548,1.,0.707106781186548,1.),(1.,0.707106781186547,1.,
0.707106781186547,1.,0.707106781186547,1.,0.707106781186547,1.),(1.,0.707106781186547,
1.,0.707106781186547,1.,0.707106781186547,1.,0.707106781186547,1.),(1.,
0.707106781186548,1.,0.707106781186548,1.,0.707106781186548,1.,0.707106781186548,
1.),(1.,0.707106781186547,1.,0.707106781186547,1.,0.707106781186547,1.,
0.707106781186547,1.),(1.,0.707106781186548,1.,0.707106781186548,1.,0.707106781186548,
1.,0.707106781186548,1.),(1.,0.707106781186547,1.,0.707106781186547,1.,
0.707106781186547,1.,0.707106781186547,1.),(1.,0.707106781186548,1.,0.707106781186548,
1.,0.707106781186548,1.,0.707106781186548,1.),(1.,0.707106781186547,1.,
0.707106781186547,1.,0.707106781186547,1.,0.707106781186547,1.),(1.,0.707106781186548,
1.,0.707106781186548,1.,0.707106781186548,1.,0.707106781186548,1.),(1.,
0.707106781186547,1.,0.707106781186547,1.,0.707106781186547,1.,0.707106781186547,
1.),(1.,0.707106781186548,1.,0.707106781186548,1.,0.707106781186548,1.,
0.707106781186548,1.),(1.,0.707106781186547,1.,0.707106781186547,1.,0.707106781186547,
1.,0.707106781186547,1.),(1.,0.707106781186548,1.,0.707106781186548,1.,
0.707106781186548,1.,0.707106781186548,1.),(1.,0.707106781186548,1.,0.707106781186548,
1.,0.707106781186548,1.,0.707106781186548,1.),(1.,0.707106781186547,1.,
0.707106781186547,1.,0.707106781186547,1.,0.707106781186547,1.),(1.,0.707106781186547,
1.,0.707106781186547,1.,0.707106781186547,1.,0.707106781186547,1.),(1.,
0.707106781186548,1.,0.707106781186548,1.,0.707106781186548,1.,0.707106781186548,
1.),(1.,0.707106781186548,1.,0.707106781186548,1.,0.707106781186548,1.,
0.707106781186548,1.),(1.,0.707106781186547,1.,0.707106781186547,1.,0.707106781186547,
1.,0.707106781186547,1.),(1.,0.707106781186547,1.,0.707106781186547,1.,
0.707106781186547,1.,0.707106781186547,1.),(1.,0.707106781186547,1.,0.707106781186547,
1.,0.707106781186547,1.,0.707106781186547,1.),(1.,0.707106781186547,1.,
0.707106781186547,1.,0.707106781186547,1.,0.707106781186547,1.),(1.,0.707106781186547,
1.,0.707106781186547,1.,0.707106781186547,1.,0.707106781186547,1.),(1.,
0.707106781186548,1.,0.707106781186548,1.,0.707106781186548,1.,0.707106781186548,
1.),(1.,0.707106781186547,1.,0.707106781186547,1.,0.707106781186547,1.,
0.707106781186547,1.),(1.,0.707106781186547,1.,0.707106781186547,1.,0.707106781186547,
1.,0.707106781186547,1.),(1.,0.707106781186548,1.,0.707106781186548,1.,
0.707106781186548,1.,0.707106781186548,1.),(1.,0.707106781186547,1.,0.707106781186547,
1.,0.707106781186547,1.,0.707106781186547,1.),(1.,0.707106781186548,1.,
0.707106781186548,1.,0.707106781186548,1.,0.707106781186548,1.),(1.,0.707106781186548,
1.,0.707106781186548,1.,0.707106781186548,1.,0.707106781186548,1.),(1.,
0.707106781186547,1.,0.707106781186547,1.,0.707106781186547,1.,0.707106781186547,
1.),(1.,0.707106781186548,1.,0.707106781186548,1.,0.707106781186548,1.,
0.707106781186548,1.),(1.,0.707106781186547,1.,0.707106781186547,1.,0.707106781186547,
1.,0.707106781186547,1.),(1.,0.707106781186548,1.,0.707106781186548,1.,
0.707106781186548,1.,0.707106781186548,1.),(1.,0.707106781186547,1.,0.707106781186547,
1.,0.707106781186547,1.,0.707106781186547,1.),(1.,0.707106781186548,1.,
0.707106781186548,1.,0.707106781186548,1.,0.707106781186548,1.),(1.,0.707106781186547,
1.,0.707106781186547,1.,0.707106781186547,1.,0.707106781186547,1.),(1.,
0.707106781186547,1.,0.707106781186547,1.,0.707106781186547,1.,0.707106781186547,
1.),(1.,0.707106781186547,1.,0.707106781186547,1.,0.707106781186547,1.,
0.707106781186547,1.),(1.,0.707106781186547,1.,0.707106781186547,1.,0.707106781186547,
1.,0.707106781186547,1.),(1.,0.707106781186547,1.,0.707106781186547,1.,
0.707106781186547,1.,0.707106781186547,1.),(1.,0.707106781186547,1.,0.707106781186547,
1.,0.707106781186547,1.,0.707106781186547,1.),(1.,0.707106781186548,1.,
0.707106781186548,1.,0.707106781186548,1.,0.707106781186548,1.),(1.,0.707106781186547,
1.,0.707106781186547,1.,0.707106781186547,1.,0.707106781186547,1.),(1.,
0.707106781186548,1.,0.707106781186548,1.,0.707106781186548,1.,0.707106781186548,
1.),(1.,0.707106781186547,1.,0.707106781186547,1.,0.707106781186547,1.,
0.707106781186547,1.),(1.,0.707106781186547,1.,0.707106781186547,1.,0.707106781186547,
1.,0.707106781186547,1.),(1.,0.707106781186547,1.,0.707106781186547,1.,
0.707106781186547,1.,0.707106781186547,1.),(1.,0.707106781186548,1.,0.707106781186548,
1.,0.707106781186548,1.,0.707106781186548,1.),(1.,0.707106781186547,1.,
0.707106781186547,1.,0.707106781186547,1.,0.707106781186547,1.),(1.,0.707106781186548,
1.,0.707106781186548,1.,0.707106781186548,1.,0.707106781186548,1.),(1.,
0.707106781186548,1.,0.707106781186548,1.,0.707106781186548,1.,0.707106781186548,
1.),(1.,0.707106781186547,1.,0.707106781186547,1.,0.707106781186547,1.,
0.707106781186547,1.),(1.,0.707106781186547,1.,0.707106781186547,1.,0.707106781186547,
1.,0.707106781186547,1.),(1.,0.707106781186548,1.,0.707106781186548,1.,
0.707106781186548,1.,0.707106781186548,1.),(1.,0.707106781186547,1.,0.707106781186547,
1.,0.707106781186547,1.,0.707106781186547,1.),(1.,0.707106781186548,1.,
0.707106781186548,1.,0.707106781186548,1.,0.707106781186548,1.),(1.,0.707106781186547,
1.,0.707106781186547,1.,0.707106781186547,1.,0.707106781186547,1.),(1.,
0.707106781186548,1.,0.707106781186548,1.,0.707106781186548,1.,0.707106781186548,
1.),(1.,0.707106781186547,1.,0.707106781186547,1.,0.707106781186547,1.,
0.707106781186547,1.),(1.,0.707106781186548,1.,0.707106781186548,1.,0.707106781186548,
1.,0.707106781186548,1.),(1.,0.707106781186547,1.,0.707106781186547,1.,
0.707106781186547,1.,0.707106781186547,1.),(1.,0.707106781186547,1.,0.707106781186547,
1.,0.707106781186547,1.,0.707106781186547,1.),(1.,0.707106781186548,1.,
0.707106781186548,1.,0.707106781186548,1.,0.707106781186548,1.),(1.,0.707106781186547,
1.,0.707106781186547,1.,0.707106781186547,1.,0.707106781186547,1.),(1.,
0.707106781186548,1.,0.707106781186548,1.,0.707106781186548,1.,0.707106781186548,
1.),(1.,0.707106781186547,1.,0.707106781186547,1.,0.707106781186547,1.,
0.707106781186547,1.),(1.,0.707106781186548,1.,0.707106781186548,1.,0.707106781186548,
1.,0.707106781186548,1.),(1.,0.707106781186548,1.,0.707106781186548,1.,
0.707106781186548,1.,0.707106781186548,1.),(1.,0.707106781186548,1.,0.707106781186548,
1.,0.707106781186548,1.,0.707106781186548,1.),(1.,0.707106781186548,1.,
0.707106781186548,1.,0.707106781186548,1.,0.707106781186548,1.),(1.,0.707106781186547,
1.,0.707106781186547,1.,0.707106781186547,1.,0.707106781186547,1.),(1.,
0.707106781186548,1.,0.707106781186548,1.,0.707106781186548,1.,0.707106781186548,
1.),(1.,0.707106781186548,1.,0.707106781186548,1.,0.707106781186548,1.,
0.707106781186548,1.),(1.,0.707106781186548,1.,0.707106781186548,1.,0.707106781186548,
1.,0.707106781186548,1.),(1.,0.707106781186547,1.,0.707106781186547,1.,
0.707106781186547,1.,0.707106781186547,1.),(1.,0.707106781186548,1.,0.707106781186548,
1.,0.707106781186548,1.,0.707106781186548,1.),(1.,0.707106781186548,1.,
0.707106781186548,1.,0.707106781186548,1.,0.707106781186548,1.),(1.,0.707106781186547,
1.,0.707106781186547,1.,0.707106781186547,1.,0.707106781186547,1.),(1.,
0.707106781186548,1.,0.707106781186548,1.,0.707106781186548,1.,0.707106781186548,
1.),(1.,0.707106781186547,1.,0.707106781186547,1.,0.707106781186547,1.,
0.707106781186547,1.),(1.,0.707106781186548,1.,0.707106781186548,1.,0.707106781186548,
1.,0.707106781186548,1.),(1.,0.707106781186547,1.,0.707106781186547,1.,
0.707106781186547,1.,0.707106781186547,1.),(1.,0.707106781186547,1.,0.707106781186547,
1.,0.707106781186547,1.,0.707106781186547,1.),(1.,0.707106781186547,1.,
0.707106781186547,1.,0.707106781186547,1.,0.707106781186547,1.),(1.,0.707106781186548,
1.,0.707106781186548,1.,0.707106781186548,1.,0.707106781186548,1.),(1.,
0.707106781186548,1.,0.707106781186548,1.,0.707106781186548,1.,0.707106781186548,
1.),(1.,0.707106781186547,1.,0.707106781186547,1.,0.707106781186547,1.,
0.707106781186547,1.),(1.,0.707106781186548,1.,0.707106781186548,1.,0.707106781186548,
1.,0.707106781186548,1.),(1.,0.707106781186547,1.,0.707106781186547,1.,
0.707106781186547,1.,0.707106781186547,1.),(1.,0.707106781186548,1.,0.707106781186548,
1.,0.707106781186548,1.,0.707106781186548,1.),(1.,0.707106781186547,1.,
0.707106781186547,1.,0.707106781186547,1.,0.707106781186547,1.),(1.,0.707106781186548,
1.,0.707106781186548,1.,0.707106781186548,1.,0.707106781186548,1.),(1.,
0.707106781186548,1.,0.707106781186548,1.,0.707106781186548,1.,0.707106781186548,
1.),(1.,0.707106781186547,1.,0.707106781186547,1.,0.707106781186547,1.,
0.707106781186547,1.),(1.,0.707106781186548,1.,0.707106781186548,1.,0.707106781186548,
1.,0.707106781186548,1.),(1.,0.707106781186547,1.,0.707106781186547,1.,
0.707106781186547,1.,0.707106781186547,1.),(1.,0.707106781186547,1.,0.707106781186547,
1.,0.707106781186547,1.,0.707106781186547,1.),(1.,0.707106781186548,1.,
0.707106781186548,1.,0.707106781186548,1.,0.707106781186548,1.),(1.,0.707106781186547,
1.,0.707106781186547,1.,0.707106781186547,1.,0.707106781186547,1.),(1.,
0.707106781186547,1.,0.707106781186547,1.,0.707106781186547,1.,0.707106781186547,
1.),(1.,0.707106781186547,1.,0.707106781186547,1.,0.707106781186547,1.,
0.707106781186547,1.),(1.,0.707106781186548,1.,0.707106781186548,1.,0.707106781186548,
1.,0.707106781186548,1.),(1.,0.707106781186547,1.,0.707106781186547,1.,
0.707106781186547,1.,0.707106781186547,1.),(1.,0.707106781186548,1.,0.707106781186548,
1.,0.707106781186548,1.,0.707106781186548,1.),(1.,0.707106781186548,1.,
0.707106781186548,1.,0.707106781186548,1.,0.707106781186548,1.),(1.,0.707106781186547,
1.,0.707106781186547,1.,0.707106781186547,1.,0.707106781186547,1.),(1.,
0.707106781186548,1.,0.707106781186548,1.,0.707106781186548,1.,0.707106781186548,
1.),(1.,0.707106781186547,1.,0.707106781186547,1.,0.707106781186547,1.,
0.707106781186547,1.),(1.,0.707106781186548,1.,0.707106781186548,1.,0.707106781186548,
1.,0.707106781186548,1.),(1.,0.707106781186548,1.,0.707106781186548,1.,
0.707106781186548,1.,0.707106781186548,1.),(1.,0.707106781186548,1.,0.707106781186548,
1.,0.707106781186548,1.,0.707106781186548,1.),(1.,0.707106781186548,1.,
0.707106781186548,1.,0.707106781186548,1.,0.707106781186548,1.),(1.,0.707106781186547,
1.,0.707106781186547,1.,0.707106781186547,1.,0.707106781186547,1.),(1.,
0.707106781186548,1.,0.707106781186548,1.,0.707106781186548,1.,0.707106781186548,
1.),(1.,0.707106781186547,1.,0.707106781186547,1.,0.707106781186547,1.,
0.707106781186547,1.),(1.,0.707106781186548,1.,0.707106781186548,1.,0.707106781186548,
1.,0.707106781186548,1.),(1.,0.707106781186547,1.,0.707106781186547,1.,
0.707106781186547,1.,0.707106781186547,1.),(1.,0.707106781186548,1.,0.707106781186548,
1.,0.707106781186548,1.,0.707106781186548,1.),(1.,0.707106781186547,1.,
0.707106781186547,1.,0.707106781186547,1.,0.707106781186547,1.),(1.,0.707106781186547,
1.,0.707106781186547,1.,0.707106781186547,1.,0.707106781186547,1.),(1.,
0.707106781186547,1.,0.707106781186547,1.,0.707106781186547,1.,0.707106781186547,
1.),(1.,0.707106781186547,1.,0.707106781186547,1.,0.707106781186547,1.,
0.707106781186547,1.),(1.,0.707106781186548,1.,0.707106781186548,1.,0.707106781186548,
1.,0.707106781186548,1.),(1.,0.707106781186547,1.,0.707106781186547,1.,
0.707106781186547,1.,0.707106781186547,1.),(1.,0.707106781186548,1.,0.707106781186548,
1.,0.707106781186548,1.,0.707106781186548,1.),(1.,0.707106781186547,1.,
0.707106781186547,1.,0.707106781186547,1.,0.707106781186547,1.),(1.,0.707106781186547,
1.,0.707106781186547,1.,0.707106781186547,1.,0.707106781186547,1.),(1.,
0.707106781186548,1.,0.707106781186548,1.,0.707106781186548,1.,0.707106781186548,
1.),(1.,0.707106781186547,1.,0.707106781186547,1.,0.707106781186547,1.,
0.707106781186547,1.),(1.,0.707106781186548,1.,0.707106781186548,1.,0.707106781186548,
1.,0.707106781186548,1.),(1.,0.707106781186547,1.,0.707106781186547,1.,
0.707106781186547,1.,0.707106781186547,1.),(1.,0.707106781186548,1.,0.707106781186548,
1.,0.707106781186548,1.,0.707106781186548,1.),(1.,0.707106781186547,1.,
0.707106781186547,1.,0.707106781186547,1.,0.707106781186547,1.),(1.,0.707106781186548,
1.,0.707106781186548,1.,0.707106781186548,1.,0.707106781186548,1.),(1.,
0.707106781186548,1.,0.707106781186548,1.,0.707106781186548,1.,0.707106781186548,
1.),(1.,0.707106781186548,1.,0.707106781186548,1.,0.707106781186548,1.,
0.707106781186548,1.),(1.,0.707106781186548,1.,0.707106781186548,1.,0.707106781186548,
1.,0.707106781186548,1.),(1.,0.707106781186547,1.,0.707106781186547,1.,
0.707106781186547,1.,0.707106781186547,1.),(1.,0.707106781186548,1.,0.707106781186548,
1.,0.707106781186548,1.,0.707106781186548,1.),(1.,0.707106781186548,1.,
0.707106781186548,1.,0.707106781186548,1.,0.707106781186548,1.),(1.,0.707106781186547,
1.,0.707106781186547,1.,0.707106781186547,1.,0.707106781186547,1.),(1.,
0.707106781186548,1.,0.707106781186548,1.,0.707106781186548,1.,0.707106781186548,
1.),(1.,0.707106781186547,1.,0.707106781186547,1.,0.707106781186547,1.,
0.707106781186547,1.),(1.,0.707106781186548,1.,0.707106781186548,1.,0.707106781186548,
1.,0.707106781186548,1.),(1.,0.707106781186547,1.,0.707106781186547,1.,
0.707106781186547,1.,0.707106781186547,1.),(1.,0.707106781186548,1.,0.707106781186548,
1.,0.707106781186548,1.,0.707106781186548,1.),(1.,0.707106781186547,1.,
0.707106781186547,1.,0.707106781186547,1.,0.707106781186547,1.),(1.,0.707106781186547,
1.,0.707106781186547,1.,0.707106781186547,1.,0.707106781186547,1.),(1.,
0.707106781186548,1.,0.707106781186548,1.,0.707106781186548,1.,0.707106781186548,
1.),(1.,0.707106781186547,1.,0.707106781186547,1.,0.707106781186547,1.,
0.707106781186547,1.),(1.,0.707106781186548,1.,0.707106781186548,1.,0.707106781186548,
1.,0.707106781186548,1.),(1.,0.707106781186547,1.,0.707106781186547,1.,
0.707106781186547,1.,0.707106781186547,1.),(1.,0.707106781186547,1.,0.707106781186547,
1.,0.707106781186547,1.,0.707106781186547,1.),(1.,0.707106781186548,1.,
0.707106781186548,1.,0.707106781186548,1.,0.707106781186548,1.),(1.,0.707106781186547,
1.,0.707106781186547,1.,0.707106781186547,1.,0.707106781186547,1.),(1.,
0.707106781186548,1.,0.707106781186548,1.,0.707106781186548,1.,0.707106781186548,
1.),(1.,0.707106781186547,1.,0.707106781186547,1.,0.707106781186547,1.,
0.707106781186547,1.),(1.,0.707106781186547,1.,0.707106781186547,1.,0.707106781186547,
1.,0.707106781186547,1.),(1.,0.707106781186548,1.,0.707106781186548,1.,
0.707106781186548,1.,0.707106781186548,1.),(1.,0.707106781186548,1.,0.707106781186548,
1.,0.707106781186548,1.,0.707106781186548,1.),(1.,0.707106781186548,1.,
0.707106781186548,1.,0.707106781186548,1.,0.707106781186548,1.),(1.,0.707106781186548,
1.,0.707106781186548,1.,0.707106781186548,1.,0.707106781186548,1.),(1.,
0.707106781186548,1.,0.707106781186548,1.,0.707106781186548,1.,0.707106781186548,
1.),(1.,0.707106781186548,1.,0.707106781186548,1.,0.707106781186548,1.,
0.707106781186548,1.),(1.,0.707106781186548,1.,0.707106781186548,1.,0.707106781186548,
1.,0.707106781186548,1.),(1.,0.707106781186548,1.,0.707106781186548,1.,
0.707106781186548,1.,0.707106781186548,1.),(1.,0.707106781186548,1.,0.707106781186548,
1.,0.707106781186548,1.,0.707106781186548,1.),(1.,0.707106781186547,1.,
0.707106781186547,1.,0.707106781186547,1.,0.707106781186547,1.),(1.,0.707106781186548,
1.,0.707106781186548,1.,0.707106781186548,1.,0.707106781186548,1.),(1.,
0.707106781186547,1.,0.707106781186547,1.,0.707106781186547,1.,0.707106781186547,
1.),(1.,0.707106781186547,1.,0.707106781186547,1.,0.707106781186547,1.,
0.707106781186547,1.),(1.,0.707106781186548,1.,0.707106781186548,1.,0.707106781186548,
1.,0.707106781186548,1.),(1.,0.707106781186547,1.,0.707106781186547,1.,
0.707106781186547,1.,0.707106781186547,1.),(1.,0.707106781186548,1.,0.707106781186548,
1.,0.707106781186548,1.,0.707106781186548,1.),(1.,0.707106781186548,1.,
0.707106781186548,1.,0.707106781186548,1.,0.707106781186548,1.),(1.,0.707106781186547,
1.,0.707106781186547,1.,0.707106781186547,1.,0.707106781186547,1.),(1.,
0.707106781186547,1.,0.707106781186547,1.,0.707106781186547,1.,0.707106781186547,
1.),(1.,0.707106781186548,1.,0.707106781186548,1.,0.707106781186548,1.,
0.707106781186548,1.),(1.,0.707106781186548,1.,0.707106781186548,1.,0.707106781186548,
1.,0.707106781186548,1.),(1.,0.707106781186547,1.,0.707106781186547,1.,
0.707106781186547,1.,0.707106781186547,1.),(1.,0.707106781186547,1.,0.707106781186547,
1.,0.707106781186547,1.,0.707106781186547,1.),(1.,0.707106781186547,1.,
0.707106781186547,1.,0.707106781186547,1.,0.707106781186547,1.),(1.,0.707106781186547,
1.,0.707106781186547,1.,0.707106781186547,1.,0.707106781186547,1.),(1.,
0.707106781186547,1.,0.707106781186547,1.,0.707106781186547,1.,0.707106781186547,
1.),(1.,0.707106781186548,1.,0.707106781186548,1.,0.707106781186548,1.,
0.707106781186548,1.),(1.,0.707106781186547,1.,0.707106781186547,1.,0.707106781186547,
1.,0.707106781186547,1.),(1.,0.707106781186548,1.,0.707106781186548,1.,
0.707106781186548,1.,0.707106781186548,1.),(1.,0.707106781186548,1.,0.707106781186548,
1.,0.707106781186548,1.,0.707106781186548,1.),(1.,0.707106781186548,1.,
0.707106781186548,1.,0.707106781186548,1.,0.707106781186548,1.),(1.,0.707106781186547,
1.,0.707106781186547,1.,0.707106781186547,1.,0.707106781186547,1.),(1.,
0.707106781186548,1.,0.707106781186548,1.,0.707106781186548,1.,0.707106781186548,
1.),(1.,0.707106781186547,1.,0.707106781186547,1.,0.707106781186547,1.,
0.707106781186547,1.),(1.,0.707106781186548,1.,0.707106781186548,1.,0.707106781186548,
1.,0.707106781186548,1.),(1.,0.707106781186547,1.,0.707106781186547,1.,
0.707106781186547,1.,0.707106781186547,1.),(1.,0.707106781186548,1.,0.707106781186548,
1.,0.707106781186548,1.,0.707106781186548,1.),(1.,0.707106781186547,1.,
0.707106781186547,1.,0.707106781186547,1.,0.707106781186547,1.),(1.,0.707106781186548,
1.,0.707106781186548,1.,0.707106781186548,1.,0.707106781186548,1.),(1.,
0.707106781186548,1.,0.707106781186548,1.,0.707106781186548,1.,0.707106781186548,
1.),(1.,0.707106781186547,1.,0.707106781186547,1.,0.707106781186547,1.,
0.707106781186547,1.),(1.,0.707106781186547,1.,0.707106781186547,1.,0.707106781186547,
1.,0.707106781186547,1.),(1.,0.707106781186548,1.,0.707106781186548,1.,
0.707106781186548,1.,0.707106781186548,1.),(1.,0.707106781186548,1.,0.707106781186548,
1.,0.707106781186548,1.,0.707106781186548,1.),(1.,0.707106781186548,1.,
0.707106781186548,1.,0.707106781186548,1.,0.707106781186548,1.),(1.,0.707106781186547,
1.,0.707106781186547,1.,0.707106781186547,1.,0.707106781186547,1.),(1.,
0.707106781186547,1.,0.707106781186547,1.,0.707106781186547,1.,0.707106781186547,
1.),(1.,0.707106781186548,1.,0.707106781186548,1.,0.707106781186548,1.,
0.707106781186548,1.),(1.,0.707106781186547,1.,0.707106781186547,1.,0.707106781186547,
1.,0.707106781186547,1.),(1.,0.707106781186547,1.,0.707106781186547,1.,
0.707106781186547,1.,0.707106781186547,1.),(1.,0.707106781186548,1.,0.707106781186548,
1.,0.707106781186548,1.,0.707106781186548,1.),(1.,0.707106781186547,1.,
0.707106781186547,1.,0.707106781186547,1.,0.707106781186547,1.),(1.,0.707106781186548,
1.,0.707106781186548,1.,0.707106781186548,1.,0.707106781186548,1.),(1.,
0.707106781186547,1.,0.707106781186547,1.,0.707106781186547,1.,0.707106781186547,
1.),(1.,0.707106781186547,1.,0.707106781186547,1.,0.707106781186547,1.,
0.707106781186547,1.),(1.,0.707106781186548,1.,0.707106781186548,1.,0.707106781186548,
1.,0.707106781186548,1.),(1.,0.707106781186548,1.,0.707106781186548,1.,
0.707106781186548,1.,0.707106781186548,1.),(1.,0.707106781186548,1.,0.707106781186548,
1.,0.707106781186548,1.,0.707106781186548,1.),(1.,0.707106781186547,1.,
0.707106781186547,1.,0.707106781186547,1.,0.707106781186547,1.),(1.,0.707106781186547,
1.,0.707106781186547,1.,0.707106781186547,1.,0.707106781186547,1.),(1.,
0.707106781186548,1.,0.707106781186548,1.,0.707106781186548,1.,0.707106781186548,
1.),(1.,0.707106781186547,1.,0.707106781186547,1.,0.707106781186547,1.,
0.707106781186547,1.),(1.,0.707106781186548,1.,0.707106781186548,1.,0.707106781186548,
1.,0.707106781186548,1.),(1.,0.707106781186547,1.,0.707106781186547,1.,
0.707106781186547,1.,0.707106781186547,1.),(1.,0.707106781186548,1.,0.707106781186548,
1.,0.707106781186548,1.,0.707106781186548,1.),(1.,0.707106781186547,1.,
0.707106781186547,1.,0.707106781186547,1.,0.707106781186547,1.),(1.,0.707106781186548,
1.,0.707106781186548,1.,0.707106781186548,1.,0.707106781186548,1.),(1.,
0.707106781186548,1.,0.707106781186548,1.,0.707106781186548,1.,0.707106781186548,
1.),(1.,0.707106781186547,1.,0.707106781186547,1.,0.707106781186547,1.,
0.707106781186547,1.),(1.,0.707106781186548,1.,0.707106781186548,1.,0.707106781186548,
1.,0.707106781186548,1.),(1.,0.707106781186547,1.,0.707106781186547,1.,
0.707106781186547,1.,0.707106781186547,1.),(1.,0.707106781186548,1.,0.707106781186548,
1.,0.707106781186548,1.,0.707106781186548,1.),(1.,0.707106781186547,1.,
0.707106781186547,1.,0.707106781186547,1.,0.707106781186547,1.),(1.,0.707106781186547,
1.,0.707106781186547,1.,0.707106781186547,1.,0.707106781186547,1.),(1.,
0.707106781186547,1.,0.707106781186547,1.,0.707106781186547,1.,0.707106781186547,
1.),(1.,0.707106781186548,1.,0.707106781186548,1.,0.707106781186548,1.,
0.707106781186548,1.),(1.,0.707106781186547,1.,0.707106781186547,1.,0.707106781186547,
1.,0.707106781186547,1.),(1.,0.707106781186548,1.,0.707106781186548,1.,
0.707106781186548,1.,0.707106781186548,1.),(1.,0.707106781186547,1.,0.707106781186547,
1.,0.707106781186547,1.,0.707106781186547,1.),(1.,0.707106781186547,1.,
0.707106781186547,1.,0.707106781186547,1.,0.707106781186547,1.),(1.,0.707106781186547,
1.,0.707106781186547,1.,0.707106781186547,1.,0.707106781186547,1.),(1.,
0.707106781186548,1.,0.707106781186548,1.,0.707106781186548,1.,0.707106781186548,
1.),(1.,0.707106781186547,1.,0.707106781186547,1.,0.707106781186547,1.,
0.707106781186547,1.),(1.,0.707106781186547,1.,0.707106781186547,1.,0.707106781186547,
1.,0.707106781186547,1.),(1.,0.707106781186548,1.,0.707106781186548,1.,
0.707106781186548,1.,0.707106781186548,1.),(1.,0.707106781186548,1.,0.707106781186548,
1.,0.707106781186548,1.,0.707106781186548,1.),(1.,0.707106781186547,1.,
0.707106781186547,1.,0.707106781186547,1.,0.707106781186547,1.),(1.,0.707106781186548,
1.,0.707106781186548,1.,0.707106781186548,1.,0.707106781186548,1.),(1.,
0.707106781186547,1.,0.707106781186547,1.,0.707106781186547,1.,0.707106781186547,
1.),(1.,0.707106781186548,1.,0.707106781186548,1.,0.707106781186548,1.,
0.707106781186548,1.),(1.,0.707106781186548,1.,0.707106781186548,1.,0.707106781186548,
1.,0.707106781186548,1.),(1.,0.707106781186547,1.,0.707106781186547,1.,
0.707106781186547,1.,0.707106781186547,1.),(1.,0.707106781186548,1.,0.707106781186548,
1.,0.707106781186548,1.,0.707106781186548,1.),(1.,0.707106781186547,1.,
0.707106781186547,1.,0.707106781186547,1.,0.707106781186547,1.),(1.,0.707106781186547,
1.,0.707106781186547,1.,0.707106781186547,1.,0.707106781186547,1.),(1.,
0.707106781186548,1.,0.707106781186548,1.,0.707106781186548,1.,0.707106781186548,
1.),(1.,0.707106781186547,1.,0.707106781186547,1.,0.707106781186547,1.,
0.707106781186547,1.),(1.,0.707106781186547,1.,0.707106781186547,1.,0.707106781186547,
1.,0.707106781186547,1.),(1.,0.707106781186547,1.,0.707106781186547,1.,
0.707106781186547,1.,0.707106781186547,1.),(1.,0.707106781186548,1.,0.707106781186548,
1.,0.707106781186548,1.,0.707106781186548,1.),(1.,0.707106781186547,1.,
0.707106781186547,1.,0.707106781186547,1.,0.707106781186547,1.),(1.,0.707106781186548,
1.,0.707106781186548,1.,0.707106781186548,1.,0.707106781186548,1.),(1.,
0.707106781186547,1.,0.707106781186547,1.,0.707106781186547,1.,0.707106781186547,
1.),(1.,0.707106781186548,1.,0.707106781186548,1.,0.707106781186548,1.,
0.707106781186548,1.),(1.,0.707106781186548,1.,0.707106781186548,1.,0.707106781186548,
1.,0.707106781186548,1.),(1.,0.707106781186548,1.,0.707106781186548,1.,
0.707106781186548,1.,0.707106781186548,1.),(1.,0.707106781186547,1.,0.707106781186547,
1.,0.707106781186547,1.,0.707106781186547,1.),(1.,0.707106781186548,1.,
0.707106781186548,1.,0.707106781186548,1.,0.707106781186548,1.),(1.,0.707106781186548,
1.,0.707106781186548,1.,0.707106781186548,1.,0.707106781186548,1.),(1.,
0.707106781186548,1.,0.707106781186548,1.,0.707106781186548,1.,0.707106781186548,
1.),(1.,0.707106781186547,1.,0.707106781186547,1.,0.707106781186547,1.,
0.707106781186547,1.),(1.,0.707106781186548,1.,0.707106781186548,1.,0.707106781186548,
1.,0.707106781186548,1.),(1.,0.707106781186547,1.,0.707106781186547,1.,
0.707106781186547,1.,0.707106781186547,1.),(1.,0.707106781186547,1.,0.707106781186547,
1.,0.707106781186547,1.,0.707106781186547,1.),(1.,0.707106781186548,1.,
0.707106781186548,1.,0.707106781186548,1.,0.707106781186548,1.),(1.,0.707106781186547,
1.,0.707106781186547,1.,0.707106781186547,1.,0.707106781186547,1.),(1.,
0.707106781186547,1.,0.707106781186547,1.,0.707106781186547,1.,0.707106781186547,
1.),(1.,0.707106781186548,1.,0.707106781186548,1.,0.707106781186548,1.,
0.707106781186548,1.),(1.,0.707106781186548,1.,0.707106781186548,1.,0.707106781186548,
1.,0.707106781186548,1.),(1.,0.707106781186547,1.,0.707106781186547,1.,
0.707106781186547,1.,0.707106781186547,1.),(1.,0.707106781186548,1.,0.707106781186548,
1.,0.707106781186548,1.,0.707106781186548,1.),(1.,0.707106781186547,1.,
0.707106781186547,1.,0.707106781186547,1.,0.707106781186547,1.),(1.,0.707106781186548,
1.,0.707106781186548,1.,0.707106781186548,1.,0.707106781186548,1.),(1.,
0.707106781186548,1.,0.707106781186548,1.,0.707106781186548,1.,0.707106781186548,
1.),(1.,0.707106781186547,1.,0.707106781186547,1.,0.707106781186547,1.,
0.707106781186547,1.),(1.,0.707106781186548,1.,0.707106781186548,1.,0.707106781186548,
1.,0.707106781186548,1.),(1.,0.707106781186547,1.,0.707106781186547,1.,
0.707106781186547,1.,0.707106781186547,1.),(1.,0.707106781186548,1.,0.707106781186548,
1.,0.707106781186548,1.,0.707106781186548,1.),(1.,0.707106781186547,1.,
0.707106781186547,1.,0.707106781186547,1.,0.707106781186547,1.),(1.,0.707106781186548,
1.,0.707106781186548,1.,0.707106781186548,1.,0.707106781186548,1.),(1.,
0.707106781186547,1.,0.707106781186547,1.,0.707106781186547,1.,0.707106781186547,
1.),(1.,0.707106781186548,1.,0.707106781186548,1.,0.707106781186548,1.,
0.707106781186548,1.),(1.,0.707106781186548,1.,0.707106781186548,1.,0.707106781186548,
1.,0.707106781186548,1.),(1.,0.707106781186548,1.,0.707106781186548,1.,
0.707106781186548,1.,0.707106781186548,1.),(1.,0.707106781186547,1.,0.707106781186547,
1.,0.707106781186547,1.,0.707106781186547,1.),(1.,0.707106781186548,1.,
0.707106781186548,1.,0.707106781186548,1.,0.707106781186548,1.),(1.,0.707106781186548,
1.,0.707106781186548,1.,0.707106781186548,1.,0.707106781186548,1.),(1.,
0.707106781186547,1.,0.707106781186547,1.,0.707106781186547,1.,0.707106781186547,
1.),(1.,0.707106781186547,1.,0.707106781186547,1.,0.707106781186547,1.,
0.707106781186547,1.),(1.,0.707106781186548,1.,0.707106781186548,1.,0.707106781186548,
1.,0.707106781186548,1.),(1.,0.707106781186547,1.,0.707106781186547,1.,
0.707106781186547,1.,0.707106781186547,1.),(1.,0.707106781186548,1.,0.707106781186548,
1.,0.707106781186548,1.,0.707106781186548,1.),(1.,0.707106781186548,1.,
0.707106781186548,1.,0.707106781186548,1.,0.707106781186548,1.),(1.,0.707106781186547,
1.,0.707106781186547,1.,0.707106781186547,1.,0.707106781186547,1.),(1.,
0.707106781186548,1.,0.707106781186548,1.,0.707106781186548,1.,0.707106781186548,
1.),(1.,0.707106781186548,1.,0.707106781186548,1.,0.707106781186548,1.,
0.707106781186548,1.),(1.,0.707106781186547,1.,0.707106781186547,1.,0.707106781186547,
1.,0.707106781186547,1.),(1.,0.707106781186548,1.,0.707106781186548,1.,
0.707106781186548,1.,0.707106781186548,1.),(1.,0.707106781186548,1.,0.707106781186548,
1.,0.707106781186548,1.,0.707106781186548,1.),(1.,0.707106781186547,1.,
0.707106781186547,1.,0.707106781186547,1.,0.707106781186547,1.),(1.,0.707106781186547,
1.,0.707106781186547,1.,0.707106781186547,1.,0.707106781186547,1.),(1.,
0.707106781186548,1.,0.707106781186548,1.,0.707106781186548,1.,0.707106781186548,
1.),(1.,0.707106781186547,1.,0.707106781186547,1.,0.707106781186547,1.,
0.707106781186547,1.),(1.,0.707106781186548,1.,0.707106781186548,1.,0.707106781186548,
1.,0.707106781186548,1.),(1.,0.707106781186547,1.,0.707106781186547,1.,
0.707106781186547,1.,0.707106781186547,1.),(1.,0.707106781186548,1.,0.707106781186548,
1.,0.707106781186548,1.,0.707106781186548,1.),(1.,0.707106781186547,1.,
0.707106781186547,1.,0.707106781186547,1.,0.707106781186547,1.),(1.,0.707106781186548,
1.,0.707106781186548,1.,0.707106781186548,1.,0.707106781186548,1.),(1.,
0.707106781186548,1.,0.707106781186548,1.,0.707106781186548,1.,0.707106781186548,
1.),(1.,0.707106781186548,1.,0.707106781186548,1.,0.707106781186548,1.,
0.707106781186548,1.),(1.,0.707106781186547,1.,0.707106781186547,1.,0.707106781186547,
1.,0.707106781186547,1.),(1.,0.707106781186548,1.,0.707106781186548,1.,
0.707106781186548,1.,0.707106781186548,1.),(1.,0.707106781186547,1.,0.707106781186547,
1.,0.707106781186547,1.,0.707106781186547,1.),(1.,0.707106781186548,1.,
0.707106781186548,1.,0.707106781186548,1.,0.707106781186548,1.),(1.,0.707106781186547,
1.,0.707106781186547,1.,0.707106781186547,1.,0.707106781186547,1.),(1.,
0.707106781186548,1.,0.707106781186548,1.,0.707106781186548,1.,0.707106781186548,
1.),(1.,0.707106781186547,1.,0.707106781186547,1.,0.707106781186547,1.,
0.707106781186547,1.),(1.,0.707106781186548,1.,0.707106781186548,1.,0.707106781186548,
1.,0.707106781186548,1.),(1.,0.707106781186547,1.,0.707106781186547,1.,
0.707106781186547,1.,0.707106781186547,1.),(1.,0.707106781186548,1.,0.707106781186548,
1.,0.707106781186548,1.,0.707106781186548,1.),(1.,0.707106781186547,1.,
0.707106781186547,1.,0.707106781186547,1.,0.707106781186547,1.),(1.,0.707106781186548,
1.,0.707106781186548,1.,0.707106781186548,1.,0.707106781186548,1.),(1.,
0.707106781186547,1.,0.707106781186547,1.,0.707106781186547,1.,0.707106781186547,
1.),(1.,0.707106781186547,1.,0.707106781186547,1.,0.707106781186547,1.,
0.707106781186547,1.),(1.,0.707106781186547,1.,0.707106781186547,1.,0.707106781186547,
1.,0.707106781186547,1.),(1.,0.707106781186548,1.,0.707106781186548,1.,
0.707106781186548,1.,0.707106781186548,1.),(1.,0.707106781186547,1.,0.707106781186547,
1.,0.707106781186547,1.,0.707106781186547,1.),(1.,0.707106781186548,1.,
0.707106781186548,1.,0.707106781186548,1.,0.707106781186548,1.),(1.,0.707106781186547,
1.,0.707106781186547,1.,0.707106781186547,1.,0.707106781186547,1.),(1.,
0.707106781186548,1.,0.707106781186548,1.,0.707106781186548,1.,0.707106781186548,
1.),(1.,0.707106781186547,1.,0.707106781186547,1.,0.707106781186547,1.,
0.707106781186547,1.),(1.,0.707106781186548,1.,0.707106781186548,1.,0.707106781186548,
1.,0.707106781186548,1.),(1.,0.707106781186547,1.,0.707106781186547,1.,
0.707106781186547,1.,0.707106781186547,1.),(1.,0.707106781186548,1.,0.707106781186548,
1.,0.707106781186548,1.,0.707106781186548,1.),(1.,0.707106781186548,1.,
0.707106781186548,1.,0.707106781186548,1.,0.707106781186548,1.),(1.,0.707106781186548,
1.,0.707106781186548,1.,0.707106781186548,1.,0.707106781186548,1.),(1.,
0.707106781186547,1.,0.707106781186547,1.,0.707106781186547,1.,0.707106781186547,
1.),(1.,0.707106781186548,1.,0.707106781186548,1.,0.707106781186548,1.,
0.707106781186548,1.),(1.,0.707106781186547,1.,0.707106781186547,1.,0.707106781186547,
1.,0.707106781186547,1.),(1.,0.707106781186548,1.,0.707106781186548,1.,
0.707106781186548,1.,0.707106781186548,1.),(1.,0.707106781186548,1.,0.707106781186548,
1.,0.707106781186548,1.,0.707106781186548,1.),(1.,0.707106781186547,1.,
0.707106781186547,1.,0.707106781186547,1.,0.707106781186547,1.),(1.,0.707106781186548,
1.,0.707106781186548,1.,0.707106781186548,1.,0.707106781186548,1.),(1.,
0.707106781186547,1.,0.707106781186547,1.,0.707106781186547,1.,0.707106781186547,
1.),(1.,0.707106781186548,1.,0.707106781186548,1.,0.707106781186548,1.,
0.707106781186548,1.),(1.,0.707106781186547,1.,0.707106781186547,1.,0.707106781186547,
1.,0.707106781186547,1.),(1.,0.707106781186548,1.,0.707106781186548,1.,
0.707106781186548,1.,0.707106781186548,1.),(1.,0.707106781186547,1.,0.707106781186547,
1.,0.707106781186547,1.,0.707106781186547,1.),(1.,0.707106781186548,1.,
0.707106781186548,1.,0.707106781186548,1.,0.707106781186548,1.),(1.,0.707106781186547,
1.,0.707106781186547,1.,0.707106781186547,1.,0.707106781186547,1.),(1.,
0.707106781186547,1.,0.707106781186547,1.,0.707106781186547,1.,0.707106781186547,
1.),(1.,0.707106781186547,1.,0.707106781186547,1.,0.707106781186547,1.,
0.707106781186547,1.),(1.,0.707106781186548,1.,0.707106781186548,1.,0.707106781186548,
1.,0.707106781186548,1.),(1.,0.707106781186547,1.,0.707106781186547,1.,
0.707106781186547,1.,0.707106781186547,1.),(1.,0.707106781186547,1.,0.707106781186547,
1.,0.707106781186547,1.,0.707106781186547,1.),(1.,0.707106781186548,1.,
0.707106781186548,1.,0.707106781186548,1.,0.707106781186548,1.),(1.,0.707106781186547,
1.,0.707106781186547,1.,0.707106781186547,1.,0.707106781186547,1.),(1.,
0.707106781186548,1.,0.707106781186548,1.,0.707106781186548,1.,0.707106781186548,
1.),(1.,0.707106781186547,1.,0.707106781186547,1.,0.707106781186547,1.,
0.707106781186547,1.),(1.,0.707106781186547,1.,0.707106781186547,1.,0.707106781186547,
1.,0.707106781186547,1.),(1.,0.707106781186548,1.,0.707106781186548,1.,
0.707106781186548,1.,0.707106781186548,1.),(1.,0.707106781186547,1.,0.707106781186547,
1.,0.707106781186547,1.,0.707106781186547,1.),(1.,0.707106781186548,1.,
0.707106781186548,1.,0.707106781186548,1.,0.707106781186548,1.),(1.,0.707106781186547,
1.,0.707106781186547,1.,0.707106781186547,1.,0.707106781186547,1.),(1.,
0.707106781186548,1.,0.707106781186548,1.,0.707106781186548,1.,0.707106781186548,
1.),(1.,0.707106781186548,1.,0.707106781186548,1.,0.707106781186548,1.,
0.707106781186548,1.),(1.,0.707106781186548,1.,0.707106781186548,1.,0.707106781186548,
1.,0.707106781186548,1.),(1.,0.707106781186547,1.,0.707106781186547,1.,
0.707106781186547,1.,0.707106781186547,1.),(1.,0.707106781186547,1.,0.707106781186547,
1.,0.707106781186547,1.,0.707106781186547,1.),(1.,0.707106781186548,1.,
0.707106781186548,1.,0.707106781186548,1.,0.707106781186548,1.),(1.,0.707106781186548,
1.,0.707106781186548,1.,0.707106781186548,1.,0.707106781186548,1.),(1.,
0.707106781186547,1.,0.707106781186547,1.,0.707106781186547,1.,0.707106781186547,
1.),(1.,0.707106781186548,1.,0.707106781186548,1.,0.707106781186548,1.,
0.707106781186548,1.),(1.,0.707106781186547,1.,0.707106781186547,1.,0.707106781186547,
1.,0.707106781186547,1.),(1.,0.707106781186547,1.,0.707106781186547,1.,
0.707106781186547,1.,0.707106781186547,1.),(1.,0.707106781186547,1.,0.707106781186547,
1.,0.707106781186547,1.,0.707106781186547,1.),(1.,0.707106781186548,1.,
0.707106781186548,1.,0.707106781186548,1.,0.707106781186548,1.),(1.,0.707106781186547,
1.,0.707106781186547,1.,0.707106781186547,1.,0.707106781186547,1.),(1.,
0.707106781186548,1.,0.707106781186548,1.,0.707106781186548,1.,0.707106781186548,
1.),(1.,0.707106781186547,1.,0.707106781186547,1.,0.707106781186547,1.,
0.707106781186547,1.),(1.,0.707106781186548,1.,0.707106781186548,1.,0.707106781186548,
1.,0.707106781186548,1.),(1.,0.707106781186548,1.,0.707106781186548,1.,
0.707106781186548,1.,0.707106781186548,1.),(1.,0.707106781186548,1.,0.707106781186548,
1.,0.707106781186548,1.,0.707106781186548,1.),(1.,0.707106781186547,1.,
0.707106781186547,1.,0.707106781186547,1.,0.707106781186547,1.),(1.,0.707106781186547,
1.,0.707106781186547,1.,0.707106781186547,1.,0.707106781186547,1.),(1.,
0.707106781186547,1.,0.707106781186547,1.,0.707106781186547,1.,0.707106781186547,
1.),(1.,0.707106781186547,1.,0.707106781186547,1.,0.707106781186547,1.,
0.707106781186547,1.),(1.,0.707106781186547,1.,0.707106781186547,1.,0.707106781186547,
1.,0.707106781186547,1.),(1.,0.707106781186547,1.,0.707106781186547,1.,
0.707106781186547,1.,0.707106781186547,1.),(1.,0.707106781186548,1.,0.707106781186548,
1.,0.707106781186548,1.,0.707106781186548,1.),(1.,0.707106781186547,1.,
0.707106781186547,1.,0.707106781186547,1.,0.707106781186547,1.),(1.,0.707106781186548,
1.,0.707106781186548,1.,0.707106781186548,1.,0.707106781186548,1.),(1.,
0.707106781186547,1.,0.707106781186547,1.,0.707106781186547,1.,0.707106781186547,
1.),(1.,0.707106781186548,1.,0.707106781186548,1.,0.707106781186548,1.,
0.707106781186548,1.),(1.,0.707106781186547,1.,0.707106781186547,1.,0.707106781186547,
1.,0.707106781186547,1.),(1.,0.707106781186547,1.,0.707106781186547,1.,
0.707106781186547,1.,0.707106781186547,1.),(1.,0.707106781186548,1.,0.707106781186548,
1.,0.707106781186548,1.,0.707106781186548,1.),(1.,0.707106781186547,1.,
0.707106781186547,1.,0.707106781186547,1.,0.707106781186547,1.),(1.,0.707106781186547,
1.,0.707106781186547,1.,0.707106781186547,1.,0.707106781186547,1.),(1.,
0.707106781186548,1.,0.707106781186548,1.,0.707106781186548,1.,0.707106781186548,
1.),(1.,0.707106781186548,1.,0.707106781186548,1.,0.707106781186548,1.,
0.707106781186548,1.),(1.,0.707106781186547,1.,0.707106781186547,1.,0.707106781186547,
1.,0.707106781186547,1.),(1.,0.707106781186547,1.,0.707106781186547,1.,
0.707106781186547,1.,0.707106781186547,1.),(1.,0.707106781186547,1.,0.707106781186547,
1.,0.707106781186547,1.,0.707106781186547,1.),(1.,0.707106781186548,1.,
0.707106781186548,1.,0.707106781186548,1.,0.707106781186548,1.),(1.,0.707106781186547,
1.,0.707106781186547,1.,0.707106781186547,1.,0.707106781186547,1.),(1.,
0.707106781186547,1.,0.707106781186547,1.,0.707106781186547,1.,0.707106781186547,
1.),(1.,0.707106781186548,1.,0.707106781186548,1.,0.707106781186548,1.,
0.707106781186548,1.),(1.,0.707106781186548,1.,0.707106781186548,1.,0.707106781186548,
1.,0.707106781186548,1.)))
REPRESENTATION_ITEM('')
SURFACE()
) ;
#62 = (
BOUNDED_SURFACE()
B_SPLINE_SURFACE(2,3,((#174417,#174418,#174419,#174420,#174421,#174422,
#174423),(#174424,#174425,#174426,#174427,#174428,#174429,#174430),(#174431,
#174432,#174433,#174434,#174435,#174436,#174437),(#174438,#174439,#174440,
#174441,#174442,#174443,#174444),(#174445,#174446,#174447,#174448,#174449,
#174450,#174451),(#174452,#174453,#174454,#174455,#174456,#174457,#174458),
(#174459,#174460,#174461,#174462,#174463,#174464,#174465),(#174466,#174467,
#174468,#174469,#174470,#174471,#174472),(#174473,#174474,#174475,#174476,
#174477,#174478,#174479)),.UNSPECIFIED.,.T.,.F.,.F.)
B_SPLINE_SURFACE_WITH_KNOTS((3,2,2,2,3),(4,1,1,1,4),(0.,0.117809724509617,
0.235619449019234,0.353429173528852,0.471238898038469),(0.,0.0911446219616379,
0.182289243923276,0.273433865884915,0.364578487846551),.UNSPECIFIED.)
GEOMETRIC_REPRESENTATION_ITEM()
RATIONAL_B_SPLINE_SURFACE(((1.,1.,1.,1.,1.,1.,1.),(0.707106781186548,0.707106781186548,
0.707106781186547,0.707106781186548,0.707106781186547,0.707106781186548,
0.707106781186548),(1.,1.,1.,1.,1.,1.,1.),(0.707106781186548,0.707106781186548,
0.707106781186547,0.707106781186548,0.707106781186547,0.707106781186548,
0.707106781186548),(1.,1.,1.,1.,1.,1.,1.),(0.707106781186548,0.707106781186548,
0.707106781186547,0.707106781186548,0.707106781186547,0.707106781186548,
0.707106781186548),(1.,1.,1.,1.,1.,1.,1.),(0.707106781186548,0.707106781186548,
0.707106781186547,0.707106781186548,0.707106781186547,0.707106781186548,
0.707106781186548),(1.,1.,1.,1.,1.,1.,1.)))
REPRESENTATION_ITEM('')
SURFACE()
) ;
#63 = (
BOUNDED_SURFACE()
B_SPLINE_SURFACE(2,3,((#174489,#174490,#174491,#174492),(#174493,#174494,
#174495,#174496),(#174497,#174498,#174499,#174500),(#174501,#174502,#174503,
#174504),(#174505,#174506,#174507,#174508),(#174509,#174510,#174511,#174512),
(#174513,#174514,#174515,#174516),(#174517,#174518,#174519,#174520),(#174521,
#174522,#174523,#174524)),.UNSPECIFIED.,.T.,.F.,.F.)
B_SPLINE_SURFACE_WITH_KNOTS((3,2,2,2,3),(4,4),(0.,0.117809724509617,0.235619449019234,
0.353429173528852,0.471238898038469),(0.,1.1454147408364),.UNSPECIFIED.)
GEOMETRIC_REPRESENTATION_ITEM()
RATIONAL_B_SPLINE_SURFACE(((1.,1.,1.,1.),(0.707106781186548,0.707106781186548,
0.707106781186547,0.707106781186548),(1.,1.,1.,1.),(0.707106781186548,0.707106781186548,
0.707106781186547,0.707106781186548),(1.,1.,1.,1.),(0.707106781186548,0.707106781186548,
0.707106781186547,0.707106781186548),(1.,1.,1.,1.),(0.707106781186548,0.707106781186548,
0.707106781186547,0.707106781186548),(1.,1.,1.,1.)))
REPRESENTATION_ITEM('')
SURFACE()
) ;
#64 = (
BOUNDED_SURFACE()
B_SPLINE_SURFACE(2,3,((#174532,#174533,#174534,#174535,#174536,#174537,
#174538,#174539,#174540,#174541,#174542,#174543,#174544,#174545,#174546,
#174547,#174548,#174549,#174550),(#174551,#174552,#174553,#174554,#174555,
#174556,#174557,#174558,#174559,#174560,#174561,#174562,#174563,#174564,
#174565,#174566,#174567,#174568,#174569),(#174570,#174571,#174572,#174573,
#174574,#174575,#174576,#174577,#174578,#174579,#174580,#174581,#174582,
#174583,#174584,#174585,#174586,#174587,#174588),(#174589,#174590,#174591,
#174592,#174593,#174594,#174595,#174596,#174597,#174598,#174599,#174600,
#174601,#174602,#174603,#174604,#174605,#174606,#174607),(#174608,#174609,
#174610,#174611,#174612,#174613,#174614,#174615,#174616,#174617,#174618,
#174619,#174620,#174621,#174622,#174623,#174624,#174625,#174626),(#174627,
#174628,#174629,#174630,#174631,#174632,#174633,#174634,#174635,#174636,
#174637,#174638,#174639,#174640,#174641,#174642,#174643,#174644,#174645),
(#174646,#174647,#174648,#174649,#174650,#174651,#174652,#174653,#174654,
#174655,#174656,#174657,#174658,#174659,#174660,#174661,#174662,#174663,
#174664),(#174665,#174666,#174667,#174668,#174669,#174670,#174671,#174672,
#174673,#174674,#174675,#174676,#174677,#174678,#174679,#174680,#174681,
#174682,#174683),(#174684,#174685,#174686,#174687,#174688,#174689,#174690,
#174691,#174692,#174693,#174694,#174695,#174696,#174697,#174698,#174699,
#174700,#174701,#174702)),.UNSPECIFIED.,.T.,.F.,.F.)
B_SPLINE_SURFACE_WITH_KNOTS((3,2,2,2,3),(4,1,1,1,1,1,1,1,1,1,1,1,1,1,1,
1,4),(0.,0.117809724509617,0.235619449019234,0.353429173528852,0.471238898038469),
(0.,0.226732296973331,0.464902013928651,0.70307173088397,0.9298040278573,
1.15653632483063,1.39470604178595,1.63287575874127,1.8596080557146,2.08634035268793,
2.32451006964325,2.56267978659857,2.7894120835719,3.01614438054523,3.25431409750055,
3.49248381445586,3.7192161114292),.UNSPECIFIED.)
GEOMETRIC_REPRESENTATION_ITEM()
RATIONAL_B_SPLINE_SURFACE(((1.,1.,1.,1.,1.,1.,1.,1.,1.,1.,1.,1.,1.,1.,1.,
1.,1.,1.,1.),(0.707106781186548,0.707106781186547,0.707106781186548,0.707106781186547,
0.707106781186548,0.707106781186547,0.707106781186548,0.707106781186547,
0.707106781186547,0.707106781186547,0.707106781186548,0.707106781186547,
0.707106781186547,0.707106781186547,0.707106781186547,0.707106781186547,
0.707106781186548,0.707106781186547,0.707106781186548),(1.,1.,1.,1.,1.,
1.,1.,1.,1.,1.,1.,1.,1.,1.,1.,1.,1.,1.,1.),(0.707106781186548,0.707106781186547,
0.707106781186548,0.707106781186547,0.707106781186548,0.707106781186547,
0.707106781186548,0.707106781186547,0.707106781186547,0.707106781186547,
0.707106781186548,0.707106781186547,0.707106781186547,0.707106781186547,
0.707106781186547,0.707106781186547,0.707106781186548,0.707106781186547,
0.707106781186548),(1.,1.,1.,1.,1.,1.,1.,1.,1.,1.,1.,1.,1.,1.,1.,1.,1.,
1.,1.),(0.707106781186548,0.707106781186547,0.707106781186548,0.707106781186547,
0.707106781186548,0.707106781186547,0.707106781186548,0.707106781186547,
0.707106781186547,0.707106781186547,0.707106781186548,0.707106781186547,
0.707106781186547,0.707106781186547,0.707106781186547,0.707106781186547,
0.707106781186548,0.707106781186547,0.707106781186548),(1.,1.,1.,1.,1.,
1.,1.,1.,1.,1.,1.,1.,1.,1.,1.,1.,1.,1.,1.),(0.707106781186548,0.707106781186547,
0.707106781186548,0.707106781186547,0.707106781186548,0.707106781186547,
0.707106781186548,0.707106781186547,0.707106781186547,0.707106781186547,
0.707106781186548,0.707106781186547,0.707106781186547,0.707106781186547,
0.707106781186547,0.707106781186547,0.707106781186548,0.707106781186547,
0.707106781186548),(1.,1.,1.,1.,1.,1.,1.,1.,1.,1.,1.,1.,1.,1.,1.,1.,1.,
1.,1.)))
REPRESENTATION_ITEM('')
SURFACE()
) ;
#65 = (
BOUNDED_SURFACE()
B_SPLINE_SURFACE(3,2,((#174725,#174726,#174727,#174728,#174729,#174730,
#174731,#174732,#174733),(#174734,#174735,#174736,#174737,#174738,#174739,
#174740,#174741,#174742),(#174743,#174744,#174745,#174746,#174747,#174748,
#174749,#174750,#174751),(#174752,#174753,#174754,#174755,#174756,#174757,
#174758,#174759,#174760),(#174761,#174762,#174763,#174764,#174765,#174766,
#174767,#174768,#174769),(#174770,#174771,#174772,#174773,#174774,#174775,
#174776,#174777,#174778),(#174779,#174780,#174781,#174782,#174783,#174784,
#174785,#174786,#174787),(#174788,#174789,#174790,#174791,#174792,#174793,
#174794,#174795,#174796),(#174797,#174798,#174799,#174800,#174801,#174802,
#174803,#174804,#174805),(#174806,#174807,#174808,#174809,#174810,#174811,
#174812,#174813,#174814),(#174815,#174816,#174817,#174818,#174819,#174820,
#174821,#174822,#174823),(#174824,#174825,#174826,#174827,#174828,#174829,
#174830,#174831,#174832),(#174833,#174834,#174835,#174836,#174837,#174838,
#174839,#174840,#174841),(#174842,#174843,#174844,#174845,#174846,#174847,
#174848,#174849,#174850),(#174851,#174852,#174853,#174854,#174855,#174856,
#174857,#174858,#174859),(#174860,#174861,#174862,#174863,#174864,#174865,
#174866,#174867,#174868),(#174869,#174870,#174871,#174872,#174873,#174874,
#174875,#174876,#174877),(#174878,#174879,#174880,#174881,#174882,#174883,
#174884,#174885,#174886),(#174887,#174888,#174889,#174890,#174891,#174892,
#174893,#174894,#174895),(#174896,#174897,#174898,#174899,#174900,#174901,
#174902,#174903,#174904),(#174905,#174906,#174907,#174908,#174909,#174910,
#174911,#174912,#174913),(#174914,#174915,#174916,#174917,#174918,#174919,
#174920,#174921,#174922),(#174923,#174924,#174925,#174926,#174927,#174928,
#174929,#174930,#174931),(#174932,#174933,#174934,#174935,#174936,#174937,
#174938,#174939,#174940),(#174941,#174942,#174943,#174944,#174945,#174946,
#174947,#174948,#174949),(#174950,#174951,#174952,#174953,#174954,#174955,
#174956,#174957,#174958),(#174959,#174960,#174961,#174962,#174963,#174964,
#174965,#174966,#174967),(#174968,#174969,#174970,#174971,#174972,#174973,
#174974,#174975,#174976),(#174977,#174978,#174979,#174980,#174981,#174982,
#174983,#174984,#174985),(#174986,#174987,#174988,#174989,#174990,#174991,
#174992,#174993,#174994),(#174995,#174996,#174997,#174998,#174999,#175000,
#175001,#175002,#175003),(#175004,#175005,#175006,#175007,#175008,#175009,
#175010,#175011,#175012),(#175013,#175014,#175015,#175016,#175017,#175018,
#175019,#175020,#175021),(#175022,#175023,#175024,#175025,#175026,#175027,
#175028,#175029,#175030),(#175031,#175032,#175033,#175034,#175035,#175036,
#175037,#175038,#175039),(#175040,#175041,#175042,#175043,#175044,#175045,
#175046,#175047,#175048),(#175049,#175050,#175051,#175052,#175053,#175054,
#175055,#175056,#175057),(#175058,#175059,#175060,#175061,#175062,#175063,
#175064,#175065,#175066),(#175067,#175068,#175069,#175070,#175071,#175072,
#175073,#175074,#175075),(#175076,#175077,#175078,#175079,#175080,#175081,
#175082,#175083,#175084),(#175085,#175086,#175087,#175088,#175089,#175090,
#175091,#175092,#175093),(#175094,#175095,#175096,#175097,#175098,#175099,
#175100,#175101,#175102),(#175103,#175104,#175105,#175106,#175107,#175108,
#175109,#175110,#175111),(#175112,#175113,#175114,#175115,#175116,#175117,
#175118,#175119,#175120),(#175121,#175122,#175123,#175124,#175125,#175126,
#175127,#175128,#175129),(#175130,#175131,#175132,#175133,#175134,#175135,
#175136,#175137,#175138),(#175139,#175140,#175141,#175142,#175143,#175144,
#175145,#175146,#175147),(#175148,#175149,#175150,#175151,#175152,#175153,
#175154,#175155,#175156),(#175157,#175158,#175159,#175160,#175161,#175162,
#175163,#175164,#175165),(#175166,#175167,#175168,#175169,#175170,#175171,
#175172,#175173,#175174),(#175175,#175176,#175177,#175178,#175179,#175180,
#175181,#175182,#175183),(#175184,#175185,#175186,#175187,#175188,#175189,
#175190,#175191,#175192),(#175193,#175194,#175195,#175196,#175197,#175198,
#175199,#175200,#175201),(#175202,#175203,#175204,#175205,#175206,#175207,
#175208,#175209,#175210),(#175211,#175212,#175213,#175214,#175215,#175216,
#175217,#175218,#175219),(#175220,#175221,#175222,#175223,#175224,#175225,
#175226,#175227,#175228),(#175229,#175230,#175231,#175232,#175233,#175234,
#175235,#175236,#175237),(#175238,#175239,#175240,#175241,#175242,#175243,
#175244,#175245,#175246),(#175247,#175248,#175249,#175250,#175251,#175252,
#175253,#175254,#175255),(#175256,#175257,#175258,#175259,#175260,#175261,
#175262,#175263,#175264),(#175265,#175266,#175267,#175268,#175269,#175270,
#175271,#175272,#175273),(#175274,#175275,#175276,#175277,#175278,#175279,
#175280,#175281,#175282),(#175283,#175284,#175285,#175286,#175287,#175288,
#175289,#175290,#175291),(#175292,#175293,#175294,#175295,#175296,#175297,
#175298,#175299,#175300),(#175301,#175302,#175303,#175304,#175305,#175306,
#175307,#175308,#175309),(#175310,#175311,#175312,#175313,#175314,#175315,
#175316,#175317,#175318),(#175319,#175320,#175321,#175322,#175323,#175324,
#175325,#175326,#175327),(#175328,#175329,#175330,#175331,#175332,#175333,
#175334,#175335,#175336),(#175337,#175338,#175339,#175340,#175341,#175342,
#175343,#175344,#175345),(#175346,#175347,#175348,#175349,#175350,#175351,
#175352,#175353,#175354),(#175355,#175356,#175357,#175358,#175359,#175360,
#175361,#175362,#175363),(#175364,#175365,#175366,#175367,#175368,#175369,
#175370,#175371,#175372),(#175373,#175374,#175375,#175376,#175377,#175378,
#175379,#175380,#175381),(#175382,#175383,#175384,#175385,#175386,#175387,
#175388,#175389,#175390),(#175391,#175392,#175393,#175394,#175395,#175396,
#175397,#175398,#175399),(#175400,#175401,#175402,#175403,#175404,#175405,
#175406,#175407,#175408),(#175409,#175410,#175411,#175412,#175413,#175414,
#175415,#175416,#175417),(#175418,#175419,#175420,#175421,#175422,#175423,
#175424,#175425,#175426),(#175427,#175428,#175429,#175430,#175431,#175432,
#175433,#175434,#175435),(#175436,#175437,#175438,#175439,#175440,#175441,
#175442,#175443,#175444),(#175445,#175446,#175447,#175448,#175449,#175450,
#175451,#175452,#175453),(#175454,#175455,#175456,#175457,#175458,#175459,
#175460,#175461,#175462),(#175463,#175464,#175465,#175466,#175467,#175468,
#175469,#175470,#175471),(#175472,#175473,#175474,#175475,#175476,#175477,
#175478,#175479,#175480),(#175481,#175482,#175483,#175484,#175485,#175486,
#175487,#175488,#175489),(#175490,#175491,#175492,#175493,#175494,#175495,
#175496,#175497,#175498),(#175499,#175500,#175501,#175502,#175503,#175504,
#175505,#175506,#175507),(#175508,#175509,#175510,#175511,#175512,#175513,
#175514,#175515,#175516),(#175517,#175518,#175519,#175520,#175521,#175522,
#175523,#175524,#175525),(#175526,#175527,#175528,#175529,#175530,#175531,
#175532,#175533,#175534),(#175535,#175536,#175537,#175538,#175539,#175540,
#175541,#175542,#175543),(#175544,#175545,#175546,#175547,#175548,#175549,
#175550,#175551,#175552),(#175553,#175554,#175555,#175556,#175557,#175558,
#175559,#175560,#175561),(#175562,#175563,#175564,#175565,#175566,#175567,
#175568,#175569,#175570),(#175571,#175572,#175573,#175574,#175575,#175576,
#175577,#175578,#175579),(#175580,#175581,#175582,#175583,#175584,#175585,
#175586,#175587,#175588),(#175589,#175590,#175591,#175592,#175593,#175594,
#175595,#175596,#175597),(#175598,#175599,#175600,#175601,#175602,#175603,
#175604,#175605,#175606),(#175607,#175608,#175609,#175610,#175611,#175612,
#175613,#175614,#175615),(#175616,#175617,#175618,#175619,#175620,#175621,
#175622,#175623,#175624),(#175625,#175626,#175627,#175628,#175629,#175630,
#175631,#175632,#175633),(#175634,#175635,#175636,#175637,#175638,#175639,
#175640,#175641,#175642),(#175643,#175644,#175645,#175646,#175647,#175648,
#175649,#175650,#175651),(#175652,#175653,#175654,#175655,#175656,#175657,
#175658,#175659,#175660),(#175661,#175662,#175663,#175664,#175665,#175666,
#175667,#175668,#175669),(#175670,#175671,#175672,#175673,#175674,#175675,
#175676,#175677,#175678),(#175679,#175680,#175681,#175682,#175683,#175684,
#175685,#175686,#175687),(#175688,#175689,#175690,#175691,#175692,#175693,
#175694,#175695,#175696),(#175697,#175698,#175699,#175700,#175701,#175702,
#175703,#175704,#175705),(#175706,#175707,#175708,#175709,#175710,#175711,
#175712,#175713,#175714),(#175715,#175716,#175717,#175718,#175719,#175720,
#175721,#175722,#175723),(#175724,#175725,#175726,#175727,#175728,#175729,
#175730,#175731,#175732),(#175733,#175734,#175735,#175736,#175737,#175738,
#175739,#175740,#175741),(#175742,#175743,#175744,#175745,#175746,#175747,
#175748,#175749,#175750),(#175751,#175752,#175753,#175754,#175755,#175756,
#175757,#175758,#175759),(#175760,#175761,#175762,#175763,#175764,#175765,
#175766,#175767,#175768),(#175769,#175770,#175771,#175772,#175773,#175774,
#175775,#175776,#175777),(#175778,#175779,#175780,#175781,#175782,#175783,
#175784,#175785,#175786),(#175787,#175788,#175789,#175790,#175791,#175792,
#175793,#175794,#175795),(#175796,#175797,#175798,#175799,#175800,#175801,
#175802,#175803,#175804),(#175805,#175806,#175807,#175808,#175809,#175810,
#175811,#175812,#175813),(#175814,#175815,#175816,#175817,#175818,#175819,
#175820,#175821,#175822),(#175823,#175824,#175825,#175826,#175827,#175828,
#175829,#175830,#175831),(#175832,#175833,#175834,#175835,#175836,#175837,
#175838,#175839,#175840),(#175841,#175842,#175843,#175844,#175845,#175846,
#175847,#175848,#175849),(#175850,#175851,#175852,#175853,#175854,#175855,
#175856,#175857,#175858),(#175859,#175860,#175861,#175862,#175863,#175864,
#175865,#175866,#175867),(#175868,#175869,#175870,#175871,#175872,#175873,
#175874,#175875,#175876),(#175877,#175878,#175879,#175880,#175881,#175882,
#175883,#175884,#175885),(#175886,#175887,#175888,#175889,#175890,#175891,
#175892,#175893,#175894),(#175895,#175896,#175897,#175898,#175899,#175900,
#175901,#175902,#175903),(#175904,#175905,#175906,#175907,#175908,#175909,
#175910,#175911,#175912),(#175913,#175914,#175915,#175916,#175917,#175918,
#175919,#175920,#175921),(#175922,#175923,#175924,#175925,#175926,#175927,
#175928,#175929,#175930),(#175931,#175932,#175933,#175934,#175935,#175936,
#175937,#175938,#175939),(#175940,#175941,#175942,#175943,#175944,#175945,
#175946,#175947,#175948),(#175949,#175950,#175951,#175952,#175953,#175954,
#175955,#175956,#175957),(#175958,#175959,#175960,#175961,#175962,#175963,
#175964,#175965,#175966),(#175967,#175968,#175969,#175970,#175971,#175972,
#175973,#175974,#175975),(#175976,#175977,#175978,#175979,#175980,#175981,
#175982,#175983,#175984),(#175985,#175986,#175987,#175988,#175989,#175990,
#175991,#175992,#175993),(#175994,#175995,#175996,#175997,#175998,#175999,
#176000,#176001,#176002),(#176003,#176004,#176005,#176006,#176007,#176008,
#176009,#176010,#176011),(#176012,#176013,#176014,#176015,#176016,#176017,
#176018,#176019,#176020),(#176021,#176022,#176023,#176024,#176025,#176026,
#176027,#176028,#176029),(#176030,#176031,#176032,#176033,#176034,#176035,
#176036,#176037,#176038),(#176039,#176040,#176041,#176042,#176043,#176044,
#176045,#176046,#176047),(#176048,#176049,#176050,#176051,#176052,#176053,
#176054,#176055,#176056),(#176057,#176058,#176059,#176060,#176061,#176062,
#176063,#176064,#176065),(#176066,#176067,#176068,#176069,#176070,#176071,
#176072,#176073,#176074),(#176075,#176076,#176077,#176078,#176079,#176080,
#176081,#176082,#176083),(#176084,#176085,#176086,#176087,#176088,#176089,
#176090,#176091,#176092),(#176093,#176094,#176095,#176096,#176097,#176098,
#176099,#176100,#176101),(#176102,#176103,#176104,#176105,#176106,#176107,
#176108,#176109,#176110),(#176111,#176112,#176113,#176114,#176115,#176116,
#176117,#176118,#176119),(#176120,#176121,#176122,#176123,#176124,#176125,
#176126,#176127,#176128),(#176129,#176130,#176131,#176132,#176133,#176134,
#176135,#176136,#176137),(#176138,#176139,#176140,#176141,#176142,#176143,
#176144,#176145,#176146),(#176147,#176148,#176149,#176150,#176151,#176152,
#176153,#176154,#176155),(#176156,#176157,#176158,#176159,#176160,#176161,
#176162,#176163,#176164),(#176165,#176166,#176167,#176168,#176169,#176170,
#176171,#176172,#176173),(#176174,#176175,#176176,#176177,#176178,#176179,
#176180,#176181,#176182),(#176183,#176184,#176185,#176186,#176187,#176188,
#176189,#176190,#176191),(#176192,#176193,#176194,#176195,#176196,#176197,
#176198,#176199,#176200),(#176201,#176202,#176203,#176204,#176205,#176206,
#176207,#176208,#176209),(#176210,#176211,#176212,#176213,#176214,#176215,
#176216,#176217,#176218),(#176219,#176220,#176221,#176222,#176223,#176224,
#176225,#176226,#176227),(#176228,#176229,#176230,#176231,#176232,#176233,
#176234,#176235,#176236),(#176237,#176238,#176239,#176240,#176241,#176242,
#176243,#176244,#176245),(#176246,#176247,#176248,#176249,#176250,#176251,
#176252,#176253,#176254),(#176255,#176256,#176257,#176258,#176259,#176260,
#176261,#176262,#176263),(#176264,#176265,#176266,#176267,#176268,#176269,
#176270,#176271,#176272),(#176273,#176274,#176275,#176276,#176277,#176278,
#176279,#176280,#176281),(#176282,#176283,#176284,#176285,#176286,#176287,
#176288,#176289,#176290),(#176291,#176292,#176293,#176294,#176295,#176296,
#176297,#176298,#176299),(#176300,#176301,#176302,#176303,#176304,#176305,
#176306,#176307,#176308),(#176309,#176310,#176311,#176312,#176313,#176314,
#176315,#176316,#176317),(#176318,#176319,#176320,#176321,#176322,#176323,
#176324,#176325,#176326),(#176327,#176328,#176329,#176330,#176331,#176332,
#176333,#176334,#176335),(#176336,#176337,#176338,#176339,#176340,#176341,
#176342,#176343,#176344),(#176345,#176346,#176347,#176348,#176349,#176350,
#176351,#176352,#176353),(#176354,#176355,#176356,#176357,#176358,#176359,
#176360,#176361,#176362),(#176363,#176364,#176365,#176366,#176367,#176368,
#176369,#176370,#176371),(#176372,#176373,#176374,#176375,#176376,#176377,
#176378,#176379,#176380),(#176381,#176382,#176383,#176384,#176385,#176386,
#176387,#176388,#176389),(#176390,#176391,#176392,#176393,#176394,#176395,
#176396,#176397,#176398),(#176399,#176400,#176401,#176402,#176403,#176404,
#176405,#176406,#176407),(#176408,#176409,#176410,#176411,#176412,#176413,
#176414,#176415,#176416),(#176417,#176418,#176419,#176420,#176421,#176422,
#176423,#176424,#176425),(#176426,#176427,#176428,#176429,#176430,#176431,
#176432,#176433,#176434),(#176435,#176436,#176437,#176438,#176439,#176440,
#176441,#176442,#176443),(#176444,#176445,#176446,#176447,#176448,#176449,
#176450,#176451,#176452),(#176453,#176454,#176455,#176456,#176457,#176458,
#176459,#176460,#176461),(#176462,#176463,#176464,#176465,#176466,#176467,
#176468,#176469,#176470),(#176471,#176472,#176473,#176474,#176475,#176476,
#176477,#176478,#176479),(#176480,#176481,#176482,#176483,#176484,#176485,
#176486,#176487,#176488),(#176489,#176490,#176491,#176492,#176493,#176494,
#176495,#176496,#176497),(#176498,#176499,#176500,#176501,#176502,#176503,
#176504,#176505,#176506),(#176507,#176508,#176509,#176510,#176511,#176512,
#176513,#176514,#176515),(#176516,#176517,#176518,#176519,#176520,#176521,
#176522,#176523,#176524),(#176525,#176526,#176527,#176528,#176529,#176530,
#176531,#176532,#176533),(#176534,#176535,#176536,#176537,#176538,#176539,
#176540,#176541,#176542),(#176543,#176544,#176545,#176546,#176547,#176548,
#176549,#176550,#176551),(#176552,#176553,#176554,#176555,#176556,#176557,
#176558,#176559,#176560),(#176561,#176562,#176563,#176564,#176565,#176566,
#176567,#176568,#176569),(#176570,#176571,#176572,#176573,#176574,#176575,
#176576,#176577,#176578),(#176579,#176580,#176581,#176582,#176583,#176584,
#176585,#176586,#176587),(#176588,#176589,#176590,#176591,#176592,#176593,
#176594,#176595,#176596),(#176597,#176598,#176599,#176600,#176601,#176602,
#176603,#176604,#176605),(#176606,#176607,#176608,#176609,#176610,#176611,
#176612,#176613,#176614),(#176615,#176616,#176617,#176618,#176619,#176620,
#176621,#176622,#176623),(#176624,#176625,#176626,#176627,#176628,#176629,
#176630,#176631,#176632),(#176633,#176634,#176635,#176636,#176637,#176638,
#176639,#176640,#176641),(#176642,#176643,#176644,#176645,#176646,#176647,
#176648,#176649,#176650),(#176651,#176652,#176653,#176654,#176655,#176656,
#176657,#176658,#176659),(#176660,#176661,#176662,#176663,#176664,#176665,
#176666,#176667,#176668),(#176669,#176670,#176671,#176672,#176673,#176674,
#176675,#176676,#176677),(#176678,#176679,#176680,#176681,#176682,#176683,
#176684,#176685,#176686),(#176687,#176688,#176689,#176690,#176691,#176692,
#176693,#176694,#176695),(#176696,#176697,#176698,#176699,#176700,#176701,
#176702,#176703,#176704),(#176705,#176706,#176707,#176708,#176709,#176710,
#176711,#176712,#176713),(#176714,#176715,#176716,#176717,#176718,#176719,
#176720,#176721,#176722),(#176723,#176724,#176725,#176726,#176727,#176728,
#176729,#176730,#176731),(#176732,#176733,#176734,#176735,#176736,#176737,
#176738,#176739,#176740),(#176741,#176742,#176743,#176744,#176745,#176746,
#176747,#176748,#176749),(#176750,#176751,#176752,#176753,#176754,#176755,
#176756,#176757,#176758),(#176759,#176760,#176761,#176762,#176763,#176764,
#176765,#176766,#176767),(#176768,#176769,#176770,#176771,#176772,#176773,
#176774,#176775,#176776),(#176777,#176778,#176779,#176780,#176781,#176782,
#176783,#176784,#176785),(#176786,#176787,#176788,#176789,#176790,#176791,
#176792,#176793,#176794),(#176795,#176796,#176797,#176798,#176799,#176800,
#176801,#176802,#176803),(#176804,#176805,#176806,#176807,#176808,#176809,
#176810,#176811,#176812),(#176813,#176814,#176815,#176816,#176817,#176818,
#176819,#176820,#176821),(#176822,#176823,#176824,#176825,#176826,#176827,
#176828,#176829,#176830),(#176831,#176832,#176833,#176834,#176835,#176836,
#176837,#176838,#176839),(#176840,#176841,#176842,#176843,#176844,#176845,
#176846,#176847,#176848),(#176849,#176850,#176851,#176852,#176853,#176854,
#176855,#176856,#176857),(#176858,#176859,#176860,#176861,#176862,#176863,
#176864,#176865,#176866),(#176867,#176868,#176869,#176870,#176871,#176872,
#176873,#176874,#176875),(#176876,#176877,#176878,#176879,#176880,#176881,
#176882,#176883,#176884),(#176885,#176886,#176887,#176888,#176889,#176890,
#176891,#176892,#176893),(#176894,#176895,#176896,#176897,#176898,#176899,
#176900,#176901,#176902),(#176903,#176904,#176905,#176906,#176907,#176908,
#176909,#176910,#176911),(#176912,#176913,#176914,#176915,#176916,#176917,
#176918,#176919,#176920),(#176921,#176922,#176923,#176924,#176925,#176926,
#176927,#176928,#176929),(#176930,#176931,#176932,#176933,#176934,#176935,
#176936,#176937,#176938),(#176939,#176940,#176941,#176942,#176943,#176944,
#176945,#176946,#176947),(#176948,#176949,#176950,#176951,#176952,#176953,
#176954,#176955,#176956),(#176957,#176958,#176959,#176960,#176961,#176962,
#176963,#176964,#176965),(#176966,#176967,#176968,#176969,#176970,#176971,
#176972,#176973,#176974),(#176975,#176976,#176977,#176978,#176979,#176980,
#176981,#176982,#176983),(#176984,#176985,#176986,#176987,#176988,#176989,
#176990,#176991,#176992),(#176993,#176994,#176995,#176996,#176997,#176998,
#176999,#177000,#177001),(#177002,#177003,#177004,#177005,#177006,#177007,
#177008,#177009,#177010),(#177011,#177012,#177013,#177014,#177015,#177016,
#177017,#177018,#177019),(#177020,#177021,#177022,#177023,#177024,#177025,
#177026,#177027,#177028),(#177029,#177030,#177031,#177032,#177033,#177034,
#177035,#177036,#177037),(#177038,#177039,#177040,#177041,#177042,#177043,
#177044,#177045,#177046),(#177047,#177048,#177049,#177050,#177051,#177052,
#177053,#177054,#177055),(#177056,#177057,#177058,#177059,#177060,#177061,
#177062,#177063,#177064),(#177065,#177066,#177067,#177068,#177069,#177070,
#177071,#177072,#177073),(#177074,#177075,#177076,#177077,#177078,#177079,
#177080,#177081,#177082),(#177083,#177084,#177085,#177086,#177087,#177088,
#177089,#177090,#177091),(#177092,#177093,#177094,#177095,#177096,#177097,
#177098,#177099,#177100),(#177101,#177102,#177103,#177104,#177105,#177106,
#177107,#177108,#177109),(#177110,#177111,#177112,#177113,#177114,#177115,
#177116,#177117,#177118),(#177119,#177120,#177121,#177122,#177123,#177124,
#177125,#177126,#177127),(#177128,#177129,#177130,#177131,#177132,#177133,
#177134,#177135,#177136),(#177137,#177138,#177139,#177140,#177141,#177142,
#177143,#177144,#177145),(#177146,#177147,#177148,#177149,#177150,#177151,
#177152,#177153,#177154),(#177155,#177156,#177157,#177158,#177159,#177160,
#177161,#177162,#177163),(#177164,#177165,#177166,#177167,#177168,#177169,
#177170,#177171,#177172),(#177173,#177174,#177175,#177176,#177177,#177178,
#177179,#177180,#177181),(#177182,#177183,#177184,#177185,#177186,#177187,
#177188,#177189,#177190),(#177191,#177192,#177193,#177194,#177195,#177196,
#177197,#177198,#177199),(#177200,#177201,#177202,#177203,#177204,#177205,
#177206,#177207,#177208),(#177209,#177210,#177211,#177212,#177213,#177214,
#177215,#177216,#177217),(#177218,#177219,#177220,#177221,#177222,#177223,
#177224,#177225,#177226),(#177227,#177228,#177229,#177230,#177231,#177232,
#177233,#177234,#177235),(#177236,#177237,#177238,#177239,#177240,#177241,
#177242,#177243,#177244),(#177245,#177246,#177247,#177248,#177249,#177250,
#177251,#177252,#177253),(#177254,#177255,#177256,#177257,#177258,#177259,
#177260,#177261,#177262),(#177263,#177264,#177265,#177266,#177267,#177268,
#177269,#177270,#177271),(#177272,#177273,#177274,#177275,#177276,#177277,
#177278,#177279,#177280),(#177281,#177282,#177283,#177284,#177285,#177286,
#177287,#177288,#177289),(#177290,#177291,#177292,#177293,#177294,#177295,
#177296,#177297,#177298),(#177299,#177300,#177301,#177302,#177303,#177304,
#177305,#177306,#177307),(#177308,#177309,#177310,#177311,#177312,#177313,
#177314,#177315,#177316),(#177317,#177318,#177319,#177320,#177321,#177322,
#177323,#177324,#177325),(#177326,#177327,#177328,#177329,#177330,#177331,
#177332,#177333,#177334),(#177335,#177336,#177337,#177338,#177339,#177340,
#177341,#177342,#177343),(#177344,#177345,#177346,#177347,#177348,#177349,
#177350,#177351,#177352),(#177353,#177354,#177355,#177356,#177357,#177358,
#177359,#177360,#177361),(#177362,#177363,#177364,#177365,#177366,#177367,
#177368,#177369,#177370),(#177371,#177372,#177373,#177374,#177375,#177376,
#177377,#177378,#177379),(#177380,#177381,#177382,#177383,#177384,#177385,
#177386,#177387,#177388),(#177389,#177390,#177391,#177392,#177393,#177394,
#177395,#177396,#177397),(#177398,#177399,#177400,#177401,#177402,#177403,
#177404,#177405,#177406),(#177407,#177408,#177409,#177410,#177411,#177412,
#177413,#177414,#177415),(#177416,#177417,#177418,#177419,#177420,#177421,
#177422,#177423,#177424),(#177425,#177426,#177427,#177428,#177429,#177430,
#177431,#177432,#177433),(#177434,#177435,#177436,#177437,#177438,#177439,
#177440,#177441,#177442),(#177443,#177444,#177445,#177446,#177447,#177448,
#177449,#177450,#177451),(#177452,#177453,#177454,#177455,#177456,#177457,
#177458,#177459,#177460),(#177461,#177462,#177463,#177464,#177465,#177466,
#177467,#177468,#177469),(#177470,#177471,#177472,#177473,#177474,#177475,
#177476,#177477,#177478),(#177479,#177480,#177481,#177482,#177483,#177484,
#177485,#177486,#177487),(#177488,#177489,#177490,#177491,#177492,#177493,
#177494,#177495,#177496),(#177497,#177498,#177499,#177500,#177501,#177502,
#177503,#177504,#177505),(#177506,#177507,#177508,#177509,#177510,#177511,
#177512,#177513,#177514),(#177515,#177516,#177517,#177518,#177519,#177520,
#177521,#177522,#177523),(#177524,#177525,#177526,#177527,#177528,#177529,
#177530,#177531,#177532),(#177533,#177534,#177535,#177536,#177537,#177538,
#177539,#177540,#177541),(#177542,#177543,#177544,#177545,#177546,#177547,
#177548,#177549,#177550),(#177551,#177552,#177553,#177554,#177555,#177556,
#177557,#177558,#177559),(#177560,#177561,#177562,#177563,#177564,#177565,
#177566,#177567,#177568),(#177569,#177570,#177571,#177572,#177573,#177574,
#177575,#177576,#177577),(#177578,#177579,#177580,#177581,#177582,#177583,
#177584,#177585,#177586),(#177587,#177588,#177589,#177590,#177591,#177592,
#177593,#177594,#177595),(#177596,#177597,#177598,#177599,#177600,#177601,
#177602,#177603,#177604),(#177605,#177606,#177607,#177608,#177609,#177610,
#177611,#177612,#177613),(#177614,#177615,#177616,#177617,#177618,#177619,
#177620,#177621,#177622),(#177623,#177624,#177625,#177626,#177627,#177628,
#177629,#177630,#177631),(#177632,#177633,#177634,#177635,#177636,#177637,
#177638,#177639,#177640),(#177641,#177642,#177643,#177644,#177645,#177646,
#177647,#177648,#177649),(#177650,#177651,#177652,#177653,#177654,#177655,
#177656,#177657,#177658),(#177659,#177660,#177661,#177662,#177663,#177664,
#177665,#177666,#177667),(#177668,#177669,#177670,#177671,#177672,#177673,
#177674,#177675,#177676),(#177677,#177678,#177679,#177680,#177681,#177682,
#177683,#177684,#177685),(#177686,#177687,#177688,#177689,#177690,#177691,
#177692,#177693,#177694),(#177695,#177696,#177697,#177698,#177699,#177700,
#177701,#177702,#177703),(#177704,#177705,#177706,#177707,#177708,#177709,
#177710,#177711,#177712),(#177713,#177714,#177715,#177716,#177717,#177718,
#177719,#177720,#177721),(#177722,#177723,#177724,#177725,#177726,#177727,
#177728,#177729,#177730),(#177731,#177732,#177733,#177734,#177735,#177736,
#177737,#177738,#177739),(#177740,#177741,#177742,#177743,#177744,#177745,
#177746,#177747,#177748),(#177749,#177750,#177751,#177752,#177753,#177754,
#177755,#177756,#177757),(#177758,#177759,#177760,#177761,#177762,#177763,
#177764,#177765,#177766),(#177767,#177768,#177769,#177770,#177771,#177772,
#177773,#177774,#177775),(#177776,#177777,#177778,#177779,#177780,#177781,
#177782,#177783,#177784),(#177785,#177786,#177787,#177788,#177789,#177790,
#177791,#177792,#177793),(#177794,#177795,#177796,#177797,#177798,#177799,
#177800,#177801,#177802),(#177803,#177804,#177805,#177806,#177807,#177808,
#177809,#177810,#177811),(#177812,#177813,#177814,#177815,#177816,#177817,
#177818,#177819,#177820),(#177821,#177822,#177823,#177824,#177825,#177826,
#177827,#177828,#177829),(#177830,#177831,#177832,#177833,#177834,#177835,
#177836,#177837,#177838),(#177839,#177840,#177841,#177842,#177843,#177844,
#177845,#177846,#177847),(#177848,#177849,#177850,#177851,#177852,#177853,
#177854,#177855,#177856),(#177857,#177858,#177859,#177860,#177861,#177862,
#177863,#177864,#177865),(#177866,#177867,#177868,#177869,#177870,#177871,
#177872,#177873,#177874),(#177875,#177876,#177877,#177878,#177879,#177880,
#177881,#177882,#177883),(#177884,#177885,#177886,#177887,#177888,#177889,
#177890,#177891,#177892),(#177893,#177894,#177895,#177896,#177897,#177898,
#177899,#177900,#177901),(#177902,#177903,#177904,#177905,#177906,#177907,
#177908,#177909,#177910),(#177911,#177912,#177913,#177914,#177915,#177916,
#177917,#177918,#177919),(#177920,#177921,#177922,#177923,#177924,#177925,
#177926,#177927,#177928),(#177929,#177930,#177931,#177932,#177933,#177934,
#177935,#177936,#177937),(#177938,#177939,#177940,#177941,#177942,#177943,
#177944,#177945,#177946),(#177947,#177948,#177949,#177950,#177951,#177952,
#177953,#177954,#177955),(#177956,#177957,#177958,#177959,#177960,#177961,
#177962,#177963,#177964),(#177965,#177966,#177967,#177968,#177969,#177970,
#177971,#177972,#177973),(#177974,#177975,#177976,#177977,#177978,#177979,
#177980,#177981,#177982),(#177983,#177984,#177985,#177986,#177987,#177988,
#177989,#177990,#177991),(#177992,#177993,#177994,#177995,#177996,#177997,
#177998,#177999,#178000),(#178001,#178002,#178003,#178004,#178005,#178006,
#178007,#178008,#178009),(#178010,#178011,#178012,#178013,#178014,#178015,
#178016,#178017,#178018),(#178019,#178020,#178021,#178022,#178023,#178024,
#178025,#178026,#178027),(#178028,#178029,#178030,#178031,#178032,#178033,
#178034,#178035,#178036),(#178037,#178038,#178039,#178040,#178041,#178042,
#178043,#178044,#178045),(#178046,#178047,#178048,#178049,#178050,#178051,
#178052,#178053,#178054),(#178055,#178056,#178057,#178058,#178059,#178060,
#178061,#178062,#178063),(#178064,#178065,#178066,#178067,#178068,#178069,
#178070,#178071,#178072),(#178073,#178074,#178075,#178076,#178077,#178078,
#178079,#178080,#178081),(#178082,#178083,#178084,#178085,#178086,#178087,
#178088,#178089,#178090),(#178091,#178092,#178093,#178094,#178095,#178096,
#178097,#178098,#178099),(#178100,#178101,#178102,#178103,#178104,#178105,
#178106,#178107,#178108),(#178109,#178110,#178111,#178112,#178113,#178114,
#178115,#178116,#178117),(#178118,#178119,#178120,#178121,#178122,#178123,
#178124,#178125,#178126),(#178127,#178128,#178129,#178130,#178131,#178132,
#178133,#178134,#178135),(#178136,#178137,#178138,#178139,#178140,#178141,
#178142,#178143,#178144),(#178145,#178146,#178147,#178148,#178149,#178150,
#178151,#178152,#178153),(#178154,#178155,#178156,#178157,#178158,#178159,
#178160,#178161,#178162),(#178163,#178164,#178165,#178166,#178167,#178168,
#178169,#178170,#178171),(#178172,#178173,#178174,#178175,#178176,#178177,
#178178,#178179,#178180),(#178181,#178182,#178183,#178184,#178185,#178186,
#178187,#178188,#178189),(#178190,#178191,#178192,#178193,#178194,#178195,
#178196,#178197,#178198),(#178199,#178200,#178201,#178202,#178203,#178204,
#178205,#178206,#178207),(#178208,#178209,#178210,#178211,#178212,#178213,
#178214,#178215,#178216),(#178217,#178218,#178219,#178220,#178221,#178222,
#178223,#178224,#178225),(#178226,#178227,#178228,#178229,#178230,#178231,
#178232,#178233,#178234),(#178235,#178236,#178237,#178238,#178239,#178240,
#178241,#178242,#178243),(#178244,#178245,#178246,#178247,#178248,#178249,
#178250,#178251,#178252),(#178253,#178254,#178255,#178256,#178257,#178258,
#178259,#178260,#178261),(#178262,#178263,#178264,#178265,#178266,#178267,
#178268,#178269,#178270),(#178271,#178272,#178273,#178274,#178275,#178276,
#178277,#178278,#178279),(#178280,#178281,#178282,#178283,#178284,#178285,
#178286,#178287,#178288),(#178289,#178290,#178291,#178292,#178293,#178294,
#178295,#178296,#178297),(#178298,#178299,#178300,#178301,#178302,#178303,
#178304,#178305,#178306),(#178307,#178308,#178309,#178310,#178311,#178312,
#178313,#178314,#178315),(#178316,#178317,#178318,#178319,#178320,#178321,
#178322,#178323,#178324),(#178325,#178326,#178327,#178328,#178329,#178330,
#178331,#178332,#178333),(#178334,#178335,#178336,#178337,#178338,#178339,
#178340,#178341,#178342),(#178343,#178344,#178345,#178346,#178347,#178348,
#178349,#178350,#178351),(#178352,#178353,#178354,#178355,#178356,#178357,
#178358,#178359,#178360),(#178361,#178362,#178363,#178364,#178365,#178366,
#178367,#178368,#178369),(#178370,#178371,#178372,#178373,#178374,#178375,
#178376,#178377,#178378),(#178379,#178380,#178381,#178382,#178383,#178384,
#178385,#178386,#178387),(#178388,#178389,#178390,#178391,#178392,#178393,
#178394,#178395,#178396),(#178397,#178398,#178399,#178400,#178401,#178402,
#178403,#178404,#178405),(#178406,#178407,#178408,#178409,#178410,#178411,
#178412,#178413,#178414),(#178415,#178416,#178417,#178418,#178419,#178420,
#178421,#178422,#178423),(#178424,#178425,#178426,#178427,#178428,#178429,
#178430,#178431,#178432),(#178433,#178434,#178435,#178436,#178437,#178438,
#178439,#178440,#178441),(#178442,#178443,#178444,#178445,#178446,#178447,
#178448,#178449,#178450),(#178451,#178452,#178453,#178454,#178455,#178456,
#178457,#178458,#178459),(#178460,#178461,#178462,#178463,#178464,#178465,
#178466,#178467,#178468),(#178469,#178470,#178471,#178472,#178473,#178474,
#178475,#178476,#178477),(#178478,#178479,#178480,#178481,#178482,#178483,
#178484,#178485,#178486),(#178487,#178488,#178489,#178490,#178491,#178492,
#178493,#178494,#178495),(#178496,#178497,#178498,#178499,#178500,#178501,
#178502,#178503,#178504),(#178505,#178506,#178507,#178508,#178509,#178510,
#178511,#178512,#178513),(#178514,#178515,#178516,#178517,#178518,#178519,
#178520,#178521,#178522),(#178523,#178524,#178525,#178526,#178527,#178528,
#178529,#178530,#178531),(#178532,#178533,#178534,#178535,#178536,#178537,
#178538,#178539,#178540),(#178541,#178542,#178543,#178544,#178545,#178546,
#178547,#178548,#178549),(#178550,#178551,#178552,#178553,#178554,#178555,
#178556,#178557,#178558),(#178559,#178560,#178561,#178562,#178563,#178564,
#178565,#178566,#178567),(#178568,#178569,#178570,#178571,#178572,#178573,
#178574,#178575,#178576),(#178577,#178578,#178579,#178580,#178581,#178582,
#178583,#178584,#178585),(#178586,#178587,#178588,#178589,#178590,#178591,
#178592,#178593,#178594),(#178595,#178596,#178597,#178598,#178599,#178600,
#178601,#178602,#178603),(#178604,#178605,#178606,#178607,#178608,#178609,
#178610,#178611,#178612),(#178613,#178614,#178615,#178616,#178617,#178618,
#178619,#178620,#178621),(#178622,#178623,#178624,#178625,#178626,#178627,
#178628,#178629,#178630),(#178631,#178632,#178633,#178634,#178635,#178636,
#178637,#178638,#178639),(#178640,#178641,#178642,#178643,#178644,#178645,
#178646,#178647,#178648),(#178649,#178650,#178651,#178652,#178653,#178654,
#178655,#178656,#178657),(#178658,#178659,#178660,#178661,#178662,#178663,
#178664,#178665,#178666),(#178667,#178668,#178669,#178670,#178671,#178672,
#178673,#178674,#178675),(#178676,#178677,#178678,#178679,#178680,#178681,
#178682,#178683,#178684),(#178685,#178686,#178687,#178688,#178689,#178690,
#178691,#178692,#178693),(#178694,#178695,#178696,#178697,#178698,#178699,
#178700,#178701,#178702),(#178703,#178704,#178705,#178706,#178707,#178708,
#178709,#178710,#178711),(#178712,#178713,#178714,#178715,#178716,#178717,
#178718,#178719,#178720),(#178721,#178722,#178723,#178724,#178725,#178726,
#178727,#178728,#178729),(#178730,#178731,#178732,#178733,#178734,#178735,
#178736,#178737,#178738),(#178739,#178740,#178741,#178742,#178743,#178744,
#178745,#178746,#178747),(#178748,#178749,#178750,#178751,#178752,#178753,
#178754,#178755,#178756),(#178757,#178758,#178759,#178760,#178761,#178762,
#178763,#178764,#178765),(#178766,#178767,#178768,#178769,#178770,#178771,
#178772,#178773,#178774),(#178775,#178776,#178777,#178778,#178779,#178780,
#178781,#178782,#178783),(#178784,#178785,#178786,#178787,#178788,#178789,
#178790,#178791,#178792),(#178793,#178794,#178795,#178796,#178797,#178798,
#178799,#178800,#178801),(#178802,#178803,#178804,#178805,#178806,#178807,
#178808,#178809,#178810),(#178811,#178812,#178813,#178814,#178815,#178816,
#178817,#178818,#178819),(#178820,#178821,#178822,#178823,#178824,#178825,
#178826,#178827,#178828),(#178829,#178830,#178831,#178832,#178833,#178834,
#178835,#178836,#178837),(#178838,#178839,#178840,#178841,#178842,#178843,
#178844,#178845,#178846),(#178847,#178848,#178849,#178850,#178851,#178852,
#178853,#178854,#178855),(#178856,#178857,#178858,#178859,#178860,#178861,
#178862,#178863,#178864),(#178865,#178866,#178867,#178868,#178869,#178870,
#178871,#178872,#178873),(#178874,#178875,#178876,#178877,#178878,#178879,
#178880,#178881,#178882),(#178883,#178884,#178885,#178886,#178887,#178888,
#178889,#178890,#178891),(#178892,#178893,#178894,#178895,#178896,#178897,
#178898,#178899,#178900),(#178901,#178902,#178903,#178904,#178905,#178906,
#178907,#178908,#178909),(#178910,#178911,#178912,#178913,#178914,#178915,
#178916,#178917,#178918),(#178919,#178920,#178921,#178922,#178923,#178924,
#178925,#178926,#178927),(#178928,#178929,#178930,#178931,#178932,#178933,
#178934,#178935,#178936),(#178937,#178938,#178939,#178940,#178941,#178942,
#178943,#178944,#178945),(#178946,#178947,#178948,#178949,#178950,#178951,
#178952,#178953,#178954),(#178955,#178956,#178957,#178958,#178959,#178960,
#178961,#178962,#178963),(#178964,#178965,#178966,#178967,#178968,#178969,
#178970,#178971,#178972),(#178973,#178974,#178975,#178976,#178977,#178978,
#178979,#178980,#178981),(#178982,#178983,#178984,#178985,#178986,#178987,
#178988,#178989,#178990),(#178991,#178992,#178993,#178994,#178995,#178996,
#178997,#178998,#178999),(#179000,#179001,#179002,#179003,#179004,#179005,
#179006,#179007,#179008),(#179009,#179010,#179011,#179012,#179013,#179014,
#179015,#179016,#179017),(#179018,#179019,#179020,#179021,#179022,#179023,
#179024,#179025,#179026),(#179027,#179028,#179029,#179030,#179031,#179032,
#179033,#179034,#179035),(#179036,#179037,#179038,#179039,#179040,#179041,
#179042,#179043,#179044),(#179045,#179046,#179047,#179048,#179049,#179050,
#179051,#179052,#179053),(#179054,#179055,#179056,#179057,#179058,#179059,
#179060,#179061,#179062),(#179063,#179064,#179065,#179066,#179067,#179068,
#179069,#179070,#179071),(#179072,#179073,#179074,#179075,#179076,#179077,
#179078,#179079,#179080),(#179081,#179082,#179083,#179084,#179085,#179086,
#179087,#179088,#179089),(#179090,#179091,#179092,#179093,#179094,#179095,
#179096,#179097,#179098),(#179099,#179100,#179101,#179102,#179103,#179104,
#179105,#179106,#179107),(#179108,#179109,#179110,#179111,#179112,#179113,
#179114,#179115,#179116),(#179117,#179118,#179119,#179120,#179121,#179122,
#179123,#179124,#179125),(#179126,#179127,#179128,#179129,#179130,#179131,
#179132,#179133,#179134),(#179135,#179136,#179137,#179138,#179139,#179140,
#179141,#179142,#179143),(#179144,#179145,#179146,#179147,#179148,#179149,
#179150,#179151,#179152),(#179153,#179154,#179155,#179156,#179157,#179158,
#179159,#179160,#179161),(#179162,#179163,#179164,#179165,#179166,#179167,
#179168,#179169,#179170),(#179171,#179172,#179173,#179174,#179175,#179176,
#179177,#179178,#179179),(#179180,#179181,#179182,#179183,#179184,#179185,
#179186,#179187,#179188),(#179189,#179190,#179191,#179192,#179193,#179194,
#179195,#179196,#179197),(#179198,#179199,#179200,#179201,#179202,#179203,
#179204,#179205,#179206),(#179207,#179208,#179209,#179210,#179211,#179212,
#179213,#179214,#179215),(#179216,#179217,#179218,#179219,#179220,#179221,
#179222,#179223,#179224),(#179225,#179226,#179227,#179228,#179229,#179230,
#179231,#179232,#179233),(#179234,#179235,#179236,#179237,#179238,#179239,
#179240,#179241,#179242),(#179243,#179244,#179245,#179246,#179247,#179248,
#179249,#179250,#179251),(#179252,#179253,#179254,#179255,#179256,#179257,
#179258,#179259,#179260),(#179261,#179262,#179263,#179264,#179265,#179266,
#179267,#179268,#179269),(#179270,#179271,#179272,#179273,#179274,#179275,
#179276,#179277,#179278),(#179279,#179280,#179281,#179282,#179283,#179284,
#179285,#179286,#179287),(#179288,#179289,#179290,#179291,#179292,#179293,
#179294,#179295,#179296),(#179297,#179298,#179299,#179300,#179301,#179302,
#179303,#179304,#179305),(#179306,#179307,#179308,#179309,#179310,#179311,
#179312,#179313,#179314),(#179315,#179316,#179317,#179318,#179319,#179320,
#179321,#179322,#179323),(#179324,#179325,#179326,#179327,#179328,#179329,
#179330,#179331,#179332),(#179333,#179334,#179335,#179336,#179337,#179338,
#179339,#179340,#179341),(#179342,#179343,#179344,#179345,#179346,#179347,
#179348,#179349,#179350),(#179351,#179352,#179353,#179354,#179355,#179356,
#179357,#179358,#179359),(#179360,#179361,#179362,#179363,#179364,#179365,
#179366,#179367,#179368),(#179369,#179370,#179371,#179372,#179373,#179374,
#179375,#179376,#179377),(#179378,#179379,#179380,#179381,#179382,#179383,
#179384,#179385,#179386),(#179387,#179388,#179389,#179390,#179391,#179392,
#179393,#179394,#179395),(#179396,#179397,#179398,#179399,#179400,#179401,
#179402,#179403,#179404),(#179405,#179406,#179407,#179408,#179409,#179410,
#179411,#179412,#179413),(#179414,#179415,#179416,#179417,#179418,#179419,
#179420,#179421,#179422),(#179423,#179424,#179425,#179426,#179427,#179428,
#179429,#179430,#179431),(#179432,#179433,#179434,#179435,#179436,#179437,
#179438,#179439,#179440),(#179441,#179442,#179443,#179444,#179445,#179446,
#179447,#179448,#179449),(#179450,#179451,#179452,#179453,#179454,#179455,
#179456,#179457,#179458),(#179459,#179460,#179461,#179462,#179463,#179464,
#179465,#179466,#179467),(#179468,#179469,#179470,#179471,#179472,#179473,
#179474,#179475,#179476),(#179477,#179478,#179479,#179480,#179481,#179482,
#179483,#179484,#179485),(#179486,#179487,#179488,#179489,#179490,#179491,
#179492,#179493,#179494),(#179495,#179496,#179497,#179498,#179499,#179500,
#179501,#179502,#179503),(#179504,#179505,#179506,#179507,#179508,#179509,
#179510,#179511,#179512),(#179513,#179514,#179515,#179516,#179517,#179518,
#179519,#179520,#179521),(#179522,#179523,#179524,#179525,#179526,#179527,
#179528,#179529,#179530),(#179531,#179532,#179533,#179534,#179535,#179536,
#179537,#179538,#179539),(#179540,#179541,#179542,#179543,#179544,#179545,
#179546,#179547,#179548),(#179549,#179550,#179551,#179552,#179553,#179554,
#179555,#179556,#179557),(#179558,#179559,#179560,#179561,#179562,#179563,
#179564,#179565,#179566),(#179567,#179568,#179569,#179570,#179571,#179572,
#179573,#179574,#179575),(#179576,#179577,#179578,#179579,#179580,#179581,
#179582,#179583,#179584),(#179585,#179586,#179587,#179588,#179589,#179590,
#179591,#179592,#179593),(#179594,#179595,#179596,#179597,#179598,#179599,
#179600,#179601,#179602),(#179603,#179604,#179605,#179606,#179607,#179608,
#179609,#179610,#179611),(#179612,#179613,#179614,#179615,#179616,#179617,
#179618,#179619,#179620),(#179621,#179622,#179623,#179624,#179625,#179626,
#179627,#179628,#179629),(#179630,#179631,#179632,#179633,#179634,#179635,
#179636,#179637,#179638),(#179639,#179640,#179641,#179642,#179643,#179644,
#179645,#179646,#179647),(#179648,#179649,#179650,#179651,#179652,#179653,
#179654,#179655,#179656),(#179657,#179658,#179659,#179660,#179661,#179662,
#179663,#179664,#179665),(#179666,#179667,#179668,#179669,#179670,#179671,
#179672,#179673,#179674),(#179675,#179676,#179677,#179678,#179679,#179680,
#179681,#179682,#179683),(#179684,#179685,#179686,#179687,#179688,#179689,
#179690,#179691,#179692),(#179693,#179694,#179695,#179696,#179697,#179698,
#179699,#179700,#179701),(#179702,#179703,#179704,#179705,#179706,#179707,
#179708,#179709,#179710),(#179711,#179712,#179713,#179714,#179715,#179716,
#179717,#179718,#179719),(#179720,#179721,#179722,#179723,#179724,#179725,
#179726,#179727,#179728),(#179729,#179730,#179731,#179732,#179733,#179734,
#179735,#179736,#179737),(#179738,#179739,#179740,#179741,#179742,#179743,
#179744,#179745,#179746),(#179747,#179748,#179749,#179750,#179751,#179752,
#179753,#179754,#179755),(#179756,#179757,#179758,#179759,#179760,#179761,
#179762,#179763,#179764),(#179765,#179766,#179767,#179768,#179769,#179770,
#179771,#179772,#179773),(#179774,#179775,#179776,#179777,#179778,#179779,
#179780,#179781,#179782),(#179783,#179784,#179785,#179786,#179787,#179788,
#179789,#179790,#179791),(#179792,#179793,#179794,#179795,#179796,#179797,
#179798,#179799,#179800),(#179801,#179802,#179803,#179804,#179805,#179806,
#179807,#179808,#179809),(#179810,#179811,#179812,#179813,#179814,#179815,
#179816,#179817,#179818),(#179819,#179820,#179821,#179822,#179823,#179824,
#179825,#179826,#179827),(#179828,#179829,#179830,#179831,#179832,#179833,
#179834,#179835,#179836),(#179837,#179838,#179839,#179840,#179841,#179842,
#179843,#179844,#179845),(#179846,#179847,#179848,#179849,#179850,#179851,
#179852,#179853,#179854),(#179855,#179856,#179857,#179858,#179859,#179860,
#179861,#179862,#179863),(#179864,#179865,#179866,#179867,#179868,#179869,
#179870,#179871,#179872),(#179873,#179874,#179875,#179876,#179877,#179878,
#179879,#179880,#179881),(#179882,#179883,#179884,#179885,#179886,#179887,
#179888,#179889,#179890),(#179891,#179892,#179893,#179894,#179895,#179896,
#179897,#179898,#179899),(#179900,#179901,#179902,#179903,#179904,#179905,
#179906,#179907,#179908),(#179909,#179910,#179911,#179912,#179913,#179914,
#179915,#179916,#179917),(#179918,#179919,#179920,#179921,#179922,#179923,
#179924,#179925,#179926),(#179927,#179928,#179929,#179930,#179931,#179932,
#179933,#179934,#179935),(#179936,#179937,#179938,#179939,#179940,#179941,
#179942,#179943,#179944),(#179945,#179946,#179947,#179948,#179949,#179950,
#179951,#179952,#179953),(#179954,#179955,#179956,#179957,#179958,#179959,
#179960,#179961,#179962),(#179963,#179964,#179965,#179966,#179967,#179968,
#179969,#179970,#179971),(#179972,#179973,#179974,#179975,#179976,#179977,
#179978,#179979,#179980),(#179981,#179982,#179983,#179984,#179985,#179986,
#179987,#179988,#179989),(#179990,#179991,#179992,#179993,#179994,#179995,
#179996,#179997,#179998),(#179999,#180000,#180001,#180002,#180003,#180004,
#180005,#180006,#180007),(#180008,#180009,#180010,#180011,#180012,#180013,
#180014,#180015,#180016),(#180017,#180018,#180019,#180020,#180021,#180022,
#180023,#180024,#180025),(#180026,#180027,#180028,#180029,#180030,#180031,
#180032,#180033,#180034),(#180035,#180036,#180037,#180038,#180039,#180040,
#180041,#180042,#180043),(#180044,#180045,#180046,#180047,#180048,#180049,
#180050,#180051,#180052),(#180053,#180054,#180055,#180056,#180057,#180058,
#180059,#180060,#180061),(#180062,#180063,#180064,#180065,#180066,#180067,
#180068,#180069,#180070),(#180071,#180072,#180073,#180074,#180075,#180076,
#180077,#180078,#180079),(#180080,#180081,#180082,#180083,#180084,#180085,
#180086,#180087,#180088),(#180089,#180090,#180091,#180092,#180093,#180094,
#180095,#180096,#180097),(#180098,#180099,#180100,#180101,#180102,#180103,
#180104,#180105,#180106),(#180107,#180108,#180109,#180110,#180111,#180112,
#180113,#180114,#180115),(#180116,#180117,#180118,#180119,#180120,#180121,
#180122,#180123,#180124),(#180125,#180126,#180127,#180128,#180129,#180130,
#180131,#180132,#180133),(#180134,#180135,#180136,#180137,#180138,#180139,
#180140,#180141,#180142),(#180143,#180144,#180145,#180146,#180147,#180148,
#180149,#180150,#180151),(#180152,#180153,#180154,#180155,#180156,#180157,
#180158,#180159,#180160),(#180161,#180162,#180163,#180164,#180165,#180166,
#180167,#180168,#180169),(#180170,#180171,#180172,#180173,#180174,#180175,
#180176,#180177,#180178),(#180179,#180180,#180181,#180182,#180183,#180184,
#180185,#180186,#180187),(#180188,#180189,#180190,#180191,#180192,#180193,
#180194,#180195,#180196),(#180197,#180198,#180199,#180200,#180201,#180202,
#180203,#180204,#180205),(#180206,#180207,#180208,#180209,#180210,#180211,
#180212,#180213,#180214),(#180215,#180216,#180217,#180218,#180219,#180220,
#180221,#180222,#180223),(#180224,#180225,#180226,#180227,#180228,#180229,
#180230,#180231,#180232),(#180233,#180234,#180235,#180236,#180237,#180238,
#180239,#180240,#180241),(#180242,#180243,#180244,#180245,#180246,#180247,
#180248,#180249,#180250),(#180251,#180252,#180253,#180254,#180255,#180256,
#180257,#180258,#180259),(#180260,#180261,#180262,#180263,#180264,#180265,
#180266,#180267,#180268),(#180269,#180270,#180271,#180272,#180273,#180274,
#180275,#180276,#180277),(#180278,#180279,#180280,#180281,#180282,#180283,
#180284,#180285,#180286),(#180287,#180288,#180289,#180290,#180291,#180292,
#180293,#180294,#180295),(#180296,#180297,#180298,#180299,#180300,#180301,
#180302,#180303,#180304),(#180305,#180306,#180307,#180308,#180309,#180310,
#180311,#180312,#180313),(#180314,#180315,#180316,#180317,#180318,#180319,
#180320,#180321,#180322),(#180323,#180324,#180325,#180326,#180327,#180328,
#180329,#180330,#180331),(#180332,#180333,#180334,#180335,#180336,#180337,
#180338,#180339,#180340),(#180341,#180342,#180343,#180344,#180345,#180346,
#180347,#180348,#180349),(#180350,#180351,#180352,#180353,#180354,#180355,
#180356,#180357,#180358),(#180359,#180360,#180361,#180362,#180363,#180364,
#180365,#180366,#180367),(#180368,#180369,#180370,#180371,#180372,#180373,
#180374,#180375,#180376),(#180377,#180378,#180379,#180380,#180381,#180382,
#180383,#180384,#180385),(#180386,#180387,#180388,#180389,#180390,#180391,
#180392,#180393,#180394),(#180395,#180396,#180397,#180398,#180399,#180400,
#180401,#180402,#180403),(#180404,#180405,#180406,#180407,#180408,#180409,
#180410,#180411,#180412),(#180413,#180414,#180415,#180416,#180417,#180418,
#180419,#180420,#180421),(#180422,#180423,#180424,#180425,#180426,#180427,
#180428,#180429,#180430),(#180431,#180432,#180433,#180434,#180435,#180436,
#180437,#180438,#180439),(#180440,#180441,#180442,#180443,#180444,#180445,
#180446,#180447,#180448),(#180449,#180450,#180451,#180452,#180453,#180454,
#180455,#180456,#180457),(#180458,#180459,#180460,#180461,#180462,#180463,
#180464,#180465,#180466),(#180467,#180468,#180469,#180470,#180471,#180472,
#180473,#180474,#180475),(#180476,#180477,#180478,#180479,#180480,#180481,
#180482,#180483,#180484),(#180485,#180486,#180487,#180488,#180489,#180490,
#180491,#180492,#180493),(#180494,#180495,#180496,#180497,#180498,#180499,
#180500,#180501,#180502),(#180503,#180504,#180505,#180506,#180507,#180508,
#180509,#180510,#180511),(#180512,#180513,#180514,#180515,#180516,#180517,
#180518,#180519,#180520),(#180521,#180522,#180523,#180524,#180525,#180526,
#180527,#180528,#180529),(#180530,#180531,#180532,#180533,#180534,#180535,
#180536,#180537,#180538),(#180539,#180540,#180541,#180542,#180543,#180544,
#180545,#180546,#180547),(#180548,#180549,#180550,#180551,#180552,#180553,
#180554,#180555,#180556),(#180557,#180558,#180559,#180560,#180561,#180562,
#180563,#180564,#180565),(#180566,#180567,#180568,#180569,#180570,#180571,
#180572,#180573,#180574),(#180575,#180576,#180577,#180578,#180579,#180580,
#180581,#180582,#180583),(#180584,#180585,#180586,#180587,#180588,#180589,
#180590,#180591,#180592),(#180593,#180594,#180595,#180596,#180597,#180598,
#180599,#180600,#180601),(#180602,#180603,#180604,#180605,#180606,#180607,
#180608,#180609,#180610),(#180611,#180612,#180613,#180614,#180615,#180616,
#180617,#180618,#180619),(#180620,#180621,#180622,#180623,#180624,#180625,
#180626,#180627,#180628),(#180629,#180630,#180631,#180632,#180633,#180634,
#180635,#180636,#180637),(#180638,#180639,#180640,#180641,#180642,#180643,
#180644,#180645,#180646),(#180647,#180648,#180649,#180650,#180651,#180652,
#180653,#180654,#180655),(#180656,#180657,#180658,#180659,#180660,#180661,
#180662,#180663,#180664),(#180665,#180666,#180667,#180668,#180669,#180670,
#180671,#180672,#180673),(#180674,#180675,#180676,#180677,#180678,#180679,
#180680,#180681,#180682),(#180683,#180684,#180685,#180686,#180687,#180688,
#180689,#180690,#180691),(#180692,#180693,#180694,#180695,#180696,#180697,
#180698,#180699,#180700),(#180701,#180702,#180703,#180704,#180705,#180706,
#180707,#180708,#180709),(#180710,#180711,#180712,#180713,#180714,#180715,
#180716,#180717,#180718),(#180719,#180720,#180721,#180722,#180723,#180724,
#180725,#180726,#180727),(#180728,#180729,#180730,#180731,#180732,#180733,
#180734,#180735,#180736),(#180737,#180738,#180739,#180740,#180741,#180742,
#180743,#180744,#180745),(#180746,#180747,#180748,#180749,#180750,#180751,
#180752,#180753,#180754),(#180755,#180756,#180757,#180758,#180759,#180760,
#180761,#180762,#180763),(#180764,#180765,#180766,#180767,#180768,#180769,
#180770,#180771,#180772),(#180773,#180774,#180775,#180776,#180777,#180778,
#180779,#180780,#180781),(#180782,#180783,#180784,#180785,#180786,#180787,
#180788,#180789,#180790),(#180791,#180792,#180793,#180794,#180795,#180796,
#180797,#180798,#180799),(#180800,#180801,#180802,#180803,#180804,#180805,
#180806,#180807,#180808),(#180809,#180810,#180811,#180812,#180813,#180814,
#180815,#180816,#180817),(#180818,#180819,#180820,#180821,#180822,#180823,
#180824,#180825,#180826),(#180827,#180828,#180829,#180830,#180831,#180832,
#180833,#180834,#180835),(#180836,#180837,#180838,#180839,#180840,#180841,
#180842,#180843,#180844),(#180845,#180846,#180847,#180848,#180849,#180850,
#180851,#180852,#180853),(#180854,#180855,#180856,#180857,#180858,#180859,
#180860,#180861,#180862),(#180863,#180864,#180865,#180866,#180867,#180868,
#180869,#180870,#180871),(#180872,#180873,#180874,#180875,#180876,#180877,
#180878,#180879,#180880),(#180881,#180882,#180883,#180884,#180885,#180886,
#180887,#180888,#180889),(#180890,#180891,#180892,#180893,#180894,#180895,
#180896,#180897,#180898),(#180899,#180900,#180901,#180902,#180903,#180904,
#180905,#180906,#180907),(#180908,#180909,#180910,#180911,#180912,#180913,
#180914,#180915,#180916),(#180917,#180918,#180919,#180920,#180921,#180922,
#180923,#180924,#180925),(#180926,#180927,#180928,#180929,#180930,#180931,
#180932,#180933,#180934),(#180935,#180936,#180937,#180938,#180939,#180940,
#180941,#180942,#180943),(#180944,#180945,#180946,#180947,#180948,#180949,
#180950,#180951,#180952),(#180953,#180954,#180955,#180956,#180957,#180958,
#180959,#180960,#180961),(#180962,#180963,#180964,#180965,#180966,#180967,
#180968,#180969,#180970),(#180971,#180972,#180973,#180974,#180975,#180976,
#180977,#180978,#180979),(#180980,#180981,#180982,#180983,#180984,#180985,
#180986,#180987,#180988),(#180989,#180990,#180991,#180992,#180993,#180994,
#180995,#180996,#180997),(#180998,#180999,#181000,#181001,#181002,#181003,
#181004,#181005,#181006),(#181007,#181008,#181009,#181010,#181011,#181012,
#181013,#181014,#181015),(#181016,#181017,#181018,#181019,#181020,#181021,
#181022,#181023,#181024),(#181025,#181026,#181027,#181028,#181029,#181030,
#181031,#181032,#181033),(#181034,#181035,#181036,#181037,#181038,#181039,
#181040,#181041,#181042),(#181043,#181044,#181045,#181046,#181047,#181048,
#181049,#181050,#181051),(#181052,#181053,#181054,#181055,#181056,#181057,
#181058,#181059,#181060),(#181061,#181062,#181063,#181064,#181065,#181066,
#181067,#181068,#181069),(#181070,#181071,#181072,#181073,#181074,#181075,
#181076,#181077,#181078),(#181079,#181080,#181081,#181082,#181083,#181084,
#181085,#181086,#181087),(#181088,#181089,#181090,#181091,#181092,#181093,
#181094,#181095,#181096),(#181097,#181098,#181099,#181100,#181101,#181102,
#181103,#181104,#181105),(#181106,#181107,#181108,#181109,#181110,#181111,
#181112,#181113,#181114),(#181115,#181116,#181117,#181118,#181119,#181120,
#181121,#181122,#181123),(#181124,#181125,#181126,#181127,#181128,#181129,
#181130,#181131,#181132),(#181133,#181134,#181135,#181136,#181137,#181138,
#181139,#181140,#181141),(#181142,#181143,#181144,#181145,#181146,#181147,
#181148,#181149,#181150),(#181151,#181152,#181153,#181154,#181155,#181156,
#181157,#181158,#181159),(#181160,#181161,#181162,#181163,#181164,#181165,
#181166,#181167,#181168),(#181169,#181170,#181171,#181172,#181173,#181174,
#181175,#181176,#181177),(#181178,#181179,#181180,#181181,#181182,#181183,
#181184,#181185,#181186),(#181187,#181188,#181189,#181190,#181191,#181192,
#181193,#181194,#181195),(#181196,#181197,#181198,#181199,#181200,#181201,
#181202,#181203,#181204),(#181205,#181206,#181207,#181208,#181209,#181210,
#181211,#181212,#181213),(#181214,#181215,#181216,#181217,#181218,#181219,
#181220,#181221,#181222),(#181223,#181224,#181225,#181226,#181227,#181228,
#181229,#181230,#181231),(#181232,#181233,#181234,#181235,#181236,#181237,
#181238,#181239,#181240),(#181241,#181242,#181243,#181244,#181245,#181246,
#181247,#181248,#181249),(#181250,#181251,#181252,#181253,#181254,#181255,
#181256,#181257,#181258),(#181259,#181260,#181261,#181262,#181263,#181264,
#181265,#181266,#181267),(#181268,#181269,#181270,#181271,#181272,#181273,
#181274,#181275,#181276),(#181277,#181278,#181279,#181280,#181281,#181282,
#181283,#181284,#181285),(#181286,#181287,#181288,#181289,#181290,#181291,
#181292,#181293,#181294),(#181295,#181296,#181297,#181298,#181299,#181300,
#181301,#181302,#181303),(#181304,#181305,#181306,#181307,#181308,#181309,
#181310,#181311,#181312),(#181313,#181314,#181315,#181316,#181317,#181318,
#181319,#181320,#181321),(#181322,#181323,#181324,#181325,#181326,#181327,
#181328,#181329,#181330),(#181331,#181332,#181333,#181334,#181335,#181336,
#181337,#181338,#181339),(#181340,#181341,#181342,#181343,#181344,#181345,
#181346,#181347,#181348),(#181349,#181350,#181351,#181352,#181353,#181354,
#181355,#181356,#181357),(#181358,#181359,#181360,#181361,#181362,#181363,
#181364,#181365,#181366),(#181367,#181368,#181369,#181370,#181371,#181372,
#181373,#181374,#181375),(#181376,#181377,#181378,#181379,#181380,#181381,
#181382,#181383,#181384),(#181385,#181386,#181387,#181388,#181389,#181390,
#181391,#181392,#181393),(#181394,#181395,#181396,#181397,#181398,#181399,
#181400,#181401,#181402),(#181403,#181404,#181405,#181406,#181407,#181408,
#181409,#181410,#181411),(#181412,#181413,#181414,#181415,#181416,#181417,
#181418,#181419,#181420),(#181421,#181422,#181423,#181424,#181425,#181426,
#181427,#181428,#181429),(#181430,#181431,#181432,#181433,#181434,#181435,
#181436,#181437,#181438),(#181439,#181440,#181441,#181442,#181443,#181444,
#181445,#181446,#181447),(#181448,#181449,#181450,#181451,#181452,#181453,
#181454,#181455,#181456),(#181457,#181458,#181459,#181460,#181461,#181462,
#181463,#181464,#181465),(#181466,#181467,#181468,#181469,#181470,#181471,
#181472,#181473,#181474),(#181475,#181476,#181477,#181478,#181479,#181480,
#181481,#181482,#181483),(#181484,#181485,#181486,#181487,#181488,#181489,
#181490,#181491,#181492),(#181493,#181494,#181495,#181496,#181497,#181498,
#181499,#181500,#181501),(#181502,#181503,#181504,#181505,#181506,#181507,
#181508,#181509,#181510),(#181511,#181512,#181513,#181514,#181515,#181516,
#181517,#181518,#181519),(#181520,#181521,#181522,#181523,#181524,#181525,
#181526,#181527,#181528),(#181529,#181530,#181531,#181532,#181533,#181534,
#181535,#181536,#181537),(#181538,#181539,#181540,#181541,#181542,#181543,
#181544,#181545,#181546),(#181547,#181548,#181549,#181550,#181551,#181552,
#181553,#181554,#181555),(#181556,#181557,#181558,#181559,#181560,#181561,
#181562,#181563,#181564),(#181565,#181566,#181567,#181568,#181569,#181570,
#181571,#181572,#181573),(#181574,#181575,#181576,#181577,#181578,#181579,
#181580,#181581,#181582),(#181583,#181584,#181585,#181586,#181587,#181588,
#181589,#181590,#181591),(#181592,#181593,#181594,#181595,#181596,#181597,
#181598,#181599,#181600),(#181601,#181602,#181603,#181604,#181605,#181606,
#181607,#181608,#181609),(#181610,#181611,#181612,#181613,#181614,#181615,
#181616,#181617,#181618),(#181619,#181620,#181621,#181622,#181623,#181624,
#181625,#181626,#181627),(#181628,#181629,#181630,#181631,#181632,#181633,
#181634,#181635,#181636),(#181637,#181638,#181639,#181640,#181641,#181642,
#181643,#181644,#181645),(#181646,#181647,#181648,#181649,#181650,#181651,
#181652,#181653,#181654),(#181655,#181656,#181657,#181658,#181659,#181660,
#181661,#181662,#181663),(#181664,#181665,#181666,#181667,#181668,#181669,
#181670,#181671,#181672),(#181673,#181674,#181675,#181676,#181677,#181678,
#181679,#181680,#181681),(#181682,#181683,#181684,#181685,#181686,#181687,
#181688,#181689,#181690),(#181691,#181692,#181693,#181694,#181695,#181696,
#181697,#181698,#181699),(#181700,#181701,#181702,#181703,#181704,#181705,
#181706,#181707,#181708),(#181709,#181710,#181711,#181712,#181713,#181714,
#181715,#181716,#181717),(#181718,#181719,#181720,#181721,#181722,#181723,
#181724,#181725,#181726),(#181727,#181728,#181729,#181730,#181731,#181732,
#181733,#181734,#181735),(#181736,#181737,#181738,#181739,#181740,#181741,
#181742,#181743,#181744),(#181745,#181746,#181747,#181748,#181749,#181750,
#181751,#181752,#181753),(#181754,#181755,#181756,#181757,#181758,#181759,
#181760,#181761,#181762),(#181763,#181764,#181765,#181766,#181767,#181768,
#181769,#181770,#181771),(#181772,#181773,#181774,#181775,#181776,#181777,
#181778,#181779,#181780),(#181781,#181782,#181783,#181784,#181785,#181786,
#181787,#181788,#181789),(#181790,#181791,#181792,#181793,#181794,#181795,
#181796,#181797,#181798),(#181799,#181800,#181801,#181802,#181803,#181804,
#181805,#181806,#181807),(#181808,#181809,#181810,#181811,#181812,#181813,
#181814,#181815,#181816),(#181817,#181818,#181819,#181820,#181821,#181822,
#181823,#181824,#181825),(#181826,#181827,#181828,#181829,#181830,#181831,
#181832,#181833,#181834),(#181835,#181836,#181837,#181838,#181839,#181840,
#181841,#181842,#181843),(#181844,#181845,#181846,#181847,#181848,#181849,
#181850,#181851,#181852),(#181853,#181854,#181855,#181856,#181857,#181858,
#181859,#181860,#181861),(#181862,#181863,#181864,#181865,#181866,#181867,
#181868,#181869,#181870),(#181871,#181872,#181873,#181874,#181875,#181876,
#181877,#181878,#181879),(#181880,#181881,#181882,#181883,#181884,#181885,
#181886,#181887,#181888),(#181889,#181890,#181891,#181892,#181893,#181894,
#181895,#181896,#181897),(#181898,#181899,#181900,#181901,#181902,#181903,
#181904,#181905,#181906),(#181907,#181908,#181909,#181910,#181911,#181912,
#181913,#181914,#181915),(#181916,#181917,#181918,#181919,#181920,#181921,
#181922,#181923,#181924),(#181925,#181926,#181927,#181928,#181929,#181930,
#181931,#181932,#181933),(#181934,#181935,#181936,#181937,#181938,#181939,
#181940,#181941,#181942),(#181943,#181944,#181945,#181946,#181947,#181948,
#181949,#181950,#181951),(#181952,#181953,#181954,#181955,#181956,#181957,
#181958,#181959,#181960),(#181961,#181962,#181963,#181964,#181965,#181966,
#181967,#181968,#181969),(#181970,#181971,#181972,#181973,#181974,#181975,
#181976,#181977,#181978),(#181979,#181980,#181981,#181982,#181983,#181984,
#181985,#181986,#181987),(#181988,#181989,#181990,#181991,#181992,#181993,
#181994,#181995,#181996),(#181997,#181998,#181999,#182000,#182001,#182002,
#182003,#182004,#182005),(#182006,#182007,#182008,#182009,#182010,#182011,
#182012,#182013,#182014),(#182015,#182016,#182017,#182018,#182019,#182020,
#182021,#182022,#182023),(#182024,#182025,#182026,#182027,#182028,#182029,
#182030,#182031,#182032),(#182033,#182034,#182035,#182036,#182037,#182038,
#182039,#182040,#182041),(#182042,#182043,#182044,#182045,#182046,#182047,
#182048,#182049,#182050),(#182051,#182052,#182053,#182054,#182055,#182056,
#182057,#182058,#182059),(#182060,#182061,#182062,#182063,#182064,#182065,
#182066,#182067,#182068),(#182069,#182070,#182071,#182072,#182073,#182074,
#182075,#182076,#182077),(#182078,#182079,#182080,#182081,#182082,#182083,
#182084,#182085,#182086),(#182087,#182088,#182089,#182090,#182091,#182092,
#182093,#182094,#182095),(#182096,#182097,#182098,#182099,#182100,#182101,
#182102,#182103,#182104),(#182105,#182106,#182107,#182108,#182109,#182110,
#182111,#182112,#182113),(#182114,#182115,#182116,#182117,#182118,#182119,
#182120,#182121,#182122),(#182123,#182124,#182125,#182126,#182127,#182128,
#182129,#182130,#182131),(#182132,#182133,#182134,#182135,#182136,#182137,
#182138,#182139,#182140),(#182141,#182142,#182143,#182144,#182145,#182146,
#182147,#182148,#182149),(#182150,#182151,#182152,#182153,#182154,#182155,
#182156,#182157,#182158),(#182159,#182160,#182161,#182162,#182163,#182164,
#182165,#182166,#182167),(#182168,#182169,#182170,#182171,#182172,#182173,
#182174,#182175,#182176),(#182177,#182178,#182179,#182180,#182181,#182182,
#182183,#182184,#182185),(#182186,#182187,#182188,#182189,#182190,#182191,
#182192,#182193,#182194),(#182195,#182196,#182197,#182198,#182199,#182200,
#182201,#182202,#182203),(#182204,#182205,#182206,#182207,#182208,#182209,
#182210,#182211,#182212),(#182213,#182214,#182215,#182216,#182217,#182218,
#182219,#182220,#182221),(#182222,#182223,#182224,#182225,#182226,#182227,
#182228,#182229,#182230),(#182231,#182232,#182233,#182234,#182235,#182236,
#182237,#182238,#182239),(#182240,#182241,#182242,#182243,#182244,#182245,
#182246,#182247,#182248),(#182249,#182250,#182251,#182252,#182253,#182254,
#182255,#182256,#182257),(#182258,#182259,#182260,#182261,#182262,#182263,
#182264,#182265,#182266),(#182267,#182268,#182269,#182270,#182271,#182272,
#182273,#182274,#182275),(#182276,#182277,#182278,#182279,#182280,#182281,
#182282,#182283,#182284),(#182285,#182286,#182287,#182288,#182289,#182290,
#182291,#182292,#182293),(#182294,#182295,#182296,#182297,#182298,#182299,
#182300,#182301,#182302),(#182303,#182304,#182305,#182306,#182307,#182308,
#182309,#182310,#182311),(#182312,#182313,#182314,#182315,#182316,#182317,
#182318,#182319,#182320),(#182321,#182322,#182323,#182324,#182325,#182326,
#182327,#182328,#182329),(#182330,#182331,#182332,#182333,#182334,#182335,
#182336,#182337,#182338),(#182339,#182340,#182341,#182342,#182343,#182344,
#182345,#182346,#182347),(#182348,#182349,#182350,#182351,#182352,#182353,
#182354,#182355,#182356),(#182357,#182358,#182359,#182360,#182361,#182362,
#182363,#182364,#182365),(#182366,#182367,#182368,#182369,#182370,#182371,
#182372,#182373,#182374),(#182375,#182376,#182377,#182378,#182379,#182380,
#182381,#182382,#182383),(#182384,#182385,#182386,#182387,#182388,#182389,
#182390,#182391,#182392),(#182393,#182394,#182395,#182396,#182397,#182398,
#182399,#182400,#182401),(#182402,#182403,#182404,#182405,#182406,#182407,
#182408,#182409,#182410),(#182411,#182412,#182413,#182414,#182415,#182416,
#182417,#182418,#182419),(#182420,#182421,#182422,#182423,#182424,#182425,
#182426,#182427,#182428),(#182429,#182430,#182431,#182432,#182433,#182434,
#182435,#182436,#182437),(#182438,#182439,#182440,#182441,#182442,#182443,
#182444,#182445,#182446),(#182447,#182448,#182449,#182450,#182451,#182452,
#182453,#182454,#182455),(#182456,#182457,#182458,#182459,#182460,#182461,
#182462,#182463,#182464),(#182465,#182466,#182467,#182468,#182469,#182470,
#182471,#182472,#182473),(#182474,#182475,#182476,#182477,#182478,#182479,
#182480,#182481,#182482),(#182483,#182484,#182485,#182486,#182487,#182488,
#182489,#182490,#182491),(#182492,#182493,#182494,#182495,#182496,#182497,
#182498,#182499,#182500),(#182501,#182502,#182503,#182504,#182505,#182506,
#182507,#182508,#182509),(#182510,#182511,#182512,#182513,#182514,#182515,
#182516,#182517,#182518),(#182519,#182520,#182521,#182522,#182523,#182524,
#182525,#182526,#182527),(#182528,#182529,#182530,#182531,#182532,#182533,
#182534,#182535,#182536),(#182537,#182538,#182539,#182540,#182541,#182542,
#182543,#182544,#182545),(#182546,#182547,#182548,#182549,#182550,#182551,
#182552,#182553,#182554),(#182555,#182556,#182557,#182558,#182559,#182560,
#182561,#182562,#182563),(#182564,#182565,#182566,#182567,#182568,#182569,
#182570,#182571,#182572),(#182573,#182574,#182575,#182576,#182577,#182578,
#182579,#182580,#182581),(#182582,#182583,#182584,#182585,#182586,#182587,
#182588,#182589,#182590),(#182591,#182592,#182593,#182594,#182595,#182596,
#182597,#182598,#182599),(#182600,#182601,#182602,#182603,#182604,#182605,
#182606,#182607,#182608),(#182609,#182610,#182611,#182612,#182613,#182614,
#182615,#182616,#182617),(#182618,#182619,#182620,#182621,#182622,#182623,
#182624,#182625,#182626),(#182627,#182628,#182629,#182630,#182631,#182632,
#182633,#182634,#182635),(#182636,#182637,#182638,#182639,#182640,#182641,
#182642,#182643,#182644),(#182645,#182646,#182647,#182648,#182649,#182650,
#182651,#182652,#182653),(#182654,#182655,#182656,#182657,#182658,#182659,
#182660,#182661,#182662),(#182663,#182664,#182665,#182666,#182667,#182668,
#182669,#182670,#182671),(#182672,#182673,#182674,#182675,#182676,#182677,
#182678,#182679,#182680),(#182681,#182682,#182683,#182684,#182685,#182686,
#182687,#182688,#182689),(#182690,#182691,#182692,#182693,#182694,#182695,
#182696,#182697,#182698),(#182699,#182700,#182701,#182702,#182703,#182704,
#182705,#182706,#182707),(#182708,#182709,#182710,#182711,#182712,#182713,
#182714,#182715,#182716),(#182717,#182718,#182719,#182720,#182721,#182722,
#182723,#182724,#182725),(#182726,#182727,#182728,#182729,#182730,#182731,
#182732,#182733,#182734),(#182735,#182736,#182737,#182738,#182739,#182740,
#182741,#182742,#182743),(#182744,#182745,#182746,#182747,#182748,#182749,
#182750,#182751,#182752),(#182753,#182754,#182755,#182756,#182757,#182758,
#182759,#182760,#182761),(#182762,#182763,#182764,#182765,#182766,#182767,
#182768,#182769,#182770),(#182771,#182772,#182773,#182774,#182775,#182776,
#182777,#182778,#182779),(#182780,#182781,#182782,#182783,#182784,#182785,
#182786,#182787,#182788),(#182789,#182790,#182791,#182792,#182793,#182794,
#182795,#182796,#182797),(#182798,#182799,#182800,#182801,#182802,#182803,
#182804,#182805,#182806),(#182807,#182808,#182809,#182810,#182811,#182812,
#182813,#182814,#182815),(#182816,#182817,#182818,#182819,#182820,#182821,
#182822,#182823,#182824),(#182825,#182826,#182827,#182828,#182829,#182830,
#182831,#182832,#182833),(#182834,#182835,#182836,#182837,#182838,#182839,
#182840,#182841,#182842),(#182843,#182844,#182845,#182846,#182847,#182848,
#182849,#182850,#182851),(#182852,#182853,#182854,#182855,#182856,#182857,
#182858,#182859,#182860),(#182861,#182862,#182863,#182864,#182865,#182866,
#182867,#182868,#182869),(#182870,#182871,#182872,#182873,#182874,#182875,
#182876,#182877,#182878),(#182879,#182880,#182881,#182882,#182883,#182884,
#182885,#182886,#182887),(#182888,#182889,#182890,#182891,#182892,#182893,
#182894,#182895,#182896),(#182897,#182898,#182899,#182900,#182901,#182902,
#182903,#182904,#182905),(#182906,#182907,#182908,#182909,#182910,#182911,
#182912,#182913,#182914),(#182915,#182916,#182917,#182918,#182919,#182920,
#182921,#182922,#182923),(#182924,#182925,#182926,#182927,#182928,#182929,
#182930,#182931,#182932),(#182933,#182934,#182935,#182936,#182937,#182938,
#182939,#182940,#182941),(#182942,#182943,#182944,#182945,#182946,#182947,
#182948,#182949,#182950),(#182951,#182952,#182953,#182954,#182955,#182956,
#182957,#182958,#182959),(#182960,#182961,#182962,#182963,#182964,#182965,
#182966,#182967,#182968),(#182969,#182970,#182971,#182972,#182973,#182974,
#182975,#182976,#182977),(#182978,#182979,#182980,#182981,#182982,#182983,
#182984,#182985,#182986),(#182987,#182988,#182989,#182990,#182991,#182992,
#182993,#182994,#182995),(#182996,#182997,#182998,#182999,#183000,#183001,
#183002,#183003,#183004),(#183005,#183006,#183007,#183008,#183009,#183010,
#183011,#183012,#183013),(#183014,#183015,#183016,#183017,#183018,#183019,
#183020,#183021,#183022),(#183023,#183024,#183025,#183026,#183027,#183028,
#183029,#183030,#183031),(#183032,#183033,#183034,#183035,#183036,#183037,
#183038,#183039,#183040),(#183041,#183042,#183043,#183044,#183045,#183046,
#183047,#183048,#183049),(#183050,#183051,#183052,#183053,#183054,#183055,
#183056,#183057,#183058),(#183059,#183060,#183061,#183062,#183063,#183064,
#183065,#183066,#183067),(#183068,#183069,#183070,#183071,#183072,#183073,
#183074,#183075,#183076),(#183077,#183078,#183079,#183080,#183081,#183082,
#183083,#183084,#183085),(#183086,#183087,#183088,#183089,#183090,#183091,
#183092,#183093,#183094),(#183095,#183096,#183097,#183098,#183099,#183100,
#183101,#183102,#183103),(#183104,#183105,#183106,#183107,#183108,#183109,
#183110,#183111,#183112),(#183113,#183114,#183115,#183116,#183117,#183118,
#183119,#183120,#183121),(#183122,#183123,#183124,#183125,#183126,#183127,
#183128,#183129,#183130),(#183131,#183132,#183133,#183134,#183135,#183136,
#183137,#183138,#183139),(#183140,#183141,#183142,#183143,#183144,#183145,
#183146,#183147,#183148),(#183149,#183150,#183151,#183152,#183153,#183154,
#183155,#183156,#183157),(#183158,#183159,#183160,#183161,#183162,#183163,
#183164,#183165,#183166),(#183167,#183168,#183169,#183170,#183171,#183172,
#183173,#183174,#183175),(#183176,#183177,#183178,#183179,#183180,#183181,
#183182,#183183,#183184),(#183185,#183186,#183187,#183188,#183189,#183190,
#183191,#183192,#183193),(#183194,#183195,#183196,#183197,#183198,#183199,
#183200,#183201,#183202),(#183203,#183204,#183205,#183206,#183207,#183208,
#183209,#183210,#183211),(#183212,#183213,#183214,#183215,#183216,#183217,
#183218,#183219,#183220),(#183221,#183222,#183223,#183224,#183225,#183226,
#183227,#183228,#183229),(#183230,#183231,#183232,#183233,#183234,#183235,
#183236,#183237,#183238),(#183239,#183240,#183241,#183242,#183243,#183244,
#183245,#183246,#183247),(#183248,#183249,#183250,#183251,#183252,#183253,
#183254,#183255,#183256),(#183257,#183258,#183259,#183260,#183261,#183262,
#183263,#183264,#183265),(#183266,#183267,#183268,#183269,#183270,#183271,
#183272,#183273,#183274),(#183275,#183276,#183277,#183278,#183279,#183280,
#183281,#183282,#183283),(#183284,#183285,#183286,#183287,#183288,#183289,
#183290,#183291,#183292),(#183293,#183294,#183295,#183296,#183297,#183298,
#183299,#183300,#183301),(#183302,#183303,#183304,#183305,#183306,#183307,
#183308,#183309,#183310),(#183311,#183312,#183313,#183314,#183315,#183316,
#183317,#183318,#183319),(#183320,#183321,#183322,#183323,#183324,#183325,
#183326,#183327,#183328),(#183329,#183330,#183331,#183332,#183333,#183334,
#183335,#183336,#183337),(#183338,#183339,#183340,#183341,#183342,#183343,
#183344,#183345,#183346),(#183347,#183348,#183349,#183350,#183351,#183352,
#183353,#183354,#183355),(#183356,#183357,#183358,#183359,#183360,#183361,
#183362,#183363,#183364),(#183365,#183366,#183367,#183368,#183369,#183370,
#183371,#183372,#183373),(#183374,#183375,#183376,#183377,#183378,#183379,
#183380,#183381,#183382),(#183383,#183384,#183385,#183386,#183387,#183388,
#183389,#183390,#183391),(#183392,#183393,#183394,#183395,#183396,#183397,
#183398,#183399,#183400),(#183401,#183402,#183403,#183404,#183405,#183406,
#183407,#183408,#183409),(#183410,#183411,#183412,#183413,#183414,#183415,
#183416,#183417,#183418),(#183419,#183420,#183421,#183422,#183423,#183424,
#183425,#183426,#183427),(#183428,#183429,#183430,#183431,#183432,#183433,
#183434,#183435,#183436),(#183437,#183438,#183439,#183440,#183441,#183442,
#183443,#183444,#183445),(#183446,#183447,#183448,#183449,#183450,#183451,
#183452,#183453,#183454),(#183455,#183456,#183457,#183458,#183459,#183460,
#183461,#183462,#183463),(#183464,#183465,#183466,#183467,#183468,#183469,
#183470,#183471,#183472),(#183473,#183474,#183475,#183476,#183477,#183478,
#183479,#183480,#183481),(#183482,#183483,#183484,#183485,#183486,#183487,
#183488,#183489,#183490),(#183491,#183492,#183493,#183494,#183495,#183496,
#183497,#183498,#183499),(#183500,#183501,#183502,#183503,#183504,#183505,
#183506,#183507,#183508),(#183509,#183510,#183511,#183512,#183513,#183514,
#183515,#183516,#183517),(#183518,#183519,#183520,#183521,#183522,#183523,
#183524,#183525,#183526),(#183527,#183528,#183529,#183530,#183531,#183532,
#183533,#183534,#183535),(#183536,#183537,#183538,#183539,#183540,#183541,
#183542,#183543,#183544),(#183545,#183546,#183547,#183548,#183549,#183550,
#183551,#183552,#183553),(#183554,#183555,#183556,#183557,#183558,#183559,
#183560,#183561,#183562),(#183563,#183564,#183565,#183566,#183567,#183568,
#183569,#183570,#183571),(#183572,#183573,#183574,#183575,#183576,#183577,
#183578,#183579,#183580),(#183581,#183582,#183583,#183584,#183585,#183586,
#183587,#183588,#183589),(#183590,#183591,#183592,#183593,#183594,#183595,
#183596,#183597,#183598),(#183599,#183600,#183601,#183602,#183603,#183604,
#183605,#183606,#183607),(#183608,#183609,#183610,#183611,#183612,#183613,
#183614,#183615,#183616),(#183617,#183618,#183619,#183620,#183621,#183622,
#183623,#183624,#183625),(#183626,#183627,#183628,#183629,#183630,#183631,
#183632,#183633,#183634),(#183635,#183636,#183637,#183638,#183639,#183640,
#183641,#183642,#183643),(#183644,#183645,#183646,#183647,#183648,#183649,
#183650,#183651,#183652),(#183653,#183654,#183655,#183656,#183657,#183658,
#183659,#183660,#183661),(#183662,#183663,#183664,#183665,#183666,#183667,
#183668,#183669,#183670),(#183671,#183672,#183673,#183674,#183675,#183676,
#183677,#183678,#183679),(#183680,#183681,#183682,#183683,#183684,#183685,
#183686,#183687,#183688),(#183689,#183690,#183691,#183692,#183693,#183694,
#183695,#183696,#183697),(#183698,#183699,#183700,#183701,#183702,#183703,
#183704,#183705,#183706),(#183707,#183708,#183709,#183710,#183711,#183712,
#183713,#183714,#183715),(#183716,#183717,#183718,#183719,#183720,#183721,
#183722,#183723,#183724),(#183725,#183726,#183727,#183728,#183729,#183730,
#183731,#183732,#183733),(#183734,#183735,#183736,#183737,#183738,#183739,
#183740,#183741,#183742),(#183743,#183744,#183745,#183746,#183747,#183748,
#183749,#183750,#183751),(#183752,#183753,#183754,#183755,#183756,#183757,
#183758,#183759,#183760),(#183761,#183762,#183763,#183764,#183765,#183766,
#183767,#183768,#183769),(#183770,#183771,#183772,#183773,#183774,#183775,
#183776,#183777,#183778),(#183779,#183780,#183781,#183782,#183783,#183784,
#183785,#183786,#183787),(#183788,#183789,#183790,#183791,#183792,#183793,
#183794,#183795,#183796),(#183797,#183798,#183799,#183800,#183801,#183802,
#183803,#183804,#183805),(#183806,#183807,#183808,#183809,#183810,#183811,
#183812,#183813,#183814),(#183815,#183816,#183817,#183818,#183819,#183820,
#183821,#183822,#183823),(#183824,#183825,#183826,#183827,#183828,#183829,
#183830,#183831,#183832),(#183833,#183834,#183835,#183836,#183837,#183838,
#183839,#183840,#183841),(#183842,#183843,#183844,#183845,#183846,#183847,
#183848,#183849,#183850),(#183851,#183852,#183853,#183854,#183855,#183856,
#183857,#183858,#183859),(#183860,#183861,#183862,#183863,#183864,#183865,
#183866,#183867,#183868),(#183869,#183870,#183871,#183872,#183873,#183874,
#183875,#183876,#183877),(#183878,#183879,#183880,#183881,#183882,#183883,
#183884,#183885,#183886),(#183887,#183888,#183889,#183890,#183891,#183892,
#183893,#183894,#183895),(#183896,#183897,#183898,#183899,#183900,#183901,
#183902,#183903,#183904),(#183905,#183906,#183907,#183908,#183909,#183910,
#183911,#183912,#183913),(#183914,#183915,#183916,#183917,#183918,#183919,
#183920,#183921,#183922),(#183923,#183924,#183925,#183926,#183927,#183928,
#183929,#183930,#183931),(#183932,#183933,#183934,#183935,#183936,#183937,
#183938,#183939,#183940),(#183941,#183942,#183943,#183944,#183945,#183946,
#183947,#183948,#183949),(#183950,#183951,#183952,#183953,#183954,#183955,
#183956,#183957,#183958),(#183959,#183960,#183961,#183962,#183963,#183964,
#183965,#183966,#183967),(#183968,#183969,#183970,#183971,#183972,#183973,
#183974,#183975,#183976),(#183977,#183978,#183979,#183980,#183981,#183982,
#183983,#183984,#183985),(#183986,#183987,#183988,#183989,#183990,#183991,
#183992,#183993,#183994),(#183995,#183996,#183997,#183998,#183999,#184000,
#184001,#184002,#184003),(#184004,#184005,#184006,#184007,#184008,#184009,
#184010,#184011,#184012),(#184013,#184014,#184015,#184016,#184017,#184018,
#184019,#184020,#184021),(#184022,#184023,#184024,#184025,#184026,#184027,
#184028,#184029,#184030),(#184031,#184032,#184033,#184034,#184035,#184036,
#184037,#184038,#184039),(#184040,#184041,#184042,#184043,#184044,#184045,
#184046,#184047,#184048),(#184049,#184050,#184051,#184052,#184053,#184054,
#184055,#184056,#184057),(#184058,#184059,#184060,#184061,#184062,#184063,
#184064,#184065,#184066),(#184067,#184068,#184069,#184070,#184071,#184072,
#184073,#184074,#184075),(#184076,#184077,#184078,#184079,#184080,#184081,
#184082,#184083,#184084),(#184085,#184086,#184087,#184088,#184089,#184090,
#184091,#184092,#184093),(#184094,#184095,#184096,#184097,#184098,#184099,
#184100,#184101,#184102),(#184103,#184104,#184105,#184106,#184107,#184108,
#184109,#184110,#184111),(#184112,#184113,#184114,#184115,#184116,#184117,
#184118,#184119,#184120),(#184121,#184122,#184123,#184124,#184125,#184126,
#184127,#184128,#184129),(#184130,#184131,#184132,#184133,#184134,#184135,
#184136,#184137,#184138),(#184139,#184140,#184141,#184142,#184143,#184144,
#184145,#184146,#184147),(#184148,#184149,#184150,#184151,#184152,#184153,
#184154,#184155,#184156),(#184157,#184158,#184159,#184160,#184161,#184162,
#184163,#184164,#184165),(#184166,#184167,#184168,#184169,#184170,#184171,
#184172,#184173,#184174),(#184175,#184176,#184177,#184178,#184179,#184180,
#184181,#184182,#184183),(#184184,#184185,#184186,#184187,#184188,#184189,
#184190,#184191,#184192),(#184193,#184194,#184195,#184196,#184197,#184198,
#184199,#184200,#184201),(#184202,#184203,#184204,#184205,#184206,#184207,
#184208,#184209,#184210),(#184211,#184212,#184213,#184214,#184215,#184216,
#184217,#184218,#184219),(#184220,#184221,#184222,#184223,#184224,#184225,
#184226,#184227,#184228),(#184229,#184230,#184231,#184232,#184233,#184234,
#184235,#184236,#184237),(#184238,#184239,#184240,#184241,#184242,#184243,
#184244,#184245,#184246),(#184247,#184248,#184249,#184250,#184251,#184252,
#184253,#184254,#184255),(#184256,#184257,#184258,#184259,#184260,#184261,
#184262,#184263,#184264),(#184265,#184266,#184267,#184268,#184269,#184270,
#184271,#184272,#184273),(#184274,#184275,#184276,#184277,#184278,#184279,
#184280,#184281,#184282),(#184283,#184284,#184285,#184286,#184287,#184288,
#184289,#184290,#184291),(#184292,#184293,#184294,#184295,#184296,#184297,
#184298,#184299,#184300),(#184301,#184302,#184303,#184304,#184305,#184306,
#184307,#184308,#184309),(#184310,#184311,#184312,#184313,#184314,#184315,
#184316,#184317,#184318),(#184319,#184320,#184321,#184322,#184323,#184324,
#184325,#184326,#184327),(#184328,#184329,#184330,#184331,#184332,#184333,
#184334,#184335,#184336),(#184337,#184338,#184339,#184340,#184341,#184342,
#184343,#184344,#184345),(#184346,#184347,#184348,#184349,#184350,#184351,
#184352,#184353,#184354),(#184355,#184356,#184357,#184358,#184359,#184360,
#184361,#184362,#184363),(#184364,#184365,#184366,#184367,#184368,#184369,
#184370,#184371,#184372),(#184373,#184374,#184375,#184376,#184377,#184378,
#184379,#184380,#184381),(#184382,#184383,#184384,#184385,#184386,#184387,
#184388,#184389,#184390),(#184391,#184392,#184393,#184394,#184395,#184396,
#184397,#184398,#184399),(#184400,#184401,#184402,#184403,#184404,#184405,
#184406,#184407,#184408),(#184409,#184410,#184411,#184412,#184413,#184414,
#184415,#184416,#184417),(#184418,#184419,#184420,#184421,#184422,#184423,
#184424,#184425,#184426),(#184427,#184428,#184429,#184430,#184431,#184432,
#184433,#184434,#184435),(#184436,#184437,#184438,#184439,#184440,#184441,
#184442,#184443,#184444),(#184445,#184446,#184447,#184448,#184449,#184450,
#184451,#184452,#184453),(#184454,#184455,#184456,#184457,#184458,#184459,
#184460,#184461,#184462),(#184463,#184464,#184465,#184466,#184467,#184468,
#184469,#184470,#184471),(#184472,#184473,#184474,#184475,#184476,#184477,
#184478,#184479,#184480),(#184481,#184482,#184483,#184484,#184485,#184486,
#184487,#184488,#184489),(#184490,#184491,#184492,#184493,#184494,#184495,
#184496,#184497,#184498),(#184499,#184500,#184501,#184502,#184503,#184504,
#184505,#184506,#184507),(#184508,#184509,#184510,#184511,#184512,#184513,
#184514,#184515,#184516),(#184517,#184518,#184519,#184520,#184521,#184522,
#184523,#184524,#184525),(#184526,#184527,#184528,#184529,#184530,#184531,
#184532,#184533,#184534),(#184535,#184536,#184537,#184538,#184539,#184540,
#184541,#184542,#184543),(#184544,#184545,#184546,#184547,#184548,#184549,
#184550,#184551,#184552),(#184553,#184554,#184555,#184556,#184557,#184558,
#184559,#184560,#184561),(#184562,#184563,#184564,#184565,#184566,#184567,
#184568,#184569,#184570),(#184571,#184572,#184573,#184574,#184575,#184576,
#184577,#184578,#184579),(#184580,#184581,#184582,#184583,#184584,#184585,
#184586,#184587,#184588),(#184589,#184590,#184591,#184592,#184593,#184594,
#184595,#184596,#184597),(#184598,#184599,#184600,#184601,#184602,#184603,
#184604,#184605,#184606),(#184607,#184608,#184609,#184610,#184611,#184612,
#184613,#184614,#184615),(#184616,#184617,#184618,#184619,#184620,#184621,
#184622,#184623,#184624),(#184625,#184626,#184627,#184628,#184629,#184630,
#184631,#184632,#184633),(#184634,#184635,#184636,#184637,#184638,#184639,
#184640,#184641,#184642),(#184643,#184644,#184645,#184646,#184647,#184648,
#184649,#184650,#184651),(#184652,#184653,#184654,#184655,#184656,#184657,
#184658,#184659,#184660),(#184661,#184662,#184663,#184664,#184665,#184666,
#184667,#184668,#184669),(#184670,#184671,#184672,#184673,#184674,#184675,
#184676,#184677,#184678),(#184679,#184680,#184681,#184682,#184683,#184684,
#184685,#184686,#184687),(#184688,#184689,#184690,#184691,#184692,#184693,
#184694,#184695,#184696),(#184697,#184698,#184699,#184700,#184701,#184702,
#184703,#184704,#184705),(#184706,#184707,#184708,#184709,#184710,#184711,
#184712,#184713,#184714),(#184715,#184716,#184717,#184718,#184719,#184720,
#184721,#184722,#184723),(#184724,#184725,#184726,#184727,#184728,#184729,
#184730,#184731,#184732),(#184733,#184734,#184735,#184736,#184737,#184738,
#184739,#184740,#184741),(#184742,#184743,#184744,#184745,#184746,#184747,
#184748,#184749,#184750),(#184751,#184752,#184753,#184754,#184755,#184756,
#184757,#184758,#184759),(#184760,#184761,#184762,#184763,#184764,#184765,
#184766,#184767,#184768),(#184769,#184770,#184771,#184772,#184773,#184774,
#184775,#184776,#184777),(#184778,#184779,#184780,#184781,#184782,#184783,
#184784,#184785,#184786),(#184787,#184788,#184789,#184790,#184791,#184792,
#184793,#184794,#184795),(#184796,#184797,#184798,#184799,#184800,#184801,
#184802,#184803,#184804),(#184805,#184806,#184807,#184808,#184809,#184810,
#184811,#184812,#184813),(#184814,#184815,#184816,#184817,#184818,#184819,
#184820,#184821,#184822),(#184823,#184824,#184825,#184826,#184827,#184828,
#184829,#184830,#184831),(#184832,#184833,#184834,#184835,#184836,#184837,
#184838,#184839,#184840),(#184841,#184842,#184843,#184844,#184845,#184846,
#184847,#184848,#184849),(#184850,#184851,#184852,#184853,#184854,#184855,
#184856,#184857,#184858),(#184859,#184860,#184861,#184862,#184863,#184864,
#184865,#184866,#184867),(#184868,#184869,#184870,#184871,#184872,#184873,
#184874,#184875,#184876),(#184877,#184878,#184879,#184880,#184881,#184882,
#184883,#184884,#184885),(#184886,#184887,#184888,#184889,#184890,#184891,
#184892,#184893,#184894),(#184895,#184896,#184897,#184898,#184899,#184900,
#184901,#184902,#184903),(#184904,#184905,#184906,#184907,#184908,#184909,
#184910,#184911,#184912),(#184913,#184914,#184915,#184916,#184917,#184918,
#184919,#184920,#184921),(#184922,#184923,#184924,#184925,#184926,#184927,
#184928,#184929,#184930),(#184931,#184932,#184933,#184934,#184935,#184936,
#184937,#184938,#184939),(#184940,#184941,#184942,#184943,#184944,#184945,
#184946,#184947,#184948),(#184949,#184950,#184951,#184952,#184953,#184954,
#184955,#184956,#184957),(#184958,#184959,#184960,#184961,#184962,#184963,
#184964,#184965,#184966),(#184967,#184968,#184969,#184970,#184971,#184972,
#184973,#184974,#184975),(#184976,#184977,#184978,#184979,#184980,#184981,
#184982,#184983,#184984),(#184985,#184986,#184987,#184988,#184989,#184990,
#184991,#184992,#184993),(#184994,#184995,#184996,#184997,#184998,#184999,
#185000,#185001,#185002),(#185003,#185004,#185005,#185006,#185007,#185008,
#185009,#185010,#185011),(#185012,#185013,#185014,#185015,#185016,#185017,
#185018,#185019,#185020),(#185021,#185022,#185023,#185024,#185025,#185026,
#185027,#185028,#185029),(#185030,#185031,#185032,#185033,#185034,#185035,
#185036,#185037,#185038),(#185039,#185040,#185041,#185042,#185043,#185044,
#185045,#185046,#185047),(#185048,#185049,#185050,#185051,#185052,#185053,
#185054,#185055,#185056),(#185057,#185058,#185059,#185060,#185061,#185062,
#185063,#185064,#185065),(#185066,#185067,#185068,#185069,#185070,#185071,
#185072,#185073,#185074),(#185075,#185076,#185077,#185078,#185079,#185080,
#185081,#185082,#185083),(#185084,#185085,#185086,#185087,#185088,#185089,
#185090,#185091,#185092),(#185093,#185094,#185095,#185096,#185097,#185098,
#185099,#185100,#185101),(#185102,#185103,#185104,#185105,#185106,#185107,
#185108,#185109,#185110),(#185111,#185112,#185113,#185114,#185115,#185116,
#185117,#185118,#185119),(#185120,#185121,#185122,#185123,#185124,#185125,
#185126,#185127,#185128),(#185129,#185130,#185131,#185132,#185133,#185134,
#185135,#185136,#185137),(#185138,#185139,#185140,#185141,#185142,#185143,
#185144,#185145,#185146),(#185147,#185148,#185149,#185150,#185151,#185152,
#185153,#185154,#185155),(#185156,#185157,#185158,#185159,#185160,#185161,
#185162,#185163,#185164),(#185165,#185166,#185167,#185168,#185169,#185170,
#185171,#185172,#185173),(#185174,#185175,#185176,#185177,#185178,#185179,
#185180,#185181,#185182),(#185183,#185184,#185185,#185186,#185187,#185188,
#185189,#185190,#185191),(#185192,#185193,#185194,#185195,#185196,#185197,
#185198,#185199,#185200),(#185201,#185202,#185203,#185204,#185205,#185206,
#185207,#185208,#185209),(#185210,#185211,#185212,#185213,#185214,#185215,
#185216,#185217,#185218),(#185219,#185220,#185221,#185222,#185223,#185224,
#185225,#185226,#185227),(#185228,#185229,#185230,#185231,#185232,#185233,
#185234,#185235,#185236),(#185237,#185238,#185239,#185240,#185241,#185242,
#185243,#185244,#185245),(#185246,#185247,#185248,#185249,#185250,#185251,
#185252,#185253,#185254),(#185255,#185256,#185257,#185258,#185259,#185260,
#185261,#185262,#185263),(#185264,#185265,#185266,#185267,#185268,#185269,
#185270,#185271,#185272),(#185273,#185274,#185275,#185276,#185277,#185278,
#185279,#185280,#185281),(#185282,#185283,#185284,#185285,#185286,#185287,
#185288,#185289,#185290),(#185291,#185292,#185293,#185294,#185295,#185296,
#185297,#185298,#185299),(#185300,#185301,#185302,#185303,#185304,#185305,
#185306,#185307,#185308),(#185309,#185310,#185311,#185312,#185313,#185314,
#185315,#185316,#185317),(#185318,#185319,#185320,#185321,#185322,#185323,
#185324,#185325,#185326),(#185327,#185328,#185329,#185330,#185331,#185332,
#185333,#185334,#185335),(#185336,#185337,#185338,#185339,#185340,#185341,
#185342,#185343,#185344),(#185345,#185346,#185347,#185348,#185349,#185350,
#185351,#185352,#185353),(#185354,#185355,#185356,#185357,#185358,#185359,
#185360,#185361,#185362),(#185363,#185364,#185365,#185366,#185367,#185368,
#185369,#185370,#185371),(#185372,#185373,#185374,#185375,#185376,#185377,
#185378,#185379,#185380),(#185381,#185382,#185383,#185384,#185385,#185386,
#185387,#185388,#185389),(#185390,#185391,#185392,#185393,#185394,#185395,
#185396,#185397,#185398),(#185399,#185400,#185401,#185402,#185403,#185404,
#185405,#185406,#185407),(#185408,#185409,#185410,#185411,#185412,#185413,
#185414,#185415,#185416),(#185417,#185418,#185419,#185420,#185421,#185422,
#185423,#185424,#185425),(#185426,#185427,#185428,#185429,#185430,#185431,
#185432,#185433,#185434),(#185435,#185436,#185437,#185438,#185439,#185440,
#185441,#185442,#185443),(#185444,#185445,#185446,#185447,#185448,#185449,
#185450,#185451,#185452),(#185453,#185454,#185455,#185456,#185457,#185458,
#185459,#185460,#185461),(#185462,#185463,#185464,#185465,#185466,#185467,
#185468,#185469,#185470),(#185471,#185472,#185473,#185474,#185475,#185476,
#185477,#185478,#185479),(#185480,#185481,#185482,#185483,#185484,#185485,
#185486,#185487,#185488),(#185489,#185490,#185491,#185492,#185493,#185494,
#185495,#185496,#185497),(#185498,#185499,#185500,#185501,#185502,#185503,
#185504,#185505,#185506),(#185507,#185508,#185509,#185510,#185511,#185512,
#185513,#185514,#185515),(#185516,#185517,#185518,#185519,#185520,#185521,
#185522,#185523,#185524),(#185525,#185526,#185527,#185528,#185529,#185530,
#185531,#185532,#185533),(#185534,#185535,#185536,#185537,#185538,#185539,
#185540,#185541,#185542),(#185543,#185544,#185545,#185546,#185547,#185548,
#185549,#185550,#185551),(#185552,#185553,#185554,#185555,#185556,#185557,
#185558,#185559,#185560),(#185561,#185562,#185563,#185564,#185565,#185566,
#185567,#185568,#185569),(#185570,#185571,#185572,#185573,#185574,#185575,
#185576,#185577,#185578),(#185579,#185580,#185581,#185582,#185583,#185584,
#185585,#185586,#185587),(#185588,#185589,#185590,#185591,#185592,#185593,
#185594,#185595,#185596),(#185597,#185598,#185599,#185600,#185601,#185602,
#185603,#185604,#185605),(#185606,#185607,#185608,#185609,#185610,#185611,
#185612,#185613,#185614),(#185615,#185616,#185617,#185618,#185619,#185620,
#185621,#185622,#185623),(#185624,#185625,#185626,#185627,#185628,#185629,
#185630,#185631,#185632),(#185633,#185634,#185635,#185636,#185637,#185638,
#185639,#185640,#185641),(#185642,#185643,#185644,#185645,#185646,#185647,
#185648,#185649,#185650),(#185651,#185652,#185653,#185654,#185655,#185656,
#185657,#185658,#185659),(#185660,#185661,#185662,#185663,#185664,#185665,
#185666,#185667,#185668),(#185669,#185670,#185671,#185672,#185673,#185674,
#185675,#185676,#185677),(#185678,#185679,#185680,#185681,#185682,#185683,
#185684,#185685,#185686),(#185687,#185688,#185689,#185690,#185691,#185692,
#185693,#185694,#185695),(#185696,#185697,#185698,#185699,#185700,#185701,
#185702,#185703,#185704),(#185705,#185706,#185707,#185708,#185709,#185710,
#185711,#185712,#185713),(#185714,#185715,#185716,#185717,#185718,#185719,
#185720,#185721,#185722),(#185723,#185724,#185725,#185726,#185727,#185728,
#185729,#185730,#185731),(#185732,#185733,#185734,#185735,#185736,#185737,
#185738,#185739,#185740),(#185741,#185742,#185743,#185744,#185745,#185746,
#185747,#185748,#185749),(#185750,#185751,#185752,#185753,#185754,#185755,
#185756,#185757,#185758),(#185759,#185760,#185761,#185762,#185763,#185764,
#185765,#185766,#185767),(#185768,#185769,#185770,#185771,#185772,#185773,
#185774,#185775,#185776),(#185777,#185778,#185779,#185780,#185781,#185782,
#185783,#185784,#185785),(#185786,#185787,#185788,#185789,#185790,#185791,
#185792,#185793,#185794),(#185795,#185796,#185797,#185798,#185799,#185800,
#185801,#185802,#185803),(#185804,#185805,#185806,#185807,#185808,#185809,
#185810,#185811,#185812),(#185813,#185814,#185815,#185816,#185817,#185818,
#185819,#185820,#185821),(#185822,#185823,#185824,#185825,#185826,#185827,
#185828,#185829,#185830),(#185831,#185832,#185833,#185834,#185835,#185836,
#185837,#185838,#185839),(#185840,#185841,#185842,#185843,#185844,#185845,
#185846,#185847,#185848),(#185849,#185850,#185851,#185852,#185853,#185854,
#185855,#185856,#185857),(#185858,#185859,#185860,#185861,#185862,#185863,
#185864,#185865,#185866),(#185867,#185868,#185869,#185870,#185871,#185872,
#185873,#185874,#185875),(#185876,#185877,#185878,#185879,#185880,#185881,
#185882,#185883,#185884),(#185885,#185886,#185887,#185888,#185889,#185890,
#185891,#185892,#185893),(#185894,#185895,#185896,#185897,#185898,#185899,
#185900,#185901,#185902),(#185903,#185904,#185905,#185906,#185907,#185908,
#185909,#185910,#185911),(#185912,#185913,#185914,#185915,#185916,#185917,
#185918,#185919,#185920),(#185921,#185922,#185923,#185924,#185925,#185926,
#185927,#185928,#185929),(#185930,#185931,#185932,#185933,#185934,#185935,
#185936,#185937,#185938),(#185939,#185940,#185941,#185942,#185943,#185944,
#185945,#185946,#185947),(#185948,#185949,#185950,#185951,#185952,#185953,
#185954,#185955,#185956),(#185957,#185958,#185959,#185960,#185961,#185962,
#185963,#185964,#185965),(#185966,#185967,#185968,#185969,#185970,#185971,
#185972,#185973,#185974),(#185975,#185976,#185977,#185978,#185979,#185980,
#185981,#185982,#185983),(#185984,#185985,#185986,#185987,#185988,#185989,
#185990,#185991,#185992),(#185993,#185994,#185995,#185996,#185997,#185998,
#185999,#186000,#186001),(#186002,#186003,#186004,#186005,#186006,#186007,
#186008,#186009,#186010),(#186011,#186012,#186013,#186014,#186015,#186016,
#186017,#186018,#186019),(#186020,#186021,#186022,#186023,#186024,#186025,
#186026,#186027,#186028),(#186029,#186030,#186031,#186032,#186033,#186034,
#186035,#186036,#186037),(#186038,#186039,#186040,#186041,#186042,#186043,
#186044,#186045,#186046),(#186047,#186048,#186049,#186050,#186051,#186052,
#186053,#186054,#186055),(#186056,#186057,#186058,#186059,#186060,#186061,
#186062,#186063,#186064),(#186065,#186066,#186067,#186068,#186069,#186070,
#186071,#186072,#186073),(#186074,#186075,#186076,#186077,#186078,#186079,
#186080,#186081,#186082),(#186083,#186084,#186085,#186086,#186087,#186088,
#186089,#186090,#186091),(#186092,#186093,#186094,#186095,#186096,#186097,
#186098,#186099,#186100),(#186101,#186102,#186103,#186104,#186105,#186106,
#186107,#186108,#186109),(#186110,#186111,#186112,#186113,#186114,#186115,
#186116,#186117,#186118),(#186119,#186120,#186121,#186122,#186123,#186124,
#186125,#186126,#186127),(#186128,#186129,#186130,#186131,#186132,#186133,
#186134,#186135,#186136),(#186137,#186138,#186139,#186140,#186141,#186142,
#186143,#186144,#186145),(#186146,#186147,#186148,#186149,#186150,#186151,
#186152,#186153,#186154),(#186155,#186156,#186157,#186158,#186159,#186160,
#186161,#186162,#186163),(#186164,#186165,#186166,#186167,#186168,#186169,
#186170,#186171,#186172),(#186173,#186174,#186175,#186176,#186177,#186178,
#186179,#186180,#186181),(#186182,#186183,#186184,#186185,#186186,#186187,
#186188,#186189,#186190),(#186191,#186192,#186193,#186194,#186195,#186196,
#186197,#186198,#186199),(#186200,#186201,#186202,#186203,#186204,#186205,
#186206,#186207,#186208),(#186209,#186210,#186211,#186212,#186213,#186214,
#186215,#186216,#186217),(#186218,#186219,#186220,#186221,#186222,#186223,
#186224,#186225,#186226),(#186227,#186228,#186229,#186230,#186231,#186232,
#186233,#186234,#186235),(#186236,#186237,#186238,#186239,#186240,#186241,
#186242,#186243,#186244),(#186245,#186246,#186247,#186248,#186249,#186250,
#186251,#186252,#186253),(#186254,#186255,#186256,#186257,#186258,#186259,
#186260,#186261,#186262),(#186263,#186264,#186265,#186266,#186267,#186268,
#186269,#186270,#186271),(#186272,#186273,#186274,#186275,#186276,#186277,
#186278,#186279,#186280),(#186281,#186282,#186283,#186284,#186285,#186286,
#186287,#186288,#186289),(#186290,#186291,#186292,#186293,#186294,#186295,
#186296,#186297,#186298),(#186299,#186300,#186301,#186302,#186303,#186304,
#186305,#186306,#186307),(#186308,#186309,#186310,#186311,#186312,#186313,
#186314,#186315,#186316),(#186317,#186318,#186319,#186320,#186321,#186322,
#186323,#186324,#186325),(#186326,#186327,#186328,#186329,#186330,#186331,
#186332,#186333,#186334),(#186335,#186336,#186337,#186338,#186339,#186340,
#186341,#186342,#186343),(#186344,#186345,#186346,#186347,#186348,#186349,
#186350,#186351,#186352),(#186353,#186354,#186355,#186356,#186357,#186358,
#186359,#186360,#186361),(#186362,#186363,#186364,#186365,#186366,#186367,
#186368,#186369,#186370),(#186371,#186372,#186373,#186374,#186375,#186376,
#186377,#186378,#186379),(#186380,#186381,#186382,#186383,#186384,#186385,
#186386,#186387,#186388),(#186389,#186390,#186391,#186392,#186393,#186394,
#186395,#186396,#186397),(#186398,#186399,#186400,#186401,#186402,#186403,
#186404,#186405,#186406),(#186407,#186408,#186409,#186410,#186411,#186412,
#186413,#186414,#186415),(#186416,#186417,#186418,#186419,#186420,#186421,
#186422,#186423,#186424),(#186425,#186426,#186427,#186428,#186429,#186430,
#186431,#186432,#186433),(#186434,#186435,#186436,#186437,#186438,#186439,
#186440,#186441,#186442),(#186443,#186444,#186445,#186446,#186447,#186448,
#186449,#186450,#186451),(#186452,#186453,#186454,#186455,#186456,#186457,
#186458,#186459,#186460),(#186461,#186462,#186463,#186464,#186465,#186466,
#186467,#186468,#186469),(#186470,#186471,#186472,#186473,#186474,#186475,
#186476,#186477,#186478),(#186479,#186480,#186481,#186482,#186483,#186484,
#186485,#186486,#186487),(#186488,#186489,#186490,#186491,#186492,#186493,
#186494,#186495,#186496),(#186497,#186498,#186499,#186500,#186501,#186502,
#186503,#186504,#186505),(#186506,#186507,#186508,#186509,#186510,#186511,
#186512,#186513,#186514),(#186515,#186516,#186517,#186518,#186519,#186520,
#186521,#186522,#186523),(#186524,#186525,#186526,#186527,#186528,#186529,
#186530,#186531,#186532),(#186533,#186534,#186535,#186536,#186537,#186538,
#186539,#186540,#186541),(#186542,#186543,#186544,#186545,#186546,#186547,
#186548,#186549,#186550),(#186551,#186552,#186553,#186554,#186555,#186556,
#186557,#186558,#186559),(#186560,#186561,#186562,#186563,#186564,#186565,
#186566,#186567,#186568),(#186569,#186570,#186571,#186572,#186573,#186574,
#186575,#186576,#186577),(#186578,#186579,#186580,#186581,#186582,#186583,
#186584,#186585,#186586),(#186587,#186588,#186589,#186590,#186591,#186592,
#186593,#186594,#186595),(#186596,#186597,#186598,#186599,#186600,#186601,
#186602,#186603,#186604),(#186605,#186606,#186607,#186608,#186609,#186610,
#186611,#186612,#186613),(#186614,#186615,#186616,#186617,#186618,#186619,
#186620,#186621,#186622),(#186623,#186624,#186625,#186626,#186627,#186628,
#186629,#186630,#186631),(#186632,#186633,#186634,#186635,#186636,#186637,
#186638,#186639,#186640),(#186641,#186642,#186643,#186644,#186645,#186646,
#186647,#186648,#186649),(#186650,#186651,#186652,#186653,#186654,#186655,
#186656,#186657,#186658),(#186659,#186660,#186661,#186662,#186663,#186664,
#186665,#186666,#186667),(#186668,#186669,#186670,#186671,#186672,#186673,
#186674,#186675,#186676),(#186677,#186678,#186679,#186680,#186681,#186682,
#186683,#186684,#186685),(#186686,#186687,#186688,#186689,#186690,#186691,
#186692,#186693,#186694),(#186695,#186696,#186697,#186698,#186699,#186700,
#186701,#186702,#186703),(#186704,#186705,#186706,#186707,#186708,#186709,
#186710,#186711,#186712),(#186713,#186714,#186715,#186716,#186717,#186718,
#186719,#186720,#186721),(#186722,#186723,#186724,#186725,#186726,#186727,
#186728,#186729,#186730),(#186731,#186732,#186733,#186734,#186735,#186736,
#186737,#186738,#186739),(#186740,#186741,#186742,#186743,#186744,#186745,
#186746,#186747,#186748),(#186749,#186750,#186751,#186752,#186753,#186754,
#186755,#186756,#186757),(#186758,#186759,#186760,#186761,#186762,#186763,
#186764,#186765,#186766),(#186767,#186768,#186769,#186770,#186771,#186772,
#186773,#186774,#186775),(#186776,#186777,#186778,#186779,#186780,#186781,
#186782,#186783,#186784),(#186785,#186786,#186787,#186788,#186789,#186790,
#186791,#186792,#186793),(#186794,#186795,#186796,#186797,#186798,#186799,
#186800,#186801,#186802),(#186803,#186804,#186805,#186806,#186807,#186808,
#186809,#186810,#186811),(#186812,#186813,#186814,#186815,#186816,#186817,
#186818,#186819,#186820),(#186821,#186822,#186823,#186824,#186825,#186826,
#186827,#186828,#186829),(#186830,#186831,#186832,#186833,#186834,#186835,
#186836,#186837,#186838),(#186839,#186840,#186841,#186842,#186843,#186844,
#186845,#186846,#186847),(#186848,#186849,#186850,#186851,#186852,#186853,
#186854,#186855,#186856),(#186857,#186858,#186859,#186860,#186861,#186862,
#186863,#186864,#186865),(#186866,#186867,#186868,#186869,#186870,#186871,
#186872,#186873,#186874),(#186875,#186876,#186877,#186878,#186879,#186880,
#186881,#186882,#186883),(#186884,#186885,#186886,#186887,#186888,#186889,
#186890,#186891,#186892),(#186893,#186894,#186895,#186896,#186897,#186898,
#186899,#186900,#186901),(#186902,#186903,#186904,#186905,#186906,#186907,
#186908,#186909,#186910),(#186911,#186912,#186913,#186914,#186915,#186916,
#186917,#186918,#186919),(#186920,#186921,#186922,#186923,#186924,#186925,
#186926,#186927,#186928),(#186929,#186930,#186931,#186932,#186933,#186934,
#186935,#186936,#186937),(#186938,#186939,#186940,#186941,#186942,#186943,
#186944,#186945,#186946),(#186947,#186948,#186949,#186950,#186951,#186952,
#186953,#186954,#186955),(#186956,#186957,#186958,#186959,#186960,#186961,
#186962,#186963,#186964),(#186965,#186966,#186967,#186968,#186969,#186970,
#186971,#186972,#186973),(#186974,#186975,#186976,#186977,#186978,#186979,
#186980,#186981,#186982),(#186983,#186984,#186985,#186986,#186987,#186988,
#186989,#186990,#186991),(#186992,#186993,#186994,#186995,#186996,#186997,
#186998,#186999,#187000),(#187001,#187002,#187003,#187004,#187005,#187006,
#187007,#187008,#187009),(#187010,#187011,#187012,#187013,#187014,#187015,
#187016,#187017,#187018),(#187019,#187020,#187021,#187022,#187023,#187024,
#187025,#187026,#187027),(#187028,#187029,#187030,#187031,#187032,#187033,
#187034,#187035,#187036),(#187037,#187038,#187039,#187040,#187041,#187042,
#187043,#187044,#187045),(#187046,#187047,#187048,#187049,#187050,#187051,
#187052,#187053,#187054),(#187055,#187056,#187057,#187058,#187059,#187060,
#187061,#187062,#187063),(#187064,#187065,#187066,#187067,#187068,#187069,
#187070,#187071,#187072),(#187073,#187074,#187075,#187076,#187077,#187078,
#187079,#187080,#187081),(#187082,#187083,#187084,#187085,#187086,#187087,
#187088,#187089,#187090),(#187091,#187092,#187093,#187094,#187095,#187096,
#187097,#187098,#187099),(#187100,#187101,#187102,#187103,#187104,#187105,
#187106,#187107,#187108),(#187109,#187110,#187111,#187112,#187113,#187114,
#187115,#187116,#187117),(#187118,#187119,#187120,#187121,#187122,#187123,
#187124,#187125,#187126),(#187127,#187128,#187129,#187130,#187131,#187132,
#187133,#187134,#187135),(#187136,#187137,#187138,#187139,#187140,#187141,
#187142,#187143,#187144),(#187145,#187146,#187147,#187148,#187149,#187150,
#187151,#187152,#187153),(#187154,#187155,#187156,#187157,#187158,#187159,
#187160,#187161,#187162),(#187163,#187164,#187165,#187166,#187167,#187168,
#187169,#187170,#187171),(#187172,#187173,#187174,#187175,#187176,#187177,
#187178,#187179,#187180),(#187181,#187182,#187183,#187184,#187185,#187186,
#187187,#187188,#187189),(#187190,#187191,#187192,#187193,#187194,#187195,
#187196,#187197,#187198),(#187199,#187200,#187201,#187202,#187203,#187204,
#187205,#187206,#187207),(#187208,#187209,#187210,#187211,#187212,#187213,
#187214,#187215,#187216),(#187217,#187218,#187219,#187220,#187221,#187222,
#187223,#187224,#187225),(#187226,#187227,#187228,#187229,#187230,#187231,
#187232,#187233,#187234),(#187235,#187236,#187237,#187238,#187239,#187240,
#187241,#187242,#187243),(#187244,#187245,#187246,#187247,#187248,#187249,
#187250,#187251,#187252),(#187253,#187254,#187255,#187256,#187257,#187258,
#187259,#187260,#187261),(#187262,#187263,#187264,#187265,#187266,#187267,
#187268,#187269,#187270),(#187271,#187272,#187273,#187274,#187275,#187276,
#187277,#187278,#187279),(#187280,#187281,#187282,#187283,#187284,#187285,
#187286,#187287,#187288),(#187289,#187290,#187291,#187292,#187293,#187294,
#187295,#187296,#187297),(#187298,#187299,#187300,#187301,#187302,#187303,
#187304,#187305,#187306),(#187307,#187308,#187309,#187310,#187311,#187312,
#187313,#187314,#187315),(#187316,#187317,#187318,#187319,#187320,#187321,
#187322,#187323,#187324),(#187325,#187326,#187327,#187328,#187329,#187330,
#187331,#187332,#187333),(#187334,#187335,#187336,#187337,#187338,#187339,
#187340,#187341,#187342),(#187343,#187344,#187345,#187346,#187347,#187348,
#187349,#187350,#187351),(#187352,#187353,#187354,#187355,#187356,#187357,
#187358,#187359,#187360),(#187361,#187362,#187363,#187364,#187365,#187366,
#187367,#187368,#187369),(#187370,#187371,#187372,#187373,#187374,#187375,
#187376,#187377,#187378),(#187379,#187380,#187381,#187382,#187383,#187384,
#187385,#187386,#187387),(#187388,#187389,#187390,#187391,#187392,#187393,
#187394,#187395,#187396),(#187397,#187398,#187399,#187400,#187401,#187402,
#187403,#187404,#187405),(#187406,#187407,#187408,#187409,#187410,#187411,
#187412,#187413,#187414),(#187415,#187416,#187417,#187418,#187419,#187420,
#187421,#187422,#187423),(#187424,#187425,#187426,#187427,#187428,#187429,
#187430,#187431,#187432),(#187433,#187434,#187435,#187436,#187437,#187438,
#187439,#187440,#187441),(#187442,#187443,#187444,#187445,#187446,#187447,
#187448,#187449,#187450),(#187451,#187452,#187453,#187454,#187455,#187456,
#187457,#187458,#187459),(#187460,#187461,#187462,#187463,#187464,#187465,
#187466,#187467,#187468),(#187469,#187470,#187471,#187472,#187473,#187474,
#187475,#187476,#187477),(#187478,#187479,#187480,#187481,#187482,#187483,
#187484,#187485,#187486),(#187487,#187488,#187489,#187490,#187491,#187492,
#187493,#187494,#187495),(#187496,#187497,#187498,#187499,#187500,#187501,
#187502,#187503,#187504),(#187505,#187506,#187507,#187508,#187509,#187510,
#187511,#187512,#187513),(#187514,#187515,#187516,#187517,#187518,#187519,
#187520,#187521,#187522),(#187523,#187524,#187525,#187526,#187527,#187528,
#187529,#187530,#187531),(#187532,#187533,#187534,#187535,#187536,#187537,
#187538,#187539,#187540),(#187541,#187542,#187543,#187544,#187545,#187546,
#187547,#187548,#187549),(#187550,#187551,#187552,#187553,#187554,#187555,
#187556,#187557,#187558),(#187559,#187560,#187561,#187562,#187563,#187564,
#187565,#187566,#187567),(#187568,#187569,#187570,#187571,#187572,#187573,
#187574,#187575,#187576),(#187577,#187578,#187579,#187580,#187581,#187582,
#187583,#187584,#187585),(#187586,#187587,#187588,#187589,#187590,#187591,
#187592,#187593,#187594),(#187595,#187596,#187597,#187598,#187599,#187600,
#187601,#187602,#187603),(#187604,#187605,#187606,#187607,#187608,#187609,
#187610,#187611,#187612),(#187613,#187614,#187615,#187616,#187617,#187618,
#187619,#187620,#187621),(#187622,#187623,#187624,#187625,#187626,#187627,
#187628,#187629,#187630),(#187631,#187632,#187633,#187634,#187635,#187636,
#187637,#187638,#187639),(#187640,#187641,#187642,#187643,#187644,#187645,
#187646,#187647,#187648),(#187649,#187650,#187651,#187652,#187653,#187654,
#187655,#187656,#187657),(#187658,#187659,#187660,#187661,#187662,#187663,
#187664,#187665,#187666),(#187667,#187668,#187669,#187670,#187671,#187672,
#187673,#187674,#187675),(#187676,#187677,#187678,#187679,#187680,#187681,
#187682,#187683,#187684),(#187685,#187686,#187687,#187688,#187689,#187690,
#187691,#187692,#187693),(#187694,#187695,#187696,#187697,#187698,#187699,
#187700,#187701,#187702),(#187703,#187704,#187705,#187706,#187707,#187708,
#187709,#187710,#187711),(#187712,#187713,#187714,#187715,#187716,#187717,
#187718,#187719,#187720),(#187721,#187722,#187723,#187724,#187725,#187726,
#187727,#187728,#187729),(#187730,#187731,#187732,#187733,#187734,#187735,
#187736,#187737,#187738),(#187739,#187740,#187741,#187742,#187743,#187744,
#187745,#187746,#187747),(#187748,#187749,#187750,#187751,#187752,#187753,
#187754,#187755,#187756),(#187757,#187758,#187759,#187760,#187761,#187762,
#187763,#187764,#187765),(#187766,#187767,#187768,#187769,#187770,#187771,
#187772,#187773,#187774),(#187775,#187776,#187777,#187778,#187779,#187780,
#187781,#187782,#187783),(#187784,#187785,#187786,#187787,#187788,#187789,
#187790,#187791,#187792),(#187793,#187794,#187795,#187796,#187797,#187798,
#187799,#187800,#187801),(#187802,#187803,#187804,#187805,#187806,#187807,
#187808,#187809,#187810),(#187811,#187812,#187813,#187814,#187815,#187816,
#187817,#187818,#187819),(#187820,#187821,#187822,#187823,#187824,#187825,
#187826,#187827,#187828),(#187829,#187830,#187831,#187832,#187833,#187834,
#187835,#187836,#187837),(#187838,#187839,#187840,#187841,#187842,#187843,
#187844,#187845,#187846),(#187847,#187848,#187849,#187850,#187851,#187852,
#187853,#187854,#187855),(#187856,#187857,#187858,#187859,#187860,#187861,
#187862,#187863,#187864),(#187865,#187866,#187867,#187868,#187869,#187870,
#187871,#187872,#187873),(#187874,#187875,#187876,#187877,#187878,#187879,
#187880,#187881,#187882),(#187883,#187884,#187885,#187886,#187887,#187888,
#187889,#187890,#187891),(#187892,#187893,#187894,#187895,#187896,#187897,
#187898,#187899,#187900),(#187901,#187902,#187903,#187904,#187905,#187906,
#187907,#187908,#187909),(#187910,#187911,#187912,#187913,#187914,#187915,
#187916,#187917,#187918),(#187919,#187920,#187921,#187922,#187923,#187924,
#187925,#187926,#187927),(#187928,#187929,#187930,#187931,#187932,#187933,
#187934,#187935,#187936),(#187937,#187938,#187939,#187940,#187941,#187942,
#187943,#187944,#187945),(#187946,#187947,#187948,#187949,#187950,#187951,
#187952,#187953,#187954),(#187955,#187956,#187957,#187958,#187959,#187960,
#187961,#187962,#187963),(#187964,#187965,#187966,#187967,#187968,#187969,
#187970,#187971,#187972),(#187973,#187974,#187975,#187976,#187977,#187978,
#187979,#187980,#187981),(#187982,#187983,#187984,#187985,#187986,#187987,
#187988,#187989,#187990),(#187991,#187992,#187993,#187994,#187995,#187996,
#187997,#187998,#187999),(#188000,#188001,#188002,#188003,#188004,#188005,
#188006,#188007,#188008),(#188009,#188010,#188011,#188012,#188013,#188014,
#188015,#188016,#188017),(#188018,#188019,#188020,#188021,#188022,#188023,
#188024,#188025,#188026),(#188027,#188028,#188029,#188030,#188031,#188032,
#188033,#188034,#188035),(#188036,#188037,#188038,#188039,#188040,#188041,
#188042,#188043,#188044),(#188045,#188046,#188047,#188048,#188049,#188050,
#188051,#188052,#188053),(#188054,#188055,#188056,#188057,#188058,#188059,
#188060,#188061,#188062),(#188063,#188064,#188065,#188066,#188067,#188068,
#188069,#188070,#188071),(#188072,#188073,#188074,#188075,#188076,#188077,
#188078,#188079,#188080),(#188081,#188082,#188083,#188084,#188085,#188086,
#188087,#188088,#188089),(#188090,#188091,#188092,#188093,#188094,#188095,
#188096,#188097,#188098),(#188099,#188100,#188101,#188102,#188103,#188104,
#188105,#188106,#188107),(#188108,#188109,#188110,#188111,#188112,#188113,
#188114,#188115,#188116),(#188117,#188118,#188119,#188120,#188121,#188122,
#188123,#188124,#188125),(#188126,#188127,#188128,#188129,#188130,#188131,
#188132,#188133,#188134),(#188135,#188136,#188137,#188138,#188139,#188140,
#188141,#188142,#188143),(#188144,#188145,#188146,#188147,#188148,#188149,
#188150,#188151,#188152),(#188153,#188154,#188155,#188156,#188157,#188158,
#188159,#188160,#188161),(#188162,#188163,#188164,#188165,#188166,#188167,
#188168,#188169,#188170),(#188171,#188172,#188173,#188174,#188175,#188176,
#188177,#188178,#188179),(#188180,#188181,#188182,#188183,#188184,#188185,
#188186,#188187,#188188),(#188189,#188190,#188191,#188192,#188193,#188194,
#188195,#188196,#188197),(#188198,#188199,#188200,#188201,#188202,#188203,
#188204,#188205,#188206),(#188207,#188208,#188209,#188210,#188211,#188212,
#188213,#188214,#188215),(#188216,#188217,#188218,#188219,#188220,#188221,
#188222,#188223,#188224),(#188225,#188226,#188227,#188228,#188229,#188230,
#188231,#188232,#188233),(#188234,#188235,#188236,#188237,#188238,#188239,
#188240,#188241,#188242),(#188243,#188244,#188245,#188246,#188247,#188248,
#188249,#188250,#188251),(#188252,#188253,#188254,#188255,#188256,#188257,
#188258,#188259,#188260),(#188261,#188262,#188263,#188264,#188265,#188266,
#188267,#188268,#188269),(#188270,#188271,#188272,#188273,#188274,#188275,
#188276,#188277,#188278),(#188279,#188280,#188281,#188282,#188283,#188284,
#188285,#188286,#188287),(#188288,#188289,#188290,#188291,#188292,#188293,
#188294,#188295,#188296),(#188297,#188298,#188299,#188300,#188301,#188302,
#188303,#188304,#188305),(#188306,#188307,#188308,#188309,#188310,#188311,
#188312,#188313,#188314),(#188315,#188316,#188317,#188318,#188319,#188320,
#188321,#188322,#188323),(#188324,#188325,#188326,#188327,#188328,#188329,
#188330,#188331,#188332),(#188333,#188334,#188335,#188336,#188337,#188338,
#188339,#188340,#188341),(#188342,#188343,#188344,#188345,#188346,#188347,
#188348,#188349,#188350),(#188351,#188352,#188353,#188354,#188355,#188356,
#188357,#188358,#188359),(#188360,#188361,#188362,#188363,#188364,#188365,
#188366,#188367,#188368),(#188369,#188370,#188371,#188372,#188373,#188374,
#188375,#188376,#188377),(#188378,#188379,#188380,#188381,#188382,#188383,
#188384,#188385,#188386),(#188387,#188388,#188389,#188390,#188391,#188392,
#188393,#188394,#188395),(#188396,#188397,#188398,#188399,#188400,#188401,
#188402,#188403,#188404),(#188405,#188406,#188407,#188408,#188409,#188410,
#188411,#188412,#188413),(#188414,#188415,#188416,#188417,#188418,#188419,
#188420,#188421,#188422),(#188423,#188424,#188425,#188426,#188427,#188428,
#188429,#188430,#188431),(#188432,#188433,#188434,#188435,#188436,#188437,
#188438,#188439,#188440),(#188441,#188442,#188443,#188444,#188445,#188446,
#188447,#188448,#188449),(#188450,#188451,#188452,#188453,#188454,#188455,
#188456,#188457,#188458),(#188459,#188460,#188461,#188462,#188463,#188464,
#188465,#188466,#188467),(#188468,#188469,#188470,#188471,#188472,#188473,
#188474,#188475,#188476),(#188477,#188478,#188479,#188480,#188481,#188482,
#188483,#188484,#188485),(#188486,#188487,#188488,#188489,#188490,#188491,
#188492,#188493,#188494),(#188495,#188496,#188497,#188498,#188499,#188500,
#188501,#188502,#188503),(#188504,#188505,#188506,#188507,#188508,#188509,
#188510,#188511,#188512),(#188513,#188514,#188515,#188516,#188517,#188518,
#188519,#188520,#188521),(#188522,#188523,#188524,#188525,#188526,#188527,
#188528,#188529,#188530),(#188531,#188532,#188533,#188534,#188535,#188536,
#188537,#188538,#188539),(#188540,#188541,#188542,#188543,#188544,#188545,
#188546,#188547,#188548),(#188549,#188550,#188551,#188552,#188553,#188554,
#188555,#188556,#188557),(#188558,#188559,#188560,#188561,#188562,#188563,
#188564,#188565,#188566),(#188567,#188568,#188569,#188570,#188571,#188572,
#188573,#188574,#188575),(#188576,#188577,#188578,#188579,#188580,#188581,
#188582,#188583,#188584),(#188585,#188586,#188587,#188588,#188589,#188590,
#188591,#188592,#188593),(#188594,#188595,#188596,#188597,#188598,#188599,
#188600,#188601,#188602),(#188603,#188604,#188605,#188606,#188607,#188608,
#188609,#188610,#188611),(#188612,#188613,#188614,#188615,#188616,#188617,
#188618,#188619,#188620),(#188621,#188622,#188623,#188624,#188625,#188626,
#188627,#188628,#188629),(#188630,#188631,#188632,#188633,#188634,#188635,
#188636,#188637,#188638),(#188639,#188640,#188641,#188642,#188643,#188644,
#188645,#188646,#188647),(#188648,#188649,#188650,#188651,#188652,#188653,
#188654,#188655,#188656),(#188657,#188658,#188659,#188660,#188661,#188662,
#188663,#188664,#188665),(#188666,#188667,#188668,#188669,#188670,#188671,
#188672,#188673,#188674),(#188675,#188676,#188677,#188678,#188679,#188680,
#188681,#188682,#188683),(#188684,#188685,#188686,#188687,#188688,#188689,
#188690,#188691,#188692),(#188693,#188694,#188695,#188696,#188697,#188698,
#188699,#188700,#188701),(#188702,#188703,#188704,#188705,#188706,#188707,
#188708,#188709,#188710),(#188711,#188712,#188713,#188714,#188715,#188716,
#188717,#188718,#188719),(#188720,#188721,#188722,#188723,#188724,#188725,
#188726,#188727,#188728),(#188729,#188730,#188731,#188732,#188733,#188734,
#188735,#188736,#188737),(#188738,#188739,#188740,#188741,#188742,#188743,
#188744,#188745,#188746),(#188747,#188748,#188749,#188750,#188751,#188752,
#188753,#188754,#188755),(#188756,#188757,#188758,#188759,#188760,#188761,
#188762,#188763,#188764),(#188765,#188766,#188767,#188768,#188769,#188770,
#188771,#188772,#188773),(#188774,#188775,#188776,#188777,#188778,#188779,
#188780,#188781,#188782),(#188783,#188784,#188785,#188786,#188787,#188788,
#188789,#188790,#188791),(#188792,#188793,#188794,#188795,#188796,#188797,
#188798,#188799,#188800),(#188801,#188802,#188803,#188804,#188805,#188806,
#188807,#188808,#188809),(#188810,#188811,#188812,#188813,#188814,#188815,
#188816,#188817,#188818),(#188819,#188820,#188821,#188822,#188823,#188824,
#188825,#188826,#188827),(#188828,#188829,#188830,#188831,#188832,#188833,
#188834,#188835,#188836),(#188837,#188838,#188839,#188840,#188841,#188842,
#188843,#188844,#188845),(#188846,#188847,#188848,#188849,#188850,#188851,
#188852,#188853,#188854),(#188855,#188856,#188857,#188858,#188859,#188860,
#188861,#188862,#188863),(#188864,#188865,#188866,#188867,#188868,#188869,
#188870,#188871,#188872),(#188873,#188874,#188875,#188876,#188877,#188878,
#188879,#188880,#188881),(#188882,#188883,#188884,#188885,#188886,#188887,
#188888,#188889,#188890),(#188891,#188892,#188893,#188894,#188895,#188896,
#188897,#188898,#188899),(#188900,#188901,#188902,#188903,#188904,#188905,
#188906,#188907,#188908),(#188909,#188910,#188911,#188912,#188913,#188914,
#188915,#188916,#188917),(#188918,#188919,#188920,#188921,#188922,#188923,
#188924,#188925,#188926),(#188927,#188928,#188929,#188930,#188931,#188932,
#188933,#188934,#188935),(#188936,#188937,#188938,#188939,#188940,#188941,
#188942,#188943,#188944),(#188945,#188946,#188947,#188948,#188949,#188950,
#188951,#188952,#188953),(#188954,#188955,#188956,#188957,#188958,#188959,
#188960,#188961,#188962),(#188963,#188964,#188965,#188966,#188967,#188968,
#188969,#188970,#188971),(#188972,#188973,#188974,#188975,#188976,#188977,
#188978,#188979,#188980),(#188981,#188982,#188983,#188984,#188985,#188986,
#188987,#188988,#188989),(#188990,#188991,#188992,#188993,#188994,#188995,
#188996,#188997,#188998),(#188999,#189000,#189001,#189002,#189003,#189004,
#189005,#189006,#189007),(#189008,#189009,#189010,#189011,#189012,#189013,
#189014,#189015,#189016),(#189017,#189018,#189019,#189020,#189021,#189022,
#189023,#189024,#189025),(#189026,#189027,#189028,#189029,#189030,#189031,
#189032,#189033,#189034),(#189035,#189036,#189037,#189038,#189039,#189040,
#189041,#189042,#189043),(#189044,#189045,#189046,#189047,#189048,#189049,
#189050,#189051,#189052),(#189053,#189054,#189055,#189056,#189057,#189058,
#189059,#189060,#189061),(#189062,#189063,#189064,#189065,#189066,#189067,
#189068,#189069,#189070),(#189071,#189072,#189073,#189074,#189075,#189076,
#189077,#189078,#189079),(#189080,#189081,#189082,#189083,#189084,#189085,
#189086,#189087,#189088),(#189089,#189090,#189091,#189092,#189093,#189094,
#189095,#189096,#189097),(#189098,#189099,#189100,#189101,#189102,#189103,
#189104,#189105,#189106),(#189107,#189108,#189109,#189110,#189111,#189112,
#189113,#189114,#189115),(#189116,#189117,#189118,#189119,#189120,#189121,
#189122,#189123,#189124),(#189125,#189126,#189127,#189128,#189129,#189130,
#189131,#189132,#189133),(#189134,#189135,#189136,#189137,#189138,#189139,
#189140,#189141,#189142),(#189143,#189144,#189145,#189146,#189147,#189148,
#189149,#189150,#189151),(#189152,#189153,#189154,#189155,#189156,#189157,
#189158,#189159,#189160),(#189161,#189162,#189163,#189164,#189165,#189166,
#189167,#189168,#189169),(#189170,#189171,#189172,#189173,#189174,#189175,
#189176,#189177,#189178),(#189179,#189180,#189181,#189182,#189183,#189184,
#189185,#189186,#189187),(#189188,#189189,#189190,#189191,#189192,#189193,
#189194,#189195,#189196),(#189197,#189198,#189199,#189200,#189201,#189202,
#189203,#189204,#189205),(#189206,#189207,#189208,#189209,#189210,#189211,
#189212,#189213,#189214),(#189215,#189216,#189217,#189218,#189219,#189220,
#189221,#189222,#189223),(#189224,#189225,#189226,#189227,#189228,#189229,
#189230,#189231,#189232),(#189233,#189234,#189235,#189236,#189237,#189238,
#189239,#189240,#189241),(#189242,#189243,#189244,#189245,#189246,#189247,
#189248,#189249,#189250),(#189251,#189252,#189253,#189254,#189255,#189256,
#189257,#189258,#189259),(#189260,#189261,#189262,#189263,#189264,#189265,
#189266,#189267,#189268),(#189269,#189270,#189271,#189272,#189273,#189274,
#189275,#189276,#189277),(#189278,#189279,#189280,#189281,#189282,#189283,
#189284,#189285,#189286),(#189287,#189288,#189289,#189290,#189291,#189292,
#189293,#189294,#189295),(#189296,#189297,#189298,#189299,#189300,#189301,
#189302,#189303,#189304),(#189305,#189306,#189307,#189308,#189309,#189310,
#189311,#189312,#189313),(#189314,#189315,#189316,#189317,#189318,#189319,
#189320,#189321,#189322),(#189323,#189324,#189325,#189326,#189327,#189328,
#189329,#189330,#189331),(#189332,#189333,#189334,#189335,#189336,#189337,
#189338,#189339,#189340),(#189341,#189342,#189343,#189344,#189345,#189346,
#189347,#189348,#189349),(#189350,#189351,#189352,#189353,#189354,#189355,
#189356,#189357,#189358),(#189359,#189360,#189361,#189362,#189363,#189364,
#189365,#189366,#189367),(#189368,#189369,#189370,#189371,#189372,#189373,
#189374,#189375,#189376),(#189377,#189378,#189379,#189380,#189381,#189382,
#189383,#189384,#189385),(#189386,#189387,#189388,#189389,#189390,#189391,
#189392,#189393,#189394),(#189395,#189396,#189397,#189398,#189399,#189400,
#189401,#189402,#189403),(#189404,#189405,#189406,#189407,#189408,#189409,
#189410,#189411,#189412),(#189413,#189414,#189415,#189416,#189417,#189418,
#189419,#189420,#189421),(#189422,#189423,#189424,#189425,#189426,#189427,
#189428,#189429,#189430),(#189431,#189432,#189433,#189434,#189435,#189436,
#189437,#189438,#189439),(#189440,#189441,#189442,#189443,#189444,#189445,
#189446,#189447,#189448),(#189449,#189450,#189451,#189452,#189453,#189454,
#189455,#189456,#189457),(#189458,#189459,#189460,#189461,#189462,#189463,
#189464,#189465,#189466),(#189467,#189468,#189469,#189470,#189471,#189472,
#189473,#189474,#189475),(#189476,#189477,#189478,#189479,#189480,#189481,
#189482,#189483,#189484),(#189485,#189486,#189487,#189488,#189489,#189490,
#189491,#189492,#189493),(#189494,#189495,#189496,#189497,#189498,#189499,
#189500,#189501,#189502),(#189503,#189504,#189505,#189506,#189507,#189508,
#189509,#189510,#189511),(#189512,#189513,#189514,#189515,#189516,#189517,
#189518,#189519,#189520),(#189521,#189522,#189523,#189524,#189525,#189526,
#189527,#189528,#189529),(#189530,#189531,#189532,#189533,#189534,#189535,
#189536,#189537,#189538),(#189539,#189540,#189541,#189542,#189543,#189544,
#189545,#189546,#189547),(#189548,#189549,#189550,#189551,#189552,#189553,
#189554,#189555,#189556),(#189557,#189558,#189559,#189560,#189561,#189562,
#189563,#189564,#189565),(#189566,#189567,#189568,#189569,#189570,#189571,
#189572,#189573,#189574),(#189575,#189576,#189577,#189578,#189579,#189580,
#189581,#189582,#189583),(#189584,#189585,#189586,#189587,#189588,#189589,
#189590,#189591,#189592),(#189593,#189594,#189595,#189596,#189597,#189598,
#189599,#189600,#189601),(#189602,#189603,#189604,#189605,#189606,#189607,
#189608,#189609,#189610),(#189611,#189612,#189613,#189614,#189615,#189616,
#189617,#189618,#189619),(#189620,#189621,#189622,#189623,#189624,#189625,
#189626,#189627,#189628),(#189629,#189630,#189631,#189632,#189633,#189634,
#189635,#189636,#189637),(#189638,#189639,#189640,#189641,#189642,#189643,
#189644,#189645,#189646),(#189647,#189648,#189649,#189650,#189651,#189652,
#189653,#189654,#189655),(#189656,#189657,#189658,#189659,#189660,#189661,
#189662,#189663,#189664),(#189665,#189666,#189667,#189668,#189669,#189670,
#189671,#189672,#189673),(#189674,#189675,#189676,#189677,#189678,#189679,
#189680,#189681,#189682),(#189683,#189684,#189685,#189686,#189687,#189688,
#189689,#189690,#189691),(#189692,#189693,#189694,#189695,#189696,#189697,
#189698,#189699,#189700),(#189701,#189702,#189703,#189704,#189705,#189706,
#189707,#189708,#189709),(#189710,#189711,#189712,#189713,#189714,#189715,
#189716,#189717,#189718),(#189719,#189720,#189721,#189722,#189723,#189724,
#189725,#189726,#189727),(#189728,#189729,#189730,#189731,#189732,#189733,
#189734,#189735,#189736),(#189737,#189738,#189739,#189740,#189741,#189742,
#189743,#189744,#189745),(#189746,#189747,#189748,#189749,#189750,#189751,
#189752,#189753,#189754),(#189755,#189756,#189757,#189758,#189759,#189760,
#189761,#189762,#189763),(#189764,#189765,#189766,#189767,#189768,#189769,
#189770,#189771,#189772),(#189773,#189774,#189775,#189776,#189777,#189778,
#189779,#189780,#189781),(#189782,#189783,#189784,#189785,#189786,#189787,
#189788,#189789,#189790),(#189791,#189792,#189793,#189794,#189795,#189796,
#189797,#189798,#189799),(#189800,#189801,#189802,#189803,#189804,#189805,
#189806,#189807,#189808),(#189809,#189810,#189811,#189812,#189813,#189814,
#189815,#189816,#189817),(#189818,#189819,#189820,#189821,#189822,#189823,
#189824,#189825,#189826),(#189827,#189828,#189829,#189830,#189831,#189832,
#189833,#189834,#189835),(#189836,#189837,#189838,#189839,#189840,#189841,
#189842,#189843,#189844),(#189845,#189846,#189847,#189848,#189849,#189850,
#189851,#189852,#189853),(#189854,#189855,#189856,#189857,#189858,#189859,
#189860,#189861,#189862),(#189863,#189864,#189865,#189866,#189867,#189868,
#189869,#189870,#189871),(#189872,#189873,#189874,#189875,#189876,#189877,
#189878,#189879,#189880),(#189881,#189882,#189883,#189884,#189885,#189886,
#189887,#189888,#189889),(#189890,#189891,#189892,#189893,#189894,#189895,
#189896,#189897,#189898),(#189899,#189900,#189901,#189902,#189903,#189904,
#189905,#189906,#189907),(#189908,#189909,#189910,#189911,#189912,#189913,
#189914,#189915,#189916),(#189917,#189918,#189919,#189920,#189921,#189922,
#189923,#189924,#189925),(#189926,#189927,#189928,#189929,#189930,#189931,
#189932,#189933,#189934),(#189935,#189936,#189937,#189938,#189939,#189940,
#189941,#189942,#189943),(#189944,#189945,#189946,#189947,#189948,#189949,
#189950,#189951,#189952),(#189953,#189954,#189955,#189956,#189957,#189958,
#189959,#189960,#189961),(#189962,#189963,#189964,#189965,#189966,#189967,
#189968,#189969,#189970),(#189971,#189972,#189973,#189974,#189975,#189976,
#189977,#189978,#189979),(#189980,#189981,#189982,#189983,#189984,#189985,
#189986,#189987,#189988),(#189989,#189990,#189991,#189992,#189993,#189994,
#189995,#189996,#189997),(#189998,#189999,#190000,#190001,#190002,#190003,
#190004,#190005,#190006),(#190007,#190008,#190009,#190010,#190011,#190012,
#190013,#190014,#190015),(#190016,#190017,#190018,#190019,#190020,#190021,
#190022,#190023,#190024),(#190025,#190026,#190027,#190028,#190029,#190030,
#190031,#190032,#190033),(#190034,#190035,#190036,#190037,#190038,#190039,
#190040,#190041,#190042),(#190043,#190044,#190045,#190046,#190047,#190048,
#190049,#190050,#190051),(#190052,#190053,#190054,#190055,#190056,#190057,
#190058,#190059,#190060),(#190061,#190062,#190063,#190064,#190065,#190066,
#190067,#190068,#190069),(#190070,#190071,#190072,#190073,#190074,#190075,
#190076,#190077,#190078),(#190079,#190080,#190081,#190082,#190083,#190084,
#190085,#190086,#190087),(#190088,#190089,#190090,#190091,#190092,#190093,
#190094,#190095,#190096),(#190097,#190098,#190099,#190100,#190101,#190102,
#190103,#190104,#190105),(#190106,#190107,#190108,#190109,#190110,#190111,
#190112,#190113,#190114),(#190115,#190116,#190117,#190118,#190119,#190120,
#190121,#190122,#190123),(#190124,#190125,#190126,#190127,#190128,#190129,
#190130,#190131,#190132),(#190133,#190134,#190135,#190136,#190137,#190138,
#190139,#190140,#190141),(#190142,#190143,#190144,#190145,#190146,#190147,
#190148,#190149,#190150),(#190151,#190152,#190153,#190154,#190155,#190156,
#190157,#190158,#190159),(#190160,#190161,#190162,#190163,#190164,#190165,
#190166,#190167,#190168),(#190169,#190170,#190171,#190172,#190173,#190174,
#190175,#190176,#190177),(#190178,#190179,#190180,#190181,#190182,#190183,
#190184,#190185,#190186),(#190187,#190188,#190189,#190190,#190191,#190192,
#190193,#190194,#190195),(#190196,#190197,#190198,#190199,#190200,#190201,
#190202,#190203,#190204),(#190205,#190206,#190207,#190208,#190209,#190210,
#190211,#190212,#190213),(#190214,#190215,#190216,#190217,#190218,#190219,
#190220,#190221,#190222),(#190223,#190224,#190225,#190226,#190227,#190228,
#190229,#190230,#190231),(#190232,#190233,#190234,#190235,#190236,#190237,
#190238,#190239,#190240),(#190241,#190242,#190243,#190244,#190245,#190246,
#190247,#190248,#190249),(#190250,#190251,#190252,#190253,#190254,#190255,
#190256,#190257,#190258),(#190259,#190260,#190261,#190262,#190263,#190264,
#190265,#190266,#190267),(#190268,#190269,#190270,#190271,#190272,#190273,
#190274,#190275,#190276),(#190277,#190278,#190279,#190280,#190281,#190282,
#190283,#190284,#190285),(#190286,#190287,#190288,#190289,#190290,#190291,
#190292,#190293,#190294),(#190295,#190296,#190297,#190298,#190299,#190300,
#190301,#190302,#190303),(#190304,#190305,#190306,#190307,#190308,#190309,
#190310,#190311,#190312),(#190313,#190314,#190315,#190316,#190317,#190318,
#190319,#190320,#190321),(#190322,#190323,#190324,#190325,#190326,#190327,
#190328,#190329,#190330),(#190331,#190332,#190333,#190334,#190335,#190336,
#190337,#190338,#190339),(#190340,#190341,#190342,#190343,#190344,#190345,
#190346,#190347,#190348),(#190349,#190350,#190351,#190352,#190353,#190354,
#190355,#190356,#190357),(#190358,#190359,#190360,#190361,#190362,#190363,
#190364,#190365,#190366),(#190367,#190368,#190369,#190370,#190371,#190372,
#190373,#190374,#190375),(#190376,#190377,#190378,#190379,#190380,#190381,
#190382,#190383,#190384),(#190385,#190386,#190387,#190388,#190389,#190390,
#190391,#190392,#190393),(#190394,#190395,#190396,#190397,#190398,#190399,
#190400,#190401,#190402),(#190403,#190404,#190405,#190406,#190407,#190408,
#190409,#190410,#190411),(#190412,#190413,#190414,#190415,#190416,#190417,
#190418,#190419,#190420),(#190421,#190422,#190423,#190424,#190425,#190426,
#190427,#190428,#190429),(#190430,#190431,#190432,#190433,#190434,#190435,
#190436,#190437,#190438),(#190439,#190440,#190441,#190442,#190443,#190444,
#190445,#190446,#190447),(#190448,#190449,#190450,#190451,#190452,#190453,
#190454,#190455,#190456),(#190457,#190458,#190459,#190460,#190461,#190462,
#190463,#190464,#190465),(#190466,#190467,#190468,#190469,#190470,#190471,
#190472,#190473,#190474),(#190475,#190476,#190477,#190478,#190479,#190480,
#190481,#190482,#190483),(#190484,#190485,#190486,#190487,#190488,#190489,
#190490,#190491,#190492),(#190493,#190494,#190495,#190496,#190497,#190498,
#190499,#190500,#190501),(#190502,#190503,#190504,#190505,#190506,#190507,
#190508,#190509,#190510),(#190511,#190512,#190513,#190514,#190515,#190516,
#190517,#190518,#190519),(#190520,#190521,#190522,#190523,#190524,#190525,
#190526,#190527,#190528),(#190529,#190530,#190531,#190532,#190533,#190534,
#190535,#190536,#190537),(#190538,#190539,#190540,#190541,#190542,#190543,
#190544,#190545,#190546),(#190547,#190548,#190549,#190550,#190551,#190552,
#190553,#190554,#190555),(#190556,#190557,#190558,#190559,#190560,#190561,
#190562,#190563,#190564),(#190565,#190566,#190567,#190568,#190569,#190570,
#190571,#190572,#190573),(#190574,#190575,#190576,#190577,#190578,#190579,
#190580,#190581,#190582),(#190583,#190584,#190585,#190586,#190587,#190588,
#190589,#190590,#190591),(#190592,#190593,#190594,#190595,#190596,#190597,
#190598,#190599,#190600),(#190601,#190602,#190603,#190604,#190605,#190606,
#190607,#190608,#190609),(#190610,#190611,#190612,#190613,#190614,#190615,
#190616,#190617,#190618),(#190619,#190620,#190621,#190622,#190623,#190624,
#190625,#190626,#190627),(#190628,#190629,#190630,#190631,#190632,#190633,
#190634,#190635,#190636),(#190637,#190638,#190639,#190640,#190641,#190642,
#190643,#190644,#190645),(#190646,#190647,#190648,#190649,#190650,#190651,
#190652,#190653,#190654),(#190655,#190656,#190657,#190658,#190659,#190660,
#190661,#190662,#190663),(#190664,#190665,#190666,#190667,#190668,#190669,
#190670,#190671,#190672),(#190673,#190674,#190675,#190676,#190677,#190678,
#190679,#190680,#190681),(#190682,#190683,#190684,#190685,#190686,#190687,
#190688,#190689,#190690),(#190691,#190692,#190693,#190694,#190695,#190696,
#190697,#190698,#190699),(#190700,#190701,#190702,#190703,#190704,#190705,
#190706,#190707,#190708),(#190709,#190710,#190711,#190712,#190713,#190714,
#190715,#190716,#190717),(#190718,#190719,#190720,#190721,#190722,#190723,
#190724,#190725,#190726),(#190727,#190728,#190729,#190730,#190731,#190732,
#190733,#190734,#190735),(#190736,#190737,#190738,#190739,#190740,#190741,
#190742,#190743,#190744),(#190745,#190746,#190747,#190748,#190749,#190750,
#190751,#190752,#190753),(#190754,#190755,#190756,#190757,#190758,#190759,
#190760,#190761,#190762),(#190763,#190764,#190765,#190766,#190767,#190768,
#190769,#190770,#190771),(#190772,#190773,#190774,#190775,#190776,#190777,
#190778,#190779,#190780),(#190781,#190782,#190783,#190784,#190785,#190786,
#190787,#190788,#190789),(#190790,#190791,#190792,#190793,#190794,#190795,
#190796,#190797,#190798),(#190799,#190800,#190801,#190802,#190803,#190804,
#190805,#190806,#190807),(#190808,#190809,#190810,#190811,#190812,#190813,
#190814,#190815,#190816),(#190817,#190818,#190819,#190820,#190821,#190822,
#190823,#190824,#190825),(#190826,#190827,#190828,#190829,#190830,#190831,
#190832,#190833,#190834),(#190835,#190836,#190837,#190838,#190839,#190840,
#190841,#190842,#190843),(#190844,#190845,#190846,#190847,#190848,#190849,
#190850,#190851,#190852),(#190853,#190854,#190855,#190856,#190857,#190858,
#190859,#190860,#190861),(#190862,#190863,#190864,#190865,#190866,#190867,
#190868,#190869,#190870),(#190871,#190872,#190873,#190874,#190875,#190876,
#190877,#190878,#190879),(#190880,#190881,#190882,#190883,#190884,#190885,
#190886,#190887,#190888),(#190889,#190890,#190891,#190892,#190893,#190894,
#190895,#190896,#190897),(#190898,#190899,#190900,#190901,#190902,#190903,
#190904,#190905,#190906),(#190907,#190908,#190909,#190910,#190911,#190912,
#190913,#190914,#190915),(#190916,#190917,#190918,#190919,#190920,#190921,
#190922,#190923,#190924),(#190925,#190926,#190927,#190928,#190929,#190930,
#190931,#190932,#190933),(#190934,#190935,#190936,#190937,#190938,#190939,
#190940,#190941,#190942),(#190943,#190944,#190945,#190946,#190947,#190948,
#190949,#190950,#190951),(#190952,#190953,#190954,#190955,#190956,#190957,
#190958,#190959,#190960),(#190961,#190962,#190963,#190964,#190965,#190966,
#190967,#190968,#190969),(#190970,#190971,#190972,#190973,#190974,#190975,
#190976,#190977,#190978),(#190979,#190980,#190981,#190982,#190983,#190984,
#190985,#190986,#190987),(#190988,#190989,#190990,#190991,#190992,#190993,
#190994,#190995,#190996),(#190997,#190998,#190999,#191000,#191001,#191002,
#191003,#191004,#191005),(#191006,#191007,#191008,#191009,#191010,#191011,
#191012,#191013,#191014),(#191015,#191016,#191017,#191018,#191019,#191020,
#191021,#191022,#191023),(#191024,#191025,#191026,#191027,#191028,#191029,
#191030,#191031,#191032),(#191033,#191034,#191035,#191036,#191037,#191038,
#191039,#191040,#191041),(#191042,#191043,#191044,#191045,#191046,#191047,
#191048,#191049,#191050),(#191051,#191052,#191053,#191054,#191055,#191056,
#191057,#191058,#191059),(#191060,#191061,#191062,#191063,#191064,#191065,
#191066,#191067,#191068),(#191069,#191070,#191071,#191072,#191073,#191074,
#191075,#191076,#191077),(#191078,#191079,#191080,#191081,#191082,#191083,
#191084,#191085,#191086),(#191087,#191088,#191089,#191090,#191091,#191092,
#191093,#191094,#191095),(#191096,#191097,#191098,#191099,#191100,#191101,
#191102,#191103,#191104),(#191105,#191106,#191107,#191108,#191109,#191110,
#191111,#191112,#191113),(#191114,#191115,#191116,#191117,#191118,#191119,
#191120,#191121,#191122),(#191123,#191124,#191125,#191126,#191127,#191128,
#191129,#191130,#191131),(#191132,#191133,#191134,#191135,#191136,#191137,
#191138,#191139,#191140),(#191141,#191142,#191143,#191144,#191145,#191146,
#191147,#191148,#191149),(#191150,#191151,#191152,#191153,#191154,#191155,
#191156,#191157,#191158),(#191159,#191160,#191161,#191162,#191163,#191164,
#191165,#191166,#191167),(#191168,#191169,#191170,#191171,#191172,#191173,
#191174,#191175,#191176),(#191177,#191178,#191179,#191180,#191181,#191182,
#191183,#191184,#191185),(#191186,#191187,#191188,#191189,#191190,#191191,
#191192,#191193,#191194),(#191195,#191196,#191197,#191198,#191199,#191200,
#191201,#191202,#191203),(#191204,#191205,#191206,#191207,#191208,#191209,
#191210,#191211,#191212),(#191213,#191214,#191215,#191216,#191217,#191218,
#191219,#191220,#191221),(#191222,#191223,#191224,#191225,#191226,#191227,
#191228,#191229,#191230),(#191231,#191232,#191233,#191234,#191235,#191236,
#191237,#191238,#191239),(#191240,#191241,#191242,#191243,#191244,#191245,
#191246,#191247,#191248),(#191249,#191250,#191251,#191252,#191253,#191254,
#191255,#191256,#191257),(#191258,#191259,#191260,#191261,#191262,#191263,
#191264,#191265,#191266),(#191267,#191268,#191269,#191270,#191271,#191272,
#191273,#191274,#191275),(#191276,#191277,#191278,#191279,#191280,#191281,
#191282,#191283,#191284),(#191285,#191286,#191287,#191288,#191289,#191290,
#191291,#191292,#191293),(#191294,#191295,#191296,#191297,#191298,#191299,
#191300,#191301,#191302),(#191303,#191304,#191305,#191306,#191307,#191308,
#191309,#191310,#191311),(#191312,#191313,#191314,#191315,#191316,#191317,
#191318,#191319,#191320),(#191321,#191322,#191323,#191324,#191325,#191326,
#191327,#191328,#191329),(#191330,#191331,#191332,#191333,#191334,#191335,
#191336,#191337,#191338),(#191339,#191340,#191341,#191342,#191343,#191344,
#191345,#191346,#191347),(#191348,#191349,#191350,#191351,#191352,#191353,
#191354,#191355,#191356),(#191357,#191358,#191359,#191360,#191361,#191362,
#191363,#191364,#191365),(#191366,#191367,#191368,#191369,#191370,#191371,
#191372,#191373,#191374),(#191375,#191376,#191377,#191378,#191379,#191380,
#191381,#191382,#191383),(#191384,#191385,#191386,#191387,#191388,#191389,
#191390,#191391,#191392),(#191393,#191394,#191395,#191396,#191397,#191398,
#191399,#191400,#191401),(#191402,#191403,#191404,#191405,#191406,#191407,
#191408,#191409,#191410),(#191411,#191412,#191413,#191414,#191415,#191416,
#191417,#191418,#191419),(#191420,#191421,#191422,#191423,#191424,#191425,
#191426,#191427,#191428),(#191429,#191430,#191431,#191432,#191433,#191434,
#191435,#191436,#191437),(#191438,#191439,#191440,#191441,#191442,#191443,
#191444,#191445,#191446),(#191447,#191448,#191449,#191450,#191451,#191452,
#191453,#191454,#191455),(#191456,#191457,#191458,#191459,#191460,#191461,
#191462,#191463,#191464),(#191465,#191466,#191467,#191468,#191469,#191470,
#191471,#191472,#191473),(#191474,#191475,#191476,#191477,#191478,#191479,
#191480,#191481,#191482),(#191483,#191484,#191485,#191486,#191487,#191488,
#191489,#191490,#191491),(#191492,#191493,#191494,#191495,#191496,#191497,
#191498,#191499,#191500),(#191501,#191502,#191503,#191504,#191505,#191506,
#191507,#191508,#191509),(#191510,#191511,#191512,#191513,#191514,#191515,
#191516,#191517,#191518),(#191519,#191520,#191521,#191522,#191523,#191524,
#191525,#191526,#191527),(#191528,#191529,#191530,#191531,#191532,#191533,
#191534,#191535,#191536),(#191537,#191538,#191539,#191540,#191541,#191542,
#191543,#191544,#191545),(#191546,#191547,#191548,#191549,#191550,#191551,
#191552,#191553,#191554),(#191555,#191556,#191557,#191558,#191559,#191560,
#191561,#191562,#191563),(#191564,#191565,#191566,#191567,#191568,#191569,
#191570,#191571,#191572),(#191573,#191574,#191575,#191576,#191577,#191578,
#191579,#191580,#191581),(#191582,#191583,#191584,#191585,#191586,#191587,
#191588,#191589,#191590),(#191591,#191592,#191593,#191594,#191595,#191596,
#191597,#191598,#191599),(#191600,#191601,#191602,#191603,#191604,#191605,
#191606,#191607,#191608),(#191609,#191610,#191611,#191612,#191613,#191614,
#191615,#191616,#191617),(#191618,#191619,#191620,#191621,#191622,#191623,
#191624,#191625,#191626),(#191627,#191628,#191629,#191630,#191631,#191632,
#191633,#191634,#191635),(#191636,#191637,#191638,#191639,#191640,#191641,
#191642,#191643,#191644),(#191645,#191646,#191647,#191648,#191649,#191650,
#191651,#191652,#191653),(#191654,#191655,#191656,#191657,#191658,#191659,
#191660,#191661,#191662),(#191663,#191664,#191665,#191666,#191667,#191668,
#191669,#191670,#191671),(#191672,#191673,#191674,#191675,#191676,#191677,
#191678,#191679,#191680),(#191681,#191682,#191683,#191684,#191685,#191686,
#191687,#191688,#191689),(#191690,#191691,#191692,#191693,#191694,#191695,
#191696,#191697,#191698),(#191699,#191700,#191701,#191702,#191703,#191704,
#191705,#191706,#191707),(#191708,#191709,#191710,#191711,#191712,#191713,
#191714,#191715,#191716),(#191717,#191718,#191719,#191720,#191721,#191722,
#191723,#191724,#191725),(#191726,#191727,#191728,#191729,#191730,#191731,
#191732,#191733,#191734),(#191735,#191736,#191737,#191738,#191739,#191740,
#191741,#191742,#191743),(#191744,#191745,#191746,#191747,#191748,#191749,
#191750,#191751,#191752),(#191753,#191754,#191755,#191756,#191757,#191758,
#191759,#191760,#191761),(#191762,#191763,#191764,#191765,#191766,#191767,
#191768,#191769,#191770),(#191771,#191772,#191773,#191774,#191775,#191776,
#191777,#191778,#191779),(#191780,#191781,#191782,#191783,#191784,#191785,
#191786,#191787,#191788),(#191789,#191790,#191791,#191792,#191793,#191794,
#191795,#191796,#191797),(#191798,#191799,#191800,#191801,#191802,#191803,
#191804,#191805,#191806),(#191807,#191808,#191809,#191810,#191811,#191812,
#191813,#191814,#191815),(#191816,#191817,#191818,#191819,#191820,#191821,
#191822,#191823,#191824),(#191825,#191826,#191827,#191828,#191829,#191830,
#191831,#191832,#191833),(#191834,#191835,#191836,#191837,#191838,#191839,
#191840,#191841,#191842),(#191843,#191844,#191845,#191846,#191847,#191848,
#191849,#191850,#191851),(#191852,#191853,#191854,#191855,#191856,#191857,
#191858,#191859,#191860),(#191861,#191862,#191863,#191864,#191865,#191866,
#191867,#191868,#191869),(#191870,#191871,#191872,#191873,#191874,#191875,
#191876,#191877,#191878),(#191879,#191880,#191881,#191882,#191883,#191884,
#191885,#191886,#191887),(#191888,#191889,#191890,#191891,#191892,#191893,
#191894,#191895,#191896),(#191897,#191898,#191899,#191900,#191901,#191902,
#191903,#191904,#191905),(#191906,#191907,#191908,#191909,#191910,#191911,
#191912,#191913,#191914),(#191915,#191916,#191917,#191918,#191919,#191920,
#191921,#191922,#191923),(#191924,#191925,#191926,#191927,#191928,#191929,
#191930,#191931,#191932),(#191933,#191934,#191935,#191936,#191937,#191938,
#191939,#191940,#191941),(#191942,#191943,#191944,#191945,#191946,#191947,
#191948,#191949,#191950),(#191951,#191952,#191953,#191954,#191955,#191956,
#191957,#191958,#191959),(#191960,#191961,#191962,#191963,#191964,#191965,
#191966,#191967,#191968),(#191969,#191970,#191971,#191972,#191973,#191974,
#191975,#191976,#191977),(#191978,#191979,#191980,#191981,#191982,#191983,
#191984,#191985,#191986),(#191987,#191988,#191989,#191990,#191991,#191992,
#191993,#191994,#191995),(#191996,#191997,#191998,#191999,#192000,#192001,
#192002,#192003,#192004),(#192005,#192006,#192007,#192008,#192009,#192010,
#192011,#192012,#192013),(#192014,#192015,#192016,#192017,#192018,#192019,
#192020,#192021,#192022),(#192023,#192024,#192025,#192026,#192027,#192028,
#192029,#192030,#192031),(#192032,#192033,#192034,#192035,#192036,#192037,
#192038,#192039,#192040),(#192041,#192042,#192043,#192044,#192045,#192046,
#192047,#192048,#192049),(#192050,#192051,#192052,#192053,#192054,#192055,
#192056,#192057,#192058),(#192059,#192060,#192061,#192062,#192063,#192064,
#192065,#192066,#192067),(#192068,#192069,#192070,#192071,#192072,#192073,
#192074,#192075,#192076),(#192077,#192078,#192079,#192080,#192081,#192082,
#192083,#192084,#192085),(#192086,#192087,#192088,#192089,#192090,#192091,
#192092,#192093,#192094),(#192095,#192096,#192097,#192098,#192099,#192100,
#192101,#192102,#192103),(#192104,#192105,#192106,#192107,#192108,#192109,
#192110,#192111,#192112),(#192113,#192114,#192115,#192116,#192117,#192118,
#192119,#192120,#192121),(#192122,#192123,#192124,#192125,#192126,#192127,
#192128,#192129,#192130),(#192131,#192132,#192133,#192134,#192135,#192136,
#192137,#192138,#192139),(#192140,#192141,#192142,#192143,#192144,#192145,
#192146,#192147,#192148),(#192149,#192150,#192151,#192152,#192153,#192154,
#192155,#192156,#192157),(#192158,#192159,#192160,#192161,#192162,#192163,
#192164,#192165,#192166),(#192167,#192168,#192169,#192170,#192171,#192172,
#192173,#192174,#192175),(#192176,#192177,#192178,#192179,#192180,#192181,
#192182,#192183,#192184),(#192185,#192186,#192187,#192188,#192189,#192190,
#192191,#192192,#192193),(#192194,#192195,#192196,#192197,#192198,#192199,
#192200,#192201,#192202),(#192203,#192204,#192205,#192206,#192207,#192208,
#192209,#192210,#192211),(#192212,#192213,#192214,#192215,#192216,#192217,
#192218,#192219,#192220),(#192221,#192222,#192223,#192224,#192225,#192226,
#192227,#192228,#192229),(#192230,#192231,#192232,#192233,#192234,#192235,
#192236,#192237,#192238),(#192239,#192240,#192241,#192242,#192243,#192244,
#192245,#192246,#192247),(#192248,#192249,#192250,#192251,#192252,#192253,
#192254,#192255,#192256),(#192257,#192258,#192259,#192260,#192261,#192262,
#192263,#192264,#192265),(#192266,#192267,#192268,#192269,#192270,#192271,
#192272,#192273,#192274),(#192275,#192276,#192277,#192278,#192279,#192280,
#192281,#192282,#192283),(#192284,#192285,#192286,#192287,#192288,#192289,
#192290,#192291,#192292),(#192293,#192294,#192295,#192296,#192297,#192298,
#192299,#192300,#192301),(#192302,#192303,#192304,#192305,#192306,#192307,
#192308,#192309,#192310),(#192311,#192312,#192313,#192314,#192315,#192316,
#192317,#192318,#192319),(#192320,#192321,#192322,#192323,#192324,#192325,
#192326,#192327,#192328),(#192329,#192330,#192331,#192332,#192333,#192334,
#192335,#192336,#192337),(#192338,#192339,#192340,#192341,#192342,#192343,
#192344,#192345,#192346),(#192347,#192348,#192349,#192350,#192351,#192352,
#192353,#192354,#192355),(#192356,#192357,#192358,#192359,#192360,#192361,
#192362,#192363,#192364),(#192365,#192366,#192367,#192368,#192369,#192370,
#192371,#192372,#192373),(#192374,#192375,#192376,#192377,#192378,#192379,
#192380,#192381,#192382),(#192383,#192384,#192385,#192386,#192387,#192388,
#192389,#192390,#192391),(#192392,#192393,#192394,#192395,#192396,#192397,
#192398,#192399,#192400),(#192401,#192402,#192403,#192404,#192405,#192406,
#192407,#192408,#192409),(#192410,#192411,#192412,#192413,#192414,#192415,
#192416,#192417,#192418),(#192419,#192420,#192421,#192422,#192423,#192424,
#192425,#192426,#192427),(#192428,#192429,#192430,#192431,#192432,#192433,
#192434,#192435,#192436),(#192437,#192438,#192439,#192440,#192441,#192442,
#192443,#192444,#192445),(#192446,#192447,#192448,#192449,#192450,#192451,
#192452,#192453,#192454),(#192455,#192456,#192457,#192458,#192459,#192460,
#192461,#192462,#192463),(#192464,#192465,#192466,#192467,#192468,#192469,
#192470,#192471,#192472),(#192473,#192474,#192475,#192476,#192477,#192478,
#192479,#192480,#192481),(#192482,#192483,#192484,#192485,#192486,#192487,
#192488,#192489,#192490),(#192491,#192492,#192493,#192494,#192495,#192496,
#192497,#192498,#192499),(#192500,#192501,#192502,#192503,#192504,#192505,
#192506,#192507,#192508),(#192509,#192510,#192511,#192512,#192513,#192514,
#192515,#192516,#192517),(#192518,#192519,#192520,#192521,#192522,#192523,
#192524,#192525,#192526),(#192527,#192528,#192529,#192530,#192531,#192532,
#192533,#192534,#192535),(#192536,#192537,#192538,#192539,#192540,#192541,
#192542,#192543,#192544),(#192545,#192546,#192547,#192548,#192549,#192550,
#192551,#192552,#192553),(#192554,#192555,#192556,#192557,#192558,#192559,
#192560,#192561,#192562),(#192563,#192564,#192565,#192566,#192567,#192568,
#192569,#192570,#192571),(#192572,#192573,#192574,#192575,#192576,#192577,
#192578,#192579,#192580),(#192581,#192582,#192583,#192584,#192585,#192586,
#192587,#192588,#192589),(#192590,#192591,#192592,#192593,#192594,#192595,
#192596,#192597,#192598),(#192599,#192600,#192601,#192602,#192603,#192604,
#192605,#192606,#192607),(#192608,#192609,#192610,#192611,#192612,#192613,
#192614,#192615,#192616),(#192617,#192618,#192619,#192620,#192621,#192622,
#192623,#192624,#192625),(#192626,#192627,#192628,#192629,#192630,#192631,
#192632,#192633,#192634),(#192635,#192636,#192637,#192638,#192639,#192640,
#192641,#192642,#192643),(#192644,#192645,#192646,#192647,#192648,#192649,
#192650,#192651,#192652),(#192653,#192654,#192655,#192656,#192657,#192658,
#192659,#192660,#192661),(#192662,#192663,#192664,#192665,#192666,#192667,
#192668,#192669,#192670),(#192671,#192672,#192673,#192674,#192675,#192676,
#192677,#192678,#192679),(#192680,#192681,#192682,#192683,#192684,#192685,
#192686,#192687,#192688),(#192689,#192690,#192691,#192692,#192693,#192694,
#192695,#192696,#192697),(#192698,#192699,#192700,#192701,#192702,#192703,
#192704,#192705,#192706),(#192707,#192708,#192709,#192710,#192711,#192712,
#192713,#192714,#192715),(#192716,#192717,#192718,#192719,#192720,#192721,
#192722,#192723,#192724),(#192725,#192726,#192727,#192728,#192729,#192730,
#192731,#192732,#192733),(#192734,#192735,#192736,#192737,#192738,#192739,
#192740,#192741,#192742),(#192743,#192744,#192745,#192746,#192747,#192748,
#192749,#192750,#192751),(#192752,#192753,#192754,#192755,#192756,#192757,
#192758,#192759,#192760),(#192761,#192762,#192763,#192764,#192765,#192766,
#192767,#192768,#192769),(#192770,#192771,#192772,#192773,#192774,#192775,
#192776,#192777,#192778),(#192779,#192780,#192781,#192782,#192783,#192784,
#192785,#192786,#192787),(#192788,#192789,#192790,#192791,#192792,#192793,
#192794,#192795,#192796),(#192797,#192798,#192799,#192800,#192801,#192802,
#192803,#192804,#192805),(#192806,#192807,#192808,#192809,#192810,#192811,
#192812,#192813,#192814),(#192815,#192816,#192817,#192818,#192819,#192820,
#192821,#192822,#192823),(#192824,#192825,#192826,#192827,#192828,#192829,
#192830,#192831,#192832),(#192833,#192834,#192835,#192836,#192837,#192838,
#192839,#192840,#192841),(#192842,#192843,#192844,#192845,#192846,#192847,
#192848,#192849,#192850),(#192851,#192852,#192853,#192854,#192855,#192856,
#192857,#192858,#192859),(#192860,#192861,#192862,#192863,#192864,#192865,
#192866,#192867,#192868),(#192869,#192870,#192871,#192872,#192873,#192874,
#192875,#192876,#192877),(#192878,#192879,#192880,#192881,#192882,#192883,
#192884,#192885,#192886),(#192887,#192888,#192889,#192890,#192891,#192892,
#192893,#192894,#192895),(#192896,#192897,#192898,#192899,#192900,#192901,
#192902,#192903,#192904),(#192905,#192906,#192907,#192908,#192909,#192910,
#192911,#192912,#192913),(#192914,#192915,#192916,#192917,#192918,#192919,
#192920,#192921,#192922),(#192923,#192924,#192925,#192926,#192927,#192928,
#192929,#192930,#192931),(#192932,#192933,#192934,#192935,#192936,#192937,
#192938,#192939,#192940),(#192941,#192942,#192943,#192944,#192945,#192946,
#192947,#192948,#192949),(#192950,#192951,#192952,#192953,#192954,#192955,
#192956,#192957,#192958),(#192959,#192960,#192961,#192962,#192963,#192964,
#192965,#192966,#192967),(#192968,#192969,#192970,#192971,#192972,#192973,
#192974,#192975,#192976),(#192977,#192978,#192979,#192980,#192981,#192982,
#192983,#192984,#192985),(#192986,#192987,#192988,#192989,#192990,#192991,
#192992,#192993,#192994),(#192995,#192996,#192997,#192998,#192999,#193000,
#193001,#193002,#193003),(#193004,#193005,#193006,#193007,#193008,#193009,
#193010,#193011,#193012),(#193013,#193014,#193015,#193016,#193017,#193018,
#193019,#193020,#193021),(#193022,#193023,#193024,#193025,#193026,#193027,
#193028,#193029,#193030),(#193031,#193032,#193033,#193034,#193035,#193036,
#193037,#193038,#193039),(#193040,#193041,#193042,#193043,#193044,#193045,
#193046,#193047,#193048),(#193049,#193050,#193051,#193052,#193053,#193054,
#193055,#193056,#193057),(#193058,#193059,#193060,#193061,#193062,#193063,
#193064,#193065,#193066),(#193067,#193068,#193069,#193070,#193071,#193072,
#193073,#193074,#193075),(#193076,#193077,#193078,#193079,#193080,#193081,
#193082,#193083,#193084),(#193085,#193086,#193087,#193088,#193089,#193090,
#193091,#193092,#193093),(#193094,#193095,#193096,#193097,#193098,#193099,
#193100,#193101,#193102),(#193103,#193104,#193105,#193106,#193107,#193108,
#193109,#193110,#193111),(#193112,#193113,#193114,#193115,#193116,#193117,
#193118,#193119,#193120),(#193121,#193122,#193123,#193124,#193125,#193126,
#193127,#193128,#193129),(#193130,#193131,#193132,#193133,#193134,#193135,
#193136,#193137,#193138),(#193139,#193140,#193141,#193142,#193143,#193144,
#193145,#193146,#193147),(#193148,#193149,#193150,#193151,#193152,#193153,
#193154,#193155,#193156),(#193157,#193158,#193159,#193160,#193161,#193162,
#193163,#193164,#193165),(#193166,#193167,#193168,#193169,#193170,#193171,
#193172,#193173,#193174),(#193175,#193176,#193177,#193178,#193179,#193180,
#193181,#193182,#193183)),.UNSPECIFIED.,.F.,.T.,.F.)
B_SPLINE_SURFACE_WITH_KNOTS((4,1,1,1,1,1,1,1,1,1,1,1,1,1,1,1,1,1,1,1,1,
1,1,1,1,1,1,1,1,1,1,1,1,1,1,1,1,1,1,1,1,1,1,1,1,1,1,1,1,1,1,1,1,1,1,1,1,
1,1,1,1,1,1,1,1,1,1,1,1,1,1,1,1,1,1,1,1,1,1,1,1,1,1,1,1,1,1,1,1,1,1,1,1,
1,1,1,1,1,1,1,1,1,1,1,1,1,1,1,1,1,1,1,1,1,1,1,1,1,1,1,1,1,1,1,1,1,1,1,1,
1,1,1,1,1,1,1,1,1,1,1,1,1,1,1,1,1,1,1,1,1,1,1,1,1,1,1,1,1,1,1,1,1,1,1,1,
1,1,1,1,1,1,1,1,1,1,1,1,1,1,1,1,1,1,1,1,1,1,1,1,1,1,1,1,1,1,1,1,1,1,1,1,
1,1,1,1,1,1,1,1,1,1,1,1,1,1,1,1,1,1,1,1,1,1,1,1,1,1,1,1,1,1,1,1,1,1,1,1,
1,1,1,1,1,1,1,1,1,1,1,1,1,1,1,1,1,1,1,1,1,1,1,1,1,1,1,1,1,1,1,1,1,1,1,1,
1,1,1,1,1,1,1,1,1,1,1,1,1,1,1,1,1,1,1,1,1,1,1,1,1,1,1,1,1,1,1,1,1,1,1,1,
1,1,1,1,1,1,1,1,1,1,1,1,1,1,1,1,1,1,1,1,1,1,1,1,1,1,1,1,1,1,1,1,1,1,1,1,
1,1,1,1,1,1,1,1,1,1,1,1,1,1,1,1,1,1,1,1,1,1,1,1,1,1,1,1,1,1,1,1,1,1,1,1,
1,1,1,1,1,1,1,1,1,1,1,1,1,1,1,1,1,1,1,1,1,1,1,1,1,1,1,1,1,1,1,1,1,1,1,1,
1,1,1,1,1,1,1,1,1,1,1,1,1,1,1,1,1,1,1,1,1,1,1,1,1,1,1,1,1,1,1,1,1,1,1,1,
1,1,1,1,1,1,1,1,1,1,1,1,1,1,1,1,1,1,1,1,1,1,1,1,1,1,1,1,1,1,1,1,1,1,1,1,
1,1,1,1,1,1,1,1,1,1,1,1,1,1,1,1,1,1,1,1,1,1,1,1,1,1,1,1,1,1,1,1,1,1,1,1,
1,1,1,1,1,1,1,1,1,1,1,1,1,1,1,1,1,1,1,1,1,1,1,1,1,1,1,1,1,1,1,1,1,1,1,1,
1,1,1,1,1,1,1,1,1,1,1,1,1,1,1,1,1,1,1,1,1,1,1,1,1,1,1,1,1,1,1,1,1,1,1,1,
1,1,1,1,1,1,1,1,1,1,1,1,1,1,1,1,1,1,1,1,1,1,1,1,1,1,1,1,1,1,1,1,1,1,1,1,
1,1,1,1,1,1,1,1,1,1,1,1,1,1,1,1,1,1,1,1,1,1,1,1,1,1,1,1,1,1,1,1,1,1,1,1,
1,1,1,1,1,1,1,1,1,1,1,1,1,1,1,1,1,1,1,1,1,1,1,1,1,1,1,1,1,1,1,1,1,1,1,1,
1,1,1,1,1,1,1,1,1,1,1,1,1,1,1,1,1,1,1,1,1,1,1,1,1,1,1,1,1,1,1,1,1,1,1,1,
1,1,1,1,1,1,1,1,1,1,1,1,1,1,1,1,1,1,1,1,1,1,1,1,1,1,1,1,1,1,1,1,1,1,1,1,
1,1,1,1,1,1,1,1,1,1,1,1,1,1,1,1,1,1,1,1,1,1,1,1,1,1,1,1,1,1,1,1,1,1,1,1,
1,1,1,1,1,1,1,1,1,1,1,1,1,1,1,1,1,1,1,1,1,1,1,1,1,1,1,1,1,1,1,1,1,1,1,1,
1,1,1,1,1,1,1,1,1,1,1,1,1,1,1,1,1,1,1,1,1,1,1,1,1,1,1,1,1,1,1,1,1,1,1,1,
1,1,1,1,1,1,1,1,1,1,1,1,1,1,1,1,1,1,1,1,1,1,1,1,1,1,1,1,1,1,1,1,1,1,1,1,
1,1,1,1,1,1,1,1,1,1,1,1,1,1,1,1,1,1,1,1,1,1,1,1,1,1,1,1,1,1,1,1,1,1,1,1,
1,1,1,1,1,1,1,1,1,1,1,1,1,1,1,1,1,1,1,1,1,1,1,1,1,1,1,1,1,1,1,1,1,1,1,1,
1,1,1,1,1,1,1,1,1,1,1,1,1,1,1,1,1,1,1,1,1,1,1,1,1,1,1,1,1,1,1,1,1,1,1,1,
1,1,1,1,1,1,1,1,1,1,1,1,1,1,1,1,1,1,1,1,1,1,1,1,1,1,1,1,1,1,1,1,1,1,1,1,
1,1,1,1,1,1,1,1,1,1,1,1,1,1,1,1,1,1,1,1,1,1,1,1,1,1,1,1,1,1,1,1,1,1,1,1,
1,1,1,1,1,1,1,1,1,1,1,1,1,1,1,1,1,1,1,1,1,1,1,1,1,1,1,1,1,1,1,1,1,1,1,1,
1,1,1,1,1,1,1,1,1,1,1,1,1,1,1,1,1,1,1,1,1,1,1,1,1,1,1,1,1,1,1,1,1,1,1,1,
1,1,1,1,1,1,1,1,1,1,1,1,1,1,1,1,1,1,1,1,1,1,1,1,1,1,1,1,1,1,1,1,1,1,1,1,
1,1,1,1,1,1,1,1,1,1,1,1,1,1,1,1,1,1,1,1,1,1,1,1,1,1,1,1,1,1,1,1,1,1,1,1,
1,1,1,1,1,1,1,1,1,1,1,1,1,1,1,1,1,1,1,1,1,1,1,1,1,1,1,1,1,1,1,1,1,1,1,1,
1,1,1,1,1,1,1,1,1,1,1,1,1,1,1,1,1,1,1,1,1,1,1,1,1,1,1,1,1,1,1,1,1,1,1,1,
1,1,1,1,1,1,1,1,1,1,1,1,1,1,1,1,1,1,1,1,1,1,1,1,1,1,1,1,1,1,1,1,1,1,1,1,
1,1,1,1,1,1,1,1,1,1,1,1,1,1,1,1,1,1,1,1,1,1,1,1,1,1,1,1,1,1,1,1,1,1,1,1,
1,1,1,1,1,1,1,1,1,1,1,1,1,1,1,1,1,1,1,1,1,1,1,1,1,1,1,1,1,1,1,1,1,1,1,1,
1,1,1,1,1,1,1,1,1,1,1,1,1,1,1,1,1,1,1,1,1,1,1,1,1,1,1,1,1,1,1,1,1,1,1,1,
1,1,1,1,1,1,1,1,1,1,1,1,1,1,1,1,1,1,1,1,1,1,1,1,1,1,1,1,1,1,1,1,1,1,1,1,
1,1,1,1,1,1,1,1,1,1,1,1,1,1,1,1,1,1,1,1,1,1,1,1,1,1,1,1,1,1,1,1,1,1,1,1,
1,1,1,1,1,1,1,1,1,1,1,1,1,1,1,1,1,1,1,1,1,1,1,1,1,1,1,1,1,1,1,1,1,1,1,1,
1,1,1,1,1,1,1,1,1,1,1,1,1,1,1,1,1,1,1,1,1,1,1,1,1,1,1,1,1,1,1,1,1,1,1,1,
1,1,1,1,1,1,1,1,1,1,1,1,1,1,1,1,1,1,1,1,1,1,1,1,1,1,1,1,1,1,1,1,1,1,1,1,
1,1,1,1,1,1,1,1,1,1,1,1,1,1,1,1,1,1,1,1,1,1,1,1,1,1,1,1,1,1,1,1,1,1,1,1,
1,1,1,1,1,1,1,1,1,1,1,1,1,1,1,1,1,1,1,1,1,1,1,1,1,1,1,1,1,1,1,1,1,1,1,1,
1,1,1,1,1,1,1,1,1,1,1,1,1,1,1,1,1,1,1,1,1,1,1,1,1,1,1,1,1,1,1,1,1,1,1,1,
1,1,1,1,1,1,1,1,1,1,1,1,1,1,1,1,1,1,1,1,1,1,1,1,1,1,1,1,1,1,1,1,1,1,1,1,
1,1,1,1,1,1,1,1,1,1,1,1,1,1,1,1,1,1,1,1,1,1,1,1,1,1,1,1,1,1,1,1,1,1,1,1,
1,1,1,1,1,1,1,1,1,1,1,1,1,1,1,1,1,1,1,1,1,1,1,1,1,1,1,1,1,1,1,1,1,1,1,1,
1,1,1,1,1,1,1,1,1,1,1,1,1,1,1,1,1,1,1,1,1,1,1,1,1,1,1,1,1,1,1,1,1,1,1,1,
1,1,1,1,1,1,1,1,1,1,1,1,1,1,1,1,1,1,1,1,1,1,1,1,1,1,1,1,1,1,1,1,1,1,1,1,
1,1,1,1,1,1,1,1,1,1,1,1,1,1,1,1,1,1,1,1,1,1,1,1,1,1,1,1,1,1,1,1,1,1,1,1,
1,1,1,1,1,1,1,1,1,1,1,1,1,1,1,1,1,1,1,1,1,1,1,1,1,1,1,1,1,1,1,1,1,1,1,1,
1,1,1,1,1,1,1,1,1,1,1,1,1,1,1,1,1,1,1,1,1,1,1,1,1,1,1,1,1,1,1,1,1,1,1,1,
1,1,1,1,1,1,1,1,1,1,1,4),(3,2,2,2,3),(0.,0.01797683372391,0.286633051710584,
0.555289278308216,0.823945516665782,1.09260176953922,1.36125803873948,1.62991432588463,
1.89857063164012,2.16722695661301,2.43588330050525,2.70453966304674,2.9731960431531,
3.24185243981471,3.51050885133453,3.77916527610465,4.04782171198515,4.31647815691489,
4.58513460847725,4.85379106430677,5.12244752187208,5.39110397865606,5.65976043217153,
5.92841687990537,6.19707331956994,6.46572974881596,6.73438616570634,7.00304256821933,
7.2716989549161,7.5403553242696,7.809011675483,8.07766800769526,8.34632432089157,
8.61498061505147,8.8836368910788,9.15229314997201,9.4209493936865,9.68960562442157,
9.95826184531348,10.226918059948,10.4955742727586,10.7642304884925,11.0328867113173,
11.3015429448574,11.5701991918227,11.8388554546081,12.1075117346518,12.3761680332469,
12.6448243507434,12.9134806874637,13.1821370428496,13.450793416388,13.7194498067883,
13.9881062128412,14.2567626326955,14.5254190645885,14.7940755062772,15.0627319555912,
15.3313884100611,15.6000448672586,15.8687013246492,16.1373577797,16.4060142299691,
16.6746706729765,16.9433271065265,17.2119835283531,17.4806399366567,17.7492963295502,
18.0179527057767,18.286609063996,18.555265403637,18.8239217240786,19.0925780255742,
19.3612343083975,19.6298905737625,19.898546823017,20.1672030584666,20.4358592827168,
20.7045154992928,20.973171712245,21.2418279262962,21.5104841459723,21.7791403749736,
22.0477966165324,22.316452872948,22.585109146262,22.8537654375589,23.1224217478187,
23.3910780770929,23.6597344254327,23.9283907920352,24.197047176159,24.4657035763222,
24.7343599911301,25.0030164185931,25.2716728568073,25.5403293034427,25.8089857562333,
26.0776422126729,26.3462986702843,26.6149551265448,26.8836115789212,27.1522680250308,
27.4209244624423,27.6895808890659,27.9582373027346,28.2268937018004,28.4955500845261,
28.7642064498512,29.0328627966379,29.3015191245544,29.5701754332357,29.838831723217,
30.1074879950829,30.3761442503694,30.6448004907916,30.9134567190168,31.1821129380756,
31.450769151893,31.7194253649682,31.9880815819663,32.2567378070174,32.5253940433706,
32.7940502938785,33.0627065604467,33.3313628447765,33.6000191476151,33.8686754696427,
34.1373318106287,34.405988170366,34.6746445478242,34.9433009420458,35.2119573513747,
35.480613774244,35.7492702085419,36.0179266522368,36.2865831029275,36.5552395582669,
36.8238960157264,37.0925524727952,37.3612089269773,37.6298653757534,37.8985218168153,
38.1671782477952,38.4358346667239,38.7044910715485,38.9731474607866,39.2418038328672,
39.5104601869391,39.7791165220837,40.0477728382212,40.3164291352602,40.5850854140292,
40.8537416754418,41.1223979213679,41.3910541539077,41.6597103761025,41.9283665914244,
42.1970228042084,42.4656790192,42.7343352406829,43.0029914723808,43.2716477171096,
43.540303977354,43.8089602546436,44.0776165503516,44.3462728649052,44.614929198697,
44.883585551232,45.1522419220568,45.4208983099307,45.6895547136931,45.9582111315299,
46.2268675617156,46.4955240020317,46.7641804503338,47.0328369041642,47.3014933611089,
47.5701498186329,47.8388062742058,48.107462725373,48.3761191696448,48.6447756048012,
48.9134320285537,49.1820884390673,49.4507448344197,49.7194012133072,49.9880575743413,
50.2567139168934,50.5253702402807,50.7940265446884,51.0626828303152,51.3313390982961,
51.5999953498901,51.8686515873141,52.1373078130706,52.4059640305862,52.6746202437936,
52.9432764573682,53.211932675918,53.480588903259,53.7492451427202,54.0179013967021,
54.2865576673334,54.5552139557853,54.823870263115,55.0925265894471,55.3611829348992,
55.6298392987282,55.8984956802486,56.1671520780245,56.4358084907065,56.7044649163381,
56.9731213530494,57.2417777985307,57.5104342505384,57.7790907065743,58.0477471641719,
58.3164036208043,58.5850600739368,58.8537165211707,59.1223729600609,59.39102938849,
59.6596858042645,59.9283422056975,60.1969985910129,60.4656549590995,60.7343113087676,
61.0029676396243,61.2716239512389,61.540280244075,61.808936518638,62.0775927763821,
62.3462490189291,62.6149052488546,62.8835614690812,63.1522176834332,63.4208738963055,
63.6895301124163,63.9581863359981,64.2268425704115,64.4954988186027,64.7641550825741,
65.0328113641112,65.3014676640435,65.5701239831253,65.8387803211949,66.1074366781083,
66.3760930528907,66.6447494446373,66.9134058517341,67.1820622726558,67.4507187053199,
67.7193751477252,67.988031597487,68.256688052277,68.5253445095709,68.7940009668648,
69.0626574216546,69.3313138714164,69.5999703138218,69.8686267464858,70.1372831674076,
70.4059395745042,70.6745959662509,70.9432523410334,71.2119086979469,71.4805650360164,
71.7492213550982,72.0178776550306,72.2865339365675,72.5551902005389,72.8238464487301,
73.0925026831433,73.3611589067251,73.6298151228357,73.8984713357081,74.1671275500599,
74.4357837702864,74.7044400002118,74.9730962427587,75.2417525005027,75.5104087750655,
75.7790650679015,76.047721379516,76.3163777103726,76.5850340600405,76.853690428127,
77.1223468134422,77.391003214875,77.6596596306495,77.9283160590784,78.1969724979684,
78.4656289452021,78.7342853983344,79.0029418549666,79.2715983125641,79.5402547685998,
79.8089112206075,80.0775676660886,80.3462241027997,80.6148805284312,80.8835369411131,
81.1521933388889,81.4208497204091,81.689506084238,81.9581624296899,82.2268187560219,
82.4954750633515,82.7641313518033,83.0327876224345,83.3014438764161,83.5701001158772,
83.838756343218,84.1074125617677,84.3760687753422,84.6447249885494,84.913381206065,
85.1820374318212,85.4506936692451,85.719349920839,85.9880061888197,86.2566624744465,
86.5253187788541,86.7939751022413,87.0626314447932,87.3312878058273,87.5999441847146,
87.8686005800667,88.1372569905802,88.4059134143327,88.6745698494889,88.9432262937606,
89.2118827449277,89.4805392005005,89.7491956580243,90.0178521149689,90.2865085687992,
90.5551650171012,90.8238214574172,91.0924778876028,91.3611343054394,91.6297907092016,
91.8984470970753,92.1671034679,92.4357598204347,92.7044161542264,92.9730724687798,
93.2417287644878,93.5103850417773,93.7790413020216,94.0476975467502,94.3163537784479,
94.5850099999307,94.8536662149221,95.1223224277061,95.390978643028,95.6596348652226,
95.9282910977624,96.1969473436883,96.4656036051009,96.7342598838697,97.0029161809086,
97.2715724970461,97.5402288321905,97.8088851862623,98.0775415583427,98.3461979475807,
98.6148543524051,98.8835107713336,99.1521672023136,99.4208236433754,99.6894800921513,
99.9581365463333,100.226793003402,100.495449460861,100.7641059162,101.032762366891,
101.301418810586,101.570075244884,101.838731667753,102.107388077082,102.376044471303,
102.644700848761,102.913357208498,103.182013549484,103.450669871511,103.71932617435,
103.98798245868,104.256638725248,104.525294975755,104.793951212108,105.062607437159,
105.331263654157,105.599919867233,105.86857608105,106.137232300108,106.405888528334,
106.674544768756,106.943201024042,107.211857295908,107.480513585889,107.74916989457,
108.017826222487,108.286482569273,108.555138934598,108.823795317324,109.09245171639,
109.361108130058,109.629764556682,109.898420994093,110.167077440202,110.435733892579,
110.704390348839,110.97304680645,111.24170326289,111.51035971568,111.779016162316,
112.04767260053,112.316329027993,112.5849854428,112.853641842963,113.122298227087,
113.39095459369,113.659610942029,113.928267271303,114.196923581563,114.46557987286,
114.734236146174,115.002892402589,115.271548644148,115.540204873149,115.808861092825,
116.077517306876,116.346173519828,116.614829736404,116.883485960654,117.152142196103,
117.420798445358,117.689454710722,117.958110993546,118.226767295041,118.495423615483,
118.764079955123,119.032736313343,119.301392689569,119.570049082462,119.838705490766,
120.107361912592,120.376018346142,120.644674789149,120.913331239418,121.181987694469,
121.45064415186,121.719300609057,121.987957063527,122.256613512841,122.525269954529,
122.793926386422,123.062582806276,123.331239212329,123.599895602729,123.868551976268,
124.137208331653,124.405864668374,124.67452098587,124.943177284465,125.211833564508,
125.480489827294,125.749146074259,126.017802307799,126.286458530624,126.555114746357,
126.823770959168,127.092427173802,127.361083394694,127.629739625429,127.898395869143,
128.167052128037,128.435708404064,128.704364698224,128.97302101142,129.241677343633,
129.510333694846,129.7789900642,130.047646450897,130.31630285341,130.5849592703,
130.853615699547,131.122272139211,131.390928586945,131.659585040461,131.928241497245,
132.19689795481,132.46555441064,132.734210862202,133.002867307132,133.271523743013,
133.540180167783,133.808836579303,134.077492975965,134.346149356071,134.614805718613,
134.883462062505,135.152118387478,135.420774693234,135.689430980379,135.958087249579,
136.226743502453,136.49539974081,136.76405596741,137.032712185392,137.301368398783,
137.570024612174,137.838680830155,138.107337056755,138.375993295112,138.644649547986,
138.913305817186,139.181962104332,139.450618410087,139.71927473506,139.987931078952,
140.256587441494,140.525243821601,140.793900218262,141.062556629782,141.331213054552,
141.599869490433,141.868525935363,142.137182386925,142.405838842755,142.67449530032,
142.943151757104,143.21180821062,143.480464658354,143.749121098019,144.017777527265,
144.286433944155,144.555090346668,144.823746733365,145.092403102719,145.361059453932,
145.629715786145,145.898372099341,146.167028393501,146.435684669529,146.704340928422,
146.972997172137,147.241653402872,147.510309623764,147.778965838398,148.047622051209,
148.316278266943,148.584934489768,148.853590723308,149.122246970274,149.390903233059,
149.659559513103,149.928215811698,150.196872129195,150.465528465915,150.734184821301,
151.00284119484,151.27149758524,151.540153991293,151.808810411148,152.077466843041,
152.34612328473,152.614779734044,152.883436188514,153.152092645711,153.420749103102,
153.689405558153,153.958062008422,154.22671845143,154.49537488498,154.764031306806,
155.03268771511,155.301344108004,155.57000048423,155.838656842449,156.107313182091,
156.375969502532,156.644625804028,156.913282086851,157.181938352216,157.450594601471,
157.719250836921,157.987907061171,158.256563277747,158.525219490699,158.793875704751,
159.062531924427,159.331188153428,159.599844394987,159.868500651403,160.137156924717,
160.405813216014,160.674469526274,160.943125855548,161.211782203888,161.480438570491,
161.749094954615,162.017751354778,162.286407769586,162.555064197049,162.823720635263,
163.092377081899,163.361033534689,163.629689991129,163.898346448741,164.167002905001,
164.435659357378,164.704315803488,164.972972240899,165.241628667523,165.510285081192,
165.778941480257,166.047597862983,166.316254228308,166.584910575095,166.853566903012,
167.122223211693,167.390879501675,167.659535773541,167.928192028827,168.19684826925,
168.465504497475,168.734160716534,169.002816930351,169.271473143427,169.540129360425,
169.808785585476,170.077441821829,170.346098072337,170.614754338905,170.883410623235,
171.152066926074,171.420723248102,171.689379589088,171.958035948825,172.226692326284,
172.495348720505,172.764005129834,173.032661552704,173.301317987002,173.569974430697,
173.838630881388,174.107287336727,174.375943794187,174.644600251255,174.913256705437,
175.181913154214,175.450569595276,175.719226026256,175.987882445184,176.256538850009,
176.525195239247,176.793851611328,177.0625079654,177.331164300545,177.599820616682,
177.868476913721,178.137133192491,178.405789453903,178.674445699829,178.943101932369,
179.211758154564,179.480414369886,179.74907058267,180.017726797662,180.286383019145,
180.555039250843,180.823695495572,181.092351755816,181.361008033106,181.629664328814,
181.898320643368,182.16697697716,182.435633329695,182.70428970052,182.972946088394,
183.241602492156,183.510258909993,183.778915340179,184.047571780495,184.316228228797,
184.584884682628,184.853541139572,185.122197597096,185.39085405267,185.659510503837,
185.928166948109,186.196823383265,186.465479807018,186.734136217531,187.002792612884,
187.271448991771,187.540105352806,187.808761695358,188.077418018745,188.346074323153,
188.61473060878,188.883386876761,189.152043128355,189.420699365779,189.689355591536,
189.958011809051,190.226668022259,190.495324235834,190.763980454383,191.032636681725,
191.301292921186,191.569949175168,191.838605445799,192.107261734251,192.375918041581,
192.644574367913,192.913230713365,193.181887077194,193.450543458715,193.719199856491,
193.987856269173,194.256512694805,194.525169131516,194.793825576997,195.062482029005,
195.331138485041,195.599794942639,195.868451399271,196.137107852404,196.405764299638,
196.674420738528,196.943077166957,197.211733582732,197.480389984165,197.749046369481,
198.017702737567,198.286359087236,198.555015418092,198.823671729707,199.092328022543,
199.360984297106,199.62964055485,199.898296797397,200.166953027323,200.43560924755,
200.704265461902,200.972921674774,201.241577890885,201.510234114467,201.77889034888,
202.047546597072,202.316202861043,202.584859142581,202.853515442513,203.122171761595,
203.390828099665,203.659484456579,203.928140831361,204.196797223108,204.465453630205,
204.734110051127,205.002766483791,205.271422926197,205.540079375959,205.808735830749,
206.077392288043,206.346048745337,206.614705200127,206.883361649889,207.152018092295,
207.420674524959,207.689330945881,207.957987352978,208.226643744725,208.495300119508,
208.763956476421,209.032612814491,209.301269133573,209.569925433505,209.838581715043,
210.107237979014,210.375894227206,210.644550461619,210.913206685201,211.181862901312,
211.450519114184,211.719175328536,211.987831548763,212.256487778689,212.525144021236,
212.79380027898,213.062456553543,213.331112846379,213.599769157994,213.868425488851,
214.137081838519,214.405738206606,214.674394591921,214.943050993354,215.211707409129,
215.480363837558,215.749020276448,216.017676723682,216.286333176815,216.554989633447,
216.823646091045,217.092302547081,217.360958999089,217.62961544457,217.898271881281,
218.166928306913,218.435584719595,218.704241117371,218.972897498892,219.241553862721,
219.510210208173,219.778866534505,220.047522841835,220.316179130287,220.584835400918,
220.8534916549,221.122147894361,221.390804121702,221.659460340252,221.928116553827,
222.196772767034,222.46542898455,222.734085210306,223.00274144773,223.271397699324,
223.540053967305,223.808710252932,224.07736655734,224.346022880728,224.61467922328,
224.883335584314,225.151991963201,225.420648358554,225.689304769068,225.95796119282,
226.226617627977,226.495274072249,226.763930523416,227.032586978989,227.301243436513,
227.569899893458,227.838556347288,228.10721279559,228.375869235907,228.644525666093,
228.913182083929,229.181838487692,229.450494875566,229.719151246391,229.987807598926,
230.256463932718,230.525120247271,230.79377654298,231.062432820269,231.331089080514,
231.599745325243,231.868401556941,232.137057778424,232.405713993415,232.674370206199,
232.943026421521,233.211682643716,233.480338876256,233.748995122182,234.017651383595,
234.286307662364,234.554963959403,234.823620275541,235.092276610685,235.360932964757,
235.629589336838,235.898245726076,236.166902130901,236.43555854983,236.70421498081,
236.972871421872,237.241527870648,237.51018432483,237.778840781899,238.047497239359,
238.316153694698,238.584810145389,238.853466589084,239.122123023382,239.390779446251,
239.65943585558,239.928092249802,240.19674862726,240.465404986998,240.734061327984,
241.002717650011,241.27137395285,241.54003023718,241.808686503748,242.077342754256,
242.345998990609,242.614655215661,242.883311432659,243.151967645734,243.420623859552,
243.68928007861,243.957936306836,244.226592547258,244.495248802545,244.763905074411,
245.032561364392,245.301217673074,245.56987400099,245.838530347777,246.107186713102,
246.375843095828,246.644499494894,246.913155908563,247.181812335186,247.450468772598,
247.719125218708,247.987781671084,248.256438127345,248.525094584956,248.793751041396,
249.062407494187,249.331063940822,249.599720379036,249.8683768065,250.137033221308,
250.405689621471,250.674346005595,250.943002372197,251.211658720537,251.480315049812,
251.748971360071,252.017627651368,252.286283924683,252.554940181098,252.823596422657,
253.092252651658,253.360908871335,253.629565085386,253.898221298338,254.166877514914,
254.435533739165,254.704189974614,254.972846223869,255.241502489234,255.510158772057,
255.778815073553,256.047471393995,256.316127733635,256.584784091854,256.85344046808,
257.122096860973,257.390753269276,257.659409691102,257.928066124652,258.196722567659,
258.465379017928,258.734035472978,259.002691930368,259.271348387566,259.540004842035,
259.808661291349,260.077317733037,260.345974164929,260.614630584783,260.883286990836,
261.151943381235,261.420599754774,261.689256110159,261.957912446879,262.226568764375,
262.49522506297,262.763881343014,263.032537605798,263.301193852763,263.569850086303,
263.838506309127,264.107162524861,264.375818737671,264.644474952305,264.913131173196,
265.181787403931,265.450443647645,265.719099906538,265.987756182565,266.256412476724,
266.52506878992,266.793725122132,267.062381473345,267.331037842698,267.599694229394,
267.868350631907,268.137007048797,268.405663478042,268.674319917706,268.94297636544,
269.211632818955,269.480289275739,269.748945733304,270.017602189133,270.286258640695,
270.554915085624,270.823571521504,271.092227946274,271.360884357793,271.629540754454,
271.89819713456,272.166853497101,272.435509840993,272.704166165965,272.97282247172,
273.241478758865,273.510135028065,273.778791280938,274.047447519295,274.316103745894,
274.584759963875,274.853416177266,275.122072390656,275.390728608637,275.659384835237,
275.928041073593,276.196697326466,276.465353595666,276.734009882811,277.002666188566,
277.271322513539,277.53997885743,277.808635219972,278.077291600077,278.345947996739,
278.614604408258,278.883260833028,279.151917268908,279.420573713837,279.689230165399,
279.957886621228,280.226543078793,280.495199535576,280.763855989092,281.032512436825,
281.301168876489,281.569825305735,281.838481722625,282.107138125138,282.375794511834,
282.644450881187,282.9131072324,283.181763564612,283.450419877808,283.719076171967,
283.987732447994,284.256388706887,284.525044950601,284.793701181336,285.062357402228,
285.331013616862,285.599669829672,285.868326045405,286.136982268229,286.405638501769,
286.674294748734,286.942951011519,287.211607291562,287.480263590157,287.748919907653,
288.017576244373,288.286232599758,288.554888973296,288.823545363696,289.092201769749,
289.360858189603,289.629514621495,289.898171063183,290.166827512497,290.435483966966,
290.704140424163,290.972796881554,291.241453336604,291.510109786873,291.77876622988,
292.047422663429,292.316079085255,292.584735493559,292.853391886452,293.122048262678,
293.390704620897,293.659360960537,293.928017280978,294.196673582474,294.465329865297,
294.733986130661,295.002642379915,295.271298615364,295.539954839614,295.808611056189,
296.077267269141,296.345923483192,296.614579702867,296.883235931868,297.151892173427,
297.420548429842,297.689204703155,297.957860994452,298.226517304711,298.495173633985,
298.763829982324,299.032486348927,299.30114273305,299.569799133212,299.83845554802,
300.107111975482,300.375768413696,300.644424860331,300.913081313121,301.181737769561,
301.450394227172,301.719050683432,301.987707135808,302.256363581917,302.525020019328,
302.793676445951,303.062332859619,303.330989258684,303.59964564141,303.868302006734,
304.136958353521,304.405614681437,304.674270990118,304.942927280098,305.211583551964,
305.48023980725,305.748896047671,306.017552275896,306.286208494954,306.554864708772,
306.823520921846,307.092177138844,307.360833363895,307.629489600247,307.898145850755,
308.166802117323,308.435458401652,308.70411470449,308.972771026517,309.241427367503,
309.51008372724,309.778740104698,310.047396498919,310.316052908247,310.584709331116,
310.853365765414,311.122022209108,311.390678659798,311.659335115137,311.927991572596,
312.196648029665,312.465304483846,312.733960932622,313.002617373684,313.271273804663,
313.539930223591,313.808586628416,314.077243017653,314.345899389733,314.614555743805,
314.883212078949,315.151868395086,315.420524692125,315.689180970894,315.957837232306,
316.226493478231,316.495149710771,316.763805932965,317.032462148286,317.30111836107,
317.569774576061,317.838430797543,318.107087029241,318.375743273969,318.644399534213,
318.913055811502,319.18171210721,319.450368421763,319.719024755555,319.987681108089,
320.256337478914,320.524993866787,320.793650270549,321.062306688385,321.33096311857,
321.599619558886,321.868276007188,322.136932461018,322.405588917962,322.674245375486,
322.942901831059,323.211558282225,323.480214726497,323.748871161653,324.017527585405,
324.286183995918,324.55484039127,324.823496770157,325.09215313119,325.360809473742,
325.629465797129,325.898122101536,326.166778387163,326.435434655143,326.704090906737,
326.97274714416,327.241403369916,327.510059587432,327.778715800638,328.047372014213,
328.316028232762,328.584684460102,328.853340699563,329.121996953545,329.390653224175,
329.659309512627,329.927965819956,330.196622146288,330.46527849174,330.733934855568,
331.002591237088,331.271247634863,331.539904047545,331.808560473176,332.077216909887,
332.345873355368,332.614529807375,332.883186263411,333.151842721008,333.42049917764,
333.689155630772,333.957812078005,334.226468516895,334.495124945324,334.763781361098,
335.03243776253,335.301094147845,335.569750515931,335.838406865599,336.107063196455,
336.375719508069,336.644375800905,336.913032075468,337.181688333211,337.450344575758,
337.719000805683,337.987657025909,338.256313240261,338.524969453133,338.793625669243,
339.062281892824,339.330938127237,339.599594375428,339.868250639399,340.136906920936,
340.405563220868,340.674219539949,340.942875878019,341.211532234932,341.480188609714,
341.74884500146,342.017501408557,342.286157829478,342.554814262142,342.823470704547,
343.092127154308,343.360783609098,343.629440066391,343.898096523685,344.166752978475,
344.435409428236,344.704065870641,344.972722303305,345.241378724226,345.510035131323,
345.778691523069,346.047347897851,346.316004254764,346.584660592834,346.853316911915,
347.121973211847,347.390629493384,347.659285757355,347.927942005546,348.196598239959,
348.46525446354,348.733910679651,349.002566892523,349.271223106874,349.5398793271,
349.808535557025,350.077191799572,350.345848057315,350.614504331878,350.883160624714,
351.151816936328,351.420473267184,351.689129616852,351.957785984938,352.226442370253,
352.495098771685,352.76375518746,353.032411615888,353.301068054778,353.569724502012,
353.838380955144,354.107037411776,354.375693869373,354.644350325408,354.913006777416,
355.181663222896,355.450319659607,355.718976085238,355.98763249792,356.256288895695,
356.524945277215,356.793601641044,357.062257986496,357.330914312827,357.599570620156,
357.868226908608,358.136883179239,358.40553943322,358.674195672681,358.942851900021,
359.211508118571,359.480164332145,359.748820545352,360.017476762867,360.286132988623,
360.554789226047,360.82344547764,361.09210174562,361.360758031247,361.629414335654,
361.898070659041,362.166727001593,362.435383362626,362.704039741513,362.972696136865,
363.241352547378,363.510008971131,363.778665406287,364.047321850558,364.315978301725,
364.584634757297,364.853291214821,365.121947671765,365.390604125595,365.659260573897,
365.927917014213,366.196573444398,366.465229862234,366.733886265996,367.002542653869,
367.271199024694,367.539855377228,367.808511711019,368.077168025573,368.34582432128,
368.614480598569,368.883136858813,369.151793103542,369.420449335239,369.689105556722,
369.957761771713,370.226417984496,370.495074199818,370.763730422012,371.032386654551,
371.301042900477,371.569699161889,371.838355440658,372.107011737697,372.375668053834,
372.644324388978,372.912980743049,373.18163711513,373.450293504367,373.718949909191,
373.98760632812,374.256262759099,374.524919200161,374.793575648936,375.062232103118,
375.330888560186,375.599545017646,375.868201472985,376.136857923675,376.40551436737,
376.674170801667,376.942827224536,377.211483633864,377.480140028085,377.748796405543,
378.01745276528,378.286109106266,378.554765428293,378.823421731131,379.092078015461,
379.360734282028,379.629390532536,379.898046768888,380.166702993939,380.435359210937,
380.704015424011,380.972671637828,381.241327856887,381.509984085112,381.778640325533,
382.047296580819,382.315952852685,382.584609142666,382.853265451347,383.121921779263,
383.390578126049,383.659234491374,383.927890874099,384.196547273165,384.465203686833,
384.733860113456,385.002516550867,385.271172996977,385.539829449352,385.808485905613,
386.077142363224,386.345798819663,386.614455272453,386.883111719088,387.151768157302,
387.420424584764,387.689080999572,387.957737399735,388.226393783858,388.49505015046,
388.7637064988,389.032362828074,389.301019138333,389.56967542963,389.838331702943,
390.106987959358,390.375644200917,390.644300429918,390.912956649593,391.181612863644,
391.450269076596,391.718925293171,391.987581517421,392.25623775287,392.524894002124,
392.793550267489,393.062206550312,393.330862851807,393.599519172248,393.868175511888,
394.136831870107,394.405488246334,394.674144639227,394.94280104753,395.211457469356,
395.480113902905,395.748770345913,396.017426796181,396.286083251232,396.554739708622,
396.823396165819,397.092052620289,397.360709069602,397.629365511291,397.898021943183,
398.166678363037,398.43533476909,398.703991159489,398.972647533028,399.241303888413,
399.509960225133,399.778616542629,400.047272841224,400.315929121267,400.584585384052,
400.853241631017,401.121897864557,401.390554087381,401.659210303115,401.927866515925,
402.196522730559,402.465178951451,402.733835182185,403.002491425899,403.271147684792,
403.539803960819,403.808460254978,404.077116568174,404.345772900386,404.614429251599,
404.883085620952,405.151742007649,405.420398410161,405.689054827051,405.957711256297,
406.226367695961,406.495024143695,406.76368059721,407.032337053993,407.300993511558,
407.569649967387,407.838306418949,408.106962863879,408.375619299759,408.644275724528,
408.912932136048,409.181588532709,409.450244912815,409.718901275356,409.987557619248,
410.25621394422,410.524870249975,410.79352653712,411.06218280632,411.330839059193,
411.599495297549,411.868151524149,412.13680774213,412.40546395552,412.674120168911,
412.942776386892,413.211432613491,413.480088851848,413.748745104721,414.017401373921,
414.286057661065,414.55471396682,414.823370291793,415.092026635685,415.360682998226,
415.629339378332,415.897995774993,416.166652186512,416.435308611282,416.703965047162,
416.972621492092,417.241277943654,417.509934399483,417.778590857048,418.047247313831,
418.315903767346,418.58456021508,418.853216654744,419.121873083989,419.390529500879,
419.659185903392,419.927842290088,420.196498659441,420.465155010654,420.733811342866,
421.002467656062,421.271123950222,421.539780226249,421.808436485141,422.077092728855,
422.34574895959,422.614405180482,422.883061395116,423.151717607926,423.42037382366,
423.689030046484,423.957686280024,424.226342526988,424.494998789773,424.763655069817,
425.032311368411,425.300967685907,425.569624022627,425.838280378013,426.106936751551,
426.375593141951,426.644249548003,426.912905967857,427.18156239975,427.450218841438,
427.718875290752,427.987531745221,428.256188202418,428.524844659809,428.793501114859,
429.062157565128,429.330814008135,429.599470441684,429.868126863511,430.136783271814,
430.405439664707,430.674096040933,430.942752399152,431.211408738792,431.480065059233,
431.748721360729,432.017377643552,432.286033908916,432.554690158171,432.823346393619,
433.092002617869,433.360658834445,433.629315047397,433.897971261447,434.166627481123,
434.435283710124,434.703939951682,434.972596208097,435.241252481411,435.509908772707,
435.778565082967,436.047221412241,436.31587776058,436.584534127182,436.853190511305,
437.121846911468,437.390503326275,437.659159753738,437.927816191952,438.196472638587,
438.465129091377,438.733785547816,439.002442005427,439.271098461688,439.539754914064,
439.808411360173,440.077067797584,440.345724224207,440.614380637875,440.883037036941,
441.151693419666,441.420349784991,441.689006131777,441.957662459693,442.226318768374,
442.494975058355,442.763631330221,443.032287585506,443.300943825928,443.569600054153,
443.838256273211,444.106912487028,444.375568700103,444.644224917101,444.912881142151,
445.181537378504,445.450193629011,445.718849895579,445.987506179909,446.256162482747,
446.524818804774,446.79347514576,447.062131505496,447.330787882954,447.599444277176,
447.868100686504,448.136757109373,448.40541354367,448.674069987365,448.942726438055,
449.211382893394,449.480039350853,449.748695807921,450.017352262103,450.286008710879,
450.55466515194,450.82332158292,451.091978001848,451.360634406672,451.62929079591,
451.89794716799,452.166603522061,452.435259857205,452.703916173343,452.972572470381,
453.24122874915,453.509885010562,453.778541256488,454.047197489028,454.315853711222,
454.584509926543,454.853166139327,455.121822354318,455.3904785758,455.659134807498,
455.927791052226,456.19644731247,456.465103589759,456.733759885467,457.00241620002,
457.271072533811,457.539728886346,457.80838525717,458.077041645044,458.345698048806,
458.614354466642,458.883010896827,459.151667337143,459.420323785445,459.688980239275,
459.957636696219,460.226293153743,460.494949609316,460.763606060482,461.032262504754,
461.300918939909,461.569575363662,461.838231774175,462.106888169527,462.375544548414,
462.644200909447,462.912857251999,463.181513575386,463.450169879794,463.71882616542,
463.987482433401,464.256138684994,464.524794922418,464.793451148174,465.062107365689,
465.330763578896,465.59941979247,465.86807601102,466.13673223836,466.405388477821,
466.674044731802,466.942701002433,467.211357290885,467.480013598214,467.748669924546,
468.017326269997,468.285982633826,468.554639015346,468.823295413121,469.091951825803,
469.360608251434,469.629264688145,469.897921133626,470.166577585633,470.435234041669,
470.703890499266,470.972546955898,471.24120340903,471.509859856263,471.778516295153,
472.047172723582,472.315829139356,472.584485540789,472.853141926103,473.12179829419,
473.390454643857,473.659110974714,473.927767286328,474.196423579164,474.465079853726,
474.73373611147,475.002392354016,475.271048583941,475.539704804167,475.808361018519,
476.077017231391,476.345673447501,476.614329671083,476.882985905496,477.151642153686,
477.420298417658,477.688954699194,477.957610999126,478.226267318208,478.494923656277,
478.76358001319,479.032236387973,479.300892779719,479.569549186815,479.838205607737,
480.106862040401,480.375518482806,480.644174932567,480.912831387357,481.18148784465,
481.450144301944,481.718800756733,481.987457206495,482.2561136489,482.524770081563,
482.793426502485,483.062082909582,483.330739301328,483.59939567611,483.868052033023,
484.136708371092,484.405364690174,484.674020990106,484.942677271643,485.211333535614,
485.479989783805,485.748646018218,486.017302241799,486.28595845791,486.554614670781,
486.823270885133,487.091927105359,487.360583335284,487.629239577831,487.897895835574,
488.166552110137,488.435208402973,488.703864714587,488.972521045443,489.241177395111,
489.509833763197,489.778490148512,490.047146549945,490.315802965719,490.584459394147,
490.853115833037,491.12177228027,491.390428733402,491.659085190034,491.927741647632,
492.196398103667,492.465054555674,492.733711001155,493.002367437866,493.271023863497,
493.539680276179,493.808336673954,494.076993055474,494.345649419303,494.614305764754,
494.882962091086,495.151618398416,495.420274686867,495.688930957498,495.95758721148,
496.22624345094,496.494899678281,496.76355589683,497.032212110404,497.300868323611,
497.569524541126,497.838180766882,498.106837004306,498.3754932559,498.64414952388,
498.912805809507,499.181462113914,499.450118437301,499.718774779852,499.987431140886,
500.256087519773,500.524743915125,500.793400325638,501.06205674939,501.330713184546,
501.599369628818,501.868026079984,502.136682535557,502.40533899308,502.673995450025,
502.942651903855,503.211308352156,503.479964792472,503.748621222657,504.017277640494,
504.285934044256,504.554590432129,504.823246802954,505.091903155488,505.360559489279,
505.629215803832,505.89787209954,506.166528376829,506.435184637073,506.703840881801,
506.972497113499,507.241153334981,507.509809549972,507.778465762756,508.047121978078,
508.315778200272,508.584434432811,508.853090678737,509.121746940149,509.390403218918,
509.659059515956,509.927715832093,510.196372167238,510.465028521309,510.733684893389,
511.002341282627,511.270997687451,511.53965410638,511.808310537359,512.076966978421,
512.345623427198,512.614279881382,512.882936338452,513.151592795914,513.420249251254,
513.688905701946,513.957562145643,514.226218579942,514.494875002812,514.763531412143,
515.032187806366,515.300844183826,515.569500543564,515.838156884552,516.106813206581,
516.375469509421,516.644125793752,516.912782060321,517.181438310831,517.450094547186,
517.718750772238,517.987406989238,518.256063202315,518.524719416134,518.793375635194,
519.062031863421,519.330688103845,519.599344359133,519.868000631,520.136656920983,
520.405313229665,520.673969557583,520.942625904371,521.211282269698,521.479938652425,
521.748595051492,522.017251465163,522.285907891788,522.554564329201,522.823220775312,
523.091877227689,523.360533683951,523.629190141564,523.897846598005,524.166503050797,
524.435159497434,524.70381593565,524.972472363114,525.241128777924,525.509785178088,
525.778441562214,526.047097928818,526.315754277159,526.584410606435,526.853066916696,
527.121723207994,527.390379481309,527.659035737726,527.927691979287,528.19634820829,
528.465004427967,528.73366064202,529.002316854973,529.270973071551,529.539629295803,
529.808285531254,530.07694178051,530.345598045876,530.614254328701,530.882910630198,
531.151566950641,531.420223290284,531.688879648504,531.957536024733,532.226192417628,
532.494848825933,532.76350524776,533.032161681312,533.30081812432,533.569474574591,
533.838131029643,534.106787487035,534.375443944235,534.644100398706,534.912756848021,
535.181413289711,535.450069721605,535.718726141461,535.987382547516,536.256038937917,
536.524695311458,536.793351666845,537.062008003567,537.330664321065,537.599320619661,
537.867976899706,538.136633162493,538.40528940946,538.673945643001,538.942601865828,
539.211258081563,539.479914294375,539.748570509011,540.017226729904,540.285882960641,
540.554539204357,540.823195463252,541.09185173928,541.360508033441,541.629164346639,
541.897820678853,542.166477030068,542.435133399423,542.703789786121,542.972446188636,
543.241102605527,543.509759034775,543.778415474441,544.047071922176,544.315728375693,
544.584384832479,544.853041290046,545.121697745877,545.390354197441,545.659010642372,
545.927667078254,546.196323503025,546.464979914547,546.733636311202,547.002292691334,
547.270949053789,547.539605397955,547.808261722147,548.076918029812,548.345574313508,
548.614230583738,548.882886864851,549.151542935882,549.420199787641,549.68885445376,
549.957511414581),(0.,0.117809724509617,0.235619449019234,0.353429173528852,
0.471238898038469),.UNSPECIFIED.)
GEOMETRIC_REPRESENTATION_ITEM()
RATIONAL_B_SPLINE_SURFACE(((1.,0.707106781186548,1.,0.707106781186548,1.,
0.707106781186548,1.,0.707106781186548,1.),(1.,0.707106781186548,1.,0.707106781186548,
1.,0.707106781186548,1.,0.707106781186548,1.),(1.,0.707106781186548,1.,
0.707106781186548,1.,0.707106781186548,1.,0.707106781186548,1.),(1.,0.707106781186547,
1.,0.707106781186547,1.,0.707106781186547,1.,0.707106781186547,1.),(1.,
0.707106781186547,1.,0.707106781186547,1.,0.707106781186547,1.,0.707106781186547,
1.),(1.,0.707106781186548,1.,0.707106781186548,1.,0.707106781186548,1.,
0.707106781186548,1.),(1.,0.707106781186547,1.,0.707106781186547,1.,0.707106781186547,
1.,0.707106781186547,1.),(1.,0.707106781186547,1.,0.707106781186547,1.,
0.707106781186547,1.,0.707106781186547,1.),(1.,0.707106781186547,1.,0.707106781186547,
1.,0.707106781186547,1.,0.707106781186547,1.),(1.,0.707106781186547,1.,
0.707106781186547,1.,0.707106781186547,1.,0.707106781186547,1.),(1.,0.707106781186547,
1.,0.707106781186547,1.,0.707106781186547,1.,0.707106781186547,1.),(1.,
0.707106781186548,1.,0.707106781186548,1.,0.707106781186548,1.,0.707106781186548,
1.),(1.,0.707106781186548,1.,0.707106781186548,1.,0.707106781186548,1.,
0.707106781186548,1.),(1.,0.707106781186548,1.,0.707106781186548,1.,0.707106781186548,
1.,0.707106781186548,1.),(1.,0.707106781186547,1.,0.707106781186547,1.,
0.707106781186547,1.,0.707106781186547,1.),(1.,0.707106781186548,1.,0.707106781186548,
1.,0.707106781186548,1.,0.707106781186548,1.),(1.,0.707106781186547,1.,
0.707106781186547,1.,0.707106781186547,1.,0.707106781186547,1.),(1.,0.707106781186547,
1.,0.707106781186547,1.,0.707106781186547,1.,0.707106781186547,1.),(1.,
0.707106781186548,1.,0.707106781186548,1.,0.707106781186548,1.,0.707106781186548,
1.),(1.,0.707106781186547,1.,0.707106781186547,1.,0.707106781186547,1.,
0.707106781186547,1.),(1.,0.707106781186548,1.,0.707106781186548,1.,0.707106781186548,
1.,0.707106781186548,1.),(1.,0.707106781186547,1.,0.707106781186547,1.,
0.707106781186547,1.,0.707106781186547,1.),(1.,0.707106781186548,1.,0.707106781186548,
1.,0.707106781186548,1.,0.707106781186548,1.),(1.,0.707106781186547,1.,
0.707106781186547,1.,0.707106781186547,1.,0.707106781186547,1.),(1.,0.707106781186548,
1.,0.707106781186548,1.,0.707106781186548,1.,0.707106781186548,1.),(1.,
0.707106781186547,1.,0.707106781186547,1.,0.707106781186547,1.,0.707106781186547,
1.),(1.,0.707106781186547,1.,0.707106781186547,1.,0.707106781186547,1.,
0.707106781186547,1.),(1.,0.707106781186547,1.,0.707106781186547,1.,0.707106781186547,
1.,0.707106781186547,1.),(1.,0.707106781186547,1.,0.707106781186547,1.,
0.707106781186547,1.,0.707106781186547,1.),(1.,0.707106781186547,1.,0.707106781186547,
1.,0.707106781186547,1.,0.707106781186547,1.),(1.,0.707106781186548,1.,
0.707106781186548,1.,0.707106781186548,1.,0.707106781186548,1.),(1.,0.707106781186547,
1.,0.707106781186547,1.,0.707106781186547,1.,0.707106781186547,1.),(1.,
0.707106781186547,1.,0.707106781186547,1.,0.707106781186547,1.,0.707106781186547,
1.),(1.,0.707106781186548,1.,0.707106781186548,1.,0.707106781186548,1.,
0.707106781186548,1.),(1.,0.707106781186547,1.,0.707106781186547,1.,0.707106781186547,
1.,0.707106781186547,1.),(1.,0.707106781186547,1.,0.707106781186547,1.,
0.707106781186547,1.,0.707106781186547,1.),(1.,0.707106781186548,1.,0.707106781186548,
1.,0.707106781186548,1.,0.707106781186548,1.),(1.,0.707106781186547,1.,
0.707106781186547,1.,0.707106781186547,1.,0.707106781186547,1.),(1.,0.707106781186547,
1.,0.707106781186547,1.,0.707106781186547,1.,0.707106781186547,1.),(1.,
0.707106781186548,1.,0.707106781186548,1.,0.707106781186548,1.,0.707106781186548,
1.),(1.,0.707106781186548,1.,0.707106781186548,1.,0.707106781186548,1.,
0.707106781186548,1.),(1.,0.707106781186547,1.,0.707106781186547,1.,0.707106781186547,
1.,0.707106781186547,1.),(1.,0.707106781186548,1.,0.707106781186548,1.,
0.707106781186548,1.,0.707106781186548,1.),(1.,0.707106781186547,1.,0.707106781186547,
1.,0.707106781186547,1.,0.707106781186547,1.),(1.,0.707106781186547,1.,
0.707106781186547,1.,0.707106781186547,1.,0.707106781186547,1.),(1.,0.707106781186547,
1.,0.707106781186547,1.,0.707106781186547,1.,0.707106781186547,1.),(1.,
0.707106781186548,1.,0.707106781186548,1.,0.707106781186548,1.,0.707106781186548,
1.),(1.,0.707106781186548,1.,0.707106781186548,1.,0.707106781186548,1.,
0.707106781186548,1.),(1.,0.707106781186547,1.,0.707106781186547,1.,0.707106781186547,
1.,0.707106781186547,1.),(1.,0.707106781186547,1.,0.707106781186547,1.,
0.707106781186547,1.,0.707106781186547,1.),(1.,0.707106781186548,1.,0.707106781186548,
1.,0.707106781186548,1.,0.707106781186548,1.),(1.,0.707106781186547,1.,
0.707106781186547,1.,0.707106781186547,1.,0.707106781186547,1.),(1.,0.707106781186548,
1.,0.707106781186548,1.,0.707106781186548,1.,0.707106781186548,1.),(1.,
0.707106781186547,1.,0.707106781186547,1.,0.707106781186547,1.,0.707106781186547,
1.),(1.,0.707106781186547,1.,0.707106781186547,1.,0.707106781186547,1.,
0.707106781186547,1.),(1.,0.707106781186547,1.,0.707106781186547,1.,0.707106781186547,
1.,0.707106781186547,1.),(1.,0.707106781186547,1.,0.707106781186547,1.,
0.707106781186547,1.,0.707106781186547,1.),(1.,0.707106781186547,1.,0.707106781186547,
1.,0.707106781186547,1.,0.707106781186547,1.),(1.,0.707106781186548,1.,
0.707106781186548,1.,0.707106781186548,1.,0.707106781186548,1.),(1.,0.707106781186547,
1.,0.707106781186547,1.,0.707106781186547,1.,0.707106781186547,1.),(1.,
0.707106781186548,1.,0.707106781186548,1.,0.707106781186548,1.,0.707106781186548,
1.),(1.,0.707106781186547,1.,0.707106781186547,1.,0.707106781186547,1.,
0.707106781186547,1.),(1.,0.707106781186548,1.,0.707106781186548,1.,0.707106781186548,
1.,0.707106781186548,1.),(1.,0.707106781186547,1.,0.707106781186547,1.,
0.707106781186547,1.,0.707106781186547,1.),(1.,0.707106781186548,1.,0.707106781186548,
1.,0.707106781186548,1.,0.707106781186548,1.),(1.,0.707106781186547,1.,
0.707106781186547,1.,0.707106781186547,1.,0.707106781186547,1.),(1.,0.707106781186547,
1.,0.707106781186547,1.,0.707106781186547,1.,0.707106781186547,1.),(1.,
0.707106781186548,1.,0.707106781186548,1.,0.707106781186548,1.,0.707106781186548,
1.),(1.,0.707106781186547,1.,0.707106781186547,1.,0.707106781186547,1.,
0.707106781186547,1.),(1.,0.707106781186547,1.,0.707106781186547,1.,0.707106781186547,
1.,0.707106781186547,1.),(1.,0.707106781186548,1.,0.707106781186548,1.,
0.707106781186548,1.,0.707106781186548,1.),(1.,0.707106781186547,1.,0.707106781186547,
1.,0.707106781186547,1.,0.707106781186547,1.),(1.,0.707106781186548,1.,
0.707106781186548,1.,0.707106781186548,1.,0.707106781186548,1.),(1.,0.707106781186547,
1.,0.707106781186547,1.,0.707106781186547,1.,0.707106781186547,1.),(1.,
0.707106781186548,1.,0.707106781186548,1.,0.707106781186548,1.,0.707106781186548,
1.),(1.,0.707106781186548,1.,0.707106781186548,1.,0.707106781186548,1.,
0.707106781186548,1.),(1.,0.707106781186547,1.,0.707106781186547,1.,0.707106781186547,
1.,0.707106781186547,1.),(1.,0.707106781186548,1.,0.707106781186548,1.,
0.707106781186548,1.,0.707106781186548,1.),(1.,0.707106781186547,1.,0.707106781186547,
1.,0.707106781186547,1.,0.707106781186547,1.),(1.,0.707106781186547,1.,
0.707106781186547,1.,0.707106781186547,1.,0.707106781186547,1.),(1.,0.707106781186548,
1.,0.707106781186548,1.,0.707106781186548,1.,0.707106781186548,1.),(1.,
0.707106781186547,1.,0.707106781186547,1.,0.707106781186547,1.,0.707106781186547,
1.),(1.,0.707106781186547,1.,0.707106781186547,1.,0.707106781186547,1.,
0.707106781186547,1.),(1.,0.707106781186547,1.,0.707106781186547,1.,0.707106781186547,
1.,0.707106781186547,1.),(1.,0.707106781186548,1.,0.707106781186548,1.,
0.707106781186548,1.,0.707106781186548,1.),(1.,0.707106781186547,1.,0.707106781186547,
1.,0.707106781186547,1.,0.707106781186547,1.),(1.,0.707106781186547,1.,
0.707106781186547,1.,0.707106781186547,1.,0.707106781186547,1.),(1.,0.707106781186547,
1.,0.707106781186547,1.,0.707106781186547,1.,0.707106781186547,1.),(1.,
0.707106781186547,1.,0.707106781186547,1.,0.707106781186547,1.,0.707106781186547,
1.),(1.,0.707106781186547,1.,0.707106781186547,1.,0.707106781186547,1.,
0.707106781186547,1.),(1.,0.707106781186547,1.,0.707106781186547,1.,0.707106781186547,
1.,0.707106781186547,1.),(1.,0.707106781186548,1.,0.707106781186548,1.,
0.707106781186548,1.,0.707106781186548,1.),(1.,0.707106781186548,1.,0.707106781186548,
1.,0.707106781186548,1.,0.707106781186548,1.),(1.,0.707106781186547,1.,
0.707106781186547,1.,0.707106781186547,1.,0.707106781186547,1.),(1.,0.707106781186548,
1.,0.707106781186548,1.,0.707106781186548,1.,0.707106781186548,1.),(1.,
0.707106781186547,1.,0.707106781186547,1.,0.707106781186547,1.,0.707106781186547,
1.),(1.,0.707106781186548,1.,0.707106781186548,1.,0.707106781186548,1.,
0.707106781186548,1.),(1.,0.707106781186548,1.,0.707106781186548,1.,0.707106781186548,
1.,0.707106781186548,1.),(1.,0.707106781186547,1.,0.707106781186547,1.,
0.707106781186547,1.,0.707106781186547,1.),(1.,0.707106781186548,1.,0.707106781186548,
1.,0.707106781186548,1.,0.707106781186548,1.),(1.,0.707106781186548,1.,
0.707106781186548,1.,0.707106781186548,1.,0.707106781186548,1.),(1.,0.707106781186548,
1.,0.707106781186548,1.,0.707106781186548,1.,0.707106781186548,1.),(1.,
0.707106781186547,1.,0.707106781186547,1.,0.707106781186547,1.,0.707106781186547,
1.),(1.,0.707106781186548,1.,0.707106781186548,1.,0.707106781186548,1.,
0.707106781186548,1.),(1.,0.707106781186547,1.,0.707106781186547,1.,0.707106781186547,
1.,0.707106781186547,1.),(1.,0.707106781186548,1.,0.707106781186548,1.,
0.707106781186548,1.,0.707106781186548,1.),(1.,0.707106781186548,1.,0.707106781186548,
1.,0.707106781186548,1.,0.707106781186548,1.),(1.,0.707106781186548,1.,
0.707106781186548,1.,0.707106781186548,1.,0.707106781186548,1.),(1.,0.707106781186547,
1.,0.707106781186547,1.,0.707106781186547,1.,0.707106781186547,1.),(1.,
0.707106781186547,1.,0.707106781186547,1.,0.707106781186547,1.,0.707106781186547,
1.),(1.,0.707106781186547,1.,0.707106781186547,1.,0.707106781186547,1.,
0.707106781186547,1.),(1.,0.707106781186548,1.,0.707106781186548,1.,0.707106781186548,
1.,0.707106781186548,1.),(1.,0.707106781186548,1.,0.707106781186548,1.,
0.707106781186548,1.,0.707106781186548,1.),(1.,0.707106781186548,1.,0.707106781186548,
1.,0.707106781186548,1.,0.707106781186548,1.),(1.,0.707106781186547,1.,
0.707106781186547,1.,0.707106781186547,1.,0.707106781186547,1.),(1.,0.707106781186547,
1.,0.707106781186547,1.,0.707106781186547,1.,0.707106781186547,1.),(1.,
0.707106781186547,1.,0.707106781186547,1.,0.707106781186547,1.,0.707106781186547,
1.),(1.,0.707106781186548,1.,0.707106781186548,1.,0.707106781186548,1.,
0.707106781186548,1.),(1.,0.707106781186548,1.,0.707106781186548,1.,0.707106781186548,
1.,0.707106781186548,1.),(1.,0.707106781186547,1.,0.707106781186547,1.,
0.707106781186547,1.,0.707106781186547,1.),(1.,0.707106781186547,1.,0.707106781186547,
1.,0.707106781186547,1.,0.707106781186547,1.),(1.,0.707106781186548,1.,
0.707106781186548,1.,0.707106781186548,1.,0.707106781186548,1.),(1.,0.707106781186547,
1.,0.707106781186547,1.,0.707106781186547,1.,0.707106781186547,1.),(1.,
0.707106781186547,1.,0.707106781186547,1.,0.707106781186547,1.,0.707106781186547,
1.),(1.,0.707106781186547,1.,0.707106781186547,1.,0.707106781186547,1.,
0.707106781186547,1.),(1.,0.707106781186547,1.,0.707106781186547,1.,0.707106781186547,
1.,0.707106781186547,1.),(1.,0.707106781186548,1.,0.707106781186548,1.,
0.707106781186548,1.,0.707106781186548,1.),(1.,0.707106781186547,1.,0.707106781186547,
1.,0.707106781186547,1.,0.707106781186547,1.),(1.,0.707106781186548,1.,
0.707106781186548,1.,0.707106781186548,1.,0.707106781186548,1.),(1.,0.707106781186547,
1.,0.707106781186547,1.,0.707106781186547,1.,0.707106781186547,1.),(1.,
0.707106781186547,1.,0.707106781186547,1.,0.707106781186547,1.,0.707106781186547,
1.),(1.,0.707106781186547,1.,0.707106781186547,1.,0.707106781186547,1.,
0.707106781186547,1.),(1.,0.707106781186548,1.,0.707106781186548,1.,0.707106781186548,
1.,0.707106781186548,1.),(1.,0.707106781186548,1.,0.707106781186548,1.,
0.707106781186548,1.,0.707106781186548,1.),(1.,0.707106781186547,1.,0.707106781186547,
1.,0.707106781186547,1.,0.707106781186547,1.),(1.,0.707106781186548,1.,
0.707106781186548,1.,0.707106781186548,1.,0.707106781186548,1.),(1.,0.707106781186548,
1.,0.707106781186548,1.,0.707106781186548,1.,0.707106781186548,1.),(1.,
0.707106781186547,1.,0.707106781186547,1.,0.707106781186547,1.,0.707106781186547,
1.),(1.,0.707106781186548,1.,0.707106781186548,1.,0.707106781186548,1.,
0.707106781186548,1.),(1.,0.707106781186547,1.,0.707106781186547,1.,0.707106781186547,
1.,0.707106781186547,1.),(1.,0.707106781186548,1.,0.707106781186548,1.,
0.707106781186548,1.,0.707106781186548,1.),(1.,0.707106781186547,1.,0.707106781186547,
1.,0.707106781186547,1.,0.707106781186547,1.),(1.,0.707106781186548,1.,
0.707106781186548,1.,0.707106781186548,1.,0.707106781186548,1.),(1.,0.707106781186547,
1.,0.707106781186547,1.,0.707106781186547,1.,0.707106781186547,1.),(1.,
0.707106781186547,1.,0.707106781186547,1.,0.707106781186547,1.,0.707106781186547,
1.),(1.,0.707106781186548,1.,0.707106781186548,1.,0.707106781186548,1.,
0.707106781186548,1.),(1.,0.707106781186547,1.,0.707106781186547,1.,0.707106781186547,
1.,0.707106781186547,1.),(1.,0.707106781186547,1.,0.707106781186547,1.,
0.707106781186547,1.,0.707106781186547,1.),(1.,0.707106781186548,1.,0.707106781186548,
1.,0.707106781186548,1.,0.707106781186548,1.),(1.,0.707106781186547,1.,
0.707106781186547,1.,0.707106781186547,1.,0.707106781186547,1.),(1.,0.707106781186547,
1.,0.707106781186547,1.,0.707106781186547,1.,0.707106781186547,1.),(1.,
0.707106781186548,1.,0.707106781186548,1.,0.707106781186548,1.,0.707106781186548,
1.),(1.,0.707106781186547,1.,0.707106781186547,1.,0.707106781186547,1.,
0.707106781186547,1.),(1.,0.707106781186548,1.,0.707106781186548,1.,0.707106781186548,
1.,0.707106781186548,1.),(1.,0.707106781186547,1.,0.707106781186547,1.,
0.707106781186547,1.,0.707106781186547,1.),(1.,0.707106781186547,1.,0.707106781186547,
1.,0.707106781186547,1.,0.707106781186547,1.),(1.,0.707106781186548,1.,
0.707106781186548,1.,0.707106781186548,1.,0.707106781186548,1.),(1.,0.707106781186548,
1.,0.707106781186548,1.,0.707106781186548,1.,0.707106781186548,1.),(1.,
0.707106781186547,1.,0.707106781186547,1.,0.707106781186547,1.,0.707106781186547,
1.),(1.,0.707106781186548,1.,0.707106781186548,1.,0.707106781186548,1.,
0.707106781186548,1.),(1.,0.707106781186547,1.,0.707106781186547,1.,0.707106781186547,
1.,0.707106781186547,1.),(1.,0.707106781186548,1.,0.707106781186548,1.,
0.707106781186548,1.,0.707106781186548,1.),(1.,0.707106781186547,1.,0.707106781186547,
1.,0.707106781186547,1.,0.707106781186547,1.),(1.,0.707106781186548,1.,
0.707106781186548,1.,0.707106781186548,1.,0.707106781186548,1.),(1.,0.707106781186547,
1.,0.707106781186547,1.,0.707106781186547,1.,0.707106781186547,1.),(1.,
0.707106781186548,1.,0.707106781186548,1.,0.707106781186548,1.,0.707106781186548,
1.),(1.,0.707106781186547,1.,0.707106781186547,1.,0.707106781186547,1.,
0.707106781186547,1.),(1.,0.707106781186548,1.,0.707106781186548,1.,0.707106781186548,
1.,0.707106781186548,1.),(1.,0.707106781186547,1.,0.707106781186547,1.,
0.707106781186547,1.,0.707106781186547,1.),(1.,0.707106781186548,1.,0.707106781186548,
1.,0.707106781186548,1.,0.707106781186548,1.),(1.,0.707106781186547,1.,
0.707106781186547,1.,0.707106781186547,1.,0.707106781186547,1.),(1.,0.707106781186548,
1.,0.707106781186548,1.,0.707106781186548,1.,0.707106781186548,1.),(1.,
0.707106781186547,1.,0.707106781186547,1.,0.707106781186547,1.,0.707106781186547,
1.),(1.,0.707106781186547,1.,0.707106781186547,1.,0.707106781186547,1.,
0.707106781186547,1.),(1.,0.707106781186548,1.,0.707106781186548,1.,0.707106781186548,
1.,0.707106781186548,1.),(1.,0.707106781186547,1.,0.707106781186547,1.,
0.707106781186547,1.,0.707106781186547,1.),(1.,0.707106781186548,1.,0.707106781186548,
1.,0.707106781186548,1.,0.707106781186548,1.),(1.,0.707106781186547,1.,
0.707106781186547,1.,0.707106781186547,1.,0.707106781186547,1.),(1.,0.707106781186548,
1.,0.707106781186548,1.,0.707106781186548,1.,0.707106781186548,1.),(1.,
0.707106781186547,1.,0.707106781186547,1.,0.707106781186547,1.,0.707106781186547,
1.),(1.,0.707106781186548,1.,0.707106781186548,1.,0.707106781186548,1.,
0.707106781186548,1.),(1.,0.707106781186547,1.,0.707106781186547,1.,0.707106781186547,
1.,0.707106781186547,1.),(1.,0.707106781186547,1.,0.707106781186547,1.,
0.707106781186547,1.,0.707106781186547,1.),(1.,0.707106781186548,1.,0.707106781186548,
1.,0.707106781186548,1.,0.707106781186548,1.),(1.,0.707106781186547,1.,
0.707106781186547,1.,0.707106781186547,1.,0.707106781186547,1.),(1.,0.707106781186548,
1.,0.707106781186548,1.,0.707106781186548,1.,0.707106781186548,1.),(1.,
0.707106781186548,1.,0.707106781186548,1.,0.707106781186548,1.,0.707106781186548,
1.),(1.,0.707106781186548,1.,0.707106781186548,1.,0.707106781186548,1.,
0.707106781186548,1.),(1.,0.707106781186547,1.,0.707106781186547,1.,0.707106781186547,
1.,0.707106781186547,1.),(1.,0.707106781186547,1.,0.707106781186547,1.,
0.707106781186547,1.,0.707106781186547,1.),(1.,0.707106781186547,1.,0.707106781186547,
1.,0.707106781186547,1.,0.707106781186547,1.),(1.,0.707106781186547,1.,
0.707106781186547,1.,0.707106781186547,1.,0.707106781186547,1.),(1.,0.707106781186548,
1.,0.707106781186548,1.,0.707106781186548,1.,0.707106781186548,1.),(1.,
0.707106781186547,1.,0.707106781186547,1.,0.707106781186547,1.,0.707106781186547,
1.),(1.,0.707106781186548,1.,0.707106781186548,1.,0.707106781186548,1.,
0.707106781186548,1.),(1.,0.707106781186548,1.,0.707106781186548,1.,0.707106781186548,
1.,0.707106781186548,1.),(1.,0.707106781186547,1.,0.707106781186547,1.,
0.707106781186547,1.,0.707106781186547,1.),(1.,0.707106781186547,1.,0.707106781186547,
1.,0.707106781186547,1.,0.707106781186547,1.),(1.,0.707106781186548,1.,
0.707106781186548,1.,0.707106781186548,1.,0.707106781186548,1.),(1.,0.707106781186548,
1.,0.707106781186548,1.,0.707106781186548,1.,0.707106781186548,1.),(1.,
0.707106781186547,1.,0.707106781186547,1.,0.707106781186547,1.,0.707106781186547,
1.),(1.,0.707106781186547,1.,0.707106781186547,1.,0.707106781186547,1.,
0.707106781186547,1.),(1.,0.707106781186548,1.,0.707106781186548,1.,0.707106781186548,
1.,0.707106781186548,1.),(1.,0.707106781186547,1.,0.707106781186547,1.,
0.707106781186547,1.,0.707106781186547,1.),(1.,0.707106781186548,1.,0.707106781186548,
1.,0.707106781186548,1.,0.707106781186548,1.),(1.,0.707106781186547,1.,
0.707106781186547,1.,0.707106781186547,1.,0.707106781186547,1.),(1.,0.707106781186547,
1.,0.707106781186547,1.,0.707106781186547,1.,0.707106781186547,1.),(1.,
0.707106781186547,1.,0.707106781186547,1.,0.707106781186547,1.,0.707106781186547,
1.),(1.,0.707106781186547,1.,0.707106781186547,1.,0.707106781186547,1.,
0.707106781186547,1.),(1.,0.707106781186547,1.,0.707106781186547,1.,0.707106781186547,
1.,0.707106781186547,1.),(1.,0.707106781186547,1.,0.707106781186547,1.,
0.707106781186547,1.,0.707106781186547,1.),(1.,0.707106781186547,1.,0.707106781186547,
1.,0.707106781186547,1.,0.707106781186547,1.),(1.,0.707106781186548,1.,
0.707106781186548,1.,0.707106781186548,1.,0.707106781186548,1.),(1.,0.707106781186547,
1.,0.707106781186547,1.,0.707106781186547,1.,0.707106781186547,1.),(1.,
0.707106781186548,1.,0.707106781186548,1.,0.707106781186548,1.,0.707106781186548,
1.),(1.,0.707106781186547,1.,0.707106781186547,1.,0.707106781186547,1.,
0.707106781186547,1.),(1.,0.707106781186548,1.,0.707106781186548,1.,0.707106781186548,
1.,0.707106781186548,1.),(1.,0.707106781186548,1.,0.707106781186548,1.,
0.707106781186548,1.,0.707106781186548,1.),(1.,0.707106781186547,1.,0.707106781186547,
1.,0.707106781186547,1.,0.707106781186547,1.),(1.,0.707106781186548,1.,
0.707106781186548,1.,0.707106781186548,1.,0.707106781186548,1.),(1.,0.707106781186548,
1.,0.707106781186548,1.,0.707106781186548,1.,0.707106781186548,1.),(1.,
0.707106781186548,1.,0.707106781186548,1.,0.707106781186548,1.,0.707106781186548,
1.),(1.,0.707106781186548,1.,0.707106781186548,1.,0.707106781186548,1.,
0.707106781186548,1.),(1.,0.707106781186547,1.,0.707106781186547,1.,0.707106781186547,
1.,0.707106781186547,1.),(1.,0.707106781186548,1.,0.707106781186548,1.,
0.707106781186548,1.,0.707106781186548,1.),(1.,0.707106781186547,1.,0.707106781186547,
1.,0.707106781186547,1.,0.707106781186547,1.),(1.,0.707106781186548,1.,
0.707106781186548,1.,0.707106781186548,1.,0.707106781186548,1.),(1.,0.707106781186547,
1.,0.707106781186547,1.,0.707106781186547,1.,0.707106781186547,1.),(1.,
0.707106781186547,1.,0.707106781186547,1.,0.707106781186547,1.,0.707106781186547,
1.),(1.,0.707106781186548,1.,0.707106781186548,1.,0.707106781186548,1.,
0.707106781186548,1.),(1.,0.707106781186548,1.,0.707106781186548,1.,0.707106781186548,
1.,0.707106781186548,1.),(1.,0.707106781186547,1.,0.707106781186547,1.,
0.707106781186547,1.,0.707106781186547,1.),(1.,0.707106781186547,1.,0.707106781186547,
1.,0.707106781186547,1.,0.707106781186547,1.),(1.,0.707106781186547,1.,
0.707106781186547,1.,0.707106781186547,1.,0.707106781186547,1.),(1.,0.707106781186547,
1.,0.707106781186547,1.,0.707106781186547,1.,0.707106781186547,1.),(1.,
0.707106781186547,1.,0.707106781186547,1.,0.707106781186547,1.,0.707106781186547,
1.),(1.,0.707106781186548,1.,0.707106781186548,1.,0.707106781186548,1.,
0.707106781186548,1.),(1.,0.707106781186548,1.,0.707106781186548,1.,0.707106781186548,
1.,0.707106781186548,1.),(1.,0.707106781186547,1.,0.707106781186547,1.,
0.707106781186547,1.,0.707106781186547,1.),(1.,0.707106781186547,1.,0.707106781186547,
1.,0.707106781186547,1.,0.707106781186547,1.),(1.,0.707106781186548,1.,
0.707106781186548,1.,0.707106781186548,1.,0.707106781186548,1.),(1.,0.707106781186548,
1.,0.707106781186548,1.,0.707106781186548,1.,0.707106781186548,1.),(1.,
0.707106781186547,1.,0.707106781186547,1.,0.707106781186547,1.,0.707106781186547,
1.),(1.,0.707106781186548,1.,0.707106781186548,1.,0.707106781186548,1.,
0.707106781186548,1.),(1.,0.707106781186547,1.,0.707106781186547,1.,0.707106781186547,
1.,0.707106781186547,1.),(1.,0.707106781186548,1.,0.707106781186548,1.,
0.707106781186548,1.,0.707106781186548,1.),(1.,0.707106781186548,1.,0.707106781186548,
1.,0.707106781186548,1.,0.707106781186548,1.),(1.,0.707106781186547,1.,
0.707106781186547,1.,0.707106781186547,1.,0.707106781186547,1.),(1.,0.707106781186547,
1.,0.707106781186547,1.,0.707106781186547,1.,0.707106781186547,1.),(1.,
0.707106781186548,1.,0.707106781186548,1.,0.707106781186548,1.,0.707106781186548,
1.),(1.,0.707106781186547,1.,0.707106781186547,1.,0.707106781186547,1.,
0.707106781186547,1.),(1.,0.707106781186547,1.,0.707106781186547,1.,0.707106781186547,
1.,0.707106781186547,1.),(1.,0.707106781186548,1.,0.707106781186548,1.,
0.707106781186548,1.,0.707106781186548,1.),(1.,0.707106781186547,1.,0.707106781186547,
1.,0.707106781186547,1.,0.707106781186547,1.),(1.,0.707106781186548,1.,
0.707106781186548,1.,0.707106781186548,1.,0.707106781186548,1.),(1.,0.707106781186547,
1.,0.707106781186547,1.,0.707106781186547,1.,0.707106781186547,1.),(1.,
0.707106781186548,1.,0.707106781186548,1.,0.707106781186548,1.,0.707106781186548,
1.),(1.,0.707106781186547,1.,0.707106781186547,1.,0.707106781186547,1.,
0.707106781186547,1.),(1.,0.707106781186547,1.,0.707106781186547,1.,0.707106781186547,
1.,0.707106781186547,1.),(1.,0.707106781186548,1.,0.707106781186548,1.,
0.707106781186548,1.,0.707106781186548,1.),(1.,0.707106781186548,1.,0.707106781186548,
1.,0.707106781186548,1.,0.707106781186548,1.),(1.,0.707106781186547,1.,
0.707106781186547,1.,0.707106781186547,1.,0.707106781186547,1.),(1.,0.707106781186547,
1.,0.707106781186547,1.,0.707106781186547,1.,0.707106781186547,1.),(1.,
0.707106781186548,1.,0.707106781186548,1.,0.707106781186548,1.,0.707106781186548,
1.),(1.,0.707106781186547,1.,0.707106781186547,1.,0.707106781186547,1.,
0.707106781186547,1.),(1.,0.707106781186547,1.,0.707106781186547,1.,0.707106781186547,
1.,0.707106781186547,1.),(1.,0.707106781186548,1.,0.707106781186548,1.,
0.707106781186548,1.,0.707106781186548,1.),(1.,0.707106781186547,1.,0.707106781186547,
1.,0.707106781186547,1.,0.707106781186547,1.),(1.,0.707106781186548,1.,
0.707106781186548,1.,0.707106781186548,1.,0.707106781186548,1.),(1.,0.707106781186547,
1.,0.707106781186547,1.,0.707106781186547,1.,0.707106781186547,1.),(1.,
0.707106781186548,1.,0.707106781186548,1.,0.707106781186548,1.,0.707106781186548,
1.),(1.,0.707106781186547,1.,0.707106781186547,1.,0.707106781186547,1.,
0.707106781186547,1.),(1.,0.707106781186548,1.,0.707106781186548,1.,0.707106781186548,
1.,0.707106781186548,1.),(1.,0.707106781186547,1.,0.707106781186547,1.,
0.707106781186547,1.,0.707106781186547,1.),(1.,0.707106781186547,1.,0.707106781186547,
1.,0.707106781186547,1.,0.707106781186547,1.),(1.,0.707106781186547,1.,
0.707106781186547,1.,0.707106781186547,1.,0.707106781186547,1.),(1.,0.707106781186547,
1.,0.707106781186547,1.,0.707106781186547,1.,0.707106781186547,1.),(1.,
0.707106781186547,1.,0.707106781186547,1.,0.707106781186547,1.,0.707106781186547,
1.),(1.,0.707106781186547,1.,0.707106781186547,1.,0.707106781186547,1.,
0.707106781186547,1.),(1.,0.707106781186548,1.,0.707106781186548,1.,0.707106781186548,
1.,0.707106781186548,1.),(1.,0.707106781186547,1.,0.707106781186547,1.,
0.707106781186547,1.,0.707106781186547,1.),(1.,0.707106781186548,1.,0.707106781186548,
1.,0.707106781186548,1.,0.707106781186548,1.),(1.,0.707106781186547,1.,
0.707106781186547,1.,0.707106781186547,1.,0.707106781186547,1.),(1.,0.707106781186548,
1.,0.707106781186548,1.,0.707106781186548,1.,0.707106781186548,1.),(1.,
0.707106781186548,1.,0.707106781186548,1.,0.707106781186548,1.,0.707106781186548,
1.),(1.,0.707106781186547,1.,0.707106781186547,1.,0.707106781186547,1.,
0.707106781186547,1.),(1.,0.707106781186548,1.,0.707106781186548,1.,0.707106781186548,
1.,0.707106781186548,1.),(1.,0.707106781186548,1.,0.707106781186548,1.,
0.707106781186548,1.,0.707106781186548,1.),(1.,0.707106781186547,1.,0.707106781186547,
1.,0.707106781186547,1.,0.707106781186547,1.),(1.,0.707106781186548,1.,
0.707106781186548,1.,0.707106781186548,1.,0.707106781186548,1.),(1.,0.707106781186547,
1.,0.707106781186547,1.,0.707106781186547,1.,0.707106781186547,1.),(1.,
0.707106781186547,1.,0.707106781186547,1.,0.707106781186547,1.,0.707106781186547,
1.),(1.,0.707106781186547,1.,0.707106781186547,1.,0.707106781186547,1.,
0.707106781186547,1.),(1.,0.707106781186548,1.,0.707106781186548,1.,0.707106781186548,
1.,0.707106781186548,1.),(1.,0.707106781186547,1.,0.707106781186547,1.,
0.707106781186547,1.,0.707106781186547,1.),(1.,0.707106781186547,1.,0.707106781186547,
1.,0.707106781186547,1.,0.707106781186547,1.),(1.,0.707106781186548,1.,
0.707106781186548,1.,0.707106781186548,1.,0.707106781186548,1.),(1.,0.707106781186547,
1.,0.707106781186547,1.,0.707106781186547,1.,0.707106781186547,1.),(1.,
0.707106781186548,1.,0.707106781186548,1.,0.707106781186548,1.,0.707106781186548,
1.),(1.,0.707106781186547,1.,0.707106781186547,1.,0.707106781186547,1.,
0.707106781186547,1.),(1.,0.707106781186547,1.,0.707106781186547,1.,0.707106781186547,
1.,0.707106781186547,1.),(1.,0.707106781186547,1.,0.707106781186547,1.,
0.707106781186547,1.,0.707106781186547,1.),(1.,0.707106781186548,1.,0.707106781186548,
1.,0.707106781186548,1.,0.707106781186548,1.),(1.,0.707106781186548,1.,
0.707106781186548,1.,0.707106781186548,1.,0.707106781186548,1.),(1.,0.707106781186547,
1.,0.707106781186547,1.,0.707106781186547,1.,0.707106781186547,1.),(1.,
0.707106781186548,1.,0.707106781186548,1.,0.707106781186548,1.,0.707106781186548,
1.),(1.,0.707106781186548,1.,0.707106781186548,1.,0.707106781186548,1.,
0.707106781186548,1.),(1.,0.707106781186547,1.,0.707106781186547,1.,0.707106781186547,
1.,0.707106781186547,1.),(1.,0.707106781186548,1.,0.707106781186548,1.,
0.707106781186548,1.,0.707106781186548,1.),(1.,0.707106781186547,1.,0.707106781186547,
1.,0.707106781186547,1.,0.707106781186547,1.),(1.,0.707106781186548,1.,
0.707106781186548,1.,0.707106781186548,1.,0.707106781186548,1.),(1.,0.707106781186548,
1.,0.707106781186548,1.,0.707106781186548,1.,0.707106781186548,1.),(1.,
0.707106781186547,1.,0.707106781186547,1.,0.707106781186547,1.,0.707106781186547,
1.),(1.,0.707106781186548,1.,0.707106781186548,1.,0.707106781186548,1.,
0.707106781186548,1.),(1.,0.707106781186548,1.,0.707106781186548,1.,0.707106781186548,
1.,0.707106781186548,1.),(1.,0.707106781186548,1.,0.707106781186548,1.,
0.707106781186548,1.,0.707106781186548,1.),(1.,0.707106781186547,1.,0.707106781186547,
1.,0.707106781186547,1.,0.707106781186547,1.),(1.,0.707106781186547,1.,
0.707106781186547,1.,0.707106781186547,1.,0.707106781186547,1.),(1.,0.707106781186548,
1.,0.707106781186548,1.,0.707106781186548,1.,0.707106781186548,1.),(1.,
0.707106781186547,1.,0.707106781186547,1.,0.707106781186547,1.,0.707106781186547,
1.),(1.,0.707106781186548,1.,0.707106781186548,1.,0.707106781186548,1.,
0.707106781186548,1.),(1.,0.707106781186547,1.,0.707106781186547,1.,0.707106781186547,
1.,0.707106781186547,1.),(1.,0.707106781186547,1.,0.707106781186547,1.,
0.707106781186547,1.,0.707106781186547,1.),(1.,0.707106781186548,1.,0.707106781186548,
1.,0.707106781186548,1.,0.707106781186548,1.),(1.,0.707106781186548,1.,
0.707106781186548,1.,0.707106781186548,1.,0.707106781186548,1.),(1.,0.707106781186548,
1.,0.707106781186548,1.,0.707106781186548,1.,0.707106781186548,1.),(1.,
0.707106781186547,1.,0.707106781186547,1.,0.707106781186547,1.,0.707106781186547,
1.),(1.,0.707106781186547,1.,0.707106781186547,1.,0.707106781186547,1.,
0.707106781186547,1.),(1.,0.707106781186548,1.,0.707106781186548,1.,0.707106781186548,
1.,0.707106781186548,1.),(1.,0.707106781186548,1.,0.707106781186548,1.,
0.707106781186548,1.,0.707106781186548,1.),(1.,0.707106781186547,1.,0.707106781186547,
1.,0.707106781186547,1.,0.707106781186547,1.),(1.,0.707106781186547,1.,
0.707106781186547,1.,0.707106781186547,1.,0.707106781186547,1.),(1.,0.707106781186548,
1.,0.707106781186548,1.,0.707106781186548,1.,0.707106781186548,1.),(1.,
0.707106781186547,1.,0.707106781186547,1.,0.707106781186547,1.,0.707106781186547,
1.),(1.,0.707106781186547,1.,0.707106781186547,1.,0.707106781186547,1.,
0.707106781186547,1.),(1.,0.707106781186548,1.,0.707106781186548,1.,0.707106781186548,
1.,0.707106781186548,1.),(1.,0.707106781186548,1.,0.707106781186548,1.,
0.707106781186548,1.,0.707106781186548,1.),(1.,0.707106781186547,1.,0.707106781186547,
1.,0.707106781186547,1.,0.707106781186547,1.),(1.,0.707106781186547,1.,
0.707106781186547,1.,0.707106781186547,1.,0.707106781186547,1.),(1.,0.707106781186547,
1.,0.707106781186547,1.,0.707106781186547,1.,0.707106781186547,1.),(1.,
0.707106781186548,1.,0.707106781186548,1.,0.707106781186548,1.,0.707106781186548,
1.),(1.,0.707106781186547,1.,0.707106781186547,1.,0.707106781186547,1.,
0.707106781186547,1.),(1.,0.707106781186547,1.,0.707106781186547,1.,0.707106781186547,
1.,0.707106781186547,1.),(1.,0.707106781186547,1.,0.707106781186547,1.,
0.707106781186547,1.,0.707106781186547,1.),(1.,0.707106781186548,1.,0.707106781186548,
1.,0.707106781186548,1.,0.707106781186548,1.),(1.,0.707106781186548,1.,
0.707106781186548,1.,0.707106781186548,1.,0.707106781186548,1.),(1.,0.707106781186547,
1.,0.707106781186547,1.,0.707106781186547,1.,0.707106781186547,1.),(1.,
0.707106781186548,1.,0.707106781186548,1.,0.707106781186548,1.,0.707106781186548,
1.),(1.,0.707106781186547,1.,0.707106781186547,1.,0.707106781186547,1.,
0.707106781186547,1.),(1.,0.707106781186548,1.,0.707106781186548,1.,0.707106781186548,
1.,0.707106781186548,1.),(1.,0.707106781186547,1.,0.707106781186547,1.,
0.707106781186547,1.,0.707106781186547,1.),(1.,0.707106781186548,1.,0.707106781186548,
1.,0.707106781186548,1.,0.707106781186548,1.),(1.,0.707106781186548,1.,
0.707106781186548,1.,0.707106781186548,1.,0.707106781186548,1.),(1.,0.707106781186547,
1.,0.707106781186547,1.,0.707106781186547,1.,0.707106781186547,1.),(1.,
0.707106781186547,1.,0.707106781186547,1.,0.707106781186547,1.,0.707106781186547,
1.),(1.,0.707106781186548,1.,0.707106781186548,1.,0.707106781186548,1.,
0.707106781186548,1.),(1.,0.707106781186547,1.,0.707106781186547,1.,0.707106781186547,
1.,0.707106781186547,1.),(1.,0.707106781186547,1.,0.707106781186547,1.,
0.707106781186547,1.,0.707106781186547,1.),(1.,0.707106781186548,1.,0.707106781186548,
1.,0.707106781186548,1.,0.707106781186548,1.),(1.,0.707106781186547,1.,
0.707106781186547,1.,0.707106781186547,1.,0.707106781186547,1.),(1.,0.707106781186548,
1.,0.707106781186548,1.,0.707106781186548,1.,0.707106781186548,1.),(1.,
0.707106781186548,1.,0.707106781186548,1.,0.707106781186548,1.,0.707106781186548,
1.),(1.,0.707106781186547,1.,0.707106781186547,1.,0.707106781186547,1.,
0.707106781186547,1.),(1.,0.707106781186548,1.,0.707106781186548,1.,0.707106781186548,
1.,0.707106781186548,1.),(1.,0.707106781186547,1.,0.707106781186547,1.,
0.707106781186547,1.,0.707106781186547,1.),(1.,0.707106781186547,1.,0.707106781186547,
1.,0.707106781186547,1.,0.707106781186547,1.),(1.,0.707106781186547,1.,
0.707106781186547,1.,0.707106781186547,1.,0.707106781186547,1.),(1.,0.707106781186548,
1.,0.707106781186548,1.,0.707106781186548,1.,0.707106781186548,1.),(1.,
0.707106781186548,1.,0.707106781186548,1.,0.707106781186548,1.,0.707106781186548,
1.),(1.,0.707106781186548,1.,0.707106781186548,1.,0.707106781186548,1.,
0.707106781186548,1.),(1.,0.707106781186547,1.,0.707106781186547,1.,0.707106781186547,
1.,0.707106781186547,1.),(1.,0.707106781186548,1.,0.707106781186548,1.,
0.707106781186548,1.,0.707106781186548,1.),(1.,0.707106781186547,1.,0.707106781186547,
1.,0.707106781186547,1.,0.707106781186547,1.),(1.,0.707106781186548,1.,
0.707106781186548,1.,0.707106781186548,1.,0.707106781186548,1.),(1.,0.707106781186547,
1.,0.707106781186547,1.,0.707106781186547,1.,0.707106781186547,1.),(1.,
0.707106781186547,1.,0.707106781186547,1.,0.707106781186547,1.,0.707106781186547,
1.),(1.,0.707106781186547,1.,0.707106781186547,1.,0.707106781186547,1.,
0.707106781186547,1.),(1.,0.707106781186547,1.,0.707106781186547,1.,0.707106781186547,
1.,0.707106781186547,1.),(1.,0.707106781186548,1.,0.707106781186548,1.,
0.707106781186548,1.,0.707106781186548,1.),(1.,0.707106781186548,1.,0.707106781186548,
1.,0.707106781186548,1.,0.707106781186548,1.),(1.,0.707106781186547,1.,
0.707106781186547,1.,0.707106781186547,1.,0.707106781186547,1.),(1.,0.707106781186547,
1.,0.707106781186547,1.,0.707106781186547,1.,0.707106781186547,1.),(1.,
0.707106781186548,1.,0.707106781186548,1.,0.707106781186548,1.,0.707106781186548,
1.),(1.,0.707106781186547,1.,0.707106781186547,1.,0.707106781186547,1.,
0.707106781186547,1.),(1.,0.707106781186548,1.,0.707106781186548,1.,0.707106781186548,
1.,0.707106781186548,1.),(1.,0.707106781186547,1.,0.707106781186547,1.,
0.707106781186547,1.,0.707106781186547,1.),(1.,0.707106781186548,1.,0.707106781186548,
1.,0.707106781186548,1.,0.707106781186548,1.),(1.,0.707106781186547,1.,
0.707106781186547,1.,0.707106781186547,1.,0.707106781186547,1.),(1.,0.707106781186547,
1.,0.707106781186547,1.,0.707106781186547,1.,0.707106781186547,1.),(1.,
0.707106781186548,1.,0.707106781186548,1.,0.707106781186548,1.,0.707106781186548,
1.),(1.,0.707106781186547,1.,0.707106781186547,1.,0.707106781186547,1.,
0.707106781186547,1.),(1.,0.707106781186548,1.,0.707106781186548,1.,0.707106781186548,
1.,0.707106781186548,1.),(1.,0.707106781186547,1.,0.707106781186547,1.,
0.707106781186547,1.,0.707106781186547,1.),(1.,0.707106781186548,1.,0.707106781186548,
1.,0.707106781186548,1.,0.707106781186548,1.),(1.,0.707106781186548,1.,
0.707106781186548,1.,0.707106781186548,1.,0.707106781186548,1.),(1.,0.707106781186547,
1.,0.707106781186547,1.,0.707106781186547,1.,0.707106781186547,1.),(1.,
0.707106781186548,1.,0.707106781186548,1.,0.707106781186548,1.,0.707106781186548,
1.),(1.,0.707106781186547,1.,0.707106781186547,1.,0.707106781186547,1.,
0.707106781186547,1.),(1.,0.707106781186548,1.,0.707106781186548,1.,0.707106781186548,
1.,0.707106781186548,1.),(1.,0.707106781186548,1.,0.707106781186548,1.,
0.707106781186548,1.,0.707106781186548,1.),(1.,0.707106781186547,1.,0.707106781186547,
1.,0.707106781186547,1.,0.707106781186547,1.),(1.,0.707106781186548,1.,
0.707106781186548,1.,0.707106781186548,1.,0.707106781186548,1.),(1.,0.707106781186547,
1.,0.707106781186547,1.,0.707106781186547,1.,0.707106781186547,1.),(1.,
0.707106781186547,1.,0.707106781186547,1.,0.707106781186547,1.,0.707106781186547,
1.),(1.,0.707106781186548,1.,0.707106781186548,1.,0.707106781186548,1.,
0.707106781186548,1.),(1.,0.707106781186547,1.,0.707106781186547,1.,0.707106781186547,
1.,0.707106781186547,1.),(1.,0.707106781186548,1.,0.707106781186548,1.,
0.707106781186548,1.,0.707106781186548,1.),(1.,0.707106781186547,1.,0.707106781186547,
1.,0.707106781186547,1.,0.707106781186547,1.),(1.,0.707106781186548,1.,
0.707106781186548,1.,0.707106781186548,1.,0.707106781186548,1.),(1.,0.707106781186547,
1.,0.707106781186547,1.,0.707106781186547,1.,0.707106781186547,1.),(1.,
0.707106781186547,1.,0.707106781186547,1.,0.707106781186547,1.,0.707106781186547,
1.),(1.,0.707106781186548,1.,0.707106781186548,1.,0.707106781186548,1.,
0.707106781186548,1.),(1.,0.707106781186548,1.,0.707106781186548,1.,0.707106781186548,
1.,0.707106781186548,1.),(1.,0.707106781186548,1.,0.707106781186548,1.,
0.707106781186548,1.,0.707106781186548,1.),(1.,0.707106781186548,1.,0.707106781186548,
1.,0.707106781186548,1.,0.707106781186548,1.),(1.,0.707106781186547,1.,
0.707106781186547,1.,0.707106781186547,1.,0.707106781186547,1.),(1.,0.707106781186548,
1.,0.707106781186548,1.,0.707106781186548,1.,0.707106781186548,1.),(1.,
0.707106781186548,1.,0.707106781186548,1.,0.707106781186548,1.,0.707106781186548,
1.),(1.,0.707106781186548,1.,0.707106781186548,1.,0.707106781186548,1.,
0.707106781186548,1.),(1.,0.707106781186547,1.,0.707106781186547,1.,0.707106781186547,
1.,0.707106781186547,1.),(1.,0.707106781186548,1.,0.707106781186548,1.,
0.707106781186548,1.,0.707106781186548,1.),(1.,0.707106781186548,1.,0.707106781186548,
1.,0.707106781186548,1.,0.707106781186548,1.),(1.,0.707106781186548,1.,
0.707106781186548,1.,0.707106781186548,1.,0.707106781186548,1.),(1.,0.707106781186547,
1.,0.707106781186547,1.,0.707106781186547,1.,0.707106781186547,1.),(1.,
0.707106781186547,1.,0.707106781186547,1.,0.707106781186547,1.,0.707106781186547,
1.),(1.,0.707106781186548,1.,0.707106781186548,1.,0.707106781186548,1.,
0.707106781186548,1.),(1.,0.707106781186547,1.,0.707106781186547,1.,0.707106781186547,
1.,0.707106781186547,1.),(1.,0.707106781186548,1.,0.707106781186548,1.,
0.707106781186548,1.,0.707106781186548,1.),(1.,0.707106781186547,1.,0.707106781186547,
1.,0.707106781186547,1.,0.707106781186547,1.),(1.,0.707106781186548,1.,
0.707106781186548,1.,0.707106781186548,1.,0.707106781186548,1.),(1.,0.707106781186548,
1.,0.707106781186548,1.,0.707106781186548,1.,0.707106781186548,1.),(1.,
0.707106781186547,1.,0.707106781186547,1.,0.707106781186547,1.,0.707106781186547,
1.),(1.,0.707106781186547,1.,0.707106781186547,1.,0.707106781186547,1.,
0.707106781186547,1.),(1.,0.707106781186548,1.,0.707106781186548,1.,0.707106781186548,
1.,0.707106781186548,1.),(1.,0.707106781186547,1.,0.707106781186547,1.,
0.707106781186547,1.,0.707106781186547,1.),(1.,0.707106781186548,1.,0.707106781186548,
1.,0.707106781186548,1.,0.707106781186548,1.),(1.,0.707106781186547,1.,
0.707106781186547,1.,0.707106781186547,1.,0.707106781186547,1.),(1.,0.707106781186548,
1.,0.707106781186548,1.,0.707106781186548,1.,0.707106781186548,1.),(1.,
0.707106781186548,1.,0.707106781186548,1.,0.707106781186548,1.,0.707106781186548,
1.),(1.,0.707106781186547,1.,0.707106781186547,1.,0.707106781186547,1.,
0.707106781186547,1.),(1.,0.707106781186547,1.,0.707106781186547,1.,0.707106781186547,
1.,0.707106781186547,1.),(1.,0.707106781186547,1.,0.707106781186547,1.,
0.707106781186547,1.,0.707106781186547,1.),(1.,0.707106781186548,1.,0.707106781186548,
1.,0.707106781186548,1.,0.707106781186548,1.),(1.,0.707106781186548,1.,
0.707106781186548,1.,0.707106781186548,1.,0.707106781186548,1.),(1.,0.707106781186547,
1.,0.707106781186547,1.,0.707106781186547,1.,0.707106781186547,1.),(1.,
0.707106781186547,1.,0.707106781186547,1.,0.707106781186547,1.,0.707106781186547,
1.),(1.,0.707106781186548,1.,0.707106781186548,1.,0.707106781186548,1.,
0.707106781186548,1.),(1.,0.707106781186548,1.,0.707106781186548,1.,0.707106781186548,
1.,0.707106781186548,1.),(1.,0.707106781186548,1.,0.707106781186548,1.,
0.707106781186548,1.,0.707106781186548,1.),(1.,0.707106781186548,1.,0.707106781186548,
1.,0.707106781186548,1.,0.707106781186548,1.),(1.,0.707106781186547,1.,
0.707106781186547,1.,0.707106781186547,1.,0.707106781186547,1.),(1.,0.707106781186547,
1.,0.707106781186547,1.,0.707106781186547,1.,0.707106781186547,1.),(1.,
0.707106781186548,1.,0.707106781186548,1.,0.707106781186548,1.,0.707106781186548,
1.),(1.,0.707106781186548,1.,0.707106781186548,1.,0.707106781186548,1.,
0.707106781186548,1.),(1.,0.707106781186547,1.,0.707106781186547,1.,0.707106781186547,
1.,0.707106781186547,1.),(1.,0.707106781186548,1.,0.707106781186548,1.,
0.707106781186548,1.,0.707106781186548,1.),(1.,0.707106781186547,1.,0.707106781186547,
1.,0.707106781186547,1.,0.707106781186547,1.),(1.,0.707106781186548,1.,
0.707106781186548,1.,0.707106781186548,1.,0.707106781186548,1.),(1.,0.707106781186547,
1.,0.707106781186547,1.,0.707106781186547,1.,0.707106781186547,1.),(1.,
0.707106781186548,1.,0.707106781186548,1.,0.707106781186548,1.,0.707106781186548,
1.),(1.,0.707106781186547,1.,0.707106781186547,1.,0.707106781186547,1.,
0.707106781186547,1.),(1.,0.707106781186547,1.,0.707106781186547,1.,0.707106781186547,
1.,0.707106781186547,1.),(1.,0.707106781186548,1.,0.707106781186548,1.,
0.707106781186548,1.,0.707106781186548,1.),(1.,0.707106781186547,1.,0.707106781186547,
1.,0.707106781186547,1.,0.707106781186547,1.),(1.,0.707106781186547,1.,
0.707106781186547,1.,0.707106781186547,1.,0.707106781186547,1.),(1.,0.707106781186548,
1.,0.707106781186548,1.,0.707106781186548,1.,0.707106781186548,1.),(1.,
0.707106781186547,1.,0.707106781186547,1.,0.707106781186547,1.,0.707106781186547,
1.),(1.,0.707106781186548,1.,0.707106781186548,1.,0.707106781186548,1.,
0.707106781186548,1.),(1.,0.707106781186547,1.,0.707106781186547,1.,0.707106781186547,
1.,0.707106781186547,1.),(1.,0.707106781186548,1.,0.707106781186548,1.,
0.707106781186548,1.,0.707106781186548,1.),(1.,0.707106781186547,1.,0.707106781186547,
1.,0.707106781186547,1.,0.707106781186547,1.),(1.,0.707106781186548,1.,
0.707106781186548,1.,0.707106781186548,1.,0.707106781186548,1.),(1.,0.707106781186547,
1.,0.707106781186547,1.,0.707106781186547,1.,0.707106781186547,1.),(1.,
0.707106781186548,1.,0.707106781186548,1.,0.707106781186548,1.,0.707106781186548,
1.),(1.,0.707106781186547,1.,0.707106781186547,1.,0.707106781186547,1.,
0.707106781186547,1.),(1.,0.707106781186548,1.,0.707106781186548,1.,0.707106781186548,
1.,0.707106781186548,1.),(1.,0.707106781186547,1.,0.707106781186547,1.,
0.707106781186547,1.,0.707106781186547,1.),(1.,0.707106781186547,1.,0.707106781186547,
1.,0.707106781186547,1.,0.707106781186547,1.),(1.,0.707106781186548,1.,
0.707106781186548,1.,0.707106781186548,1.,0.707106781186548,1.),(1.,0.707106781186548,
1.,0.707106781186548,1.,0.707106781186548,1.,0.707106781186548,1.),(1.,
0.707106781186547,1.,0.707106781186547,1.,0.707106781186547,1.,0.707106781186547,
1.),(1.,0.707106781186547,1.,0.707106781186547,1.,0.707106781186547,1.,
0.707106781186547,1.),(1.,0.707106781186547,1.,0.707106781186547,1.,0.707106781186547,
1.,0.707106781186547,1.),(1.,0.707106781186548,1.,0.707106781186548,1.,
0.707106781186548,1.,0.707106781186548,1.),(1.,0.707106781186547,1.,0.707106781186547,
1.,0.707106781186547,1.,0.707106781186547,1.),(1.,0.707106781186548,1.,
0.707106781186548,1.,0.707106781186548,1.,0.707106781186548,1.),(1.,0.707106781186547,
1.,0.707106781186547,1.,0.707106781186547,1.,0.707106781186547,1.),(1.,
0.707106781186548,1.,0.707106781186548,1.,0.707106781186548,1.,0.707106781186548,
1.),(1.,0.707106781186547,1.,0.707106781186547,1.,0.707106781186547,1.,
0.707106781186547,1.),(1.,0.707106781186548,1.,0.707106781186548,1.,0.707106781186548,
1.,0.707106781186548,1.),(1.,0.707106781186547,1.,0.707106781186547,1.,
0.707106781186547,1.,0.707106781186547,1.),(1.,0.707106781186547,1.,0.707106781186547,
1.,0.707106781186547,1.,0.707106781186547,1.),(1.,0.707106781186547,1.,
0.707106781186547,1.,0.707106781186547,1.,0.707106781186547,1.),(1.,0.707106781186548,
1.,0.707106781186548,1.,0.707106781186548,1.,0.707106781186548,1.),(1.,
0.707106781186547,1.,0.707106781186547,1.,0.707106781186547,1.,0.707106781186547,
1.),(1.,0.707106781186548,1.,0.707106781186548,1.,0.707106781186548,1.,
0.707106781186548,1.),(1.,0.707106781186548,1.,0.707106781186548,1.,0.707106781186548,
1.,0.707106781186548,1.),(1.,0.707106781186547,1.,0.707106781186547,1.,
0.707106781186547,1.,0.707106781186547,1.),(1.,0.707106781186548,1.,0.707106781186548,
1.,0.707106781186548,1.,0.707106781186548,1.),(1.,0.707106781186547,1.,
0.707106781186547,1.,0.707106781186547,1.,0.707106781186547,1.),(1.,0.707106781186547,
1.,0.707106781186547,1.,0.707106781186547,1.,0.707106781186547,1.),(1.,
0.707106781186548,1.,0.707106781186548,1.,0.707106781186548,1.,0.707106781186548,
1.),(1.,0.707106781186547,1.,0.707106781186547,1.,0.707106781186547,1.,
0.707106781186547,1.),(1.,0.707106781186547,1.,0.707106781186547,1.,0.707106781186547,
1.,0.707106781186547,1.),(1.,0.707106781186548,1.,0.707106781186548,1.,
0.707106781186548,1.,0.707106781186548,1.),(1.,0.707106781186547,1.,0.707106781186547,
1.,0.707106781186547,1.,0.707106781186547,1.),(1.,0.707106781186547,1.,
0.707106781186547,1.,0.707106781186547,1.,0.707106781186547,1.),(1.,0.707106781186547,
1.,0.707106781186547,1.,0.707106781186547,1.,0.707106781186547,1.),(1.,
0.707106781186547,1.,0.707106781186547,1.,0.707106781186547,1.,0.707106781186547,
1.),(1.,0.707106781186548,1.,0.707106781186548,1.,0.707106781186548,1.,
0.707106781186548,1.),(1.,0.707106781186547,1.,0.707106781186547,1.,0.707106781186547,
1.,0.707106781186547,1.),(1.,0.707106781186547,1.,0.707106781186547,1.,
0.707106781186547,1.,0.707106781186547,1.),(1.,0.707106781186547,1.,0.707106781186547,
1.,0.707106781186547,1.,0.707106781186547,1.),(1.,0.707106781186548,1.,
0.707106781186548,1.,0.707106781186548,1.,0.707106781186548,1.),(1.,0.707106781186547,
1.,0.707106781186547,1.,0.707106781186547,1.,0.707106781186547,1.),(1.,
0.707106781186547,1.,0.707106781186547,1.,0.707106781186547,1.,0.707106781186547,
1.),(1.,0.707106781186548,1.,0.707106781186548,1.,0.707106781186548,1.,
0.707106781186548,1.),(1.,0.707106781186548,1.,0.707106781186548,1.,0.707106781186548,
1.,0.707106781186548,1.),(1.,0.707106781186547,1.,0.707106781186547,1.,
0.707106781186547,1.,0.707106781186547,1.),(1.,0.707106781186548,1.,0.707106781186548,
1.,0.707106781186548,1.,0.707106781186548,1.),(1.,0.707106781186548,1.,
0.707106781186548,1.,0.707106781186548,1.,0.707106781186548,1.),(1.,0.707106781186547,
1.,0.707106781186547,1.,0.707106781186547,1.,0.707106781186547,1.),(1.,
0.707106781186547,1.,0.707106781186547,1.,0.707106781186547,1.,0.707106781186547,
1.),(1.,0.707106781186548,1.,0.707106781186548,1.,0.707106781186548,1.,
0.707106781186548,1.),(1.,0.707106781186547,1.,0.707106781186547,1.,0.707106781186547,
1.,0.707106781186547,1.),(1.,0.707106781186547,1.,0.707106781186547,1.,
0.707106781186547,1.,0.707106781186547,1.),(1.,0.707106781186548,1.,0.707106781186548,
1.,0.707106781186548,1.,0.707106781186548,1.),(1.,0.707106781186547,1.,
0.707106781186547,1.,0.707106781186547,1.,0.707106781186547,1.),(1.,0.707106781186547,
1.,0.707106781186547,1.,0.707106781186547,1.,0.707106781186547,1.),(1.,
0.707106781186547,1.,0.707106781186547,1.,0.707106781186547,1.,0.707106781186547,
1.),(1.,0.707106781186548,1.,0.707106781186548,1.,0.707106781186548,1.,
0.707106781186548,1.),(1.,0.707106781186547,1.,0.707106781186547,1.,0.707106781186547,
1.,0.707106781186547,1.),(1.,0.707106781186548,1.,0.707106781186548,1.,
0.707106781186548,1.,0.707106781186548,1.),(1.,0.707106781186547,1.,0.707106781186547,
1.,0.707106781186547,1.,0.707106781186547,1.),(1.,0.707106781186548,1.,
0.707106781186548,1.,0.707106781186548,1.,0.707106781186548,1.),(1.,0.707106781186547,
1.,0.707106781186547,1.,0.707106781186547,1.,0.707106781186547,1.),(1.,
0.707106781186548,1.,0.707106781186548,1.,0.707106781186548,1.,0.707106781186548,
1.),(1.,0.707106781186547,1.,0.707106781186547,1.,0.707106781186547,1.,
0.707106781186547,1.),(1.,0.707106781186548,1.,0.707106781186548,1.,0.707106781186548,
1.,0.707106781186548,1.),(1.,0.707106781186547,1.,0.707106781186547,1.,
0.707106781186547,1.,0.707106781186547,1.),(1.,0.707106781186548,1.,0.707106781186548,
1.,0.707106781186548,1.,0.707106781186548,1.),(1.,0.707106781186548,1.,
0.707106781186548,1.,0.707106781186548,1.,0.707106781186548,1.),(1.,0.707106781186547,
1.,0.707106781186547,1.,0.707106781186547,1.,0.707106781186547,1.),(1.,
0.707106781186547,1.,0.707106781186547,1.,0.707106781186547,1.,0.707106781186547,
1.),(1.,0.707106781186548,1.,0.707106781186548,1.,0.707106781186548,1.,
0.707106781186548,1.),(1.,0.707106781186547,1.,0.707106781186547,1.,0.707106781186547,
1.,0.707106781186547,1.),(1.,0.707106781186548,1.,0.707106781186548,1.,
0.707106781186548,1.,0.707106781186548,1.),(1.,0.707106781186547,1.,0.707106781186547,
1.,0.707106781186547,1.,0.707106781186547,1.),(1.,0.707106781186548,1.,
0.707106781186548,1.,0.707106781186548,1.,0.707106781186548,1.),(1.,0.707106781186548,
1.,0.707106781186548,1.,0.707106781186548,1.,0.707106781186548,1.),(1.,
0.707106781186547,1.,0.707106781186547,1.,0.707106781186547,1.,0.707106781186547,
1.),(1.,0.707106781186548,1.,0.707106781186548,1.,0.707106781186548,1.,
0.707106781186548,1.),(1.,0.707106781186547,1.,0.707106781186547,1.,0.707106781186547,
1.,0.707106781186547,1.),(1.,0.707106781186548,1.,0.707106781186548,1.,
0.707106781186548,1.,0.707106781186548,1.),(1.,0.707106781186548,1.,0.707106781186548,
1.,0.707106781186548,1.,0.707106781186548,1.),(1.,0.707106781186547,1.,
0.707106781186547,1.,0.707106781186547,1.,0.707106781186547,1.),(1.,0.707106781186547,
1.,0.707106781186547,1.,0.707106781186547,1.,0.707106781186547,1.),(1.,
0.707106781186548,1.,0.707106781186548,1.,0.707106781186548,1.,0.707106781186548,
1.),(1.,0.707106781186547,1.,0.707106781186547,1.,0.707106781186547,1.,
0.707106781186547,1.),(1.,0.707106781186548,1.,0.707106781186548,1.,0.707106781186548,
1.,0.707106781186548,1.),(1.,0.707106781186547,1.,0.707106781186547,1.,
0.707106781186547,1.,0.707106781186547,1.),(1.,0.707106781186548,1.,0.707106781186548,
1.,0.707106781186548,1.,0.707106781186548,1.),(1.,0.707106781186547,1.,
0.707106781186547,1.,0.707106781186547,1.,0.707106781186547,1.),(1.,0.707106781186548,
1.,0.707106781186548,1.,0.707106781186548,1.,0.707106781186548,1.),(1.,
0.707106781186547,1.,0.707106781186547,1.,0.707106781186547,1.,0.707106781186547,
1.),(1.,0.707106781186547,1.,0.707106781186547,1.,0.707106781186547,1.,
0.707106781186547,1.),(1.,0.707106781186547,1.,0.707106781186547,1.,0.707106781186547,
1.,0.707106781186547,1.),(1.,0.707106781186547,1.,0.707106781186547,1.,
0.707106781186547,1.,0.707106781186547,1.),(1.,0.707106781186547,1.,0.707106781186547,
1.,0.707106781186547,1.,0.707106781186547,1.),(1.,0.707106781186547,1.,
0.707106781186547,1.,0.707106781186547,1.,0.707106781186547,1.),(1.,0.707106781186547,
1.,0.707106781186547,1.,0.707106781186547,1.,0.707106781186547,1.),(1.,
0.707106781186547,1.,0.707106781186547,1.,0.707106781186547,1.,0.707106781186547,
1.),(1.,0.707106781186548,1.,0.707106781186548,1.,0.707106781186548,1.,
0.707106781186548,1.),(1.,0.707106781186547,1.,0.707106781186547,1.,0.707106781186547,
1.,0.707106781186547,1.),(1.,0.707106781186548,1.,0.707106781186548,1.,
0.707106781186548,1.,0.707106781186548,1.),(1.,0.707106781186547,1.,0.707106781186547,
1.,0.707106781186547,1.,0.707106781186547,1.),(1.,0.707106781186547,1.,
0.707106781186547,1.,0.707106781186547,1.,0.707106781186547,1.),(1.,0.707106781186548,
1.,0.707106781186548,1.,0.707106781186548,1.,0.707106781186548,1.),(1.,
0.707106781186547,1.,0.707106781186547,1.,0.707106781186547,1.,0.707106781186547,
1.),(1.,0.707106781186548,1.,0.707106781186548,1.,0.707106781186548,1.,
0.707106781186548,1.),(1.,0.707106781186547,1.,0.707106781186547,1.,0.707106781186547,
1.,0.707106781186547,1.),(1.,0.707106781186547,1.,0.707106781186547,1.,
0.707106781186547,1.,0.707106781186547,1.),(1.,0.707106781186548,1.,0.707106781186548,
1.,0.707106781186548,1.,0.707106781186548,1.),(1.,0.707106781186547,1.,
0.707106781186547,1.,0.707106781186547,1.,0.707106781186547,1.),(1.,0.707106781186548,
1.,0.707106781186548,1.,0.707106781186548,1.,0.707106781186548,1.),(1.,
0.707106781186547,1.,0.707106781186547,1.,0.707106781186547,1.,0.707106781186547,
1.),(1.,0.707106781186548,1.,0.707106781186548,1.,0.707106781186548,1.,
0.707106781186548,1.),(1.,0.707106781186547,1.,0.707106781186547,1.,0.707106781186547,
1.,0.707106781186547,1.),(1.,0.707106781186548,1.,0.707106781186548,1.,
0.707106781186548,1.,0.707106781186548,1.),(1.,0.707106781186547,1.,0.707106781186547,
1.,0.707106781186547,1.,0.707106781186547,1.),(1.,0.707106781186548,1.,
0.707106781186548,1.,0.707106781186548,1.,0.707106781186548,1.),(1.,0.707106781186547,
1.,0.707106781186547,1.,0.707106781186547,1.,0.707106781186547,1.),(1.,
0.707106781186548,1.,0.707106781186548,1.,0.707106781186548,1.,0.707106781186548,
1.),(1.,0.707106781186547,1.,0.707106781186547,1.,0.707106781186547,1.,
0.707106781186547,1.),(1.,0.707106781186548,1.,0.707106781186548,1.,0.707106781186548,
1.,0.707106781186548,1.),(1.,0.707106781186548,1.,0.707106781186548,1.,
0.707106781186548,1.,0.707106781186548,1.),(1.,0.707106781186547,1.,0.707106781186547,
1.,0.707106781186547,1.,0.707106781186547,1.),(1.,0.707106781186548,1.,
0.707106781186548,1.,0.707106781186548,1.,0.707106781186548,1.),(1.,0.707106781186547,
1.,0.707106781186547,1.,0.707106781186547,1.,0.707106781186547,1.),(1.,
0.707106781186547,1.,0.707106781186547,1.,0.707106781186547,1.,0.707106781186547,
1.),(1.,0.707106781186547,1.,0.707106781186547,1.,0.707106781186547,1.,
0.707106781186547,1.),(1.,0.707106781186548,1.,0.707106781186548,1.,0.707106781186548,
1.,0.707106781186548,1.),(1.,0.707106781186547,1.,0.707106781186547,1.,
0.707106781186547,1.,0.707106781186547,1.),(1.,0.707106781186547,1.,0.707106781186547,
1.,0.707106781186547,1.,0.707106781186547,1.),(1.,0.707106781186547,1.,
0.707106781186547,1.,0.707106781186547,1.,0.707106781186547,1.),(1.,0.707106781186548,
1.,0.707106781186548,1.,0.707106781186548,1.,0.707106781186548,1.),(1.,
0.707106781186547,1.,0.707106781186547,1.,0.707106781186547,1.,0.707106781186547,
1.),(1.,0.707106781186547,1.,0.707106781186547,1.,0.707106781186547,1.,
0.707106781186547,1.),(1.,0.707106781186548,1.,0.707106781186548,1.,0.707106781186548,
1.,0.707106781186548,1.),(1.,0.707106781186547,1.,0.707106781186547,1.,
0.707106781186547,1.,0.707106781186547,1.),(1.,0.707106781186547,1.,0.707106781186547,
1.,0.707106781186547,1.,0.707106781186547,1.),(1.,0.707106781186547,1.,
0.707106781186547,1.,0.707106781186547,1.,0.707106781186547,1.),(1.,0.707106781186547,
1.,0.707106781186547,1.,0.707106781186547,1.,0.707106781186547,1.),(1.,
0.707106781186548,1.,0.707106781186548,1.,0.707106781186548,1.,0.707106781186548,
1.),(1.,0.707106781186547,1.,0.707106781186547,1.,0.707106781186547,1.,
0.707106781186547,1.),(1.,0.707106781186547,1.,0.707106781186547,1.,0.707106781186547,
1.,0.707106781186547,1.),(1.,0.707106781186547,1.,0.707106781186547,1.,
0.707106781186547,1.,0.707106781186547,1.),(1.,0.707106781186548,1.,0.707106781186548,
1.,0.707106781186548,1.,0.707106781186548,1.),(1.,0.707106781186548,1.,
0.707106781186548,1.,0.707106781186548,1.,0.707106781186548,1.),(1.,0.707106781186548,
1.,0.707106781186548,1.,0.707106781186548,1.,0.707106781186548,1.),(1.,
0.707106781186548,1.,0.707106781186548,1.,0.707106781186548,1.,0.707106781186548,
1.),(1.,0.707106781186547,1.,0.707106781186547,1.,0.707106781186547,1.,
0.707106781186547,1.),(1.,0.707106781186548,1.,0.707106781186548,1.,0.707106781186548,
1.,0.707106781186548,1.),(1.,0.707106781186547,1.,0.707106781186547,1.,
0.707106781186547,1.,0.707106781186547,1.),(1.,0.707106781186547,1.,0.707106781186547,
1.,0.707106781186547,1.,0.707106781186547,1.),(1.,0.707106781186548,1.,
0.707106781186548,1.,0.707106781186548,1.,0.707106781186548,1.),(1.,0.707106781186547,
1.,0.707106781186547,1.,0.707106781186547,1.,0.707106781186547,1.),(1.,
0.707106781186548,1.,0.707106781186548,1.,0.707106781186548,1.,0.707106781186548,
1.),(1.,0.707106781186547,1.,0.707106781186547,1.,0.707106781186547,1.,
0.707106781186547,1.),(1.,0.707106781186547,1.,0.707106781186547,1.,0.707106781186547,
1.,0.707106781186547,1.),(1.,0.707106781186548,1.,0.707106781186548,1.,
0.707106781186548,1.,0.707106781186548,1.),(1.,0.707106781186547,1.,0.707106781186547,
1.,0.707106781186547,1.,0.707106781186547,1.),(1.,0.707106781186547,1.,
0.707106781186547,1.,0.707106781186547,1.,0.707106781186547,1.),(1.,0.707106781186547,
1.,0.707106781186547,1.,0.707106781186547,1.,0.707106781186547,1.),(1.,
0.707106781186547,1.,0.707106781186547,1.,0.707106781186547,1.,0.707106781186547,
1.),(1.,0.707106781186548,1.,0.707106781186548,1.,0.707106781186548,1.,
0.707106781186548,1.),(1.,0.707106781186548,1.,0.707106781186548,1.,0.707106781186548,
1.,0.707106781186548,1.),(1.,0.707106781186547,1.,0.707106781186547,1.,
0.707106781186547,1.,0.707106781186547,1.),(1.,0.707106781186547,1.,0.707106781186547,
1.,0.707106781186547,1.,0.707106781186547,1.),(1.,0.707106781186548,1.,
0.707106781186548,1.,0.707106781186548,1.,0.707106781186548,1.),(1.,0.707106781186547,
1.,0.707106781186547,1.,0.707106781186547,1.,0.707106781186547,1.),(1.,
0.707106781186548,1.,0.707106781186548,1.,0.707106781186548,1.,0.707106781186548,
1.),(1.,0.707106781186547,1.,0.707106781186547,1.,0.707106781186547,1.,
0.707106781186547,1.),(1.,0.707106781186548,1.,0.707106781186548,1.,0.707106781186548,
1.,0.707106781186548,1.),(1.,0.707106781186548,1.,0.707106781186548,1.,
0.707106781186548,1.,0.707106781186548,1.),(1.,0.707106781186547,1.,0.707106781186547,
1.,0.707106781186547,1.,0.707106781186547,1.),(1.,0.707106781186547,1.,
0.707106781186547,1.,0.707106781186547,1.,0.707106781186547,1.),(1.,0.707106781186548,
1.,0.707106781186548,1.,0.707106781186548,1.,0.707106781186548,1.),(1.,
0.707106781186548,1.,0.707106781186548,1.,0.707106781186548,1.,0.707106781186548,
1.),(1.,0.707106781186547,1.,0.707106781186547,1.,0.707106781186547,1.,
0.707106781186547,1.),(1.,0.707106781186548,1.,0.707106781186548,1.,0.707106781186548,
1.,0.707106781186548,1.),(1.,0.707106781186548,1.,0.707106781186548,1.,
0.707106781186548,1.,0.707106781186548,1.),(1.,0.707106781186547,1.,0.707106781186547,
1.,0.707106781186547,1.,0.707106781186547,1.),(1.,0.707106781186548,1.,
0.707106781186548,1.,0.707106781186548,1.,0.707106781186548,1.),(1.,0.707106781186548,
1.,0.707106781186548,1.,0.707106781186548,1.,0.707106781186548,1.),(1.,
0.707106781186548,1.,0.707106781186548,1.,0.707106781186548,1.,0.707106781186548,
1.),(1.,0.707106781186547,1.,0.707106781186547,1.,0.707106781186547,1.,
0.707106781186547,1.),(1.,0.707106781186548,1.,0.707106781186548,1.,0.707106781186548,
1.,0.707106781186548,1.),(1.,0.707106781186547,1.,0.707106781186547,1.,
0.707106781186547,1.,0.707106781186547,1.),(1.,0.707106781186548,1.,0.707106781186548,
1.,0.707106781186548,1.,0.707106781186548,1.),(1.,0.707106781186547,1.,
0.707106781186547,1.,0.707106781186547,1.,0.707106781186547,1.),(1.,0.707106781186548,
1.,0.707106781186548,1.,0.707106781186548,1.,0.707106781186548,1.),(1.,
0.707106781186547,1.,0.707106781186547,1.,0.707106781186547,1.,0.707106781186547,
1.),(1.,0.707106781186548,1.,0.707106781186548,1.,0.707106781186548,1.,
0.707106781186548,1.),(1.,0.707106781186547,1.,0.707106781186547,1.,0.707106781186547,
1.,0.707106781186547,1.),(1.,0.707106781186548,1.,0.707106781186548,1.,
0.707106781186548,1.,0.707106781186548,1.),(1.,0.707106781186548,1.,0.707106781186548,
1.,0.707106781186548,1.,0.707106781186548,1.),(1.,0.707106781186547,1.,
0.707106781186547,1.,0.707106781186547,1.,0.707106781186547,1.),(1.,0.707106781186547,
1.,0.707106781186547,1.,0.707106781186547,1.,0.707106781186547,1.),(1.,
0.707106781186548,1.,0.707106781186548,1.,0.707106781186548,1.,0.707106781186548,
1.),(1.,0.707106781186547,1.,0.707106781186547,1.,0.707106781186547,1.,
0.707106781186547,1.),(1.,0.707106781186548,1.,0.707106781186548,1.,0.707106781186548,
1.,0.707106781186548,1.),(1.,0.707106781186547,1.,0.707106781186547,1.,
0.707106781186547,1.,0.707106781186547,1.),(1.,0.707106781186548,1.,0.707106781186548,
1.,0.707106781186548,1.,0.707106781186548,1.),(1.,0.707106781186548,1.,
0.707106781186548,1.,0.707106781186548,1.,0.707106781186548,1.),(1.,0.707106781186548,
1.,0.707106781186548,1.,0.707106781186548,1.,0.707106781186548,1.),(1.,
0.707106781186548,1.,0.707106781186548,1.,0.707106781186548,1.,0.707106781186548,
1.),(1.,0.707106781186548,1.,0.707106781186548,1.,0.707106781186548,1.,
0.707106781186548,1.),(1.,0.707106781186547,1.,0.707106781186547,1.,0.707106781186547,
1.,0.707106781186547,1.),(1.,0.707106781186547,1.,0.707106781186547,1.,
0.707106781186547,1.,0.707106781186547,1.),(1.,0.707106781186547,1.,0.707106781186547,
1.,0.707106781186547,1.,0.707106781186547,1.),(1.,0.707106781186547,1.,
0.707106781186547,1.,0.707106781186547,1.,0.707106781186547,1.),(1.,0.707106781186548,
1.,0.707106781186548,1.,0.707106781186548,1.,0.707106781186548,1.),(1.,
0.707106781186547,1.,0.707106781186547,1.,0.707106781186547,1.,0.707106781186547,
1.),(1.,0.707106781186548,1.,0.707106781186548,1.,0.707106781186548,1.,
0.707106781186548,1.),(1.,0.707106781186547,1.,0.707106781186547,1.,0.707106781186547,
1.,0.707106781186547,1.),(1.,0.707106781186547,1.,0.707106781186547,1.,
0.707106781186547,1.,0.707106781186547,1.),(1.,0.707106781186548,1.,0.707106781186548,
1.,0.707106781186548,1.,0.707106781186548,1.),(1.,0.707106781186548,1.,
0.707106781186548,1.,0.707106781186548,1.,0.707106781186548,1.),(1.,0.707106781186547,
1.,0.707106781186547,1.,0.707106781186547,1.,0.707106781186547,1.),(1.,
0.707106781186548,1.,0.707106781186548,1.,0.707106781186548,1.,0.707106781186548,
1.),(1.,0.707106781186547,1.,0.707106781186547,1.,0.707106781186547,1.,
0.707106781186547,1.),(1.,0.707106781186548,1.,0.707106781186548,1.,0.707106781186548,
1.,0.707106781186548,1.),(1.,0.707106781186548,1.,0.707106781186548,1.,
0.707106781186548,1.,0.707106781186548,1.),(1.,0.707106781186547,1.,0.707106781186547,
1.,0.707106781186547,1.,0.707106781186547,1.),(1.,0.707106781186547,1.,
0.707106781186547,1.,0.707106781186547,1.,0.707106781186547,1.),(1.,0.707106781186548,
1.,0.707106781186548,1.,0.707106781186548,1.,0.707106781186548,1.),(1.,
0.707106781186547,1.,0.707106781186547,1.,0.707106781186547,1.,0.707106781186547,
1.),(1.,0.707106781186548,1.,0.707106781186548,1.,0.707106781186548,1.,
0.707106781186548,1.),(1.,0.707106781186547,1.,0.707106781186547,1.,0.707106781186547,
1.,0.707106781186547,1.),(1.,0.707106781186548,1.,0.707106781186548,1.,
0.707106781186548,1.,0.707106781186548,1.),(1.,0.707106781186547,1.,0.707106781186547,
1.,0.707106781186547,1.,0.707106781186547,1.),(1.,0.707106781186548,1.,
0.707106781186548,1.,0.707106781186548,1.,0.707106781186548,1.),(1.,0.707106781186547,
1.,0.707106781186547,1.,0.707106781186547,1.,0.707106781186547,1.),(1.,
0.707106781186548,1.,0.707106781186548,1.,0.707106781186548,1.,0.707106781186548,
1.),(1.,0.707106781186547,1.,0.707106781186547,1.,0.707106781186547,1.,
0.707106781186547,1.),(1.,0.707106781186548,1.,0.707106781186548,1.,0.707106781186548,
1.,0.707106781186548,1.),(1.,0.707106781186547,1.,0.707106781186547,1.,
0.707106781186547,1.,0.707106781186547,1.),(1.,0.707106781186548,1.,0.707106781186548,
1.,0.707106781186548,1.,0.707106781186548,1.),(1.,0.707106781186548,1.,
0.707106781186548,1.,0.707106781186548,1.,0.707106781186548,1.),(1.,0.707106781186547,
1.,0.707106781186547,1.,0.707106781186547,1.,0.707106781186547,1.),(1.,
0.707106781186548,1.,0.707106781186548,1.,0.707106781186548,1.,0.707106781186548,
1.),(1.,0.707106781186547,1.,0.707106781186547,1.,0.707106781186547,1.,
0.707106781186547,1.),(1.,0.707106781186548,1.,0.707106781186548,1.,0.707106781186548,
1.,0.707106781186548,1.),(1.,0.707106781186547,1.,0.707106781186547,1.,
0.707106781186547,1.,0.707106781186547,1.),(1.,0.707106781186548,1.,0.707106781186548,
1.,0.707106781186548,1.,0.707106781186548,1.),(1.,0.707106781186548,1.,
0.707106781186548,1.,0.707106781186548,1.,0.707106781186548,1.),(1.,0.707106781186548,
1.,0.707106781186548,1.,0.707106781186548,1.,0.707106781186548,1.),(1.,
0.707106781186547,1.,0.707106781186547,1.,0.707106781186547,1.,0.707106781186547,
1.),(1.,0.707106781186547,1.,0.707106781186547,1.,0.707106781186547,1.,
0.707106781186547,1.),(1.,0.707106781186548,1.,0.707106781186548,1.,0.707106781186548,
1.,0.707106781186548,1.),(1.,0.707106781186548,1.,0.707106781186548,1.,
0.707106781186548,1.,0.707106781186548,1.),(1.,0.707106781186547,1.,0.707106781186547,
1.,0.707106781186547,1.,0.707106781186547,1.),(1.,0.707106781186547,1.,
0.707106781186547,1.,0.707106781186547,1.,0.707106781186547,1.),(1.,0.707106781186547,
1.,0.707106781186547,1.,0.707106781186547,1.,0.707106781186547,1.),(1.,
0.707106781186548,1.,0.707106781186548,1.,0.707106781186548,1.,0.707106781186548,
1.),(1.,0.707106781186547,1.,0.707106781186547,1.,0.707106781186547,1.,
0.707106781186547,1.),(1.,0.707106781186548,1.,0.707106781186548,1.,0.707106781186548,
1.,0.707106781186548,1.),(1.,0.707106781186547,1.,0.707106781186547,1.,
0.707106781186547,1.,0.707106781186547,1.),(1.,0.707106781186548,1.,0.707106781186548,
1.,0.707106781186548,1.,0.707106781186548,1.),(1.,0.707106781186547,1.,
0.707106781186547,1.,0.707106781186547,1.,0.707106781186547,1.),(1.,0.707106781186547,
1.,0.707106781186547,1.,0.707106781186547,1.,0.707106781186547,1.),(1.,
0.707106781186547,1.,0.707106781186547,1.,0.707106781186547,1.,0.707106781186547,
1.),(1.,0.707106781186548,1.,0.707106781186548,1.,0.707106781186548,1.,
0.707106781186548,1.),(1.,0.707106781186547,1.,0.707106781186547,1.,0.707106781186547,
1.,0.707106781186547,1.),(1.,0.707106781186548,1.,0.707106781186548,1.,
0.707106781186548,1.,0.707106781186548,1.),(1.,0.707106781186547,1.,0.707106781186547,
1.,0.707106781186547,1.,0.707106781186547,1.),(1.,0.707106781186548,1.,
0.707106781186548,1.,0.707106781186548,1.,0.707106781186548,1.),(1.,0.707106781186547,
1.,0.707106781186547,1.,0.707106781186547,1.,0.707106781186547,1.),(1.,
0.707106781186548,1.,0.707106781186548,1.,0.707106781186548,1.,0.707106781186548,
1.),(1.,0.707106781186547,1.,0.707106781186547,1.,0.707106781186547,1.,
0.707106781186547,1.),(1.,0.707106781186547,1.,0.707106781186547,1.,0.707106781186547,
1.,0.707106781186547,1.),(1.,0.707106781186548,1.,0.707106781186548,1.,
0.707106781186548,1.,0.707106781186548,1.),(1.,0.707106781186547,1.,0.707106781186547,
1.,0.707106781186547,1.,0.707106781186547,1.),(1.,0.707106781186547,1.,
0.707106781186547,1.,0.707106781186547,1.,0.707106781186547,1.),(1.,0.707106781186548,
1.,0.707106781186548,1.,0.707106781186548,1.,0.707106781186548,1.),(1.,
0.707106781186547,1.,0.707106781186547,1.,0.707106781186547,1.,0.707106781186547,
1.),(1.,0.707106781186547,1.,0.707106781186547,1.,0.707106781186547,1.,
0.707106781186547,1.),(1.,0.707106781186548,1.,0.707106781186548,1.,0.707106781186548,
1.,0.707106781186548,1.),(1.,0.707106781186547,1.,0.707106781186547,1.,
0.707106781186547,1.,0.707106781186547,1.),(1.,0.707106781186547,1.,0.707106781186547,
1.,0.707106781186547,1.,0.707106781186547,1.),(1.,0.707106781186547,1.,
0.707106781186547,1.,0.707106781186547,1.,0.707106781186547,1.),(1.,0.707106781186548,
1.,0.707106781186548,1.,0.707106781186548,1.,0.707106781186548,1.),(1.,
0.707106781186547,1.,0.707106781186547,1.,0.707106781186547,1.,0.707106781186547,
1.),(1.,0.707106781186548,1.,0.707106781186548,1.,0.707106781186548,1.,
0.707106781186548,1.),(1.,0.707106781186547,1.,0.707106781186547,1.,0.707106781186547,
1.,0.707106781186547,1.),(1.,0.707106781186547,1.,0.707106781186547,1.,
0.707106781186547,1.,0.707106781186547,1.),(1.,0.707106781186547,1.,0.707106781186547,
1.,0.707106781186547,1.,0.707106781186547,1.),(1.,0.707106781186548,1.,
0.707106781186548,1.,0.707106781186548,1.,0.707106781186548,1.),(1.,0.707106781186548,
1.,0.707106781186548,1.,0.707106781186548,1.,0.707106781186548,1.),(1.,
0.707106781186547,1.,0.707106781186547,1.,0.707106781186547,1.,0.707106781186547,
1.),(1.,0.707106781186547,1.,0.707106781186547,1.,0.707106781186547,1.,
0.707106781186547,1.),(1.,0.707106781186548,1.,0.707106781186548,1.,0.707106781186548,
1.,0.707106781186548,1.),(1.,0.707106781186548,1.,0.707106781186548,1.,
0.707106781186548,1.,0.707106781186548,1.),(1.,0.707106781186548,1.,0.707106781186548,
1.,0.707106781186548,1.,0.707106781186548,1.),(1.,0.707106781186547,1.,
0.707106781186547,1.,0.707106781186547,1.,0.707106781186547,1.),(1.,0.707106781186548,
1.,0.707106781186548,1.,0.707106781186548,1.,0.707106781186548,1.),(1.,
0.707106781186547,1.,0.707106781186547,1.,0.707106781186547,1.,0.707106781186547,
1.),(1.,0.707106781186548,1.,0.707106781186548,1.,0.707106781186548,1.,
0.707106781186548,1.),(1.,0.707106781186547,1.,0.707106781186547,1.,0.707106781186547,
1.,0.707106781186547,1.),(1.,0.707106781186548,1.,0.707106781186548,1.,
0.707106781186548,1.,0.707106781186548,1.),(1.,0.707106781186547,1.,0.707106781186547,
1.,0.707106781186547,1.,0.707106781186547,1.),(1.,0.707106781186547,1.,
0.707106781186547,1.,0.707106781186547,1.,0.707106781186547,1.),(1.,0.707106781186547,
1.,0.707106781186547,1.,0.707106781186547,1.,0.707106781186547,1.),(1.,
0.707106781186547,1.,0.707106781186547,1.,0.707106781186547,1.,0.707106781186547,
1.),(1.,0.707106781186548,1.,0.707106781186548,1.,0.707106781186548,1.,
0.707106781186548,1.),(1.,0.707106781186547,1.,0.707106781186547,1.,0.707106781186547,
1.,0.707106781186547,1.),(1.,0.707106781186548,1.,0.707106781186548,1.,
0.707106781186548,1.,0.707106781186548,1.),(1.,0.707106781186548,1.,0.707106781186548,
1.,0.707106781186548,1.,0.707106781186548,1.),(1.,0.707106781186547,1.,
0.707106781186547,1.,0.707106781186547,1.,0.707106781186547,1.),(1.,0.707106781186548,
1.,0.707106781186548,1.,0.707106781186548,1.,0.707106781186548,1.),(1.,
0.707106781186547,1.,0.707106781186547,1.,0.707106781186547,1.,0.707106781186547,
1.),(1.,0.707106781186547,1.,0.707106781186547,1.,0.707106781186547,1.,
0.707106781186547,1.),(1.,0.707106781186547,1.,0.707106781186547,1.,0.707106781186547,
1.,0.707106781186547,1.),(1.,0.707106781186547,1.,0.707106781186547,1.,
0.707106781186547,1.,0.707106781186547,1.),(1.,0.707106781186548,1.,0.707106781186548,
1.,0.707106781186548,1.,0.707106781186548,1.),(1.,0.707106781186547,1.,
0.707106781186547,1.,0.707106781186547,1.,0.707106781186547,1.),(1.,0.707106781186548,
1.,0.707106781186548,1.,0.707106781186548,1.,0.707106781186548,1.),(1.,
0.707106781186547,1.,0.707106781186547,1.,0.707106781186547,1.,0.707106781186547,
1.),(1.,0.707106781186548,1.,0.707106781186548,1.,0.707106781186548,1.,
0.707106781186548,1.),(1.,0.707106781186548,1.,0.707106781186548,1.,0.707106781186548,
1.,0.707106781186548,1.),(1.,0.707106781186547,1.,0.707106781186547,1.,
0.707106781186547,1.,0.707106781186547,1.),(1.,0.707106781186548,1.,0.707106781186548,
1.,0.707106781186548,1.,0.707106781186548,1.),(1.,0.707106781186547,1.,
0.707106781186547,1.,0.707106781186547,1.,0.707106781186547,1.),(1.,0.707106781186547,
1.,0.707106781186547,1.,0.707106781186547,1.,0.707106781186547,1.),(1.,
0.707106781186547,1.,0.707106781186547,1.,0.707106781186547,1.,0.707106781186547,
1.),(1.,0.707106781186547,1.,0.707106781186547,1.,0.707106781186547,1.,
0.707106781186547,1.),(1.,0.707106781186548,1.,0.707106781186548,1.,0.707106781186548,
1.,0.707106781186548,1.),(1.,0.707106781186547,1.,0.707106781186547,1.,
0.707106781186547,1.,0.707106781186547,1.),(1.,0.707106781186548,1.,0.707106781186548,
1.,0.707106781186548,1.,0.707106781186548,1.),(1.,0.707106781186548,1.,
0.707106781186548,1.,0.707106781186548,1.,0.707106781186548,1.),(1.,0.707106781186547,
1.,0.707106781186547,1.,0.707106781186547,1.,0.707106781186547,1.),(1.,
0.707106781186548,1.,0.707106781186548,1.,0.707106781186548,1.,0.707106781186548,
1.),(1.,0.707106781186547,1.,0.707106781186547,1.,0.707106781186547,1.,
0.707106781186547,1.),(1.,0.707106781186548,1.,0.707106781186548,1.,0.707106781186548,
1.,0.707106781186548,1.),(1.,0.707106781186547,1.,0.707106781186547,1.,
0.707106781186547,1.,0.707106781186547,1.),(1.,0.707106781186547,1.,0.707106781186547,
1.,0.707106781186547,1.,0.707106781186547,1.),(1.,0.707106781186548,1.,
0.707106781186548,1.,0.707106781186548,1.,0.707106781186548,1.),(1.,0.707106781186547,
1.,0.707106781186547,1.,0.707106781186547,1.,0.707106781186547,1.),(1.,
0.707106781186548,1.,0.707106781186548,1.,0.707106781186548,1.,0.707106781186548,
1.),(1.,0.707106781186548,1.,0.707106781186548,1.,0.707106781186548,1.,
0.707106781186548,1.),(1.,0.707106781186547,1.,0.707106781186547,1.,0.707106781186547,
1.,0.707106781186547,1.),(1.,0.707106781186547,1.,0.707106781186547,1.,
0.707106781186547,1.,0.707106781186547,1.),(1.,0.707106781186548,1.,0.707106781186548,
1.,0.707106781186548,1.,0.707106781186548,1.),(1.,0.707106781186548,1.,
0.707106781186548,1.,0.707106781186548,1.,0.707106781186548,1.),(1.,0.707106781186547,
1.,0.707106781186547,1.,0.707106781186547,1.,0.707106781186547,1.),(1.,
0.707106781186547,1.,0.707106781186547,1.,0.707106781186547,1.,0.707106781186547,
1.),(1.,0.707106781186548,1.,0.707106781186548,1.,0.707106781186548,1.,
0.707106781186548,1.),(1.,0.707106781186547,1.,0.707106781186547,1.,0.707106781186547,
1.,0.707106781186547,1.),(1.,0.707106781186547,1.,0.707106781186547,1.,
0.707106781186547,1.,0.707106781186547,1.),(1.,0.707106781186548,1.,0.707106781186548,
1.,0.707106781186548,1.,0.707106781186548,1.),(1.,0.707106781186547,1.,
0.707106781186547,1.,0.707106781186547,1.,0.707106781186547,1.),(1.,0.707106781186547,
1.,0.707106781186547,1.,0.707106781186547,1.,0.707106781186547,1.),(1.,
0.707106781186548,1.,0.707106781186548,1.,0.707106781186548,1.,0.707106781186548,
1.),(1.,0.707106781186547,1.,0.707106781186547,1.,0.707106781186547,1.,
0.707106781186547,1.),(1.,0.707106781186548,1.,0.707106781186548,1.,0.707106781186548,
1.,0.707106781186548,1.),(1.,0.707106781186547,1.,0.707106781186547,1.,
0.707106781186547,1.,0.707106781186547,1.),(1.,0.707106781186547,1.,0.707106781186547,
1.,0.707106781186547,1.,0.707106781186547,1.),(1.,0.707106781186548,1.,
0.707106781186548,1.,0.707106781186548,1.,0.707106781186548,1.),(1.,0.707106781186547,
1.,0.707106781186547,1.,0.707106781186547,1.,0.707106781186547,1.),(1.,
0.707106781186548,1.,0.707106781186548,1.,0.707106781186548,1.,0.707106781186548,
1.),(1.,0.707106781186547,1.,0.707106781186547,1.,0.707106781186547,1.,
0.707106781186547,1.),(1.,0.707106781186548,1.,0.707106781186548,1.,0.707106781186548,
1.,0.707106781186548,1.),(1.,0.707106781186547,1.,0.707106781186547,1.,
0.707106781186547,1.,0.707106781186547,1.),(1.,0.707106781186547,1.,0.707106781186547,
1.,0.707106781186547,1.,0.707106781186547,1.),(1.,0.707106781186547,1.,
0.707106781186547,1.,0.707106781186547,1.,0.707106781186547,1.),(1.,0.707106781186548,
1.,0.707106781186548,1.,0.707106781186548,1.,0.707106781186548,1.),(1.,
0.707106781186547,1.,0.707106781186547,1.,0.707106781186547,1.,0.707106781186547,
1.),(1.,0.707106781186548,1.,0.707106781186548,1.,0.707106781186548,1.,
0.707106781186548,1.),(1.,0.707106781186547,1.,0.707106781186547,1.,0.707106781186547,
1.,0.707106781186547,1.),(1.,0.707106781186548,1.,0.707106781186548,1.,
0.707106781186548,1.,0.707106781186548,1.),(1.,0.707106781186548,1.,0.707106781186548,
1.,0.707106781186548,1.,0.707106781186548,1.),(1.,0.707106781186548,1.,
0.707106781186548,1.,0.707106781186548,1.,0.707106781186548,1.),(1.,0.707106781186548,
1.,0.707106781186548,1.,0.707106781186548,1.,0.707106781186548,1.),(1.,
0.707106781186547,1.,0.707106781186547,1.,0.707106781186547,1.,0.707106781186547,
1.),(1.,0.707106781186547,1.,0.707106781186547,1.,0.707106781186547,1.,
0.707106781186547,1.),(1.,0.707106781186547,1.,0.707106781186547,1.,0.707106781186547,
1.,0.707106781186547,1.),(1.,0.707106781186548,1.,0.707106781186548,1.,
0.707106781186548,1.,0.707106781186548,1.),(1.,0.707106781186547,1.,0.707106781186547,
1.,0.707106781186547,1.,0.707106781186547,1.),(1.,0.707106781186548,1.,
0.707106781186548,1.,0.707106781186548,1.,0.707106781186548,1.),(1.,0.707106781186547,
1.,0.707106781186547,1.,0.707106781186547,1.,0.707106781186547,1.),(1.,
0.707106781186547,1.,0.707106781186547,1.,0.707106781186547,1.,0.707106781186547,
1.),(1.,0.707106781186548,1.,0.707106781186548,1.,0.707106781186548,1.,
0.707106781186548,1.),(1.,0.707106781186547,1.,0.707106781186547,1.,0.707106781186547,
1.,0.707106781186547,1.),(1.,0.707106781186547,1.,0.707106781186547,1.,
0.707106781186547,1.,0.707106781186547,1.),(1.,0.707106781186548,1.,0.707106781186548,
1.,0.707106781186548,1.,0.707106781186548,1.),(1.,0.707106781186547,1.,
0.707106781186547,1.,0.707106781186547,1.,0.707106781186547,1.),(1.,0.707106781186547,
1.,0.707106781186547,1.,0.707106781186547,1.,0.707106781186547,1.),(1.,
0.707106781186548,1.,0.707106781186548,1.,0.707106781186548,1.,0.707106781186548,
1.),(1.,0.707106781186548,1.,0.707106781186548,1.,0.707106781186548,1.,
0.707106781186548,1.),(1.,0.707106781186547,1.,0.707106781186547,1.,0.707106781186547,
1.,0.707106781186547,1.),(1.,0.707106781186548,1.,0.707106781186548,1.,
0.707106781186548,1.,0.707106781186548,1.),(1.,0.707106781186547,1.,0.707106781186547,
1.,0.707106781186547,1.,0.707106781186547,1.),(1.,0.707106781186547,1.,
0.707106781186547,1.,0.707106781186547,1.,0.707106781186547,1.),(1.,0.707106781186548,
1.,0.707106781186548,1.,0.707106781186548,1.,0.707106781186548,1.),(1.,
0.707106781186547,1.,0.707106781186547,1.,0.707106781186547,1.,0.707106781186547,
1.),(1.,0.707106781186548,1.,0.707106781186548,1.,0.707106781186548,1.,
0.707106781186548,1.),(1.,0.707106781186547,1.,0.707106781186547,1.,0.707106781186547,
1.,0.707106781186547,1.),(1.,0.707106781186548,1.,0.707106781186548,1.,
0.707106781186548,1.,0.707106781186548,1.),(1.,0.707106781186547,1.,0.707106781186547,
1.,0.707106781186547,1.,0.707106781186547,1.),(1.,0.707106781186547,1.,
0.707106781186547,1.,0.707106781186547,1.,0.707106781186547,1.),(1.,0.707106781186547,
1.,0.707106781186547,1.,0.707106781186547,1.,0.707106781186547,1.),(1.,
0.707106781186548,1.,0.707106781186548,1.,0.707106781186548,1.,0.707106781186548,
1.),(1.,0.707106781186547,1.,0.707106781186547,1.,0.707106781186547,1.,
0.707106781186547,1.),(1.,0.707106781186548,1.,0.707106781186548,1.,0.707106781186548,
1.,0.707106781186548,1.),(1.,0.707106781186547,1.,0.707106781186547,1.,
0.707106781186547,1.,0.707106781186547,1.),(1.,0.707106781186548,1.,0.707106781186548,
1.,0.707106781186548,1.,0.707106781186548,1.),(1.,0.707106781186547,1.,
0.707106781186547,1.,0.707106781186547,1.,0.707106781186547,1.),(1.,0.707106781186547,
1.,0.707106781186547,1.,0.707106781186547,1.,0.707106781186547,1.),(1.,
0.707106781186548,1.,0.707106781186548,1.,0.707106781186548,1.,0.707106781186548,
1.),(1.,0.707106781186548,1.,0.707106781186548,1.,0.707106781186548,1.,
0.707106781186548,1.),(1.,0.707106781186548,1.,0.707106781186548,1.,0.707106781186548,
1.,0.707106781186548,1.),(1.,0.707106781186547,1.,0.707106781186547,1.,
0.707106781186547,1.,0.707106781186547,1.),(1.,0.707106781186548,1.,0.707106781186548,
1.,0.707106781186548,1.,0.707106781186548,1.),(1.,0.707106781186547,1.,
0.707106781186547,1.,0.707106781186547,1.,0.707106781186547,1.),(1.,0.707106781186548,
1.,0.707106781186548,1.,0.707106781186548,1.,0.707106781186548,1.),(1.,
0.707106781186547,1.,0.707106781186547,1.,0.707106781186547,1.,0.707106781186547,
1.),(1.,0.707106781186548,1.,0.707106781186548,1.,0.707106781186548,1.,
0.707106781186548,1.),(1.,0.707106781186547,1.,0.707106781186547,1.,0.707106781186547,
1.,0.707106781186547,1.),(1.,0.707106781186548,1.,0.707106781186548,1.,
0.707106781186548,1.,0.707106781186548,1.),(1.,0.707106781186548,1.,0.707106781186548,
1.,0.707106781186548,1.,0.707106781186548,1.),(1.,0.707106781186547,1.,
0.707106781186547,1.,0.707106781186547,1.,0.707106781186547,1.),(1.,0.707106781186547,
1.,0.707106781186547,1.,0.707106781186547,1.,0.707106781186547,1.),(1.,
0.707106781186547,1.,0.707106781186547,1.,0.707106781186547,1.,0.707106781186547,
1.),(1.,0.707106781186548,1.,0.707106781186548,1.,0.707106781186548,1.,
0.707106781186548,1.),(1.,0.707106781186547,1.,0.707106781186547,1.,0.707106781186547,
1.,0.707106781186547,1.),(1.,0.707106781186547,1.,0.707106781186547,1.,
0.707106781186547,1.,0.707106781186547,1.),(1.,0.707106781186548,1.,0.707106781186548,
1.,0.707106781186548,1.,0.707106781186548,1.),(1.,0.707106781186547,1.,
0.707106781186547,1.,0.707106781186547,1.,0.707106781186547,1.),(1.,0.707106781186547,
1.,0.707106781186547,1.,0.707106781186547,1.,0.707106781186547,1.),(1.,
0.707106781186548,1.,0.707106781186548,1.,0.707106781186548,1.,0.707106781186548,
1.),(1.,0.707106781186547,1.,0.707106781186547,1.,0.707106781186547,1.,
0.707106781186547,1.),(1.,0.707106781186548,1.,0.707106781186548,1.,0.707106781186548,
1.,0.707106781186548,1.),(1.,0.707106781186548,1.,0.707106781186548,1.,
0.707106781186548,1.,0.707106781186548,1.),(1.,0.707106781186548,1.,0.707106781186548,
1.,0.707106781186548,1.,0.707106781186548,1.),(1.,0.707106781186547,1.,
0.707106781186547,1.,0.707106781186547,1.,0.707106781186547,1.),(1.,0.707106781186548,
1.,0.707106781186548,1.,0.707106781186548,1.,0.707106781186548,1.),(1.,
0.707106781186547,1.,0.707106781186547,1.,0.707106781186547,1.,0.707106781186547,
1.),(1.,0.707106781186548,1.,0.707106781186548,1.,0.707106781186548,1.,
0.707106781186548,1.),(1.,0.707106781186547,1.,0.707106781186547,1.,0.707106781186547,
1.,0.707106781186547,1.),(1.,0.707106781186548,1.,0.707106781186548,1.,
0.707106781186548,1.,0.707106781186548,1.),(1.,0.707106781186547,1.,0.707106781186547,
1.,0.707106781186547,1.,0.707106781186547,1.),(1.,0.707106781186548,1.,
0.707106781186548,1.,0.707106781186548,1.,0.707106781186548,1.),(1.,0.707106781186547,
1.,0.707106781186547,1.,0.707106781186547,1.,0.707106781186547,1.),(1.,
0.707106781186548,1.,0.707106781186548,1.,0.707106781186548,1.,0.707106781186548,
1.),(1.,0.707106781186547,1.,0.707106781186547,1.,0.707106781186547,1.,
0.707106781186547,1.),(1.,0.707106781186548,1.,0.707106781186548,1.,0.707106781186548,
1.,0.707106781186548,1.),(1.,0.707106781186548,1.,0.707106781186548,1.,
0.707106781186548,1.,0.707106781186548,1.),(1.,0.707106781186547,1.,0.707106781186547,
1.,0.707106781186547,1.,0.707106781186547,1.),(1.,0.707106781186548,1.,
0.707106781186548,1.,0.707106781186548,1.,0.707106781186548,1.),(1.,0.707106781186547,
1.,0.707106781186547,1.,0.707106781186547,1.,0.707106781186547,1.),(1.,
0.707106781186548,1.,0.707106781186548,1.,0.707106781186548,1.,0.707106781186548,
1.),(1.,0.707106781186548,1.,0.707106781186548,1.,0.707106781186548,1.,
0.707106781186548,1.),(1.,0.707106781186547,1.,0.707106781186547,1.,0.707106781186547,
1.,0.707106781186547,1.),(1.,0.707106781186547,1.,0.707106781186547,1.,
0.707106781186547,1.,0.707106781186547,1.),(1.,0.707106781186548,1.,0.707106781186548,
1.,0.707106781186548,1.,0.707106781186548,1.),(1.,0.707106781186547,1.,
0.707106781186547,1.,0.707106781186547,1.,0.707106781186547,1.),(1.,0.707106781186547,
1.,0.707106781186547,1.,0.707106781186547,1.,0.707106781186547,1.),(1.,
0.707106781186548,1.,0.707106781186548,1.,0.707106781186548,1.,0.707106781186548,
1.),(1.,0.707106781186547,1.,0.707106781186547,1.,0.707106781186547,1.,
0.707106781186547,1.),(1.,0.707106781186548,1.,0.707106781186548,1.,0.707106781186548,
1.,0.707106781186548,1.),(1.,0.707106781186548,1.,0.707106781186548,1.,
0.707106781186548,1.,0.707106781186548,1.),(1.,0.707106781186547,1.,0.707106781186547,
1.,0.707106781186547,1.,0.707106781186547,1.),(1.,0.707106781186548,1.,
0.707106781186548,1.,0.707106781186548,1.,0.707106781186548,1.),(1.,0.707106781186548,
1.,0.707106781186548,1.,0.707106781186548,1.,0.707106781186548,1.),(1.,
0.707106781186548,1.,0.707106781186548,1.,0.707106781186548,1.,0.707106781186548,
1.),(1.,0.707106781186548,1.,0.707106781186548,1.,0.707106781186548,1.,
0.707106781186548,1.),(1.,0.707106781186548,1.,0.707106781186548,1.,0.707106781186548,
1.,0.707106781186548,1.),(1.,0.707106781186547,1.,0.707106781186547,1.,
0.707106781186547,1.,0.707106781186547,1.),(1.,0.707106781186548,1.,0.707106781186548,
1.,0.707106781186548,1.,0.707106781186548,1.),(1.,0.707106781186548,1.,
0.707106781186548,1.,0.707106781186548,1.,0.707106781186548,1.),(1.,0.707106781186548,
1.,0.707106781186548,1.,0.707106781186548,1.,0.707106781186548,1.),(1.,
0.707106781186547,1.,0.707106781186547,1.,0.707106781186547,1.,0.707106781186547,
1.),(1.,0.707106781186548,1.,0.707106781186548,1.,0.707106781186548,1.,
0.707106781186548,1.),(1.,0.707106781186547,1.,0.707106781186547,1.,0.707106781186547,
1.,0.707106781186547,1.),(1.,0.707106781186548,1.,0.707106781186548,1.,
0.707106781186548,1.,0.707106781186548,1.),(1.,0.707106781186547,1.,0.707106781186547,
1.,0.707106781186547,1.,0.707106781186547,1.),(1.,0.707106781186548,1.,
0.707106781186548,1.,0.707106781186548,1.,0.707106781186548,1.),(1.,0.707106781186547,
1.,0.707106781186547,1.,0.707106781186547,1.,0.707106781186547,1.),(1.,
0.707106781186548,1.,0.707106781186548,1.,0.707106781186548,1.,0.707106781186548,
1.),(1.,0.707106781186547,1.,0.707106781186547,1.,0.707106781186547,1.,
0.707106781186547,1.),(1.,0.707106781186548,1.,0.707106781186548,1.,0.707106781186548,
1.,0.707106781186548,1.),(1.,0.707106781186547,1.,0.707106781186547,1.,
0.707106781186547,1.,0.707106781186547,1.),(1.,0.707106781186547,1.,0.707106781186547,
1.,0.707106781186547,1.,0.707106781186547,1.),(1.,0.707106781186548,1.,
0.707106781186548,1.,0.707106781186548,1.,0.707106781186548,1.),(1.,0.707106781186547,
1.,0.707106781186547,1.,0.707106781186547,1.,0.707106781186547,1.),(1.,
0.707106781186547,1.,0.707106781186547,1.,0.707106781186547,1.,0.707106781186547,
1.),(1.,0.707106781186548,1.,0.707106781186548,1.,0.707106781186548,1.,
0.707106781186548,1.),(1.,0.707106781186547,1.,0.707106781186547,1.,0.707106781186547,
1.,0.707106781186547,1.),(1.,0.707106781186548,1.,0.707106781186548,1.,
0.707106781186548,1.,0.707106781186548,1.),(1.,0.707106781186547,1.,0.707106781186547,
1.,0.707106781186547,1.,0.707106781186547,1.),(1.,0.707106781186548,1.,
0.707106781186548,1.,0.707106781186548,1.,0.707106781186548,1.),(1.,0.707106781186547,
1.,0.707106781186547,1.,0.707106781186547,1.,0.707106781186547,1.),(1.,
0.707106781186548,1.,0.707106781186548,1.,0.707106781186548,1.,0.707106781186548,
1.),(1.,0.707106781186547,1.,0.707106781186547,1.,0.707106781186547,1.,
0.707106781186547,1.),(1.,0.707106781186547,1.,0.707106781186547,1.,0.707106781186547,
1.,0.707106781186547,1.),(1.,0.707106781186548,1.,0.707106781186548,1.,
0.707106781186548,1.,0.707106781186548,1.),(1.,0.707106781186547,1.,0.707106781186547,
1.,0.707106781186547,1.,0.707106781186547,1.),(1.,0.707106781186547,1.,
0.707106781186547,1.,0.707106781186547,1.,0.707106781186547,1.),(1.,0.707106781186548,
1.,0.707106781186548,1.,0.707106781186548,1.,0.707106781186548,1.),(1.,
0.707106781186547,1.,0.707106781186547,1.,0.707106781186547,1.,0.707106781186547,
1.),(1.,0.707106781186548,1.,0.707106781186548,1.,0.707106781186548,1.,
0.707106781186548,1.),(1.,0.707106781186547,1.,0.707106781186547,1.,0.707106781186547,
1.,0.707106781186547,1.),(1.,0.707106781186547,1.,0.707106781186547,1.,
0.707106781186547,1.,0.707106781186547,1.),(1.,0.707106781186548,1.,0.707106781186548,
1.,0.707106781186548,1.,0.707106781186548,1.),(1.,0.707106781186548,1.,
0.707106781186548,1.,0.707106781186548,1.,0.707106781186548,1.),(1.,0.707106781186547,
1.,0.707106781186547,1.,0.707106781186547,1.,0.707106781186547,1.),(1.,
0.707106781186548,1.,0.707106781186548,1.,0.707106781186548,1.,0.707106781186548,
1.),(1.,0.707106781186547,1.,0.707106781186547,1.,0.707106781186547,1.,
0.707106781186547,1.),(1.,0.707106781186547,1.,0.707106781186547,1.,0.707106781186547,
1.,0.707106781186547,1.),(1.,0.707106781186547,1.,0.707106781186547,1.,
0.707106781186547,1.,0.707106781186547,1.),(1.,0.707106781186548,1.,0.707106781186548,
1.,0.707106781186548,1.,0.707106781186548,1.),(1.,0.707106781186547,1.,
0.707106781186547,1.,0.707106781186547,1.,0.707106781186547,1.),(1.,0.707106781186547,
1.,0.707106781186547,1.,0.707106781186547,1.,0.707106781186547,1.),(1.,
0.707106781186548,1.,0.707106781186548,1.,0.707106781186548,1.,0.707106781186548,
1.),(1.,0.707106781186547,1.,0.707106781186547,1.,0.707106781186547,1.,
0.707106781186547,1.),(1.,0.707106781186547,1.,0.707106781186547,1.,0.707106781186547,
1.,0.707106781186547,1.),(1.,0.707106781186547,1.,0.707106781186547,1.,
0.707106781186547,1.,0.707106781186547,1.),(1.,0.707106781186548,1.,0.707106781186548,
1.,0.707106781186548,1.,0.707106781186548,1.),(1.,0.707106781186548,1.,
0.707106781186548,1.,0.707106781186548,1.,0.707106781186548,1.),(1.,0.707106781186547,
1.,0.707106781186547,1.,0.707106781186547,1.,0.707106781186547,1.),(1.,
0.707106781186548,1.,0.707106781186548,1.,0.707106781186548,1.,0.707106781186548,
1.),(1.,0.707106781186547,1.,0.707106781186547,1.,0.707106781186547,1.,
0.707106781186547,1.),(1.,0.707106781186548,1.,0.707106781186548,1.,0.707106781186548,
1.,0.707106781186548,1.),(1.,0.707106781186547,1.,0.707106781186547,1.,
0.707106781186547,1.,0.707106781186547,1.),(1.,0.707106781186547,1.,0.707106781186547,
1.,0.707106781186547,1.,0.707106781186547,1.),(1.,0.707106781186548,1.,
0.707106781186548,1.,0.707106781186548,1.,0.707106781186548,1.),(1.,0.707106781186547,
1.,0.707106781186547,1.,0.707106781186547,1.,0.707106781186547,1.),(1.,
0.707106781186548,1.,0.707106781186548,1.,0.707106781186548,1.,0.707106781186548,
1.),(1.,0.707106781186547,1.,0.707106781186547,1.,0.707106781186547,1.,
0.707106781186547,1.),(1.,0.707106781186547,1.,0.707106781186547,1.,0.707106781186547,
1.,0.707106781186547,1.),(1.,0.707106781186547,1.,0.707106781186547,1.,
0.707106781186547,1.,0.707106781186547,1.),(1.,0.707106781186547,1.,0.707106781186547,
1.,0.707106781186547,1.,0.707106781186547,1.),(1.,0.707106781186548,1.,
0.707106781186548,1.,0.707106781186548,1.,0.707106781186548,1.),(1.,0.707106781186547,
1.,0.707106781186547,1.,0.707106781186547,1.,0.707106781186547,1.),(1.,
0.707106781186547,1.,0.707106781186547,1.,0.707106781186547,1.,0.707106781186547,
1.),(1.,0.707106781186547,1.,0.707106781186547,1.,0.707106781186547,1.,
0.707106781186547,1.),(1.,0.707106781186547,1.,0.707106781186547,1.,0.707106781186547,
1.,0.707106781186547,1.),(1.,0.707106781186547,1.,0.707106781186547,1.,
0.707106781186547,1.,0.707106781186547,1.),(1.,0.707106781186548,1.,0.707106781186548,
1.,0.707106781186548,1.,0.707106781186548,1.),(1.,0.707106781186547,1.,
0.707106781186547,1.,0.707106781186547,1.,0.707106781186547,1.),(1.,0.707106781186547,
1.,0.707106781186547,1.,0.707106781186547,1.,0.707106781186547,1.),(1.,
0.707106781186547,1.,0.707106781186547,1.,0.707106781186547,1.,0.707106781186547,
1.),(1.,0.707106781186547,1.,0.707106781186547,1.,0.707106781186547,1.,
0.707106781186547,1.),(1.,0.707106781186548,1.,0.707106781186548,1.,0.707106781186548,
1.,0.707106781186548,1.),(1.,0.707106781186547,1.,0.707106781186547,1.,
0.707106781186547,1.,0.707106781186547,1.),(1.,0.707106781186548,1.,0.707106781186548,
1.,0.707106781186548,1.,0.707106781186548,1.),(1.,0.707106781186547,1.,
0.707106781186547,1.,0.707106781186547,1.,0.707106781186547,1.),(1.,0.707106781186547,
1.,0.707106781186547,1.,0.707106781186547,1.,0.707106781186547,1.),(1.,
0.707106781186548,1.,0.707106781186548,1.,0.707106781186548,1.,0.707106781186548,
1.),(1.,0.707106781186547,1.,0.707106781186547,1.,0.707106781186547,1.,
0.707106781186547,1.),(1.,0.707106781186548,1.,0.707106781186548,1.,0.707106781186548,
1.,0.707106781186548,1.),(1.,0.707106781186547,1.,0.707106781186547,1.,
0.707106781186547,1.,0.707106781186547,1.),(1.,0.707106781186547,1.,0.707106781186547,
1.,0.707106781186547,1.,0.707106781186547,1.),(1.,0.707106781186548,1.,
0.707106781186548,1.,0.707106781186548,1.,0.707106781186548,1.),(1.,0.707106781186547,
1.,0.707106781186547,1.,0.707106781186547,1.,0.707106781186547,1.),(1.,
0.707106781186547,1.,0.707106781186547,1.,0.707106781186547,1.,0.707106781186547,
1.),(1.,0.707106781186548,1.,0.707106781186548,1.,0.707106781186548,1.,
0.707106781186548,1.),(1.,0.707106781186547,1.,0.707106781186547,1.,0.707106781186547,
1.,0.707106781186547,1.),(1.,0.707106781186547,1.,0.707106781186547,1.,
0.707106781186547,1.,0.707106781186547,1.),(1.,0.707106781186547,1.,0.707106781186547,
1.,0.707106781186547,1.,0.707106781186547,1.),(1.,0.707106781186547,1.,
0.707106781186547,1.,0.707106781186547,1.,0.707106781186547,1.),(1.,0.707106781186548,
1.,0.707106781186548,1.,0.707106781186548,1.,0.707106781186548,1.),(1.,
0.707106781186547,1.,0.707106781186547,1.,0.707106781186547,1.,0.707106781186547,
1.),(1.,0.707106781186548,1.,0.707106781186548,1.,0.707106781186548,1.,
0.707106781186548,1.),(1.,0.707106781186548,1.,0.707106781186548,1.,0.707106781186548,
1.,0.707106781186548,1.),(1.,0.707106781186547,1.,0.707106781186547,1.,
0.707106781186547,1.,0.707106781186547,1.),(1.,0.707106781186548,1.,0.707106781186548,
1.,0.707106781186548,1.,0.707106781186548,1.),(1.,0.707106781186548,1.,
0.707106781186548,1.,0.707106781186548,1.,0.707106781186548,1.),(1.,0.707106781186547,
1.,0.707106781186547,1.,0.707106781186547,1.,0.707106781186547,1.),(1.,
0.707106781186547,1.,0.707106781186547,1.,0.707106781186547,1.,0.707106781186547,
1.),(1.,0.707106781186548,1.,0.707106781186548,1.,0.707106781186548,1.,
0.707106781186548,1.),(1.,0.707106781186547,1.,0.707106781186547,1.,0.707106781186547,
1.,0.707106781186547,1.),(1.,0.707106781186547,1.,0.707106781186547,1.,
0.707106781186547,1.,0.707106781186547,1.),(1.,0.707106781186547,1.,0.707106781186547,
1.,0.707106781186547,1.,0.707106781186547,1.),(1.,0.707106781186548,1.,
0.707106781186548,1.,0.707106781186548,1.,0.707106781186548,1.),(1.,0.707106781186547,
1.,0.707106781186547,1.,0.707106781186547,1.,0.707106781186547,1.),(1.,
0.707106781186547,1.,0.707106781186547,1.,0.707106781186547,1.,0.707106781186547,
1.),(1.,0.707106781186548,1.,0.707106781186548,1.,0.707106781186548,1.,
0.707106781186548,1.),(1.,0.707106781186547,1.,0.707106781186547,1.,0.707106781186547,
1.,0.707106781186547,1.),(1.,0.707106781186548,1.,0.707106781186548,1.,
0.707106781186548,1.,0.707106781186548,1.),(1.,0.707106781186547,1.,0.707106781186547,
1.,0.707106781186547,1.,0.707106781186547,1.),(1.,0.707106781186548,1.,
0.707106781186548,1.,0.707106781186548,1.,0.707106781186548,1.),(1.,0.707106781186547,
1.,0.707106781186547,1.,0.707106781186547,1.,0.707106781186547,1.),(1.,
0.707106781186547,1.,0.707106781186547,1.,0.707106781186547,1.,0.707106781186547,
1.),(1.,0.707106781186548,1.,0.707106781186548,1.,0.707106781186548,1.,
0.707106781186548,1.),(1.,0.707106781186547,1.,0.707106781186547,1.,0.707106781186547,
1.,0.707106781186547,1.),(1.,0.707106781186548,1.,0.707106781186548,1.,
0.707106781186548,1.,0.707106781186548,1.),(1.,0.707106781186547,1.,0.707106781186547,
1.,0.707106781186547,1.,0.707106781186547,1.),(1.,0.707106781186548,1.,
0.707106781186548,1.,0.707106781186548,1.,0.707106781186548,1.),(1.,0.707106781186547,
1.,0.707106781186547,1.,0.707106781186547,1.,0.707106781186547,1.),(1.,
0.707106781186548,1.,0.707106781186548,1.,0.707106781186548,1.,0.707106781186548,
1.),(1.,0.707106781186547,1.,0.707106781186547,1.,0.707106781186547,1.,
0.707106781186547,1.),(1.,0.707106781186548,1.,0.707106781186548,1.,0.707106781186548,
1.,0.707106781186548,1.),(1.,0.707106781186547,1.,0.707106781186547,1.,
0.707106781186547,1.,0.707106781186547,1.),(1.,0.707106781186547,1.,0.707106781186547,
1.,0.707106781186547,1.,0.707106781186547,1.),(1.,0.707106781186547,1.,
0.707106781186547,1.,0.707106781186547,1.,0.707106781186547,1.),(1.,0.707106781186547,
1.,0.707106781186547,1.,0.707106781186547,1.,0.707106781186547,1.),(1.,
0.707106781186548,1.,0.707106781186548,1.,0.707106781186548,1.,0.707106781186548,
1.),(1.,0.707106781186548,1.,0.707106781186548,1.,0.707106781186548,1.,
0.707106781186548,1.),(1.,0.707106781186547,1.,0.707106781186547,1.,0.707106781186547,
1.,0.707106781186547,1.),(1.,0.707106781186548,1.,0.707106781186548,1.,
0.707106781186548,1.,0.707106781186548,1.),(1.,0.707106781186548,1.,0.707106781186548,
1.,0.707106781186548,1.,0.707106781186548,1.),(1.,0.707106781186547,1.,
0.707106781186547,1.,0.707106781186547,1.,0.707106781186547,1.),(1.,0.707106781186548,
1.,0.707106781186548,1.,0.707106781186548,1.,0.707106781186548,1.),(1.,
0.707106781186547,1.,0.707106781186547,1.,0.707106781186547,1.,0.707106781186547,
1.),(1.,0.707106781186547,1.,0.707106781186547,1.,0.707106781186547,1.,
0.707106781186547,1.),(1.,0.707106781186548,1.,0.707106781186548,1.,0.707106781186548,
1.,0.707106781186548,1.),(1.,0.707106781186547,1.,0.707106781186547,1.,
0.707106781186547,1.,0.707106781186547,1.),(1.,0.707106781186547,1.,0.707106781186547,
1.,0.707106781186547,1.,0.707106781186547,1.),(1.,0.707106781186547,1.,
0.707106781186547,1.,0.707106781186547,1.,0.707106781186547,1.),(1.,0.707106781186547,
1.,0.707106781186547,1.,0.707106781186547,1.,0.707106781186547,1.),(1.,
0.707106781186548,1.,0.707106781186548,1.,0.707106781186548,1.,0.707106781186548,
1.),(1.,0.707106781186547,1.,0.707106781186547,1.,0.707106781186547,1.,
0.707106781186547,1.),(1.,0.707106781186547,1.,0.707106781186547,1.,0.707106781186547,
1.,0.707106781186547,1.),(1.,0.707106781186547,1.,0.707106781186547,1.,
0.707106781186547,1.,0.707106781186547,1.),(1.,0.707106781186548,1.,0.707106781186548,
1.,0.707106781186548,1.,0.707106781186548,1.),(1.,0.707106781186547,1.,
0.707106781186547,1.,0.707106781186547,1.,0.707106781186547,1.),(1.,0.707106781186547,
1.,0.707106781186547,1.,0.707106781186547,1.,0.707106781186547,1.),(1.,
0.707106781186548,1.,0.707106781186548,1.,0.707106781186548,1.,0.707106781186548,
1.),(1.,0.707106781186547,1.,0.707106781186547,1.,0.707106781186547,1.,
0.707106781186547,1.),(1.,0.707106781186548,1.,0.707106781186548,1.,0.707106781186548,
1.,0.707106781186548,1.),(1.,0.707106781186548,1.,0.707106781186548,1.,
0.707106781186548,1.,0.707106781186548,1.),(1.,0.707106781186547,1.,0.707106781186547,
1.,0.707106781186547,1.,0.707106781186547,1.),(1.,0.707106781186548,1.,
0.707106781186548,1.,0.707106781186548,1.,0.707106781186548,1.),(1.,0.707106781186547,
1.,0.707106781186547,1.,0.707106781186547,1.,0.707106781186547,1.),(1.,
0.707106781186548,1.,0.707106781186548,1.,0.707106781186548,1.,0.707106781186548,
1.),(1.,0.707106781186547,1.,0.707106781186547,1.,0.707106781186547,1.,
0.707106781186547,1.),(1.,0.707106781186548,1.,0.707106781186548,1.,0.707106781186548,
1.,0.707106781186548,1.),(1.,0.707106781186547,1.,0.707106781186547,1.,
0.707106781186547,1.,0.707106781186547,1.),(1.,0.707106781186547,1.,0.707106781186547,
1.,0.707106781186547,1.,0.707106781186547,1.),(1.,0.707106781186548,1.,
0.707106781186548,1.,0.707106781186548,1.,0.707106781186548,1.),(1.,0.707106781186547,
1.,0.707106781186547,1.,0.707106781186547,1.,0.707106781186547,1.),(1.,
0.707106781186548,1.,0.707106781186548,1.,0.707106781186548,1.,0.707106781186548,
1.),(1.,0.707106781186548,1.,0.707106781186548,1.,0.707106781186548,1.,
0.707106781186548,1.),(1.,0.707106781186547,1.,0.707106781186547,1.,0.707106781186547,
1.,0.707106781186547,1.),(1.,0.707106781186547,1.,0.707106781186547,1.,
0.707106781186547,1.,0.707106781186547,1.),(1.,0.707106781186548,1.,0.707106781186548,
1.,0.707106781186548,1.,0.707106781186548,1.),(1.,0.707106781186547,1.,
0.707106781186547,1.,0.707106781186547,1.,0.707106781186547,1.),(1.,0.707106781186548,
1.,0.707106781186548,1.,0.707106781186548,1.,0.707106781186548,1.),(1.,
0.707106781186547,1.,0.707106781186547,1.,0.707106781186547,1.,0.707106781186547,
1.),(1.,0.707106781186548,1.,0.707106781186548,1.,0.707106781186548,1.,
0.707106781186548,1.),(1.,0.707106781186547,1.,0.707106781186547,1.,0.707106781186547,
1.,0.707106781186547,1.),(1.,0.707106781186547,1.,0.707106781186547,1.,
0.707106781186547,1.,0.707106781186547,1.),(1.,0.707106781186548,1.,0.707106781186548,
1.,0.707106781186548,1.,0.707106781186548,1.),(1.,0.707106781186548,1.,
0.707106781186548,1.,0.707106781186548,1.,0.707106781186548,1.),(1.,0.707106781186547,
1.,0.707106781186547,1.,0.707106781186547,1.,0.707106781186547,1.),(1.,
0.707106781186548,1.,0.707106781186548,1.,0.707106781186548,1.,0.707106781186548,
1.),(1.,0.707106781186548,1.,0.707106781186548,1.,0.707106781186548,1.,
0.707106781186548,1.),(1.,0.707106781186547,1.,0.707106781186547,1.,0.707106781186547,
1.,0.707106781186547,1.),(1.,0.707106781186548,1.,0.707106781186548,1.,
0.707106781186548,1.,0.707106781186548,1.),(1.,0.707106781186548,1.,0.707106781186548,
1.,0.707106781186548,1.,0.707106781186548,1.),(1.,0.707106781186547,1.,
0.707106781186547,1.,0.707106781186547,1.,0.707106781186547,1.),(1.,0.707106781186548,
1.,0.707106781186548,1.,0.707106781186548,1.,0.707106781186548,1.),(1.,
0.707106781186547,1.,0.707106781186547,1.,0.707106781186547,1.,0.707106781186547,
1.),(1.,0.707106781186548,1.,0.707106781186548,1.,0.707106781186548,1.,
0.707106781186548,1.),(1.,0.707106781186547,1.,0.707106781186547,1.,0.707106781186547,
1.,0.707106781186547,1.),(1.,0.707106781186548,1.,0.707106781186548,1.,
0.707106781186548,1.,0.707106781186548,1.),(1.,0.707106781186547,1.,0.707106781186547,
1.,0.707106781186547,1.,0.707106781186547,1.),(1.,0.707106781186548,1.,
0.707106781186548,1.,0.707106781186548,1.,0.707106781186548,1.),(1.,0.707106781186547,
1.,0.707106781186547,1.,0.707106781186547,1.,0.707106781186547,1.),(1.,
0.707106781186547,1.,0.707106781186547,1.,0.707106781186547,1.,0.707106781186547,
1.),(1.,0.707106781186548,1.,0.707106781186548,1.,0.707106781186548,1.,
0.707106781186548,1.),(1.,0.707106781186547,1.,0.707106781186547,1.,0.707106781186547,
1.,0.707106781186547,1.),(1.,0.707106781186547,1.,0.707106781186547,1.,
0.707106781186547,1.,0.707106781186547,1.),(1.,0.707106781186548,1.,0.707106781186548,
1.,0.707106781186548,1.,0.707106781186548,1.),(1.,0.707106781186547,1.,
0.707106781186547,1.,0.707106781186547,1.,0.707106781186547,1.),(1.,0.707106781186548,
1.,0.707106781186548,1.,0.707106781186548,1.,0.707106781186548,1.),(1.,
0.707106781186548,1.,0.707106781186548,1.,0.707106781186548,1.,0.707106781186548,
1.),(1.,0.707106781186547,1.,0.707106781186547,1.,0.707106781186547,1.,
0.707106781186547,1.),(1.,0.707106781186547,1.,0.707106781186547,1.,0.707106781186547,
1.,0.707106781186547,1.),(1.,0.707106781186547,1.,0.707106781186547,1.,
0.707106781186547,1.,0.707106781186547,1.),(1.,0.707106781186548,1.,0.707106781186548,
1.,0.707106781186548,1.,0.707106781186548,1.),(1.,0.707106781186547,1.,
0.707106781186547,1.,0.707106781186547,1.,0.707106781186547,1.),(1.,0.707106781186548,
1.,0.707106781186548,1.,0.707106781186548,1.,0.707106781186548,1.),(1.,
0.707106781186548,1.,0.707106781186548,1.,0.707106781186548,1.,0.707106781186548,
1.),(1.,0.707106781186547,1.,0.707106781186547,1.,0.707106781186547,1.,
0.707106781186547,1.),(1.,0.707106781186548,1.,0.707106781186548,1.,0.707106781186548,
1.,0.707106781186548,1.),(1.,0.707106781186547,1.,0.707106781186547,1.,
0.707106781186547,1.,0.707106781186547,1.),(1.,0.707106781186548,1.,0.707106781186548,
1.,0.707106781186548,1.,0.707106781186548,1.),(1.,0.707106781186547,1.,
0.707106781186547,1.,0.707106781186547,1.,0.707106781186547,1.),(1.,0.707106781186548,
1.,0.707106781186548,1.,0.707106781186548,1.,0.707106781186548,1.),(1.,
0.707106781186547,1.,0.707106781186547,1.,0.707106781186547,1.,0.707106781186547,
1.),(1.,0.707106781186547,1.,0.707106781186547,1.,0.707106781186547,1.,
0.707106781186547,1.),(1.,0.707106781186548,1.,0.707106781186548,1.,0.707106781186548,
1.,0.707106781186548,1.),(1.,0.707106781186548,1.,0.707106781186548,1.,
0.707106781186548,1.,0.707106781186548,1.),(1.,0.707106781186548,1.,0.707106781186548,
1.,0.707106781186548,1.,0.707106781186548,1.),(1.,0.707106781186547,1.,
0.707106781186547,1.,0.707106781186547,1.,0.707106781186547,1.),(1.,0.707106781186548,
1.,0.707106781186548,1.,0.707106781186548,1.,0.707106781186548,1.),(1.,
0.707106781186548,1.,0.707106781186548,1.,0.707106781186548,1.,0.707106781186548,
1.),(1.,0.707106781186547,1.,0.707106781186547,1.,0.707106781186547,1.,
0.707106781186547,1.),(1.,0.707106781186548,1.,0.707106781186548,1.,0.707106781186548,
1.,0.707106781186548,1.),(1.,0.707106781186547,1.,0.707106781186547,1.,
0.707106781186547,1.,0.707106781186547,1.),(1.,0.707106781186548,1.,0.707106781186548,
1.,0.707106781186548,1.,0.707106781186548,1.),(1.,0.707106781186548,1.,
0.707106781186548,1.,0.707106781186548,1.,0.707106781186548,1.),(1.,0.707106781186548,
1.,0.707106781186548,1.,0.707106781186548,1.,0.707106781186548,1.),(1.,
0.707106781186548,1.,0.707106781186548,1.,0.707106781186548,1.,0.707106781186548,
1.),(1.,0.707106781186548,1.,0.707106781186548,1.,0.707106781186548,1.,
0.707106781186548,1.),(1.,0.707106781186548,1.,0.707106781186548,1.,0.707106781186548,
1.,0.707106781186548,1.),(1.,0.707106781186547,1.,0.707106781186547,1.,
0.707106781186547,1.,0.707106781186547,1.),(1.,0.707106781186547,1.,0.707106781186547,
1.,0.707106781186547,1.,0.707106781186547,1.),(1.,0.707106781186548,1.,
0.707106781186548,1.,0.707106781186548,1.,0.707106781186548,1.),(1.,0.707106781186547,
1.,0.707106781186547,1.,0.707106781186547,1.,0.707106781186547,1.),(1.,
0.707106781186547,1.,0.707106781186547,1.,0.707106781186547,1.,0.707106781186547,
1.),(1.,0.707106781186548,1.,0.707106781186548,1.,0.707106781186548,1.,
0.707106781186548,1.),(1.,0.707106781186547,1.,0.707106781186547,1.,0.707106781186547,
1.,0.707106781186547,1.),(1.,0.707106781186547,1.,0.707106781186547,1.,
0.707106781186547,1.,0.707106781186547,1.),(1.,0.707106781186548,1.,0.707106781186548,
1.,0.707106781186548,1.,0.707106781186548,1.),(1.,0.707106781186547,1.,
0.707106781186547,1.,0.707106781186547,1.,0.707106781186547,1.),(1.,0.707106781186548,
1.,0.707106781186548,1.,0.707106781186548,1.,0.707106781186548,1.),(1.,
0.707106781186547,1.,0.707106781186547,1.,0.707106781186547,1.,0.707106781186547,
1.),(1.,0.707106781186548,1.,0.707106781186548,1.,0.707106781186548,1.,
0.707106781186548,1.),(1.,0.707106781186547,1.,0.707106781186547,1.,0.707106781186547,
1.,0.707106781186547,1.),(1.,0.707106781186547,1.,0.707106781186547,1.,
0.707106781186547,1.,0.707106781186547,1.),(1.,0.707106781186547,1.,0.707106781186547,
1.,0.707106781186547,1.,0.707106781186547,1.),(1.,0.707106781186548,1.,
0.707106781186548,1.,0.707106781186548,1.,0.707106781186548,1.),(1.,0.707106781186547,
1.,0.707106781186547,1.,0.707106781186547,1.,0.707106781186547,1.),(1.,
0.707106781186547,1.,0.707106781186547,1.,0.707106781186547,1.,0.707106781186547,
1.),(1.,0.707106781186548,1.,0.707106781186548,1.,0.707106781186548,1.,
0.707106781186548,1.),(1.,0.707106781186547,1.,0.707106781186547,1.,0.707106781186547,
1.,0.707106781186547,1.),(1.,0.707106781186548,1.,0.707106781186548,1.,
0.707106781186548,1.,0.707106781186548,1.),(1.,0.707106781186547,1.,0.707106781186547,
1.,0.707106781186547,1.,0.707106781186547,1.),(1.,0.707106781186548,1.,
0.707106781186548,1.,0.707106781186548,1.,0.707106781186548,1.),(1.,0.707106781186547,
1.,0.707106781186547,1.,0.707106781186547,1.,0.707106781186547,1.),(1.,
0.707106781186547,1.,0.707106781186547,1.,0.707106781186547,1.,0.707106781186547,
1.),(1.,0.707106781186547,1.,0.707106781186547,1.,0.707106781186547,1.,
0.707106781186547,1.),(1.,0.707106781186547,1.,0.707106781186547,1.,0.707106781186547,
1.,0.707106781186547,1.),(1.,0.707106781186548,1.,0.707106781186548,1.,
0.707106781186548,1.,0.707106781186548,1.),(1.,0.707106781186547,1.,0.707106781186547,
1.,0.707106781186547,1.,0.707106781186547,1.),(1.,0.707106781186547,1.,
0.707106781186547,1.,0.707106781186547,1.,0.707106781186547,1.),(1.,0.707106781186548,
1.,0.707106781186548,1.,0.707106781186548,1.,0.707106781186548,1.),(1.,
0.707106781186548,1.,0.707106781186548,1.,0.707106781186548,1.,0.707106781186548,
1.),(1.,0.707106781186547,1.,0.707106781186547,1.,0.707106781186547,1.,
0.707106781186547,1.),(1.,0.707106781186548,1.,0.707106781186548,1.,0.707106781186548,
1.,0.707106781186548,1.),(1.,0.707106781186547,1.,0.707106781186547,1.,
0.707106781186547,1.,0.707106781186547,1.),(1.,0.707106781186548,1.,0.707106781186548,
1.,0.707106781186548,1.,0.707106781186548,1.),(1.,0.707106781186547,1.,
0.707106781186547,1.,0.707106781186547,1.,0.707106781186547,1.),(1.,0.707106781186547,
1.,0.707106781186547,1.,0.707106781186547,1.,0.707106781186547,1.),(1.,
0.707106781186548,1.,0.707106781186548,1.,0.707106781186548,1.,0.707106781186548,
1.),(1.,0.707106781186547,1.,0.707106781186547,1.,0.707106781186547,1.,
0.707106781186547,1.),(1.,0.707106781186548,1.,0.707106781186548,1.,0.707106781186548,
1.,0.707106781186548,1.),(1.,0.707106781186547,1.,0.707106781186547,1.,
0.707106781186547,1.,0.707106781186547,1.),(1.,0.707106781186548,1.,0.707106781186548,
1.,0.707106781186548,1.,0.707106781186548,1.),(1.,0.707106781186547,1.,
0.707106781186547,1.,0.707106781186547,1.,0.707106781186547,1.),(1.,0.707106781186548,
1.,0.707106781186548,1.,0.707106781186548,1.,0.707106781186548,1.),(1.,
0.707106781186548,1.,0.707106781186548,1.,0.707106781186548,1.,0.707106781186548,
1.),(1.,0.707106781186547,1.,0.707106781186547,1.,0.707106781186547,1.,
0.707106781186547,1.),(1.,0.707106781186548,1.,0.707106781186548,1.,0.707106781186548,
1.,0.707106781186548,1.),(1.,0.707106781186547,1.,0.707106781186547,1.,
0.707106781186547,1.,0.707106781186547,1.),(1.,0.707106781186547,1.,0.707106781186547,
1.,0.707106781186547,1.,0.707106781186547,1.),(1.,0.707106781186548,1.,
0.707106781186548,1.,0.707106781186548,1.,0.707106781186548,1.),(1.,0.707106781186547,
1.,0.707106781186547,1.,0.707106781186547,1.,0.707106781186547,1.),(1.,
0.707106781186547,1.,0.707106781186547,1.,0.707106781186547,1.,0.707106781186547,
1.),(1.,0.707106781186548,1.,0.707106781186548,1.,0.707106781186548,1.,
0.707106781186548,1.),(1.,0.707106781186548,1.,0.707106781186548,1.,0.707106781186548,
1.,0.707106781186548,1.),(1.,0.707106781186548,1.,0.707106781186548,1.,
0.707106781186548,1.,0.707106781186548,1.),(1.,0.707106781186547,1.,0.707106781186547,
1.,0.707106781186547,1.,0.707106781186547,1.),(1.,0.707106781186548,1.,
0.707106781186548,1.,0.707106781186548,1.,0.707106781186548,1.),(1.,0.707106781186547,
1.,0.707106781186547,1.,0.707106781186547,1.,0.707106781186547,1.),(1.,
0.707106781186547,1.,0.707106781186547,1.,0.707106781186547,1.,0.707106781186547,
1.),(1.,0.707106781186547,1.,0.707106781186547,1.,0.707106781186547,1.,
0.707106781186547,1.),(1.,0.707106781186548,1.,0.707106781186548,1.,0.707106781186548,
1.,0.707106781186548,1.),(1.,0.707106781186547,1.,0.707106781186547,1.,
0.707106781186547,1.,0.707106781186547,1.),(1.,0.707106781186548,1.,0.707106781186548,
1.,0.707106781186548,1.,0.707106781186548,1.),(1.,0.707106781186548,1.,
0.707106781186548,1.,0.707106781186548,1.,0.707106781186548,1.),(1.,0.707106781186548,
1.,0.707106781186548,1.,0.707106781186548,1.,0.707106781186548,1.),(1.,
0.707106781186547,1.,0.707106781186547,1.,0.707106781186547,1.,0.707106781186547,
1.),(1.,0.707106781186547,1.,0.707106781186547,1.,0.707106781186547,1.,
0.707106781186547,1.),(1.,0.707106781186547,1.,0.707106781186547,1.,0.707106781186547,
1.,0.707106781186547,1.),(1.,0.707106781186547,1.,0.707106781186547,1.,
0.707106781186547,1.,0.707106781186547,1.),(1.,0.707106781186548,1.,0.707106781186548,
1.,0.707106781186548,1.,0.707106781186548,1.),(1.,0.707106781186547,1.,
0.707106781186547,1.,0.707106781186547,1.,0.707106781186547,1.),(1.,0.707106781186547,
1.,0.707106781186547,1.,0.707106781186547,1.,0.707106781186547,1.),(1.,
0.707106781186548,1.,0.707106781186548,1.,0.707106781186548,1.,0.707106781186548,
1.),(1.,0.707106781186547,1.,0.707106781186547,1.,0.707106781186547,1.,
0.707106781186547,1.),(1.,0.707106781186548,1.,0.707106781186548,1.,0.707106781186548,
1.,0.707106781186548,1.),(1.,0.707106781186547,1.,0.707106781186547,1.,
0.707106781186547,1.,0.707106781186547,1.),(1.,0.707106781186547,1.,0.707106781186547,
1.,0.707106781186547,1.,0.707106781186547,1.),(1.,0.707106781186548,1.,
0.707106781186548,1.,0.707106781186548,1.,0.707106781186548,1.),(1.,0.707106781186547,
1.,0.707106781186547,1.,0.707106781186547,1.,0.707106781186547,1.),(1.,
0.707106781186548,1.,0.707106781186548,1.,0.707106781186548,1.,0.707106781186548,
1.),(1.,0.707106781186547,1.,0.707106781186547,1.,0.707106781186547,1.,
0.707106781186547,1.),(1.,0.707106781186548,1.,0.707106781186548,1.,0.707106781186548,
1.,0.707106781186548,1.),(1.,0.707106781186547,1.,0.707106781186547,1.,
0.707106781186547,1.,0.707106781186547,1.),(1.,0.707106781186547,1.,0.707106781186547,
1.,0.707106781186547,1.,0.707106781186547,1.),(1.,0.707106781186547,1.,
0.707106781186547,1.,0.707106781186547,1.,0.707106781186547,1.),(1.,0.707106781186547,
1.,0.707106781186547,1.,0.707106781186547,1.,0.707106781186547,1.),(1.,
0.707106781186547,1.,0.707106781186547,1.,0.707106781186547,1.,0.707106781186547,
1.),(1.,0.707106781186547,1.,0.707106781186547,1.,0.707106781186547,1.,
0.707106781186547,1.),(1.,0.707106781186548,1.,0.707106781186548,1.,0.707106781186548,
1.,0.707106781186548,1.),(1.,0.707106781186547,1.,0.707106781186547,1.,
0.707106781186547,1.,0.707106781186547,1.),(1.,0.707106781186547,1.,0.707106781186547,
1.,0.707106781186547,1.,0.707106781186547,1.),(1.,0.707106781186548,1.,
0.707106781186548,1.,0.707106781186548,1.,0.707106781186548,1.),(1.,0.707106781186548,
1.,0.707106781186548,1.,0.707106781186548,1.,0.707106781186548,1.),(1.,
0.707106781186547,1.,0.707106781186547,1.,0.707106781186547,1.,0.707106781186547,
1.),(1.,0.707106781186548,1.,0.707106781186548,1.,0.707106781186548,1.,
0.707106781186548,1.),(1.,0.707106781186548,1.,0.707106781186548,1.,0.707106781186548,
1.,0.707106781186548,1.),(1.,0.707106781186547,1.,0.707106781186547,1.,
0.707106781186547,1.,0.707106781186547,1.),(1.,0.707106781186547,1.,0.707106781186547,
1.,0.707106781186547,1.,0.707106781186547,1.),(1.,0.707106781186548,1.,
0.707106781186548,1.,0.707106781186548,1.,0.707106781186548,1.),(1.,0.707106781186547,
1.,0.707106781186547,1.,0.707106781186547,1.,0.707106781186547,1.),(1.,
0.707106781186547,1.,0.707106781186547,1.,0.707106781186547,1.,0.707106781186547,
1.),(1.,0.707106781186548,1.,0.707106781186548,1.,0.707106781186548,1.,
0.707106781186548,1.),(1.,0.707106781186547,1.,0.707106781186547,1.,0.707106781186547,
1.,0.707106781186547,1.),(1.,0.707106781186548,1.,0.707106781186548,1.,
0.707106781186548,1.,0.707106781186548,1.),(1.,0.707106781186548,1.,0.707106781186548,
1.,0.707106781186548,1.,0.707106781186548,1.),(1.,0.707106781186548,1.,
0.707106781186548,1.,0.707106781186548,1.,0.707106781186548,1.),(1.,0.707106781186547,
1.,0.707106781186547,1.,0.707106781186547,1.,0.707106781186547,1.),(1.,
0.707106781186547,1.,0.707106781186547,1.,0.707106781186547,1.,0.707106781186547,
1.),(1.,0.707106781186547,1.,0.707106781186547,1.,0.707106781186547,1.,
0.707106781186547,1.),(1.,0.707106781186547,1.,0.707106781186547,1.,0.707106781186547,
1.,0.707106781186547,1.),(1.,0.707106781186548,1.,0.707106781186548,1.,
0.707106781186548,1.,0.707106781186548,1.),(1.,0.707106781186548,1.,0.707106781186548,
1.,0.707106781186548,1.,0.707106781186548,1.),(1.,0.707106781186548,1.,
0.707106781186548,1.,0.707106781186548,1.,0.707106781186548,1.),(1.,0.707106781186547,
1.,0.707106781186547,1.,0.707106781186547,1.,0.707106781186547,1.),(1.,
0.707106781186548,1.,0.707106781186548,1.,0.707106781186548,1.,0.707106781186548,
1.),(1.,0.707106781186547,1.,0.707106781186547,1.,0.707106781186547,1.,
0.707106781186547,1.),(1.,0.707106781186548,1.,0.707106781186548,1.,0.707106781186548,
1.,0.707106781186548,1.),(1.,0.707106781186548,1.,0.707106781186548,1.,
0.707106781186548,1.,0.707106781186548,1.),(1.,0.707106781186547,1.,0.707106781186547,
1.,0.707106781186547,1.,0.707106781186547,1.),(1.,0.707106781186548,1.,
0.707106781186548,1.,0.707106781186548,1.,0.707106781186548,1.),(1.,0.707106781186547,
1.,0.707106781186547,1.,0.707106781186547,1.,0.707106781186547,1.),(1.,
0.707106781186548,1.,0.707106781186548,1.,0.707106781186548,1.,0.707106781186548,
1.),(1.,0.707106781186548,1.,0.707106781186548,1.,0.707106781186548,1.,
0.707106781186548,1.),(1.,0.707106781186547,1.,0.707106781186547,1.,0.707106781186547,
1.,0.707106781186547,1.),(1.,0.707106781186547,1.,0.707106781186547,1.,
0.707106781186547,1.,0.707106781186547,1.),(1.,0.707106781186548,1.,0.707106781186548,
1.,0.707106781186548,1.,0.707106781186548,1.),(1.,0.707106781186547,1.,
0.707106781186547,1.,0.707106781186547,1.,0.707106781186547,1.),(1.,0.707106781186548,
1.,0.707106781186548,1.,0.707106781186548,1.,0.707106781186548,1.),(1.,
0.707106781186547,1.,0.707106781186547,1.,0.707106781186547,1.,0.707106781186547,
1.),(1.,0.707106781186548,1.,0.707106781186548,1.,0.707106781186548,1.,
0.707106781186548,1.),(1.,0.707106781186548,1.,0.707106781186548,1.,0.707106781186548,
1.,0.707106781186548,1.),(1.,0.707106781186548,1.,0.707106781186548,1.,
0.707106781186548,1.,0.707106781186548,1.),(1.,0.707106781186547,1.,0.707106781186547,
1.,0.707106781186547,1.,0.707106781186547,1.),(1.,0.707106781186548,1.,
0.707106781186548,1.,0.707106781186548,1.,0.707106781186548,1.),(1.,0.707106781186547,
1.,0.707106781186547,1.,0.707106781186547,1.,0.707106781186547,1.),(1.,
0.707106781186547,1.,0.707106781186547,1.,0.707106781186547,1.,0.707106781186547,
1.),(1.,0.707106781186547,1.,0.707106781186547,1.,0.707106781186547,1.,
0.707106781186547,1.),(1.,0.707106781186547,1.,0.707106781186547,1.,0.707106781186547,
1.,0.707106781186547,1.),(1.,0.707106781186548,1.,0.707106781186548,1.,
0.707106781186548,1.,0.707106781186548,1.),(1.,0.707106781186548,1.,0.707106781186548,
1.,0.707106781186548,1.,0.707106781186548,1.),(1.,0.707106781186547,1.,
0.707106781186547,1.,0.707106781186547,1.,0.707106781186547,1.),(1.,0.707106781186547,
1.,0.707106781186547,1.,0.707106781186547,1.,0.707106781186547,1.),(1.,
0.707106781186547,1.,0.707106781186547,1.,0.707106781186547,1.,0.707106781186547,
1.),(1.,0.707106781186548,1.,0.707106781186548,1.,0.707106781186548,1.,
0.707106781186548,1.),(1.,0.707106781186547,1.,0.707106781186547,1.,0.707106781186547,
1.,0.707106781186547,1.),(1.,0.707106781186547,1.,0.707106781186547,1.,
0.707106781186547,1.,0.707106781186547,1.),(1.,0.707106781186548,1.,0.707106781186548,
1.,0.707106781186548,1.,0.707106781186548,1.),(1.,0.707106781186547,1.,
0.707106781186547,1.,0.707106781186547,1.,0.707106781186547,1.),(1.,0.707106781186548,
1.,0.707106781186548,1.,0.707106781186548,1.,0.707106781186548,1.),(1.,
0.707106781186548,1.,0.707106781186548,1.,0.707106781186548,1.,0.707106781186548,
1.),(1.,0.707106781186548,1.,0.707106781186548,1.,0.707106781186548,1.,
0.707106781186548,1.),(1.,0.707106781186547,1.,0.707106781186547,1.,0.707106781186547,
1.,0.707106781186547,1.),(1.,0.707106781186547,1.,0.707106781186547,1.,
0.707106781186547,1.,0.707106781186547,1.),(1.,0.707106781186547,1.,0.707106781186547,
1.,0.707106781186547,1.,0.707106781186547,1.),(1.,0.707106781186547,1.,
0.707106781186547,1.,0.707106781186547,1.,0.707106781186547,1.),(1.,0.707106781186548,
1.,0.707106781186548,1.,0.707106781186548,1.,0.707106781186548,1.),(1.,
0.707106781186548,1.,0.707106781186548,1.,0.707106781186548,1.,0.707106781186548,
1.),(1.,0.707106781186547,1.,0.707106781186547,1.,0.707106781186547,1.,
0.707106781186547,1.),(1.,0.707106781186548,1.,0.707106781186548,1.,0.707106781186548,
1.,0.707106781186548,1.),(1.,0.707106781186547,1.,0.707106781186547,1.,
0.707106781186547,1.,0.707106781186547,1.),(1.,0.707106781186548,1.,0.707106781186548,
1.,0.707106781186548,1.,0.707106781186548,1.),(1.,0.707106781186548,1.,
0.707106781186548,1.,0.707106781186548,1.,0.707106781186548,1.),(1.,0.707106781186547,
1.,0.707106781186547,1.,0.707106781186547,1.,0.707106781186547,1.),(1.,
0.707106781186548,1.,0.707106781186548,1.,0.707106781186548,1.,0.707106781186548,
1.),(1.,0.707106781186547,1.,0.707106781186547,1.,0.707106781186547,1.,
0.707106781186547,1.),(1.,0.707106781186548,1.,0.707106781186548,1.,0.707106781186548,
1.,0.707106781186548,1.),(1.,0.707106781186547,1.,0.707106781186547,1.,
0.707106781186547,1.,0.707106781186547,1.),(1.,0.707106781186547,1.,0.707106781186547,
1.,0.707106781186547,1.,0.707106781186547,1.),(1.,0.707106781186547,1.,
0.707106781186547,1.,0.707106781186547,1.,0.707106781186547,1.),(1.,0.707106781186548,
1.,0.707106781186548,1.,0.707106781186548,1.,0.707106781186548,1.),(1.,
0.707106781186547,1.,0.707106781186547,1.,0.707106781186547,1.,0.707106781186547,
1.),(1.,0.707106781186548,1.,0.707106781186548,1.,0.707106781186548,1.,
0.707106781186548,1.),(1.,0.707106781186547,1.,0.707106781186547,1.,0.707106781186547,
1.,0.707106781186547,1.),(1.,0.707106781186548,1.,0.707106781186548,1.,
0.707106781186548,1.,0.707106781186548,1.),(1.,0.707106781186547,1.,0.707106781186547,
1.,0.707106781186547,1.,0.707106781186547,1.),(1.,0.707106781186548,1.,
0.707106781186548,1.,0.707106781186548,1.,0.707106781186548,1.),(1.,0.707106781186547,
1.,0.707106781186547,1.,0.707106781186547,1.,0.707106781186547,1.),(1.,
0.707106781186548,1.,0.707106781186548,1.,0.707106781186548,1.,0.707106781186548,
1.),(1.,0.707106781186547,1.,0.707106781186547,1.,0.707106781186547,1.,
0.707106781186547,1.),(1.,0.707106781186547,1.,0.707106781186547,1.,0.707106781186547,
1.,0.707106781186547,1.),(1.,0.707106781186548,1.,0.707106781186548,1.,
0.707106781186548,1.,0.707106781186548,1.),(1.,0.707106781186547,1.,0.707106781186547,
1.,0.707106781186547,1.,0.707106781186547,1.),(1.,0.707106781186548,1.,
0.707106781186548,1.,0.707106781186548,1.,0.707106781186548,1.),(1.,0.707106781186547,
1.,0.707106781186547,1.,0.707106781186547,1.,0.707106781186547,1.),(1.,
0.707106781186547,1.,0.707106781186547,1.,0.707106781186547,1.,0.707106781186547,
1.),(1.,0.707106781186548,1.,0.707106781186548,1.,0.707106781186548,1.,
0.707106781186548,1.),(1.,0.707106781186548,1.,0.707106781186548,1.,0.707106781186548,
1.,0.707106781186548,1.),(1.,0.707106781186547,1.,0.707106781186547,1.,
0.707106781186547,1.,0.707106781186547,1.),(1.,0.707106781186548,1.,0.707106781186548,
1.,0.707106781186548,1.,0.707106781186548,1.),(1.,0.707106781186548,1.,
0.707106781186548,1.,0.707106781186548,1.,0.707106781186548,1.),(1.,0.707106781186547,
1.,0.707106781186547,1.,0.707106781186547,1.,0.707106781186547,1.),(1.,
0.707106781186548,1.,0.707106781186548,1.,0.707106781186548,1.,0.707106781186548,
1.),(1.,0.707106781186547,1.,0.707106781186547,1.,0.707106781186547,1.,
0.707106781186547,1.),(1.,0.707106781186548,1.,0.707106781186548,1.,0.707106781186548,
1.,0.707106781186548,1.),(1.,0.707106781186547,1.,0.707106781186547,1.,
0.707106781186547,1.,0.707106781186547,1.),(1.,0.707106781186547,1.,0.707106781186547,
1.,0.707106781186547,1.,0.707106781186547,1.),(1.,0.707106781186547,1.,
0.707106781186547,1.,0.707106781186547,1.,0.707106781186547,1.),(1.,0.707106781186548,
1.,0.707106781186548,1.,0.707106781186548,1.,0.707106781186548,1.),(1.,
0.707106781186547,1.,0.707106781186547,1.,0.707106781186547,1.,0.707106781186547,
1.),(1.,0.707106781186547,1.,0.707106781186547,1.,0.707106781186547,1.,
0.707106781186547,1.),(1.,0.707106781186548,1.,0.707106781186548,1.,0.707106781186548,
1.,0.707106781186548,1.),(1.,0.707106781186547,1.,0.707106781186547,1.,
0.707106781186547,1.,0.707106781186547,1.),(1.,0.707106781186548,1.,0.707106781186548,
1.,0.707106781186548,1.,0.707106781186548,1.),(1.,0.707106781186547,1.,
0.707106781186547,1.,0.707106781186547,1.,0.707106781186547,1.),(1.,0.707106781186548,
1.,0.707106781186548,1.,0.707106781186548,1.,0.707106781186548,1.),(1.,
0.707106781186548,1.,0.707106781186548,1.,0.707106781186548,1.,0.707106781186548,
1.),(1.,0.707106781186547,1.,0.707106781186547,1.,0.707106781186547,1.,
0.707106781186547,1.),(1.,0.707106781186548,1.,0.707106781186548,1.,0.707106781186548,
1.,0.707106781186548,1.),(1.,0.707106781186547,1.,0.707106781186547,1.,
0.707106781186547,1.,0.707106781186547,1.),(1.,0.707106781186548,1.,0.707106781186548,
1.,0.707106781186548,1.,0.707106781186548,1.),(1.,0.707106781186548,1.,
0.707106781186548,1.,0.707106781186548,1.,0.707106781186548,1.),(1.,0.707106781186548,
1.,0.707106781186548,1.,0.707106781186548,1.,0.707106781186548,1.),(1.,
0.707106781186548,1.,0.707106781186548,1.,0.707106781186548,1.,0.707106781186548,
1.),(1.,0.707106781186547,1.,0.707106781186547,1.,0.707106781186547,1.,
0.707106781186547,1.),(1.,0.707106781186547,1.,0.707106781186547,1.,0.707106781186547,
1.,0.707106781186547,1.),(1.,0.707106781186548,1.,0.707106781186548,1.,
0.707106781186548,1.,0.707106781186548,1.),(1.,0.707106781186547,1.,0.707106781186547,
1.,0.707106781186547,1.,0.707106781186547,1.),(1.,0.707106781186547,1.,
0.707106781186547,1.,0.707106781186547,1.,0.707106781186547,1.),(1.,0.707106781186548,
1.,0.707106781186548,1.,0.707106781186548,1.,0.707106781186548,1.),(1.,
0.707106781186548,1.,0.707106781186548,1.,0.707106781186548,1.,0.707106781186548,
1.),(1.,0.707106781186547,1.,0.707106781186547,1.,0.707106781186547,1.,
0.707106781186547,1.),(1.,0.707106781186547,1.,0.707106781186547,1.,0.707106781186547,
1.,0.707106781186547,1.),(1.,0.707106781186548,1.,0.707106781186548,1.,
0.707106781186548,1.,0.707106781186548,1.),(1.,0.707106781186547,1.,0.707106781186547,
1.,0.707106781186547,1.,0.707106781186547,1.),(1.,0.707106781186547,1.,
0.707106781186547,1.,0.707106781186547,1.,0.707106781186547,1.),(1.,0.707106781186548,
1.,0.707106781186548,1.,0.707106781186548,1.,0.707106781186548,1.),(1.,
0.707106781186547,1.,0.707106781186547,1.,0.707106781186547,1.,0.707106781186547,
1.),(1.,0.707106781186548,1.,0.707106781186548,1.,0.707106781186548,1.,
0.707106781186548,1.),(1.,0.707106781186547,1.,0.707106781186547,1.,0.707106781186547,
1.,0.707106781186547,1.),(1.,0.707106781186548,1.,0.707106781186548,1.,
0.707106781186548,1.,0.707106781186548,1.),(1.,0.707106781186547,1.,0.707106781186547,
1.,0.707106781186547,1.,0.707106781186547,1.),(1.,0.707106781186547,1.,
0.707106781186547,1.,0.707106781186547,1.,0.707106781186547,1.),(1.,0.707106781186547,
1.,0.707106781186547,1.,0.707106781186547,1.,0.707106781186547,1.),(1.,
0.707106781186548,1.,0.707106781186548,1.,0.707106781186548,1.,0.707106781186548,
1.),(1.,0.707106781186547,1.,0.707106781186547,1.,0.707106781186547,1.,
0.707106781186547,1.),(1.,0.707106781186547,1.,0.707106781186547,1.,0.707106781186547,
1.,0.707106781186547,1.),(1.,0.707106781186548,1.,0.707106781186548,1.,
0.707106781186548,1.,0.707106781186548,1.),(1.,0.707106781186547,1.,0.707106781186547,
1.,0.707106781186547,1.,0.707106781186547,1.),(1.,0.707106781186548,1.,
0.707106781186548,1.,0.707106781186548,1.,0.707106781186548,1.),(1.,0.707106781186548,
1.,0.707106781186548,1.,0.707106781186548,1.,0.707106781186548,1.),(1.,
0.707106781186548,1.,0.707106781186548,1.,0.707106781186548,1.,0.707106781186548,
1.),(1.,0.707106781186547,1.,0.707106781186547,1.,0.707106781186547,1.,
0.707106781186547,1.),(1.,0.707106781186547,1.,0.707106781186547,1.,0.707106781186547,
1.,0.707106781186547,1.),(1.,0.707106781186547,1.,0.707106781186547,1.,
0.707106781186547,1.,0.707106781186547,1.),(1.,0.707106781186548,1.,0.707106781186548,
1.,0.707106781186548,1.,0.707106781186548,1.),(1.,0.707106781186548,1.,
0.707106781186548,1.,0.707106781186548,1.,0.707106781186548,1.),(1.,0.707106781186547,
1.,0.707106781186547,1.,0.707106781186547,1.,0.707106781186547,1.),(1.,
0.707106781186547,1.,0.707106781186547,1.,0.707106781186547,1.,0.707106781186547,
1.),(1.,0.707106781186547,1.,0.707106781186547,1.,0.707106781186547,1.,
0.707106781186547,1.),(1.,0.707106781186547,1.,0.707106781186547,1.,0.707106781186547,
1.,0.707106781186547,1.),(1.,0.707106781186548,1.,0.707106781186548,1.,
0.707106781186548,1.,0.707106781186548,1.),(1.,0.707106781186548,1.,0.707106781186548,
1.,0.707106781186548,1.,0.707106781186548,1.),(1.,0.707106781186547,1.,
0.707106781186547,1.,0.707106781186547,1.,0.707106781186547,1.),(1.,0.707106781186547,
1.,0.707106781186547,1.,0.707106781186547,1.,0.707106781186547,1.),(1.,
0.707106781186547,1.,0.707106781186547,1.,0.707106781186547,1.,0.707106781186547,
1.),(1.,0.707106781186548,1.,0.707106781186548,1.,0.707106781186548,1.,
0.707106781186548,1.),(1.,0.707106781186548,1.,0.707106781186548,1.,0.707106781186548,
1.,0.707106781186548,1.),(1.,0.707106781186547,1.,0.707106781186547,1.,
0.707106781186547,1.,0.707106781186547,1.),(1.,0.707106781186548,1.,0.707106781186548,
1.,0.707106781186548,1.,0.707106781186548,1.),(1.,0.707106781186547,1.,
0.707106781186547,1.,0.707106781186547,1.,0.707106781186547,1.),(1.,0.707106781186548,
1.,0.707106781186548,1.,0.707106781186548,1.,0.707106781186548,1.),(1.,
0.707106781186547,1.,0.707106781186547,1.,0.707106781186547,1.,0.707106781186547,
1.),(1.,0.707106781186548,1.,0.707106781186548,1.,0.707106781186548,1.,
0.707106781186548,1.),(1.,0.707106781186548,1.,0.707106781186548,1.,0.707106781186548,
1.,0.707106781186548,1.),(1.,0.707106781186547,1.,0.707106781186547,1.,
0.707106781186547,1.,0.707106781186547,1.),(1.,0.707106781186548,1.,0.707106781186548,
1.,0.707106781186548,1.,0.707106781186548,1.),(1.,0.707106781186548,1.,
0.707106781186548,1.,0.707106781186548,1.,0.707106781186548,1.),(1.,0.707106781186548,
1.,0.707106781186548,1.,0.707106781186548,1.,0.707106781186548,1.),(1.,
0.707106781186547,1.,0.707106781186547,1.,0.707106781186547,1.,0.707106781186547,
1.),(1.,0.707106781186547,1.,0.707106781186547,1.,0.707106781186547,1.,
0.707106781186547,1.),(1.,0.707106781186547,1.,0.707106781186547,1.,0.707106781186547,
1.,0.707106781186547,1.),(1.,0.707106781186548,1.,0.707106781186548,1.,
0.707106781186548,1.,0.707106781186548,1.),(1.,0.707106781186548,1.,0.707106781186548,
1.,0.707106781186548,1.,0.707106781186548,1.),(1.,0.707106781186548,1.,
0.707106781186548,1.,0.707106781186548,1.,0.707106781186548,1.),(1.,0.707106781186547,
1.,0.707106781186547,1.,0.707106781186547,1.,0.707106781186547,1.),(1.,
0.707106781186547,1.,0.707106781186547,1.,0.707106781186547,1.,0.707106781186547,
1.),(1.,0.707106781186548,1.,0.707106781186548,1.,0.707106781186548,1.,
0.707106781186548,1.),(1.,0.707106781186548,1.,0.707106781186548,1.,0.707106781186548,
1.,0.707106781186548,1.),(1.,0.707106781186547,1.,0.707106781186547,1.,
0.707106781186547,1.,0.707106781186547,1.),(1.,0.707106781186548,1.,0.707106781186548,
1.,0.707106781186548,1.,0.707106781186548,1.),(1.,0.707106781186547,1.,
0.707106781186547,1.,0.707106781186547,1.,0.707106781186547,1.),(1.,0.707106781186547,
1.,0.707106781186547,1.,0.707106781186547,1.,0.707106781186547,1.),(1.,
0.707106781186548,1.,0.707106781186548,1.,0.707106781186548,1.,0.707106781186548,
1.),(1.,0.707106781186547,1.,0.707106781186547,1.,0.707106781186547,1.,
0.707106781186547,1.),(1.,0.707106781186548,1.,0.707106781186548,1.,0.707106781186548,
1.,0.707106781186548,1.),(1.,0.707106781186547,1.,0.707106781186547,1.,
0.707106781186547,1.,0.707106781186547,1.),(1.,0.707106781186547,1.,0.707106781186547,
1.,0.707106781186547,1.,0.707106781186547,1.),(1.,0.707106781186548,1.,
0.707106781186548,1.,0.707106781186548,1.,0.707106781186548,1.),(1.,0.707106781186547,
1.,0.707106781186547,1.,0.707106781186547,1.,0.707106781186547,1.),(1.,
0.707106781186548,1.,0.707106781186548,1.,0.707106781186548,1.,0.707106781186548,
1.),(1.,0.707106781186548,1.,0.707106781186548,1.,0.707106781186548,1.,
0.707106781186548,1.),(1.,0.707106781186547,1.,0.707106781186547,1.,0.707106781186547,
1.,0.707106781186547,1.),(1.,0.707106781186547,1.,0.707106781186547,1.,
0.707106781186547,1.,0.707106781186547,1.),(1.,0.707106781186548,1.,0.707106781186548,
1.,0.707106781186548,1.,0.707106781186548,1.),(1.,0.707106781186547,1.,
0.707106781186547,1.,0.707106781186547,1.,0.707106781186547,1.),(1.,0.707106781186548,
1.,0.707106781186548,1.,0.707106781186548,1.,0.707106781186548,1.),(1.,
0.707106781186547,1.,0.707106781186547,1.,0.707106781186547,1.,0.707106781186547,
1.),(1.,0.707106781186547,1.,0.707106781186547,1.,0.707106781186547,1.,
0.707106781186547,1.),(1.,0.707106781186548,1.,0.707106781186548,1.,0.707106781186548,
1.,0.707106781186548,1.),(1.,0.707106781186547,1.,0.707106781186547,1.,
0.707106781186547,1.,0.707106781186547,1.),(1.,0.707106781186548,1.,0.707106781186548,
1.,0.707106781186548,1.,0.707106781186548,1.),(1.,0.707106781186547,1.,
0.707106781186547,1.,0.707106781186547,1.,0.707106781186547,1.),(1.,0.707106781186548,
1.,0.707106781186548,1.,0.707106781186548,1.,0.707106781186548,1.),(1.,
0.707106781186547,1.,0.707106781186547,1.,0.707106781186547,1.,0.707106781186547,
1.),(1.,0.707106781186547,1.,0.707106781186547,1.,0.707106781186547,1.,
0.707106781186547,1.),(1.,0.707106781186548,1.,0.707106781186548,1.,0.707106781186548,
1.,0.707106781186548,1.),(1.,0.707106781186547,1.,0.707106781186547,1.,
0.707106781186547,1.,0.707106781186547,1.),(1.,0.707106781186547,1.,0.707106781186547,
1.,0.707106781186547,1.,0.707106781186547,1.),(1.,0.707106781186547,1.,
0.707106781186547,1.,0.707106781186547,1.,0.707106781186547,1.),(1.,0.707106781186547,
1.,0.707106781186547,1.,0.707106781186547,1.,0.707106781186547,1.),(1.,
0.707106781186547,1.,0.707106781186547,1.,0.707106781186547,1.,0.707106781186547,
1.),(1.,0.707106781186547,1.,0.707106781186547,1.,0.707106781186547,1.,
0.707106781186547,1.),(1.,0.707106781186548,1.,0.707106781186548,1.,0.707106781186548,
1.,0.707106781186548,1.),(1.,0.707106781186547,1.,0.707106781186547,1.,
0.707106781186547,1.,0.707106781186547,1.),(1.,0.707106781186548,1.,0.707106781186548,
1.,0.707106781186548,1.,0.707106781186548,1.),(1.,0.707106781186548,1.,
0.707106781186548,1.,0.707106781186548,1.,0.707106781186548,1.),(1.,0.707106781186548,
1.,0.707106781186548,1.,0.707106781186548,1.,0.707106781186548,1.),(1.,
0.707106781186547,1.,0.707106781186547,1.,0.707106781186547,1.,0.707106781186547,
1.),(1.,0.707106781186547,1.,0.707106781186547,1.,0.707106781186547,1.,
0.707106781186547,1.),(1.,0.707106781186547,1.,0.707106781186547,1.,0.707106781186547,
1.,0.707106781186547,1.),(1.,0.707106781186548,1.,0.707106781186548,1.,
0.707106781186548,1.,0.707106781186548,1.),(1.,0.707106781186547,1.,0.707106781186547,
1.,0.707106781186547,1.,0.707106781186547,1.),(1.,0.707106781186548,1.,
0.707106781186548,1.,0.707106781186548,1.,0.707106781186548,1.),(1.,0.707106781186547,
1.,0.707106781186547,1.,0.707106781186547,1.,0.707106781186547,1.),(1.,
0.707106781186547,1.,0.707106781186547,1.,0.707106781186547,1.,0.707106781186547,
1.),(1.,0.707106781186548,1.,0.707106781186548,1.,0.707106781186548,1.,
0.707106781186548,1.),(1.,0.707106781186547,1.,0.707106781186547,1.,0.707106781186547,
1.,0.707106781186547,1.),(1.,0.707106781186547,1.,0.707106781186547,1.,
0.707106781186547,1.,0.707106781186547,1.),(1.,0.707106781186547,1.,0.707106781186547,
1.,0.707106781186547,1.,0.707106781186547,1.),(1.,0.707106781186547,1.,
0.707106781186547,1.,0.707106781186547,1.,0.707106781186547,1.),(1.,0.707106781186547,
1.,0.707106781186547,1.,0.707106781186547,1.,0.707106781186547,1.),(1.,
0.707106781186548,1.,0.707106781186548,1.,0.707106781186548,1.,0.707106781186548,
1.),(1.,0.707106781186547,1.,0.707106781186547,1.,0.707106781186547,1.,
0.707106781186547,1.),(1.,0.707106781186548,1.,0.707106781186548,1.,0.707106781186548,
1.,0.707106781186548,1.),(1.,0.707106781186547,1.,0.707106781186547,1.,
0.707106781186547,1.,0.707106781186547,1.),(1.,0.707106781186547,1.,0.707106781186547,
1.,0.707106781186547,1.,0.707106781186547,1.),(1.,0.707106781186548,1.,
0.707106781186548,1.,0.707106781186548,1.,0.707106781186548,1.),(1.,0.707106781186548,
1.,0.707106781186548,1.,0.707106781186548,1.,0.707106781186548,1.),(1.,
0.707106781186547,1.,0.707106781186547,1.,0.707106781186547,1.,0.707106781186547,
1.),(1.,0.707106781186547,1.,0.707106781186547,1.,0.707106781186547,1.,
0.707106781186547,1.),(1.,0.707106781186547,1.,0.707106781186547,1.,0.707106781186547,
1.,0.707106781186547,1.),(1.,0.707106781186548,1.,0.707106781186548,1.,
0.707106781186548,1.,0.707106781186548,1.),(1.,0.707106781186547,1.,0.707106781186547,
1.,0.707106781186547,1.,0.707106781186547,1.),(1.,0.707106781186547,1.,
0.707106781186547,1.,0.707106781186547,1.,0.707106781186547,1.),(1.,0.707106781186548,
1.,0.707106781186548,1.,0.707106781186548,1.,0.707106781186548,1.),(1.,
0.707106781186548,1.,0.707106781186548,1.,0.707106781186548,1.,0.707106781186548,
1.),(1.,0.707106781186547,1.,0.707106781186547,1.,0.707106781186547,1.,
0.707106781186547,1.),(1.,0.707106781186548,1.,0.707106781186548,1.,0.707106781186548,
1.,0.707106781186548,1.),(1.,0.707106781186547,1.,0.707106781186547,1.,
0.707106781186547,1.,0.707106781186547,1.),(1.,0.707106781186548,1.,0.707106781186548,
1.,0.707106781186548,1.,0.707106781186548,1.),(1.,0.707106781186548,1.,
0.707106781186548,1.,0.707106781186548,1.,0.707106781186548,1.),(1.,0.707106781186547,
1.,0.707106781186547,1.,0.707106781186547,1.,0.707106781186547,1.),(1.,
0.707106781186547,1.,0.707106781186547,1.,0.707106781186547,1.,0.707106781186547,
1.),(1.,0.707106781186547,1.,0.707106781186547,1.,0.707106781186547,1.,
0.707106781186547,1.),(1.,0.707106781186548,1.,0.707106781186548,1.,0.707106781186548,
1.,0.707106781186548,1.),(1.,0.707106781186548,1.,0.707106781186548,1.,
0.707106781186548,1.,0.707106781186548,1.),(1.,0.707106781186547,1.,0.707106781186547,
1.,0.707106781186547,1.,0.707106781186547,1.),(1.,0.707106781186548,1.,
0.707106781186548,1.,0.707106781186548,1.,0.707106781186548,1.),(1.,0.707106781186547,
1.,0.707106781186547,1.,0.707106781186547,1.,0.707106781186547,1.),(1.,
0.707106781186548,1.,0.707106781186548,1.,0.707106781186548,1.,0.707106781186548,
1.),(1.,0.707106781186548,1.,0.707106781186548,1.,0.707106781186548,1.,
0.707106781186548,1.),(1.,0.707106781186547,1.,0.707106781186547,1.,0.707106781186547,
1.,0.707106781186547,1.),(1.,0.707106781186548,1.,0.707106781186548,1.,
0.707106781186548,1.,0.707106781186548,1.),(1.,0.707106781186547,1.,0.707106781186547,
1.,0.707106781186547,1.,0.707106781186547,1.),(1.,0.707106781186547,1.,
0.707106781186547,1.,0.707106781186547,1.,0.707106781186547,1.),(1.,0.707106781186547,
1.,0.707106781186547,1.,0.707106781186547,1.,0.707106781186547,1.),(1.,
0.707106781186548,1.,0.707106781186548,1.,0.707106781186548,1.,0.707106781186548,
1.),(1.,0.707106781186547,1.,0.707106781186547,1.,0.707106781186547,1.,
0.707106781186547,1.),(1.,0.707106781186548,1.,0.707106781186548,1.,0.707106781186548,
1.,0.707106781186548,1.),(1.,0.707106781186547,1.,0.707106781186547,1.,
0.707106781186547,1.,0.707106781186547,1.),(1.,0.707106781186548,1.,0.707106781186548,
1.,0.707106781186548,1.,0.707106781186548,1.),(1.,0.707106781186547,1.,
0.707106781186547,1.,0.707106781186547,1.,0.707106781186547,1.),(1.,0.707106781186547,
1.,0.707106781186547,1.,0.707106781186547,1.,0.707106781186547,1.),(1.,
0.707106781186547,1.,0.707106781186547,1.,0.707106781186547,1.,0.707106781186547,
1.),(1.,0.707106781186547,1.,0.707106781186547,1.,0.707106781186547,1.,
0.707106781186547,1.),(1.,0.707106781186547,1.,0.707106781186547,1.,0.707106781186547,
1.,0.707106781186547,1.),(1.,0.707106781186548,1.,0.707106781186548,1.,
0.707106781186548,1.,0.707106781186548,1.),(1.,0.707106781186547,1.,0.707106781186547,
1.,0.707106781186547,1.,0.707106781186547,1.),(1.,0.707106781186548,1.,
0.707106781186548,1.,0.707106781186548,1.,0.707106781186548,1.),(1.,0.707106781186547,
1.,0.707106781186547,1.,0.707106781186547,1.,0.707106781186547,1.),(1.,
0.707106781186548,1.,0.707106781186548,1.,0.707106781186548,1.,0.707106781186548,
1.),(1.,0.707106781186547,1.,0.707106781186547,1.,0.707106781186547,1.,
0.707106781186547,1.),(1.,0.707106781186548,1.,0.707106781186548,1.,0.707106781186548,
1.,0.707106781186548,1.),(1.,0.707106781186547,1.,0.707106781186547,1.,
0.707106781186547,1.,0.707106781186547,1.),(1.,0.707106781186547,1.,0.707106781186547,
1.,0.707106781186547,1.,0.707106781186547,1.),(1.,0.707106781186547,1.,
0.707106781186547,1.,0.707106781186547,1.,0.707106781186547,1.),(1.,0.707106781186547,
1.,0.707106781186547,1.,0.707106781186547,1.,0.707106781186547,1.),(1.,
0.707106781186547,1.,0.707106781186547,1.,0.707106781186547,1.,0.707106781186547,
1.),(1.,0.707106781186548,1.,0.707106781186548,1.,0.707106781186548,1.,
0.707106781186548,1.),(1.,0.707106781186548,1.,0.707106781186548,1.,0.707106781186548,
1.,0.707106781186548,1.),(1.,0.707106781186548,1.,0.707106781186548,1.,
0.707106781186548,1.,0.707106781186548,1.),(1.,0.707106781186547,1.,0.707106781186547,
1.,0.707106781186547,1.,0.707106781186547,1.),(1.,0.707106781186548,1.,
0.707106781186548,1.,0.707106781186548,1.,0.707106781186548,1.),(1.,0.707106781186547,
1.,0.707106781186547,1.,0.707106781186547,1.,0.707106781186547,1.),(1.,
0.707106781186548,1.,0.707106781186548,1.,0.707106781186548,1.,0.707106781186548,
1.),(1.,0.707106781186547,1.,0.707106781186547,1.,0.707106781186547,1.,
0.707106781186547,1.),(1.,0.707106781186547,1.,0.707106781186547,1.,0.707106781186547,
1.,0.707106781186547,1.),(1.,0.707106781186548,1.,0.707106781186548,1.,
0.707106781186548,1.,0.707106781186548,1.),(1.,0.707106781186547,1.,0.707106781186547,
1.,0.707106781186547,1.,0.707106781186547,1.),(1.,0.707106781186548,1.,
0.707106781186548,1.,0.707106781186548,1.,0.707106781186548,1.),(1.,0.707106781186547,
1.,0.707106781186547,1.,0.707106781186547,1.,0.707106781186547,1.),(1.,
0.707106781186547,1.,0.707106781186547,1.,0.707106781186547,1.,0.707106781186547,
1.),(1.,0.707106781186547,1.,0.707106781186547,1.,0.707106781186547,1.,
0.707106781186547,1.),(1.,0.707106781186548,1.,0.707106781186548,1.,0.707106781186548,
1.,0.707106781186548,1.),(1.,0.707106781186548,1.,0.707106781186548,1.,
0.707106781186548,1.,0.707106781186548,1.),(1.,0.707106781186547,1.,0.707106781186547,
1.,0.707106781186547,1.,0.707106781186547,1.),(1.,0.707106781186548,1.,
0.707106781186548,1.,0.707106781186548,1.,0.707106781186548,1.),(1.,0.707106781186547,
1.,0.707106781186547,1.,0.707106781186547,1.,0.707106781186547,1.),(1.,
0.707106781186548,1.,0.707106781186548,1.,0.707106781186548,1.,0.707106781186548,
1.),(1.,0.707106781186548,1.,0.707106781186548,1.,0.707106781186548,1.,
0.707106781186548,1.),(1.,0.707106781186547,1.,0.707106781186547,1.,0.707106781186547,
1.,0.707106781186547,1.),(1.,0.707106781186548,1.,0.707106781186548,1.,
0.707106781186548,1.,0.707106781186548,1.),(1.,0.707106781186547,1.,0.707106781186547,
1.,0.707106781186547,1.,0.707106781186547,1.),(1.,0.707106781186548,1.,
0.707106781186548,1.,0.707106781186548,1.,0.707106781186548,1.),(1.,0.707106781186548,
1.,0.707106781186548,1.,0.707106781186548,1.,0.707106781186548,1.),(1.,
0.707106781186547,1.,0.707106781186547,1.,0.707106781186547,1.,0.707106781186547,
1.),(1.,0.707106781186547,1.,0.707106781186547,1.,0.707106781186547,1.,
0.707106781186547,1.),(1.,0.707106781186547,1.,0.707106781186547,1.,0.707106781186547,
1.,0.707106781186547,1.),(1.,0.707106781186547,1.,0.707106781186547,1.,
0.707106781186547,1.,0.707106781186547,1.),(1.,0.707106781186547,1.,0.707106781186547,
1.,0.707106781186547,1.,0.707106781186547,1.),(1.,0.707106781186547,1.,
0.707106781186547,1.,0.707106781186547,1.,0.707106781186547,1.),(1.,0.707106781186548,
1.,0.707106781186548,1.,0.707106781186548,1.,0.707106781186548,1.),(1.,
0.707106781186548,1.,0.707106781186548,1.,0.707106781186548,1.,0.707106781186548,
1.),(1.,0.707106781186547,1.,0.707106781186547,1.,0.707106781186547,1.,
0.707106781186547,1.),(1.,0.707106781186548,1.,0.707106781186548,1.,0.707106781186548,
1.,0.707106781186548,1.),(1.,0.707106781186547,1.,0.707106781186547,1.,
0.707106781186547,1.,0.707106781186547,1.),(1.,0.707106781186547,1.,0.707106781186547,
1.,0.707106781186547,1.,0.707106781186547,1.),(1.,0.707106781186548,1.,
0.707106781186548,1.,0.707106781186548,1.,0.707106781186548,1.),(1.,0.707106781186547,
1.,0.707106781186547,1.,0.707106781186547,1.,0.707106781186547,1.),(1.,
0.707106781186547,1.,0.707106781186547,1.,0.707106781186547,1.,0.707106781186547,
1.),(1.,0.707106781186548,1.,0.707106781186548,1.,0.707106781186548,1.,
0.707106781186548,1.),(1.,0.707106781186547,1.,0.707106781186547,1.,0.707106781186547,
1.,0.707106781186547,1.),(1.,0.707106781186547,1.,0.707106781186547,1.,
0.707106781186547,1.,0.707106781186547,1.),(1.,0.707106781186547,1.,0.707106781186547,
1.,0.707106781186547,1.,0.707106781186547,1.),(1.,0.707106781186548,1.,
0.707106781186548,1.,0.707106781186548,1.,0.707106781186548,1.),(1.,0.707106781186547,
1.,0.707106781186547,1.,0.707106781186547,1.,0.707106781186547,1.),(1.,
0.707106781186547,1.,0.707106781186547,1.,0.707106781186547,1.,0.707106781186547,
1.),(1.,0.707106781186548,1.,0.707106781186548,1.,0.707106781186548,1.,
0.707106781186548,1.),(1.,0.707106781186547,1.,0.707106781186547,1.,0.707106781186547,
1.,0.707106781186547,1.),(1.,0.707106781186548,1.,0.707106781186548,1.,
0.707106781186548,1.,0.707106781186548,1.),(1.,0.707106781186548,1.,0.707106781186548,
1.,0.707106781186548,1.,0.707106781186548,1.),(1.,0.707106781186547,1.,
0.707106781186547,1.,0.707106781186547,1.,0.707106781186547,1.),(1.,0.707106781186547,
1.,0.707106781186547,1.,0.707106781186547,1.,0.707106781186547,1.),(1.,
0.707106781186547,1.,0.707106781186547,1.,0.707106781186547,1.,0.707106781186547,
1.),(1.,0.707106781186548,1.,0.707106781186548,1.,0.707106781186548,1.,
0.707106781186548,1.),(1.,0.707106781186547,1.,0.707106781186547,1.,0.707106781186547,
1.,0.707106781186547,1.),(1.,0.707106781186547,1.,0.707106781186547,1.,
0.707106781186547,1.,0.707106781186547,1.),(1.,0.707106781186548,1.,0.707106781186548,
1.,0.707106781186548,1.,0.707106781186548,1.),(1.,0.707106781186548,1.,
0.707106781186548,1.,0.707106781186548,1.,0.707106781186548,1.),(1.,0.707106781186548,
1.,0.707106781186548,1.,0.707106781186548,1.,0.707106781186548,1.),(1.,
0.707106781186548,1.,0.707106781186548,1.,0.707106781186548,1.,0.707106781186548,
1.),(1.,0.707106781186547,1.,0.707106781186547,1.,0.707106781186547,1.,
0.707106781186547,1.),(1.,0.707106781186548,1.,0.707106781186548,1.,0.707106781186548,
1.,0.707106781186548,1.),(1.,0.707106781186548,1.,0.707106781186548,1.,
0.707106781186548,1.,0.707106781186548,1.),(1.,0.707106781186547,1.,0.707106781186547,
1.,0.707106781186547,1.,0.707106781186547,1.),(1.,0.707106781186547,1.,
0.707106781186547,1.,0.707106781186547,1.,0.707106781186547,1.),(1.,0.707106781186548,
1.,0.707106781186548,1.,0.707106781186548,1.,0.707106781186548,1.),(1.,
0.707106781186547,1.,0.707106781186547,1.,0.707106781186547,1.,0.707106781186547,
1.),(1.,0.707106781186548,1.,0.707106781186548,1.,0.707106781186548,1.,
0.707106781186548,1.),(1.,0.707106781186547,1.,0.707106781186547,1.,0.707106781186547,
1.,0.707106781186547,1.),(1.,0.707106781186547,1.,0.707106781186547,1.,
0.707106781186547,1.,0.707106781186547,1.),(1.,0.707106781186548,1.,0.707106781186548,
1.,0.707106781186548,1.,0.707106781186548,1.),(1.,0.707106781186547,1.,
0.707106781186547,1.,0.707106781186547,1.,0.707106781186547,1.),(1.,0.707106781186547,
1.,0.707106781186547,1.,0.707106781186547,1.,0.707106781186547,1.),(1.,
0.707106781186548,1.,0.707106781186548,1.,0.707106781186548,1.,0.707106781186548,
1.),(1.,0.707106781186547,1.,0.707106781186547,1.,0.707106781186547,1.,
0.707106781186547,1.),(1.,0.707106781186548,1.,0.707106781186548,1.,0.707106781186548,
1.,0.707106781186548,1.),(1.,0.707106781186547,1.,0.707106781186547,1.,
0.707106781186547,1.,0.707106781186547,1.),(1.,0.707106781186548,1.,0.707106781186548,
1.,0.707106781186548,1.,0.707106781186548,1.),(1.,0.707106781186547,1.,
0.707106781186547,1.,0.707106781186547,1.,0.707106781186547,1.),(1.,0.707106781186548,
1.,0.707106781186548,1.,0.707106781186548,1.,0.707106781186548,1.),(1.,
0.707106781186547,1.,0.707106781186547,1.,0.707106781186547,1.,0.707106781186547,
1.),(1.,0.707106781186548,1.,0.707106781186548,1.,0.707106781186548,1.,
0.707106781186548,1.),(1.,0.707106781186547,1.,0.707106781186547,1.,0.707106781186547,
1.,0.707106781186547,1.),(1.,0.707106781186548,1.,0.707106781186548,1.,
0.707106781186548,1.,0.707106781186548,1.),(1.,0.707106781186548,1.,0.707106781186548,
1.,0.707106781186548,1.,0.707106781186548,1.),(1.,0.707106781186547,1.,
0.707106781186547,1.,0.707106781186547,1.,0.707106781186547,1.),(1.,0.707106781186547,
1.,0.707106781186547,1.,0.707106781186547,1.,0.707106781186547,1.),(1.,
0.707106781186548,1.,0.707106781186548,1.,0.707106781186548,1.,0.707106781186548,
1.),(1.,0.707106781186548,1.,0.707106781186548,1.,0.707106781186548,1.,
0.707106781186548,1.),(1.,0.707106781186547,1.,0.707106781186547,1.,0.707106781186547,
1.,0.707106781186547,1.),(1.,0.707106781186547,1.,0.707106781186547,1.,
0.707106781186547,1.,0.707106781186547,1.),(1.,0.707106781186547,1.,0.707106781186547,
1.,0.707106781186547,1.,0.707106781186547,1.),(1.,0.707106781186547,1.,
0.707106781186547,1.,0.707106781186547,1.,0.707106781186547,1.),(1.,0.707106781186547,
1.,0.707106781186547,1.,0.707106781186547,1.,0.707106781186547,1.),(1.,
0.707106781186548,1.,0.707106781186548,1.,0.707106781186548,1.,0.707106781186548,
1.),(1.,0.707106781186547,1.,0.707106781186547,1.,0.707106781186547,1.,
0.707106781186547,1.),(1.,0.707106781186547,1.,0.707106781186547,1.,0.707106781186547,
1.,0.707106781186547,1.),(1.,0.707106781186548,1.,0.707106781186548,1.,
0.707106781186548,1.,0.707106781186548,1.),(1.,0.707106781186547,1.,0.707106781186547,
1.,0.707106781186547,1.,0.707106781186547,1.),(1.,0.707106781186548,1.,
0.707106781186548,1.,0.707106781186548,1.,0.707106781186548,1.),(1.,0.707106781186548,
1.,0.707106781186548,1.,0.707106781186548,1.,0.707106781186548,1.),(1.,
0.707106781186547,1.,0.707106781186547,1.,0.707106781186547,1.,0.707106781186547,
1.),(1.,0.707106781186548,1.,0.707106781186548,1.,0.707106781186548,1.,
0.707106781186548,1.),(1.,0.707106781186547,1.,0.707106781186547,1.,0.707106781186547,
1.,0.707106781186547,1.),(1.,0.707106781186548,1.,0.707106781186548,1.,
0.707106781186548,1.,0.707106781186548,1.),(1.,0.707106781186547,1.,0.707106781186547,
1.,0.707106781186547,1.,0.707106781186547,1.),(1.,0.707106781186548,1.,
0.707106781186548,1.,0.707106781186548,1.,0.707106781186548,1.),(1.,0.707106781186547,
1.,0.707106781186547,1.,0.707106781186547,1.,0.707106781186547,1.),(1.,
0.707106781186547,1.,0.707106781186547,1.,0.707106781186547,1.,0.707106781186547,
1.),(1.,0.707106781186547,1.,0.707106781186547,1.,0.707106781186547,1.,
0.707106781186547,1.),(1.,0.707106781186547,1.,0.707106781186547,1.,0.707106781186547,
1.,0.707106781186547,1.),(1.,0.707106781186547,1.,0.707106781186547,1.,
0.707106781186547,1.,0.707106781186547,1.),(1.,0.707106781186547,1.,0.707106781186547,
1.,0.707106781186547,1.,0.707106781186547,1.),(1.,0.707106781186548,1.,
0.707106781186548,1.,0.707106781186548,1.,0.707106781186548,1.),(1.,0.707106781186547,
1.,0.707106781186547,1.,0.707106781186547,1.,0.707106781186547,1.),(1.,
0.707106781186548,1.,0.707106781186548,1.,0.707106781186548,1.,0.707106781186548,
1.),(1.,0.707106781186547,1.,0.707106781186547,1.,0.707106781186547,1.,
0.707106781186547,1.),(1.,0.707106781186547,1.,0.707106781186547,1.,0.707106781186547,
1.,0.707106781186547,1.),(1.,0.707106781186547,1.,0.707106781186547,1.,
0.707106781186547,1.,0.707106781186547,1.),(1.,0.707106781186548,1.,0.707106781186548,
1.,0.707106781186548,1.,0.707106781186548,1.),(1.,0.707106781186547,1.,
0.707106781186547,1.,0.707106781186547,1.,0.707106781186547,1.),(1.,0.707106781186548,
1.,0.707106781186548,1.,0.707106781186548,1.,0.707106781186548,1.),(1.,
0.707106781186548,1.,0.707106781186548,1.,0.707106781186548,1.,0.707106781186548,
1.),(1.,0.707106781186547,1.,0.707106781186547,1.,0.707106781186547,1.,
0.707106781186547,1.),(1.,0.707106781186547,1.,0.707106781186547,1.,0.707106781186547,
1.,0.707106781186547,1.),(1.,0.707106781186548,1.,0.707106781186548,1.,
0.707106781186548,1.,0.707106781186548,1.),(1.,0.707106781186547,1.,0.707106781186547,
1.,0.707106781186547,1.,0.707106781186547,1.),(1.,0.707106781186548,1.,
0.707106781186548,1.,0.707106781186548,1.,0.707106781186548,1.),(1.,0.707106781186547,
1.,0.707106781186547,1.,0.707106781186547,1.,0.707106781186547,1.),(1.,
0.707106781186548,1.,0.707106781186548,1.,0.707106781186548,1.,0.707106781186548,
1.),(1.,0.707106781186547,1.,0.707106781186547,1.,0.707106781186547,1.,
0.707106781186547,1.),(1.,0.707106781186548,1.,0.707106781186548,1.,0.707106781186548,
1.,0.707106781186548,1.),(1.,0.707106781186547,1.,0.707106781186547,1.,
0.707106781186547,1.,0.707106781186547,1.),(1.,0.707106781186547,1.,0.707106781186547,
1.,0.707106781186547,1.,0.707106781186547,1.),(1.,0.707106781186548,1.,
0.707106781186548,1.,0.707106781186548,1.,0.707106781186548,1.),(1.,0.707106781186547,
1.,0.707106781186547,1.,0.707106781186547,1.,0.707106781186547,1.),(1.,
0.707106781186548,1.,0.707106781186548,1.,0.707106781186548,1.,0.707106781186548,
1.),(1.,0.707106781186547,1.,0.707106781186547,1.,0.707106781186547,1.,
0.707106781186547,1.),(1.,0.707106781186548,1.,0.707106781186548,1.,0.707106781186548,
1.,0.707106781186548,1.),(1.,0.707106781186548,1.,0.707106781186548,1.,
0.707106781186548,1.,0.707106781186548,1.),(1.,0.707106781186548,1.,0.707106781186548,
1.,0.707106781186548,1.,0.707106781186548,1.),(1.,0.707106781186548,1.,
0.707106781186548,1.,0.707106781186548,1.,0.707106781186548,1.),(1.,0.707106781186547,
1.,0.707106781186547,1.,0.707106781186547,1.,0.707106781186547,1.),(1.,
0.707106781186548,1.,0.707106781186548,1.,0.707106781186548,1.,0.707106781186548,
1.),(1.,0.707106781186548,1.,0.707106781186548,1.,0.707106781186548,1.,
0.707106781186548,1.),(1.,0.707106781186548,1.,0.707106781186548,1.,0.707106781186548,
1.,0.707106781186548,1.),(1.,0.707106781186547,1.,0.707106781186547,1.,
0.707106781186547,1.,0.707106781186547,1.),(1.,0.707106781186548,1.,0.707106781186548,
1.,0.707106781186548,1.,0.707106781186548,1.),(1.,0.707106781186548,1.,
0.707106781186548,1.,0.707106781186548,1.,0.707106781186548,1.),(1.,0.707106781186547,
1.,0.707106781186547,1.,0.707106781186547,1.,0.707106781186547,1.),(1.,
0.707106781186548,1.,0.707106781186548,1.,0.707106781186548,1.,0.707106781186548,
1.),(1.,0.707106781186547,1.,0.707106781186547,1.,0.707106781186547,1.,
0.707106781186547,1.),(1.,0.707106781186548,1.,0.707106781186548,1.,0.707106781186548,
1.,0.707106781186548,1.),(1.,0.707106781186547,1.,0.707106781186547,1.,
0.707106781186547,1.,0.707106781186547,1.),(1.,0.707106781186547,1.,0.707106781186547,
1.,0.707106781186547,1.,0.707106781186547,1.),(1.,0.707106781186547,1.,
0.707106781186547,1.,0.707106781186547,1.,0.707106781186547,1.),(1.,0.707106781186548,
1.,0.707106781186548,1.,0.707106781186548,1.,0.707106781186548,1.),(1.,
0.707106781186548,1.,0.707106781186548,1.,0.707106781186548,1.,0.707106781186548,
1.),(1.,0.707106781186547,1.,0.707106781186547,1.,0.707106781186547,1.,
0.707106781186547,1.),(1.,0.707106781186548,1.,0.707106781186548,1.,0.707106781186548,
1.,0.707106781186548,1.),(1.,0.707106781186547,1.,0.707106781186547,1.,
0.707106781186547,1.,0.707106781186547,1.),(1.,0.707106781186548,1.,0.707106781186548,
1.,0.707106781186548,1.,0.707106781186548,1.),(1.,0.707106781186547,1.,
0.707106781186547,1.,0.707106781186547,1.,0.707106781186547,1.),(1.,0.707106781186548,
1.,0.707106781186548,1.,0.707106781186548,1.,0.707106781186548,1.),(1.,
0.707106781186548,1.,0.707106781186548,1.,0.707106781186548,1.,0.707106781186548,
1.),(1.,0.707106781186547,1.,0.707106781186547,1.,0.707106781186547,1.,
0.707106781186547,1.),(1.,0.707106781186548,1.,0.707106781186548,1.,0.707106781186548,
1.,0.707106781186548,1.),(1.,0.707106781186547,1.,0.707106781186547,1.,
0.707106781186547,1.,0.707106781186547,1.),(1.,0.707106781186547,1.,0.707106781186547,
1.,0.707106781186547,1.,0.707106781186547,1.),(1.,0.707106781186548,1.,
0.707106781186548,1.,0.707106781186548,1.,0.707106781186548,1.),(1.,0.707106781186547,
1.,0.707106781186547,1.,0.707106781186547,1.,0.707106781186547,1.),(1.,
0.707106781186547,1.,0.707106781186547,1.,0.707106781186547,1.,0.707106781186547,
1.),(1.,0.707106781186547,1.,0.707106781186547,1.,0.707106781186547,1.,
0.707106781186547,1.),(1.,0.707106781186548,1.,0.707106781186548,1.,0.707106781186548,
1.,0.707106781186548,1.),(1.,0.707106781186547,1.,0.707106781186547,1.,
0.707106781186547,1.,0.707106781186547,1.),(1.,0.707106781186548,1.,0.707106781186548,
1.,0.707106781186548,1.,0.707106781186548,1.),(1.,0.707106781186548,1.,
0.707106781186548,1.,0.707106781186548,1.,0.707106781186548,1.),(1.,0.707106781186547,
1.,0.707106781186547,1.,0.707106781186547,1.,0.707106781186547,1.),(1.,
0.707106781186548,1.,0.707106781186548,1.,0.707106781186548,1.,0.707106781186548,
1.),(1.,0.707106781186547,1.,0.707106781186547,1.,0.707106781186547,1.,
0.707106781186547,1.),(1.,0.707106781186548,1.,0.707106781186548,1.,0.707106781186548,
1.,0.707106781186548,1.),(1.,0.707106781186548,1.,0.707106781186548,1.,
0.707106781186548,1.,0.707106781186548,1.),(1.,0.707106781186548,1.,0.707106781186548,
1.,0.707106781186548,1.,0.707106781186548,1.),(1.,0.707106781186548,1.,
0.707106781186548,1.,0.707106781186548,1.,0.707106781186548,1.),(1.,0.707106781186547,
1.,0.707106781186547,1.,0.707106781186547,1.,0.707106781186547,1.),(1.,
0.707106781186548,1.,0.707106781186548,1.,0.707106781186548,1.,0.707106781186548,
1.),(1.,0.707106781186547,1.,0.707106781186547,1.,0.707106781186547,1.,
0.707106781186547,1.),(1.,0.707106781186548,1.,0.707106781186548,1.,0.707106781186548,
1.,0.707106781186548,1.),(1.,0.707106781186547,1.,0.707106781186547,1.,
0.707106781186547,1.,0.707106781186547,1.),(1.,0.707106781186548,1.,0.707106781186548,
1.,0.707106781186548,1.,0.707106781186548,1.),(1.,0.707106781186547,1.,
0.707106781186547,1.,0.707106781186547,1.,0.707106781186547,1.),(1.,0.707106781186547,
1.,0.707106781186547,1.,0.707106781186547,1.,0.707106781186547,1.),(1.,
0.707106781186547,1.,0.707106781186547,1.,0.707106781186547,1.,0.707106781186547,
1.),(1.,0.707106781186547,1.,0.707106781186547,1.,0.707106781186547,1.,
0.707106781186547,1.),(1.,0.707106781186548,1.,0.707106781186548,1.,0.707106781186548,
1.,0.707106781186548,1.),(1.,0.707106781186547,1.,0.707106781186547,1.,
0.707106781186547,1.,0.707106781186547,1.),(1.,0.707106781186548,1.,0.707106781186548,
1.,0.707106781186548,1.,0.707106781186548,1.),(1.,0.707106781186547,1.,
0.707106781186547,1.,0.707106781186547,1.,0.707106781186547,1.),(1.,0.707106781186547,
1.,0.707106781186547,1.,0.707106781186547,1.,0.707106781186547,1.),(1.,
0.707106781186548,1.,0.707106781186548,1.,0.707106781186548,1.,0.707106781186548,
1.),(1.,0.707106781186547,1.,0.707106781186547,1.,0.707106781186547,1.,
0.707106781186547,1.),(1.,0.707106781186548,1.,0.707106781186548,1.,0.707106781186548,
1.,0.707106781186548,1.),(1.,0.707106781186547,1.,0.707106781186547,1.,
0.707106781186547,1.,0.707106781186547,1.),(1.,0.707106781186548,1.,0.707106781186548,
1.,0.707106781186548,1.,0.707106781186548,1.),(1.,0.707106781186547,1.,
0.707106781186547,1.,0.707106781186547,1.,0.707106781186547,1.),(1.,0.707106781186548,
1.,0.707106781186548,1.,0.707106781186548,1.,0.707106781186548,1.),(1.,
0.707106781186548,1.,0.707106781186548,1.,0.707106781186548,1.,0.707106781186548,
1.),(1.,0.707106781186548,1.,0.707106781186548,1.,0.707106781186548,1.,
0.707106781186548,1.),(1.,0.707106781186548,1.,0.707106781186548,1.,0.707106781186548,
1.,0.707106781186548,1.),(1.,0.707106781186547,1.,0.707106781186547,1.,
0.707106781186547,1.,0.707106781186547,1.),(1.,0.707106781186548,1.,0.707106781186548,
1.,0.707106781186548,1.,0.707106781186548,1.),(1.,0.707106781186548,1.,
0.707106781186548,1.,0.707106781186548,1.,0.707106781186548,1.),(1.,0.707106781186547,
1.,0.707106781186547,1.,0.707106781186547,1.,0.707106781186547,1.),(1.,
0.707106781186548,1.,0.707106781186548,1.,0.707106781186548,1.,0.707106781186548,
1.),(1.,0.707106781186547,1.,0.707106781186547,1.,0.707106781186547,1.,
0.707106781186547,1.),(1.,0.707106781186548,1.,0.707106781186548,1.,0.707106781186548,
1.,0.707106781186548,1.),(1.,0.707106781186547,1.,0.707106781186547,1.,
0.707106781186547,1.,0.707106781186547,1.),(1.,0.707106781186548,1.,0.707106781186548,
1.,0.707106781186548,1.,0.707106781186548,1.),(1.,0.707106781186547,1.,
0.707106781186547,1.,0.707106781186547,1.,0.707106781186547,1.),(1.,0.707106781186547,
1.,0.707106781186547,1.,0.707106781186547,1.,0.707106781186547,1.),(1.,
0.707106781186548,1.,0.707106781186548,1.,0.707106781186548,1.,0.707106781186548,
1.),(1.,0.707106781186547,1.,0.707106781186547,1.,0.707106781186547,1.,
0.707106781186547,1.),(1.,0.707106781186548,1.,0.707106781186548,1.,0.707106781186548,
1.,0.707106781186548,1.),(1.,0.707106781186547,1.,0.707106781186547,1.,
0.707106781186547,1.,0.707106781186547,1.),(1.,0.707106781186547,1.,0.707106781186547,
1.,0.707106781186547,1.,0.707106781186547,1.),(1.,0.707106781186548,1.,
0.707106781186548,1.,0.707106781186548,1.,0.707106781186548,1.),(1.,0.707106781186547,
1.,0.707106781186547,1.,0.707106781186547,1.,0.707106781186547,1.),(1.,
0.707106781186548,1.,0.707106781186548,1.,0.707106781186548,1.,0.707106781186548,
1.),(1.,0.707106781186547,1.,0.707106781186547,1.,0.707106781186547,1.,
0.707106781186547,1.),(1.,0.707106781186547,1.,0.707106781186547,1.,0.707106781186547,
1.,0.707106781186547,1.),(1.,0.707106781186548,1.,0.707106781186548,1.,
0.707106781186548,1.,0.707106781186548,1.),(1.,0.707106781186548,1.,0.707106781186548,
1.,0.707106781186548,1.,0.707106781186548,1.),(1.,0.707106781186548,1.,
0.707106781186548,1.,0.707106781186548,1.,0.707106781186548,1.),(1.,0.707106781186548,
1.,0.707106781186548,1.,0.707106781186548,1.,0.707106781186548,1.),(1.,
0.707106781186548,1.,0.707106781186548,1.,0.707106781186548,1.,0.707106781186548,
1.),(1.,0.707106781186548,1.,0.707106781186548,1.,0.707106781186548,1.,
0.707106781186548,1.),(1.,0.707106781186548,1.,0.707106781186548,1.,0.707106781186548,
1.,0.707106781186548,1.),(1.,0.707106781186548,1.,0.707106781186548,1.,
0.707106781186548,1.,0.707106781186548,1.),(1.,0.707106781186548,1.,0.707106781186548,
1.,0.707106781186548,1.,0.707106781186548,1.),(1.,0.707106781186547,1.,
0.707106781186547,1.,0.707106781186547,1.,0.707106781186547,1.),(1.,0.707106781186548,
1.,0.707106781186548,1.,0.707106781186548,1.,0.707106781186548,1.),(1.,
0.707106781186547,1.,0.707106781186547,1.,0.707106781186547,1.,0.707106781186547,
1.),(1.,0.707106781186547,1.,0.707106781186547,1.,0.707106781186547,1.,
0.707106781186547,1.),(1.,0.707106781186548,1.,0.707106781186548,1.,0.707106781186548,
1.,0.707106781186548,1.),(1.,0.707106781186547,1.,0.707106781186547,1.,
0.707106781186547,1.,0.707106781186547,1.),(1.,0.707106781186548,1.,0.707106781186548,
1.,0.707106781186548,1.,0.707106781186548,1.),(1.,0.707106781186548,1.,
0.707106781186548,1.,0.707106781186548,1.,0.707106781186548,1.),(1.,0.707106781186547,
1.,0.707106781186547,1.,0.707106781186547,1.,0.707106781186547,1.),(1.,
0.707106781186547,1.,0.707106781186547,1.,0.707106781186547,1.,0.707106781186547,
1.),(1.,0.707106781186548,1.,0.707106781186548,1.,0.707106781186548,1.,
0.707106781186548,1.),(1.,0.707106781186548,1.,0.707106781186548,1.,0.707106781186548,
1.,0.707106781186548,1.),(1.,0.707106781186547,1.,0.707106781186547,1.,
0.707106781186547,1.,0.707106781186547,1.),(1.,0.707106781186547,1.,0.707106781186547,
1.,0.707106781186547,1.,0.707106781186547,1.),(1.,0.707106781186547,1.,
0.707106781186547,1.,0.707106781186547,1.,0.707106781186547,1.),(1.,0.707106781186547,
1.,0.707106781186547,1.,0.707106781186547,1.,0.707106781186547,1.),(1.,
0.707106781186547,1.,0.707106781186547,1.,0.707106781186547,1.,0.707106781186547,
1.),(1.,0.707106781186548,1.,0.707106781186548,1.,0.707106781186548,1.,
0.707106781186548,1.),(1.,0.707106781186547,1.,0.707106781186547,1.,0.707106781186547,
1.,0.707106781186547,1.),(1.,0.707106781186548,1.,0.707106781186548,1.,
0.707106781186548,1.,0.707106781186548,1.),(1.,0.707106781186548,1.,0.707106781186548,
1.,0.707106781186548,1.,0.707106781186548,1.),(1.,0.707106781186548,1.,
0.707106781186548,1.,0.707106781186548,1.,0.707106781186548,1.),(1.,0.707106781186547,
1.,0.707106781186547,1.,0.707106781186547,1.,0.707106781186547,1.),(1.,
0.707106781186548,1.,0.707106781186548,1.,0.707106781186548,1.,0.707106781186548,
1.),(1.,0.707106781186547,1.,0.707106781186547,1.,0.707106781186547,1.,
0.707106781186547,1.),(1.,0.707106781186548,1.,0.707106781186548,1.,0.707106781186548,
1.,0.707106781186548,1.),(1.,0.707106781186547,1.,0.707106781186547,1.,
0.707106781186547,1.,0.707106781186547,1.),(1.,0.707106781186548,1.,0.707106781186548,
1.,0.707106781186548,1.,0.707106781186548,1.),(1.,0.707106781186547,1.,
0.707106781186547,1.,0.707106781186547,1.,0.707106781186547,1.),(1.,0.707106781186548,
1.,0.707106781186548,1.,0.707106781186548,1.,0.707106781186548,1.),(1.,
0.707106781186548,1.,0.707106781186548,1.,0.707106781186548,1.,0.707106781186548,
1.),(1.,0.707106781186547,1.,0.707106781186547,1.,0.707106781186547,1.,
0.707106781186547,1.),(1.,0.707106781186547,1.,0.707106781186547,1.,0.707106781186547,
1.,0.707106781186547,1.),(1.,0.707106781186548,1.,0.707106781186548,1.,
0.707106781186548,1.,0.707106781186548,1.),(1.,0.707106781186548,1.,0.707106781186548,
1.,0.707106781186548,1.,0.707106781186548,1.),(1.,0.707106781186548,1.,
0.707106781186548,1.,0.707106781186548,1.,0.707106781186548,1.),(1.,0.707106781186547,
1.,0.707106781186547,1.,0.707106781186547,1.,0.707106781186547,1.),(1.,
0.707106781186547,1.,0.707106781186547,1.,0.707106781186547,1.,0.707106781186547,
1.),(1.,0.707106781186548,1.,0.707106781186548,1.,0.707106781186548,1.,
0.707106781186548,1.),(1.,0.707106781186547,1.,0.707106781186547,1.,0.707106781186547,
1.,0.707106781186547,1.),(1.,0.707106781186547,1.,0.707106781186547,1.,
0.707106781186547,1.,0.707106781186547,1.),(1.,0.707106781186548,1.,0.707106781186548,
1.,0.707106781186548,1.,0.707106781186548,1.),(1.,0.707106781186547,1.,
0.707106781186547,1.,0.707106781186547,1.,0.707106781186547,1.),(1.,0.707106781186548,
1.,0.707106781186548,1.,0.707106781186548,1.,0.707106781186548,1.),(1.,
0.707106781186547,1.,0.707106781186547,1.,0.707106781186547,1.,0.707106781186547,
1.),(1.,0.707106781186547,1.,0.707106781186547,1.,0.707106781186547,1.,
0.707106781186547,1.),(1.,0.707106781186548,1.,0.707106781186548,1.,0.707106781186548,
1.,0.707106781186548,1.),(1.,0.707106781186548,1.,0.707106781186548,1.,
0.707106781186548,1.,0.707106781186548,1.),(1.,0.707106781186548,1.,0.707106781186548,
1.,0.707106781186548,1.,0.707106781186548,1.),(1.,0.707106781186547,1.,
0.707106781186547,1.,0.707106781186547,1.,0.707106781186547,1.),(1.,0.707106781186547,
1.,0.707106781186547,1.,0.707106781186547,1.,0.707106781186547,1.),(1.,
0.707106781186548,1.,0.707106781186548,1.,0.707106781186548,1.,0.707106781186548,
1.),(1.,0.707106781186547,1.,0.707106781186547,1.,0.707106781186547,1.,
0.707106781186547,1.),(1.,0.707106781186548,1.,0.707106781186548,1.,0.707106781186548,
1.,0.707106781186548,1.),(1.,0.707106781186547,1.,0.707106781186547,1.,
0.707106781186547,1.,0.707106781186547,1.),(1.,0.707106781186548,1.,0.707106781186548,
1.,0.707106781186548,1.,0.707106781186548,1.),(1.,0.707106781186547,1.,
0.707106781186547,1.,0.707106781186547,1.,0.707106781186547,1.),(1.,0.707106781186548,
1.,0.707106781186548,1.,0.707106781186548,1.,0.707106781186548,1.),(1.,
0.707106781186548,1.,0.707106781186548,1.,0.707106781186548,1.,0.707106781186548,
1.),(1.,0.707106781186547,1.,0.707106781186547,1.,0.707106781186547,1.,
0.707106781186547,1.),(1.,0.707106781186548,1.,0.707106781186548,1.,0.707106781186548,
1.,0.707106781186548,1.),(1.,0.707106781186547,1.,0.707106781186547,1.,
0.707106781186547,1.,0.707106781186547,1.),(1.,0.707106781186548,1.,0.707106781186548,
1.,0.707106781186548,1.,0.707106781186548,1.),(1.,0.707106781186547,1.,
0.707106781186547,1.,0.707106781186547,1.,0.707106781186547,1.),(1.,0.707106781186547,
1.,0.707106781186547,1.,0.707106781186547,1.,0.707106781186547,1.),(1.,
0.707106781186547,1.,0.707106781186547,1.,0.707106781186547,1.,0.707106781186547,
1.),(1.,0.707106781186548,1.,0.707106781186548,1.,0.707106781186548,1.,
0.707106781186548,1.),(1.,0.707106781186547,1.,0.707106781186547,1.,0.707106781186547,
1.,0.707106781186547,1.),(1.,0.707106781186548,1.,0.707106781186548,1.,
0.707106781186548,1.,0.707106781186548,1.),(1.,0.707106781186547,1.,0.707106781186547,
1.,0.707106781186547,1.,0.707106781186547,1.),(1.,0.707106781186547,1.,
0.707106781186547,1.,0.707106781186547,1.,0.707106781186547,1.),(1.,0.707106781186547,
1.,0.707106781186547,1.,0.707106781186547,1.,0.707106781186547,1.),(1.,
0.707106781186548,1.,0.707106781186548,1.,0.707106781186548,1.,0.707106781186548,
1.),(1.,0.707106781186547,1.,0.707106781186547,1.,0.707106781186547,1.,
0.707106781186547,1.),(1.,0.707106781186547,1.,0.707106781186547,1.,0.707106781186547,
1.,0.707106781186547,1.),(1.,0.707106781186548,1.,0.707106781186548,1.,
0.707106781186548,1.,0.707106781186548,1.),(1.,0.707106781186548,1.,0.707106781186548,
1.,0.707106781186548,1.,0.707106781186548,1.),(1.,0.707106781186547,1.,
0.707106781186547,1.,0.707106781186547,1.,0.707106781186547,1.),(1.,0.707106781186548,
1.,0.707106781186548,1.,0.707106781186548,1.,0.707106781186548,1.),(1.,
0.707106781186547,1.,0.707106781186547,1.,0.707106781186547,1.,0.707106781186547,
1.),(1.,0.707106781186548,1.,0.707106781186548,1.,0.707106781186548,1.,
0.707106781186548,1.),(1.,0.707106781186548,1.,0.707106781186548,1.,0.707106781186548,
1.,0.707106781186548,1.),(1.,0.707106781186547,1.,0.707106781186547,1.,
0.707106781186547,1.,0.707106781186547,1.),(1.,0.707106781186548,1.,0.707106781186548,
1.,0.707106781186548,1.,0.707106781186548,1.),(1.,0.707106781186547,1.,
0.707106781186547,1.,0.707106781186547,1.,0.707106781186547,1.),(1.,0.707106781186547,
1.,0.707106781186547,1.,0.707106781186547,1.,0.707106781186547,1.),(1.,
0.707106781186548,1.,0.707106781186548,1.,0.707106781186548,1.,0.707106781186548,
1.),(1.,0.707106781186547,1.,0.707106781186547,1.,0.707106781186547,1.,
0.707106781186547,1.),(1.,0.707106781186547,1.,0.707106781186547,1.,0.707106781186547,
1.,0.707106781186547,1.),(1.,0.707106781186547,1.,0.707106781186547,1.,
0.707106781186547,1.,0.707106781186547,1.),(1.,0.707106781186548,1.,0.707106781186548,
1.,0.707106781186548,1.,0.707106781186548,1.),(1.,0.707106781186547,1.,
0.707106781186547,1.,0.707106781186547,1.,0.707106781186547,1.),(1.,0.707106781186548,
1.,0.707106781186548,1.,0.707106781186548,1.,0.707106781186548,1.),(1.,
0.707106781186547,1.,0.707106781186547,1.,0.707106781186547,1.,0.707106781186547,
1.),(1.,0.707106781186548,1.,0.707106781186548,1.,0.707106781186548,1.,
0.707106781186548,1.),(1.,0.707106781186548,1.,0.707106781186548,1.,0.707106781186548,
1.,0.707106781186548,1.),(1.,0.707106781186548,1.,0.707106781186548,1.,
0.707106781186548,1.,0.707106781186548,1.),(1.,0.707106781186547,1.,0.707106781186547,
1.,0.707106781186547,1.,0.707106781186547,1.),(1.,0.707106781186548,1.,
0.707106781186548,1.,0.707106781186548,1.,0.707106781186548,1.),(1.,0.707106781186548,
1.,0.707106781186548,1.,0.707106781186548,1.,0.707106781186548,1.),(1.,
0.707106781186548,1.,0.707106781186548,1.,0.707106781186548,1.,0.707106781186548,
1.),(1.,0.707106781186547,1.,0.707106781186547,1.,0.707106781186547,1.,
0.707106781186547,1.),(1.,0.707106781186548,1.,0.707106781186548,1.,0.707106781186548,
1.,0.707106781186548,1.),(1.,0.707106781186547,1.,0.707106781186547,1.,
0.707106781186547,1.,0.707106781186547,1.),(1.,0.707106781186547,1.,0.707106781186547,
1.,0.707106781186547,1.,0.707106781186547,1.),(1.,0.707106781186548,1.,
0.707106781186548,1.,0.707106781186548,1.,0.707106781186548,1.),(1.,0.707106781186547,
1.,0.707106781186547,1.,0.707106781186547,1.,0.707106781186547,1.),(1.,
0.707106781186547,1.,0.707106781186547,1.,0.707106781186547,1.,0.707106781186547,
1.),(1.,0.707106781186548,1.,0.707106781186548,1.,0.707106781186548,1.,
0.707106781186548,1.),(1.,0.707106781186548,1.,0.707106781186548,1.,0.707106781186548,
1.,0.707106781186548,1.),(1.,0.707106781186547,1.,0.707106781186547,1.,
0.707106781186547,1.,0.707106781186547,1.),(1.,0.707106781186548,1.,0.707106781186548,
1.,0.707106781186548,1.,0.707106781186548,1.),(1.,0.707106781186547,1.,
0.707106781186547,1.,0.707106781186547,1.,0.707106781186547,1.),(1.,0.707106781186548,
1.,0.707106781186548,1.,0.707106781186548,1.,0.707106781186548,1.),(1.,
0.707106781186548,1.,0.707106781186548,1.,0.707106781186548,1.,0.707106781186548,
1.),(1.,0.707106781186547,1.,0.707106781186547,1.,0.707106781186547,1.,
0.707106781186547,1.),(1.,0.707106781186548,1.,0.707106781186548,1.,0.707106781186548,
1.,0.707106781186548,1.),(1.,0.707106781186547,1.,0.707106781186547,1.,
0.707106781186547,1.,0.707106781186547,1.),(1.,0.707106781186548,1.,0.707106781186548,
1.,0.707106781186548,1.,0.707106781186548,1.),(1.,0.707106781186547,1.,
0.707106781186547,1.,0.707106781186547,1.,0.707106781186547,1.),(1.,0.707106781186548,
1.,0.707106781186548,1.,0.707106781186548,1.,0.707106781186548,1.),(1.,
0.707106781186547,1.,0.707106781186547,1.,0.707106781186547,1.,0.707106781186547,
1.),(1.,0.707106781186548,1.,0.707106781186548,1.,0.707106781186548,1.,
0.707106781186548,1.),(1.,0.707106781186548,1.,0.707106781186548,1.,0.707106781186548,
1.,0.707106781186548,1.),(1.,0.707106781186548,1.,0.707106781186548,1.,
0.707106781186548,1.,0.707106781186548,1.),(1.,0.707106781186547,1.,0.707106781186547,
1.,0.707106781186547,1.,0.707106781186547,1.),(1.,0.707106781186548,1.,
0.707106781186548,1.,0.707106781186548,1.,0.707106781186548,1.),(1.,0.707106781186548,
1.,0.707106781186548,1.,0.707106781186548,1.,0.707106781186548,1.),(1.,
0.707106781186547,1.,0.707106781186547,1.,0.707106781186547,1.,0.707106781186547,
1.),(1.,0.707106781186547,1.,0.707106781186547,1.,0.707106781186547,1.,
0.707106781186547,1.),(1.,0.707106781186548,1.,0.707106781186548,1.,0.707106781186548,
1.,0.707106781186548,1.),(1.,0.707106781186547,1.,0.707106781186547,1.,
0.707106781186547,1.,0.707106781186547,1.),(1.,0.707106781186548,1.,0.707106781186548,
1.,0.707106781186548,1.,0.707106781186548,1.),(1.,0.707106781186548,1.,
0.707106781186548,1.,0.707106781186548,1.,0.707106781186548,1.),(1.,0.707106781186547,
1.,0.707106781186547,1.,0.707106781186547,1.,0.707106781186547,1.),(1.,
0.707106781186548,1.,0.707106781186548,1.,0.707106781186548,1.,0.707106781186548,
1.),(1.,0.707106781186548,1.,0.707106781186548,1.,0.707106781186548,1.,
0.707106781186548,1.),(1.,0.707106781186547,1.,0.707106781186547,1.,0.707106781186547,
1.,0.707106781186547,1.),(1.,0.707106781186548,1.,0.707106781186548,1.,
0.707106781186548,1.,0.707106781186548,1.),(1.,0.707106781186548,1.,0.707106781186548,
1.,0.707106781186548,1.,0.707106781186548,1.),(1.,0.707106781186547,1.,
0.707106781186547,1.,0.707106781186547,1.,0.707106781186547,1.),(1.,0.707106781186547,
1.,0.707106781186547,1.,0.707106781186547,1.,0.707106781186547,1.),(1.,
0.707106781186548,1.,0.707106781186548,1.,0.707106781186548,1.,0.707106781186548,
1.),(1.,0.707106781186547,1.,0.707106781186547,1.,0.707106781186547,1.,
0.707106781186547,1.),(1.,0.707106781186548,1.,0.707106781186548,1.,0.707106781186548,
1.,0.707106781186548,1.),(1.,0.707106781186547,1.,0.707106781186547,1.,
0.707106781186547,1.,0.707106781186547,1.),(1.,0.707106781186548,1.,0.707106781186548,
1.,0.707106781186548,1.,0.707106781186548,1.),(1.,0.707106781186547,1.,
0.707106781186547,1.,0.707106781186547,1.,0.707106781186547,1.),(1.,0.707106781186548,
1.,0.707106781186548,1.,0.707106781186548,1.,0.707106781186548,1.),(1.,
0.707106781186548,1.,0.707106781186548,1.,0.707106781186548,1.,0.707106781186548,
1.),(1.,0.707106781186548,1.,0.707106781186548,1.,0.707106781186548,1.,
0.707106781186548,1.),(1.,0.707106781186547,1.,0.707106781186547,1.,0.707106781186547,
1.,0.707106781186547,1.),(1.,0.707106781186548,1.,0.707106781186548,1.,
0.707106781186548,1.,0.707106781186548,1.),(1.,0.707106781186547,1.,0.707106781186547,
1.,0.707106781186547,1.,0.707106781186547,1.),(1.,0.707106781186548,1.,
0.707106781186548,1.,0.707106781186548,1.,0.707106781186548,1.),(1.,0.707106781186547,
1.,0.707106781186547,1.,0.707106781186547,1.,0.707106781186547,1.),(1.,
0.707106781186548,1.,0.707106781186548,1.,0.707106781186548,1.,0.707106781186548,
1.),(1.,0.707106781186547,1.,0.707106781186547,1.,0.707106781186547,1.,
0.707106781186547,1.),(1.,0.707106781186548,1.,0.707106781186548,1.,0.707106781186548,
1.,0.707106781186548,1.),(1.,0.707106781186547,1.,0.707106781186547,1.,
0.707106781186547,1.,0.707106781186547,1.),(1.,0.707106781186548,1.,0.707106781186548,
1.,0.707106781186548,1.,0.707106781186548,1.),(1.,0.707106781186547,1.,
0.707106781186547,1.,0.707106781186547,1.,0.707106781186547,1.),(1.,0.707106781186548,
1.,0.707106781186548,1.,0.707106781186548,1.,0.707106781186548,1.),(1.,
0.707106781186547,1.,0.707106781186547,1.,0.707106781186547,1.,0.707106781186547,
1.),(1.,0.707106781186547,1.,0.707106781186547,1.,0.707106781186547,1.,
0.707106781186547,1.),(1.,0.707106781186547,1.,0.707106781186547,1.,0.707106781186547,
1.,0.707106781186547,1.),(1.,0.707106781186548,1.,0.707106781186548,1.,
0.707106781186548,1.,0.707106781186548,1.),(1.,0.707106781186547,1.,0.707106781186547,
1.,0.707106781186547,1.,0.707106781186547,1.),(1.,0.707106781186548,1.,
0.707106781186548,1.,0.707106781186548,1.,0.707106781186548,1.),(1.,0.707106781186547,
1.,0.707106781186547,1.,0.707106781186547,1.,0.707106781186547,1.),(1.,
0.707106781186548,1.,0.707106781186548,1.,0.707106781186548,1.,0.707106781186548,
1.),(1.,0.707106781186547,1.,0.707106781186547,1.,0.707106781186547,1.,
0.707106781186547,1.),(1.,0.707106781186548,1.,0.707106781186548,1.,0.707106781186548,
1.,0.707106781186548,1.),(1.,0.707106781186547,1.,0.707106781186547,1.,
0.707106781186547,1.,0.707106781186547,1.),(1.,0.707106781186548,1.,0.707106781186548,
1.,0.707106781186548,1.,0.707106781186548,1.),(1.,0.707106781186548,1.,
0.707106781186548,1.,0.707106781186548,1.,0.707106781186548,1.),(1.,0.707106781186548,
1.,0.707106781186548,1.,0.707106781186548,1.,0.707106781186548,1.),(1.,
0.707106781186547,1.,0.707106781186547,1.,0.707106781186547,1.,0.707106781186547,
1.),(1.,0.707106781186548,1.,0.707106781186548,1.,0.707106781186548,1.,
0.707106781186548,1.),(1.,0.707106781186547,1.,0.707106781186547,1.,0.707106781186547,
1.,0.707106781186547,1.),(1.,0.707106781186548,1.,0.707106781186548,1.,
0.707106781186548,1.,0.707106781186548,1.),(1.,0.707106781186548,1.,0.707106781186548,
1.,0.707106781186548,1.,0.707106781186548,1.),(1.,0.707106781186547,1.,
0.707106781186547,1.,0.707106781186547,1.,0.707106781186547,1.),(1.,0.707106781186548,
1.,0.707106781186548,1.,0.707106781186548,1.,0.707106781186548,1.),(1.,
0.707106781186547,1.,0.707106781186547,1.,0.707106781186547,1.,0.707106781186547,
1.),(1.,0.707106781186548,1.,0.707106781186548,1.,0.707106781186548,1.,
0.707106781186548,1.),(1.,0.707106781186547,1.,0.707106781186547,1.,0.707106781186547,
1.,0.707106781186547,1.),(1.,0.707106781186548,1.,0.707106781186548,1.,
0.707106781186548,1.,0.707106781186548,1.),(1.,0.707106781186547,1.,0.707106781186547,
1.,0.707106781186547,1.,0.707106781186547,1.),(1.,0.707106781186548,1.,
0.707106781186548,1.,0.707106781186548,1.,0.707106781186548,1.),(1.,0.707106781186547,
1.,0.707106781186547,1.,0.707106781186547,1.,0.707106781186547,1.),(1.,
0.707106781186547,1.,0.707106781186547,1.,0.707106781186547,1.,0.707106781186547,
1.),(1.,0.707106781186547,1.,0.707106781186547,1.,0.707106781186547,1.,
0.707106781186547,1.),(1.,0.707106781186548,1.,0.707106781186548,1.,0.707106781186548,
1.,0.707106781186548,1.),(1.,0.707106781186547,1.,0.707106781186547,1.,
0.707106781186547,1.,0.707106781186547,1.),(1.,0.707106781186547,1.,0.707106781186547,
1.,0.707106781186547,1.,0.707106781186547,1.),(1.,0.707106781186548,1.,
0.707106781186548,1.,0.707106781186548,1.,0.707106781186548,1.),(1.,0.707106781186547,
1.,0.707106781186547,1.,0.707106781186547,1.,0.707106781186547,1.),(1.,
0.707106781186548,1.,0.707106781186548,1.,0.707106781186548,1.,0.707106781186548,
1.),(1.,0.707106781186547,1.,0.707106781186547,1.,0.707106781186547,1.,
0.707106781186547,1.),(1.,0.707106781186547,1.,0.707106781186547,1.,0.707106781186547,
1.,0.707106781186547,1.),(1.,0.707106781186548,1.,0.707106781186548,1.,
0.707106781186548,1.,0.707106781186548,1.),(1.,0.707106781186547,1.,0.707106781186547,
1.,0.707106781186547,1.,0.707106781186547,1.),(1.,0.707106781186548,1.,
0.707106781186548,1.,0.707106781186548,1.,0.707106781186548,1.),(1.,0.707106781186547,
1.,0.707106781186547,1.,0.707106781186547,1.,0.707106781186547,1.),(1.,
0.707106781186548,1.,0.707106781186548,1.,0.707106781186548,1.,0.707106781186548,
1.),(1.,0.707106781186548,1.,0.707106781186548,1.,0.707106781186548,1.,
0.707106781186548,1.),(1.,0.707106781186548,1.,0.707106781186548,1.,0.707106781186548,
1.,0.707106781186548,1.),(1.,0.707106781186547,1.,0.707106781186547,1.,
0.707106781186547,1.,0.707106781186547,1.),(1.,0.707106781186547,1.,0.707106781186547,
1.,0.707106781186547,1.,0.707106781186547,1.),(1.,0.707106781186548,1.,
0.707106781186548,1.,0.707106781186548,1.,0.707106781186548,1.),(1.,0.707106781186548,
1.,0.707106781186548,1.,0.707106781186548,1.,0.707106781186548,1.),(1.,
0.707106781186547,1.,0.707106781186547,1.,0.707106781186547,1.,0.707106781186547,
1.),(1.,0.707106781186548,1.,0.707106781186548,1.,0.707106781186548,1.,
0.707106781186548,1.),(1.,0.707106781186547,1.,0.707106781186547,1.,0.707106781186547,
1.,0.707106781186547,1.),(1.,0.707106781186547,1.,0.707106781186547,1.,
0.707106781186547,1.,0.707106781186547,1.),(1.,0.707106781186547,1.,0.707106781186547,
1.,0.707106781186547,1.,0.707106781186547,1.),(1.,0.707106781186548,1.,
0.707106781186548,1.,0.707106781186548,1.,0.707106781186548,1.),(1.,0.707106781186547,
1.,0.707106781186547,1.,0.707106781186547,1.,0.707106781186547,1.),(1.,
0.707106781186548,1.,0.707106781186548,1.,0.707106781186548,1.,0.707106781186548,
1.),(1.,0.707106781186547,1.,0.707106781186547,1.,0.707106781186547,1.,
0.707106781186547,1.),(1.,0.707106781186548,1.,0.707106781186548,1.,0.707106781186548,
1.,0.707106781186548,1.),(1.,0.707106781186548,1.,0.707106781186548,1.,
0.707106781186548,1.,0.707106781186548,1.),(1.,0.707106781186548,1.,0.707106781186548,
1.,0.707106781186548,1.,0.707106781186548,1.),(1.,0.707106781186547,1.,
0.707106781186547,1.,0.707106781186547,1.,0.707106781186547,1.),(1.,0.707106781186547,
1.,0.707106781186547,1.,0.707106781186547,1.,0.707106781186547,1.),(1.,
0.707106781186547,1.,0.707106781186547,1.,0.707106781186547,1.,0.707106781186547,
1.),(1.,0.707106781186547,1.,0.707106781186547,1.,0.707106781186547,1.,
0.707106781186547,1.),(1.,0.707106781186547,1.,0.707106781186547,1.,0.707106781186547,
1.,0.707106781186547,1.),(1.,0.707106781186547,1.,0.707106781186547,1.,
0.707106781186547,1.,0.707106781186547,1.),(1.,0.707106781186548,1.,0.707106781186548,
1.,0.707106781186548,1.,0.707106781186548,1.),(1.,0.707106781186547,1.,
0.707106781186547,1.,0.707106781186547,1.,0.707106781186547,1.),(1.,0.707106781186548,
1.,0.707106781186548,1.,0.707106781186548,1.,0.707106781186548,1.),(1.,
0.707106781186547,1.,0.707106781186547,1.,0.707106781186547,1.,0.707106781186547,
1.),(1.,0.707106781186548,1.,0.707106781186548,1.,0.707106781186548,1.,
0.707106781186548,1.),(1.,0.707106781186547,1.,0.707106781186547,1.,0.707106781186547,
1.,0.707106781186547,1.),(1.,0.707106781186547,1.,0.707106781186547,1.,
0.707106781186547,1.,0.707106781186547,1.),(1.,0.707106781186548,1.,0.707106781186548,
1.,0.707106781186548,1.,0.707106781186548,1.),(1.,0.707106781186547,1.,
0.707106781186547,1.,0.707106781186547,1.,0.707106781186547,1.),(1.,0.707106781186547,
1.,0.707106781186547,1.,0.707106781186547,1.,0.707106781186547,1.),(1.,
0.707106781186548,1.,0.707106781186548,1.,0.707106781186548,1.,0.707106781186548,
1.),(1.,0.707106781186548,1.,0.707106781186548,1.,0.707106781186548,1.,
0.707106781186548,1.),(1.,0.707106781186547,1.,0.707106781186547,1.,0.707106781186547,
1.,0.707106781186547,1.),(1.,0.707106781186547,1.,0.707106781186547,1.,
0.707106781186547,1.,0.707106781186547,1.),(1.,0.707106781186547,1.,0.707106781186547,
1.,0.707106781186547,1.,0.707106781186547,1.),(1.,0.707106781186548,1.,
0.707106781186548,1.,0.707106781186548,1.,0.707106781186548,1.),(1.,0.707106781186547,
1.,0.707106781186547,1.,0.707106781186547,1.,0.707106781186547,1.),(1.,
0.707106781186547,1.,0.707106781186547,1.,0.707106781186547,1.,0.707106781186547,
1.),(1.,0.707106781186548,1.,0.707106781186548,1.,0.707106781186548,1.,
0.707106781186548,1.),(1.,0.707106781186548,1.,0.707106781186548,1.,0.707106781186548,
1.,0.707106781186548,1.)))
REPRESENTATION_ITEM('')
SURFACE()
) ;
#66 = (
BOUNDED_SURFACE()
B_SPLINE_SURFACE(2,3,((#194404,#194405,#194406,#194407,#194408,#194409,
#194410),(#194411,#194412,#194413,#194414,#194415,#194416,#194417),(#194418,
#194419,#194420,#194421,#194422,#194423,#194424),(#194425,#194426,#194427,
#194428,#194429,#194430,#194431),(#194432,#194433,#194434,#194435,#194436,
#194437,#194438),(#194439,#194440,#194441,#194442,#194443,#194444,#194445),
(#194446,#194447,#194448,#194449,#194450,#194451,#194452),(#194453,#194454,
#194455,#194456,#194457,#194458,#194459),(#194460,#194461,#194462,#194463,
#194464,#194465,#194466)),.UNSPECIFIED.,.T.,.F.,.F.)
B_SPLINE_SURFACE_WITH_KNOTS((3,2,2,2,3),(4,1,1,1,4),(0.,0.117809724509617,
0.235619449019234,0.353429173528852,0.471238898038469),(0.,0.0911446219616379,
0.182289243923276,0.273433865884915,0.364578487846551),.UNSPECIFIED.)
GEOMETRIC_REPRESENTATION_ITEM()
RATIONAL_B_SPLINE_SURFACE(((1.,1.,1.,1.,1.,1.,1.),(0.707106781186548,0.707106781186548,
0.707106781186547,0.707106781186548,0.707106781186547,0.707106781186548,
0.707106781186548),(1.,1.,1.,1.,1.,1.,1.),(0.707106781186548,0.707106781186548,
0.707106781186547,0.707106781186548,0.707106781186547,0.707106781186548,
0.707106781186548),(1.,1.,1.,1.,1.,1.,1.),(0.707106781186548,0.707106781186548,
0.707106781186547,0.707106781186548,0.707106781186547,0.707106781186548,
0.707106781186548),(1.,1.,1.,1.,1.,1.,1.),(0.707106781186548,0.707106781186548,
0.707106781186547,0.707106781186548,0.707106781186547,0.707106781186548,
0.707106781186548),(1.,1.,1.,1.,1.,1.,1.)))
REPRESENTATION_ITEM('')
SURFACE()
) ;
#67 = (
BOUNDED_SURFACE()
B_SPLINE_SURFACE(2,3,((#194476,#194477,#194478,#194479),(#194480,#194481,
#194482,#194483),(#194484,#194485,#194486,#194487),(#194488,#194489,#194490,
#194491),(#194492,#194493,#194494,#194495),(#194496,#194497,#194498,#194499),
(#194500,#194501,#194502,#194503),(#194504,#194505,#194506,#194507),(#194508,
#194509,#194510,#194511)),.UNSPECIFIED.,.T.,.F.,.F.)
B_SPLINE_SURFACE_WITH_KNOTS((3,2,2,2,3),(4,4),(0.,0.117809724509617,0.235619449019234,
0.353429173528852,0.471238898038469),(0.,1.1454147408364),.UNSPECIFIED.)
GEOMETRIC_REPRESENTATION_ITEM()
RATIONAL_B_SPLINE_SURFACE(((1.,1.,1.,1.),(0.707106781186548,0.707106781186548,
0.707106781186547,0.707106781186548),(1.,1.,1.,1.),(0.707106781186548,0.707106781186548,
0.707106781186547,0.707106781186548),(1.,1.,1.,1.),(0.707106781186548,0.707106781186548,
0.707106781186547,0.707106781186548),(1.,1.,1.,1.),(0.707106781186548,0.707106781186548,
0.707106781186547,0.707106781186548),(1.,1.,1.,1.)))
REPRESENTATION_ITEM('')
SURFACE()
) ;
#68 = (
BOUNDED_SURFACE()
B_SPLINE_SURFACE(2,3,((#194519,#194520,#194521,#194522,#194523,#194524,
#194525,#194526,#194527,#194528,#194529,#194530,#194531,#194532,#194533,
#194534,#194535,#194536,#194537),(#194538,#194539,#194540,#194541,#194542,
#194543,#194544,#194545,#194546,#194547,#194548,#194549,#194550,#194551,
#194552,#194553,#194554,#194555,#194556),(#194557,#194558,#194559,#194560,
#194561,#194562,#194563,#194564,#194565,#194566,#194567,#194568,#194569,
#194570,#194571,#194572,#194573,#194574,#194575),(#194576,#194577,#194578,
#194579,#194580,#194581,#194582,#194583,#194584,#194585,#194586,#194587,
#194588,#194589,#194590,#194591,#194592,#194593,#194594),(#194595,#194596,
#194597,#194598,#194599,#194600,#194601,#194602,#194603,#194604,#194605,
#194606,#194607,#194608,#194609,#194610,#194611,#194612,#194613),(#194614,
#194615,#194616,#194617,#194618,#194619,#194620,#194621,#194622,#194623,
#194624,#194625,#194626,#194627,#194628,#194629,#194630,#194631,#194632),
(#194633,#194634,#194635,#194636,#194637,#194638,#194639,#194640,#194641,
#194642,#194643,#194644,#194645,#194646,#194647,#194648,#194649,#194650,
#194651),(#194652,#194653,#194654,#194655,#194656,#194657,#194658,#194659,
#194660,#194661,#194662,#194663,#194664,#194665,#194666,#194667,#194668,
#194669,#194670),(#194671,#194672,#194673,#194674,#194675,#194676,#194677,
#194678,#194679,#194680,#194681,#194682,#194683,#194684,#194685,#194686,
#194687,#194688,#194689)),.UNSPECIFIED.,.T.,.F.,.F.)
B_SPLINE_SURFACE_WITH_KNOTS((3,2,2,2,3),(4,1,1,1,1,1,1,1,1,1,1,1,1,1,1,
1,4),(0.,0.117809724509617,0.235619449019234,0.353429173528852,0.471238898038469),
(0.,0.226732296973331,0.464902013928651,0.70307173088397,0.9298040278573,
1.15653632483063,1.39470604178595,1.63287575874127,1.8596080557146,2.08634035268793,
2.32451006964325,2.56267978659857,2.7894120835719,3.01614438054523,3.25431409750055,
3.49248381445586,3.7192161114292),.UNSPECIFIED.)
GEOMETRIC_REPRESENTATION_ITEM()
RATIONAL_B_SPLINE_SURFACE(((1.,1.,1.,1.,1.,1.,1.,1.,1.,1.,1.,1.,1.,1.,1.,
1.,1.,1.,1.),(0.707106781186548,0.707106781186547,0.707106781186548,0.707106781186547,
0.707106781186548,0.707106781186547,0.707106781186548,0.707106781186547,
0.707106781186547,0.707106781186547,0.707106781186548,0.707106781186547,
0.707106781186547,0.707106781186547,0.707106781186547,0.707106781186547,
0.707106781186548,0.707106781186547,0.707106781186548),(1.,1.,1.,1.,1.,
1.,1.,1.,1.,1.,1.,1.,1.,1.,1.,1.,1.,1.,1.),(0.707106781186548,0.707106781186547,
0.707106781186548,0.707106781186547,0.707106781186548,0.707106781186547,
0.707106781186548,0.707106781186547,0.707106781186547,0.707106781186547,
0.707106781186548,0.707106781186547,0.707106781186547,0.707106781186547,
0.707106781186547,0.707106781186547,0.707106781186548,0.707106781186547,
0.707106781186548),(1.,1.,1.,1.,1.,1.,1.,1.,1.,1.,1.,1.,1.,1.,1.,1.,1.,
1.,1.),(0.707106781186548,0.707106781186547,0.707106781186548,0.707106781186547,
0.707106781186548,0.707106781186547,0.707106781186548,0.707106781186547,
0.707106781186547,0.707106781186547,0.707106781186548,0.707106781186547,
0.707106781186547,0.707106781186547,0.707106781186547,0.707106781186547,
0.707106781186548,0.707106781186547,0.707106781186548),(1.,1.,1.,1.,1.,
1.,1.,1.,1.,1.,1.,1.,1.,1.,1.,1.,1.,1.,1.),(0.707106781186548,0.707106781186547,
0.707106781186548,0.707106781186547,0.707106781186548,0.707106781186547,
0.707106781186548,0.707106781186547,0.707106781186547,0.707106781186547,
0.707106781186548,0.707106781186547,0.707106781186547,0.707106781186547,
0.707106781186547,0.707106781186547,0.707106781186548,0.707106781186547,
0.707106781186548),(1.,1.,1.,1.,1.,1.,1.,1.,1.,1.,1.,1.,1.,1.,1.,1.,1.,
1.,1.)))
REPRESENTATION_ITEM('')
SURFACE()
) ;
#69 = (
BOUNDED_SURFACE()
B_SPLINE_SURFACE(2,1,((#194720,#194721),(#194722,#194723),(#194724,#194725)),
 .UNSPECIFIED.,.F.,.F.,.F.)
B_SPLINE_SURFACE_WITH_KNOTS((3,3),(2,2),(-66.4194892732842,-6.49328858992507),
(0.,0.36),.UNSPECIFIED.)
GEOMETRIC_REPRESENTATION_ITEM()
RATIONAL_B_SPLINE_SURFACE(((1.,1.),(0.999060551236508,0.999060551236508),
(1.,1.)))
REPRESENTATION_ITEM('')
SURFACE()
) ;
#70 = (
BOUNDED_SURFACE()
B_SPLINE_SURFACE(2,1,((#194797,#194798),(#194799,#194800),(#194801,#194802)),
 .UNSPECIFIED.,.F.,.F.,.F.)
B_SPLINE_SURFACE_WITH_KNOTS((3,3),(2,2),(47.1134450647953,104.780247485259),
(0.,0.36),.UNSPECIFIED.)
GEOMETRIC_REPRESENTATION_ITEM()
RATIONAL_B_SPLINE_SURFACE(((1.,1.),(0.998981521269156,0.998981521269156),
(1.,1.)))
REPRESENTATION_ITEM('')
SURFACE()
) ;
#71 = (
BOUNDED_SURFACE()
B_SPLINE_SURFACE(2,1,((#194862,#194863),(#194864,#194865),(#194866,#194867),
(#194868,#194869),(#194870,#194871)),.UNSPECIFIED.,.F.,.F.,.F.)
B_SPLINE_SURFACE_WITH_KNOTS((3,2,3),(2,2),(-88.8644935634662,-88.8637621488937,
-87.3177026764144),(0.,0.72),.UNSPECIFIED.)
GEOMETRIC_REPRESENTATION_ITEM()
RATIONAL_B_SPLINE_SURFACE(((1.,1.),(1.00013629089276,1.00013629089276),
(1.0002727088269,1.0002727088269),(0.711913347097769,0.711913347097769),
(0.991190559346467,0.991190559346467)))
REPRESENTATION_ITEM('')
SURFACE()
) ;
#72 = (
BOUNDED_SURFACE()
B_SPLINE_SURFACE(2,1,((#194889,#194890),(#194891,#194892),(#194893,#194894),
(#194895,#194896),(#194897,#194898)),.UNSPECIFIED.,.F.,.F.,.F.)
B_SPLINE_SURFACE_WITH_KNOTS((3,2,3),(2,2),(-82.6275148008652,-82.6267833862927,
-81.0807239138134),(0.,0.720000000000001),.UNSPECIFIED.)
GEOMETRIC_REPRESENTATION_ITEM()
RATIONAL_B_SPLINE_SURFACE(((0.991190559346467,0.991190559346467),(0.991325649592695,
0.991325649592695),(0.991460865761138,0.991460865761138),(0.705641788716053,
0.705641788716053),(0.982458724937563,0.982458724937563)))
REPRESENTATION_ITEM('')
SURFACE()
) ;
#73 = (
BOUNDED_SURFACE()
B_SPLINE_SURFACE(2,1,((#194916,#194917),(#194918,#194919),(#194920,#194921),
(#194922,#194923),(#194924,#194925)),.UNSPECIFIED.,.F.,.F.,.F.)
B_SPLINE_SURFACE_WITH_KNOTS((3,2,3),(2,2),(-76.3905360382642,-76.3898046236916,
-74.8437451512123),(0.,0.720000000000001),.UNSPECIFIED.)
GEOMETRIC_REPRESENTATION_ITEM()
RATIONAL_B_SPLINE_SURFACE(((0.982458724937563,0.982458724937563),(0.982592625114284,
0.982592625114284),(0.982726650103915,0.982726650103915),(0.699425479255707,
0.699425479255707),(0.97380381310568,0.97380381310568)))
REPRESENTATION_ITEM('')
SURFACE()
) ;
#74 = (
BOUNDED_SURFACE()
B_SPLINE_SURFACE(2,1,((#194943,#194944),(#194945,#194946),(#194947,#194948),
(#194949,#194950),(#194951,#194952)),.UNSPECIFIED.,.F.,.F.,.F.)
B_SPLINE_SURFACE_WITH_KNOTS((3,2,3),(2,2),(-70.1535572756631,-70.1528258610906,
-68.6067663886113),(0.,0.720000000000001),.UNSPECIFIED.)
GEOMETRIC_REPRESENTATION_ITEM()
RATIONAL_B_SPLINE_SURFACE(((0.97380381310568,0.97380381310568),(0.97393653369674,
0.97393653369674),(0.974069378001179,0.974069378001179),(0.693263932004635,
0.693263932004635),(0.965225146205942,0.965225146205942)))
REPRESENTATION_ITEM('')
SURFACE()
) ;
#75 = (
BOUNDED_SURFACE()
B_SPLINE_SURFACE(2,1,((#194970,#194971),(#194972,#194973),(#194974,#194975),
(#194976,#194977),(#194978,#194979)),.UNSPECIFIED.,.F.,.F.,.F.)
B_SPLINE_SURFACE_WITH_KNOTS((3,2,3),(2,2),(-63.9165785130621,-63.9158470984896,
-62.3697876260103),(0.,0.72),.UNSPECIFIED.)
GEOMETRIC_REPRESENTATION_ITEM()
RATIONAL_B_SPLINE_SURFACE(((0.965225146205942,0.965225146205942),(0.965356697602832,
0.965356697602832),(0.965488371623255,0.965488371623255),(0.687156664538405,
0.687156664538405),(0.956722052563143,0.956722052563143)))
REPRESENTATION_ITEM('')
SURFACE()
) ;
#76 = (
BOUNDED_SURFACE()
B_SPLINE_SURFACE(2,1,((#194997,#194998),(#194999,#195000),(#195001,#195002),
(#195003,#195004),(#195005,#195006)),.UNSPECIFIED.,.F.,.F.,.F.)
B_SPLINE_SURFACE_WITH_KNOTS((3,2,3),(2,2),(-57.6795997504611,-57.6788683358886,
-56.1328088634093),(0.,0.720000000000001),.UNSPECIFIED.)
GEOMETRIC_REPRESENTATION_ITEM()
RATIONAL_B_SPLINE_SURFACE(((0.956722052563143,0.956722052563143),(0.956852445065809,
0.956852445065809),(0.956982959111764,0.956982959111764),(0.681103198682475,
0.681103198682475),(0.948293866419162,0.948293866419162)))
REPRESENTATION_ITEM('')
SURFACE()
) ;
#77 = (
BOUNDED_SURFACE()
B_SPLINE_SURFACE(2,1,((#195024,#195025),(#195026,#195027),(#195028,#195029),
(#195030,#195031),(#195032,#195033)),.UNSPECIFIED.,.F.,.F.,.F.)
B_SPLINE_SURFACE_WITH_KNOTS((3,2,3),(2,2),(-51.4426209878601,-51.4418895732875,
-49.8958301008082),(0.,0.720000000000001),.UNSPECIFIED.)
GEOMETRIC_REPRESENTATION_ITEM()
RATIONAL_B_SPLINE_SURFACE(((0.948293866419162,0.948293866419162),(0.948423110236814,
0.948423110236814),(0.948552474527026,0.948552474527026),(0.67510306047475,
0.67510306047475),(0.939939927880833,0.939939927880833)))
REPRESENTATION_ITEM('')
SURFACE()
) ;
#78 = (
BOUNDED_SURFACE()
B_SPLINE_SURFACE(2,1,((#195051,#195052),(#195053,#195054),(#195055,#195056),
(#195057,#195058),(#195059,#195060)),.UNSPECIFIED.,.F.,.F.,.F.)
B_SPLINE_SURFACE_WITH_KNOTS((3,2,3),(2,2),(-45.205642225259,-45.2049108106865,
-43.6588513382072),(0.,0.72),.UNSPECIFIED.)
GEOMETRIC_REPRESENTATION_ITEM()
RATIONAL_B_SPLINE_SURFACE(((0.939939927880833,0.939939927880833),(0.940068033132744,
0.940068033132744),(0.940196257795919,0.940196257795919),(0.66915578012848,
0.66915578012848),(0.931659582868281,0.931659582868281)))
REPRESENTATION_ITEM('')
SURFACE()
) ;
#79 = (
BOUNDED_SURFACE()
B_SPLINE_SURFACE(2,1,((#195078,#195079),(#195080,#195081),(#195082,#195083),
(#195084,#195085),(#195086,#195087)),.UNSPECIFIED.,.F.,.F.,.F.)
B_SPLINE_SURFACE_WITH_KNOTS((3,2,3),(2,2),(-38.968663462658,-38.9679320480855,
-37.4218725756062),(0.,0.720000000000001),.UNSPECIFIED.)
GEOMETRIC_REPRESENTATION_ITEM()
RATIONAL_B_SPLINE_SURFACE(((0.931659582868281,0.931659582868281),(0.931786559584578,
0.931786559584578),(0.931913654660192,0.931913654660192),(0.663260891995469,
0.663260891995469),(0.923452183063708,0.923452183063708)))
REPRESENTATION_ITEM('')
SURFACE()
) ;
#80 = (
BOUNDED_SURFACE()
B_SPLINE_SURFACE(2,1,((#195105,#195106),(#195107,#195108),(#195109,#195110),
(#195111,#195112),(#195113,#195114)),.UNSPECIFIED.,.F.,.F.,.F.)
B_SPLINE_SURFACE_WITH_KNOTS((3,2,3),(2,2),(-32.731684700057,-32.7309532854845,
-31.1848938130052),(0.,0.720000000000001),.UNSPECIFIED.)
GEOMETRIC_REPRESENTATION_ITEM()
RATIONAL_B_SPLINE_SURFACE(((0.923452183063708,0.923452183063708),(0.923578041186158,
0.923578041186158),(0.923704016625246,0.923704016625246),(0.657417934529626,
0.657417934529626),(0.915317085860633,0.915317085860633)))
REPRESENTATION_ITEM('')
SURFACE()
) ;
#81 = (
BOUNDED_SURFACE()
B_SPLINE_SURFACE(2,1,((#195132,#195133),(#195134,#195135),(#195136,#195137),
(#195138,#195139),(#195140,#195141)),.UNSPECIFIED.,.F.,.F.,.F.)
B_SPLINE_SURFACE_WITH_KNOTS((3,2,3),(2,2),(-26.4947059374559,-26.4939745228834,
-24.9479150504041),(0.,0.720000000000004),.UNSPECIFIED.)
GEOMETRIC_REPRESENTATION_ITEM()
RATIONAL_B_SPLINE_SURFACE(((0.915317085860633,0.915317085860633),(0.915441835243423,
0.915441835243423),(0.915566700909357,0.915566700909357),(0.651626450250819,
0.651626450250819),(0.907253654313579,0.907253654313579)))
REPRESENTATION_ITEM('')
SURFACE()
) ;
#82 = (
BOUNDED_SURFACE()
B_SPLINE_SURFACE(2,1,((#195159,#195160),(#195161,#195162),(#195163,#195164),
(#195165,#195166),(#195167,#195168)),.UNSPECIFIED.,.F.,.F.,.F.)
B_SPLINE_SURFACE_WITH_KNOTS((3,2,3),(2,2),(-20.2577271748549,-20.2569957602824,
-18.7109362878031),(0.,0.720000000000001),.UNSPECIFIED.)
GEOMETRIC_REPRESENTATION_ITEM()
RATIONAL_B_SPLINE_SURFACE(((0.907253654313579,0.907253654313579),(0.907377304724085,
0.907377304724085),(0.907501070393345,0.907501070393345),(0.645885985709063,
0.645885985709063),(0.899261257088203,0.899261257088203)))
REPRESENTATION_ITEM('')
SURFACE()
) ;
#83 = (
BOUNDED_SURFACE()
B_SPLINE_SURFACE(2,1,((#195186,#195187),(#195188,#195189),(#195190,#195191),
(#195192,#195193),(#195194,#195195)),.UNSPECIFIED.,.F.,.F.,.F.)
B_SPLINE_SURFACE_WITH_KNOTS((3,2,3),(2,2),(-14.0207484122539,-14.0200169976814,
-12.4739575252021),(0.,0.72),.UNSPECIFIED.)
GEOMETRIC_REPRESENTATION_ITEM()
RATIONAL_B_SPLINE_SURFACE(((0.899261257088203,0.899261257088203),(0.899383818207756,
0.899383818207756),(0.899506493570697,0.899506493570697),(0.64019609144901,
0.64019609144901),(0.891339268411863,0.891339268411863)))
REPRESENTATION_ITEM('')
SURFACE()
) ;
#84 = (
BOUNDED_SURFACE()
B_SPLINE_SURFACE(2,1,((#195213,#195214),(#195215,#195216),(#195217,#195218),
(#195219,#195220),(#195221,#195222)),.UNSPECIFIED.,.F.,.F.,.F.)
B_SPLINE_SURFACE_WITH_KNOTS((3,2,3),(2,2),(-7.78376964965284,-7.78303823508033,
-6.23697876260103),(0.,0.72),.UNSPECIFIED.)
GEOMETRIC_REPRESENTATION_ITEM()
RATIONAL_B_SPLINE_SURFACE(((0.891339268411863,0.891339268411863),(0.891460749836507,
0.891460749836507),(0.891582344498119,0.891582344498119),(0.634556321974766,
0.634556321974766),(0.883487068024626,0.883487068024626)))
REPRESENTATION_ITEM('')
SURFACE()
) ;
#85 = (
BOUNDED_SURFACE()
B_SPLINE_SURFACE(2,1,((#195240,#195241),(#195242,#195243),(#195244,#195245),
(#195246,#195247),(#195248,#195249)),.UNSPECIFIED.,.F.,.F.,.F.)
B_SPLINE_SURFACE_WITH_KNOTS((3,2,3),(2,2),(-1.54679088705182,-1.54605947247931,
0.),(0.,0.72),.UNSPECIFIED.)
GEOMETRIC_REPRESENTATION_ITEM()
RATIONAL_B_SPLINE_SURFACE(((0.883487068024626,0.883487068024626),(0.883607479265868,
0.883607479265868),(0.883728002746525,0.883728002746525),(0.628966235715006,
0.628966235715006),(0.875704041130699,0.875704041130699)))
REPRESENTATION_ITEM('')
SURFACE()
) ;
#86 = (
BOUNDED_SURFACE()
B_SPLINE_SURFACE(2,1,((#195267,#195268),(#195269,#195270),(#195271,#195272),
(#195273,#195274),(#195275,#195276)),.UNSPECIFIED.,.F.,.F.,.F.)
B_SPLINE_SURFACE_WITH_KNOTS((3,2,3),(2,2),(4.69018787554921,4.69091929012172,
6.23697876260103),(0.,0.72),.UNSPECIFIED.)
GEOMETRIC_REPRESENTATION_ITEM()
RATIONAL_B_SPLINE_SURFACE(((0.875704041130699,0.875704041130699),(0.875823391616258,
0.875823391616258),(0.875942853352465,0.875942853352465),(0.623425394988399,
0.623425394988399),(0.8679895783503,0.8679895783503)))
REPRESENTATION_ITEM('')
SURFACE()
) ;
#87 = (
BOUNDED_SURFACE()
B_SPLINE_SURFACE(2,1,((#195294,#195295),(#195296,#195297),(#195298,#195299),
(#195300,#195301),(#195302,#195303)),.UNSPECIFIED.,.F.,.F.,.F.)
B_SPLINE_SURFACE_WITH_KNOTS((3,2,3),(2,2),(10.9271666381502,10.9278980527228,
12.4739575252021),(0.,0.72),.UNSPECIFIED.)
GEOMETRIC_REPRESENTATION_ITEM()
RATIONAL_B_SPLINE_SURFACE(((0.8679895783503,0.8679895783503),(0.868107877424839,
0.868107877424839),(0.86822628676997,0.86822628676997),(0.617933365969343,
0.617933365969343),(0.860343075671938,0.860343075671938)))
REPRESENTATION_ITEM('')
SURFACE()
) ;
#88 = (
BOUNDED_SURFACE()
B_SPLINE_SURFACE(2,1,((#195321,#195322),(#195323,#195324),(#195325,#195326),
(#195327,#195328),(#195329,#195330)),.UNSPECIFIED.,.F.,.F.,.F.)
B_SPLINE_SURFACE_WITH_KNOTS((3,2,3),(2,2),(17.1641454007513,17.1648768153238,
18.7109362878031),(0.,0.72),.UNSPECIFIED.)
GEOMETRIC_REPRESENTATION_ITEM()
RATIONAL_B_SPLINE_SURFACE(((0.860343075671938,0.860343075671938),(0.8604603325978,
0.8604603325978),(0.860577698822833,0.860577698822833),(0.612489718653998,
0.612489718653998),(0.852763934405128,0.852763934405128)))
REPRESENTATION_ITEM('')
SURFACE()
) ;
#89 = (
BOUNDED_SURFACE()
B_SPLINE_SURFACE(2,1,((#195348,#195349),(#195350,#195351),(#195352,#195353),
(#195354,#195355),(#195356,#195357)),.UNSPECIFIED.,.F.,.F.,.F.)
B_SPLINE_SURFACE_WITH_KNOTS((3,2,3),(2,2),(23.4011241633523,23.4018555779248,
24.9479150504041),(0.,0.72),.UNSPECIFIED.)
GEOMETRIC_REPRESENTATION_ITEM()
RATIONAL_B_SPLINE_SURFACE(((0.852763934405128,0.852763934405128),(0.852880158363061,
0.852880158363061),(0.8529964906573,0.8529964906573),(0.607094026826617,
0.607094026826617),(0.845251561133513,0.845251561133513)))
REPRESENTATION_ITEM('')
SURFACE()
) ;
#90 = (
BOUNDED_SURFACE()
B_SPLINE_SURFACE(2,1,((#195375,#195376),(#195377,#195378),(#195379,#195380),
(#195381,#195382),(#195383,#195384)),.UNSPECIFIED.,.F.,.F.,.F.)
B_SPLINE_SURFACE_WITH_KNOTS((3,2,3),(2,2),(29.6381029259533,29.6388343405258,
31.1848938130052),(0.,0.72),.UNSPECIFIED.)
GEOMETRIC_REPRESENTATION_ITEM()
RATIONAL_B_SPLINE_SURFACE(((0.845251561133513,0.845251561133513),(0.845366761223386,
0.845366761223386),(0.845482068695182,0.845482068695182),(0.601745868026174,
0.601745868026174),(0.837805367668402,0.837805367668402)))
REPRESENTATION_ITEM('')
SURFACE()
) ;
#91 = (
BOUNDED_SURFACE()
B_SPLINE_SURFACE(2,1,((#195402,#195403),(#195404,#195405),(#195406,#195407),
(#195408,#195409),(#195410,#195411)),.UNSPECIFIED.,.F.,.F.,.F.)
B_SPLINE_SURFACE_WITH_KNOTS((3,2,3),(2,2),(35.8750816885544,35.8758131031269,
37.4218725756062),(0.,0.72),.UNSPECIFIED.)
GEOMETRIC_REPRESENTATION_ITEM()
RATIONAL_B_SPLINE_SURFACE(((0.837805367668402,0.837805367668402),(0.83791955290992,
0.83791955290992),(0.838033844587386,0.838033844587386),(0.596444823513289,
0.596444823513289),(0.830424771002716,0.830424771002716)))
REPRESENTATION_ITEM('')
SURFACE()
) ;
#92 = (
BOUNDED_SURFACE()
B_SPLINE_SURFACE(2,1,((#195429,#195430),(#195431,#195432),(#195433,#195434),
(#195435,#195436),(#195437,#195438)),.UNSPECIFIED.,.F.,.F.,.F.)
B_SPLINE_SURFACE_WITH_KNOTS((3,2,3),(2,2),(42.1120604511554,42.1127918657279,
43.6588513382072),(0.,0.72),.UNSPECIFIED.)
GEOMETRIC_REPRESENTATION_ITEM()
RATIONAL_B_SPLINE_SURFACE(((0.830424771002716,0.830424771002716),(0.830537950336125,
0.830537950336125),(0.830651235167842,0.830651235167842),(0.591190478237442,
0.591190478237442),(0.823109193265344,0.823109193265344)))
REPRESENTATION_ITEM('')
SURFACE()
) ;
#93 = (
BOUNDED_SURFACE()
B_SPLINE_SURFACE(2,1,((#195456,#195457),(#195458,#195459),(#195460,#195461),
(#195462,#195463),(#195464,#195465)),.UNSPECIFIED.,.F.,.F.,.F.)
B_SPLINE_SURFACE_WITH_KNOTS((3,2,3),(2,2),(48.3490392137564,48.3497706283289,
49.8958301008082),(0.,0.72),.UNSPECIFIED.)
GEOMETRIC_REPRESENTATION_ITEM()
RATIONAL_B_SPLINE_SURFACE(((0.823109193265344,0.823109193265344),(0.823221375552132,
0.823221375552132),(0.823333662407847,0.823333662407847),(0.585982420804475,
0.585982420804475),(0.815858061675895,0.815858061675895)))
REPRESENTATION_ITEM('')
SURFACE()
) ;
#94 = (
BOUNDED_SURFACE()
B_SPLINE_SURFACE(2,1,((#195483,#195484),(#195485,#195486),(#195487,#195488),
(#195489,#195490),(#195491,#195492)),.UNSPECIFIED.,.F.,.F.,.F.)
B_SPLINE_SURFACE_WITH_KNOTS((3,2,3),(2,2),(54.5860179763575,54.58674939093,
56.1328088634093),(0.,0.720000000000001),.UNSPECIFIED.)
GEOMETRIC_REPRESENTATION_ITEM()
RATIONAL_B_SPLINE_SURFACE(((0.815858061675895,0.815858061675895),(0.815969255699486,
0.815969255699486),(0.816080553370809,0.816080553370809),(0.580820243444385,
0.580820243444385),(0.808670808499855,0.808670808499855)))
REPRESENTATION_ITEM('')
SURFACE()
) ;
#95 = (
BOUNDED_SURFACE()
B_SPLINE_SURFACE(2,1,((#195510,#195511),(#195512,#195513),(#195514,#195515),
(#195516,#195517),(#195518,#195519)),.UNSPECIFIED.,.F.,.F.,.F.)
B_SPLINE_SURFACE_WITH_KNOTS((3,2,3),(2,2),(60.8229967389585,60.823728153531,
62.3697876260103),(0.,0.720000000000001),.UNSPECIFIED.)
GEOMETRIC_REPRESENTATION_ITEM()
RATIONAL_B_SPLINE_SURFACE(((0.808670808499855,0.808670808499855),(0.808781022966294,
0.808781022966294),(0.808891340167387,0.808891340167387),(0.575703541979391,
0.575703541979391),(0.801546871004132,0.801546871004132)))
REPRESENTATION_ITEM('')
SURFACE()
) ;
#96 = (
BOUNDED_SURFACE()
B_SPLINE_SURFACE(2,1,((#195537,#195538),(#195539,#195540),(#195541,#195542),
(#195543,#195544),(#195545,#195546)),.UNSPECIFIED.,.F.,.F.,.F.)
B_SPLINE_SURFACE_WITH_KNOTS((3,2,3),(2,2),(67.0599755015595,67.060706916132,
68.6067663886113),(0.,0.72),.UNSPECIFIED.)
GEOMETRIC_REPRESENTATION_ITEM()
RATIONAL_B_SPLINE_SURFACE(((0.801546871004132,0.801546871004132),(0.801656114542769,
0.801656114542769),(0.801765459911026,0.801765459911026),(0.570631915792295,
0.570631915792295),(0.794485691412996,0.794485691412996)))
REPRESENTATION_ITEM('')
SURFACE()
) ;
#97 = (
BOUNDED_SURFACE()
B_SPLINE_SURFACE(2,1,((#195564,#195565),(#195566,#195567),(#195568,#195569),
(#195570,#195571),(#195572,#195573)),.UNSPECIFIED.,.F.,.F.,.F.)
B_SPLINE_SURFACE_WITH_KNOTS((3,2,3),(2,2),(73.2969542641605,73.2976856787331,
74.8437451512124),(0.,0.720000000000001),.UNSPECIFIED.)
GEOMETRIC_REPRESENTATION_ITEM()
RATIONAL_B_SPLINE_SURFACE(((0.794485691412996,0.794485691412996),(0.794593972577163,
0.794593972577163),(0.794702354673887,0.794702354673887),(0.565604967795111,
0.565604967795111),(0.787486716864412,0.787486716864412)))
REPRESENTATION_ITEM('')
SURFACE()
) ;
#98 = (
BOUNDED_SURFACE()
B_SPLINE_SURFACE(2,1,((#195591,#195592),(#195593,#195594),(#195595,#195596),
(#195597,#195598),(#195599,#195600)),.UNSPECIFIED.,.F.,.F.,.F.)
B_SPLINE_SURFACE_WITH_KNOTS((3,2,3),(2,2),(79.5339330267616,79.5346644413341,
81.0807239138134),(0.,0.72),.UNSPECIFIED.)
GEOMETRIC_REPRESENTATION_ITEM()
RATIONAL_B_SPLINE_SURFACE(((0.787486716864412,0.787486716864412),(0.78759404413209,
0.78759404413209),(0.787701471443165,0.787701471443165),(0.560622304397977,
0.560622304397977),(0.78054939936675,0.78054939936675)))
REPRESENTATION_ITEM('')
SURFACE()
) ;
#99 = (
BOUNDED_SURFACE()
B_SPLINE_SURFACE(2,1,((#195618,#195619),(#195620,#195621),(#195622,#195623),
(#195624,#195625),(#195626,#195627)),.UNSPECIFIED.,.F.,.F.,.F.)
B_SPLINE_SURFACE_WITH_KNOTS((3,2,3),(2,2),(85.7709117893626,85.7716432039351,
87.3177026764144),(0.,0.72),.UNSPECIFIED.)
GEOMETRIC_REPRESENTATION_ITEM()
RATIONAL_B_SPLINE_SURFACE(((0.78054939936675,0.78054939936675),(0.780655781141232,
0.780655781141232),(0.780762262077786,0.780762262077786),(0.555683535478336,
0.555683535478336),(0.773673195755878,0.773673195755878)))
REPRESENTATION_ITEM('')
SURFACE()
) ;
#100 = (
BOUNDED_SURFACE()
B_SPLINE_SURFACE(2,1,((#195645,#195646),(#195647,#195648),(#195649,#195650),
(#195651,#195652),(#195653,#195654)),.UNSPECIFIED.,.F.,.F.,.F.)
B_SPLINE_SURFACE_WITH_KNOTS((3,2,3),(2,2),(92.0078905519636,92.0086219665361,
93.5546814390155),(0.,0.720000000000001),.UNSPECIFIED.)
GEOMETRIC_REPRESENTATION_ITEM()
RATIONAL_B_SPLINE_SURFACE(((0.773673195755878,0.773673195755878),(0.773778640366431,
0.773778640366431),(0.773884183265494,0.773884183265494),(0.550788274350394,
0.550788274350394),(0.766857567652637,0.766857567652637)))
REPRESENTATION_ITEM('')
SURFACE()
) ;
#101 = (
BOUNDED_SURFACE()
B_SPLINE_SURFACE(2,1,((#195672,#195673),(#195674,#195675),(#195676,#195677),
(#195678,#195679),(#195680,#195681)),.UNSPECIFIED.,.F.,.F.,.F.)
B_SPLINE_SURFACE_WITH_KNOTS((3,2,3),(2,2),(98.2448693145647,98.2456007291372,
99.7916602016165),(0.,0.720000000000001),.UNSPECIFIED.)
GEOMETRIC_REPRESENTATION_ITEM()
RATIONAL_B_SPLINE_SURFACE(((0.766857567652637,0.766857567652637),(0.766962083355152,
0.766962083355152),(0.767066696480309,0.767066696480309),(0.545936137734843,
0.545936137734843),(0.760101981420689,0.760101981420689)))
REPRESENTATION_ITEM('')
SURFACE()
) ;
#102 = (
BOUNDED_SURFACE()
B_SPLINE_SURFACE(2,1,((#195699,#195700),(#195701,#195702),(#195703,#195704),
(#195705,#195706),(#195707,#195708)),.UNSPECIFIED.,.F.,.F.,.F.)
B_SPLINE_SURFACE_WITH_KNOTS((3,2,3),(2,2),(104.481848077166,104.482579491738,
106.028638964218),(0.,0.720000000000001),.UNSPECIFIED.)
GEOMETRIC_REPRESENTATION_ITEM()
RATIONAL_B_SPLINE_SURFACE(((0.760101981420689,0.760101981420689),(0.760205576398325,
0.760205576398325),(0.760309267940364,0.760309267940364),(0.541126745728849,
0.541126745728849),(0.753405908124731,0.753405908124731)))
REPRESENTATION_ITEM('')
SURFACE()
) ;
#103 = (
BOUNDED_SURFACE()
B_SPLINE_SURFACE(2,1,((#195726,#195727),(#195728,#195729),(#195730,#195731),
(#195732,#195733),(#195734,#195735)),.UNSPECIFIED.,.F.,.F.,.F.)
B_SPLINE_SURFACE_WITH_KNOTS((3,2,3),(2,2),(110.718826839767,110.719558254339,
112.265617726819),(0.,0.720000000000001),.UNSPECIFIED.)
GEOMETRIC_REPRESENTATION_ITEM()
RATIONAL_B_SPLINE_SURFACE(((0.753405908124731,0.753405908124731),(0.753508590488559,
0.753508590488559),(0.753611368566113,0.753611368566113),(0.536359721776312,
0.536359721776312),(0.746768823489085,0.746768823489085)))
REPRESENTATION_ITEM('')
SURFACE()
) ;
#104 = (
BOUNDED_SURFACE()
B_SPLINE_SURFACE(2,1,((#195753,#195754),(#195755,#195756),(#195757,#195758),
(#195759,#195760),(#195761,#195762)),.UNSPECIFIED.,.F.,.F.,.F.)
B_SPLINE_SURFACE_WITH_KNOTS((3,2,3),(2,2),(116.955805602368,116.95653701694,
118.50259648942),(0.,0.720000000000001),.UNSPECIFIED.)
GEOMETRIC_REPRESENTATION_ITEM()
RATIONAL_B_SPLINE_SURFACE(((0.746768823489085,0.746768823489085),(0.746870601278723,
0.746870601278723),(0.746972473938902,0.746972473938902),(0.531634692638378,
0.531634692638378),(0.74019020785665,0.74019020785665)))
REPRESENTATION_ITEM('')
SURFACE()
) ;
#105 = (
BOUNDED_SURFACE()
B_SPLINE_SURFACE(2,1,((#195780,#195781),(#195782,#195783),(#195784,#195785),
(#195786,#195787),(#195788,#195789)),.UNSPECIFIED.,.F.,.F.,.F.)
B_SPLINE_SURFACE_WITH_KNOTS((3,2,3),(2,2),(123.192784364969,123.193515779541,
124.739575252021),(0.,0.720000000000001),.UNSPECIFIED.)
GEOMETRIC_REPRESENTATION_ITEM()
RATIONAL_B_SPLINE_SURFACE(((0.74019020785665,0.74019020785665),(0.74029108904089,
0.74029108904089),(0.740392064259915,0.740392064259915),(0.526951288364221,
0.526951288364221),(0.73366954614821,0.73366954614821)))
REPRESENTATION_ITEM('')
SURFACE()
) ;
#106 = (
BOUNDED_SURFACE()
B_SPLINE_SURFACE(2,1,((#195807,#195808),(#195809,#195810),(#195811,#195812),
(#195813,#195814),(#195815,#195816)),.UNSPECIFIED.,.F.,.F.,.F.)
B_SPLINE_SURFACE_WITH_KNOTS((3,2,3),(2,2),(129.42976312757,129.430494542142,
130.976554014622),(0.,0.720000000000003),.UNSPECIFIED.)
GEOMETRIC_REPRESENTATION_ITEM()
RATIONAL_B_SPLINE_SURFACE(((0.73366954614821,0.73366954614821),(0.733769538625645,
0.733769538625645),(0.73386962430947,0.73386962430947),(0.522309142262074,
0.522309142262074),(0.727206327822113,0.727206327822113)))
REPRESENTATION_ITEM('')
SURFACE()
) ;
#107 = (
BOUNDED_SURFACE()
B_SPLINE_SURFACE(2,1,((#195834,#195835),(#195836,#195837),(#195838,#195839),
(#195840,#195841),(#195842,#195843)),.UNSPECIFIED.,.F.,.F.,.F.)
B_SPLINE_SURFACE_WITH_KNOTS((3,2,3),(2,2),(135.666741890171,135.667473304743,
137.213532777223),(0.,0.72),.UNSPECIFIED.)
GEOMETRIC_REPRESENTATION_ITEM()
RATIONAL_B_SPLINE_SURFACE(((0.727206327822113,0.727206327822113),(0.727305439421753,
0.727305439421753),(0.727404643406686,0.727404643406686),(0.517707890870518,
0.517707890870518),(0.720800046834291,0.720800046834291)))
REPRESENTATION_ITEM('')
SURFACE()
) ;
#108 = (
BOUNDED_SURFACE()
B_SPLINE_SURFACE(2,1,((#195861,#195862),(#195863,#195864),(#195865,#195866),
(#195867,#195868),(#195869,#195870)),.UNSPECIFIED.,.F.,.F.,.F.)
B_SPLINE_SURFACE_WITH_KNOTS((3,2,3),(2,2),(141.903720652772,141.904452067344,
143.450511539824),(0.,0.72),.UNSPECIFIED.)
GEOMETRIC_REPRESENTATION_ITEM()
RATIONAL_B_SPLINE_SURFACE(((0.720800046834291,0.720800046834291),(0.720898285316175,
0.720898285316175),(0.72099661536949,0.72099661536949),(0.513147173930029,
0.513147173930029),(0.714450201598641,0.714450201598641)))
REPRESENTATION_ITEM('')
SURFACE()
) ;
#109 = (
BOUNDED_SURFACE()
B_SPLINE_SURFACE(2,1,((#195888,#195889),(#195890,#195891),(#195892,#195893),
(#195894,#195895),(#195896,#195897)),.UNSPECIFIED.,.F.,.F.,.F.)
B_SPLINE_SURFACE_WITH_KNOTS((3,2,3),(2,2),(148.140699415373,148.141430829945,
149.687490302425),(0.,0.72),.UNSPECIFIED.)
GEOMETRIC_REPRESENTATION_ITEM()
RATIONAL_B_SPLINE_SURFACE(((0.714450201598641,0.714450201598641),(0.714547574654449,
0.714547574654449),(0.714645038474995,0.714645038474995),(0.508626634354764,
0.508626634354764),(0.708156294947753,0.708156294947753)))
REPRESENTATION_ITEM('')
SURFACE()
) ;
#110 = (
BOUNDED_SURFACE()
B_SPLINE_SURFACE(2,1,((#195915,#195916),(#195917,#195918),(#195919,#195920),
(#195921,#195922),(#195923,#195924)),.UNSPECIFIED.,.F.,.F.,.F.)
B_SPLINE_SURFACE_WITH_KNOTS((3,2,3),(2,2),(154.377678177974,154.378409592546,
155.924469065026),(0.,0.72),.UNSPECIFIED.)
GEOMETRIC_REPRESENTATION_ITEM()
RATIONAL_B_SPLINE_SURFACE(((0.708156294947753,0.708156294947753),(0.708252810201405,
0.708252810201405),(0.708349415420208,0.708349415420208),(0.50414591820461,
0.50414591820461),(0.701917834093985,0.701917834093985)))
REPRESENTATION_ITEM('')
SURFACE()
) ;
#111 = (
BOUNDED_SURFACE()
B_SPLINE_SURFACE(2,1,((#195942,#195943),(#195944,#195945),(#195946,#195947),
(#195948,#195949),(#195950,#195951)),.UNSPECIFIED.,.F.,.F.,.F.)
B_SPLINE_SURFACE_WITH_KNOTS((3,2,3),(2,2),(160.614656940575,160.615388355147,
162.161447827627),(0.,0.72),.UNSPECIFIED.)
GEOMETRIC_REPRESENTATION_ITEM()
RATIONAL_B_SPLINE_SURFACE(((0.701917834093985,0.701917834093985),(0.702013499102238,
0.702013499102238),(0.702109253283099,0.702109253283099),(0.499704674657466,
0.499704674657466),(0.695734330590878,0.695734330590878)))
REPRESENTATION_ITEM('')
SURFACE()
) ;
#112 = (
BOUNDED_SURFACE()
B_SPLINE_SURFACE(2,1,((#195969,#195970),(#195971,#195972),(#195973,#195974),
(#195975,#195976),(#195977,#195978)),.UNSPECIFIED.,.F.,.F.,.F.)
B_SPLINE_SURFACE_WITH_KNOTS((3,2,3),(2,2),(166.851635703176,166.852367117749,
168.398426590228),(0.,0.720000000000001),.UNSPECIFIED.)
GEOMETRIC_REPRESENTATION_ITEM()
RATIONAL_B_SPLINE_SURFACE(((0.695734330590878,0.695734330590878),(0.695829152843917,
0.695829152843917),(0.695924063484005,0.695924063484005),(0.495302555981778,
0.495302555981778),(0.689605300294912,0.689605300294912)))
REPRESENTATION_ITEM('')
SURFACE()
) ;
#113 = (
BOUNDED_SURFACE()
B_SPLINE_SURFACE(2,1,((#195996,#195997),(#195998,#195999),(#196000,#196001),
(#196002,#196003),(#196004,#196005)),.UNSPECIFIED.,.F.,.F.,.F.)
B_SPLINE_SURFACE_WITH_KNOTS((3,2,3),(2,2),(173.088614465777,173.08934588035,
174.635405352829),(0.,0.72),.UNSPECIFIED.)
GEOMETRIC_REPRESENTATION_ITEM()
RATIONAL_B_SPLINE_SURFACE(((0.689605300294912,0.689605300294912),(0.689699287216941,
0.689699287216941),(0.689793361747377,0.689793361747377),(0.490939217509313,
0.490939217509313),(0.683530263327603,0.683530263327603)))
REPRESENTATION_ITEM('')
SURFACE()
) ;
#114 = (
BOUNDED_SURFACE()
B_SPLINE_SURFACE(2,1,((#196023,#196024),(#196025,#196026),(#196027,#196028),
(#196029,#196030),(#196031,#196032)),.UNSPECIFIED.,.F.,.F.,.F.)
B_SPLINE_SURFACE_WITH_KNOTS((3,2,3),(2,2),(179.325593228378,179.326324642951,
180.87238411543),(0.,0.72),.UNSPECIFIED.)
GEOMETRIC_REPRESENTATION_ITEM()
RATIONAL_B_SPLINE_SURFACE(((0.683530263327603,0.683530263327603),(0.68362342227742,
0.68362342227742),(0.683716668063863,0.683716668063863),(0.486614317608173,
0.486614317608173),(0.677508744037925,0.677508744037925)))
REPRESENTATION_ITEM('')
SURFACE()
) ;
#115 = (
BOUNDED_SURFACE()
B_SPLINE_SURFACE(2,1,((#196050,#196051),(#196052,#196053),(#196054,#196055),
(#196056,#196057),(#196058,#196059)),.UNSPECIFIED.,.F.,.F.,.F.)
B_SPLINE_SURFACE_WITH_KNOTS((3,2,3),(2,2),(185.562571990979,185.563303405552,
187.109362878031),(0.,0.72),.UNSPECIFIED.)
GEOMETRIC_REPRESENTATION_ITEM()
RATIONAL_B_SPLINE_SURFACE(((0.677508744037925,0.677508744037925),(0.677601082309502,
0.677601082309502),(0.677693506652723,0.677693506652723),(0.482327517656045,
0.482327517656045),(0.671540270965073,0.671540270965073)))
REPRESENTATION_ITEM('')
SURFACE()
) ;
#116 = (
BOUNDED_SURFACE()
B_SPLINE_SURFACE(2,1,((#196077,#196078),(#196079,#196080),(#196081,#196082),
(#196083,#196084),(#196085,#196086)),.UNSPECIFIED.,.F.,.F.,.F.)
B_SPLINE_SURFACE_WITH_KNOTS((3,2,3),(2,2),(191.79955075358,191.800282168153,
193.346341640632),(0.,0.72),.UNSPECIFIED.)
GEOMETRIC_REPRESENTATION_ITEM()
RATIONAL_B_SPLINE_SURFACE(((0.671540270965073,0.671540270965073),(0.671631795788127,
0.671631795788127),(0.671723405924582,0.671723405924582),(0.478078482013688,
0.478078482013688),(0.665624376801549,0.665624376801549)))
REPRESENTATION_ITEM('')
SURFACE()
) ;
#117 = (
BOUNDED_SURFACE()
B_SPLINE_SURFACE(2,1,((#196104,#196105),(#196106,#196107),(#196108,#196109),
(#196110,#196111),(#196112,#196113)),.UNSPECIFIED.,.F.,.F.,.F.)
B_SPLINE_SURFACE_WITH_KNOTS((3,2,3),(2,2),(198.036529516181,198.037260930754,
199.583320403233),(0.,0.72),.UNSPECIFIED.)
GEOMETRIC_REPRESENTATION_ITEM()
RATIONAL_B_SPLINE_SURFACE(((0.665624376801549,0.665624376801549),(0.665715095342106,
0.665715095342106),(0.6658058984445,0.6658058984445),(0.473866877998657,
0.473866877998657),(0.659760598356571,0.659760598356571)))
REPRESENTATION_ITEM('')
SURFACE()
) ;
#118 = (
BOUNDED_SURFACE()
B_SPLINE_SURFACE(2,1,((#196131,#196132),(#196133,#196134),(#196135,#196136),
(#196137,#196138),(#196139,#196140)),.UNSPECIFIED.,.F.,.F.,.F.)
B_SPLINE_SURFACE_WITH_KNOTS((3,2,3),(2,2),(204.273508278782,204.274239693355,
205.820299165834),(0.,0.72),.UNSPECIFIED.)
GEOMETRIC_REPRESENTATION_ITEM()
RATIONAL_B_SPLINE_SURFACE(((0.659760598356571,0.659760598356571),(0.659850517717528,
0.659850517717528),(0.659940520895381,0.659940520895381),(0.469692375859253,
0.469692375859253),(0.65394847651981,0.65394847651981)))
REPRESENTATION_ITEM('')
SURFACE()
) ;
#119 = (
BOUNDED_SURFACE()
B_SPLINE_SURFACE(2,1,((#196158,#196159),(#196160,#196161),(#196162,#196163),
(#196164,#196165),(#196166,#196167)),.UNSPECIFIED.,.F.,.F.,.F.)
B_SPLINE_SURFACE_WITH_KNOTS((3,2,3),(2,2),(210.510487041383,210.511218455956,
212.057277928435),(0.,0.72),.UNSPECIFIED.)
GEOMETRIC_REPRESENTATION_ITEM()
RATIONAL_B_SPLINE_SURFACE(((0.65394847651981,0.65394847651981),(0.654037603741493,
0.654037603741493),(0.654126814041692,0.654126814041692),(0.465554648748704,
0.465554648748704),(0.64818755622544,0.64818755622544)))
REPRESENTATION_ITEM('')
SURFACE()
) ;
#120 = (
BOUNDED_SURFACE()
B_SPLINE_SURFACE(2,1,((#196185,#196186),(#196187,#196188),(#196189,#196190),
(#196191,#196192),(#196193,#196194)),.UNSPECIFIED.,.F.,.F.,.F.)
B_SPLINE_SURFACE_WITH_KNOTS((3,2,3),(2,2),(216.747465803984,216.748197218557,
218.294256691036),(0.,0.720000000000001),.UNSPECIFIED.)
GEOMETRIC_REPRESENTATION_ITEM()
RATIONAL_B_SPLINE_SURFACE(((0.64818755622544,0.64818755622544),(0.648275898286154,
0.648275898286154),(0.648364322693508,0.648364322693508),(0.461453372699577,
0.461453372699577),(0.642477386416514,0.642477386416514)))
REPRESENTATION_ITEM('')
SURFACE()
) ;
#121 = (
BOUNDED_SURFACE()
B_SPLINE_SURFACE(2,1,((#196212,#196213),(#196214,#196215),(#196216,#196217),
(#196218,#196219),(#196220,#196221)),.UNSPECIFIED.,.F.,.F.,.F.)
B_SPLINE_SURFACE_WITH_KNOTS((3,2,3),(2,2),(222.984444566585,222.985175981158,
224.531235453637),(0.,0.72),.UNSPECIFIED.)
GEOMETRIC_REPRESENTATION_ITEM()
RATIONAL_B_SPLINE_SURFACE(((0.642477386416514,0.642477386416514),(0.642564950233086,
0.642564950233086),(0.642652595670871,0.642652595670871),(0.457388226598407,
0.457388226598407),(0.636817520009641,0.636817520009641)))
REPRESENTATION_ITEM('')
SURFACE()
) ;
#122 = (
BOUNDED_SURFACE()
B_SPLINE_SURFACE(2,1,((#196239,#196240),(#196241,#196242),(#196243,#196244),
(#196245,#196246),(#196247,#196248)),.UNSPECIFIED.,.F.,.F.,.F.)
B_SPLINE_SURFACE_WITH_KNOTS((3,2,3),(2,2),(229.221423329186,229.222154743759,
230.768214216238),(0.,0.72),.UNSPECIFIED.)
GEOMETRIC_REPRESENTATION_ITEM()
RATIONAL_B_SPLINE_SURFACE(((0.636817520009641,0.636817520009641),(0.636904312437968,
0.636904312437968),(0.63699118576847,0.63699118576847),(0.453358892160564,
0.453358892160564),(0.631207513859986,0.631207513859986)))
REPRESENTATION_ITEM('')
SURFACE()
) ;
#123 = (
BOUNDED_SURFACE()
B_SPLINE_SURFACE(2,1,((#196266,#196267),(#196268,#196269),(#196270,#196271),
(#196272,#196273),(#196274,#196275)),.UNSPECIFIED.,.F.,.F.,.F.)
B_SPLINE_SURFACE_WITH_KNOTS((3,2,3),(2,2),(235.458402091787,235.45913350636,
237.005192978839),(0.,0.72),.UNSPECIFIED.)
GEOMETRIC_REPRESENTATION_ITEM()
RATIONAL_B_SPLINE_SURFACE(((0.631207513859986,0.631207513859986),(0.631293541695566,
0.631293541695566),(0.631379649720619,0.631379649720619),(0.449365053905324,
0.449365053905324),(0.625646928726572,0.625646928726572)))
REPRESENTATION_ITEM('')
SURFACE()
) ;
#124 = (
BOUNDED_SURFACE()
B_SPLINE_SURFACE(2,1,((#196293,#196294),(#196295,#196296),(#196297,#196298),
(#196299,#196300),(#196301,#196302)),.UNSPECIFIED.,.F.,.F.,.F.)
B_SPLINE_SURFACE_WITH_KNOTS((3,2,3),(2,2),(241.695380854388,241.696112268961,
243.24217174144),(0.,0.72),.UNSPECIFIED.)
GEOMETRIC_REPRESENTATION_ITEM()
RATIONAL_B_SPLINE_SURFACE(((0.625646928726572,0.625646928726572),(0.625732198705041,
0.625732198705041),(0.625817548166557,0.625817548166557),(0.445406399131173,
0.445406399131173),(0.620135329237891,0.620135329237891)))
REPRESENTATION_ITEM('')
SURFACE()
) ;
#125 = (
BOUNDED_SURFACE()
B_SPLINE_SURFACE(2,1,((#196320,#196321),(#196322,#196323),(#196324,#196325),
(#196326,#196327),(#196328,#196329)),.UNSPECIFIED.,.F.,.F.,.F.)
B_SPLINE_SURFACE_WITH_KNOTS((3,2,3),(2,2),(247.932359616989,247.933091031562,
249.479150504041),(0.,0.72),.UNSPECIFIED.)
GEOMETRIC_REPRESENTATION_ITEM()
RATIONAL_B_SPLINE_SURFACE(((0.620135329237891,0.620135329237891),(0.620219848035544,
0.620219848035544),(0.620304445616044,0.620304445616044),(0.441482617891324,
0.441482617891324),(0.61467228385781,0.61467228385781)))
REPRESENTATION_ITEM('')
SURFACE()
) ;
#126 = (
BOUNDED_SURFACE()
B_SPLINE_SURFACE(2,1,((#196347,#196348),(#196349,#196350),(#196351,#196352),
(#196353,#196354),(#196355,#196356)),.UNSPECIFIED.,.F.,.F.,.F.)
B_SPLINE_SURFACE_WITH_KNOTS((3,2,3),(2,2),(254.16933837959,254.170069794163,
255.716129266642),(0.,0.72),.UNSPECIFIED.)
GEOMETRIC_REPRESENTATION_ITEM()
RATIONAL_B_SPLINE_SURFACE(((0.61467228385781,0.61467228385781),(0.614756058092132,
0.614756058092132),(0.614839910415267,0.614839910415267),(0.437593402969444,
0.437593402969444),(0.609257364851794,0.609257364851794)))
REPRESENTATION_ITEM('')
SURFACE()
) ;
#127 = (
BOUNDED_SURFACE()
B_SPLINE_SURFACE(2,1,((#196374,#196375),(#196376,#196377),(#196378,#196379),
(#196380,#196381),(#196382,#196383)),.UNSPECIFIED.,.F.,.F.,.F.)
B_SPLINE_SURFACE_WITH_KNOTS((3,2,3),(2,2),(260.406317142191,260.407048556764,
261.953108029243),(0.,0.720000000000001),.UNSPECIFIED.)
GEOMETRIC_REPRESENTATION_ITEM()
RATIONAL_B_SPLINE_SURFACE(((0.609257364851794,0.609257364851794),(0.609340401081969,
0.609340401081969),(0.60942351471304,0.60942351471304),(0.433738449855607,
0.433738449855607),(0.603890148253404,0.603890148253404)))
REPRESENTATION_ITEM('')
SURFACE()
) ;
#128 = (
BOUNDED_SURFACE()
B_SPLINE_SURFACE(2,1,((#196401,#196402),(#196403,#196404),(#196405,#196406),
(#196407,#196408),(#196409,#196410)),.UNSPECIFIED.,.F.,.F.,.F.)
B_SPLINE_SURFACE_WITH_KNOTS((3,2,3),(2,2),(266.643295904792,266.644027319365,
268.190086791844),(0.,0.72),.UNSPECIFIED.)
GEOMETRIC_REPRESENTATION_ITEM()
RATIONAL_B_SPLINE_SURFACE(((0.603890148253404,0.603890148253404),(0.603972452980838,
0.603972452980838),(0.604054834427309,0.604054834427309),(0.429917456722449,
0.429917456722449),(0.598570213831113,0.598570213831113)))
REPRESENTATION_ITEM('')
SURFACE()
) ;
#129 = (
BOUNDED_SURFACE()
B_SPLINE_SURFACE(2,1,((#196428,#196429),(#196430,#196431),(#196432,#196433),
(#196434,#196435),(#196436,#196437)),.UNSPECIFIED.,.F.,.F.,.F.)
B_SPLINE_SURFACE_WITH_KNOTS((3,2,3),(2,2),(272.880274667394,272.881006081966,
274.427065554445),(0.,0.72),.UNSPECIFIED.)
GEOMETRIC_REPRESENTATION_ITEM()
RATIONAL_B_SPLINE_SURFACE(((0.598570213831113,0.598570213831113),(0.598651793499935,
0.598651793499935),(0.598733449211942,0.598733449211942),(0.426130124401535,
0.426130124401535),(0.593297145055395,0.593297145055395)))
REPRESENTATION_ITEM('')
SURFACE()
) ;
#130 = (
BOUNDED_SURFACE()
B_SPLINE_SURFACE(2,1,((#196455,#196456),(#196457,#196458),(#196459,#196460),
(#196461,#196462),(#196463,#196464)),.UNSPECIFIED.,.F.,.F.,.F.)
B_SPLINE_SURFACE_WITH_KNOTS((3,2,3),(2,2),(279.117253429995,279.117984844567,
280.664044317046),(0.,0.720000000000001),.UNSPECIFIED.)
GEOMETRIC_REPRESENTATION_ITEM()
RATIONAL_B_SPLINE_SURFACE(((0.593297145055395,0.593297145055395),(0.593378006052966,
0.593378006052966),(0.593458942423824,0.593458942423824),(0.422376156359937,
0.422376156359937),(0.588070529066119,0.588070529066119)))
REPRESENTATION_ITEM('')
SURFACE()
) ;
#131 = ELLIPSE('',#8872,15.4840898363667,13.4083590367118) ;
#132 = ELLIPSE('',#8873,20.0777465510975,17.3862071407653) ;
#133 = ELLIPSE('',#8874,8.52758831083714,7.38294286669008) ;
#134 = ELLIPSE('',#8875,5.66235728936404,4.9022943840305) ;
#135 = ELLIPSE('',#8916,15.4840898354346,13.4083590350904) ;
#136 = ELLIPSE('',#8917,20.0777465510709,17.3862071407216) ;
#137 = ELLIPSE('',#8918,8.52758470717412,7.38293667736543) ;
#138 = ELLIPSE('',#8919,5.66235729881268,4.90229438477269) ;
#139 = ELLIPSE('',#8975,0.90392506178254,0.899999999999994) ;
#140 = ELLIPSE('',#8976,1.00436117975839,0.999999999999988) ;
#141 = ELLIPSE('',#8978,1.00436117975839,0.999999999999988) ;
#142 = ELLIPSE('',#8979,1.00436117975839,0.999999999999988) ;
#143 = ELLIPSE('',#8980,1.00436117975839,0.999999999999998) ;
#144 = ELLIPSE('',#8982,0.903925061782534,0.900000000000005) ;
#145 = ELLIPSE('',#8984,1.00436117975838,0.999999999999987) ;
#146 = ELLIPSE('',#8985,1.00436117975838,0.999999999999987) ;
#147 = ELLIPSE('',#8986,1.00436117975838,0.999999999999987) ;
#148 = ELLIPSE('',#8987,1.00436117975838,0.999999999999987) ;
#149 = ELLIPSE('',#8989,0.0751099188439569,0.0750000000000024) ;
#150 = ELLIPSE('',#8990,0.0753270884818842,0.07500000000001) ;
#151 = ELLIPSE('',#8991,0.0753270884818842,0.07500000000001) ;
#152 = ELLIPSE('',#8992,0.0753270884818842,0.07500000000001) ;
#153 = ELLIPSE('',#8993,0.0752842013001122,0.0750000000000016) ;
#154 = ELLIPSE('',#8994,0.0752842013001065,0.0750000000000022) ;
#155 = ELLIPSE('',#8995,0.0752842013001065,0.0750000000000022) ;
#156 = ELLIPSE('',#8996,0.0752842013001065,0.0750000000000022) ;
#157 = ELLIPSE('',#8998,0.0751099188439449,0.0750000000000012) ;
#158 = ELLIPSE('',#8999,0.0753270884818742,0.07500000000003) ;
#159 = ELLIPSE('',#9000,0.0753270884818742,0.07500000000003) ;
#160 = ELLIPSE('',#9001,0.0753270884818742,0.07500000000003) ;
#161 = ELLIPSE('',#9002,0.0752842013001133,0.0749999999999984) ;
#162 = ELLIPSE('',#9003,0.0752842013001184,0.074999999999999) ;
#163 = ELLIPSE('',#9004,0.0752842013001184,0.074999999999999) ;
#164 = ELLIPSE('',#9005,0.0752842013001184,0.074999999999999) ;
#165 = ELLIPSE('',#9009,0.932157550311777,0.900000000000004) ;
#166 = ELLIPSE('',#9011,1.03573061145752,0.999999999999994) ;
#167 = ELLIPSE('',#9012,1.03573061145752,0.999999999999994) ;
#168 = ELLIPSE('',#9013,1.03573061145752,0.999999999999994) ;
#169 = ELLIPSE('',#9014,1.03573061145752,0.999999999999994) ;
#170 = ELLIPSE('',#9016,0.932157550311782,0.900000000000012) ;
#171 = ELLIPSE('',#9017,1.03573061145752,1.) ;
#172 = ELLIPSE('',#9019,1.03573061145752,1.) ;
#173 = ELLIPSE('',#9020,1.03573061145752,1.) ;
#174 = ELLIPSE('',#9021,1.03573061145752,1.) ;
#175 = ELLIPSE('',#9023,0.075909797816342,0.0750000000000059) ;
#176 = ELLIPSE('',#9024,0.0776797958593107,0.0750000000000013) ;
#177 = ELLIPSE('',#9025,0.0776797958593107,0.0750000000000013) ;
#178 = ELLIPSE('',#9026,0.0776797958593107,0.0750000000000013) ;
#179 = ELLIPSE('',#9027,0.0773330605240012,0.0750000000000033) ;
#180 = ELLIPSE('',#9028,0.0773330605239995,0.0750000000000025) ;
#181 = ELLIPSE('',#9029,0.0773330605239995,0.0750000000000025) ;
#182 = ELLIPSE('',#9030,0.0773330605239995,0.0750000000000025) ;
#183 = ELLIPSE('',#9032,0.0759097978163331,0.0750000000000011) ;
#184 = ELLIPSE('',#9033,0.0776797958593144,0.0750000000000244) ;
#185 = ELLIPSE('',#9034,0.0776797958593144,0.0750000000000244) ;
#186 = ELLIPSE('',#9035,0.0776797958593144,0.0750000000000244) ;
#187 = ELLIPSE('',#9036,0.0773330605240056,0.0750000000000024) ;
#188 = ELLIPSE('',#9037,0.077333060524004,0.0750000000000015) ;
#189 = ELLIPSE('',#9038,0.077333060524004,0.0750000000000015) ;
#190 = ELLIPSE('',#9039,0.077333060524004,0.0750000000000015) ;
#191 = ELLIPSE('',#9102,8.73317010092234,3.9982389407695) ;
#192 = ELLIPSE('',#9103,8.73317010092295,3.99823894076973) ;
#193 = ELLIPSE('',#9106,8.73317010092743,3.99823894077223) ;
#194 = ELLIPSE('',#9107,8.73317010092743,3.99823894077213) ;
#195 = ELLIPSE('',#9110,8.73317010092711,3.99823894077243) ;
#196 = ELLIPSE('',#9111,8.73317010092743,3.9982389407726) ;
#197 = ELLIPSE('',#9114,8.73317010092821,3.9982389407731) ;
#198 = ELLIPSE('',#9115,8.73317010092973,3.99823894077377) ;
#199 = ELLIPSE('',#9118,8.73317010092634,3.99823894077158) ;
#200 = ELLIPSE('',#9119,8.73317010092438,3.99823894077077) ;
#201 = ELLIPSE('',#9122,8.73317010092548,3.99823894077123) ;
#202 = ELLIPSE('',#9123,8.73317010092314,3.99823894077033) ;
#203 = ELLIPSE('',#9126,8.73317010092227,3.99823894076999) ;
#204 = ELLIPSE('',#9127,8.73317010092042,3.99823894076914) ;
#205 = ELLIPSE('',#9130,8.7331701009258,3.99823894077184) ;
#206 = ELLIPSE('',#9131,8.73317010092579,3.99823894077183) ;
#207 = ELLIPSE('',#9134,8.73317010092678,3.99823894077257) ;
#208 = ELLIPSE('',#9135,8.73317010092553,3.99823894077202) ;
#209 = ELLIPSE('',#9138,8.7331701009272,3.99823894077287) ;
#210 = ELLIPSE('',#9139,8.73317010092561,3.99823894077221) ;
#211 = ELLIPSE('',#9142,8.73317010092469,3.99823894077177) ;
#212 = ELLIPSE('',#9143,8.7331701009245,3.99823894077166) ;
#213 = ELLIPSE('',#9146,8.73317010092758,3.99823894077321) ;
#214 = ELLIPSE('',#9147,8.73317010092748,3.99823894077321) ;
#215 = ELLIPSE('',#9150,8.73317010092198,3.99823894076988) ;
#216 = ELLIPSE('',#9151,8.73317010092244,3.99823894077009) ;
#217 = ELLIPSE('',#9154,8.73317010092626,3.99823894077208) ;
#218 = ELLIPSE('',#9155,8.73317010092699,3.99823894077238) ;
#219 = ELLIPSE('',#9158,8.73317010092677,3.99823894077194) ;
#220 = ELLIPSE('',#9159,8.73317010092738,3.99823894077216) ;
#221 = ELLIPSE('',#9162,8.73317010092297,3.99823894077055) ;
#222 = ELLIPSE('',#9163,8.73317010092318,3.99823894077063) ;
#223 = ELLIPSE('',#9166,8.73317010092442,3.99823894077025) ;
#224 = ELLIPSE('',#9167,8.73317010092408,3.9982389407701) ;
#225 = ELLIPSE('',#9170,8.73317010092396,3.99823894077075) ;
#226 = ELLIPSE('',#9171,8.73317010092319,3.9982389407704) ;
#227 = ELLIPSE('',#9174,8.73317010092369,3.99823894077059) ;
#228 = ELLIPSE('',#9175,8.73317010092371,3.9982389407706) ;
#229 = ELLIPSE('',#9178,8.73317010092631,3.99823894077224) ;
#230 = ELLIPSE('',#9179,8.73317010092631,3.99823894077225) ;
#231 = ELLIPSE('',#9182,8.73317010092421,3.99823894077116) ;
#232 = ELLIPSE('',#9183,8.7331701009243,3.99823894077121) ;
#233 = ELLIPSE('',#9186,8.73317010092502,3.99823894077177) ;
#234 = ELLIPSE('',#9187,8.7331701009251,3.99823894077182) ;
#235 = ELLIPSE('',#9190,8.73317010092506,3.99823894077112) ;
#236 = ELLIPSE('',#9191,8.73317010092501,3.99823894077111) ;
#237 = ELLIPSE('',#9194,8.73317010092443,3.99823894077097) ;
#238 = ELLIPSE('',#9195,8.73317010092454,3.99823894077102) ;
#239 = ELLIPSE('',#9198,8.73317010092613,3.99823894077172) ;
#240 = ELLIPSE('',#9199,8.73317010092622,3.99823894077175) ;
#241 = ELLIPSE('',#9202,8.73317010092691,3.99823894077243) ;
#242 = ELLIPSE('',#9203,8.73317010092707,3.9982389407725) ;
#243 = ELLIPSE('',#9206,8.73317010092902,3.99823894077356) ;
#244 = ELLIPSE('',#9207,8.73317010092857,3.99823894077338) ;
#245 = ELLIPSE('',#9210,8.7331701009226,3.99823894077018) ;
#246 = ELLIPSE('',#9211,8.73317010092281,3.99823894077021) ;
#247 = ELLIPSE('',#9214,8.73317010092556,3.99823894077181) ;
#248 = ELLIPSE('',#9215,8.73317010092559,3.99823894077178) ;
#249 = ELLIPSE('',#9218,8.73317010092635,3.99823894077231) ;
#250 = ELLIPSE('',#9219,8.73317010092611,3.9982389407722) ;
#251 = ELLIPSE('',#9222,8.73317010092494,3.99823894077155) ;
#252 = ELLIPSE('',#9223,8.73317010092546,3.9982389407718) ;
#253 = ELLIPSE('',#9226,8.73317010092672,3.9982389407724) ;
#254 = ELLIPSE('',#9227,8.73317010092759,3.99823894077281) ;
#255 = ELLIPSE('',#9230,8.73317010092427,3.99823894077119) ;
#256 = ELLIPSE('',#9231,8.73317010092464,3.99823894077128) ;
#257 = ELLIPSE('',#9234,8.73317010092349,3.99823894076998) ;
#258 = ELLIPSE('',#9235,8.73317010092349,3.99823894076998) ;
#259 = ELLIPSE('',#9238,8.733170100929,3.99823894077289) ;
#260 = ELLIPSE('',#9239,8.73317010092749,3.99823894077221) ;
#261 = ELLIPSE('',#9242,8.73317010092275,3.99823894077023) ;
#262 = ELLIPSE('',#9243,8.7331701009221,3.99823894077012) ;
#263 = ELLIPSE('',#9246,8.7331701009272,3.99823894077234) ;
#264 = ELLIPSE('',#9247,8.73317010092575,3.99823894077179) ;
#265 = ELLIPSE('',#9250,8.73317010092357,3.9982389407703) ;
#266 = ELLIPSE('',#9251,8.73317010092264,3.99823894076992) ;
#267 = ELLIPSE('',#9254,8.73317010092163,3.99823894076961) ;
#268 = ELLIPSE('',#9255,8.73317010092226,3.99823894076974) ;
#269 = ELLIPSE('',#9258,8.73317010092482,3.99823894077158) ;
#270 = ELLIPSE('',#9259,8.73317010092302,3.99823894077092) ;
#271 = ELLIPSE('',#9262,8.733170100925,3.99823894077123) ;
#272 = ELLIPSE('',#9263,8.73317010092482,3.99823894077119) ;
#273 = ELLIPSE('',#9266,8.73317010092451,3.99823894077103) ;
#274 = ELLIPSE('',#9267,8.73317010092509,3.99823894077124) ;
#275 = ELLIPSE('',#9270,8.73317010092322,3.99823894077001) ;
#276 = ELLIPSE('',#9271,8.7331701009224,3.99823894076959) ;
#277 = ELLIPSE('',#9274,8.73317010092819,3.9982389407725) ;
#278 = ELLIPSE('',#9275,8.73317010092786,3.99823894077243) ;
#279 = ELLIPSE('',#9278,8.7331701009259,3.99823894077201) ;
#280 = ELLIPSE('',#9279,8.73317010092555,3.99823894077185) ;
#281 = ELLIPSE('',#9282,8.73317010092734,3.99823894077257) ;
#282 = ELLIPSE('',#9283,8.73317010092781,3.99823894077276) ;
#283 = ELLIPSE('',#9286,8.73317010092432,3.99823894077033) ;
#284 = ELLIPSE('',#9287,8.73317010092421,3.99823894077031) ;
#285 = ELLIPSE('',#9290,8.73317010092571,3.99823894077219) ;
#286 = ELLIPSE('',#9291,8.73317010092551,3.99823894077214) ;
#287 = ELLIPSE('',#9294,8.73317010092575,3.99823894077112) ;
#288 = ELLIPSE('',#9295,8.73317010092583,3.99823894077117) ;
#289 = ELLIPSE('',#9298,8.73317010092938,3.99823894077288) ;
#290 = ELLIPSE('',#9299,8.73317010092941,3.99823894077288) ;
#291 = ELLIPSE('',#9302,8.73317010092498,3.99823894077171) ;
#292 = ELLIPSE('',#9303,8.73317010092507,3.99823894077176) ;
#293 = ELLIPSE('',#9306,8.73317010092869,3.99823894077326) ;
#294 = ELLIPSE('',#9307,8.73317010092866,3.99823894077325) ;
#295 = ELLIPSE('',#9310,8.73317010092302,3.99823894077023) ;
#296 = ELLIPSE('',#9311,8.73317010092305,3.99823894077024) ;
#297 = ELLIPSE('',#9314,8.73317010092288,3.99823894077039) ;
#298 = ELLIPSE('',#9315,8.73317010092291,3.99823894077042) ;
#299 = ELLIPSE('',#9318,8.73317010092245,3.99823894077027) ;
#300 = ELLIPSE('',#9319,8.73317010092265,3.99823894077034) ;
#301 = ELLIPSE('',#9322,8.7331701009217,3.99823894076996) ;
#302 = ELLIPSE('',#9323,8.73317010092196,3.99823894077008) ;
#303 = ELLIPSE('',#9326,8.73317010092363,3.99823894077092) ;
#304 = ELLIPSE('',#9327,8.73317010092318,3.99823894077077) ;
#305 = ELLIPSE('',#9330,8.73317010092656,3.99823894077185) ;
#306 = ELLIPSE('',#9331,8.73317010092601,3.99823894077162) ;
#307 = ELLIPSE('',#9334,8.73317010092627,3.99823894077187) ;
#308 = ELLIPSE('',#9335,8.73317010092609,3.99823894077178) ;
#309 = ELLIPSE('',#9338,8.73317010092587,3.99823894077181) ;
#310 = ELLIPSE('',#9339,8.73317010092569,3.99823894077163) ;
#311 = CONICAL_SURFACE('',#8772,1.12500000002727,1.15997123047796) ;
#312 = CONICAL_SURFACE('',#8775,1.12500000002727,1.15997123047796) ;
#313 = CONICAL_SURFACE('',#8812,0.119992720241923,1.10714871779409) ;
#314 = CONICAL_SURFACE('',#8814,0.239985440483837,1.10714871779409) ;
#315 = CONICAL_SURFACE('',#8815,0.199999999999988,1.10714871779409) ;
#316 = CONICAL_SURFACE('',#8832,0.119992720241926,1.10714871779409) ;
#317 = CONICAL_SURFACE('',#8834,0.23998544048385,1.10714871779409) ;
#318 = CONICAL_SURFACE('',#8835,0.199999999999993,1.10714871779409) ;
#319 = STYLED_ITEM('',(#196765),#338) ;
#320 = STYLED_ITEM('',(#196765),#339) ;
#321 = STYLED_ITEM('',(#196765),#340) ;
#322 = STYLED_ITEM('',(#196765),#341) ;
#323 = STYLED_ITEM('',(#196765),#342) ;
#324 = STYLED_ITEM('',(#196765),#343) ;
#325 = STYLED_ITEM('',(#196765),#344) ;
#326 = STYLED_ITEM('',(#196765),#345) ;
#327 = STYLED_ITEM('',(#196765),#346) ;
#328 = STYLED_ITEM('',(#196765),#347) ;
#329 = STYLED_ITEM('',(#196765),#348) ;
#330 = STYLED_ITEM('',(#196765),#349) ;
#331 = STYLED_ITEM('',(#196765),#350) ;
#332 = STYLED_ITEM('',(#196765),#351) ;
#333 = STYLED_ITEM('',(#196765),#352) ;
#334 = STYLED_ITEM('',(#196765),#353) ;
#335 = STYLED_ITEM('',(#196765),#354) ;
#336 = STYLED_ITEM('',(#196765),#355) ;
#337 = STYLED_ITEM('',(#196765),#356) ;
#338 = MANIFOLD_SOLID_BREP('Pendulum Rod',#8715) ;
#339 = MANIFOLD_SOLID_BREP('Arbor',#8716) ;
#340 = MANIFOLD_SOLID_BREP('Entry Pallet Nib',#8717) ;
#341 = MANIFOLD_SOLID_BREP('Exit Pallet Nib',#8718) ;
#342 = MANIFOLD_SOLID_BREP('Pivot Collar',#8719) ;
#343 = MANIFOLD_SOLID_BREP('b196906x',#8720) ;
#344 = MANIFOLD_SOLID_BREP('Entry Pallet Arm',#8721) ;
#345 = MANIFOLD_SOLID_BREP('Exit Pallet Arm',#8722) ;
#346 = MANIFOLD_SOLID_BREP('Pallet Pivot Pin',#8723) ;
#347 = MANIFOLD_SOLID_BREP('Composer Arm',#8724) ;
#348 = MANIFOLD_SOLID_BREP('Composer Pin',#8725) ;
#349 = MANIFOLD_SOLID_BREP('b197050x',#8726) ;
#350 = MANIFOLD_SOLID_BREP('Entry Return Spring',#8727) ;
#351 = MANIFOLD_SOLID_BREP('Entry Stop Pin',#8728) ;
#352 = MANIFOLD_SOLID_BREP('Exit Stop Pin',#8729) ;
#353 = MANIFOLD_SOLID_BREP('Exit Return Spring',#8730) ;
#354 = MANIFOLD_SOLID_BREP('Lever Arm',#8731) ;
#355 = MANIFOLD_SOLID_BREP('Escape Wheel Hub',#8732) ;
#356 = MANIFOLD_SOLID_BREP('Escape Wheel',#8733) ;
#357 = PLANE('',#8753) ;
#358 = PLANE('',#8754) ;
#359 = PLANE('',#8770) ;
#360 = PLANE('',#8771) ;
#361 = PLANE('',#8778) ;
#362 = PLANE('',#8781) ;
#363 = PLANE('',#8787) ;
#364 = PLANE('',#8788) ;
#365 = PLANE('',#8798) ;
#366 = PLANE('',#8799) ;
#367 = PLANE('',#8803) ;
#368 = PLANE('',#8804) ;
#369 = PLANE('',#8817) ;
#370 = PLANE('',#8818) ;
#371 = PLANE('',#8819) ;
#372 = PLANE('',#8820) ;
#373 = PLANE('',#8821) ;
#374 = PLANE('',#8822) ;
#375 = PLANE('',#8823) ;
#376 = PLANE('',#8824) ;
#377 = PLANE('',#8837) ;
#378 = PLANE('',#8838) ;
#379 = PLANE('',#8839) ;
#380 = PLANE('',#8840) ;
#381 = PLANE('',#8841) ;
#382 = PLANE('',#8842) ;
#383 = PLANE('',#8843) ;
#384 = PLANE('',#8844) ;
#385 = PLANE('',#8860) ;
#386 = PLANE('',#8871) ;
#387 = PLANE('',#8903) ;
#388 = PLANE('',#8915) ;
#389 = PLANE('',#8938) ;
#390 = PLANE('',#8939) ;
#391 = PLANE('',#8943) ;
#392 = PLANE('',#8950) ;
#393 = PLANE('',#8951) ;
#394 = PLANE('',#8955) ;
#395 = PLANE('',#8962) ;
#396 = PLANE('',#8966) ;
#397 = PLANE('',#8969) ;
#398 = PLANE('',#8974) ;
#399 = PLANE('',#8981) ;
#400 = PLANE('',#8988) ;
#401 = PLANE('',#8997) ;
#402 = PLANE('',#9006) ;
#403 = PLANE('',#9007) ;
#404 = PLANE('',#9008) ;
#405 = PLANE('',#9015) ;
#406 = PLANE('',#9022) ;
#407 = PLANE('',#9031) ;
#408 = PLANE('',#9040) ;
#409 = PLANE('',#9041) ;
#410 = PLANE('',#9042) ;
#411 = PLANE('',#9060) ;
#412 = PLANE('',#9064) ;
#413 = PLANE('',#9076) ;
#414 = PLANE('',#9083) ;
#415 = PLANE('',#9084) ;
#416 = PLANE('',#9088) ;
#417 = PLANE('',#9091) ;
#418 = PLANE('',#9096) ;
#419 = PLANE('',#9098) ;
#420 = PLANE('',#9101) ;
#421 = PLANE('',#9104) ;
#422 = PLANE('',#9105) ;
#423 = PLANE('',#9108) ;
#424 = PLANE('',#9109) ;
#425 = PLANE('',#9112) ;
#426 = PLANE('',#9113) ;
#427 = PLANE('',#9116) ;
#428 = PLANE('',#9117) ;
#429 = PLANE('',#9120) ;
#430 = PLANE('',#9121) ;
#431 = PLANE('',#9124) ;
#432 = PLANE('',#9125) ;
#433 = PLANE('',#9128) ;
#434 = PLANE('',#9129) ;
#435 = PLANE('',#9132) ;
#436 = PLANE('',#9133) ;
#437 = PLANE('',#9136) ;
#438 = PLANE('',#9137) ;
#439 = PLANE('',#9140) ;
#440 = PLANE('',#9141) ;
#441 = PLANE('',#9144) ;
#442 = PLANE('',#9145) ;
#443 = PLANE('',#9148) ;
#444 = PLANE('',#9149) ;
#445 = PLANE('',#9152) ;
#446 = PLANE('',#9153) ;
#447 = PLANE('',#9156) ;
#448 = PLANE('',#9157) ;
#449 = PLANE('',#9160) ;
#450 = PLANE('',#9161) ;
#451 = PLANE('',#9164) ;
#452 = PLANE('',#9165) ;
#453 = PLANE('',#9168) ;
#454 = PLANE('',#9169) ;
#455 = PLANE('',#9172) ;
#456 = PLANE('',#9173) ;
#457 = PLANE('',#9176) ;
#458 = PLANE('',#9177) ;
#459 = PLANE('',#9180) ;
#460 = PLANE('',#9181) ;
#461 = PLANE('',#9184) ;
#462 = PLANE('',#9185) ;
#463 = PLANE('',#9188) ;
#464 = PLANE('',#9189) ;
#465 = PLANE('',#9192) ;
#466 = PLANE('',#9193) ;
#467 = PLANE('',#9196) ;
#468 = PLANE('',#9197) ;
#469 = PLANE('',#9200) ;
#470 = PLANE('',#9201) ;
#471 = PLANE('',#9204) ;
#472 = PLANE('',#9205) ;
#473 = PLANE('',#9208) ;
#474 = PLANE('',#9209) ;
#475 = PLANE('',#9212) ;
#476 = PLANE('',#9213) ;
#477 = PLANE('',#9216) ;
#478 = PLANE('',#9217) ;
#479 = PLANE('',#9220) ;
#480 = PLANE('',#9221) ;
#481 = PLANE('',#9224) ;
#482 = PLANE('',#9225) ;
#483 = PLANE('',#9228) ;
#484 = PLANE('',#9229) ;
#485 = PLANE('',#9232) ;
#486 = PLANE('',#9233) ;
#487 = PLANE('',#9236) ;
#488 = PLANE('',#9237) ;
#489 = PLANE('',#9240) ;
#490 = PLANE('',#9241) ;
#491 = PLANE('',#9244) ;
#492 = PLANE('',#9245) ;
#493 = PLANE('',#9248) ;
#494 = PLANE('',#9249) ;
#495 = PLANE('',#9252) ;
#496 = PLANE('',#9253) ;
#497 = PLANE('',#9256) ;
#498 = PLANE('',#9257) ;
#499 = PLANE('',#9260) ;
#500 = PLANE('',#9261) ;
#501 = PLANE('',#9264) ;
#502 = PLANE('',#9265) ;
#503 = PLANE('',#9268) ;
#504 = PLANE('',#9269) ;
#505 = PLANE('',#9272) ;
#506 = PLANE('',#9273) ;
#507 = PLANE('',#9276) ;
#508 = PLANE('',#9277) ;
#509 = PLANE('',#9280) ;
#510 = PLANE('',#9281) ;
#511 = PLANE('',#9284) ;
#512 = PLANE('',#9285) ;
#513 = PLANE('',#9288) ;
#514 = PLANE('',#9289) ;
#515 = PLANE('',#9292) ;
#516 = PLANE('',#9293) ;
#517 = PLANE('',#9296) ;
#518 = PLANE('',#9297) ;
#519 = PLANE('',#9300) ;
#520 = PLANE('',#9301) ;
#521 = PLANE('',#9304) ;
#522 = PLANE('',#9305) ;
#523 = PLANE('',#9308) ;
#524 = PLANE('',#9309) ;
#525 = PLANE('',#9312) ;
#526 = PLANE('',#9313) ;
#527 = PLANE('',#9316) ;
#528 = PLANE('',#9317) ;
#529 = PLANE('',#9320) ;
#530 = PLANE('',#9321) ;
#531 = PLANE('',#9324) ;
#532 = PLANE('',#9325) ;
#533 = PLANE('',#9328) ;
#534 = PLANE('',#9329) ;
#535 = PLANE('',#9332) ;
#536 = PLANE('',#9333) ;
#537 = PLANE('',#9336) ;
#538 = PLANE('',#9337) ;
#539 = PLANE('',#9340) ;
#540 = PLANE('',#9341) ;
#541 = PLANE('',#9373) ;
#542 = PLANE('',#9379) ;
#543 = PLANE('',#9386) ;
#544 = PLANE('',#9395) ;
#545 = PLANE('',#9402) ;
#546 = PLANE('',#9409) ;
#547 = PLANE('',#9416) ;
#548 = PLANE('',#9423) ;
#549 = PLANE('',#9430) ;
#550 = PLANE('',#9437) ;
#551 = PLANE('',#9444) ;
#552 = PLANE('',#9452) ;
#553 = PLANE('',#9453) ;
#554 = FACE_BOUND('',#1339,.T.) ;
#555 = FACE_BOUND('',#1340,.T.) ;
#556 = FACE_BOUND('',#1341,.T.) ;
#557 = FACE_BOUND('',#1342,.T.) ;
#558 = FACE_BOUND('',#1358,.T.) ;
#559 = FACE_BOUND('',#1359,.T.) ;
#560 = FACE_BOUND('',#1360,.T.) ;
#561 = FACE_BOUND('',#1361,.T.) ;
#562 = FACE_BOUND('',#1363,.T.) ;
#563 = FACE_BOUND('',#1365,.T.) ;
#564 = FACE_BOUND('',#1412,.T.) ;
#565 = FACE_BOUND('',#1431,.T.) ;
#566 = FACE_BOUND('',#1445,.T.) ;
#567 = FACE_BOUND('',#1446,.T.) ;
#568 = FACE_BOUND('',#1447,.T.) ;
#569 = FACE_BOUND('',#1448,.T.) ;
#570 = FACE_BOUND('',#1449,.T.) ;
#571 = FACE_BOUND('',#1451,.T.) ;
#572 = FACE_BOUND('',#1452,.T.) ;
#573 = FACE_BOUND('',#1453,.T.) ;
#574 = FACE_BOUND('',#1454,.T.) ;
#575 = FACE_BOUND('',#1455,.T.) ;
#576 = FACE_BOUND('',#1481,.T.) ;
#577 = FACE_BOUND('',#1482,.T.) ;
#578 = FACE_BOUND('',#1483,.T.) ;
#579 = FACE_BOUND('',#1484,.T.) ;
#580 = FACE_BOUND('',#1485,.T.) ;
#581 = FACE_BOUND('',#1487,.T.) ;
#582 = FACE_BOUND('',#1488,.T.) ;
#583 = FACE_BOUND('',#1489,.T.) ;
#584 = FACE_BOUND('',#1490,.T.) ;
#585 = FACE_BOUND('',#1491,.T.) ;
#586 = FACE_BOUND('',#1532,.T.) ;
#587 = FACE_BOUND('',#1533,.T.) ;
#588 = FACE_BOUND('',#1535,.T.) ;
#589 = FACE_BOUND('',#1536,.T.) ;
#590 = FACE_BOUND('',#1605,.T.) ;
#591 = FACE_BOUND('',#1606,.T.) ;
#592 = FACE_BOUND('',#1608,.T.) ;
#593 = FACE_BOUND('',#1609,.T.) ;
#594 = FACE_BOUND('',#1612,.T.) ;
#595 = FACE_BOUND('',#1614,.T.) ;
#596 = FACE_BOUND('',#1617,.T.) ;
#597 = FACE_BOUND('',#1619,.T.) ;
#598 = FACE_BOUND('',#1803,.T.) ;
#599 = FACE_BOUND('',#1804,.T.) ;
#600 = FACE_BOUND('',#1805,.T.) ;
#601 = FACE_BOUND('',#1806,.T.) ;
#602 = FACE_BOUND('',#1807,.T.) ;
#603 = FACE_BOUND('',#1808,.T.) ;
#604 = FACE_BOUND('',#1810,.T.) ;
#605 = FACE_BOUND('',#1855,.T.) ;
#606 = FACE_BOUND('',#1857,.T.) ;
#607 = FACE_BOUND('',#1858,.T.) ;
#608 = FACE_BOUND('',#1859,.T.) ;
#609 = FACE_BOUND('',#1860,.T.) ;
#610 = FACE_BOUND('',#1861,.T.) ;
#611 = FACE_BOUND('',#1862,.T.) ;
#612 = CIRCLE('',#8751,2.99999999999999) ;
#613 = CIRCLE('',#8752,2.99999999999999) ;
#614 = CIRCLE('',#8756,1.25000000003034) ;
#615 = CIRCLE('',#8762,1.25000000003052) ;
#616 = CIRCLE('',#8768,2.00000000000001) ;
#617 = CIRCLE('',#8769,2.) ;
#618 = CIRCLE('',#8773,1.2500000000303) ;
#619 = CIRCLE('',#8774,1.2500000000303) ;
#620 = CIRCLE('',#8776,1.2500000000303) ;
#621 = CIRCLE('',#8777,1.2500000000303) ;
#622 = CIRCLE('',#8779,1.2500000000303) ;
#623 = CIRCLE('',#8782,1.25000000003031) ;
#624 = CIRCLE('',#8785,1.25000000003032) ;
#625 = CIRCLE('',#8786,1.25000000003029) ;
#626 = CIRCLE('',#8795,0.299999999999999) ;
#627 = CIRCLE('',#8796,0.300000000000007) ;
#628 = CIRCLE('',#8797,0.300000000000007) ;
#629 = CIRCLE('',#8801,0.300000000000005) ;
#630 = CIRCLE('',#8802,0.3) ;
#631 = CIRCLE('',#8806,1.21492637222366) ;
#632 = CIRCLE('',#8811,1.21492629244945) ;
#633 = CIRCLE('',#8813,0.599963601209611) ;
#634 = CIRCLE('',#8816,1.00467112588555) ;
#635 = CIRCLE('',#8826,1.21492637222396) ;
#636 = CIRCLE('',#8831,1.21492629244947) ;
#637 = CIRCLE('',#8833,0.599963601209621) ;
#638 = CIRCLE('',#8836,1.00467112588556) ;
#639 = CIRCLE('',#8846,28.7407375552552) ;
#640 = CIRCLE('',#8847,28.7407375552552) ;
#641 = CIRCLE('',#8849,15.) ;
#642 = CIRCLE('',#8850,15.) ;
#643 = CIRCLE('',#8852,28.7407375552563) ;
#644 = CIRCLE('',#8853,28.7407375552563) ;
#645 = CIRCLE('',#8855,10.3432265401781) ;
#646 = CIRCLE('',#8856,10.3432265401781) ;
#647 = CIRCLE('',#8858,1.00000000000001) ;
#648 = CIRCLE('',#8859,1.00000000000001) ;
#649 = CIRCLE('',#8861,2.) ;
#650 = CIRCLE('',#8862,23.0149881946395) ;
#651 = CIRCLE('',#8863,2.4999999999999) ;
#652 = CIRCLE('',#8864,18.0149881946822) ;
#653 = CIRCLE('',#8865,2.49999999999983) ;
#654 = CIRCLE('',#8866,7.00000000000001) ;
#655 = CIRCLE('',#8867,1.50000000000001) ;
#656 = CIRCLE('',#8868,6.6716132701064) ;
#657 = CIRCLE('',#8869,1.49999999999977) ;
#658 = CIRCLE('',#8870,9.6716132700902) ;
#659 = CIRCLE('',#8877,2.00000000000002) ;
#660 = CIRCLE('',#8880,18.0149881946813) ;
#661 = CIRCLE('',#8884,7.00000000000001) ;
#662 = CIRCLE('',#8887,1.49999999999978) ;
#663 = CIRCLE('',#8889,6.6716132701049) ;
#664 = CIRCLE('',#8892,28.7407375552556) ;
#665 = CIRCLE('',#8893,28.7407375552556) ;
#666 = CIRCLE('',#8895,15.) ;
#667 = CIRCLE('',#8896,15.) ;
#668 = CIRCLE('',#8898,28.7407375552573) ;
#669 = CIRCLE('',#8899,28.7407375552573) ;
#670 = CIRCLE('',#8901,10.3432265401781) ;
#671 = CIRCLE('',#8902,10.3432265401781) ;
#672 = CIRCLE('',#8904,2.) ;
#673 = CIRCLE('',#8905,23.0149881946393) ;
#674 = CIRCLE('',#8906,2.4999999999999) ;
#675 = CIRCLE('',#8907,18.0149881946822) ;
#676 = CIRCLE('',#8908,2.49999999999984) ;
#677 = CIRCLE('',#8909,7.) ;
#678 = CIRCLE('',#8910,1.49999999999999) ;
#679 = CIRCLE('',#8911,6.67161327010524) ;
#680 = CIRCLE('',#8912,1.49999999999977) ;
#681 = CIRCLE('',#8913,9.67161327008901) ;
#682 = CIRCLE('',#8914,0.999999999999985) ;
#683 = CIRCLE('',#8921,2.00000000000002) ;
#684 = CIRCLE('',#8924,18.0149881946818) ;
#685 = CIRCLE('',#8928,7.) ;
#686 = CIRCLE('',#8932,6.67161327010476) ;
#687 = CIRCLE('',#8936,2.00000000000002) ;
#688 = CIRCLE('',#8937,2.00000000000002) ;
#689 = CIRCLE('',#8941,6.00000000000002) ;
#690 = CIRCLE('',#8942,6.00000000000002) ;
#691 = CIRCLE('',#8945,2.1716132700891) ;
#692 = CIRCLE('',#8946,2.1716132700891) ;
#693 = CIRCLE('',#8948,2.50000000000001) ;
#694 = CIRCLE('',#8949,2.50000000000001) ;
#695 = CIRCLE('',#8953,3.49999999999995) ;
#696 = CIRCLE('',#8954,3.49999999999995) ;
#697 = CIRCLE('',#8957,2.50000000000018) ;
#698 = CIRCLE('',#8958,2.50000000000018) ;
#699 = CIRCLE('',#8960,5.99999999999934) ;
#700 = CIRCLE('',#8961,5.99999999999934) ;
#701 = CIRCLE('',#8964,2.49999999999992) ;
#702 = CIRCLE('',#8965,2.49999999999992) ;
#703 = CIRCLE('',#8967,0.999999999999994) ;
#704 = CIRCLE('',#8968,2.00000000000002) ;
#705 = CIRCLE('',#8970,0.999999999999994) ;
#706 = CIRCLE('',#8971,2.00000000000002) ;
#707 = CIRCLE('',#8977,1.94783572104092) ;
#708 = CIRCLE('',#8983,1.94783572104076) ;
#709 = CIRCLE('',#9010,1.94783572104088) ;
#710 = CIRCLE('',#9018,1.94783572104112) ;
#711 = CIRCLE('',#9043,691.195967278452) ;
#712 = CIRCLE('',#9044,691.195967278452) ;
#713 = CIRCLE('',#9046,2.49999999999962) ;
#714 = CIRCLE('',#9047,2.49999999999962) ;
#715 = CIRCLE('',#9049,5.99999999999934) ;
#716 = CIRCLE('',#9050,5.99999999999934) ;
#717 = CIRCLE('',#9052,2.50000000000002) ;
#718 = CIRCLE('',#9053,2.50000000000002) ;
#719 = CIRCLE('',#9055,2.17161327008905) ;
#720 = CIRCLE('',#9056,2.17161327008905) ;
#721 = CIRCLE('',#9058,2.50000000000002) ;
#722 = CIRCLE('',#9059,2.50000000000002) ;
#723 = CIRCLE('',#9062,6.00000000000005) ;
#724 = CIRCLE('',#9063,6.00000000000005) ;
#725 = CIRCLE('',#9066,2.49999999999997) ;
#726 = CIRCLE('',#9067,2.49999999999997) ;
#727 = CIRCLE('',#9069,6.00000000000009) ;
#728 = CIRCLE('',#9070,6.00000000000009) ;
#729 = CIRCLE('',#9072,2.50000000000032) ;
#730 = CIRCLE('',#9073,2.50000000000032) ;
#731 = CIRCLE('',#9074,638.804590655714) ;
#732 = CIRCLE('',#9075,638.804590655714) ;
#733 = CIRCLE('',#9078,2.00000000000002) ;
#734 = CIRCLE('',#9079,2.00000000000002) ;
#735 = CIRCLE('',#9081,1.) ;
#736 = CIRCLE('',#9082,1.) ;
#737 = CIRCLE('',#9086,7.) ;
#738 = CIRCLE('',#9087,7.) ;
#739 = CIRCLE('',#9089,7.) ;
#740 = CIRCLE('',#9090,3.00000000000006) ;
#741 = CIRCLE('',#9092,3.00000000000006) ;
#742 = CIRCLE('',#9094,13.7469842874597) ;
#743 = CIRCLE('',#9095,13.7469842874597) ;
#744 = CIRCLE('',#9097,7.) ;
#745 = CIRCLE('',#9342,2.49999999999987) ;
#746 = CIRCLE('',#9343,78.9146368237007) ;
#747 = CIRCLE('',#9344,2.49999999999996) ;
#748 = CIRCLE('',#9345,2.49999999999929) ;
#749 = CIRCLE('',#9346,17.4999999999883) ;
#750 = CIRCLE('',#9347,2.49999999999988) ;
#751 = CIRCLE('',#9348,8.00000000000006) ;
#752 = CIRCLE('',#9349,2.50000000000011) ;
#753 = CIRCLE('',#9350,78.9146368237009) ;
#754 = CIRCLE('',#9351,2.50000000000036) ;
#755 = CIRCLE('',#9352,2.49999999999919) ;
#756 = CIRCLE('',#9353,17.4999999999808) ;
#757 = CIRCLE('',#9354,2.50000000000025) ;
#758 = CIRCLE('',#9355,2.49999999999974) ;
#759 = CIRCLE('',#9356,78.9146368237008) ;
#760 = CIRCLE('',#9357,2.49999999999989) ;
#761 = CIRCLE('',#9358,2.49999999999919) ;
#762 = CIRCLE('',#9359,17.4999999999877) ;
#763 = CIRCLE('',#9360,2.50000000000021) ;
#764 = CIRCLE('',#9361,2.49999999999996) ;
#765 = CIRCLE('',#9362,78.9146368237009) ;
#766 = CIRCLE('',#9363,2.49999999999969) ;
#767 = CIRCLE('',#9364,2.49999999999911) ;
#768 = CIRCLE('',#9365,17.4999999999922) ;
#769 = CIRCLE('',#9366,2.49999999999997) ;
#770 = CIRCLE('',#9367,2.49999999999985) ;
#771 = CIRCLE('',#9368,78.9146368237006) ;
#772 = CIRCLE('',#9369,2.50000000000015) ;
#773 = CIRCLE('',#9370,2.49999999999888) ;
#774 = CIRCLE('',#9371,17.4999999999909) ;
#775 = CIRCLE('',#9372,2.49999999999995) ;
#776 = CIRCLE('',#9374,83.314636823702) ;
#777 = CIRCLE('',#9376,17.4999999999885) ;
#778 = CIRCLE('',#9378,2.49999999999986) ;
#779 = CIRCLE('',#9381,2.49999999999987) ;
#780 = CIRCLE('',#9383,78.9146368237007) ;
#781 = CIRCLE('',#9385,2.49999999999997) ;
#782 = CIRCLE('',#9388,2.49999999999928) ;
#783 = CIRCLE('',#9390,8.00000000000006) ;
#784 = CIRCLE('',#9392,17.4999999999808) ;
#785 = CIRCLE('',#9394,2.50000000000025) ;
#786 = CIRCLE('',#9397,2.50000000000011) ;
#787 = CIRCLE('',#9399,78.9146368237007) ;
#788 = CIRCLE('',#9401,2.50000000000036) ;
#789 = CIRCLE('',#9404,2.4999999999992) ;
#790 = CIRCLE('',#9406,17.4999999999878) ;
#791 = CIRCLE('',#9408,2.50000000000022) ;
#792 = CIRCLE('',#9411,2.49999999999976) ;
#793 = CIRCLE('',#9413,78.9146368237008) ;
#794 = CIRCLE('',#9415,2.4999999999999) ;
#795 = CIRCLE('',#9418,2.49999999999919) ;
#796 = CIRCLE('',#9420,17.4999999999923) ;
#797 = CIRCLE('',#9422,2.49999999999998) ;
#798 = CIRCLE('',#9425,2.49999999999996) ;
#799 = CIRCLE('',#9427,78.9146368237009) ;
#800 = CIRCLE('',#9429,2.49999999999968) ;
#801 = CIRCLE('',#9432,2.49999999999912) ;
#802 = CIRCLE('',#9434,17.4999999999908) ;
#803 = CIRCLE('',#9436,2.49999999999996) ;
#804 = CIRCLE('',#9439,2.49999999999987) ;
#805 = CIRCLE('',#9441,78.9146368237006) ;
#806 = CIRCLE('',#9443,2.50000000000016) ;
#807 = CIRCLE('',#9446,2.49999999999888) ;
#808 = CIRCLE('',#9448,83.314636823702) ;
#809 = CIRCLE('',#9450,81.1146368237019) ;
#810 = CIRCLE('',#9451,81.1146368237019) ;
#811 = B_SPLINE_SURFACE_WITH_KNOTS('',1,3,((#12126,#12127,#12128,#12129,#12130,
#12131,#12132,#12133,#12134,#12135,#12136,#12137,#12138,#12139,#12140),
(#12141,#12142,#12143,#12144,#12145,#12146,#12147,#12148,#12149,#12150,
#12151,#12152,#12153,#12154,#12155)),.UNSPECIFIED.,.F.,.T.,.F.,(2,2),(4,
1,1,1,1,1,1,1,1,1,1,1,4),(-8.8354979436913E-5,0.241230871771051),(0.,0.433069184072941,
0.613631069879533,0.707969844415473,0.800502285413489,0.982878828682618,
1.41593872955056,1.84899944094778,2.03137686036412,2.12390982409441,2.21644278782049,
2.39882020722706,2.83187996119986),.UNSPECIFIED.) ;
#812 = B_SPLINE_SURFACE_WITH_KNOTS('',1,3,((#12173,#12174,#12175,#12176,#12177,
#12178,#12179,#12180,#12181,#12182,#12183,#12184,#12185,#12186,#12187),
(#12188,#12189,#12190,#12191,#12192,#12193,#12194,#12195,#12196,#12197,
#12198,#12199,#12200,#12201,#12202)),.UNSPECIFIED.,.F.,.T.,.F.,(2,2),(4,
1,1,1,1,1,1,1,1,1,1,1,4),(-8.82843032138443E-5,0.241231935350036),(0.,0.433059753999551,
0.615437173415573,0.707970137120889,0.802309447772199,0.982872196325326,
1.41594123358707,1.84900113443533,2.03137767770577,2.12391011870702,2.21824889324341,
2.39881077905672,2.83187996310763),.UNSPECIFIED.) ;
#813 = B_SPLINE_SURFACE_WITH_KNOTS('',1,3,((#12220,#12221,#12222,#12223,#12224,
#12225,#12226,#12227,#12228,#12229,#12230,#12231,#12232,#12233,#12234),
(#12235,#12236,#12237,#12238,#12239,#12240,#12241,#12242,#12243,#12244,
#12245,#12246,#12247,#12248,#12249)),.UNSPECIFIED.,.F.,.T.,.F.,(2,2),(4,
1,1,1,1,1,1,1,1,1,1,1,4),(-8.85365464214024E-5,0.241919354715635),(0.,0.433059753978827,
0.615437173388124,0.707970137104854,0.802309447755686,0.982872196316439,
1.41594123355621,1.84900113442618,2.03137767770062,2.12391011869139,2.21824889322736,
2.39881077903564,2.83187996310738),.UNSPECIFIED.) ;
#814 = B_SPLINE_SURFACE_WITH_KNOTS('',1,3,((#12267,#12268,#12269,#12270,#12271,
#12272,#12273,#12274,#12275,#12276,#12277,#12278,#12279,#12280,#12281),
(#12282,#12283,#12284,#12285,#12286,#12287,#12288,#12289,#12290,#12291,
#12292,#12293,#12294,#12295,#12296)),.UNSPECIFIED.,.F.,.T.,.F.,(2,2),(4,
1,1,1,1,1,1,1,1,1,1,1,4),(-8.86192306118932E-5,0.241918274947197),(0.,0.433069184052406,
0.61363106986425,0.707969844400602,0.800502285411225,0.982878828678875,
1.41593872952055,1.849007766784,2.02957051533547,2.12390982598676,2.21644278969928,
2.39882020911001,2.83187996310763),.UNSPECIFIED.) ;
#815 = B_SPLINE_SURFACE_WITH_KNOTS('',1,3,((#12362,#12363,#12364,#12365,#12366,
#12367,#12368,#12369,#12370,#12371,#12372,#12373,#12374,#12375,#12376,#12377,
#12378,#12379,#12380),(#12381,#12382,#12383,#12384,#12385,#12386,#12387,
#12388,#12389,#12390,#12391,#12392,#12393,#12394,#12395,#12396,#12397,#12398,
#12399)),.UNSPECIFIED.,.F.,.T.,.F.,(2,2),(4,1,1,1,1,1,1,1,1,1,1,1,1,1,1,
1,4),(0.,0.214916064382941),(0.,1.11916410687735,2.23832821375471,3.35749232063191,
4.47665642750911,5.59582053438647,6.71498464126383,7.83414874814102,8.95331285501821,
10.0724769618908,11.1916410687635,12.3108051756408,13.4299692825182,14.5491333893954,
15.6682974962725,16.7874616031499,17.9066257100273),.UNSPECIFIED.) ;
#816 = B_SPLINE_SURFACE_WITH_KNOTS('',3,1,((#12401,#12402),(#12403,#12404),
(#12405,#12406),(#12407,#12408),(#12409,#12410),(#12411,#12412),(#12413,
#12414),(#12415,#12416),(#12417,#12418),(#12419,#12420),(#12421,#12422),
(#12423,#12424),(#12425,#12426),(#12427,#12428),(#12429,#12430),(#12431,
#12432),(#12433,#12434),(#12435,#12436),(#12437,#12438)),.UNSPECIFIED.,
 .T.,.F.,.F.,(4,1,1,1,1,1,1,1,1,1,1,1,1,1,1,1,4),(2,2),(0.,1.11916410687736,
2.23832821375472,3.35749232063194,4.47665642750915,5.5958205343865,6.71498464126385,
7.83414874813648,8.95331285500911,10.0724769618863,11.1916410687635,12.3108051756408,
13.4299692825181,14.5491333893953,15.6682974962725,16.7874616031499,17.9066257100273),
(0.,0.214916064382901),.UNSPECIFIED.) ;
#817 = B_SPLINE_SURFACE_WITH_KNOTS('',1,3,((#18888,#18889,#18890,#18891,#18892,
#18893,#18894,#18895,#18896,#18897,#18898,#18899,#18900,#18901,#18902,#18903,
#18904,#18905,#18906),(#18907,#18908,#18909,#18910,#18911,#18912,#18913,
#18914,#18915,#18916,#18917,#18918,#18919,#18920,#18921,#18922,#18923,#18924,
#18925)),.UNSPECIFIED.,.F.,.T.,.F.,(2,2),(4,1,1,1,1,1,1,1,1,1,1,1,1,1,1,
1,4),(0.,0.431146952730279),(0.,0.667571568814075,1.33514313762815,2.00271471386764,
2.67028629010714,3.33785785892123,4.00542942773531,4.67300100397479,5.34057258021427,
6.00814415645105,6.67571573268784,7.34328730150191,8.01085887031598,8.67843044655548,
9.34600202279497,10.0135735916091,10.6811451604231),.UNSPECIFIED.) ;
#818 = B_SPLINE_SURFACE_WITH_KNOTS('',3,1,((#18927,#18928),(#18929,#18930),
(#18931,#18932),(#18933,#18934),(#18935,#18936),(#18937,#18938),(#18939,
#18940),(#18941,#18942),(#18943,#18944),(#18945,#18946),(#18947,#18948),
(#18949,#18950),(#18951,#18952),(#18953,#18954),(#18955,#18956),(#18957,
#18958),(#18959,#18960),(#18961,#18962),(#18963,#18964)),.UNSPECIFIED.,
 .T.,.F.,.F.,(4,1,1,1,1,1,1,1,1,1,1,1,1,1,1,1,4),(2,2),(0.,0.66757156881407,
1.33514313762814,2.00271471386764,2.67028629010714,3.33785785892123,4.00542942773532,
4.67300100397479,5.34057258021426,6.00814415645105,6.67571573268784,7.34328730150192,
8.01085887031599,8.67843044655547,9.34600202279495,10.013573591609,10.6811451604231),
(0.,0.431146952730297),.UNSPECIFIED.) ;
#819 = B_SPLINE_SURFACE_WITH_KNOTS('',3,1,((#18980,#18981),(#18982,#18983),
(#18984,#18985),(#18986,#18987),(#18988,#18989),(#18990,#18991),(#18992,
#18993),(#18994,#18995),(#18996,#18997),(#18998,#18999),(#19000,#19001),
(#19002,#19003),(#19004,#19005),(#19006,#19007),(#19008,#19009),(#19010,
#19011),(#19012,#19013),(#19014,#19015),(#19016,#19017),(#19018,#19019),
(#19020,#19021),(#19022,#19023),(#19024,#19025),(#19026,#19027),(#19028,
#19029),(#19030,#19031),(#19032,#19033),(#19034,#19035),(#19036,#19037),
(#19038,#19039),(#19040,#19041),(#19042,#19043),(#19044,#19045),(#19046,
#19047),(#19048,#19049),(#19050,#19051),(#19052,#19053),(#19054,#19055),
(#19056,#19057),(#19058,#19059),(#19060,#19061),(#19062,#19063),(#19064,
#19065),(#19066,#19067),(#19068,#19069),(#19070,#19071),(#19072,#19073),
(#19074,#19075),(#19076,#19077),(#19078,#19079),(#19080,#19081),(#19082,
#19083),(#19084,#19085),(#19086,#19087),(#19088,#19089),(#19090,#19091),
(#19092,#19093),(#19094,#19095),(#19096,#19097),(#19098,#19099),(#19100,
#19101),(#19102,#19103),(#19104,#19105),(#19106,#19107),(#19108,#19109),
(#19110,#19111),(#19112,#19113),(#19114,#19115),(#19116,#19117),(#19118,
#19119),(#19120,#19121),(#19122,#19123),(#19124,#19125),(#19126,#19127),
(#19128,#19129),(#19130,#19131),(#19132,#19133),(#19134,#19135),(#19136,
#19137),(#19138,#19139),(#19140,#19141),(#19142,#19143),(#19144,#19145),
(#19146,#19147),(#19148,#19149),(#19150,#19151),(#19152,#19153),(#19154,
#19155),(#19156,#19157),(#19158,#19159),(#19160,#19161),(#19162,#19163),
(#19164,#19165),(#19166,#19167),(#19168,#19169),(#19170,#19171),(#19172,
#19173),(#19174,#19175),(#19176,#19177),(#19178,#19179),(#19180,#19181),
(#19182,#19183),(#19184,#19185),(#19186,#19187),(#19188,#19189),(#19190,
#19191),(#19192,#19193),(#19194,#19195),(#19196,#19197),(#19198,#19199),
(#19200,#19201),(#19202,#19203),(#19204,#19205),(#19206,#19207),(#19208,
#19209),(#19210,#19211),(#19212,#19213),(#19214,#19215),(#19216,#19217),
(#19218,#19219),(#19220,#19221),(#19222,#19223),(#19224,#19225),(#19226,
#19227),(#19228,#19229),(#19230,#19231),(#19232,#19233),(#19234,#19235),
(#19236,#19237),(#19238,#19239),(#19240,#19241),(#19242,#19243),(#19244,
#19245),(#19246,#19247),(#19248,#19249),(#19250,#19251),(#19252,#19253),
(#19254,#19255),(#19256,#19257),(#19258,#19259),(#19260,#19261),(#19262,
#19263),(#19264,#19265),(#19266,#19267),(#19268,#19269),(#19270,#19271),
(#19272,#19273),(#19274,#19275),(#19276,#19277),(#19278,#19279),(#19280,
#19281),(#19282,#19283),(#19284,#19285),(#19286,#19287),(#19288,#19289),
(#19290,#19291),(#19292,#19293),(#19294,#19295),(#19296,#19297),(#19298,
#19299),(#19300,#19301),(#19302,#19303),(#19304,#19305),(#19306,#19307),
(#19308,#19309),(#19310,#19311),(#19312,#19313),(#19314,#19315),(#19316,
#19317),(#19318,#19319),(#19320,#19321),(#19322,#19323),(#19324,#19325),
(#19326,#19327),(#19328,#19329),(#19330,#19331),(#19332,#19333),(#19334,
#19335),(#19336,#19337),(#19338,#19339),(#19340,#19341),(#19342,#19343),
(#19344,#19345),(#19346,#19347),(#19348,#19349),(#19350,#19351),(#19352,
#19353),(#19354,#19355),(#19356,#19357),(#19358,#19359),(#19360,#19361),
(#19362,#19363),(#19364,#19365),(#19366,#19367),(#19368,#19369),(#19370,
#19371),(#19372,#19373),(#19374,#19375),(#19376,#19377),(#19378,#19379),
(#19380,#19381),(#19382,#19383),(#19384,#19385),(#19386,#19387),(#19388,
#19389),(#19390,#19391),(#19392,#19393),(#19394,#19395),(#19396,#19397),
(#19398,#19399),(#19400,#19401),(#19402,#19403),(#19404,#19405),(#19406,
#19407),(#19408,#19409),(#19410,#19411),(#19412,#19413),(#19414,#19415),
(#19416,#19417),(#19418,#19419),(#19420,#19421),(#19422,#19423),(#19424,
#19425),(#19426,#19427),(#19428,#19429),(#19430,#19431),(#19432,#19433),
(#19434,#19435),(#19436,#19437),(#19438,#19439),(#19440,#19441),(#19442,
#19443),(#19444,#19445),(#19446,#19447),(#19448,#19449),(#19450,#19451),
(#19452,#19453),(#19454,#19455),(#19456,#19457),(#19458,#19459),(#19460,
#19461),(#19462,#19463),(#19464,#19465),(#19466,#19467),(#19468,#19469),
(#19470,#19471),(#19472,#19473),(#19474,#19475),(#19476,#19477),(#19478,
#19479),(#19480,#19481),(#19482,#19483),(#19484,#19485),(#19486,#19487),
(#19488,#19489),(#19490,#19491),(#19492,#19493),(#19494,#19495),(#19496,
#19497),(#19498,#19499),(#19500,#19501),(#19502,#19503),(#19504,#19505),
(#19506,#19507),(#19508,#19509),(#19510,#19511),(#19512,#19513),(#19514,
#19515),(#19516,#19517),(#19518,#19519),(#19520,#19521),(#19522,#19523),
(#19524,#19525),(#19526,#19527),(#19528,#19529),(#19530,#19531),(#19532,
#19533),(#19534,#19535),(#19536,#19537),(#19538,#19539),(#19540,#19541),
(#19542,#19543),(#19544,#19545),(#19546,#19547),(#19548,#19549),(#19550,
#19551),(#19552,#19553),(#19554,#19555),(#19556,#19557),(#19558,#19559),
(#19560,#19561),(#19562,#19563),(#19564,#19565),(#19566,#19567),(#19568,
#19569),(#19570,#19571),(#19572,#19573),(#19574,#19575),(#19576,#19577),
(#19578,#19579),(#19580,#19581),(#19582,#19583),(#19584,#19585),(#19586,
#19587),(#19588,#19589),(#19590,#19591),(#19592,#19593),(#19594,#19595),
(#19596,#19597),(#19598,#19599),(#19600,#19601),(#19602,#19603),(#19604,
#19605),(#19606,#19607),(#19608,#19609),(#19610,#19611),(#19612,#19613),
(#19614,#19615),(#19616,#19617),(#19618,#19619),(#19620,#19621),(#19622,
#19623),(#19624,#19625),(#19626,#19627),(#19628,#19629),(#19630,#19631),
(#19632,#19633),(#19634,#19635),(#19636,#19637),(#19638,#19639),(#19640,
#19641),(#19642,#19643),(#19644,#19645),(#19646,#19647),(#19648,#19649),
(#19650,#19651),(#19652,#19653),(#19654,#19655),(#19656,#19657),(#19658,
#19659),(#19660,#19661),(#19662,#19663),(#19664,#19665),(#19666,#19667),
(#19668,#19669),(#19670,#19671),(#19672,#19673),(#19674,#19675),(#19676,
#19677),(#19678,#19679),(#19680,#19681),(#19682,#19683),(#19684,#19685),
(#19686,#19687),(#19688,#19689),(#19690,#19691),(#19692,#19693),(#19694,
#19695),(#19696,#19697),(#19698,#19699),(#19700,#19701),(#19702,#19703),
(#19704,#19705),(#19706,#19707),(#19708,#19709),(#19710,#19711),(#19712,
#19713),(#19714,#19715),(#19716,#19717),(#19718,#19719),(#19720,#19721),
(#19722,#19723),(#19724,#19725),(#19726,#19727),(#19728,#19729),(#19730,
#19731),(#19732,#19733),(#19734,#19735),(#19736,#19737),(#19738,#19739),
(#19740,#19741),(#19742,#19743),(#19744,#19745),(#19746,#19747),(#19748,
#19749),(#19750,#19751),(#19752,#19753),(#19754,#19755),(#19756,#19757),
(#19758,#19759),(#19760,#19761),(#19762,#19763),(#19764,#19765),(#19766,
#19767),(#19768,#19769),(#19770,#19771),(#19772,#19773),(#19774,#19775),
(#19776,#19777),(#19778,#19779),(#19780,#19781),(#19782,#19783),(#19784,
#19785),(#19786,#19787),(#19788,#19789),(#19790,#19791),(#19792,#19793),
(#19794,#19795),(#19796,#19797),(#19798,#19799),(#19800,#19801),(#19802,
#19803),(#19804,#19805),(#19806,#19807),(#19808,#19809),(#19810,#19811),
(#19812,#19813),(#19814,#19815),(#19816,#19817),(#19818,#19819),(#19820,
#19821),(#19822,#19823),(#19824,#19825),(#19826,#19827),(#19828,#19829),
(#19830,#19831),(#19832,#19833),(#19834,#19835),(#19836,#19837),(#19838,
#19839),(#19840,#19841),(#19842,#19843),(#19844,#19845),(#19846,#19847),
(#19848,#19849),(#19850,#19851),(#19852,#19853),(#19854,#19855),(#19856,
#19857),(#19858,#19859),(#19860,#19861),(#19862,#19863),(#19864,#19865),
(#19866,#19867),(#19868,#19869),(#19870,#19871),(#19872,#19873),(#19874,
#19875),(#19876,#19877),(#19878,#19879),(#19880,#19881),(#19882,#19883),
(#19884,#19885),(#19886,#19887),(#19888,#19889),(#19890,#19891),(#19892,
#19893),(#19894,#19895),(#19896,#19897),(#19898,#19899),(#19900,#19901),
(#19902,#19903),(#19904,#19905),(#19906,#19907),(#19908,#19909),(#19910,
#19911),(#19912,#19913),(#19914,#19915),(#19916,#19917),(#19918,#19919),
(#19920,#19921),(#19922,#19923),(#19924,#19925),(#19926,#19927),(#19928,
#19929),(#19930,#19931),(#19932,#19933),(#19934,#19935),(#19936,#19937),
(#19938,#19939),(#19940,#19941),(#19942,#19943),(#19944,#19945),(#19946,
#19947),(#19948,#19949),(#19950,#19951),(#19952,#19953),(#19954,#19955),
(#19956,#19957),(#19958,#19959),(#19960,#19961),(#19962,#19963),(#19964,
#19965),(#19966,#19967),(#19968,#19969),(#19970,#19971),(#19972,#19973),
(#19974,#19975),(#19976,#19977),(#19978,#19979),(#19980,#19981),(#19982,
#19983),(#19984,#19985),(#19986,#19987),(#19988,#19989),(#19990,#19991),
(#19992,#19993),(#19994,#19995),(#19996,#19997),(#19998,#19999),(#20000,
#20001),(#20002,#20003),(#20004,#20005),(#20006,#20007),(#20008,#20009),
(#20010,#20011),(#20012,#20013),(#20014,#20015),(#20016,#20017),(#20018,
#20019),(#20020,#20021),(#20022,#20023),(#20024,#20025),(#20026,#20027),
(#20028,#20029),(#20030,#20031),(#20032,#20033),(#20034,#20035),(#20036,
#20037),(#20038,#20039),(#20040,#20041),(#20042,#20043),(#20044,#20045),
(#20046,#20047),(#20048,#20049),(#20050,#20051),(#20052,#20053),(#20054,
#20055),(#20056,#20057),(#20058,#20059),(#20060,#20061),(#20062,#20063),
(#20064,#20065),(#20066,#20067),(#20068,#20069),(#20070,#20071),(#20072,
#20073),(#20074,#20075),(#20076,#20077),(#20078,#20079),(#20080,#20081),
(#20082,#20083),(#20084,#20085),(#20086,#20087),(#20088,#20089),(#20090,
#20091),(#20092,#20093),(#20094,#20095),(#20096,#20097),(#20098,#20099),
(#20100,#20101),(#20102,#20103),(#20104,#20105),(#20106,#20107),(#20108,
#20109),(#20110,#20111),(#20112,#20113),(#20114,#20115),(#20116,#20117),
(#20118,#20119),(#20120,#20121),(#20122,#20123),(#20124,#20125),(#20126,
#20127),(#20128,#20129),(#20130,#20131),(#20132,#20133),(#20134,#20135),
(#20136,#20137),(#20138,#20139),(#20140,#20141),(#20142,#20143),(#20144,
#20145),(#20146,#20147),(#20148,#20149),(#20150,#20151),(#20152,#20153),
(#20154,#20155),(#20156,#20157),(#20158,#20159),(#20160,#20161),(#20162,
#20163),(#20164,#20165),(#20166,#20167),(#20168,#20169),(#20170,#20171),
(#20172,#20173),(#20174,#20175),(#20176,#20177),(#20178,#20179),(#20180,
#20181),(#20182,#20183),(#20184,#20185),(#20186,#20187),(#20188,#20189),
(#20190,#20191),(#20192,#20193),(#20194,#20195),(#20196,#20197),(#20198,
#20199),(#20200,#20201),(#20202,#20203),(#20204,#20205),(#20206,#20207),
(#20208,#20209),(#20210,#20211),(#20212,#20213),(#20214,#20215),(#20216,
#20217),(#20218,#20219),(#20220,#20221),(#20222,#20223),(#20224,#20225),
(#20226,#20227),(#20228,#20229),(#20230,#20231),(#20232,#20233),(#20234,
#20235),(#20236,#20237),(#20238,#20239),(#20240,#20241),(#20242,#20243),
(#20244,#20245),(#20246,#20247),(#20248,#20249),(#20250,#20251),(#20252,
#20253),(#20254,#20255),(#20256,#20257),(#20258,#20259),(#20260,#20261),
(#20262,#20263),(#20264,#20265),(#20266,#20267),(#20268,#20269),(#20270,
#20271),(#20272,#20273),(#20274,#20275),(#20276,#20277),(#20278,#20279),
(#20280,#20281),(#20282,#20283),(#20284,#20285),(#20286,#20287),(#20288,
#20289),(#20290,#20291),(#20292,#20293),(#20294,#20295),(#20296,#20297),
(#20298,#20299),(#20300,#20301),(#20302,#20303),(#20304,#20305),(#20306,
#20307),(#20308,#20309),(#20310,#20311),(#20312,#20313),(#20314,#20315),
(#20316,#20317),(#20318,#20319),(#20320,#20321),(#20322,#20323),(#20324,
#20325),(#20326,#20327),(#20328,#20329),(#20330,#20331),(#20332,#20333),
(#20334,#20335),(#20336,#20337),(#20338,#20339),(#20340,#20341),(#20342,
#20343),(#20344,#20345),(#20346,#20347),(#20348,#20349),(#20350,#20351),
(#20352,#20353),(#20354,#20355),(#20356,#20357),(#20358,#20359),(#20360,
#20361),(#20362,#20363),(#20364,#20365),(#20366,#20367),(#20368,#20369),
(#20370,#20371),(#20372,#20373),(#20374,#20375),(#20376,#20377),(#20378,
#20379),(#20380,#20381),(#20382,#20383),(#20384,#20385),(#20386,#20387),
(#20388,#20389),(#20390,#20391),(#20392,#20393),(#20394,#20395),(#20396,
#20397),(#20398,#20399),(#20400,#20401),(#20402,#20403),(#20404,#20405),
(#20406,#20407),(#20408,#20409),(#20410,#20411),(#20412,#20413),(#20414,
#20415),(#20416,#20417),(#20418,#20419),(#20420,#20421),(#20422,#20423),
(#20424,#20425),(#20426,#20427),(#20428,#20429),(#20430,#20431),(#20432,
#20433),(#20434,#20435),(#20436,#20437),(#20438,#20439),(#20440,#20441),
(#20442,#20443),(#20444,#20445),(#20446,#20447),(#20448,#20449),(#20450,
#20451),(#20452,#20453),(#20454,#20455),(#20456,#20457),(#20458,#20459),
(#20460,#20461),(#20462,#20463),(#20464,#20465),(#20466,#20467),(#20468,
#20469),(#20470,#20471),(#20472,#20473),(#20474,#20475),(#20476,#20477),
(#20478,#20479),(#20480,#20481),(#20482,#20483),(#20484,#20485),(#20486,
#20487),(#20488,#20489),(#20490,#20491),(#20492,#20493),(#20494,#20495),
(#20496,#20497),(#20498,#20499),(#20500,#20501),(#20502,#20503),(#20504,
#20505),(#20506,#20507),(#20508,#20509),(#20510,#20511),(#20512,#20513),
(#20514,#20515),(#20516,#20517),(#20518,#20519),(#20520,#20521),(#20522,
#20523),(#20524,#20525),(#20526,#20527),(#20528,#20529),(#20530,#20531),
(#20532,#20533),(#20534,#20535),(#20536,#20537),(#20538,#20539),(#20540,
#20541),(#20542,#20543),(#20544,#20545),(#20546,#20547),(#20548,#20549),
(#20550,#20551),(#20552,#20553),(#20554,#20555),(#20556,#20557),(#20558,
#20559),(#20560,#20561),(#20562,#20563),(#20564,#20565),(#20566,#20567),
(#20568,#20569),(#20570,#20571),(#20572,#20573),(#20574,#20575),(#20576,
#20577),(#20578,#20579),(#20580,#20581),(#20582,#20583),(#20584,#20585),
(#20586,#20587),(#20588,#20589),(#20590,#20591),(#20592,#20593),(#20594,
#20595),(#20596,#20597),(#20598,#20599),(#20600,#20601),(#20602,#20603),
(#20604,#20605),(#20606,#20607),(#20608,#20609),(#20610,#20611),(#20612,
#20613),(#20614,#20615),(#20616,#20617),(#20618,#20619),(#20620,#20621),
(#20622,#20623),(#20624,#20625),(#20626,#20627),(#20628,#20629),(#20630,
#20631),(#20632,#20633),(#20634,#20635),(#20636,#20637),(#20638,#20639),
(#20640,#20641),(#20642,#20643),(#20644,#20645),(#20646,#20647),(#20648,
#20649),(#20650,#20651),(#20652,#20653),(#20654,#20655),(#20656,#20657),
(#20658,#20659),(#20660,#20661),(#20662,#20663),(#20664,#20665),(#20666,
#20667),(#20668,#20669),(#20670,#20671),(#20672,#20673),(#20674,#20675),
(#20676,#20677),(#20678,#20679),(#20680,#20681),(#20682,#20683),(#20684,
#20685),(#20686,#20687),(#20688,#20689),(#20690,#20691),(#20692,#20693),
(#20694,#20695),(#20696,#20697),(#20698,#20699),(#20700,#20701),(#20702,
#20703),(#20704,#20705),(#20706,#20707),(#20708,#20709),(#20710,#20711),
(#20712,#20713),(#20714,#20715),(#20716,#20717),(#20718,#20719),(#20720,
#20721),(#20722,#20723),(#20724,#20725),(#20726,#20727),(#20728,#20729),
(#20730,#20731),(#20732,#20733),(#20734,#20735),(#20736,#20737),(#20738,
#20739),(#20740,#20741),(#20742,#20743),(#20744,#20745),(#20746,#20747),
(#20748,#20749),(#20750,#20751),(#20752,#20753),(#20754,#20755),(#20756,
#20757),(#20758,#20759),(#20760,#20761),(#20762,#20763),(#20764,#20765),
(#20766,#20767),(#20768,#20769),(#20770,#20771),(#20772,#20773),(#20774,
#20775),(#20776,#20777),(#20778,#20779),(#20780,#20781),(#20782,#20783),
(#20784,#20785),(#20786,#20787),(#20788,#20789),(#20790,#20791),(#20792,
#20793),(#20794,#20795),(#20796,#20797),(#20798,#20799),(#20800,#20801),
(#20802,#20803),(#20804,#20805),(#20806,#20807),(#20808,#20809),(#20810,
#20811),(#20812,#20813),(#20814,#20815),(#20816,#20817),(#20818,#20819),
(#20820,#20821),(#20822,#20823),(#20824,#20825),(#20826,#20827),(#20828,
#20829),(#20830,#20831),(#20832,#20833),(#20834,#20835),(#20836,#20837),
(#20838,#20839),(#20840,#20841),(#20842,#20843),(#20844,#20845),(#20846,
#20847),(#20848,#20849),(#20850,#20851),(#20852,#20853),(#20854,#20855),
(#20856,#20857),(#20858,#20859),(#20860,#20861),(#20862,#20863),(#20864,
#20865),(#20866,#20867),(#20868,#20869),(#20870,#20871),(#20872,#20873),
(#20874,#20875),(#20876,#20877),(#20878,#20879),(#20880,#20881),(#20882,
#20883),(#20884,#20885),(#20886,#20887),(#20888,#20889),(#20890,#20891),
(#20892,#20893),(#20894,#20895),(#20896,#20897),(#20898,#20899),(#20900,
#20901),(#20902,#20903),(#20904,#20905),(#20906,#20907),(#20908,#20909),
(#20910,#20911),(#20912,#20913),(#20914,#20915),(#20916,#20917),(#20918,
#20919),(#20920,#20921),(#20922,#20923),(#20924,#20925),(#20926,#20927),
(#20928,#20929),(#20930,#20931),(#20932,#20933),(#20934,#20935),(#20936,
#20937),(#20938,#20939),(#20940,#20941),(#20942,#20943),(#20944,#20945),
(#20946,#20947),(#20948,#20949),(#20950,#20951),(#20952,#20953),(#20954,
#20955),(#20956,#20957),(#20958,#20959),(#20960,#20961),(#20962,#20963),
(#20964,#20965),(#20966,#20967),(#20968,#20969),(#20970,#20971),(#20972,
#20973),(#20974,#20975),(#20976,#20977),(#20978,#20979),(#20980,#20981),
(#20982,#20983),(#20984,#20985),(#20986,#20987),(#20988,#20989),(#20990,
#20991),(#20992,#20993),(#20994,#20995),(#20996,#20997),(#20998,#20999),
(#21000,#21001),(#21002,#21003),(#21004,#21005),(#21006,#21007),(#21008,
#21009),(#21010,#21011),(#21012,#21013),(#21014,#21015),(#21016,#21017),
(#21018,#21019),(#21020,#21021),(#21022,#21023),(#21024,#21025),(#21026,
#21027),(#21028,#21029),(#21030,#21031),(#21032,#21033),(#21034,#21035),
(#21036,#21037),(#21038,#21039),(#21040,#21041),(#21042,#21043),(#21044,
#21045),(#21046,#21047),(#21048,#21049),(#21050,#21051),(#21052,#21053),
(#21054,#21055),(#21056,#21057),(#21058,#21059),(#21060,#21061),(#21062,
#21063),(#21064,#21065),(#21066,#21067),(#21068,#21069),(#21070,#21071),
(#21072,#21073),(#21074,#21075),(#21076,#21077),(#21078,#21079),(#21080,
#21081),(#21082,#21083),(#21084,#21085),(#21086,#21087),(#21088,#21089),
(#21090,#21091),(#21092,#21093),(#21094,#21095),(#21096,#21097),(#21098,
#21099),(#21100,#21101),(#21102,#21103),(#21104,#21105),(#21106,#21107),
(#21108,#21109),(#21110,#21111),(#21112,#21113),(#21114,#21115),(#21116,
#21117),(#21118,#21119),(#21120,#21121),(#21122,#21123),(#21124,#21125),
(#21126,#21127),(#21128,#21129),(#21130,#21131),(#21132,#21133),(#21134,
#21135),(#21136,#21137),(#21138,#21139),(#21140,#21141),(#21142,#21143),
(#21144,#21145),(#21146,#21147),(#21148,#21149),(#21150,#21151),(#21152,
#21153),(#21154,#21155),(#21156,#21157),(#21158,#21159),(#21160,#21161),
(#21162,#21163),(#21164,#21165),(#21166,#21167),(#21168,#21169),(#21170,
#21171),(#21172,#21173),(#21174,#21175),(#21176,#21177),(#21178,#21179),
(#21180,#21181),(#21182,#21183),(#21184,#21185),(#21186,#21187),(#21188,
#21189),(#21190,#21191),(#21192,#21193),(#21194,#21195),(#21196,#21197),
(#21198,#21199),(#21200,#21201),(#21202,#21203),(#21204,#21205),(#21206,
#21207),(#21208,#21209),(#21210,#21211),(#21212,#21213),(#21214,#21215),
(#21216,#21217),(#21218,#21219),(#21220,#21221),(#21222,#21223),(#21224,
#21225),(#21226,#21227),(#21228,#21229),(#21230,#21231),(#21232,#21233),
(#21234,#21235),(#21236,#21237),(#21238,#21239),(#21240,#21241),(#21242,
#21243),(#21244,#21245),(#21246,#21247),(#21248,#21249),(#21250,#21251),
(#21252,#21253),(#21254,#21255),(#21256,#21257),(#21258,#21259),(#21260,
#21261),(#21262,#21263),(#21264,#21265),(#21266,#21267),(#21268,#21269),
(#21270,#21271),(#21272,#21273),(#21274,#21275),(#21276,#21277),(#21278,
#21279),(#21280,#21281),(#21282,#21283),(#21284,#21285),(#21286,#21287),
(#21288,#21289),(#21290,#21291),(#21292,#21293),(#21294,#21295),(#21296,
#21297),(#21298,#21299),(#21300,#21301),(#21302,#21303),(#21304,#21305),
(#21306,#21307),(#21308,#21309),(#21310,#21311),(#21312,#21313),(#21314,
#21315),(#21316,#21317),(#21318,#21319),(#21320,#21321),(#21322,#21323),
(#21324,#21325),(#21326,#21327),(#21328,#21329),(#21330,#21331),(#21332,
#21333),(#21334,#21335),(#21336,#21337),(#21338,#21339),(#21340,#21341),
(#21342,#21343),(#21344,#21345),(#21346,#21347),(#21348,#21349),(#21350,
#21351),(#21352,#21353),(#21354,#21355),(#21356,#21357),(#21358,#21359),
(#21360,#21361),(#21362,#21363),(#21364,#21365),(#21366,#21367),(#21368,
#21369),(#21370,#21371),(#21372,#21373),(#21374,#21375),(#21376,#21377),
(#21378,#21379),(#21380,#21381),(#21382,#21383),(#21384,#21385),(#21386,
#21387),(#21388,#21389),(#21390,#21391),(#21392,#21393),(#21394,#21395),
(#21396,#21397),(#21398,#21399),(#21400,#21401),(#21402,#21403),(#21404,
#21405),(#21406,#21407),(#21408,#21409),(#21410,#21411),(#21412,#21413),
(#21414,#21415),(#21416,#21417),(#21418,#21419),(#21420,#21421),(#21422,
#21423),(#21424,#21425),(#21426,#21427),(#21428,#21429),(#21430,#21431),
(#21432,#21433),(#21434,#21435),(#21436,#21437),(#21438,#21439),(#21440,
#21441),(#21442,#21443),(#21444,#21445),(#21446,#21447),(#21448,#21449),
(#21450,#21451),(#21452,#21453),(#21454,#21455),(#21456,#21457),(#21458,
#21459),(#21460,#21461),(#21462,#21463),(#21464,#21465),(#21466,#21467),
(#21468,#21469),(#21470,#21471),(#21472,#21473),(#21474,#21475),(#21476,
#21477),(#21478,#21479),(#21480,#21481),(#21482,#21483),(#21484,#21485),
(#21486,#21487),(#21488,#21489),(#21490,#21491),(#21492,#21493),(#21494,
#21495),(#21496,#21497),(#21498,#21499),(#21500,#21501),(#21502,#21503),
(#21504,#21505),(#21506,#21507),(#21508,#21509),(#21510,#21511),(#21512,
#21513),(#21514,#21515),(#21516,#21517),(#21518,#21519),(#21520,#21521),
(#21522,#21523),(#21524,#21525),(#21526,#21527),(#21528,#21529),(#21530,
#21531),(#21532,#21533),(#21534,#21535),(#21536,#21537),(#21538,#21539),
(#21540,#21541),(#21542,#21543),(#21544,#21545),(#21546,#21547),(#21548,
#21549),(#21550,#21551),(#21552,#21553),(#21554,#21555),(#21556,#21557),
(#21558,#21559),(#21560,#21561),(#21562,#21563),(#21564,#21565),(#21566,
#21567),(#21568,#21569),(#21570,#21571),(#21572,#21573),(#21574,#21575),
(#21576,#21577),(#21578,#21579),(#21580,#21581),(#21582,#21583),(#21584,
#21585),(#21586,#21587),(#21588,#21589),(#21590,#21591),(#21592,#21593),
(#21594,#21595),(#21596,#21597),(#21598,#21599),(#21600,#21601),(#21602,
#21603),(#21604,#21605),(#21606,#21607),(#21608,#21609),(#21610,#21611),
(#21612,#21613),(#21614,#21615),(#21616,#21617),(#21618,#21619),(#21620,
#21621),(#21622,#21623),(#21624,#21625),(#21626,#21627),(#21628,#21629),
(#21630,#21631),(#21632,#21633),(#21634,#21635),(#21636,#21637),(#21638,
#21639),(#21640,#21641),(#21642,#21643),(#21644,#21645),(#21646,#21647),
(#21648,#21649),(#21650,#21651),(#21652,#21653),(#21654,#21655),(#21656,
#21657),(#21658,#21659),(#21660,#21661),(#21662,#21663),(#21664,#21665),
(#21666,#21667),(#21668,#21669),(#21670,#21671),(#21672,#21673),(#21674,
#21675),(#21676,#21677),(#21678,#21679),(#21680,#21681),(#21682,#21683),
(#21684,#21685),(#21686,#21687),(#21688,#21689),(#21690,#21691),(#21692,
#21693),(#21694,#21695),(#21696,#21697),(#21698,#21699),(#21700,#21701),
(#21702,#21703),(#21704,#21705),(#21706,#21707),(#21708,#21709),(#21710,
#21711),(#21712,#21713),(#21714,#21715),(#21716,#21717),(#21718,#21719),
(#21720,#21721),(#21722,#21723),(#21724,#21725),(#21726,#21727),(#21728,
#21729),(#21730,#21731),(#21732,#21733),(#21734,#21735),(#21736,#21737),
(#21738,#21739),(#21740,#21741),(#21742,#21743),(#21744,#21745),(#21746,
#21747),(#21748,#21749),(#21750,#21751),(#21752,#21753),(#21754,#21755),
(#21756,#21757),(#21758,#21759),(#21760,#21761),(#21762,#21763),(#21764,
#21765),(#21766,#21767),(#21768,#21769),(#21770,#21771),(#21772,#21773),
(#21774,#21775),(#21776,#21777),(#21778,#21779),(#21780,#21781),(#21782,
#21783),(#21784,#21785),(#21786,#21787),(#21788,#21789),(#21790,#21791),
(#21792,#21793),(#21794,#21795),(#21796,#21797),(#21798,#21799),(#21800,
#21801),(#21802,#21803),(#21804,#21805),(#21806,#21807),(#21808,#21809),
(#21810,#21811),(#21812,#21813),(#21814,#21815),(#21816,#21817),(#21818,
#21819),(#21820,#21821),(#21822,#21823),(#21824,#21825),(#21826,#21827),
(#21828,#21829),(#21830,#21831),(#21832,#21833),(#21834,#21835),(#21836,
#21837),(#21838,#21839),(#21840,#21841),(#21842,#21843),(#21844,#21845),
(#21846,#21847),(#21848,#21849),(#21850,#21851),(#21852,#21853),(#21854,
#21855),(#21856,#21857),(#21858,#21859),(#21860,#21861),(#21862,#21863),
(#21864,#21865),(#21866,#21867),(#21868,#21869),(#21870,#21871),(#21872,
#21873),(#21874,#21875),(#21876,#21877),(#21878,#21879),(#21880,#21881),
(#21882,#21883),(#21884,#21885),(#21886,#21887),(#21888,#21889),(#21890,
#21891),(#21892,#21893),(#21894,#21895),(#21896,#21897),(#21898,#21899),
(#21900,#21901),(#21902,#21903),(#21904,#21905),(#21906,#21907),(#21908,
#21909),(#21910,#21911),(#21912,#21913),(#21914,#21915),(#21916,#21917),
(#21918,#21919),(#21920,#21921),(#21922,#21923),(#21924,#21925),(#21926,
#21927),(#21928,#21929),(#21930,#21931),(#21932,#21933),(#21934,#21935),
(#21936,#21937),(#21938,#21939),(#21940,#21941),(#21942,#21943),(#21944,
#21945),(#21946,#21947),(#21948,#21949),(#21950,#21951),(#21952,#21953),
(#21954,#21955),(#21956,#21957),(#21958,#21959),(#21960,#21961),(#21962,
#21963),(#21964,#21965),(#21966,#21967),(#21968,#21969),(#21970,#21971),
(#21972,#21973),(#21974,#21975),(#21976,#21977),(#21978,#21979),(#21980,
#21981),(#21982,#21983),(#21984,#21985),(#21986,#21987),(#21988,#21989),
(#21990,#21991),(#21992,#21993),(#21994,#21995),(#21996,#21997),(#21998,
#21999),(#22000,#22001),(#22002,#22003),(#22004,#22005),(#22006,#22007),
(#22008,#22009),(#22010,#22011),(#22012,#22013),(#22014,#22015),(#22016,
#22017),(#22018,#22019),(#22020,#22021),(#22022,#22023),(#22024,#22025),
(#22026,#22027),(#22028,#22029),(#22030,#22031),(#22032,#22033),(#22034,
#22035),(#22036,#22037),(#22038,#22039),(#22040,#22041),(#22042,#22043),
(#22044,#22045),(#22046,#22047),(#22048,#22049),(#22050,#22051),(#22052,
#22053),(#22054,#22055),(#22056,#22057),(#22058,#22059),(#22060,#22061),
(#22062,#22063),(#22064,#22065),(#22066,#22067),(#22068,#22069),(#22070,
#22071),(#22072,#22073),(#22074,#22075),(#22076,#22077),(#22078,#22079),
(#22080,#22081),(#22082,#22083),(#22084,#22085),(#22086,#22087),(#22088,
#22089),(#22090,#22091),(#22092,#22093),(#22094,#22095),(#22096,#22097),
(#22098,#22099),(#22100,#22101),(#22102,#22103),(#22104,#22105),(#22106,
#22107),(#22108,#22109),(#22110,#22111),(#22112,#22113),(#22114,#22115),
(#22116,#22117),(#22118,#22119),(#22120,#22121),(#22122,#22123),(#22124,
#22125),(#22126,#22127),(#22128,#22129),(#22130,#22131),(#22132,#22133),
(#22134,#22135),(#22136,#22137),(#22138,#22139),(#22140,#22141),(#22142,
#22143),(#22144,#22145),(#22146,#22147),(#22148,#22149),(#22150,#22151),
(#22152,#22153),(#22154,#22155),(#22156,#22157),(#22158,#22159),(#22160,
#22161),(#22162,#22163),(#22164,#22165),(#22166,#22167),(#22168,#22169),
(#22170,#22171),(#22172,#22173),(#22174,#22175),(#22176,#22177),(#22178,
#22179),(#22180,#22181),(#22182,#22183),(#22184,#22185),(#22186,#22187),
(#22188,#22189),(#22190,#22191),(#22192,#22193),(#22194,#22195),(#22196,
#22197),(#22198,#22199),(#22200,#22201),(#22202,#22203),(#22204,#22205),
(#22206,#22207),(#22208,#22209),(#22210,#22211),(#22212,#22213),(#22214,
#22215),(#22216,#22217),(#22218,#22219),(#22220,#22221),(#22222,#22223),
(#22224,#22225),(#22226,#22227),(#22228,#22229),(#22230,#22231),(#22232,
#22233),(#22234,#22235),(#22236,#22237),(#22238,#22239),(#22240,#22241),
(#22242,#22243),(#22244,#22245),(#22246,#22247),(#22248,#22249),(#22250,
#22251),(#22252,#22253),(#22254,#22255),(#22256,#22257),(#22258,#22259),
(#22260,#22261),(#22262,#22263),(#22264,#22265),(#22266,#22267),(#22268,
#22269),(#22270,#22271),(#22272,#22273),(#22274,#22275),(#22276,#22277),
(#22278,#22279),(#22280,#22281),(#22282,#22283),(#22284,#22285),(#22286,
#22287),(#22288,#22289),(#22290,#22291),(#22292,#22293),(#22294,#22295),
(#22296,#22297),(#22298,#22299),(#22300,#22301),(#22302,#22303),(#22304,
#22305),(#22306,#22307),(#22308,#22309),(#22310,#22311),(#22312,#22313),
(#22314,#22315),(#22316,#22317),(#22318,#22319),(#22320,#22321),(#22322,
#22323),(#22324,#22325),(#22326,#22327),(#22328,#22329),(#22330,#22331),
(#22332,#22333),(#22334,#22335),(#22336,#22337),(#22338,#22339),(#22340,
#22341),(#22342,#22343),(#22344,#22345),(#22346,#22347),(#22348,#22349),
(#22350,#22351),(#22352,#22353),(#22354,#22355),(#22356,#22357),(#22358,
#22359),(#22360,#22361),(#22362,#22363),(#22364,#22365),(#22366,#22367),
(#22368,#22369),(#22370,#22371),(#22372,#22373),(#22374,#22375),(#22376,
#22377),(#22378,#22379),(#22380,#22381),(#22382,#22383),(#22384,#22385),
(#22386,#22387),(#22388,#22389),(#22390,#22391),(#22392,#22393),(#22394,
#22395),(#22396,#22397),(#22398,#22399),(#22400,#22401),(#22402,#22403),
(#22404,#22405),(#22406,#22407),(#22408,#22409),(#22410,#22411),(#22412,
#22413),(#22414,#22415),(#22416,#22417),(#22418,#22419),(#22420,#22421),
(#22422,#22423),(#22424,#22425),(#22426,#22427),(#22428,#22429),(#22430,
#22431),(#22432,#22433),(#22434,#22435),(#22436,#22437),(#22438,#22439),
(#22440,#22441),(#22442,#22443),(#22444,#22445),(#22446,#22447),(#22448,
#22449),(#22450,#22451),(#22452,#22453),(#22454,#22455),(#22456,#22457),
(#22458,#22459),(#22460,#22461),(#22462,#22463),(#22464,#22465),(#22466,
#22467),(#22468,#22469),(#22470,#22471),(#22472,#22473),(#22474,#22475),
(#22476,#22477),(#22478,#22479),(#22480,#22481),(#22482,#22483),(#22484,
#22485),(#22486,#22487),(#22488,#22489),(#22490,#22491),(#22492,#22493),
(#22494,#22495),(#22496,#22497),(#22498,#22499),(#22500,#22501),(#22502,
#22503),(#22504,#22505),(#22506,#22507),(#22508,#22509),(#22510,#22511),
(#22512,#22513),(#22514,#22515),(#22516,#22517),(#22518,#22519),(#22520,
#22521),(#22522,#22523),(#22524,#22525),(#22526,#22527),(#22528,#22529),
(#22530,#22531),(#22532,#22533),(#22534,#22535),(#22536,#22537),(#22538,
#22539),(#22540,#22541),(#22542,#22543),(#22544,#22545),(#22546,#22547),
(#22548,#22549),(#22550,#22551),(#22552,#22553),(#22554,#22555),(#22556,
#22557),(#22558,#22559),(#22560,#22561),(#22562,#22563),(#22564,#22565),
(#22566,#22567),(#22568,#22569),(#22570,#22571),(#22572,#22573),(#22574,
#22575),(#22576,#22577),(#22578,#22579),(#22580,#22581),(#22582,#22583),
(#22584,#22585),(#22586,#22587),(#22588,#22589),(#22590,#22591),(#22592,
#22593),(#22594,#22595),(#22596,#22597),(#22598,#22599),(#22600,#22601),
(#22602,#22603),(#22604,#22605),(#22606,#22607),(#22608,#22609),(#22610,
#22611),(#22612,#22613),(#22614,#22615),(#22616,#22617),(#22618,#22619),
(#22620,#22621),(#22622,#22623),(#22624,#22625),(#22626,#22627),(#22628,
#22629),(#22630,#22631),(#22632,#22633),(#22634,#22635),(#22636,#22637),
(#22638,#22639),(#22640,#22641),(#22642,#22643),(#22644,#22645),(#22646,
#22647),(#22648,#22649),(#22650,#22651),(#22652,#22653),(#22654,#22655),
(#22656,#22657),(#22658,#22659),(#22660,#22661),(#22662,#22663),(#22664,
#22665),(#22666,#22667),(#22668,#22669),(#22670,#22671),(#22672,#22673),
(#22674,#22675),(#22676,#22677),(#22678,#22679),(#22680,#22681),(#22682,
#22683),(#22684,#22685),(#22686,#22687),(#22688,#22689),(#22690,#22691),
(#22692,#22693),(#22694,#22695),(#22696,#22697),(#22698,#22699),(#22700,
#22701),(#22702,#22703),(#22704,#22705),(#22706,#22707),(#22708,#22709),
(#22710,#22711),(#22712,#22713),(#22714,#22715),(#22716,#22717),(#22718,
#22719),(#22720,#22721),(#22722,#22723),(#22724,#22725),(#22726,#22727),
(#22728,#22729),(#22730,#22731),(#22732,#22733),(#22734,#22735),(#22736,
#22737),(#22738,#22739),(#22740,#22741),(#22742,#22743),(#22744,#22745),
(#22746,#22747),(#22748,#22749),(#22750,#22751),(#22752,#22753),(#22754,
#22755),(#22756,#22757),(#22758,#22759),(#22760,#22761),(#22762,#22763),
(#22764,#22765),(#22766,#22767),(#22768,#22769),(#22770,#22771),(#22772,
#22773),(#22774,#22775),(#22776,#22777),(#22778,#22779),(#22780,#22781),
(#22782,#22783),(#22784,#22785),(#22786,#22787),(#22788,#22789),(#22790,
#22791),(#22792,#22793),(#22794,#22795),(#22796,#22797),(#22798,#22799),
(#22800,#22801),(#22802,#22803),(#22804,#22805),(#22806,#22807),(#22808,
#22809),(#22810,#22811),(#22812,#22813),(#22814,#22815),(#22816,#22817),
(#22818,#22819),(#22820,#22821),(#22822,#22823),(#22824,#22825),(#22826,
#22827),(#22828,#22829),(#22830,#22831),(#22832,#22833),(#22834,#22835),
(#22836,#22837),(#22838,#22839),(#22840,#22841),(#22842,#22843),(#22844,
#22845),(#22846,#22847),(#22848,#22849),(#22850,#22851),(#22852,#22853),
(#22854,#22855),(#22856,#22857),(#22858,#22859),(#22860,#22861),(#22862,
#22863),(#22864,#22865),(#22866,#22867),(#22868,#22869),(#22870,#22871),
(#22872,#22873),(#22874,#22875),(#22876,#22877),(#22878,#22879),(#22880,
#22881),(#22882,#22883),(#22884,#22885),(#22886,#22887),(#22888,#22889),
(#22890,#22891),(#22892,#22893),(#22894,#22895),(#22896,#22897),(#22898,
#22899),(#22900,#22901),(#22902,#22903),(#22904,#22905),(#22906,#22907),
(#22908,#22909),(#22910,#22911),(#22912,#22913),(#22914,#22915),(#22916,
#22917),(#22918,#22919),(#22920,#22921),(#22922,#22923),(#22924,#22925),
(#22926,#22927),(#22928,#22929),(#22930,#22931),(#22932,#22933),(#22934,
#22935),(#22936,#22937),(#22938,#22939),(#22940,#22941),(#22942,#22943),
(#22944,#22945),(#22946,#22947),(#22948,#22949),(#22950,#22951),(#22952,
#22953),(#22954,#22955),(#22956,#22957),(#22958,#22959),(#22960,#22961),
(#22962,#22963),(#22964,#22965),(#22966,#22967),(#22968,#22969),(#22970,
#22971),(#22972,#22973),(#22974,#22975),(#22976,#22977),(#22978,#22979),
(#22980,#22981),(#22982,#22983),(#22984,#22985),(#22986,#22987),(#22988,
#22989),(#22990,#22991),(#22992,#22993),(#22994,#22995),(#22996,#22997),
(#22998,#22999),(#23000,#23001),(#23002,#23003),(#23004,#23005),(#23006,
#23007),(#23008,#23009),(#23010,#23011),(#23012,#23013),(#23014,#23015),
(#23016,#23017),(#23018,#23019),(#23020,#23021),(#23022,#23023),(#23024,
#23025),(#23026,#23027),(#23028,#23029),(#23030,#23031),(#23032,#23033),
(#23034,#23035),(#23036,#23037),(#23038,#23039),(#23040,#23041),(#23042,
#23043),(#23044,#23045),(#23046,#23047),(#23048,#23049),(#23050,#23051),
(#23052,#23053),(#23054,#23055),(#23056,#23057),(#23058,#23059),(#23060,
#23061),(#23062,#23063),(#23064,#23065),(#23066,#23067),(#23068,#23069),
(#23070,#23071),(#23072,#23073),(#23074,#23075),(#23076,#23077),(#23078,
#23079),(#23080,#23081),(#23082,#23083),(#23084,#23085),(#23086,#23087),
(#23088,#23089),(#23090,#23091),(#23092,#23093),(#23094,#23095),(#23096,
#23097),(#23098,#23099),(#23100,#23101),(#23102,#23103),(#23104,#23105),
(#23106,#23107),(#23108,#23109),(#23110,#23111),(#23112,#23113),(#23114,
#23115),(#23116,#23117),(#23118,#23119),(#23120,#23121),(#23122,#23123),
(#23124,#23125),(#23126,#23127),(#23128,#23129),(#23130,#23131),(#23132,
#23133),(#23134,#23135),(#23136,#23137),(#23138,#23139),(#23140,#23141),
(#23142,#23143),(#23144,#23145),(#23146,#23147),(#23148,#23149),(#23150,
#23151),(#23152,#23153),(#23154,#23155),(#23156,#23157),(#23158,#23159),
(#23160,#23161),(#23162,#23163),(#23164,#23165),(#23166,#23167),(#23168,
#23169),(#23170,#23171),(#23172,#23173),(#23174,#23175),(#23176,#23177),
(#23178,#23179),(#23180,#23181),(#23182,#23183),(#23184,#23185),(#23186,
#23187),(#23188,#23189),(#23190,#23191),(#23192,#23193),(#23194,#23195),
(#23196,#23197),(#23198,#23199),(#23200,#23201),(#23202,#23203),(#23204,
#23205),(#23206,#23207),(#23208,#23209),(#23210,#23211),(#23212,#23213),
(#23214,#23215),(#23216,#23217),(#23218,#23219),(#23220,#23221),(#23222,
#23223),(#23224,#23225),(#23226,#23227),(#23228,#23229),(#23230,#23231),
(#23232,#23233),(#23234,#23235),(#23236,#23237),(#23238,#23239),(#23240,
#23241),(#23242,#23243),(#23244,#23245),(#23246,#23247),(#23248,#23249),
(#23250,#23251),(#23252,#23253),(#23254,#23255),(#23256,#23257),(#23258,
#23259),(#23260,#23261),(#23262,#23263),(#23264,#23265),(#23266,#23267),
(#23268,#23269),(#23270,#23271),(#23272,#23273),(#23274,#23275),(#23276,
#23277),(#23278,#23279),(#23280,#23281),(#23282,#23283),(#23284,#23285),
(#23286,#23287),(#23288,#23289),(#23290,#23291),(#23292,#23293),(#23294,
#23295),(#23296,#23297),(#23298,#23299),(#23300,#23301),(#23302,#23303),
(#23304,#23305),(#23306,#23307),(#23308,#23309),(#23310,#23311),(#23312,
#23313),(#23314,#23315),(#23316,#23317),(#23318,#23319),(#23320,#23321),
(#23322,#23323),(#23324,#23325),(#23326,#23327),(#23328,#23329),(#23330,
#23331),(#23332,#23333),(#23334,#23335),(#23336,#23337),(#23338,#23339),
(#23340,#23341),(#23342,#23343),(#23344,#23345),(#23346,#23347),(#23348,
#23349),(#23350,#23351),(#23352,#23353),(#23354,#23355),(#23356,#23357),
(#23358,#23359),(#23360,#23361),(#23362,#23363),(#23364,#23365),(#23366,
#23367),(#23368,#23369),(#23370,#23371),(#23372,#23373),(#23374,#23375),
(#23376,#23377),(#23378,#23379),(#23380,#23381),(#23382,#23383),(#23384,
#23385),(#23386,#23387),(#23388,#23389),(#23390,#23391),(#23392,#23393),
(#23394,#23395),(#23396,#23397),(#23398,#23399),(#23400,#23401),(#23402,
#23403),(#23404,#23405),(#23406,#23407),(#23408,#23409),(#23410,#23411),
(#23412,#23413),(#23414,#23415),(#23416,#23417),(#23418,#23419),(#23420,
#23421),(#23422,#23423),(#23424,#23425),(#23426,#23427),(#23428,#23429),
(#23430,#23431),(#23432,#23433),(#23434,#23435),(#23436,#23437),(#23438,
#23439),(#23440,#23441),(#23442,#23443),(#23444,#23445),(#23446,#23447),
(#23448,#23449),(#23450,#23451),(#23452,#23453),(#23454,#23455),(#23456,
#23457),(#23458,#23459),(#23460,#23461),(#23462,#23463),(#23464,#23465),
(#23466,#23467),(#23468,#23469),(#23470,#23471),(#23472,#23473),(#23474,
#23475),(#23476,#23477),(#23478,#23479),(#23480,#23481),(#23482,#23483),
(#23484,#23485),(#23486,#23487),(#23488,#23489),(#23490,#23491),(#23492,
#23493),(#23494,#23495),(#23496,#23497),(#23498,#23499),(#23500,#23501),
(#23502,#23503),(#23504,#23505),(#23506,#23507),(#23508,#23509),(#23510,
#23511),(#23512,#23513),(#23514,#23515),(#23516,#23517),(#23518,#23519),
(#23520,#23521),(#23522,#23523),(#23524,#23525),(#23526,#23527),(#23528,
#23529),(#23530,#23531),(#23532,#23533),(#23534,#23535),(#23536,#23537),
(#23538,#23539),(#23540,#23541),(#23542,#23543),(#23544,#23545),(#23546,
#23547),(#23548,#23549),(#23550,#23551),(#23552,#23553),(#23554,#23555),
(#23556,#23557),(#23558,#23559),(#23560,#23561),(#23562,#23563),(#23564,
#23565),(#23566,#23567),(#23568,#23569),(#23570,#23571),(#23572,#23573),
(#23574,#23575),(#23576,#23577),(#23578,#23579),(#23580,#23581),(#23582,
#23583),(#23584,#23585),(#23586,#23587),(#23588,#23589),(#23590,#23591),
(#23592,#23593),(#23594,#23595),(#23596,#23597),(#23598,#23599),(#23600,
#23601),(#23602,#23603),(#23604,#23605),(#23606,#23607),(#23608,#23609),
(#23610,#23611),(#23612,#23613),(#23614,#23615),(#23616,#23617),(#23618,
#23619),(#23620,#23621),(#23622,#23623),(#23624,#23625),(#23626,#23627),
(#23628,#23629),(#23630,#23631),(#23632,#23633),(#23634,#23635),(#23636,
#23637),(#23638,#23639),(#23640,#23641),(#23642,#23643),(#23644,#23645),
(#23646,#23647),(#23648,#23649),(#23650,#23651),(#23652,#23653),(#23654,
#23655),(#23656,#23657),(#23658,#23659),(#23660,#23661),(#23662,#23663),
(#23664,#23665),(#23666,#23667),(#23668,#23669),(#23670,#23671),(#23672,
#23673),(#23674,#23675),(#23676,#23677),(#23678,#23679),(#23680,#23681),
(#23682,#23683),(#23684,#23685),(#23686,#23687),(#23688,#23689),(#23690,
#23691),(#23692,#23693),(#23694,#23695),(#23696,#23697),(#23698,#23699),
(#23700,#23701),(#23702,#23703),(#23704,#23705),(#23706,#23707),(#23708,
#23709),(#23710,#23711),(#23712,#23713),(#23714,#23715),(#23716,#23717),
(#23718,#23719),(#23720,#23721),(#23722,#23723),(#23724,#23725),(#23726,
#23727),(#23728,#23729),(#23730,#23731),(#23732,#23733),(#23734,#23735),
(#23736,#23737),(#23738,#23739),(#23740,#23741),(#23742,#23743),(#23744,
#23745),(#23746,#23747),(#23748,#23749),(#23750,#23751),(#23752,#23753),
(#23754,#23755),(#23756,#23757),(#23758,#23759),(#23760,#23761),(#23762,
#23763),(#23764,#23765),(#23766,#23767),(#23768,#23769),(#23770,#23771),
(#23772,#23773),(#23774,#23775),(#23776,#23777),(#23778,#23779),(#23780,
#23781),(#23782,#23783),(#23784,#23785),(#23786,#23787),(#23788,#23789),
(#23790,#23791),(#23792,#23793),(#23794,#23795),(#23796,#23797),(#23798,
#23799),(#23800,#23801),(#23802,#23803),(#23804,#23805),(#23806,#23807),
(#23808,#23809),(#23810,#23811),(#23812,#23813),(#23814,#23815),(#23816,
#23817),(#23818,#23819),(#23820,#23821),(#23822,#23823),(#23824,#23825),
(#23826,#23827),(#23828,#23829),(#23830,#23831),(#23832,#23833),(#23834,
#23835),(#23836,#23837),(#23838,#23839),(#23840,#23841),(#23842,#23843),
(#23844,#23845),(#23846,#23847),(#23848,#23849),(#23850,#23851),(#23852,
#23853),(#23854,#23855),(#23856,#23857),(#23858,#23859),(#23860,#23861),
(#23862,#23863),(#23864,#23865),(#23866,#23867),(#23868,#23869),(#23870,
#23871),(#23872,#23873),(#23874,#23875),(#23876,#23877),(#23878,#23879),
(#23880,#23881),(#23882,#23883),(#23884,#23885),(#23886,#23887),(#23888,
#23889),(#23890,#23891),(#23892,#23893),(#23894,#23895),(#23896,#23897),
(#23898,#23899),(#23900,#23901),(#23902,#23903),(#23904,#23905),(#23906,
#23907),(#23908,#23909),(#23910,#23911),(#23912,#23913),(#23914,#23915),
(#23916,#23917),(#23918,#23919),(#23920,#23921),(#23922,#23923),(#23924,
#23925),(#23926,#23927),(#23928,#23929),(#23930,#23931),(#23932,#23933),
(#23934,#23935),(#23936,#23937),(#23938,#23939),(#23940,#23941),(#23942,
#23943),(#23944,#23945),(#23946,#23947),(#23948,#23949),(#23950,#23951),
(#23952,#23953),(#23954,#23955),(#23956,#23957),(#23958,#23959),(#23960,
#23961),(#23962,#23963),(#23964,#23965),(#23966,#23967),(#23968,#23969),
(#23970,#23971),(#23972,#23973),(#23974,#23975),(#23976,#23977),(#23978,
#23979),(#23980,#23981),(#23982,#23983),(#23984,#23985),(#23986,#23987),
(#23988,#23989),(#23990,#23991),(#23992,#23993),(#23994,#23995),(#23996,
#23997),(#23998,#23999),(#24000,#24001),(#24002,#24003),(#24004,#24005),
(#24006,#24007),(#24008,#24009),(#24010,#24011),(#24012,#24013),(#24014,
#24015),(#24016,#24017),(#24018,#24019),(#24020,#24021),(#24022,#24023),
(#24024,#24025),(#24026,#24027),(#24028,#24029),(#24030,#24031),(#24032,
#24033),(#24034,#24035),(#24036,#24037),(#24038,#24039),(#24040,#24041),
(#24042,#24043),(#24044,#24045),(#24046,#24047),(#24048,#24049),(#24050,
#24051),(#24052,#24053),(#24054,#24055),(#24056,#24057),(#24058,#24059),
(#24060,#24061),(#24062,#24063),(#24064,#24065),(#24066,#24067),(#24068,
#24069),(#24070,#24071),(#24072,#24073),(#24074,#24075),(#24076,#24077),
(#24078,#24079),(#24080,#24081),(#24082,#24083),(#24084,#24085),(#24086,
#24087),(#24088,#24089),(#24090,#24091),(#24092,#24093),(#24094,#24095),
(#24096,#24097),(#24098,#24099),(#24100,#24101),(#24102,#24103),(#24104,
#24105),(#24106,#24107),(#24108,#24109),(#24110,#24111),(#24112,#24113),
(#24114,#24115),(#24116,#24117),(#24118,#24119),(#24120,#24121),(#24122,
#24123),(#24124,#24125),(#24126,#24127),(#24128,#24129),(#24130,#24131),
(#24132,#24133),(#24134,#24135),(#24136,#24137),(#24138,#24139),(#24140,
#24141),(#24142,#24143),(#24144,#24145),(#24146,#24147),(#24148,#24149),
(#24150,#24151),(#24152,#24153),(#24154,#24155),(#24156,#24157),(#24158,
#24159),(#24160,#24161),(#24162,#24163),(#24164,#24165),(#24166,#24167),
(#24168,#24169),(#24170,#24171),(#24172,#24173),(#24174,#24175),(#24176,
#24177),(#24178,#24179),(#24180,#24181),(#24182,#24183),(#24184,#24185),
(#24186,#24187),(#24188,#24189),(#24190,#24191),(#24192,#24193),(#24194,
#24195),(#24196,#24197),(#24198,#24199),(#24200,#24201),(#24202,#24203),
(#24204,#24205),(#24206,#24207),(#24208,#24209),(#24210,#24211),(#24212,
#24213),(#24214,#24215),(#24216,#24217),(#24218,#24219),(#24220,#24221),
(#24222,#24223),(#24224,#24225),(#24226,#24227),(#24228,#24229),(#24230,
#24231),(#24232,#24233),(#24234,#24235),(#24236,#24237),(#24238,#24239),
(#24240,#24241),(#24242,#24243),(#24244,#24245),(#24246,#24247),(#24248,
#24249),(#24250,#24251),(#24252,#24253),(#24254,#24255),(#24256,#24257),
(#24258,#24259),(#24260,#24261),(#24262,#24263),(#24264,#24265),(#24266,
#24267),(#24268,#24269),(#24270,#24271),(#24272,#24273),(#24274,#24275),
(#24276,#24277),(#24278,#24279),(#24280,#24281),(#24282,#24283),(#24284,
#24285),(#24286,#24287),(#24288,#24289),(#24290,#24291),(#24292,#24293),
(#24294,#24295),(#24296,#24297),(#24298,#24299),(#24300,#24301),(#24302,
#24303),(#24304,#24305),(#24306,#24307),(#24308,#24309),(#24310,#24311),
(#24312,#24313),(#24314,#24315),(#24316,#24317),(#24318,#24319),(#24320,
#24321),(#24322,#24323),(#24324,#24325),(#24326,#24327),(#24328,#24329),
(#24330,#24331),(#24332,#24333),(#24334,#24335),(#24336,#24337),(#24338,
#24339),(#24340,#24341),(#24342,#24343),(#24344,#24345),(#24346,#24347),
(#24348,#24349),(#24350,#24351),(#24352,#24353),(#24354,#24355),(#24356,
#24357),(#24358,#24359),(#24360,#24361),(#24362,#24363),(#24364,#24365),
(#24366,#24367),(#24368,#24369),(#24370,#24371),(#24372,#24373),(#24374,
#24375),(#24376,#24377),(#24378,#24379),(#24380,#24381),(#24382,#24383),
(#24384,#24385),(#24386,#24387),(#24388,#24389),(#24390,#24391),(#24392,
#24393),(#24394,#24395),(#24396,#24397),(#24398,#24399),(#24400,#24401),
(#24402,#24403),(#24404,#24405),(#24406,#24407),(#24408,#24409),(#24410,
#24411),(#24412,#24413),(#24414,#24415),(#24416,#24417),(#24418,#24419),
(#24420,#24421),(#24422,#24423),(#24424,#24425),(#24426,#24427),(#24428,
#24429),(#24430,#24431),(#24432,#24433),(#24434,#24435),(#24436,#24437),
(#24438,#24439),(#24440,#24441),(#24442,#24443),(#24444,#24445),(#24446,
#24447),(#24448,#24449),(#24450,#24451),(#24452,#24453),(#24454,#24455),
(#24456,#24457),(#24458,#24459),(#24460,#24461),(#24462,#24463),(#24464,
#24465),(#24466,#24467),(#24468,#24469),(#24470,#24471),(#24472,#24473),
(#24474,#24475),(#24476,#24477),(#24478,#24479),(#24480,#24481),(#24482,
#24483),(#24484,#24485),(#24486,#24487),(#24488,#24489),(#24490,#24491),
(#24492,#24493),(#24494,#24495),(#24496,#24497),(#24498,#24499),(#24500,
#24501),(#24502,#24503),(#24504,#24505),(#24506,#24507),(#24508,#24509),
(#24510,#24511),(#24512,#24513),(#24514,#24515),(#24516,#24517),(#24518,
#24519),(#24520,#24521),(#24522,#24523),(#24524,#24525),(#24526,#24527),
(#24528,#24529),(#24530,#24531),(#24532,#24533),(#24534,#24535),(#24536,
#24537),(#24538,#24539),(#24540,#24541),(#24542,#24543),(#24544,#24545),
(#24546,#24547),(#24548,#24549),(#24550,#24551),(#24552,#24553),(#24554,
#24555),(#24556,#24557),(#24558,#24559),(#24560,#24561),(#24562,#24563),
(#24564,#24565),(#24566,#24567),(#24568,#24569),(#24570,#24571),(#24572,
#24573),(#24574,#24575),(#24576,#24577),(#24578,#24579),(#24580,#24581),
(#24582,#24583),(#24584,#24585),(#24586,#24587),(#24588,#24589),(#24590,
#24591),(#24592,#24593),(#24594,#24595),(#24596,#24597),(#24598,#24599),
(#24600,#24601),(#24602,#24603),(#24604,#24605),(#24606,#24607),(#24608,
#24609),(#24610,#24611),(#24612,#24613),(#24614,#24615),(#24616,#24617),
(#24618,#24619),(#24620,#24621),(#24622,#24623),(#24624,#24625),(#24626,
#24627),(#24628,#24629),(#24630,#24631),(#24632,#24633),(#24634,#24635),
(#24636,#24637),(#24638,#24639),(#24640,#24641),(#24642,#24643),(#24644,
#24645),(#24646,#24647),(#24648,#24649),(#24650,#24651),(#24652,#24653),
(#24654,#24655),(#24656,#24657),(#24658,#24659),(#24660,#24661),(#24662,
#24663),(#24664,#24665),(#24666,#24667),(#24668,#24669),(#24670,#24671),
(#24672,#24673),(#24674,#24675),(#24676,#24677),(#24678,#24679),(#24680,
#24681),(#24682,#24683),(#24684,#24685),(#24686,#24687),(#24688,#24689),
(#24690,#24691),(#24692,#24693),(#24694,#24695),(#24696,#24697),(#24698,
#24699),(#24700,#24701),(#24702,#24703),(#24704,#24705),(#24706,#24707),
(#24708,#24709),(#24710,#24711),(#24712,#24713),(#24714,#24715),(#24716,
#24717),(#24718,#24719),(#24720,#24721),(#24722,#24723),(#24724,#24725),
(#24726,#24727),(#24728,#24729),(#24730,#24731),(#24732,#24733),(#24734,
#24735),(#24736,#24737),(#24738,#24739),(#24740,#24741),(#24742,#24743),
(#24744,#24745),(#24746,#24747),(#24748,#24749),(#24750,#24751),(#24752,
#24753),(#24754,#24755),(#24756,#24757),(#24758,#24759),(#24760,#24761),
(#24762,#24763),(#24764,#24765),(#24766,#24767),(#24768,#24769),(#24770,
#24771),(#24772,#24773),(#24774,#24775),(#24776,#24777),(#24778,#24779),
(#24780,#24781),(#24782,#24783),(#24784,#24785),(#24786,#24787),(#24788,
#24789),(#24790,#24791),(#24792,#24793),(#24794,#24795),(#24796,#24797),
(#24798,#24799),(#24800,#24801),(#24802,#24803),(#24804,#24805),(#24806,
#24807),(#24808,#24809),(#24810,#24811),(#24812,#24813),(#24814,#24815),
(#24816,#24817),(#24818,#24819),(#24820,#24821),(#24822,#24823),(#24824,
#24825),(#24826,#24827),(#24828,#24829),(#24830,#24831),(#24832,#24833),
(#24834,#24835),(#24836,#24837),(#24838,#24839),(#24840,#24841),(#24842,
#24843),(#24844,#24845),(#24846,#24847),(#24848,#24849),(#24850,#24851),
(#24852,#24853),(#24854,#24855),(#24856,#24857),(#24858,#24859),(#24860,
#24861),(#24862,#24863),(#24864,#24865),(#24866,#24867),(#24868,#24869),
(#24870,#24871),(#24872,#24873),(#24874,#24875),(#24876,#24877),(#24878,
#24879),(#24880,#24881),(#24882,#24883),(#24884,#24885),(#24886,#24887),
(#24888,#24889),(#24890,#24891),(#24892,#24893),(#24894,#24895),(#24896,
#24897),(#24898,#24899),(#24900,#24901),(#24902,#24903),(#24904,#24905),
(#24906,#24907),(#24908,#24909),(#24910,#24911),(#24912,#24913),(#24914,
#24915),(#24916,#24917),(#24918,#24919),(#24920,#24921),(#24922,#24923),
(#24924,#24925),(#24926,#24927),(#24928,#24929),(#24930,#24931),(#24932,
#24933),(#24934,#24935),(#24936,#24937),(#24938,#24939),(#24940,#24941),
(#24942,#24943),(#24944,#24945),(#24946,#24947),(#24948,#24949),(#24950,
#24951),(#24952,#24953),(#24954,#24955),(#24956,#24957),(#24958,#24959),
(#24960,#24961),(#24962,#24963),(#24964,#24965),(#24966,#24967),(#24968,
#24969),(#24970,#24971),(#24972,#24973),(#24974,#24975),(#24976,#24977),
(#24978,#24979),(#24980,#24981),(#24982,#24983),(#24984,#24985),(#24986,
#24987),(#24988,#24989),(#24990,#24991),(#24992,#24993),(#24994,#24995),
(#24996,#24997),(#24998,#24999),(#25000,#25001),(#25002,#25003),(#25004,
#25005),(#25006,#25007),(#25008,#25009),(#25010,#25011),(#25012,#25013),
(#25014,#25015),(#25016,#25017),(#25018,#25019),(#25020,#25021),(#25022,
#25023),(#25024,#25025),(#25026,#25027),(#25028,#25029),(#25030,#25031),
(#25032,#25033),(#25034,#25035),(#25036,#25037),(#25038,#25039),(#25040,
#25041),(#25042,#25043),(#25044,#25045),(#25046,#25047),(#25048,#25049),
(#25050,#25051),(#25052,#25053),(#25054,#25055),(#25056,#25057),(#25058,
#25059),(#25060,#25061),(#25062,#25063),(#25064,#25065),(#25066,#25067),
(#25068,#25069),(#25070,#25071),(#25072,#25073),(#25074,#25075),(#25076,
#25077),(#25078,#25079),(#25080,#25081),(#25082,#25083),(#25084,#25085),
(#25086,#25087),(#25088,#25089),(#25090,#25091),(#25092,#25093),(#25094,
#25095),(#25096,#25097),(#25098,#25099),(#25100,#25101),(#25102,#25103),
(#25104,#25105),(#25106,#25107),(#25108,#25109),(#25110,#25111),(#25112,
#25113),(#25114,#25115),(#25116,#25117),(#25118,#25119),(#25120,#25121),
(#25122,#25123),(#25124,#25125),(#25126,#25127),(#25128,#25129),(#25130,
#25131),(#25132,#25133),(#25134,#25135),(#25136,#25137),(#25138,#25139),
(#25140,#25141),(#25142,#25143),(#25144,#25145),(#25146,#25147),(#25148,
#25149),(#25150,#25151),(#25152,#25153),(#25154,#25155),(#25156,#25157),
(#25158,#25159),(#25160,#25161),(#25162,#25163),(#25164,#25165),(#25166,
#25167),(#25168,#25169),(#25170,#25171),(#25172,#25173),(#25174,#25175),
(#25176,#25177),(#25178,#25179),(#25180,#25181),(#25182,#25183),(#25184,
#25185),(#25186,#25187),(#25188,#25189),(#25190,#25191),(#25192,#25193),
(#25194,#25195),(#25196,#25197),(#25198,#25199),(#25200,#25201),(#25202,
#25203),(#25204,#25205),(#25206,#25207),(#25208,#25209),(#25210,#25211),
(#25212,#25213),(#25214,#25215),(#25216,#25217),(#25218,#25219),(#25220,
#25221),(#25222,#25223),(#25224,#25225),(#25226,#25227),(#25228,#25229),
(#25230,#25231),(#25232,#25233),(#25234,#25235),(#25236,#25237),(#25238,
#25239),(#25240,#25241),(#25242,#25243),(#25244,#25245),(#25246,#25247),
(#25248,#25249),(#25250,#25251),(#25252,#25253),(#25254,#25255),(#25256,
#25257),(#25258,#25259),(#25260,#25261),(#25262,#25263),(#25264,#25265),
(#25266,#25267),(#25268,#25269),(#25270,#25271),(#25272,#25273),(#25274,
#25275),(#25276,#25277),(#25278,#25279),(#25280,#25281),(#25282,#25283),
(#25284,#25285),(#25286,#25287),(#25288,#25289),(#25290,#25291),(#25292,
#25293),(#25294,#25295),(#25296,#25297),(#25298,#25299),(#25300,#25301),
(#25302,#25303),(#25304,#25305),(#25306,#25307),(#25308,#25309),(#25310,
#25311),(#25312,#25313),(#25314,#25315),(#25316,#25317),(#25318,#25319),
(#25320,#25321),(#25322,#25323),(#25324,#25325),(#25326,#25327),(#25328,
#25329),(#25330,#25331),(#25332,#25333),(#25334,#25335),(#25336,#25337),
(#25338,#25339),(#25340,#25341),(#25342,#25343),(#25344,#25345),(#25346,
#25347),(#25348,#25349),(#25350,#25351),(#25352,#25353),(#25354,#25355),
(#25356,#25357),(#25358,#25359),(#25360,#25361),(#25362,#25363),(#25364,
#25365),(#25366,#25367),(#25368,#25369),(#25370,#25371),(#25372,#25373),
(#25374,#25375),(#25376,#25377),(#25378,#25379),(#25380,#25381),(#25382,
#25383),(#25384,#25385),(#25386,#25387),(#25388,#25389),(#25390,#25391),
(#25392,#25393),(#25394,#25395),(#25396,#25397),(#25398,#25399),(#25400,
#25401),(#25402,#25403),(#25404,#25405),(#25406,#25407),(#25408,#25409),
(#25410,#25411),(#25412,#25413),(#25414,#25415),(#25416,#25417),(#25418,
#25419),(#25420,#25421),(#25422,#25423),(#25424,#25425),(#25426,#25427),
(#25428,#25429),(#25430,#25431),(#25432,#25433),(#25434,#25435),(#25436,
#25437),(#25438,#25439),(#25440,#25441),(#25442,#25443),(#25444,#25445),
(#25446,#25447),(#25448,#25449),(#25450,#25451),(#25452,#25453),(#25454,
#25455),(#25456,#25457),(#25458,#25459),(#25460,#25461),(#25462,#25463),
(#25464,#25465),(#25466,#25467),(#25468,#25469),(#25470,#25471),(#25472,
#25473),(#25474,#25475),(#25476,#25477),(#25478,#25479),(#25480,#25481),
(#25482,#25483),(#25484,#25485),(#25486,#25487),(#25488,#25489),(#25490,
#25491),(#25492,#25493),(#25494,#25495),(#25496,#25497),(#25498,#25499),
(#25500,#25501),(#25502,#25503),(#25504,#25505),(#25506,#25507),(#25508,
#25509),(#25510,#25511),(#25512,#25513),(#25514,#25515),(#25516,#25517),
(#25518,#25519),(#25520,#25521),(#25522,#25523),(#25524,#25525),(#25526,
#25527),(#25528,#25529),(#25530,#25531),(#25532,#25533),(#25534,#25535),
(#25536,#25537),(#25538,#25539),(#25540,#25541),(#25542,#25543),(#25544,
#25545),(#25546,#25547),(#25548,#25549),(#25550,#25551),(#25552,#25553),
(#25554,#25555),(#25556,#25557),(#25558,#25559),(#25560,#25561),(#25562,
#25563),(#25564,#25565),(#25566,#25567),(#25568,#25569),(#25570,#25571),
(#25572,#25573),(#25574,#25575),(#25576,#25577),(#25578,#25579),(#25580,
#25581),(#25582,#25583),(#25584,#25585),(#25586,#25587),(#25588,#25589),
(#25590,#25591),(#25592,#25593),(#25594,#25595),(#25596,#25597),(#25598,
#25599),(#25600,#25601),(#25602,#25603),(#25604,#25605),(#25606,#25607),
(#25608,#25609),(#25610,#25611),(#25612,#25613),(#25614,#25615),(#25616,
#25617),(#25618,#25619),(#25620,#25621),(#25622,#25623),(#25624,#25625),
(#25626,#25627),(#25628,#25629),(#25630,#25631),(#25632,#25633),(#25634,
#25635),(#25636,#25637),(#25638,#25639),(#25640,#25641),(#25642,#25643),
(#25644,#25645),(#25646,#25647),(#25648,#25649),(#25650,#25651),(#25652,
#25653),(#25654,#25655),(#25656,#25657),(#25658,#25659),(#25660,#25661),
(#25662,#25663),(#25664,#25665),(#25666,#25667),(#25668,#25669),(#25670,
#25671),(#25672,#25673),(#25674,#25675),(#25676,#25677),(#25678,#25679),
(#25680,#25681),(#25682,#25683),(#25684,#25685),(#25686,#25687),(#25688,
#25689),(#25690,#25691),(#25692,#25693),(#25694,#25695),(#25696,#25697),
(#25698,#25699),(#25700,#25701),(#25702,#25703),(#25704,#25705),(#25706,
#25707),(#25708,#25709),(#25710,#25711),(#25712,#25713),(#25714,#25715),
(#25716,#25717),(#25718,#25719),(#25720,#25721),(#25722,#25723),(#25724,
#25725),(#25726,#25727),(#25728,#25729),(#25730,#25731),(#25732,#25733),
(#25734,#25735),(#25736,#25737),(#25738,#25739),(#25740,#25741),(#25742,
#25743),(#25744,#25745),(#25746,#25747),(#25748,#25749),(#25750,#25751),
(#25752,#25753),(#25754,#25755),(#25756,#25757),(#25758,#25759),(#25760,
#25761),(#25762,#25763),(#25764,#25765),(#25766,#25767),(#25768,#25769),
(#25770,#25771),(#25772,#25773),(#25774,#25775),(#25776,#25777),(#25778,
#25779),(#25780,#25781),(#25782,#25783),(#25784,#25785),(#25786,#25787),
(#25788,#25789),(#25790,#25791),(#25792,#25793),(#25794,#25795),(#25796,
#25797),(#25798,#25799),(#25800,#25801),(#25802,#25803),(#25804,#25805),
(#25806,#25807),(#25808,#25809),(#25810,#25811),(#25812,#25813),(#25814,
#25815),(#25816,#25817),(#25818,#25819),(#25820,#25821),(#25822,#25823),
(#25824,#25825),(#25826,#25827),(#25828,#25829),(#25830,#25831),(#25832,
#25833),(#25834,#25835),(#25836,#25837),(#25838,#25839),(#25840,#25841),
(#25842,#25843),(#25844,#25845),(#25846,#25847),(#25848,#25849),(#25850,
#25851),(#25852,#25853),(#25854,#25855),(#25856,#25857),(#25858,#25859),
(#25860,#25861),(#25862,#25863),(#25864,#25865),(#25866,#25867),(#25868,
#25869),(#25870,#25871),(#25872,#25873),(#25874,#25875),(#25876,#25877),
(#25878,#25879),(#25880,#25881),(#25882,#25883),(#25884,#25885),(#25886,
#25887),(#25888,#25889),(#25890,#25891),(#25892,#25893),(#25894,#25895),
(#25896,#25897),(#25898,#25899),(#25900,#25901),(#25902,#25903),(#25904,
#25905),(#25906,#25907),(#25908,#25909),(#25910,#25911),(#25912,#25913),
(#25914,#25915),(#25916,#25917),(#25918,#25919),(#25920,#25921),(#25922,
#25923),(#25924,#25925),(#25926,#25927),(#25928,#25929),(#25930,#25931),
(#25932,#25933),(#25934,#25935),(#25936,#25937),(#25938,#25939),(#25940,
#25941),(#25942,#25943),(#25944,#25945),(#25946,#25947),(#25948,#25949)),
 .UNSPECIFIED.,.F.,.F.,.F.,(4,1,1,1,1,1,1,1,1,1,1,1,1,1,1,1,1,1,1,1,1,1,
1,1,1,1,1,1,1,1,1,1,1,1,1,1,1,1,1,1,1,1,1,1,1,1,1,1,1,1,1,1,1,1,1,1,1,1,
1,1,1,1,1,1,1,1,1,1,1,1,1,1,1,1,1,1,1,1,1,1,1,1,1,1,1,1,1,1,1,1,1,1,1,1,
1,1,1,1,1,1,1,1,1,1,1,1,1,1,1,1,1,1,1,1,1,1,1,1,1,1,1,1,1,1,1,1,1,1,1,1,
1,1,1,1,1,1,1,1,1,1,1,1,1,1,1,1,1,1,1,1,1,1,1,1,1,1,1,1,1,1,1,1,1,1,1,1,
1,1,1,1,1,1,1,1,1,1,1,1,1,1,1,1,1,1,1,1,1,1,1,1,1,1,1,1,1,1,1,1,1,1,1,1,
1,1,1,1,1,1,1,1,1,1,1,1,1,1,1,1,1,1,1,1,1,1,1,1,1,1,1,1,1,1,1,1,1,1,1,1,
1,1,1,1,1,1,1,1,1,1,1,1,1,1,1,1,1,1,1,1,1,1,1,1,1,1,1,1,1,1,1,1,1,1,1,1,
1,1,1,1,1,1,1,1,1,1,1,1,1,1,1,1,1,1,1,1,1,1,1,1,1,1,1,1,1,1,1,1,1,1,1,1,
1,1,1,1,1,1,1,1,1,1,1,1,1,1,1,1,1,1,1,1,1,1,1,1,1,1,1,1,1,1,1,1,1,1,1,1,
1,1,1,1,1,1,1,1,1,1,1,1,1,1,1,1,1,1,1,1,1,1,1,1,1,1,1,1,1,1,1,1,1,1,1,1,
1,1,1,1,1,1,1,1,1,1,1,1,1,1,1,1,1,1,1,1,1,1,1,1,1,1,1,1,1,1,1,1,1,1,1,1,
1,1,1,1,1,1,1,1,1,1,1,1,1,1,1,1,1,1,1,1,1,1,1,1,1,1,1,1,1,1,1,1,1,1,1,1,
1,1,1,1,1,1,1,1,1,1,1,1,1,1,1,1,1,1,1,1,1,1,1,1,1,1,1,1,1,1,1,1,1,1,1,1,
1,1,1,1,1,1,1,1,1,1,1,1,1,1,1,1,1,1,1,1,1,1,1,1,1,1,1,1,1,1,1,1,1,1,1,1,
1,1,1,1,1,1,1,1,1,1,1,1,1,1,1,1,1,1,1,1,1,1,1,1,1,1,1,1,1,1,1,1,1,1,1,1,
1,1,1,1,1,1,1,1,1,1,1,1,1,1,1,1,1,1,1,1,1,1,1,1,1,1,1,1,1,1,1,1,1,1,1,1,
1,1,1,1,1,1,1,1,1,1,1,1,1,1,1,1,1,1,1,1,1,1,1,1,1,1,1,1,1,1,1,1,1,1,1,1,
1,1,1,1,1,1,1,1,1,1,1,1,1,1,1,1,1,1,1,1,1,1,1,1,1,1,1,1,1,1,1,1,1,1,1,1,
1,1,1,1,1,1,1,1,1,1,1,1,1,1,1,1,1,1,1,1,1,1,1,1,1,1,1,1,1,1,1,1,1,1,1,1,
1,1,1,1,1,1,1,1,1,1,1,1,1,1,1,1,1,1,1,1,1,1,1,1,1,1,1,1,1,1,1,1,1,1,1,1,
1,1,1,1,1,1,1,1,1,1,1,1,1,1,1,1,1,1,1,1,1,1,1,1,1,1,1,1,1,1,1,1,1,1,1,1,
1,1,1,1,1,1,1,1,1,1,1,1,1,1,1,1,1,1,1,1,1,1,1,1,1,1,1,1,1,1,1,1,1,1,1,1,
1,1,1,1,1,1,1,1,1,1,1,1,1,1,1,1,1,1,1,1,1,1,1,1,1,1,1,1,1,1,1,1,1,1,1,1,
1,1,1,1,1,1,1,1,1,1,1,1,1,1,1,1,1,1,1,1,1,1,1,1,1,1,1,1,1,1,1,1,1,1,1,1,
1,1,1,1,1,1,1,1,1,1,1,1,1,1,1,1,1,1,1,1,1,1,1,1,1,1,1,1,1,1,1,1,1,1,1,1,
1,1,1,1,1,1,1,1,1,1,1,1,1,1,1,1,1,1,1,1,1,1,1,1,1,1,1,1,1,1,1,1,1,1,1,1,
1,1,1,1,1,1,1,1,1,1,1,1,1,1,1,1,1,1,1,1,1,1,1,1,1,1,1,1,1,1,1,1,1,1,1,1,
1,1,1,1,1,1,1,1,1,1,1,1,1,1,1,1,1,1,1,1,1,1,1,1,1,1,1,1,1,1,1,1,1,1,1,1,
1,1,1,1,1,1,1,1,1,1,1,1,1,1,1,1,1,1,1,1,1,1,1,1,1,1,1,1,1,1,1,1,1,1,1,1,
1,1,1,1,1,1,1,1,1,1,1,1,1,1,1,1,1,1,1,1,1,1,1,1,1,1,1,1,1,1,1,1,1,1,1,1,
1,1,1,1,1,1,1,1,1,1,1,1,1,1,1,1,1,1,1,1,1,1,1,1,1,1,1,1,1,1,1,1,1,1,1,1,
1,1,1,1,1,1,1,1,1,1,1,1,1,1,1,1,1,1,1,1,1,1,1,1,1,1,1,1,1,1,1,1,1,1,1,1,
1,1,1,1,1,1,1,1,1,1,1,1,1,1,1,1,1,1,1,1,1,1,1,1,1,1,1,1,1,1,1,1,1,1,1,1,
1,1,1,1,1,1,1,1,1,1,1,1,1,1,1,1,1,1,1,1,1,1,1,1,1,1,1,1,1,1,1,1,1,1,1,1,
1,1,1,1,1,1,1,1,1,1,1,1,1,1,1,1,1,1,1,1,1,1,1,1,1,1,1,1,1,1,1,1,1,1,1,1,
1,1,1,1,1,1,1,1,1,1,1,1,1,1,1,1,1,1,1,1,1,1,1,1,1,1,1,1,1,1,1,1,1,1,1,1,
1,1,1,1,1,1,1,1,1,1,1,1,1,1,1,1,1,1,1,1,1,1,1,1,1,1,1,1,1,1,1,1,1,1,1,1,
1,1,1,1,1,1,1,1,1,1,1,1,1,1,1,1,1,1,1,1,1,1,1,1,1,1,1,1,1,1,1,1,1,1,1,1,
1,1,1,1,1,1,1,1,1,1,1,1,1,1,1,1,1,1,1,1,1,1,1,1,1,1,1,1,1,1,1,1,1,1,1,1,
1,1,1,1,1,1,1,1,1,1,1,1,1,1,1,1,1,1,1,1,1,1,1,1,1,1,1,1,1,1,1,1,1,1,1,1,
1,1,1,1,1,1,1,1,1,1,1,1,1,1,1,1,1,1,1,1,1,1,1,1,1,1,1,1,1,1,1,1,1,1,1,1,
1,1,1,1,1,1,1,1,1,1,1,1,1,1,1,1,1,1,1,1,1,1,1,1,1,1,1,1,1,1,1,1,1,1,1,1,
1,1,1,1,1,1,1,1,1,1,1,1,1,1,1,1,1,1,1,1,1,1,1,1,1,1,1,1,1,1,1,1,1,1,1,1,
1,1,1,1,1,1,1,1,1,1,1,1,1,1,1,1,1,1,1,1,1,1,1,1,1,1,1,1,1,1,1,1,1,1,1,1,
1,1,1,1,1,1,1,1,1,1,1,1,1,1,1,1,1,1,1,1,1,1,1,1,1,1,1,1,1,1,1,1,1,1,1,1,
1,1,1,1,1,1,1,1,1,1,1,1,1,1,1,1,1,1,1,1,1,1,1,1,1,1,1,1,1,1,1,1,1,1,1,1,
1,1,1,1,1,1,1,1,1,1,1,1,1,1,1,1,1,1,1,1,1,1,1,1,1,1,1,1,1,1,1,1,1,1,1,1,
1,1,1,1,1,1,1,1,1,1,1,1,1,1,1,1,1,1,1,1,1,1,1,1,1,1,1,1,1,1,1,1,1,1,1,1,
1,1,1,1,1,1,1,1,1,1,1,1,1,1,1,1,1,1,1,1,1,1,1,1,1,1,1,1,1,1,1,1,1,1,1,1,
1,1,1,1,1,1,1,1,1,1,1,1,1,1,1,1,1,1,1,1,1,1,1,1,1,1,1,1,1,1,1,1,1,1,1,1,
1,1,1,1,1,1,1,1,1,1,1,1,1,1,1,1,1,1,1,1,1,1,1,1,1,1,1,1,1,1,1,1,1,1,1,1,
1,1,1,1,1,1,1,1,1,1,1,1,1,1,1,1,1,1,1,1,1,1,1,1,1,1,1,1,1,1,1,1,1,1,1,1,
1,1,1,1,1,1,1,1,1,1,1,1,1,1,1,1,1,1,1,1,1,1,1,1,1,1,1,1,1,1,1,1,1,1,1,1,
1,1,1,1,1,1,1,1,1,1,1,1,1,1,1,1,1,1,1,1,1,1,1,1,1,1,1,1,1,1,1,1,1,1,1,1,
1,1,1,1,1,1,1,1,1,1,1,1,1,1,1,1,1,1,1,1,1,1,1,1,1,1,1,1,1,1,1,1,1,1,1,1,
1,1,1,1,1,1,1,1,1,1,1,1,1,1,1,1,1,1,1,1,1,1,1,1,1,1,1,1,1,1,1,1,1,1,1,1,
1,1,1,1,1,1,1,1,1,1,1,1,1,1,1,1,1,1,1,1,1,1,1,1,1,1,1,1,1,1,1,1,1,1,1,1,
1,1,1,1,1,1,1,1,1,1,1,1,1,1,1,1,1,1,1,1,1,1,1,1,1,1,1,1,1,1,1,1,1,1,1,1,
1,1,1,1,1,1,1,1,1,1,1,1,1,1,1,1,1,1,1,1,1,1,1,1,1,1,1,1,1,1,1,1,1,1,1,1,
1,1,1,1,1,1,1,1,1,1,1,1,1,1,1,1,1,1,1,1,1,1,1,1,1,1,1,1,1,1,1,1,1,1,1,1,
1,1,1,1,1,1,1,1,1,1,1,1,1,1,1,1,1,1,1,1,1,1,1,1,1,1,1,1,1,1,1,1,1,1,1,1,
1,1,1,1,1,1,1,1,1,1,1,1,1,1,1,1,1,1,1,1,1,1,1,1,1,1,1,1,1,1,1,1,1,1,1,1,
1,1,1,1,1,1,1,1,1,1,1,1,1,1,1,1,1,1,1,1,1,1,1,1,1,1,1,1,1,1,1,1,1,1,1,1,
1,1,1,1,1,1,1,1,1,1,1,1,1,1,1,1,1,1,1,1,1,1,1,1,1,1,1,1,1,1,1,1,1,1,1,1,
1,1,1,1,1,1,1,1,1,1,1,1,1,1,1,1,1,1,1,1,1,1,1,1,1,1,1,1,1,1,1,1,1,1,1,1,
1,1,1,1,1,1,1,1,1,1,1,1,1,1,1,1,1,1,1,1,1,1,1,1,1,1,1,1,1,1,1,1,1,1,1,1,
1,1,1,1,1,1,1,1,1,1,1,1,1,1,1,1,1,1,1,1,1,1,1,1,1,1,1,1,1,1,1,1,1,1,1,1,
1,1,1,1,1,1,1,1,1,1,1,1,1,1,1,1,1,1,1,1,1,1,1,1,1,1,1,1,1,1,1,1,1,1,1,1,
1,1,1,1,1,1,1,1,1,1,1,1,1,1,1,1,1,1,1,1,1,1,1,1,1,1,1,1,1,1,1,1,1,1,1,1,
1,1,1,1,1,1,1,1,1,1,1,1,1,1,1,1,1,1,1,1,1,1,1,1,1,1,1,1,1,1,1,1,1,1,1,1,
1,1,1,1,1,1,1,1,1,1,1,1,1,1,1,1,1,1,1,1,1,1,1,1,1,1,1,1,1,1,1,1,1,1,1,1,
1,1,1,1,1,1,1,1,1,1,1,1,1,1,1,1,1,1,1,1,1,1,1,1,1,1,1,1,1,1,1,1,1,1,1,1,
1,1,1,1,1,1,1,1,1,1,1,1,1,1,1,1,1,1,1,1,1,1,1,1,1,1,1,1,1,1,1,1,1,1,1,1,
1,1,1,1,1,1,1,1,1,1,1,1,1,1,1,1,1,1,1,1,1,1,1,1,1,1,1,1,1,1,1,1,1,1,1,1,
1,1,1,1,1,1,1,1,1,1,1,1,1,1,1,1,1,1,1,1,1,1,1,1,1,1,1,1,1,1,1,1,1,1,1,1,
1,1,1,1,1,1,1,1,1,1,1,1,1,1,1,1,1,1,1,1,1,1,1,1,1,1,1,1,1,1,1,1,1,1,1,1,
1,1,1,1,1,1,1,1,1,1,1,1,1,1,1,1,1,1,1,1,1,1,1,1,1,1,1,1,1,1,1,1,1,1,1,1,
1,1,1,1,1,1,1,1,1,1,1,1,1,1,1,1,1,1,1,1,1,1,1,1,1,1,1,1,1,1,1,1,1,1,1,1,
1,1,1,1,1,1,1,1,1,1,1,1,1,1,1,1,1,1,1,1,1,1,1,1,1,1,1,1,1,1,1,1,1,1,1,1,
1,1,1,1,1,1,1,1,1,1,1,1,1,1,1,1,1,1,1,1,1,1,1,1,1,1,1,1,1,1,1,1,1,1,1,1,
1,1,1,1,1,1,1,1,1,1,1,1,1,1,1,1,1,1,1,1,1,1,1,1,1,1,1,1,1,1,1,1,1,1,1,1,
1,1,1,1,1,1,1,1,1,1,1,1,1,1,1,1,1,1,1,1,1,1,1,1,1,1,1,1,1,1,1,1,1,1,1,1,
1,1,1,1,1,1,1,1,1,1,1,1,1,1,1,1,1,1,1,1,1,1,1,1,1,1,1,1,1,1,1,1,1,1,1,1,
1,1,1,1,1,1,1,1,1,1,1,1,1,1,1,1,1,1,1,1,1,1,1,1,1,1,1,1,1,1,1,1,1,1,1,1,
1,1,1,1,1,1,1,1,1,1,1,1,1,1,1,1,1,1,1,1,1,1,1,1,1,1,1,1,1,1,1,1,1,1,1,1,
1,1,1,1,1,1,1,1,1,1,1,1,1,1,1,1,1,1,1,1,1,1,1,1,1,1,1,1,1,1,1,1,1,1,1,1,
1,1,1,1,1,1,1,1,1,1,1,1,1,1,1,1,1,1,1,1,1,1,1,1,1,1,1,1,1,1,1,1,1,1,1,1,
1,1,1,1,1,1,1,1,1,1,1,1,1,1,1,1,1,1,1,1,1,1,1,1,1,1,1,1,1,1,1,1,1,1,1,1,
1,1,1,1,1,1,1,1,1,1,1,1,1,1,1,1,1,1,1,1,1,1,1,1,1,1,1,1,1,1,1,1,1,1,1,1,
1,1,1,1,1,1,1,1,1,1,1,1,1,1,1,1,1,1,1,1,1,1,1,1,1,1,1,1,1,1,1,1,1,1,1,1,
1,1,1,1,1,1,1,1,1,1,1,1,1,1,1,1,1,1,1,1,1,1,1,1,1,1,1,1,1,1,1,1,1,1,1,1,
1,1,1,1,1,1,1,1,1,1,1,1,1,1,1,1,1,1,1,1,1,1,1,1,1,1,1,1,1,1,1,1,1,1,1,1,
1,1,1,1,1,1,1,1,1,1,1,1,1,1,1,1,1,1,1,1,1,1,1,1,1,1,1,1,1,1,1,1,1,1,1,1,
1,1,1,1,1,1,1,1,1,1,1,1,1,1,1,1,1,1,1,1,1,1,1,1,1,1,1,1,1,1,1,1,1,1,1,1,
1,1,1,1,1,1,1,1,1,1,1,1,1,1,1,1,1,1,1,1,1,1,1,1,1,1,1,1,1,1,1,1,1,1,1,1,
1,1,1,1,1,1,1,1,1,1,1,1,1,1,1,1,1,1,1,1,1,1,1,1,1,1,1,1,1,1,1,1,1,1,1,1,
1,1,1,1,4),(2,2),(0.,0.869746702321014,1.7394931589914,2.60923976624962,
3.47983908319159,4.35043840179749,5.22018503077054,6.08993165951504,6.95967828799171,
7.82942491616733,8.69917154401062,9.56891817149224,10.4395174886835,11.3101168056706,
12.179863432132,13.049610058144,13.9193566836854,14.7891033087372,15.6588499332817,
16.5285965573034,17.3991958717975,18.2697951860185,18.7046684974166,19.1395418086746,
19.5744151197912,20.0092884307654,20.4441617415962,20.8790350522825,21.7487816732187,
22.1836549834672,22.6185282935685,23.0534016035221,23.4882749133276,23.9231482229848,
24.3588742245859,24.794600226187,25.2294735355468,26.0992201538203,26.5340934627341,
26.9689667714994,27.4038400801166,27.838713388586,28.2735866969081,28.7084600050832,
29.143333313112,29.5782066209952,30.0130799287334,30.4479532363275,30.8828265437783,
31.3185525442794,31.7542785447804,32.1891518519474,32.6240251589741,33.0588984658616,
33.4937717726112,33.928645079224,34.3635183857014,34.7983916920448,35.2332649982556,
35.6681383043353,36.1030116102854,36.5378849161076,36.9727582218035,37.4076315273749,
37.8425048328235,38.2782308323341,38.7139568318446,39.1488301370532,39.5837034421446,
40.0185767471208,40.4534500519838,40.8883233567357,41.3231966613787,41.7580699659148,
42.1929432703463,42.6278165746754,43.0626898789044,43.4975631830356,43.9324364870714,
44.3673097910142,44.8021830948664,45.2379090935952,45.673635092324,46.1085083960024,
46.5433816995978,46.9782550031127,47.4131283065497,47.8480016099115,48.2828749132006,
48.7177482164198,49.1526215195718,49.5874948226593,50.0223681256851,50.457241428652,
50.8921147315628,51.3269880344203,51.7618613372274,52.197587335454,52.6333133336805,
53.0681866363954,53.5030599390685,53.9379332417027,54.3728065443011,54.8076798468664,
55.2425531494018,55.6774264519101,56.1122997543943,56.5471730568575,56.9820463593026,
57.4169196617326,57.8517929641506,58.2866662665595,58.7215395689624,59.157265567009,
59.5929915650557,60.0278648674556,60.4627381698584,60.8976114722673,61.3324847746853,
61.7673580771153,62.2022313795604,62.6371046820236,63.0719779845079,63.5068512870162,
63.9417245895516,64.376597892117,64.8114711947155,65.2463444973499,65.6812178000231,
66.1169437982275,66.5526697964318,66.9875430991915,67.4224164019987,67.8572897048563,
68.2921630077673,68.7270363107343,69.1619096137603,69.5967829168479,70.0316562200001,
70.4665295232194,70.9014028265087,71.3362761298705,71.7711494333077,72.2060227368227,
72.6408960404182,73.0766220391044,73.5123480377905,73.9472213415547,74.382094645407,
74.8169679493499,75.2518412533859,75.6867145575172,76.1215878617464,76.5564611660756,
76.9913344705072,77.4262077750435,77.8610810796866,78.2959543844386,78.7308276893018,
79.1657009942781,79.6005742993696,80.0363002988208,80.4720262982719,80.9068996035997,
81.3417729090484,81.7766462146199,82.211519520316,82.6463928261383,83.0812661320886,
83.5161394381684,83.9510127443794,84.3858860507229,84.8207593572004,85.2556326638134,
85.6905059705631,86.1253792774507,86.5602525844776,86.995978584908,87.4317045853384,
87.8665778926469,88.3014512000977,88.7363245076919,89.1711978154302,89.6060711233134,
90.0409444313423,90.4758177395175,90.9106910478396,91.345564356309,91.7804376649263,
92.2153109736917,92.6501842826055,93.085057591668,93.5199309008791,93.9556569024059,
94.3913829039327,94.8262562134414,95.2611295230986,95.6960028329042,96.1308761428578,
96.5657494529591,97.0006227632077,97.4354960736028,97.870369384144,98.3052426948304,
98.7401160056612,99.1749893166354,99.6098626277522,100.04473593901,100.915335253024,
101.351061255639,101.785934567313,102.220807879124,102.655681191068,103.090554503145,
103.525427815353,104.395174440154,105.264921065453,105.699794378283,106.134667691232,
106.569541004295,107.004414317471,107.8750136343,108.745612951339,109.615359578629,
110.485106206296,111.354852834309,112.224599462639,113.094346091254,113.964092720119,
114.834692038763,115.705291357499,116.575037986826,117.444784616267,118.314531245777,
119.184277875311,120.054024504821,120.923771134261,121.794370453112,122.66496977189,
123.534716400968,124.404463029834,125.274209658448,126.143956286779,127.013702914792,
127.883449542458,128.754048859798,129.624648176939,130.494394803617,131.364141429857,
132.233888055637,133.103634680937,133.973381305737,134.843127930023,135.71372724472,
136.584326559147,137.019199870684,137.454073182083,137.888946493341,138.323819804458,
139.193566426263,140.063313047491,140.498186357887,140.933059668136,141.367932978237,
141.802806288191,142.237679597997,142.673405599673,143.109131601348,143.544004910857,
143.978878220217,144.413751529429,144.848624838491,145.283498147405,145.718371456171,
146.153244764789,146.588118073258,147.022991381581,147.457864689756,147.892737997785,
148.327611305669,148.762484613407,149.197357921002,149.633083921574,150.068809922147,
150.503683229455,150.938556536623,151.37342984365,151.808303150538,152.243176457288,
152.678049763901,153.112923070379,153.547796376722,153.982669682934,154.417542989014,
154.852416294964,155.287289600787,155.722162906483,156.157036212055,156.592762211626,
157.028488211198,157.463361516526,157.898234821735,158.333108126826,158.767981431803,
159.202854736666,159.637728041419,160.072601346062,160.507474650599,160.94234795503,
161.37722125936,161.812094563589,162.246967867721,162.681841171757,163.1167144757,
163.552440474473,163.988166473247,164.423039777011,164.85791308069,165.292786384286,
165.727659687801,166.162532991238,166.597406294601,167.03227959789,167.46715290111,
167.902026204262,168.33689950735,168.771772810376,169.206646113343,169.641519416254,
170.076392719112,170.512118717363,170.947844715614,171.382718018374,171.817591321089,
172.252464623762,172.687337926397,173.122211228996,173.557084531561,173.991957834097,
174.426831136606,174.86170443909,175.296577741554,175.731451044,176.16632434643,
176.601197648848,177.036070951258,177.471796949306,177.907522947355,178.342396249755,
178.777269552155,179.212142854558,179.647016156968,180.081889459386,180.516762761816,
180.951636064262,181.386509366726,181.82138266921,182.256255971719,182.691129274255,
183.12600257682,183.560875879419,183.995749182054,184.431475180237,184.867201178421,
185.302074481136,185.736947783896,186.171821086704,186.606694389561,187.041567692473,
187.47644099544,187.911314298466,188.346187601554,188.781060904706,189.215934207926,
189.650807511215,190.085680814577,190.520554118015,190.95542742153,191.391153420175,
191.82687941882,192.261752722499,192.696626026263,193.131499330116,193.566372634059,
194.001245938095,194.436119242227,194.870992546456,195.305865850785,195.740739155217,
196.175612459754,196.610485764397,197.045359069149,197.480232374013,197.915105678989,
198.350831678382,198.786557677775,199.221430982984,199.656304288312,200.091177593761,
200.526050899333,200.960924205029,201.395797510852,201.830670816802,202.265544122882,
202.700417429093,203.135290735437,203.570164041915,204.005037348528,204.439910655278,
204.874783962166,205.310509962526,205.746235962887,206.181109270054,206.615982577363,
207.050855884814,207.485729192409,207.920602500147,208.355475808031,208.79034911606,
209.225222424235,209.660095732558,210.094969041027,210.529842349645,210.96471565841,
211.399588967324,211.834462276387,212.27018827784,212.705914279292,213.140787588653,
213.575660898161,214.010534207819,214.880280827579,215.31515413768,215.750027447929,
216.184900758324,216.619774068866,217.054647379553,217.489520690384,218.359267312475,
219.22986662628,219.665592628826,220.100465940363,220.535339252038,220.970212563848,
221.83995918787,222.709705812416,223.579452437468,224.014325750179,224.44919906301,
225.318945689022,226.189545005688,227.060144322571,227.929890949664,228.799637577146,
229.66938420499,230.539130833166,231.408877461643,232.278624090388,233.149223408954,
234.019822727623,234.889569356878,235.759315986267,236.629062615749,237.498809245277,
238.368555874806,239.238302504287,240.108901823183,240.979501142017,241.849247771189,
242.718994400167,243.588741028911,244.458487657389,245.328234285565,246.197980913409,
247.068580230891,247.939179548182,248.80892617507,249.678672801532,250.548419427545,
251.418166053087,252.287912678139,253.157659302684,254.028258617581,254.898857932211,
255.333731243885,255.768604555423,256.203477866821,256.63835117808,257.508097800171,
258.377844421689,258.812717732231,259.247591042627,259.682464352876,260.117337662977,
260.552210972931,260.987936974682,261.858536286089,262.293409595598,262.728282904958,
263.16315621417,263.598029523233,264.032902832147,264.467776140913,264.902649449531,
265.337522758001,265.772396066323,266.207269374499,266.642142682528,267.077015990412,
267.511889298151,267.947615298795,268.383341299439,268.81821460689,269.2530879142,
269.687961221367,270.122834528394,270.557707835282,270.992581142032,271.427454448646,
271.862327755124,272.297201061468,272.732074367679,273.166947673759,273.60182097971,
274.036694285533,274.471567591229,274.907293590862,275.343019590495,275.777892895944,
276.212766201272,276.647639506481,277.082512811573,277.51738611655,277.952259421414,
278.387132726166,278.82200603081,279.256879335346,279.691752639779,280.126625944108,
280.561499248338,280.996372552469,281.431245856506,281.866971855324,282.302697854143,
282.737571157996,283.172444461761,283.60731776544,284.042191069036,284.477064372551,
284.911937675989,285.346810979351,285.781684282641,286.216557585861,286.651430889013,
287.086304192101,287.521177495128,287.956050798095,288.390924101007,288.826650099283,
289.262376097559,289.697249400366,290.132122703127,290.566996005842,291.001869308516,
291.43674261115,291.871615913749,292.306489216315,292.741362518851,293.17623582136,
293.611109123845,294.045982426308,294.480855728754,294.915729031185,295.350602333603,
295.786328331655,296.222054329707,296.65692763211,297.091800934511,297.526674236911,
297.961547539314,298.396420841724,298.831294144142,299.266167446573,299.701040749018,
300.135914051482,300.570787353967,301.005660656476,301.440533959012,301.875407261578,
302.310280564177,302.746006562341,303.181732560506,303.616605863179,304.051479165895,
304.486352468655,304.921225771462,305.35609907432,305.790972377232,306.225845680199,
306.660718983226,307.095592286314,307.530465589466,307.965338892686,308.400212195976,
308.835085499338,309.269958802776,309.705684801381,310.141410799985,310.576284103581,
311.01115740726,311.446030711025,311.880904014878,312.315777318821,312.750650622858,
313.185523926989,313.620397231219,314.055270535549,314.490143839981,314.925017144517,
315.359890449161,315.794763753913,316.229637058777,316.665363058112,317.101089057448,
317.53596236254,317.970835667749,318.405708973077,318.840582278526,319.275455584098,
319.710328889795,320.145202195618,320.580075501568,321.014948807648,321.44982211386,
321.884695420204,322.319568726682,322.754442033295,323.189315340045,323.625041340336,
324.060767340628,324.495640647655,324.930513954822,325.365387262131,325.800260569583,
326.235133877177,326.670007184916,327.1048804928,327.539753800829,327.974627109005,
328.409500417327,328.844373725797,329.279247034415,329.714120343181,330.148993652095,
330.584719653474,331.020445654852,331.455318964064,331.890192273424,332.325065582933,
332.759938892591,333.194812202397,333.629685512351,334.064558822453,334.499432132702,
334.934305443098,335.369178753639,335.804052064326,336.673798686132,337.108671997249,
337.544397999725,337.980124002201,338.4149973136,338.849870625137,339.284743936812,
340.154490560568,341.024237184854,341.459110497191,341.893983809655,342.328857122244,
342.763730434955,343.633477060735,344.504076377234,345.374675693955,346.244422320844,
347.114168948136,347.983915575803,348.853662203817,349.723408832148,350.593155460764,
351.463754779246,352.334354097839,353.204100727012,354.07384735634,354.943593985781,
355.813340615292,356.683087244827,357.552833874338,358.423433193272,359.294032512154,
360.163779141409,361.033525770489,361.903272399355,362.77301902797,363.642765656301,
364.512512284316,365.383111601936,366.253710919371,367.123457546465,367.993204173143,
368.862950799383,369.732697425164,370.602444050463,371.472190675265,372.342789990359,
373.21338930519,373.648262617,374.083135928675,374.952882551611,375.822629173987,
376.257502484962,376.692375795793,377.12724910648,377.562122417021,377.996995727417,
378.431869037666,378.866742347767,379.302468349591,379.738194351416,380.173067661222,
380.607940970879,381.042814280388,381.477687589749,381.91256089896,382.347434208023,
382.782307516937,383.217180825703,383.652054134321,384.086927442791,384.521800751113,
384.956674059289,385.391547367318,385.826420675202,386.262146675918,386.697872676635,
387.13274598423,387.567619291681,388.00249259899,388.437365906157,388.872239213185,
389.307112520073,389.741985826823,390.176859133436,390.611732439914,391.046605746258,
391.48147905247,391.91635235855,392.351225664501,392.786098970323,393.221824970019,
393.657550969714,394.092424275286,394.527297580735,394.962170886063,395.397044191272,
395.831917496364,396.266790801341,396.701664106204,397.136537410957,397.5714107156,
398.006284020137,398.441157324569,398.876030628899,399.310903933128,399.74577723726,
400.181503236126,400.617229234991,401.052102538934,401.486975842787,401.921849146551,
402.356722450231,402.791595753827,403.226469057342,403.66134236078,404.096215664142,
404.531088967432,404.965962270651,405.400835573804,405.835708876892,406.270582179918,
406.705455482886,407.141181481189,407.576907479491,408.01178078235,408.446654085157,
408.881527387917,409.316400690633,409.751273993306,410.186147295941,410.62102059854,
411.055893901106,411.490767203642,411.925640506151,412.360513808636,412.795387111099,
413.230260413545,413.665133715976,414.100859714032,414.536585712088,414.971459014498,
415.406332316901,415.841205619301,416.276078921702,416.710952224105,417.145825526515,
417.580698828933,418.015572131364,418.45044543381,418.885318736273,419.320192038758,
419.755065341267,420.189938643803,420.624811946369,421.060537944515,421.496263942662,
421.931137245297,422.36601054797,422.800883850686,423.235757153446,423.670630456253,
424.105503759112,424.540377062023,424.975250364991,425.410123668017,425.844996971105,
426.279870274258,426.714743577477,427.149616880767,427.584490184129,428.020216182695,
428.455942181261,428.890815484776,429.325688788373,429.760562092052,430.195435395816,
430.630308699669,431.065182003612,431.500055307649,431.93492861178,432.36980191601,
432.80467522034,433.239548524772,433.674421829309,434.109295133952,434.544168438705,
434.979894437984,435.415620437262,435.850493742239,436.285367047331,436.72024035254,
437.155113657869,437.589986963318,438.024860268889,438.459733574586,438.894606880409,
439.32948018636,439.76435349244,440.199226798651,440.634100104995,441.068973411473,
441.503846718087,441.939572718309,442.375298718531,442.810172025419,443.245045332447,
443.679918639614,444.114791946923,444.549665254374,444.984538561969,445.419411869708,
445.854285177591,446.289158485621,446.724031793796,447.158905102119,447.593778410589,
448.028651719207,448.463525027973,448.899251029277,449.334977030581,449.769850339644,
450.639596958216,451.074470267725,451.509343577383,451.944216887189,452.379090197143,
452.813963507244,453.248836817493,453.683710127889,454.118583438431,454.553456749117,
454.988330059949,455.423203370923,455.858929373329,456.294655375734,456.729528686993,
457.164401998391,457.599275309929,458.469021933414,458.90389524536,459.338768557437,
459.773641869646,460.208515181983,460.643388494447,461.078261807036,461.948008432578,
462.818607748906,463.689207065461,464.55895369214,465.428700319234,466.298446946716,
467.16819357456,468.037940202737,468.907686831215,469.778286149605,470.648885468116,
471.518632097196,472.388378726451,473.258125355841,474.127871985322,474.997618614851,
475.86736524438,476.737964563343,477.608563882265,478.478310511593,479.348057140765,
480.217803769743,481.087550398488,481.957297026966,482.827043655142,483.697642972895,
484.568242290469,485.43798891776,486.307735544649,487.177482171112,488.047228797125,
488.916975422667,489.78672204772,490.657321363009,491.09304736596,491.527920678038,
492.397667301793,493.267413925005,494.137160547663,494.57203385878,495.006907169755,
495.441780480586,495.876653791273,496.311527101814,496.74640041221,497.616999724357,
498.052725726255,498.487599036209,498.922472346015,499.357345655673,499.792218965182,
500.227092274542,500.661965583754,501.096838892816,501.531712201731,501.966585510497,
502.401458819114,502.836332127584,503.271205435907,503.706078744082,504.140952052112,
504.576678052901,505.01240405369,505.447277361429,505.882150669023,506.317023976474,
506.751897283783,507.186770590951,507.621643897978,508.056517204866,508.491390511616,
508.92626381823,509.361137124708,509.796010431052,510.230883737263,510.665757043344,
511.100630349294,511.536356349053,511.972082348811,512.406955654506,512.841828960076,
513.276702265523,513.711575570849,514.146448876056,514.581322181146,515.016195486121,
515.451068790983,515.885942095733,516.320815400375,516.75568870491,517.19056200934,
517.625435313668,518.060308617896,518.496034616807,518.931760615718,519.366633919752,
519.801507223694,520.236380527545,520.671253831307,521.106127134985,521.541000438579,
521.975873742092,522.410747045528,522.845620348888,523.280493652176,523.715366955394,
524.150240258545,524.585113561631,525.019986864656,525.455712862985,525.891438861313,
526.326312164223,526.761185467079,527.196058769885,527.630932072643,528.065805375356,
528.500678678029,528.935551980661,529.370425283258,529.805298585822,530.240171888356,
530.675045190863,531.109918493346,531.544791795808,531.979665098252,532.415391096312,
532.851117094373,533.285990396789,533.720863699197,534.155737001598,534.590610303997,
535.025483606395,535.460356908796,535.895230211204,536.330103513621,536.764976816049,
537.199850118493,537.634723420955,538.069596723438,538.504470025945,538.93934332848,
539.375069326608,539.810795324736,540.245668627333,540.680541929966,541.115415232637,
541.550288535351,541.985161838109,542.420035140915,542.854908443771,543.28978174668,
543.724655049646,544.15952835267,544.594401655757,545.029274958907,545.464148262125,
545.899021565413,546.334747563939,546.770473562465,547.205346865901,547.640220169415,
548.075093473009,548.509966776686,548.944840080449,549.3797133843,549.814586688241,
550.249459992276,550.684333296405,551.119206600633,551.554079904961,551.988953209391,
552.423826513926,552.858699818567,553.294425817789,553.73015181701,554.165025121872,
554.599898426846,555.034771731937,555.469645037144,555.90451834247,556.339391647917,
556.774264953487,557.209138259182,557.644011565003,558.078884870951,558.51375817703,
558.948631483239,559.383504789581,559.818378096058,560.254104096209,560.689830096361,
561.12470340311,561.559576709996,561.994450017021,562.429323324187,562.864196631494,
563.299069938943,563.733943246536,564.168816554273,564.603689862154,565.038563170182,
565.473436478355,565.908309786676,566.343183095144,566.77805640376,567.213782404988,
567.649508406216,568.084381715128,568.519255024189,568.954128333399,569.389001642757,
569.823874952264,570.258748261921,570.693621571725,571.128494881677,571.563368191777,
572.433114812417,572.867988122957,573.302861433642,573.737734744471,574.173460746804,
574.609186749136,575.044060060251,575.913806682904,576.783553306113,577.218426617922,
577.653299929865,578.08817324194,578.523046554147,579.392793178944,580.26253980424,
581.13313912039,581.568865123709,582.003738436771,582.87348506323,583.743231690115,
584.612978317402,585.482724945065,586.352471573076,587.222218201403,588.092817519691,
588.963416838109,589.833163467083,590.702910096251,591.572656725575,592.442403355013,
593.31214998452,594.181896614051,595.05249593303,595.92309525198,596.792841881366,
597.662588510618,598.532335139693,599.402081768556,600.271828397167,601.141575025495,
602.012174343369,602.882773661074,603.752520288553,604.622266915642,605.492013542317,
606.361760168553,607.23150679433,608.101253419626,608.971852735101,609.842452050322,
610.71219867434,611.581945297822,612.451691920754,612.886565232011,613.321438543126,
613.756311854099,614.191185164928,615.060931786153,615.931531098516,616.367257100486,
616.802130410586,617.237003720538,617.671877030342,618.106750339998,618.541623649505,
618.976496958863,619.411370268073,619.846243577134,620.281116886046,620.71599019481,
621.150863503426,621.585736811894,622.020610120214,622.455483428388,622.891209429248,
623.326935430108,623.761808737989,624.196682045726,624.631555353319,625.066428660769,
625.501301968075,625.936175275241,626.371048582266,626.805921889153,627.240795195901,
627.675668502512,628.110541808988,628.54541511533,628.98028842154,629.415161727618,
629.850887727438,630.286613727259,630.72148703308,631.156360338774,631.591233644344,
632.026106949791,632.460980255118,632.895853560325,633.330726865415,633.76560017039,
634.200473475251,634.635346780002,635.070220084644,635.505093389179,635.939966693609,
636.374839997937,636.810565996897,637.246291995857,637.681165299986,638.116038604021,
638.550911907962,638.985785211813,639.420658515576,639.855531819253,640.290405122847,
640.725278426361,641.160151729796,641.595025033157,642.029898336444,642.464771639662,
642.899644942813,643.334518245899,643.770244244257,644.205970242616,644.640843545581,
645.075716848491,645.510590151347,645.945463454153,646.380336756911,646.815210059625,
647.250083362296,647.684956664929,648.119829967526,648.55470327009,648.989576572624,
649.424449875131,649.859323177614,650.294196480076,650.729922478144,651.165648476212,
651.600521778641,652.035395081057,652.470268383465,652.905141685866,653.340014988265,
653.774888290663,654.209761593065,654.644634895472,655.079508197889,655.514381500318,
655.949254802762,656.384128105224,656.819001407706,657.253874710213,657.689600708326,
658.12532670644,658.560200009004,658.995073311601,659.429946614234,659.864819916905,
660.299693219619,660.734566522377,661.169439825183,661.604313128039,662.039186430948,
662.474059733914,662.908933036938,663.343806340025,663.778679643175,664.213552946393,
664.649278944883,665.085004943373,665.519878246733,665.954751550169,666.389624853683,
666.824498157277,667.259371460954,667.694244764717,668.129118068568,668.563991372509,
668.998864676544,669.433737980674,669.868611284901,670.303484589229,670.738357893659,
671.173231198194,671.608957197361,672.044683196528,672.479556501278,672.91442980614,
673.349303111115,673.784176416205,674.219049721412,674.653923026738,675.088796332185,
675.523669637755,675.95854294345,676.393416249271,676.82828955522,677.263162861298,
677.698036167508,678.13290947385,678.568635473934,679.004361474018,679.439234780629,
679.874108087377,680.308981394264,680.743854701289,681.178728008455,681.613601315762,
682.048474623211,682.483347930804,682.91822123854,683.353094546422,683.78796785445,
684.222841162623,684.657714470944,685.092587779412,685.528313780566,685.96403978172,
686.398913090483,686.833786399396,687.268659708457,687.703533017666,688.138406327025,
688.573279636532,689.008152946187,689.443026255992,689.877899565944,690.312772876043,
690.74764618629,691.182519496684,691.617392807224,692.052266117909,692.487992120169,
692.92371812243,693.358591433403,694.228338055774,694.663211367171,695.098084678707,
695.532957990379,695.967831302188,696.402704614131,696.837577926207,697.707324550749,
698.577071175797,699.011944488507,699.447670491767,699.883396495028,700.318269807975,
701.188016434211,702.057763060886,702.927509687976,703.797256315454,704.667002943295,
705.536749571467,706.407348889651,707.277948207973,708.147694836835,709.017441465911,
709.887188095163,710.756934724548,711.626681354026,712.496427983551,713.367027302543,
714.237626621516,715.107373250954,715.977119880277,716.846866509446,717.716613138419,
718.586359767161,719.456106395635,720.32670571363,721.197305031464,722.067051659126,
722.936798286414,723.806544913299,724.676291539758,725.546038165767,726.415784791305,
727.286384106969,728.156983422381,729.026730046663,729.896476670415,730.331349982088,
730.766223293624,731.201096605021,731.635969916278,732.505716538366,733.37546315988,
733.81033647042,734.246062472462,734.681788474505,735.116661784752,735.551535094852,
735.986408404804,736.421281714608,736.856155024264,737.291028333771,737.72590164313,
738.160774952339,738.5956482614,739.030521570312,739.465394879076,739.900268187692,
740.33514149616,740.77001480448,741.205740805414,741.641466806347,742.076340114374,
742.511213422256,742.946086729993,743.380960037585,743.815833345035,744.250706652341,
744.685579959507,745.120453266533,745.555326573419,745.990199880167,746.425073186778,
746.859946493254,747.294819799596,747.729693105806,748.165419105691,748.601145105576,
749.036018411525,749.470891717346,749.90576502304,750.34063832861,750.775511634057,
751.210384939384,751.645258244591,752.080131549682,752.515004854656,752.949878159518,
753.384751464269,753.81962476891,754.254498073445,754.689371377875,755.125097376885,
755.560823375895,755.995696680123,756.430569984253,756.865443288287,757.300316592228,
757.735189896079,758.170063199842,758.604936503519,759.039809807113,759.474683110627,
759.909556414062,760.344429717423,760.779303020711,761.214176323929,761.649049627079,
762.084775625469,762.520501623858,762.955374926883,763.390248229848,763.825121532758,
764.259994835614,764.694868138419,765.129741441178,765.564614743891,765.999488046563,
766.434361349196,766.869234651793,767.304107954357,767.738981256891,768.173854559398,
768.608727861881,769.044453859958,769.480179858035,769.915053160479,770.349926462907,
770.784799765324,771.219673067731,771.654546370133,772.089419672531,772.52429297493,
772.959166277331,773.394039579739,773.828912882155,774.263786184584,774.698659487028,
775.13353278949,775.568406091973,776.004132090072,776.439858088172,776.874731390706,
777.30960469327,777.744477995867,778.1793512985,778.614224601171,779.049097903885,
779.483971206643,779.918844509449,780.353717812305,780.788591115215,781.22346441818,
781.658337721205,782.093211024291,782.528084327442,782.963810325897,783.399536324352,
783.834409627639,784.269282931,784.704156234435,785.139029537949,785.573902841543,
786.00877614522,786.443649448983,786.878522752834,787.313396056775,787.74826936081,
788.183142664939,788.618015969167,789.052889273495,789.487762577925,789.923488577038,
790.359214576152,790.794087880793,791.228961185544,791.663834490406,792.098707795381,
792.533581100471,792.968454405678,793.403327711004,793.838201016451,794.273074322021,
794.707947627716,795.142820933537,795.577694239486,796.012567545564,796.447440851774,
796.883166851791,797.318892851808,797.753766158284,798.188639464895,798.623512771643,
799.058386078529,799.493259385555,799.92813269272,800.363006000027,800.797879307477,
801.232752615069,801.667625922806,802.102499230688,802.537372538715,802.972245846889,
803.40711915521,803.84284515629,804.27857115737,804.713444465985,805.148317774749,
805.583191083662,806.018064392723,806.452937701933,806.887811011291,807.322684320798,
808.192430940258,808.62730425021,809.06217756031,809.497050870557,809.931924180951,
810.36679749149,810.802523493679,811.238249495867,811.673122806697,812.542869428785,
812.977742740041,813.412616051438,813.847489362974,814.282362674646,814.717235986455,
815.152109298398,816.021855922681,816.891602547478,817.326475860065,817.762201863265,
818.197927866466,818.632801179295,819.502547805304,820.372294431763,821.242041058648,
822.111787685935,822.981534313598,823.851280941609,824.721880259681,825.5924795779,
826.462226206642,827.331972835616,828.201719464785,829.071466094109,829.941212723546,
830.810959353053,831.681558672047,832.552157991036,833.421904620514,834.2916512499,
835.161397879151,836.031144508226,836.900891137089,837.770637765701,838.641237083811,
839.511836401767,840.381583029608,841.251329657086,842.121076284176,842.990822910851,
843.860569537087,844.730316162863,845.600915478712,846.471514794314,847.341261418855,
848.211008042874,848.645881354683,849.080754666356,849.515627977891,849.950501289288,
850.82024791166,851.689994533462,852.124867844147,852.560593846263,852.996319848379,
853.431193158772,853.866066469019,854.300939779119,855.170686398875,855.605559708531,
856.040433018038,856.475306327397,856.910179636606,857.345052945667,857.77992625458,
858.214799563344,858.64967287196,859.084546180427,859.520272181434,859.95599818244,
860.390871490614,860.825744798641,861.260618106523,861.69549141426,862.130364721852,
862.565238029302,863.000111336609,863.434984643774,863.8698579508,864.304731257686,
864.739604564434,865.174477871045,865.609351177521,866.044224483863,866.479950483814,
866.915676483765,867.350549789843,867.785423095792,868.220296401613,868.655169707307,
869.090043012877,869.524916318325,869.959789623651,870.394662928858,870.829536233948,
871.264409538923,871.699282843785,872.134156148535,872.569029453177,873.003902757712,
873.439628756773,873.875354755834,874.310228060162,874.745101364389,875.179974668519,
875.614847972553,876.049721276495,876.484594580346,876.919467884108,877.354341187786,
877.78921449138,878.224087794893,878.658961098329,879.093834401689,879.528707704977,
879.963581008195,880.399307006616,880.835033005038,881.269906308124,881.704779611148,
882.139652914114,882.574526217024,883.00939951988,883.444272822685,883.879146125444,
884.314019428157,884.748892730829,885.183766033462,885.618639336059,886.053512638623,
886.488385941157,886.923259243664,887.358985241751,887.794711239839,888.2295845423,
888.664457844744,889.099331147173,889.534204449589,889.969077751997,890.403951054398,
890.838824356797,891.273697659195,891.708570961597,892.143444264004,892.578317566421,
893.01319086885,893.448064171293,893.882937473755,894.318663471843,894.75438946993,
895.189262772437,895.624136074971,896.059009377535,896.493882680132,896.928755982765,
897.363629285437,897.798502588151,898.233375890909,898.668249193715,899.103122496571,
899.53799579948,899.972869102446,900.40774240547,900.842615708556,901.278341706978,
901.714067705399,902.148941008617,902.583814311905,903.018687615265,903.453560918701,
903.888434222214,904.323307525808,904.758180829485,905.193054133248,905.627927437099,
906.06280074104,906.497674045075,906.932547349205,907.367420653433,907.80229395776,
908.238019956821,908.673745955883,909.108619260417,909.543492565059,909.978365869809,
910.413239174671,910.848112479646,911.282985784736,911.717859089943,912.152732395269,
912.587605700716,913.022479006287,913.457352311981,913.892225617802,914.327098923751,
914.761972229829,915.19769822978,915.633424229731,916.068297536072,916.503170842548,
916.93804414916,917.372917455908,917.807790762794,918.24266406982,918.677537376985,
919.112410684292,919.547283991742,919.982157299334,920.417030607071,920.851903914953,
921.28677722298,921.721650531154,922.15737653216,922.593102533167,923.027975841635,
923.46284915025,923.897722459014,924.332595767926,924.767469076987,925.202342386197,
925.637215695556,926.072089005063,926.506962314719,926.941835624523,927.376708934475,
927.811582244575,928.246455554822,928.681328865215,929.117054867331,929.987654180132,
930.422527490961,930.857400801934,931.292274113049,931.727147424306,932.162020735703,
932.596894047238,933.46664067072,934.336387294739,934.771260606945,935.20613391928,
935.641007231742,936.076733234882,936.94733255073,937.817079176507,938.686825802743,
939.556572429418,940.426319056508,941.296065683986,942.165812311827,943.036411629783,
943.907010947893,944.776757576505,945.646504205367,946.516250834443,947.385997463694,
948.25574409308,949.125490722558,949.996090041546,950.86668936054,951.736435990048,
952.606182619485,953.475929248809,954.345675877978,955.215422506951,956.085169135693,
956.955768453912,957.826367771985,958.696114399995,959.565861027658,960.435607654946,
961.305354281831,962.175100908289,963.044847534298,963.915446850328,964.786046166116,
965.655792790913,966.525539415195,966.960412727138,967.395286038947,968.265032662155,
969.134779284809,969.569652595924,970.004525906897,970.439399217726,970.875125219914,
971.310851222103,971.745724532643,972.615471153283,973.485217773335,973.920091083139,
974.354964392795,974.789837702302,975.22471101166,975.65958432087,976.094457629931,
976.529330938844,976.964204247608,977.399077556223,977.834803557303,978.270529558383,
978.705402866704,979.140276174877,979.575149482905,980.010022790786,980.444896098523,
980.879769406116,981.314642713565,981.749516020872,982.184389328038,982.619262635063,
983.05413594195,983.489009248698,983.923882555309,984.358755861785,984.794481861802,
985.230207861819,985.665081168029,986.099954474107,986.534827780056,986.969701085877,
987.404574391571,987.839447697141,988.274321002589,988.709194307915,989.144067613122,
989.578940918212,990.013814223187,990.448687528048,990.883560832799,991.31843413744,
991.754160136554,992.189886135667,992.624759440097,993.059632744425,993.494506048653,
993.929379352783,994.364252656817,994.799125960758,995.233999264609,995.668872568372,
996.103745872049,996.538619175643,996.973492479157,997.408365782593,997.843239085953,
998.278112389241,998.713838387696,999.149564386151,999.584437689301,1000.01931099239,
1000.45418429541,1000.88905759838,1001.32393090129,1001.75880420414,1002.19367750695,
1002.62855080971,1003.06342411242,1003.49829741509,1003.93317071773,1004.36804402032,
1004.80291732289,1005.23779062542,1005.67351662352,1006.10924262162,1006.5441159241,
1006.97898922656,1007.41386252901,1007.84873583144,1008.28360913385,1008.71848243626,
1009.15335573866,1009.58822904106,1010.02310234346,1010.45797564586,1010.89284894827,
1011.32772225069,1011.76259555311,1012.19746885556,1012.63319485364,1013.06892085171,
1013.5037941542,1013.9386674567,1014.37354075924,1014.8084140618,1015.2432873644,
1015.67816066703,1016.1130339697,1016.54790727242,1016.98278057517,1017.41765387798,
1017.85252718084,1018.28740048375,1018.72227378671,1019.15714708974,1019.59287308813,
1020.02859908651,1020.46347238967,1020.89834569288,1021.33321899617,1021.76809229953,
1022.20296560297,1022.63783890648,1023.07271221007,1023.50758551375,1023.94245881752,
1024.37733212137,1024.81220542531,1025.24707872935,1025.68195203348,1026.11682533771,
1026.55255133672,1026.98827733573,1027.42315064016,1027.8580239447,1028.29289724934,
1028.72777055409,1029.16264385896,1029.59751716393,1030.03239046902,1030.46726377423,
1030.90213707956,1031.33701038501,1031.77188369058,1032.20675699628,1032.6416303021,
1033.07650360805,1033.51222960793,1033.94795560782,1034.38282891403,1034.81770222038,
1035.25257552685,1035.68744883347,1036.12232214022,1036.5571954471,1036.99206875413,
1037.4269420613,1037.86181536861,1038.29668867606,1038.73156198365,1039.16643529139,
1039.60130859927,1040.0361819073,1040.47190790824,1040.90763390917,1041.34250721749,
1041.77738052596,1042.21225383458,1042.64712714334,1043.08200045226,1043.95174707053,
1044.38662037989,1044.8214936894,1045.25636699906,1045.69124030886,1046.12611361882,
1046.56098692892,1046.99586023917,1047.43158624121,1047.86731224325,1048.3021855538,
1048.73705886448,1049.17193217531,1049.60680548629,1050.0416787974,1050.47655210866,
1050.91142542006,1051.78117204327,1052.21604535508,1052.65091866703,1053.0857919791,
1053.52066529131,1053.95553860365,1054.39126460673,1055.26186392239,1056.13161054793,
1057.00135717395,1057.43623048712,1057.87110380041,1058.7408504273,1059.61059705459,
1060.48034368225,1061.35094300009,1062.22154231809,1063.09128894656,1063.96103557531,
1064.83078220429,1065.70052883346,1066.57027546278,1067.44002209222,1068.3106214112,
1069.18122073019,1070.05096735972,1070.9207139892,1071.79046061859,1072.66020724785,
1073.52995387693,1074.39970050579,1075.27029982411,1076.1408991423,1077.01064577048,
1077.88039239832,1078.7501390258,1079.61988565289,1080.48963227957,1081.35937890581,
1082.22997822202,1083.100577538,1083.97032416305,1084.84007078759,1085.70981741161,
1086.5795640351,1087.44931065803,1087.88418396929,1088.31905728041,1088.75393059138,
1089.18965659365,1089.62538259591,1090.06025590659,1090.93000252753,1091.36487583778,
1091.79974914788,1092.23462245783,1092.66949576764,1093.1043690773,1093.5392423868,
1093.97411569616,1094.40898900538,1094.84386231444,1095.27873562335,1095.71360893212,
1096.14933493327,1096.58506093443,1097.0199342429,1097.45480755122,1097.88968085939,
1098.32455416742,1098.75942747531,1099.19430078305,1099.62917409064,1100.06404739809,
1100.4989207054,1100.93379401257,1101.36866731959,1101.80354062648,1102.23841393323,
1102.67328723984,1103.10901323993,1103.54473924001,1103.97961254636,1104.41448585257,
1104.84935915865,1105.2842324646,1105.71910577042,1106.15397907612,1106.58885238169,
1107.02372568714,1107.45859899246,1107.89347229767,1108.32834560276,1108.76321890774,
1109.1980922126,1109.63296551736,1110.06869151652,1110.50441751569,1110.93929082023,
1111.37416412466,1111.80903742899,1112.24391073322,1112.67878403735,1113.11365734139,
1113.54853064533,1113.98340394918,1114.41827725295,1114.85315055662,1115.28802386022,
1115.72289716374,1116.15777046717,1116.59264377053,1117.02836976903,1117.46409576752,
1117.89896907074,1118.33384237389,1118.76871567698,1119.20358898,1119.63846228297,
1120.07333558588,1120.50820888874,1120.94308219154,1121.3779554943,1121.81282879702,
1122.24770209969,1122.68257540233,1123.11744870492,1123.55232200749,1123.98804800561,
1124.42377400372,1124.85864730623,1125.29352060871,1125.72839391118,1126.16326721362,
1126.59814051605,1127.03301381847,1127.46788712088,1127.90276042328,1128.33763372568,
1128.77250702808,1129.20738033048,1129.64225363289,1130.07712693531,1130.51200023774,
1130.94772623581,1131.38345223388,1131.81832553634,1132.25319883883,1132.68807214134,
1133.12294544387,1133.55781874644,1133.99269204904,1134.42756535167,1134.86243865434,
1135.29731195706,1135.73218525982,1136.16705856263,1136.60193186548,1137.03680516839,
1137.47167847136,1137.90740446972,1138.34313046808,1138.77800377117,1139.21287707432,
1139.64775037754,1140.08262368083,1140.51749698419,1140.95237028763,1141.38724359114,
1141.82211689474,1142.25699019842,1142.69186350218,1143.12673680603,1143.56161010998,
1143.99648341401,1144.43135671814,1144.86708271711,1145.30280871607,1145.7376820204,
1146.17255532483,1146.60742862936,1147.04230193401,1147.47717523876,1147.91204854362,
1148.3469218486,1148.78179515369,1149.2166684589,1149.65154176423,1150.08641506968,
1150.52128837525,1150.95616168094,1151.39103498677,1151.82676098659,1152.26248698641,
1152.69736029249,1153.1322335987,1153.56710690504,1154.00198021152,1154.43685351813,
1154.87172682488,1155.30660013177,1155.7414734388,1156.17634674597,1156.61122005327,
1157.04609336073,1157.48096666832,1157.91583997606,1158.35071328394,1158.7864392848,
1159.22216528566,1159.65703859384,1160.09191190216,1160.52678521063,1160.96165851925,
1161.39653182801,1161.83140513693,1162.26627844599,1162.7011517552,1163.13602506456,
1163.57089837407,1164.00577168373,1164.44064499353,1164.87551830349,1165.74611761556,
1166.18184361753,1166.61671692792,1167.05159023846,1167.48646354915,1167.92133685998,
1168.35621017096,1169.22595679333,1170.09570341627,1170.53057672794,1170.96545003975,
1171.4003233517,1171.83519666377,1172.27006997598,1172.705795979,1173.57639529447,
1174.44614191977,1174.8810152326,1175.31588854555,1176.18563517179,1177.05538179847,
1177.92512842556,1178.79487505304,1179.66547437075,1180.53607368863,1181.40582031696,
1182.27556694557,1183.14531357444,1184.01506020352,1184.88480683277,1185.75455346216,
1186.62515278112,1187.4957521001,1188.36549872963,1189.23524535914,1190.10499198858,
1190.97473861791,1191.84448524708,1192.71423187606,1193.58483119448,1194.45543051277,
1195.3251771411,1196.19492376911,1197.06467039678,1197.93441702407,1198.80416365096,
1199.67391027742,1200.5445095938,1201.41510890996,1202.28485553525,1203.15460216005,
1204.02434878434,1204.89409540809,1205.76384203131,1206.1987153427,1206.63358865396,
1207.06846196508,1207.50418796741,1208.37478728058,1209.2445339018,1209.6794072122,
1210.11428052245,1210.54915383255,1210.9840271425,1211.41890045231,1211.85377376197,
1212.28864707147,1212.72352038083,1213.15839369005,1213.59326699911,1214.02814030802,
1214.46386630925,1214.89959231048,1215.3344656191,1215.76933892757,1216.20421223589,
1216.63908554406,1217.07395885209,1217.50883215998,1217.94370546771,1218.37857877531,
1218.81345208276,1219.24832539007,1219.68319869724,1220.11807200426,1220.55294531115,
1220.9878186179,1221.42354461805,1221.85927061821,1222.29414392468,1222.72901723103,
1223.16389053724,1223.59876384332,1224.03363714927,1224.46851045509,1224.90338376079,
1225.33825706636,1225.77313037181,1226.20800367713,1226.64287698234,1227.07775028743,
1227.51262359241,1227.94749689727,1228.3832228965,1228.81894889572,1229.25382220036,
1229.6886955049,1230.12356880933,1230.55844211366,1230.99331541789,1231.42818872202,
1231.86306202606,1232.29793533,1232.73280863385,1233.16768193762,1233.60255524129,
1234.03742854489,1234.4723018484,1234.90717515184,1235.34290115037,1235.7786271489,
1236.21350045219,1236.64837375541,1237.08324705856,1237.51812036165,1237.95299366467,
1238.38786696764,1238.82274027055,1239.25761357341,1239.69248687621,1240.12736017897,
1240.56223348169,1240.99710678436,1241.431980087,1241.8668533896,1242.30257938773,
1242.73830538585,1243.17317868839,1243.6080519909,1244.04292529338,1244.47779859585,
1244.91267189829,1245.34754520072,1245.78241850314,1246.21729180555,1246.65216510795,
1247.08703841035,1247.52191171275,1247.95678501515,1248.39165831756,1248.82653161998,
1249.26225761804,1249.69798361611,1250.13285691855,1250.56773022101,1251.0026035235,
1251.43747682601,1251.87235012854,1252.30722343111,1252.74209673371,1253.17697003634,
1253.61184333901,1254.04671664173,1254.48158994449,1254.9164632473,1255.35133655015,
1255.78620985306,1256.22193585139,1256.65766184973,1257.09253515275,1257.52740845584,
1257.96228175899,1258.39715506221,1258.8320283655,1259.26690166886,1259.7017749723,
1260.13664827581,1260.57152157941,1261.00639488309,1261.44126818685,1261.8761414907,
1262.31101479465,1262.74588809868,1263.1816140976,1263.61734009651,1264.05221340074,
1264.48708670507,1264.9219600095,1265.35683331403,1265.79170661868,1266.22657992343,
1266.66145322829,1267.09632653327,1267.53119983836,1267.96607314357,1268.4009464489,
1268.83581975434,1269.27069305992,1269.70556636561,1270.14129236537,1270.57701836513,
1271.01189167108,1271.44676497716,1271.88163828337,1272.31651158971,1272.75138489619,
1273.1862582028,1273.62113150955,1274.05600481644,1274.49087812347,1274.92575143063,
1275.36062473794,1275.79549804539,1276.23037135299,1276.66524466073,1277.10097066151,
1277.5366966623,1277.97156997033,1278.40644327851,1278.84131658683,1279.2761898953,
1279.71106320392,1280.14593651268,1280.5808098216,1281.01568313066,1281.45055643987,
1281.88542974923,1282.32030305874,1282.75517636839,1283.1900496782,1283.62492298815,
1284.06064899005,1284.49637499195,1284.9312483022,1285.36612161259,1285.80099492313,
1286.23586823382,1286.67074154465,1287.54048816674,1287.975361478,1288.4102347894,
1288.84510810093,1289.27998141261,1289.71485472442,1290.14972803636,1291.02032735139,
1291.89092666668,1292.32579997914,1292.76067329173,1293.19554660444,1293.63041991727,
1294.50016654328,1295.36991316974,1296.23965979663,1297.10940642392,1297.9800057415,
1298.85060505925,1299.72035168742,1300.5900983159,1301.45984494464,1302.32959157362,
1303.19933820279,1304.06908483212,1304.93968415104,1305.81028347,1306.68003009953,
1307.54977672906,1308.41952335854,1309.28926998793,1310.15901661718,1311.02876324626,
1311.89936256477,1312.76996188316,1313.63970851164,1314.50945513981,1315.37920176765,
1316.24894839514,1317.11869502223,1317.98844164891,1318.85904096546,1319.72964028179,
1320.59938690733,1321.46913353238,1322.33888015692,1323.20862678095,1323.64350009276,
1324.07837340443,1324.51324671597,1324.94812002737,1325.81871934103,1326.68931865441,
1327.12419196524,1327.55906527593,1327.99393858647,1328.42881189686,1328.86368520711,
1329.29855851721,1329.73343182716,1330.16830513697,1330.60317844663,1331.03805175614,
1331.4729250655,1331.90779837471,1332.34267168377,1332.77839768507,1333.21412368638,
1333.64899699514,1334.08387030376,1334.51874361223,1334.95361692055,1335.38849022873,
1335.82336353676,1336.25823684464,1336.69311015238,1337.12798345997,1337.56285676742,
1337.99773007473,1338.4326033819,1338.86747668892,1339.30234999581,1339.73807599603,
1340.17380199625,1340.60867530287,1341.04354860934,1341.47842191569,1341.9132952219,
1342.34816852798,1342.78304183393,1343.21791513975,1343.65278844545,1344.08766175102,
1344.52253505647,1344.95740836179,1345.392281667,1345.82715497209,1346.26202827707,
1346.69775427635,1347.13348027563,1347.56835358038,1348.00322688502,1348.43810018956,
1348.87297349399,1349.30784679832,1349.74272010255,1350.17759340668,1350.61246671072,
1351.04734001466,1351.48221331851,1351.91708662228,1352.35195992595,1352.78683322955,
1353.22170653306,1353.65743253163,1354.09315853019,1354.52803183356,1354.96290513685,
1355.39777844007,1355.83265174322,1356.26752504631,1356.70239834933,1357.1372716523,
1357.57214495521,1358.00701825807,1358.44189156087,1358.87676486363,1359.31163816635,
1359.74651146902,1360.18138477166,1360.6171107698,1361.05283676795,1361.48771007051,
1361.92258337305,1362.35745667556,1362.79232997804,1363.2272032805,1363.66207658295,
1364.09694988538,1364.5318231878,1364.96669649021,1365.40156979261,1365.83644309501,
1366.27131639741,1366.70618969981,1367.14106300222,1367.57678900028,1368.01251499834,
1368.44738830077,1368.88226160321,1369.31713490567,1369.75200820816,1370.18688151067,
1370.6217548132,1371.05662811577,1371.49150141837,1371.926374721,1372.36124802367,
1372.79612132639,1373.23099462915,1373.66586793196,1374.10074123481,1374.53646723311,
1374.97219323142,1375.40706653438,1375.84193983741,1376.2768131405,1376.71168644365,
1377.14655974687,1377.58143305016,1378.01630635352,1378.45117965696,1378.88605296047,
1379.32092626407,1379.75579956775,1380.19067287151,1380.62554617536,1381.06041947931,
1381.49614547817,1381.93187147704,1382.36674478117,1382.8016180854,1383.23649138973,
1383.67136469416,1384.10623799869,1384.54111130334,1384.97598460809,1385.41085791295,
1385.84573121793,1386.28060452302,1386.71547782823,1387.15035113356,1387.585224439,
1388.02009774458,1388.45582374427,1388.89154974397,1389.32642304979,1389.76129635574,
1390.19616966182,1390.63104296803,1391.06591627437,1391.50078958085,1391.93566288746,
1392.37053619421,1392.8054095011,1393.24028280813,1393.6751561153,1394.1100294226,
1394.54490273005,1394.97977603765,1395.41550203836,1395.85122803908,1396.28610134696,
1396.72097465499,1397.15584796317,1397.59072127149,1398.02559457996,1398.46046788858,
1398.89534119734,1399.33021450626,1399.76508781532,1400.19996112453,1400.63483443389,
1401.50458105306,1401.93945436286,1402.37518036469,1402.81090636651,1403.24577967661,
1403.68065298686,1404.11552629725,1404.5503996078,1404.98527291848,1405.85501954029,
1406.2898928514,1406.72476616266,1407.15963947406,1407.5945127856,1408.02938609727,
1408.46425940908,1409.33485872391,1410.205458039,1410.64033135134,1411.07520466381,
1411.51007797639,1411.9449512891,1412.81469791488,1413.68444454112,1414.5541911678,
1415.42393779489,1416.29453711233,1417.16513642995,1418.03488305796,1418.90462968629,
1419.77437631491,1420.64412294377,1421.51386957285,1422.38361620211,1423.25421552099,
1424.12481483992,1424.99456146943,1425.86430809896,1426.73405472847,1427.60380135791,
1428.47354798724,1429.34329461641,1430.21389393501,1431.08449325349,1431.9542398821,
1432.82398651043,1433.69373313844,1434.56347976611,1435.4332263934,1436.30297302029,
1437.17357233701,1438.04417165351,1438.91391827929,1439.78366490459,1440.65341152939,
1441.52315815367,1441.95803146562,1442.39290477743,1442.8277780891,1443.26265140064,
1444.13325071451,1445.00385002811,1445.43872333908,1445.87359664991,1446.3084699606,
1446.74334327114,1447.17821658153,1447.61308989178,1448.48283651184,1448.91770982164,
1449.3525831313,1449.78745644081,1450.22232975017,1450.65720305938,1451.09292906076,
1451.52865506214,1451.96352837105,1452.39840167982,1452.83327498843,1453.2681482969,
1453.70302160522,1454.1378949134,1454.57276822143,1455.00764152931,1455.44251483705,
1455.87738814464,1456.31226145209,1456.7471347594,1457.18200806657,1457.6168813736,
1458.05260737389,1458.48833337418,1458.92320668093,1459.35807998754,1459.79295329402,
1460.22782660036,1460.66269990657,1461.09757321265,1461.5324465186,1461.96731982443,
1462.40219313012,1462.83706643569,1463.27193974114,1463.70681304647,1464.14168635168,
1464.57655965677,1465.0122856561,1465.44801165544,1465.8828849603,1466.31775826505,
1466.7526315697,1467.18750487423,1467.62237817866,1468.05725148299,1468.49212478722,
1468.92699809135,1469.36187139539,1469.79674469933,1470.23161800319,1470.66649130695,
1471.10136461063,1471.53623791422,1471.97196391283,1472.40768991143,1472.84256321487,
1473.27743651823,1473.71230982152,1474.14718312474,1474.58205642789,1475.01692973098,
1475.451803034,1475.88667633697,1476.32154963988,1476.75642294274,1477.19129624555,
1477.62616954831,1478.06104285102,1478.4959161537,1478.93164215186,1479.36736815002,
1479.80224145262,1480.23711475519,1480.67198805772,1481.10686136023,1481.54173466272,
1481.97660796518,1482.41148126762,1482.84635457005,1483.28122787247,1483.71610117488,
1484.15097447728,1484.58584777968,1485.02072108208,1485.45559438449,1485.89132038254,
1486.32704638059,1486.76191968301,1487.19679298544,1487.63166628788,1488.06653959035,
1488.50141289283,1488.93628619534,1489.37115949787,1489.80603280044,1490.24090610304,
1490.67577940567,1491.11065270835,1491.54552601106,1491.98039931382,1492.41527261663,
1492.8509986149,1493.28672461318,1493.72159791609,1494.15647121906,1494.59134452208,
1495.02621782517,1495.46109112832,1495.89596443154,1496.33083773483,1496.76571103819,
1497.20058434163,1497.63545764515,1498.07033094874,1498.50520425242,1498.94007755618,
1499.37495086004,1499.81067685885,1500.24640285767,1500.68127616171,1501.11614946584,
1501.55102277007,1501.9858960744,1502.42076937883,1502.85564268337,1503.29051598801,
1503.72538929276,1504.16026259762,1504.5951359026,1505.03000920769,1505.4648825129,
1505.89975581823,1506.33462912368,1506.77035512331,1507.20608112294,1507.64095442864,
1508.07582773446,1508.51070104041,1508.94557434649,1509.3804476527,1509.81532095904,
1510.25019426552,1510.68506757213,1511.11994087888,1511.55481418577,1511.9896874928,
1512.42456079996,1512.85943410727,1513.29430741472,1513.73003341537,1514.16575941601,
1514.60063272375,1515.03550603163,1515.47037933966,1515.90525264784,1516.34012595616,
1516.77499926463,1517.20987257325,1517.64474588201,1518.07961919093,1518.51449249999,
1518.9493658092,1519.38423911856,1519.81911242807,1520.25398573772,1520.68971173947,
1521.12543774122,1521.56031105118,1521.99518436128,1522.43005767153,1523.29980429246,
1523.73467760315,1524.16955091398,1524.60442422495,1525.03929753607,1525.47417084733,
1525.90904415873,1526.77879078194,1527.64939009657,1528.08511609939,1528.51998941146,
1528.95486272367,1529.38973603601,1530.25948266106,1531.1292292866,1531.99897591261,
1532.86872253907,1533.73846916596,1534.60906848325,1535.47966780073,1536.34941442858,
1537.21916105675,1538.08890768523,1538.95865431398,1539.82840094295,1540.69814757212,
1541.56874689096,1542.43934620985,1543.30909283933,1544.17883946886,1545.04858609839,
1545.91833272787,1546.78807935726,1547.65782598651,1548.52842530518,1549.39902462375,
1550.26877125249,1551.13851788097,1552.00826450914,1552.87801113699,1553.74775776447,
1554.61750439156,1555.48810370844,1556.35870302511,1557.22844965112,1558.09819627666,
1558.96794290171,1559.83768952626,1560.27256283834,1560.70743615028,1561.57718277377,
1562.44778208785,1563.31838140165,1563.75325471277,1564.18812802374,1564.62300133457,
1565.05787464526,1565.9276212662,1566.79736788655,1567.2322411965,1567.66711450631,
1568.10198781596,1568.53686112547,1568.97173443483,1569.40746043628,1569.84318643774,
1570.2780597468,1570.71293305571,1571.14780636448,1571.5826796731,1572.01755298157,
1572.45242628989,1572.88729959806,1573.32217290609,1573.75704621397,1574.19191952171,
1574.62679282931,1575.06166613676,1575.49653944407,1575.93141275123,1576.36713875159,
1576.80286475195,1577.23773805884,1577.67261136559,1578.1074846722,1578.54235797868,
1578.97723128502,1579.41210459124,1579.84697789732,1580.28185120327,1580.71672450909,
1581.15159781478,1581.58647112036,1582.0213444258,1582.45621773113,1582.89109103634,
1583.32681703573,1583.76254303513,1584.1974163401,1584.63228964497,1585.06716294972,
1585.50203625436,1585.9369095589,1586.37178286333,1586.80665616766,1587.24152947189,
1587.67640277602,1588.11127608005,1588.546149384,1588.98102268785,1589.41589599161,
1589.85076929529,1590.28649529394,1590.72222129258,1591.1570945961,1591.59196789953,
1592.0268412029,1592.46171450619,1592.8965878094,1593.33146111256,1593.76633441564,
1594.20120771867,1594.63608102164,1595.07095432455,1595.50582762741,1595.94070093021,
1596.37557423297,1596.81044753569,1597.24617353387,1597.68189953206,1598.11677283469,
1598.55164613729,1598.98651943985,1599.42139274239,1599.8562660449,1600.29113934738,
1600.72601264985,1601.16088595229,1601.59575925472,1602.03063255714,1602.46550585955,
1602.90037916195,1603.33525246435,1603.77012576675,1604.2058517648,1604.64157776285,
1605.07645106526,1605.51132436768,1605.94619767011,1606.38107097255,1606.81594427502,
1607.2508175775,1607.68569088001,1608.12056418254,1608.55543748511,1608.99031078771,
1609.42518409034,1609.86005739302,1610.29493069573,1610.72980399849,1611.16552999674,
1611.60125599499,1612.03612929785,1612.47100260076,1612.90587590373,1613.34074920675,
1613.77562250984,1614.21049581299,1614.64536911621,1615.0802424195,1615.51511572286,
1615.9499890263,1616.38486232981,1616.81973563341,1617.25460893709,1617.68948224085,
1618.12520823963,1618.5609342384,1618.99580754234,1619.43068084638,1619.86555415051,
1620.30042745474,1620.73530075907,1621.1701740635,1621.60504736804,1622.03992067268,
1622.47479397743,1622.90966728229,1623.34454058727,1623.77941389236,1624.21428719757,
1624.6491605029,1625.08488650247,1625.52061250204,1625.95548580761,1626.39035911331,
1626.82523241913,1627.26010572508,1627.69497903116,1628.12985233737,1628.56472564372,
1628.99959895019,1629.43447225681,1629.86934556356,1630.30421887044,1630.73909217747,
1631.17396548464,1631.60883879195,1632.04456479252,1632.48029079309,1632.91516410068,
1633.35003740842,1633.78491071631,1634.21978402433,1634.65465733251,1635.08953064083,
1635.5244039493,1635.95927725792,1636.39415056668,1636.8290238756,1637.26389718466,
1637.69877049387,1638.13364380323,1638.56851711274,1639.00424311442,1639.43996911609,
1639.8748424259,1640.30971573585,1640.74458904595,1641.6143356666,1642.04920897714,
1642.48408228782,1642.91895559865,1643.35382890963,1643.78870222074,1644.223575532,
1645.09332215494,1645.52819546661,1645.96392146936,1646.39964747212,1646.83452078406,
1647.26939409614,1647.70426740834,1648.57401403314,1649.44376065844,1650.31350728422,
1650.74838059729,1651.18325391046,1652.05300053714,1652.92359985428,1653.79419917162,
1654.66394579929,1655.5336924273,1656.40343905563,1657.27318568424,1658.14293231311,
1659.01267894219,1659.88327826096,1660.75387757982,1661.62362420926,1662.49337083877,
1663.3631174683,1664.23286409781,1665.10261072725,1665.97235735658,1666.84295667531,
1667.71355599396,1668.58330262282,1669.45304925143,1670.32279587976,1671.19254250778,
1672.06228913544,1672.93203576273,1673.80263507977,1674.6732343966,1675.54298102284,
1676.41272764862,1677.28247427392,1678.15222089872,1679.021967523,1679.89171414676,
1680.76231346105,1681.19803946366,1681.63291277506,1682.06778608632,1682.50265939743,
1682.93753270841,1683.37240601924,1684.24215264047,1684.67702595086,1685.11189926111,
1685.54677257121,1685.98164588116,1686.41651919097,1686.85139250063,1687.28626581014,
1687.72199181166,1688.15771781319,1688.5925911224,1689.02746443146,1689.46233774038,
1689.89721104914,1690.33208435776,1690.76695766623,1691.20183097455,1691.63670428272,
1692.07157759075,1692.50645089864,1692.94132420637,1693.37619751397,1693.81107082142,
1694.24594412873,1694.68167012916,1695.11739612959,1695.55226943662,1695.9871427435,
1696.42201605025,1696.85688935687,1697.29176266334,1697.72663596969,1698.1615092759,
1698.59638258198,1699.03125588793,1699.46612919375,1699.90100249945,1700.33587580502,
1700.77074911047,1701.20562241579,1701.64134841525,1702.0770744147,1702.51194771979,
1702.94682102476,1703.38169432963,1703.81656763438,1704.25144093902,1704.68631424356,
1705.12118754799,1705.55606085232,1705.99093415655,1706.42580746068,1706.86068076471,
1707.29555406866,1707.73042737251,1708.16530067627,1708.60102667496,1709.03675267365,
1709.47162597724,1709.90649928076,1710.34137258419,1710.77624588756,1711.21111919085,
1711.64599249406,1712.08086579722,1712.5157391003,1712.95061240333,1713.3854857063,
1713.82035900921,1714.25523231207,1714.69010561487,1715.12497891763,1715.56070491584,
1715.99643091404,1716.43130421671,1716.86617751935,1717.30105082195,1717.73592412451,
1718.17079742705,1718.60567072956,1719.04054403204,1719.4754173345,1719.91029063695,
1720.34516393938,1720.7800372418,1721.21491054421,1721.64978384661,1722.08465714901,
1722.52038314706,1722.9561091451,1723.39098244751,1723.82585574992,1724.26072905233,
1724.69560235476,1725.13047565721,1725.56534895967,1726.00022226216,1726.43509556467,
1726.8699688672,1727.30484216977,1727.73971547236,1728.174588775,1728.60946207767,
1729.04433538039,1729.48006137861,1729.91578737684,1730.35066067965,1730.78553398251,
1731.22040728542,1731.65528058838,1732.09015389141,1732.5250271945,1732.95990049765,
1733.39477380087,1733.82964710416,1734.26452040752,1734.69939371096,1735.13426701447,
1735.56914031807,1736.00401362175,1736.43973962048,1736.8754656192,1737.31033892306,
1737.745212227,1738.18008553104,1738.61495883517,1739.0498321394,1739.48470544373,
1739.91957874816,1740.35445205269,1740.78932535734,1741.22419866209,1741.65907196695,
1742.09394527193,1742.52881857702,1742.96369188223,1743.39941788174,1743.83514388125,
1744.2700171867,1744.70489049227,1745.13976379797,1745.57463710379,1746.00951040974,
1746.44438371582,1746.87925702203,1747.31413032837,1747.74900363485,1748.18387694146,
1748.61875024821,1749.0536235551,1749.48849686213,1749.92337016929,1750.3590961698,
1750.7948221703,1751.22969547775,1751.66456878534,1752.09944209308,1752.53431540096,
1752.96918870899,1753.40406201717,1753.83893532549,1754.27380863396,1754.70868194258,
1755.14355525134,1755.57842856026,1756.01330186932,1756.44817517853,1756.88304848789,
1757.31877448949,1757.75450049109,1758.18937380075,1759.05912042051,1759.49399373061,
1759.92886704086,1760.36374035125,1760.79861366179,1761.23348697248,1761.66836028331,
1762.10323359429,1762.5381069054,1763.40785352806,1763.8427268396,1764.27845284228,
1764.71417884496,1765.14905215677,1765.58392546872,1766.0187987808,1766.88854540534,
1767.75829203039,1768.1931653431,1768.62803865593,1769.06291196888,1769.49778528195,
1770.36753190841,1771.2381312254,1772.10873054259,1772.97847717007,1773.84822379791,
1774.71797042609,1775.58771705456,1776.45746368331,1777.32721031228,1778.19780963089,
1779.06840894783,1779.93815555508,1780.80790201176,1781.67764871408),(-0.58309518948453,
0.),.UNSPECIFIED.) ;
#820 = B_SPLINE_SURFACE_WITH_KNOTS('',3,1,((#26267,#26268),(#26269,#26270),
(#26271,#26272),(#26273,#26274),(#26275,#26276),(#26277,#26278),(#26279,
#26280),(#26281,#26282),(#26283,#26284),(#26285,#26286),(#26287,#26288),
(#26289,#26290),(#26291,#26292),(#26293,#26294),(#26295,#26296),(#26297,
#26298),(#26299,#26300),(#26301,#26302),(#26303,#26304),(#26305,#26306),
(#26307,#26308),(#26309,#26310),(#26311,#26312),(#26313,#26314),(#26315,
#26316),(#26317,#26318),(#26319,#26320),(#26321,#26322),(#26323,#26324),
(#26325,#26326),(#26327,#26328),(#26329,#26330),(#26331,#26332),(#26333,
#26334),(#26335,#26336),(#26337,#26338),(#26339,#26340),(#26341,#26342),
(#26343,#26344),(#26345,#26346),(#26347,#26348),(#26349,#26350),(#26351,
#26352),(#26353,#26354),(#26355,#26356),(#26357,#26358),(#26359,#26360),
(#26361,#26362),(#26363,#26364),(#26365,#26366),(#26367,#26368),(#26369,
#26370),(#26371,#26372),(#26373,#26374),(#26375,#26376),(#26377,#26378),
(#26379,#26380),(#26381,#26382),(#26383,#26384),(#26385,#26386),(#26387,
#26388),(#26389,#26390),(#26391,#26392),(#26393,#26394),(#26395,#26396),
(#26397,#26398),(#26399,#26400),(#26401,#26402),(#26403,#26404),(#26405,
#26406),(#26407,#26408),(#26409,#26410),(#26411,#26412),(#26413,#26414),
(#26415,#26416),(#26417,#26418),(#26419,#26420),(#26421,#26422),(#26423,
#26424),(#26425,#26426),(#26427,#26428),(#26429,#26430),(#26431,#26432),
(#26433,#26434),(#26435,#26436),(#26437,#26438),(#26439,#26440),(#26441,
#26442),(#26443,#26444),(#26445,#26446),(#26447,#26448),(#26449,#26450),
(#26451,#26452),(#26453,#26454),(#26455,#26456),(#26457,#26458),(#26459,
#26460),(#26461,#26462),(#26463,#26464),(#26465,#26466),(#26467,#26468),
(#26469,#26470),(#26471,#26472),(#26473,#26474),(#26475,#26476),(#26477,
#26478),(#26479,#26480),(#26481,#26482),(#26483,#26484),(#26485,#26486),
(#26487,#26488),(#26489,#26490),(#26491,#26492),(#26493,#26494),(#26495,
#26496),(#26497,#26498),(#26499,#26500),(#26501,#26502),(#26503,#26504),
(#26505,#26506),(#26507,#26508),(#26509,#26510),(#26511,#26512),(#26513,
#26514),(#26515,#26516),(#26517,#26518),(#26519,#26520),(#26521,#26522),
(#26523,#26524),(#26525,#26526),(#26527,#26528),(#26529,#26530),(#26531,
#26532),(#26533,#26534),(#26535,#26536),(#26537,#26538),(#26539,#26540),
(#26541,#26542),(#26543,#26544),(#26545,#26546),(#26547,#26548),(#26549,
#26550),(#26551,#26552),(#26553,#26554),(#26555,#26556),(#26557,#26558),
(#26559,#26560),(#26561,#26562),(#26563,#26564),(#26565,#26566),(#26567,
#26568),(#26569,#26570),(#26571,#26572),(#26573,#26574),(#26575,#26576),
(#26577,#26578),(#26579,#26580),(#26581,#26582),(#26583,#26584),(#26585,
#26586),(#26587,#26588),(#26589,#26590),(#26591,#26592),(#26593,#26594),
(#26595,#26596),(#26597,#26598),(#26599,#26600),(#26601,#26602),(#26603,
#26604),(#26605,#26606),(#26607,#26608),(#26609,#26610),(#26611,#26612),
(#26613,#26614),(#26615,#26616),(#26617,#26618),(#26619,#26620),(#26621,
#26622),(#26623,#26624),(#26625,#26626),(#26627,#26628),(#26629,#26630),
(#26631,#26632),(#26633,#26634),(#26635,#26636),(#26637,#26638),(#26639,
#26640),(#26641,#26642),(#26643,#26644),(#26645,#26646),(#26647,#26648),
(#26649,#26650),(#26651,#26652),(#26653,#26654),(#26655,#26656),(#26657,
#26658),(#26659,#26660),(#26661,#26662),(#26663,#26664),(#26665,#26666),
(#26667,#26668),(#26669,#26670),(#26671,#26672),(#26673,#26674),(#26675,
#26676),(#26677,#26678),(#26679,#26680),(#26681,#26682),(#26683,#26684),
(#26685,#26686),(#26687,#26688),(#26689,#26690),(#26691,#26692),(#26693,
#26694),(#26695,#26696),(#26697,#26698),(#26699,#26700),(#26701,#26702),
(#26703,#26704),(#26705,#26706),(#26707,#26708),(#26709,#26710),(#26711,
#26712),(#26713,#26714),(#26715,#26716),(#26717,#26718),(#26719,#26720),
(#26721,#26722),(#26723,#26724),(#26725,#26726),(#26727,#26728),(#26729,
#26730),(#26731,#26732),(#26733,#26734),(#26735,#26736),(#26737,#26738),
(#26739,#26740),(#26741,#26742),(#26743,#26744),(#26745,#26746),(#26747,
#26748),(#26749,#26750),(#26751,#26752),(#26753,#26754),(#26755,#26756),
(#26757,#26758),(#26759,#26760),(#26761,#26762),(#26763,#26764),(#26765,
#26766),(#26767,#26768),(#26769,#26770),(#26771,#26772),(#26773,#26774),
(#26775,#26776),(#26777,#26778),(#26779,#26780),(#26781,#26782),(#26783,
#26784),(#26785,#26786),(#26787,#26788),(#26789,#26790),(#26791,#26792),
(#26793,#26794),(#26795,#26796),(#26797,#26798),(#26799,#26800),(#26801,
#26802),(#26803,#26804),(#26805,#26806),(#26807,#26808),(#26809,#26810),
(#26811,#26812),(#26813,#26814),(#26815,#26816),(#26817,#26818),(#26819,
#26820),(#26821,#26822),(#26823,#26824),(#26825,#26826),(#26827,#26828),
(#26829,#26830),(#26831,#26832),(#26833,#26834),(#26835,#26836),(#26837,
#26838),(#26839,#26840),(#26841,#26842),(#26843,#26844),(#26845,#26846),
(#26847,#26848),(#26849,#26850),(#26851,#26852),(#26853,#26854),(#26855,
#26856),(#26857,#26858),(#26859,#26860),(#26861,#26862),(#26863,#26864),
(#26865,#26866),(#26867,#26868),(#26869,#26870),(#26871,#26872),(#26873,
#26874),(#26875,#26876),(#26877,#26878),(#26879,#26880),(#26881,#26882),
(#26883,#26884),(#26885,#26886),(#26887,#26888),(#26889,#26890),(#26891,
#26892),(#26893,#26894),(#26895,#26896),(#26897,#26898),(#26899,#26900),
(#26901,#26902),(#26903,#26904),(#26905,#26906),(#26907,#26908),(#26909,
#26910),(#26911,#26912),(#26913,#26914),(#26915,#26916),(#26917,#26918),
(#26919,#26920),(#26921,#26922),(#26923,#26924),(#26925,#26926),(#26927,
#26928),(#26929,#26930),(#26931,#26932),(#26933,#26934),(#26935,#26936),
(#26937,#26938),(#26939,#26940),(#26941,#26942),(#26943,#26944),(#26945,
#26946),(#26947,#26948),(#26949,#26950),(#26951,#26952),(#26953,#26954),
(#26955,#26956),(#26957,#26958),(#26959,#26960),(#26961,#26962),(#26963,
#26964),(#26965,#26966),(#26967,#26968),(#26969,#26970),(#26971,#26972),
(#26973,#26974),(#26975,#26976),(#26977,#26978),(#26979,#26980),(#26981,
#26982),(#26983,#26984),(#26985,#26986),(#26987,#26988),(#26989,#26990),
(#26991,#26992),(#26993,#26994),(#26995,#26996),(#26997,#26998),(#26999,
#27000),(#27001,#27002),(#27003,#27004),(#27005,#27006),(#27007,#27008),
(#27009,#27010),(#27011,#27012),(#27013,#27014),(#27015,#27016),(#27017,
#27018),(#27019,#27020),(#27021,#27022),(#27023,#27024),(#27025,#27026),
(#27027,#27028),(#27029,#27030),(#27031,#27032),(#27033,#27034),(#27035,
#27036),(#27037,#27038),(#27039,#27040),(#27041,#27042),(#27043,#27044),
(#27045,#27046),(#27047,#27048),(#27049,#27050),(#27051,#27052),(#27053,
#27054),(#27055,#27056),(#27057,#27058),(#27059,#27060),(#27061,#27062),
(#27063,#27064),(#27065,#27066),(#27067,#27068),(#27069,#27070),(#27071,
#27072),(#27073,#27074),(#27075,#27076),(#27077,#27078),(#27079,#27080),
(#27081,#27082),(#27083,#27084),(#27085,#27086),(#27087,#27088),(#27089,
#27090),(#27091,#27092),(#27093,#27094),(#27095,#27096),(#27097,#27098),
(#27099,#27100),(#27101,#27102),(#27103,#27104),(#27105,#27106),(#27107,
#27108),(#27109,#27110),(#27111,#27112),(#27113,#27114),(#27115,#27116),
(#27117,#27118),(#27119,#27120),(#27121,#27122),(#27123,#27124),(#27125,
#27126),(#27127,#27128),(#27129,#27130),(#27131,#27132),(#27133,#27134),
(#27135,#27136),(#27137,#27138),(#27139,#27140),(#27141,#27142),(#27143,
#27144),(#27145,#27146),(#27147,#27148),(#27149,#27150),(#27151,#27152),
(#27153,#27154),(#27155,#27156),(#27157,#27158),(#27159,#27160),(#27161,
#27162),(#27163,#27164),(#27165,#27166),(#27167,#27168),(#27169,#27170),
(#27171,#27172),(#27173,#27174),(#27175,#27176),(#27177,#27178),(#27179,
#27180),(#27181,#27182),(#27183,#27184),(#27185,#27186),(#27187,#27188),
(#27189,#27190),(#27191,#27192),(#27193,#27194),(#27195,#27196),(#27197,
#27198),(#27199,#27200),(#27201,#27202),(#27203,#27204),(#27205,#27206),
(#27207,#27208),(#27209,#27210),(#27211,#27212),(#27213,#27214),(#27215,
#27216),(#27217,#27218),(#27219,#27220),(#27221,#27222),(#27223,#27224),
(#27225,#27226),(#27227,#27228),(#27229,#27230),(#27231,#27232),(#27233,
#27234),(#27235,#27236),(#27237,#27238),(#27239,#27240),(#27241,#27242),
(#27243,#27244),(#27245,#27246),(#27247,#27248),(#27249,#27250),(#27251,
#27252),(#27253,#27254),(#27255,#27256),(#27257,#27258),(#27259,#27260),
(#27261,#27262),(#27263,#27264),(#27265,#27266),(#27267,#27268),(#27269,
#27270),(#27271,#27272),(#27273,#27274),(#27275,#27276),(#27277,#27278),
(#27279,#27280),(#27281,#27282),(#27283,#27284),(#27285,#27286),(#27287,
#27288),(#27289,#27290),(#27291,#27292),(#27293,#27294),(#27295,#27296),
(#27297,#27298),(#27299,#27300),(#27301,#27302),(#27303,#27304),(#27305,
#27306),(#27307,#27308),(#27309,#27310),(#27311,#27312),(#27313,#27314),
(#27315,#27316),(#27317,#27318),(#27319,#27320),(#27321,#27322),(#27323,
#27324),(#27325,#27326),(#27327,#27328),(#27329,#27330),(#27331,#27332),
(#27333,#27334),(#27335,#27336),(#27337,#27338),(#27339,#27340),(#27341,
#27342),(#27343,#27344),(#27345,#27346),(#27347,#27348),(#27349,#27350),
(#27351,#27352),(#27353,#27354),(#27355,#27356),(#27357,#27358),(#27359,
#27360),(#27361,#27362),(#27363,#27364),(#27365,#27366),(#27367,#27368),
(#27369,#27370),(#27371,#27372),(#27373,#27374),(#27375,#27376),(#27377,
#27378),(#27379,#27380),(#27381,#27382),(#27383,#27384),(#27385,#27386),
(#27387,#27388),(#27389,#27390),(#27391,#27392),(#27393,#27394),(#27395,
#27396),(#27397,#27398),(#27399,#27400),(#27401,#27402),(#27403,#27404),
(#27405,#27406),(#27407,#27408),(#27409,#27410),(#27411,#27412),(#27413,
#27414),(#27415,#27416),(#27417,#27418),(#27419,#27420),(#27421,#27422),
(#27423,#27424),(#27425,#27426),(#27427,#27428),(#27429,#27430),(#27431,
#27432),(#27433,#27434),(#27435,#27436),(#27437,#27438),(#27439,#27440),
(#27441,#27442),(#27443,#27444),(#27445,#27446),(#27447,#27448),(#27449,
#27450),(#27451,#27452),(#27453,#27454),(#27455,#27456),(#27457,#27458),
(#27459,#27460),(#27461,#27462),(#27463,#27464),(#27465,#27466),(#27467,
#27468),(#27469,#27470),(#27471,#27472),(#27473,#27474),(#27475,#27476),
(#27477,#27478),(#27479,#27480),(#27481,#27482),(#27483,#27484),(#27485,
#27486),(#27487,#27488),(#27489,#27490),(#27491,#27492),(#27493,#27494),
(#27495,#27496),(#27497,#27498),(#27499,#27500),(#27501,#27502),(#27503,
#27504),(#27505,#27506),(#27507,#27508),(#27509,#27510),(#27511,#27512),
(#27513,#27514),(#27515,#27516),(#27517,#27518),(#27519,#27520),(#27521,
#27522),(#27523,#27524),(#27525,#27526),(#27527,#27528),(#27529,#27530),
(#27531,#27532),(#27533,#27534),(#27535,#27536),(#27537,#27538),(#27539,
#27540),(#27541,#27542),(#27543,#27544),(#27545,#27546),(#27547,#27548),
(#27549,#27550),(#27551,#27552),(#27553,#27554),(#27555,#27556),(#27557,
#27558),(#27559,#27560),(#27561,#27562),(#27563,#27564),(#27565,#27566),
(#27567,#27568),(#27569,#27570),(#27571,#27572),(#27573,#27574),(#27575,
#27576),(#27577,#27578),(#27579,#27580),(#27581,#27582),(#27583,#27584),
(#27585,#27586),(#27587,#27588),(#27589,#27590),(#27591,#27592),(#27593,
#27594),(#27595,#27596),(#27597,#27598),(#27599,#27600),(#27601,#27602),
(#27603,#27604),(#27605,#27606),(#27607,#27608),(#27609,#27610),(#27611,
#27612),(#27613,#27614),(#27615,#27616),(#27617,#27618),(#27619,#27620),
(#27621,#27622),(#27623,#27624),(#27625,#27626),(#27627,#27628),(#27629,
#27630),(#27631,#27632),(#27633,#27634),(#27635,#27636),(#27637,#27638),
(#27639,#27640),(#27641,#27642),(#27643,#27644),(#27645,#27646),(#27647,
#27648),(#27649,#27650),(#27651,#27652),(#27653,#27654),(#27655,#27656),
(#27657,#27658),(#27659,#27660),(#27661,#27662),(#27663,#27664),(#27665,
#27666),(#27667,#27668),(#27669,#27670),(#27671,#27672),(#27673,#27674),
(#27675,#27676),(#27677,#27678),(#27679,#27680),(#27681,#27682),(#27683,
#27684),(#27685,#27686),(#27687,#27688),(#27689,#27690),(#27691,#27692),
(#27693,#27694),(#27695,#27696),(#27697,#27698),(#27699,#27700),(#27701,
#27702),(#27703,#27704),(#27705,#27706),(#27707,#27708),(#27709,#27710),
(#27711,#27712),(#27713,#27714),(#27715,#27716),(#27717,#27718),(#27719,
#27720),(#27721,#27722),(#27723,#27724),(#27725,#27726),(#27727,#27728),
(#27729,#27730),(#27731,#27732),(#27733,#27734),(#27735,#27736),(#27737,
#27738),(#27739,#27740),(#27741,#27742),(#27743,#27744),(#27745,#27746),
(#27747,#27748),(#27749,#27750),(#27751,#27752),(#27753,#27754),(#27755,
#27756),(#27757,#27758),(#27759,#27760),(#27761,#27762),(#27763,#27764),
(#27765,#27766),(#27767,#27768),(#27769,#27770),(#27771,#27772),(#27773,
#27774),(#27775,#27776),(#27777,#27778),(#27779,#27780),(#27781,#27782),
(#27783,#27784),(#27785,#27786),(#27787,#27788),(#27789,#27790),(#27791,
#27792),(#27793,#27794),(#27795,#27796),(#27797,#27798),(#27799,#27800),
(#27801,#27802),(#27803,#27804),(#27805,#27806),(#27807,#27808),(#27809,
#27810),(#27811,#27812),(#27813,#27814),(#27815,#27816),(#27817,#27818),
(#27819,#27820),(#27821,#27822),(#27823,#27824),(#27825,#27826),(#27827,
#27828),(#27829,#27830),(#27831,#27832),(#27833,#27834),(#27835,#27836),
(#27837,#27838),(#27839,#27840),(#27841,#27842),(#27843,#27844),(#27845,
#27846),(#27847,#27848),(#27849,#27850),(#27851,#27852),(#27853,#27854),
(#27855,#27856),(#27857,#27858),(#27859,#27860),(#27861,#27862),(#27863,
#27864),(#27865,#27866),(#27867,#27868),(#27869,#27870),(#27871,#27872),
(#27873,#27874),(#27875,#27876),(#27877,#27878),(#27879,#27880),(#27881,
#27882),(#27883,#27884),(#27885,#27886),(#27887,#27888),(#27889,#27890),
(#27891,#27892),(#27893,#27894),(#27895,#27896),(#27897,#27898),(#27899,
#27900),(#27901,#27902),(#27903,#27904),(#27905,#27906),(#27907,#27908),
(#27909,#27910),(#27911,#27912),(#27913,#27914),(#27915,#27916),(#27917,
#27918),(#27919,#27920),(#27921,#27922),(#27923,#27924),(#27925,#27926),
(#27927,#27928),(#27929,#27930),(#27931,#27932),(#27933,#27934),(#27935,
#27936),(#27937,#27938),(#27939,#27940),(#27941,#27942),(#27943,#27944),
(#27945,#27946),(#27947,#27948),(#27949,#27950),(#27951,#27952),(#27953,
#27954),(#27955,#27956),(#27957,#27958),(#27959,#27960),(#27961,#27962),
(#27963,#27964),(#27965,#27966),(#27967,#27968),(#27969,#27970),(#27971,
#27972),(#27973,#27974),(#27975,#27976),(#27977,#27978),(#27979,#27980),
(#27981,#27982),(#27983,#27984),(#27985,#27986),(#27987,#27988),(#27989,
#27990),(#27991,#27992),(#27993,#27994),(#27995,#27996),(#27997,#27998),
(#27999,#28000),(#28001,#28002),(#28003,#28004),(#28005,#28006),(#28007,
#28008),(#28009,#28010),(#28011,#28012),(#28013,#28014),(#28015,#28016),
(#28017,#28018),(#28019,#28020),(#28021,#28022),(#28023,#28024),(#28025,
#28026),(#28027,#28028),(#28029,#28030),(#28031,#28032),(#28033,#28034),
(#28035,#28036),(#28037,#28038),(#28039,#28040),(#28041,#28042),(#28043,
#28044),(#28045,#28046),(#28047,#28048),(#28049,#28050),(#28051,#28052),
(#28053,#28054),(#28055,#28056),(#28057,#28058),(#28059,#28060),(#28061,
#28062),(#28063,#28064),(#28065,#28066),(#28067,#28068),(#28069,#28070),
(#28071,#28072),(#28073,#28074),(#28075,#28076),(#28077,#28078),(#28079,
#28080),(#28081,#28082),(#28083,#28084),(#28085,#28086),(#28087,#28088),
(#28089,#28090),(#28091,#28092),(#28093,#28094),(#28095,#28096),(#28097,
#28098),(#28099,#28100),(#28101,#28102),(#28103,#28104),(#28105,#28106),
(#28107,#28108),(#28109,#28110),(#28111,#28112),(#28113,#28114),(#28115,
#28116),(#28117,#28118),(#28119,#28120),(#28121,#28122),(#28123,#28124),
(#28125,#28126),(#28127,#28128),(#28129,#28130),(#28131,#28132),(#28133,
#28134),(#28135,#28136),(#28137,#28138),(#28139,#28140),(#28141,#28142),
(#28143,#28144),(#28145,#28146),(#28147,#28148),(#28149,#28150),(#28151,
#28152),(#28153,#28154),(#28155,#28156),(#28157,#28158),(#28159,#28160),
(#28161,#28162),(#28163,#28164),(#28165,#28166),(#28167,#28168),(#28169,
#28170),(#28171,#28172),(#28173,#28174),(#28175,#28176),(#28177,#28178),
(#28179,#28180),(#28181,#28182),(#28183,#28184),(#28185,#28186),(#28187,
#28188),(#28189,#28190),(#28191,#28192),(#28193,#28194),(#28195,#28196),
(#28197,#28198),(#28199,#28200),(#28201,#28202),(#28203,#28204),(#28205,
#28206),(#28207,#28208),(#28209,#28210),(#28211,#28212),(#28213,#28214),
(#28215,#28216),(#28217,#28218),(#28219,#28220),(#28221,#28222),(#28223,
#28224),(#28225,#28226),(#28227,#28228),(#28229,#28230),(#28231,#28232),
(#28233,#28234),(#28235,#28236),(#28237,#28238),(#28239,#28240),(#28241,
#28242),(#28243,#28244),(#28245,#28246),(#28247,#28248),(#28249,#28250),
(#28251,#28252),(#28253,#28254),(#28255,#28256),(#28257,#28258),(#28259,
#28260),(#28261,#28262),(#28263,#28264),(#28265,#28266),(#28267,#28268),
(#28269,#28270),(#28271,#28272),(#28273,#28274),(#28275,#28276),(#28277,
#28278),(#28279,#28280),(#28281,#28282),(#28283,#28284),(#28285,#28286),
(#28287,#28288),(#28289,#28290),(#28291,#28292),(#28293,#28294),(#28295,
#28296),(#28297,#28298),(#28299,#28300),(#28301,#28302),(#28303,#28304),
(#28305,#28306),(#28307,#28308),(#28309,#28310),(#28311,#28312),(#28313,
#28314),(#28315,#28316),(#28317,#28318),(#28319,#28320),(#28321,#28322),
(#28323,#28324),(#28325,#28326),(#28327,#28328),(#28329,#28330),(#28331,
#28332),(#28333,#28334),(#28335,#28336),(#28337,#28338),(#28339,#28340),
(#28341,#28342),(#28343,#28344),(#28345,#28346),(#28347,#28348),(#28349,
#28350),(#28351,#28352),(#28353,#28354),(#28355,#28356),(#28357,#28358),
(#28359,#28360),(#28361,#28362),(#28363,#28364),(#28365,#28366),(#28367,
#28368),(#28369,#28370),(#28371,#28372),(#28373,#28374),(#28375,#28376),
(#28377,#28378),(#28379,#28380),(#28381,#28382),(#28383,#28384),(#28385,
#28386),(#28387,#28388),(#28389,#28390),(#28391,#28392),(#28393,#28394),
(#28395,#28396),(#28397,#28398),(#28399,#28400),(#28401,#28402),(#28403,
#28404),(#28405,#28406),(#28407,#28408),(#28409,#28410),(#28411,#28412),
(#28413,#28414),(#28415,#28416),(#28417,#28418),(#28419,#28420),(#28421,
#28422),(#28423,#28424),(#28425,#28426),(#28427,#28428),(#28429,#28430),
(#28431,#28432),(#28433,#28434),(#28435,#28436),(#28437,#28438),(#28439,
#28440),(#28441,#28442),(#28443,#28444),(#28445,#28446),(#28447,#28448),
(#28449,#28450),(#28451,#28452),(#28453,#28454),(#28455,#28456),(#28457,
#28458),(#28459,#28460),(#28461,#28462),(#28463,#28464),(#28465,#28466),
(#28467,#28468),(#28469,#28470),(#28471,#28472),(#28473,#28474),(#28475,
#28476),(#28477,#28478),(#28479,#28480),(#28481,#28482),(#28483,#28484),
(#28485,#28486),(#28487,#28488),(#28489,#28490),(#28491,#28492),(#28493,
#28494),(#28495,#28496),(#28497,#28498),(#28499,#28500),(#28501,#28502),
(#28503,#28504),(#28505,#28506),(#28507,#28508),(#28509,#28510),(#28511,
#28512),(#28513,#28514),(#28515,#28516),(#28517,#28518),(#28519,#28520),
(#28521,#28522),(#28523,#28524),(#28525,#28526),(#28527,#28528),(#28529,
#28530),(#28531,#28532),(#28533,#28534),(#28535,#28536),(#28537,#28538),
(#28539,#28540),(#28541,#28542),(#28543,#28544),(#28545,#28546),(#28547,
#28548),(#28549,#28550),(#28551,#28552),(#28553,#28554),(#28555,#28556),
(#28557,#28558),(#28559,#28560),(#28561,#28562),(#28563,#28564),(#28565,
#28566),(#28567,#28568),(#28569,#28570),(#28571,#28572),(#28573,#28574),
(#28575,#28576),(#28577,#28578),(#28579,#28580),(#28581,#28582),(#28583,
#28584),(#28585,#28586),(#28587,#28588),(#28589,#28590),(#28591,#28592),
(#28593,#28594),(#28595,#28596),(#28597,#28598),(#28599,#28600),(#28601,
#28602),(#28603,#28604),(#28605,#28606),(#28607,#28608),(#28609,#28610),
(#28611,#28612),(#28613,#28614),(#28615,#28616),(#28617,#28618),(#28619,
#28620),(#28621,#28622),(#28623,#28624),(#28625,#28626),(#28627,#28628),
(#28629,#28630),(#28631,#28632),(#28633,#28634),(#28635,#28636),(#28637,
#28638),(#28639,#28640),(#28641,#28642),(#28643,#28644),(#28645,#28646),
(#28647,#28648),(#28649,#28650),(#28651,#28652),(#28653,#28654),(#28655,
#28656),(#28657,#28658),(#28659,#28660),(#28661,#28662),(#28663,#28664),
(#28665,#28666),(#28667,#28668),(#28669,#28670),(#28671,#28672),(#28673,
#28674),(#28675,#28676),(#28677,#28678),(#28679,#28680),(#28681,#28682),
(#28683,#28684),(#28685,#28686),(#28687,#28688),(#28689,#28690),(#28691,
#28692),(#28693,#28694),(#28695,#28696),(#28697,#28698),(#28699,#28700),
(#28701,#28702),(#28703,#28704),(#28705,#28706),(#28707,#28708),(#28709,
#28710),(#28711,#28712),(#28713,#28714),(#28715,#28716),(#28717,#28718),
(#28719,#28720),(#28721,#28722),(#28723,#28724),(#28725,#28726),(#28727,
#28728),(#28729,#28730),(#28731,#28732),(#28733,#28734),(#28735,#28736),
(#28737,#28738),(#28739,#28740),(#28741,#28742),(#28743,#28744),(#28745,
#28746),(#28747,#28748),(#28749,#28750),(#28751,#28752),(#28753,#28754),
(#28755,#28756),(#28757,#28758),(#28759,#28760),(#28761,#28762),(#28763,
#28764),(#28765,#28766),(#28767,#28768),(#28769,#28770),(#28771,#28772),
(#28773,#28774),(#28775,#28776),(#28777,#28778),(#28779,#28780),(#28781,
#28782),(#28783,#28784),(#28785,#28786),(#28787,#28788),(#28789,#28790),
(#28791,#28792),(#28793,#28794),(#28795,#28796),(#28797,#28798),(#28799,
#28800),(#28801,#28802),(#28803,#28804),(#28805,#28806),(#28807,#28808),
(#28809,#28810),(#28811,#28812),(#28813,#28814),(#28815,#28816),(#28817,
#28818),(#28819,#28820),(#28821,#28822),(#28823,#28824),(#28825,#28826),
(#28827,#28828),(#28829,#28830),(#28831,#28832),(#28833,#28834),(#28835,
#28836),(#28837,#28838),(#28839,#28840),(#28841,#28842),(#28843,#28844),
(#28845,#28846),(#28847,#28848),(#28849,#28850),(#28851,#28852),(#28853,
#28854),(#28855,#28856),(#28857,#28858),(#28859,#28860),(#28861,#28862),
(#28863,#28864),(#28865,#28866),(#28867,#28868),(#28869,#28870),(#28871,
#28872),(#28873,#28874),(#28875,#28876),(#28877,#28878),(#28879,#28880),
(#28881,#28882),(#28883,#28884),(#28885,#28886),(#28887,#28888),(#28889,
#28890),(#28891,#28892),(#28893,#28894),(#28895,#28896),(#28897,#28898),
(#28899,#28900),(#28901,#28902),(#28903,#28904),(#28905,#28906),(#28907,
#28908),(#28909,#28910),(#28911,#28912),(#28913,#28914),(#28915,#28916),
(#28917,#28918),(#28919,#28920),(#28921,#28922),(#28923,#28924),(#28925,
#28926),(#28927,#28928),(#28929,#28930),(#28931,#28932),(#28933,#28934),
(#28935,#28936),(#28937,#28938),(#28939,#28940),(#28941,#28942),(#28943,
#28944),(#28945,#28946),(#28947,#28948),(#28949,#28950),(#28951,#28952),
(#28953,#28954),(#28955,#28956),(#28957,#28958),(#28959,#28960),(#28961,
#28962),(#28963,#28964),(#28965,#28966),(#28967,#28968),(#28969,#28970),
(#28971,#28972),(#28973,#28974),(#28975,#28976),(#28977,#28978),(#28979,
#28980),(#28981,#28982),(#28983,#28984),(#28985,#28986),(#28987,#28988),
(#28989,#28990),(#28991,#28992),(#28993,#28994),(#28995,#28996),(#28997,
#28998),(#28999,#29000),(#29001,#29002),(#29003,#29004),(#29005,#29006),
(#29007,#29008),(#29009,#29010),(#29011,#29012),(#29013,#29014),(#29015,
#29016),(#29017,#29018),(#29019,#29020),(#29021,#29022),(#29023,#29024),
(#29025,#29026),(#29027,#29028),(#29029,#29030),(#29031,#29032),(#29033,
#29034),(#29035,#29036),(#29037,#29038),(#29039,#29040),(#29041,#29042),
(#29043,#29044),(#29045,#29046),(#29047,#29048),(#29049,#29050),(#29051,
#29052),(#29053,#29054),(#29055,#29056),(#29057,#29058),(#29059,#29060),
(#29061,#29062),(#29063,#29064),(#29065,#29066),(#29067,#29068),(#29069,
#29070),(#29071,#29072),(#29073,#29074),(#29075,#29076),(#29077,#29078),
(#29079,#29080),(#29081,#29082),(#29083,#29084),(#29085,#29086),(#29087,
#29088),(#29089,#29090),(#29091,#29092),(#29093,#29094),(#29095,#29096),
(#29097,#29098),(#29099,#29100),(#29101,#29102),(#29103,#29104),(#29105,
#29106),(#29107,#29108),(#29109,#29110),(#29111,#29112),(#29113,#29114),
(#29115,#29116),(#29117,#29118),(#29119,#29120),(#29121,#29122),(#29123,
#29124),(#29125,#29126),(#29127,#29128),(#29129,#29130),(#29131,#29132),
(#29133,#29134),(#29135,#29136),(#29137,#29138),(#29139,#29140),(#29141,
#29142),(#29143,#29144),(#29145,#29146),(#29147,#29148),(#29149,#29150),
(#29151,#29152),(#29153,#29154),(#29155,#29156),(#29157,#29158),(#29159,
#29160),(#29161,#29162),(#29163,#29164),(#29165,#29166),(#29167,#29168),
(#29169,#29170),(#29171,#29172),(#29173,#29174),(#29175,#29176),(#29177,
#29178),(#29179,#29180),(#29181,#29182),(#29183,#29184),(#29185,#29186),
(#29187,#29188),(#29189,#29190),(#29191,#29192),(#29193,#29194),(#29195,
#29196),(#29197,#29198),(#29199,#29200),(#29201,#29202),(#29203,#29204),
(#29205,#29206),(#29207,#29208),(#29209,#29210),(#29211,#29212),(#29213,
#29214),(#29215,#29216),(#29217,#29218),(#29219,#29220),(#29221,#29222),
(#29223,#29224),(#29225,#29226),(#29227,#29228),(#29229,#29230),(#29231,
#29232),(#29233,#29234),(#29235,#29236),(#29237,#29238),(#29239,#29240),
(#29241,#29242),(#29243,#29244),(#29245,#29246),(#29247,#29248),(#29249,
#29250),(#29251,#29252),(#29253,#29254),(#29255,#29256),(#29257,#29258),
(#29259,#29260),(#29261,#29262),(#29263,#29264),(#29265,#29266),(#29267,
#29268),(#29269,#29270),(#29271,#29272),(#29273,#29274),(#29275,#29276),
(#29277,#29278),(#29279,#29280),(#29281,#29282),(#29283,#29284),(#29285,
#29286),(#29287,#29288),(#29289,#29290),(#29291,#29292),(#29293,#29294),
(#29295,#29296),(#29297,#29298),(#29299,#29300),(#29301,#29302),(#29303,
#29304),(#29305,#29306),(#29307,#29308),(#29309,#29310),(#29311,#29312),
(#29313,#29314),(#29315,#29316),(#29317,#29318),(#29319,#29320),(#29321,
#29322),(#29323,#29324),(#29325,#29326),(#29327,#29328),(#29329,#29330),
(#29331,#29332),(#29333,#29334),(#29335,#29336),(#29337,#29338),(#29339,
#29340),(#29341,#29342),(#29343,#29344),(#29345,#29346),(#29347,#29348),
(#29349,#29350),(#29351,#29352),(#29353,#29354),(#29355,#29356),(#29357,
#29358),(#29359,#29360),(#29361,#29362),(#29363,#29364),(#29365,#29366),
(#29367,#29368),(#29369,#29370),(#29371,#29372),(#29373,#29374),(#29375,
#29376),(#29377,#29378),(#29379,#29380),(#29381,#29382),(#29383,#29384),
(#29385,#29386),(#29387,#29388),(#29389,#29390),(#29391,#29392),(#29393,
#29394),(#29395,#29396),(#29397,#29398),(#29399,#29400),(#29401,#29402),
(#29403,#29404),(#29405,#29406),(#29407,#29408),(#29409,#29410),(#29411,
#29412),(#29413,#29414),(#29415,#29416),(#29417,#29418),(#29419,#29420),
(#29421,#29422),(#29423,#29424),(#29425,#29426),(#29427,#29428),(#29429,
#29430),(#29431,#29432),(#29433,#29434),(#29435,#29436),(#29437,#29438),
(#29439,#29440),(#29441,#29442),(#29443,#29444),(#29445,#29446),(#29447,
#29448),(#29449,#29450),(#29451,#29452),(#29453,#29454),(#29455,#29456),
(#29457,#29458),(#29459,#29460),(#29461,#29462),(#29463,#29464),(#29465,
#29466),(#29467,#29468),(#29469,#29470),(#29471,#29472),(#29473,#29474),
(#29475,#29476),(#29477,#29478),(#29479,#29480),(#29481,#29482),(#29483,
#29484),(#29485,#29486),(#29487,#29488),(#29489,#29490),(#29491,#29492),
(#29493,#29494),(#29495,#29496),(#29497,#29498),(#29499,#29500),(#29501,
#29502),(#29503,#29504),(#29505,#29506),(#29507,#29508),(#29509,#29510),
(#29511,#29512),(#29513,#29514),(#29515,#29516),(#29517,#29518),(#29519,
#29520),(#29521,#29522),(#29523,#29524),(#29525,#29526),(#29527,#29528),
(#29529,#29530),(#29531,#29532),(#29533,#29534),(#29535,#29536),(#29537,
#29538),(#29539,#29540),(#29541,#29542),(#29543,#29544),(#29545,#29546),
(#29547,#29548),(#29549,#29550),(#29551,#29552),(#29553,#29554),(#29555,
#29556),(#29557,#29558),(#29559,#29560),(#29561,#29562),(#29563,#29564),
(#29565,#29566),(#29567,#29568),(#29569,#29570),(#29571,#29572),(#29573,
#29574),(#29575,#29576),(#29577,#29578),(#29579,#29580),(#29581,#29582),
(#29583,#29584),(#29585,#29586),(#29587,#29588),(#29589,#29590),(#29591,
#29592),(#29593,#29594),(#29595,#29596),(#29597,#29598),(#29599,#29600),
(#29601,#29602),(#29603,#29604),(#29605,#29606),(#29607,#29608),(#29609,
#29610),(#29611,#29612),(#29613,#29614),(#29615,#29616),(#29617,#29618),
(#29619,#29620),(#29621,#29622),(#29623,#29624),(#29625,#29626),(#29627,
#29628),(#29629,#29630),(#29631,#29632),(#29633,#29634),(#29635,#29636),
(#29637,#29638),(#29639,#29640),(#29641,#29642),(#29643,#29644),(#29645,
#29646),(#29647,#29648),(#29649,#29650),(#29651,#29652),(#29653,#29654),
(#29655,#29656),(#29657,#29658),(#29659,#29660),(#29661,#29662),(#29663,
#29664),(#29665,#29666),(#29667,#29668),(#29669,#29670),(#29671,#29672),
(#29673,#29674),(#29675,#29676),(#29677,#29678),(#29679,#29680),(#29681,
#29682),(#29683,#29684),(#29685,#29686),(#29687,#29688),(#29689,#29690),
(#29691,#29692),(#29693,#29694),(#29695,#29696),(#29697,#29698),(#29699,
#29700),(#29701,#29702),(#29703,#29704),(#29705,#29706),(#29707,#29708),
(#29709,#29710),(#29711,#29712),(#29713,#29714),(#29715,#29716),(#29717,
#29718),(#29719,#29720),(#29721,#29722),(#29723,#29724),(#29725,#29726),
(#29727,#29728),(#29729,#29730),(#29731,#29732),(#29733,#29734),(#29735,
#29736),(#29737,#29738),(#29739,#29740),(#29741,#29742),(#29743,#29744),
(#29745,#29746),(#29747,#29748),(#29749,#29750),(#29751,#29752),(#29753,
#29754),(#29755,#29756),(#29757,#29758),(#29759,#29760),(#29761,#29762),
(#29763,#29764),(#29765,#29766),(#29767,#29768),(#29769,#29770),(#29771,
#29772),(#29773,#29774),(#29775,#29776),(#29777,#29778),(#29779,#29780),
(#29781,#29782),(#29783,#29784),(#29785,#29786),(#29787,#29788),(#29789,
#29790),(#29791,#29792),(#29793,#29794),(#29795,#29796),(#29797,#29798),
(#29799,#29800),(#29801,#29802),(#29803,#29804),(#29805,#29806),(#29807,
#29808),(#29809,#29810),(#29811,#29812),(#29813,#29814),(#29815,#29816),
(#29817,#29818),(#29819,#29820),(#29821,#29822),(#29823,#29824),(#29825,
#29826),(#29827,#29828),(#29829,#29830),(#29831,#29832),(#29833,#29834),
(#29835,#29836),(#29837,#29838),(#29839,#29840),(#29841,#29842),(#29843,
#29844),(#29845,#29846),(#29847,#29848),(#29849,#29850),(#29851,#29852),
(#29853,#29854),(#29855,#29856),(#29857,#29858),(#29859,#29860),(#29861,
#29862),(#29863,#29864),(#29865,#29866),(#29867,#29868),(#29869,#29870),
(#29871,#29872),(#29873,#29874),(#29875,#29876),(#29877,#29878),(#29879,
#29880),(#29881,#29882),(#29883,#29884),(#29885,#29886),(#29887,#29888),
(#29889,#29890),(#29891,#29892),(#29893,#29894),(#29895,#29896),(#29897,
#29898),(#29899,#29900),(#29901,#29902),(#29903,#29904),(#29905,#29906),
(#29907,#29908),(#29909,#29910),(#29911,#29912),(#29913,#29914),(#29915,
#29916),(#29917,#29918),(#29919,#29920),(#29921,#29922),(#29923,#29924),
(#29925,#29926),(#29927,#29928),(#29929,#29930),(#29931,#29932),(#29933,
#29934),(#29935,#29936),(#29937,#29938),(#29939,#29940),(#29941,#29942),
(#29943,#29944),(#29945,#29946),(#29947,#29948),(#29949,#29950),(#29951,
#29952),(#29953,#29954),(#29955,#29956),(#29957,#29958),(#29959,#29960),
(#29961,#29962),(#29963,#29964),(#29965,#29966),(#29967,#29968),(#29969,
#29970),(#29971,#29972),(#29973,#29974),(#29975,#29976),(#29977,#29978),
(#29979,#29980),(#29981,#29982),(#29983,#29984),(#29985,#29986),(#29987,
#29988),(#29989,#29990),(#29991,#29992),(#29993,#29994),(#29995,#29996),
(#29997,#29998),(#29999,#30000),(#30001,#30002),(#30003,#30004),(#30005,
#30006),(#30007,#30008),(#30009,#30010),(#30011,#30012),(#30013,#30014),
(#30015,#30016),(#30017,#30018),(#30019,#30020),(#30021,#30022),(#30023,
#30024),(#30025,#30026),(#30027,#30028),(#30029,#30030),(#30031,#30032),
(#30033,#30034),(#30035,#30036),(#30037,#30038),(#30039,#30040),(#30041,
#30042),(#30043,#30044),(#30045,#30046),(#30047,#30048),(#30049,#30050),
(#30051,#30052),(#30053,#30054),(#30055,#30056),(#30057,#30058),(#30059,
#30060),(#30061,#30062),(#30063,#30064),(#30065,#30066),(#30067,#30068),
(#30069,#30070),(#30071,#30072),(#30073,#30074),(#30075,#30076),(#30077,
#30078),(#30079,#30080),(#30081,#30082),(#30083,#30084),(#30085,#30086),
(#30087,#30088),(#30089,#30090),(#30091,#30092),(#30093,#30094),(#30095,
#30096),(#30097,#30098),(#30099,#30100),(#30101,#30102),(#30103,#30104),
(#30105,#30106),(#30107,#30108),(#30109,#30110),(#30111,#30112),(#30113,
#30114),(#30115,#30116),(#30117,#30118),(#30119,#30120),(#30121,#30122),
(#30123,#30124),(#30125,#30126),(#30127,#30128),(#30129,#30130),(#30131,
#30132),(#30133,#30134),(#30135,#30136),(#30137,#30138),(#30139,#30140),
(#30141,#30142),(#30143,#30144),(#30145,#30146),(#30147,#30148),(#30149,
#30150),(#30151,#30152),(#30153,#30154),(#30155,#30156),(#30157,#30158),
(#30159,#30160),(#30161,#30162),(#30163,#30164),(#30165,#30166),(#30167,
#30168),(#30169,#30170),(#30171,#30172),(#30173,#30174),(#30175,#30176),
(#30177,#30178),(#30179,#30180),(#30181,#30182),(#30183,#30184),(#30185,
#30186),(#30187,#30188),(#30189,#30190),(#30191,#30192),(#30193,#30194),
(#30195,#30196),(#30197,#30198),(#30199,#30200),(#30201,#30202),(#30203,
#30204),(#30205,#30206),(#30207,#30208),(#30209,#30210),(#30211,#30212),
(#30213,#30214),(#30215,#30216),(#30217,#30218),(#30219,#30220),(#30221,
#30222),(#30223,#30224),(#30225,#30226),(#30227,#30228),(#30229,#30230),
(#30231,#30232),(#30233,#30234),(#30235,#30236),(#30237,#30238),(#30239,
#30240),(#30241,#30242),(#30243,#30244),(#30245,#30246),(#30247,#30248),
(#30249,#30250),(#30251,#30252),(#30253,#30254),(#30255,#30256),(#30257,
#30258),(#30259,#30260),(#30261,#30262),(#30263,#30264),(#30265,#30266),
(#30267,#30268),(#30269,#30270),(#30271,#30272),(#30273,#30274),(#30275,
#30276),(#30277,#30278),(#30279,#30280),(#30281,#30282),(#30283,#30284),
(#30285,#30286),(#30287,#30288),(#30289,#30290),(#30291,#30292),(#30293,
#30294),(#30295,#30296),(#30297,#30298),(#30299,#30300),(#30301,#30302),
(#30303,#30304),(#30305,#30306),(#30307,#30308),(#30309,#30310),(#30311,
#30312),(#30313,#30314),(#30315,#30316),(#30317,#30318),(#30319,#30320),
(#30321,#30322),(#30323,#30324),(#30325,#30326),(#30327,#30328),(#30329,
#30330),(#30331,#30332),(#30333,#30334),(#30335,#30336),(#30337,#30338),
(#30339,#30340),(#30341,#30342),(#30343,#30344),(#30345,#30346),(#30347,
#30348),(#30349,#30350),(#30351,#30352),(#30353,#30354),(#30355,#30356),
(#30357,#30358),(#30359,#30360),(#30361,#30362),(#30363,#30364),(#30365,
#30366),(#30367,#30368),(#30369,#30370),(#30371,#30372),(#30373,#30374),
(#30375,#30376),(#30377,#30378),(#30379,#30380),(#30381,#30382),(#30383,
#30384),(#30385,#30386),(#30387,#30388),(#30389,#30390),(#30391,#30392),
(#30393,#30394),(#30395,#30396),(#30397,#30398),(#30399,#30400),(#30401,
#30402),(#30403,#30404),(#30405,#30406),(#30407,#30408),(#30409,#30410),
(#30411,#30412),(#30413,#30414),(#30415,#30416),(#30417,#30418),(#30419,
#30420),(#30421,#30422),(#30423,#30424),(#30425,#30426),(#30427,#30428),
(#30429,#30430),(#30431,#30432),(#30433,#30434),(#30435,#30436),(#30437,
#30438),(#30439,#30440),(#30441,#30442),(#30443,#30444),(#30445,#30446),
(#30447,#30448),(#30449,#30450),(#30451,#30452),(#30453,#30454),(#30455,
#30456),(#30457,#30458),(#30459,#30460),(#30461,#30462),(#30463,#30464),
(#30465,#30466),(#30467,#30468),(#30469,#30470),(#30471,#30472),(#30473,
#30474),(#30475,#30476),(#30477,#30478),(#30479,#30480),(#30481,#30482),
(#30483,#30484),(#30485,#30486),(#30487,#30488),(#30489,#30490),(#30491,
#30492),(#30493,#30494),(#30495,#30496),(#30497,#30498),(#30499,#30500),
(#30501,#30502),(#30503,#30504),(#30505,#30506),(#30507,#30508),(#30509,
#30510),(#30511,#30512),(#30513,#30514),(#30515,#30516),(#30517,#30518),
(#30519,#30520),(#30521,#30522),(#30523,#30524),(#30525,#30526),(#30527,
#30528),(#30529,#30530),(#30531,#30532),(#30533,#30534),(#30535,#30536),
(#30537,#30538),(#30539,#30540),(#30541,#30542),(#30543,#30544),(#30545,
#30546),(#30547,#30548),(#30549,#30550),(#30551,#30552),(#30553,#30554),
(#30555,#30556),(#30557,#30558),(#30559,#30560),(#30561,#30562),(#30563,
#30564),(#30565,#30566),(#30567,#30568),(#30569,#30570),(#30571,#30572),
(#30573,#30574),(#30575,#30576),(#30577,#30578),(#30579,#30580),(#30581,
#30582),(#30583,#30584),(#30585,#30586),(#30587,#30588),(#30589,#30590),
(#30591,#30592),(#30593,#30594),(#30595,#30596),(#30597,#30598),(#30599,
#30600),(#30601,#30602),(#30603,#30604),(#30605,#30606),(#30607,#30608),
(#30609,#30610),(#30611,#30612),(#30613,#30614),(#30615,#30616),(#30617,
#30618),(#30619,#30620),(#30621,#30622),(#30623,#30624),(#30625,#30626),
(#30627,#30628),(#30629,#30630),(#30631,#30632),(#30633,#30634),(#30635,
#30636),(#30637,#30638),(#30639,#30640),(#30641,#30642),(#30643,#30644),
(#30645,#30646),(#30647,#30648),(#30649,#30650),(#30651,#30652),(#30653,
#30654),(#30655,#30656),(#30657,#30658),(#30659,#30660),(#30661,#30662),
(#30663,#30664),(#30665,#30666),(#30667,#30668),(#30669,#30670),(#30671,
#30672),(#30673,#30674),(#30675,#30676),(#30677,#30678),(#30679,#30680),
(#30681,#30682),(#30683,#30684),(#30685,#30686),(#30687,#30688),(#30689,
#30690),(#30691,#30692),(#30693,#30694),(#30695,#30696),(#30697,#30698),
(#30699,#30700),(#30701,#30702),(#30703,#30704),(#30705,#30706),(#30707,
#30708),(#30709,#30710),(#30711,#30712),(#30713,#30714),(#30715,#30716),
(#30717,#30718),(#30719,#30720),(#30721,#30722),(#30723,#30724),(#30725,
#30726),(#30727,#30728),(#30729,#30730),(#30731,#30732),(#30733,#30734),
(#30735,#30736),(#30737,#30738),(#30739,#30740),(#30741,#30742),(#30743,
#30744),(#30745,#30746),(#30747,#30748),(#30749,#30750),(#30751,#30752),
(#30753,#30754),(#30755,#30756),(#30757,#30758),(#30759,#30760),(#30761,
#30762),(#30763,#30764),(#30765,#30766),(#30767,#30768),(#30769,#30770),
(#30771,#30772),(#30773,#30774),(#30775,#30776),(#30777,#30778),(#30779,
#30780),(#30781,#30782),(#30783,#30784),(#30785,#30786),(#30787,#30788),
(#30789,#30790),(#30791,#30792),(#30793,#30794),(#30795,#30796),(#30797,
#30798),(#30799,#30800),(#30801,#30802),(#30803,#30804),(#30805,#30806),
(#30807,#30808),(#30809,#30810),(#30811,#30812),(#30813,#30814),(#30815,
#30816),(#30817,#30818),(#30819,#30820),(#30821,#30822),(#30823,#30824),
(#30825,#30826),(#30827,#30828),(#30829,#30830),(#30831,#30832),(#30833,
#30834),(#30835,#30836),(#30837,#30838),(#30839,#30840),(#30841,#30842),
(#30843,#30844),(#30845,#30846),(#30847,#30848),(#30849,#30850),(#30851,
#30852),(#30853,#30854),(#30855,#30856),(#30857,#30858),(#30859,#30860),
(#30861,#30862),(#30863,#30864),(#30865,#30866),(#30867,#30868),(#30869,
#30870),(#30871,#30872),(#30873,#30874),(#30875,#30876),(#30877,#30878),
(#30879,#30880),(#30881,#30882),(#30883,#30884),(#30885,#30886),(#30887,
#30888),(#30889,#30890),(#30891,#30892),(#30893,#30894),(#30895,#30896),
(#30897,#30898),(#30899,#30900),(#30901,#30902),(#30903,#30904),(#30905,
#30906),(#30907,#30908),(#30909,#30910),(#30911,#30912),(#30913,#30914),
(#30915,#30916),(#30917,#30918),(#30919,#30920),(#30921,#30922),(#30923,
#30924),(#30925,#30926),(#30927,#30928),(#30929,#30930),(#30931,#30932),
(#30933,#30934),(#30935,#30936),(#30937,#30938),(#30939,#30940),(#30941,
#30942),(#30943,#30944),(#30945,#30946),(#30947,#30948),(#30949,#30950),
(#30951,#30952),(#30953,#30954),(#30955,#30956),(#30957,#30958),(#30959,
#30960),(#30961,#30962),(#30963,#30964),(#30965,#30966),(#30967,#30968),
(#30969,#30970),(#30971,#30972),(#30973,#30974),(#30975,#30976),(#30977,
#30978),(#30979,#30980),(#30981,#30982),(#30983,#30984),(#30985,#30986),
(#30987,#30988),(#30989,#30990),(#30991,#30992),(#30993,#30994),(#30995,
#30996),(#30997,#30998),(#30999,#31000),(#31001,#31002),(#31003,#31004),
(#31005,#31006),(#31007,#31008),(#31009,#31010),(#31011,#31012),(#31013,
#31014),(#31015,#31016),(#31017,#31018),(#31019,#31020),(#31021,#31022),
(#31023,#31024),(#31025,#31026),(#31027,#31028),(#31029,#31030),(#31031,
#31032),(#31033,#31034),(#31035,#31036),(#31037,#31038),(#31039,#31040),
(#31041,#31042),(#31043,#31044),(#31045,#31046),(#31047,#31048),(#31049,
#31050),(#31051,#31052),(#31053,#31054),(#31055,#31056),(#31057,#31058),
(#31059,#31060),(#31061,#31062),(#31063,#31064),(#31065,#31066),(#31067,
#31068),(#31069,#31070),(#31071,#31072),(#31073,#31074),(#31075,#31076),
(#31077,#31078),(#31079,#31080),(#31081,#31082),(#31083,#31084),(#31085,
#31086),(#31087,#31088),(#31089,#31090),(#31091,#31092),(#31093,#31094),
(#31095,#31096),(#31097,#31098),(#31099,#31100),(#31101,#31102),(#31103,
#31104),(#31105,#31106),(#31107,#31108),(#31109,#31110),(#31111,#31112),
(#31113,#31114),(#31115,#31116),(#31117,#31118),(#31119,#31120),(#31121,
#31122),(#31123,#31124),(#31125,#31126),(#31127,#31128),(#31129,#31130),
(#31131,#31132),(#31133,#31134),(#31135,#31136),(#31137,#31138),(#31139,
#31140),(#31141,#31142),(#31143,#31144),(#31145,#31146),(#31147,#31148),
(#31149,#31150),(#31151,#31152),(#31153,#31154),(#31155,#31156),(#31157,
#31158),(#31159,#31160),(#31161,#31162),(#31163,#31164),(#31165,#31166),
(#31167,#31168),(#31169,#31170),(#31171,#31172),(#31173,#31174),(#31175,
#31176),(#31177,#31178),(#31179,#31180),(#31181,#31182),(#31183,#31184),
(#31185,#31186),(#31187,#31188),(#31189,#31190),(#31191,#31192),(#31193,
#31194),(#31195,#31196),(#31197,#31198),(#31199,#31200),(#31201,#31202),
(#31203,#31204),(#31205,#31206),(#31207,#31208),(#31209,#31210),(#31211,
#31212),(#31213,#31214),(#31215,#31216),(#31217,#31218),(#31219,#31220),
(#31221,#31222),(#31223,#31224),(#31225,#31226),(#31227,#31228),(#31229,
#31230),(#31231,#31232),(#31233,#31234),(#31235,#31236),(#31237,#31238),
(#31239,#31240),(#31241,#31242),(#31243,#31244),(#31245,#31246),(#31247,
#31248),(#31249,#31250),(#31251,#31252),(#31253,#31254),(#31255,#31256),
(#31257,#31258),(#31259,#31260),(#31261,#31262),(#31263,#31264),(#31265,
#31266),(#31267,#31268),(#31269,#31270),(#31271,#31272),(#31273,#31274),
(#31275,#31276),(#31277,#31278),(#31279,#31280),(#31281,#31282),(#31283,
#31284),(#31285,#31286),(#31287,#31288),(#31289,#31290),(#31291,#31292),
(#31293,#31294),(#31295,#31296),(#31297,#31298),(#31299,#31300),(#31301,
#31302),(#31303,#31304),(#31305,#31306),(#31307,#31308),(#31309,#31310),
(#31311,#31312),(#31313,#31314),(#31315,#31316),(#31317,#31318),(#31319,
#31320),(#31321,#31322),(#31323,#31324),(#31325,#31326),(#31327,#31328),
(#31329,#31330),(#31331,#31332),(#31333,#31334),(#31335,#31336),(#31337,
#31338),(#31339,#31340),(#31341,#31342),(#31343,#31344),(#31345,#31346),
(#31347,#31348),(#31349,#31350),(#31351,#31352),(#31353,#31354),(#31355,
#31356),(#31357,#31358),(#31359,#31360),(#31361,#31362),(#31363,#31364),
(#31365,#31366),(#31367,#31368),(#31369,#31370),(#31371,#31372),(#31373,
#31374),(#31375,#31376),(#31377,#31378),(#31379,#31380),(#31381,#31382),
(#31383,#31384),(#31385,#31386),(#31387,#31388),(#31389,#31390),(#31391,
#31392),(#31393,#31394),(#31395,#31396),(#31397,#31398),(#31399,#31400),
(#31401,#31402),(#31403,#31404),(#31405,#31406),(#31407,#31408),(#31409,
#31410),(#31411,#31412),(#31413,#31414),(#31415,#31416),(#31417,#31418),
(#31419,#31420),(#31421,#31422),(#31423,#31424),(#31425,#31426),(#31427,
#31428),(#31429,#31430),(#31431,#31432),(#31433,#31434),(#31435,#31436),
(#31437,#31438),(#31439,#31440),(#31441,#31442),(#31443,#31444),(#31445,
#31446),(#31447,#31448),(#31449,#31450),(#31451,#31452),(#31453,#31454),
(#31455,#31456),(#31457,#31458),(#31459,#31460),(#31461,#31462),(#31463,
#31464),(#31465,#31466),(#31467,#31468),(#31469,#31470),(#31471,#31472),
(#31473,#31474),(#31475,#31476),(#31477,#31478),(#31479,#31480),(#31481,
#31482),(#31483,#31484),(#31485,#31486),(#31487,#31488),(#31489,#31490),
(#31491,#31492),(#31493,#31494),(#31495,#31496),(#31497,#31498),(#31499,
#31500),(#31501,#31502),(#31503,#31504),(#31505,#31506),(#31507,#31508),
(#31509,#31510),(#31511,#31512),(#31513,#31514),(#31515,#31516),(#31517,
#31518),(#31519,#31520),(#31521,#31522),(#31523,#31524),(#31525,#31526),
(#31527,#31528),(#31529,#31530),(#31531,#31532),(#31533,#31534),(#31535,
#31536),(#31537,#31538),(#31539,#31540),(#31541,#31542),(#31543,#31544),
(#31545,#31546),(#31547,#31548),(#31549,#31550),(#31551,#31552),(#31553,
#31554),(#31555,#31556),(#31557,#31558),(#31559,#31560),(#31561,#31562),
(#31563,#31564),(#31565,#31566),(#31567,#31568),(#31569,#31570),(#31571,
#31572),(#31573,#31574),(#31575,#31576),(#31577,#31578),(#31579,#31580),
(#31581,#31582),(#31583,#31584),(#31585,#31586),(#31587,#31588),(#31589,
#31590),(#31591,#31592),(#31593,#31594),(#31595,#31596),(#31597,#31598),
(#31599,#31600),(#31601,#31602),(#31603,#31604),(#31605,#31606),(#31607,
#31608),(#31609,#31610),(#31611,#31612),(#31613,#31614),(#31615,#31616),
(#31617,#31618),(#31619,#31620),(#31621,#31622),(#31623,#31624),(#31625,
#31626),(#31627,#31628),(#31629,#31630),(#31631,#31632),(#31633,#31634),
(#31635,#31636),(#31637,#31638),(#31639,#31640),(#31641,#31642),(#31643,
#31644),(#31645,#31646),(#31647,#31648),(#31649,#31650),(#31651,#31652),
(#31653,#31654),(#31655,#31656),(#31657,#31658),(#31659,#31660),(#31661,
#31662),(#31663,#31664),(#31665,#31666),(#31667,#31668),(#31669,#31670),
(#31671,#31672),(#31673,#31674),(#31675,#31676),(#31677,#31678),(#31679,
#31680),(#31681,#31682),(#31683,#31684),(#31685,#31686),(#31687,#31688),
(#31689,#31690),(#31691,#31692),(#31693,#31694),(#31695,#31696),(#31697,
#31698),(#31699,#31700),(#31701,#31702),(#31703,#31704),(#31705,#31706),
(#31707,#31708),(#31709,#31710),(#31711,#31712),(#31713,#31714),(#31715,
#31716),(#31717,#31718),(#31719,#31720),(#31721,#31722),(#31723,#31724),
(#31725,#31726),(#31727,#31728),(#31729,#31730),(#31731,#31732),(#31733,
#31734),(#31735,#31736),(#31737,#31738),(#31739,#31740),(#31741,#31742),
(#31743,#31744),(#31745,#31746),(#31747,#31748),(#31749,#31750),(#31751,
#31752),(#31753,#31754),(#31755,#31756),(#31757,#31758),(#31759,#31760),
(#31761,#31762),(#31763,#31764),(#31765,#31766),(#31767,#31768),(#31769,
#31770),(#31771,#31772),(#31773,#31774),(#31775,#31776),(#31777,#31778),
(#31779,#31780),(#31781,#31782),(#31783,#31784),(#31785,#31786),(#31787,
#31788),(#31789,#31790),(#31791,#31792),(#31793,#31794),(#31795,#31796),
(#31797,#31798),(#31799,#31800),(#31801,#31802),(#31803,#31804),(#31805,
#31806),(#31807,#31808),(#31809,#31810),(#31811,#31812),(#31813,#31814),
(#31815,#31816),(#31817,#31818),(#31819,#31820),(#31821,#31822),(#31823,
#31824),(#31825,#31826),(#31827,#31828),(#31829,#31830),(#31831,#31832),
(#31833,#31834),(#31835,#31836),(#31837,#31838),(#31839,#31840),(#31841,
#31842),(#31843,#31844),(#31845,#31846),(#31847,#31848),(#31849,#31850),
(#31851,#31852),(#31853,#31854),(#31855,#31856),(#31857,#31858),(#31859,
#31860),(#31861,#31862),(#31863,#31864),(#31865,#31866),(#31867,#31868),
(#31869,#31870),(#31871,#31872),(#31873,#31874),(#31875,#31876),(#31877,
#31878),(#31879,#31880),(#31881,#31882),(#31883,#31884),(#31885,#31886),
(#31887,#31888),(#31889,#31890),(#31891,#31892),(#31893,#31894),(#31895,
#31896),(#31897,#31898),(#31899,#31900),(#31901,#31902),(#31903,#31904),
(#31905,#31906),(#31907,#31908),(#31909,#31910),(#31911,#31912),(#31913,
#31914),(#31915,#31916),(#31917,#31918),(#31919,#31920),(#31921,#31922),
(#31923,#31924),(#31925,#31926),(#31927,#31928),(#31929,#31930),(#31931,
#31932),(#31933,#31934),(#31935,#31936),(#31937,#31938),(#31939,#31940),
(#31941,#31942),(#31943,#31944),(#31945,#31946),(#31947,#31948),(#31949,
#31950),(#31951,#31952),(#31953,#31954),(#31955,#31956),(#31957,#31958),
(#31959,#31960),(#31961,#31962),(#31963,#31964),(#31965,#31966),(#31967,
#31968),(#31969,#31970),(#31971,#31972),(#31973,#31974),(#31975,#31976),
(#31977,#31978),(#31979,#31980),(#31981,#31982),(#31983,#31984),(#31985,
#31986),(#31987,#31988),(#31989,#31990),(#31991,#31992),(#31993,#31994),
(#31995,#31996),(#31997,#31998),(#31999,#32000),(#32001,#32002),(#32003,
#32004),(#32005,#32006),(#32007,#32008),(#32009,#32010),(#32011,#32012),
(#32013,#32014),(#32015,#32016),(#32017,#32018),(#32019,#32020),(#32021,
#32022),(#32023,#32024),(#32025,#32026),(#32027,#32028),(#32029,#32030),
(#32031,#32032),(#32033,#32034),(#32035,#32036),(#32037,#32038),(#32039,
#32040),(#32041,#32042),(#32043,#32044),(#32045,#32046),(#32047,#32048),
(#32049,#32050),(#32051,#32052),(#32053,#32054),(#32055,#32056),(#32057,
#32058),(#32059,#32060),(#32061,#32062),(#32063,#32064),(#32065,#32066),
(#32067,#32068),(#32069,#32070),(#32071,#32072),(#32073,#32074),(#32075,
#32076),(#32077,#32078),(#32079,#32080),(#32081,#32082),(#32083,#32084),
(#32085,#32086),(#32087,#32088),(#32089,#32090),(#32091,#32092),(#32093,
#32094),(#32095,#32096),(#32097,#32098),(#32099,#32100),(#32101,#32102),
(#32103,#32104),(#32105,#32106),(#32107,#32108),(#32109,#32110),(#32111,
#32112),(#32113,#32114),(#32115,#32116),(#32117,#32118),(#32119,#32120),
(#32121,#32122),(#32123,#32124),(#32125,#32126),(#32127,#32128),(#32129,
#32130),(#32131,#32132),(#32133,#32134),(#32135,#32136),(#32137,#32138),
(#32139,#32140),(#32141,#32142),(#32143,#32144),(#32145,#32146),(#32147,
#32148),(#32149,#32150),(#32151,#32152),(#32153,#32154),(#32155,#32156),
(#32157,#32158),(#32159,#32160),(#32161,#32162),(#32163,#32164),(#32165,
#32166),(#32167,#32168),(#32169,#32170),(#32171,#32172),(#32173,#32174),
(#32175,#32176),(#32177,#32178),(#32179,#32180),(#32181,#32182),(#32183,
#32184),(#32185,#32186),(#32187,#32188),(#32189,#32190),(#32191,#32192),
(#32193,#32194),(#32195,#32196),(#32197,#32198),(#32199,#32200),(#32201,
#32202),(#32203,#32204),(#32205,#32206),(#32207,#32208),(#32209,#32210),
(#32211,#32212),(#32213,#32214),(#32215,#32216),(#32217,#32218),(#32219,
#32220),(#32221,#32222),(#32223,#32224),(#32225,#32226),(#32227,#32228),
(#32229,#32230),(#32231,#32232),(#32233,#32234),(#32235,#32236),(#32237,
#32238),(#32239,#32240),(#32241,#32242),(#32243,#32244),(#32245,#32246),
(#32247,#32248),(#32249,#32250),(#32251,#32252),(#32253,#32254),(#32255,
#32256),(#32257,#32258),(#32259,#32260),(#32261,#32262),(#32263,#32264),
(#32265,#32266),(#32267,#32268),(#32269,#32270),(#32271,#32272),(#32273,
#32274),(#32275,#32276),(#32277,#32278),(#32279,#32280),(#32281,#32282),
(#32283,#32284),(#32285,#32286),(#32287,#32288),(#32289,#32290),(#32291,
#32292),(#32293,#32294),(#32295,#32296),(#32297,#32298),(#32299,#32300),
(#32301,#32302),(#32303,#32304),(#32305,#32306),(#32307,#32308),(#32309,
#32310),(#32311,#32312),(#32313,#32314),(#32315,#32316),(#32317,#32318),
(#32319,#32320),(#32321,#32322),(#32323,#32324),(#32325,#32326),(#32327,
#32328),(#32329,#32330),(#32331,#32332),(#32333,#32334),(#32335,#32336),
(#32337,#32338),(#32339,#32340),(#32341,#32342),(#32343,#32344),(#32345,
#32346),(#32347,#32348),(#32349,#32350),(#32351,#32352),(#32353,#32354),
(#32355,#32356),(#32357,#32358),(#32359,#32360),(#32361,#32362),(#32363,
#32364),(#32365,#32366),(#32367,#32368),(#32369,#32370),(#32371,#32372),
(#32373,#32374),(#32375,#32376),(#32377,#32378),(#32379,#32380),(#32381,
#32382),(#32383,#32384),(#32385,#32386),(#32387,#32388),(#32389,#32390),
(#32391,#32392),(#32393,#32394),(#32395,#32396),(#32397,#32398),(#32399,
#32400),(#32401,#32402),(#32403,#32404),(#32405,#32406),(#32407,#32408),
(#32409,#32410),(#32411,#32412),(#32413,#32414),(#32415,#32416),(#32417,
#32418),(#32419,#32420),(#32421,#32422),(#32423,#32424),(#32425,#32426),
(#32427,#32428),(#32429,#32430),(#32431,#32432),(#32433,#32434),(#32435,
#32436),(#32437,#32438),(#32439,#32440),(#32441,#32442),(#32443,#32444),
(#32445,#32446),(#32447,#32448),(#32449,#32450),(#32451,#32452),(#32453,
#32454),(#32455,#32456),(#32457,#32458),(#32459,#32460),(#32461,#32462),
(#32463,#32464),(#32465,#32466),(#32467,#32468),(#32469,#32470),(#32471,
#32472),(#32473,#32474),(#32475,#32476),(#32477,#32478),(#32479,#32480),
(#32481,#32482),(#32483,#32484),(#32485,#32486),(#32487,#32488),(#32489,
#32490),(#32491,#32492),(#32493,#32494),(#32495,#32496),(#32497,#32498),
(#32499,#32500),(#32501,#32502),(#32503,#32504),(#32505,#32506),(#32507,
#32508),(#32509,#32510),(#32511,#32512),(#32513,#32514),(#32515,#32516),
(#32517,#32518),(#32519,#32520),(#32521,#32522),(#32523,#32524),(#32525,
#32526),(#32527,#32528),(#32529,#32530),(#32531,#32532),(#32533,#32534),
(#32535,#32536),(#32537,#32538),(#32539,#32540),(#32541,#32542),(#32543,
#32544),(#32545,#32546),(#32547,#32548),(#32549,#32550),(#32551,#32552),
(#32553,#32554),(#32555,#32556),(#32557,#32558),(#32559,#32560),(#32561,
#32562),(#32563,#32564),(#32565,#32566),(#32567,#32568),(#32569,#32570),
(#32571,#32572),(#32573,#32574),(#32575,#32576),(#32577,#32578),(#32579,
#32580),(#32581,#32582),(#32583,#32584),(#32585,#32586),(#32587,#32588),
(#32589,#32590),(#32591,#32592),(#32593,#32594),(#32595,#32596),(#32597,
#32598),(#32599,#32600),(#32601,#32602),(#32603,#32604),(#32605,#32606),
(#32607,#32608),(#32609,#32610),(#32611,#32612),(#32613,#32614),(#32615,
#32616),(#32617,#32618),(#32619,#32620),(#32621,#32622),(#32623,#32624),
(#32625,#32626),(#32627,#32628),(#32629,#32630),(#32631,#32632),(#32633,
#32634),(#32635,#32636),(#32637,#32638),(#32639,#32640),(#32641,#32642),
(#32643,#32644),(#32645,#32646),(#32647,#32648),(#32649,#32650),(#32651,
#32652),(#32653,#32654),(#32655,#32656),(#32657,#32658),(#32659,#32660),
(#32661,#32662),(#32663,#32664),(#32665,#32666),(#32667,#32668),(#32669,
#32670),(#32671,#32672),(#32673,#32674),(#32675,#32676),(#32677,#32678),
(#32679,#32680),(#32681,#32682),(#32683,#32684),(#32685,#32686),(#32687,
#32688),(#32689,#32690),(#32691,#32692),(#32693,#32694),(#32695,#32696),
(#32697,#32698),(#32699,#32700),(#32701,#32702),(#32703,#32704),(#32705,
#32706),(#32707,#32708),(#32709,#32710),(#32711,#32712),(#32713,#32714),
(#32715,#32716),(#32717,#32718),(#32719,#32720),(#32721,#32722),(#32723,
#32724),(#32725,#32726),(#32727,#32728),(#32729,#32730),(#32731,#32732),
(#32733,#32734),(#32735,#32736),(#32737,#32738),(#32739,#32740),(#32741,
#32742),(#32743,#32744),(#32745,#32746),(#32747,#32748),(#32749,#32750),
(#32751,#32752),(#32753,#32754),(#32755,#32756),(#32757,#32758),(#32759,
#32760),(#32761,#32762),(#32763,#32764),(#32765,#32766),(#32767,#32768),
(#32769,#32770),(#32771,#32772),(#32773,#32774),(#32775,#32776),(#32777,
#32778),(#32779,#32780),(#32781,#32782),(#32783,#32784),(#32785,#32786),
(#32787,#32788),(#32789,#32790),(#32791,#32792),(#32793,#32794),(#32795,
#32796),(#32797,#32798),(#32799,#32800),(#32801,#32802),(#32803,#32804),
(#32805,#32806),(#32807,#32808),(#32809,#32810),(#32811,#32812),(#32813,
#32814),(#32815,#32816),(#32817,#32818),(#32819,#32820),(#32821,#32822),
(#32823,#32824),(#32825,#32826),(#32827,#32828),(#32829,#32830),(#32831,
#32832),(#32833,#32834),(#32835,#32836),(#32837,#32838),(#32839,#32840),
(#32841,#32842),(#32843,#32844),(#32845,#32846),(#32847,#32848),(#32849,
#32850),(#32851,#32852),(#32853,#32854),(#32855,#32856),(#32857,#32858),
(#32859,#32860),(#32861,#32862),(#32863,#32864),(#32865,#32866),(#32867,
#32868),(#32869,#32870),(#32871,#32872),(#32873,#32874),(#32875,#32876),
(#32877,#32878),(#32879,#32880),(#32881,#32882),(#32883,#32884),(#32885,
#32886),(#32887,#32888),(#32889,#32890),(#32891,#32892),(#32893,#32894),
(#32895,#32896),(#32897,#32898),(#32899,#32900),(#32901,#32902),(#32903,
#32904),(#32905,#32906),(#32907,#32908),(#32909,#32910),(#32911,#32912),
(#32913,#32914),(#32915,#32916),(#32917,#32918),(#32919,#32920),(#32921,
#32922),(#32923,#32924),(#32925,#32926),(#32927,#32928),(#32929,#32930),
(#32931,#32932),(#32933,#32934),(#32935,#32936),(#32937,#32938),(#32939,
#32940),(#32941,#32942),(#32943,#32944),(#32945,#32946),(#32947,#32948),
(#32949,#32950),(#32951,#32952),(#32953,#32954),(#32955,#32956),(#32957,
#32958),(#32959,#32960),(#32961,#32962),(#32963,#32964),(#32965,#32966),
(#32967,#32968),(#32969,#32970),(#32971,#32972),(#32973,#32974),(#32975,
#32976),(#32977,#32978),(#32979,#32980),(#32981,#32982),(#32983,#32984),
(#32985,#32986),(#32987,#32988),(#32989,#32990),(#32991,#32992),(#32993,
#32994),(#32995,#32996),(#32997,#32998),(#32999,#33000),(#33001,#33002),
(#33003,#33004),(#33005,#33006),(#33007,#33008),(#33009,#33010),(#33011,
#33012),(#33013,#33014),(#33015,#33016),(#33017,#33018),(#33019,#33020),
(#33021,#33022),(#33023,#33024),(#33025,#33026),(#33027,#33028),(#33029,
#33030),(#33031,#33032),(#33033,#33034),(#33035,#33036),(#33037,#33038),
(#33039,#33040),(#33041,#33042),(#33043,#33044),(#33045,#33046),(#33047,
#33048),(#33049,#33050),(#33051,#33052),(#33053,#33054),(#33055,#33056),
(#33057,#33058),(#33059,#33060),(#33061,#33062),(#33063,#33064),(#33065,
#33066),(#33067,#33068),(#33069,#33070),(#33071,#33072),(#33073,#33074),
(#33075,#33076),(#33077,#33078),(#33079,#33080),(#33081,#33082),(#33083,
#33084),(#33085,#33086),(#33087,#33088),(#33089,#33090),(#33091,#33092),
(#33093,#33094),(#33095,#33096),(#33097,#33098),(#33099,#33100),(#33101,
#33102),(#33103,#33104),(#33105,#33106),(#33107,#33108),(#33109,#33110),
(#33111,#33112),(#33113,#33114),(#33115,#33116),(#33117,#33118),(#33119,
#33120),(#33121,#33122),(#33123,#33124),(#33125,#33126),(#33127,#33128),
(#33129,#33130),(#33131,#33132),(#33133,#33134),(#33135,#33136),(#33137,
#33138),(#33139,#33140),(#33141,#33142),(#33143,#33144),(#33145,#33146),
(#33147,#33148),(#33149,#33150),(#33151,#33152),(#33153,#33154),(#33155,
#33156),(#33157,#33158),(#33159,#33160),(#33161,#33162),(#33163,#33164),
(#33165,#33166),(#33167,#33168),(#33169,#33170),(#33171,#33172),(#33173,
#33174),(#33175,#33176),(#33177,#33178),(#33179,#33180),(#33181,#33182),
(#33183,#33184),(#33185,#33186),(#33187,#33188),(#33189,#33190),(#33191,
#33192),(#33193,#33194),(#33195,#33196),(#33197,#33198),(#33199,#33200),
(#33201,#33202),(#33203,#33204),(#33205,#33206),(#33207,#33208),(#33209,
#33210),(#33211,#33212),(#33213,#33214),(#33215,#33216),(#33217,#33218),
(#33219,#33220),(#33221,#33222),(#33223,#33224),(#33225,#33226),(#33227,
#33228),(#33229,#33230),(#33231,#33232),(#33233,#33234),(#33235,#33236)),
 .UNSPECIFIED.,.F.,.F.,.F.,(4,1,1,1,1,1,1,1,1,1,1,1,1,1,1,1,1,1,1,1,1,1,
1,1,1,1,1,1,1,1,1,1,1,1,1,1,1,1,1,1,1,1,1,1,1,1,1,1,1,1,1,1,1,1,1,1,1,1,
1,1,1,1,1,1,1,1,1,1,1,1,1,1,1,1,1,1,1,1,1,1,1,1,1,1,1,1,1,1,1,1,1,1,1,1,
1,1,1,1,1,1,1,1,1,1,1,1,1,1,1,1,1,1,1,1,1,1,1,1,1,1,1,1,1,1,1,1,1,1,1,1,
1,1,1,1,1,1,1,1,1,1,1,1,1,1,1,1,1,1,1,1,1,1,1,1,1,1,1,1,1,1,1,1,1,1,1,1,
1,1,1,1,1,1,1,1,1,1,1,1,1,1,1,1,1,1,1,1,1,1,1,1,1,1,1,1,1,1,1,1,1,1,1,1,
1,1,1,1,1,1,1,1,1,1,1,1,1,1,1,1,1,1,1,1,1,1,1,1,1,1,1,1,1,1,1,1,1,1,1,1,
1,1,1,1,1,1,1,1,1,1,1,1,1,1,1,1,1,1,1,1,1,1,1,1,1,1,1,1,1,1,1,1,1,1,1,1,
1,1,1,1,1,1,1,1,1,1,1,1,1,1,1,1,1,1,1,1,1,1,1,1,1,1,1,1,1,1,1,1,1,1,1,1,
1,1,1,1,1,1,1,1,1,1,1,1,1,1,1,1,1,1,1,1,1,1,1,1,1,1,1,1,1,1,1,1,1,1,1,1,
1,1,1,1,1,1,1,1,1,1,1,1,1,1,1,1,1,1,1,1,1,1,1,1,1,1,1,1,1,1,1,1,1,1,1,1,
1,1,1,1,1,1,1,1,1,1,1,1,1,1,1,1,1,1,1,1,1,1,1,1,1,1,1,1,1,1,1,1,1,1,1,1,
1,1,1,1,1,1,1,1,1,1,1,1,1,1,1,1,1,1,1,1,1,1,1,1,1,1,1,1,1,1,1,1,1,1,1,1,
1,1,1,1,1,1,1,1,1,1,1,1,1,1,1,1,1,1,1,1,1,1,1,1,1,1,1,1,1,1,1,1,1,1,1,1,
1,1,1,1,1,1,1,1,1,1,1,1,1,1,1,1,1,1,1,1,1,1,1,1,1,1,1,1,1,1,1,1,1,1,1,1,
1,1,1,1,1,1,1,1,1,1,1,1,1,1,1,1,1,1,1,1,1,1,1,1,1,1,1,1,1,1,1,1,1,1,1,1,
1,1,1,1,1,1,1,1,1,1,1,1,1,1,1,1,1,1,1,1,1,1,1,1,1,1,1,1,1,1,1,1,1,1,1,1,
1,1,1,1,1,1,1,1,1,1,1,1,1,1,1,1,1,1,1,1,1,1,1,1,1,1,1,1,1,1,1,1,1,1,1,1,
1,1,1,1,1,1,1,1,1,1,1,1,1,1,1,1,1,1,1,1,1,1,1,1,1,1,1,1,1,1,1,1,1,1,1,1,
1,1,1,1,1,1,1,1,1,1,1,1,1,1,1,1,1,1,1,1,1,1,1,1,1,1,1,1,1,1,1,1,1,1,1,1,
1,1,1,1,1,1,1,1,1,1,1,1,1,1,1,1,1,1,1,1,1,1,1,1,1,1,1,1,1,1,1,1,1,1,1,1,
1,1,1,1,1,1,1,1,1,1,1,1,1,1,1,1,1,1,1,1,1,1,1,1,1,1,1,1,1,1,1,1,1,1,1,1,
1,1,1,1,1,1,1,1,1,1,1,1,1,1,1,1,1,1,1,1,1,1,1,1,1,1,1,1,1,1,1,1,1,1,1,1,
1,1,1,1,1,1,1,1,1,1,1,1,1,1,1,1,1,1,1,1,1,1,1,1,1,1,1,1,1,1,1,1,1,1,1,1,
1,1,1,1,1,1,1,1,1,1,1,1,1,1,1,1,1,1,1,1,1,1,1,1,1,1,1,1,1,1,1,1,1,1,1,1,
1,1,1,1,1,1,1,1,1,1,1,1,1,1,1,1,1,1,1,1,1,1,1,1,1,1,1,1,1,1,1,1,1,1,1,1,
1,1,1,1,1,1,1,1,1,1,1,1,1,1,1,1,1,1,1,1,1,1,1,1,1,1,1,1,1,1,1,1,1,1,1,1,
1,1,1,1,1,1,1,1,1,1,1,1,1,1,1,1,1,1,1,1,1,1,1,1,1,1,1,1,1,1,1,1,1,1,1,1,
1,1,1,1,1,1,1,1,1,1,1,1,1,1,1,1,1,1,1,1,1,1,1,1,1,1,1,1,1,1,1,1,1,1,1,1,
1,1,1,1,1,1,1,1,1,1,1,1,1,1,1,1,1,1,1,1,1,1,1,1,1,1,1,1,1,1,1,1,1,1,1,1,
1,1,1,1,1,1,1,1,1,1,1,1,1,1,1,1,1,1,1,1,1,1,1,1,1,1,1,1,1,1,1,1,1,1,1,1,
1,1,1,1,1,1,1,1,1,1,1,1,1,1,1,1,1,1,1,1,1,1,1,1,1,1,1,1,1,1,1,1,1,1,1,1,
1,1,1,1,1,1,1,1,1,1,1,1,1,1,1,1,1,1,1,1,1,1,1,1,1,1,1,1,1,1,1,1,1,1,1,1,
1,1,1,1,1,1,1,1,1,1,1,1,1,1,1,1,1,1,1,1,1,1,1,1,1,1,1,1,1,1,1,1,1,1,1,1,
1,1,1,1,1,1,1,1,1,1,1,1,1,1,1,1,1,1,1,1,1,1,1,1,1,1,1,1,1,1,1,1,1,1,1,1,
1,1,1,1,1,1,1,1,1,1,1,1,1,1,1,1,1,1,1,1,1,1,1,1,1,1,1,1,1,1,1,1,1,1,1,1,
1,1,1,1,1,1,1,1,1,1,1,1,1,1,1,1,1,1,1,1,1,1,1,1,1,1,1,1,1,1,1,1,1,1,1,1,
1,1,1,1,1,1,1,1,1,1,1,1,1,1,1,1,1,1,1,1,1,1,1,1,1,1,1,1,1,1,1,1,1,1,1,1,
1,1,1,1,1,1,1,1,1,1,1,1,1,1,1,1,1,1,1,1,1,1,1,1,1,1,1,1,1,1,1,1,1,1,1,1,
1,1,1,1,1,1,1,1,1,1,1,1,1,1,1,1,1,1,1,1,1,1,1,1,1,1,1,1,1,1,1,1,1,1,1,1,
1,1,1,1,1,1,1,1,1,1,1,1,1,1,1,1,1,1,1,1,1,1,1,1,1,1,1,1,1,1,1,1,1,1,1,1,
1,1,1,1,1,1,1,1,1,1,1,1,1,1,1,1,1,1,1,1,1,1,1,1,1,1,1,1,1,1,1,1,1,1,1,1,
1,1,1,1,1,1,1,1,1,1,1,1,1,1,1,1,1,1,1,1,1,1,1,1,1,1,1,1,1,1,1,1,1,1,1,1,
1,1,1,1,1,1,1,1,1,1,1,1,1,1,1,1,1,1,1,1,1,1,1,1,1,1,1,1,1,1,1,1,1,1,1,1,
1,1,1,1,1,1,1,1,1,1,1,1,1,1,1,1,1,1,1,1,1,1,1,1,1,1,1,1,1,1,1,1,1,1,1,1,
1,1,1,1,1,1,1,1,1,1,1,1,1,1,1,1,1,1,1,1,1,1,1,1,1,1,1,1,1,1,1,1,1,1,1,1,
1,1,1,1,1,1,1,1,1,1,1,1,1,1,1,1,1,1,1,1,1,1,1,1,1,1,1,1,1,1,1,1,1,1,1,1,
1,1,1,1,1,1,1,1,1,1,1,1,1,1,1,1,1,1,1,1,1,1,1,1,1,1,1,1,1,1,1,1,1,1,1,1,
1,1,1,1,1,1,1,1,1,1,1,1,1,1,1,1,1,1,1,1,1,1,1,1,1,1,1,1,1,1,1,1,1,1,1,1,
1,1,1,1,1,1,1,1,1,1,1,1,1,1,1,1,1,1,1,1,1,1,1,1,1,1,1,1,1,1,1,1,1,1,1,1,
1,1,1,1,1,1,1,1,1,1,1,1,1,1,1,1,1,1,1,1,1,1,1,1,1,1,1,1,1,1,1,1,1,1,1,1,
1,1,1,1,1,1,1,1,1,1,1,1,1,1,1,1,1,1,1,1,1,1,1,1,1,1,1,1,1,1,1,1,1,1,1,1,
1,1,1,1,1,1,1,1,1,1,1,1,1,1,1,1,1,1,1,1,1,1,1,1,1,1,1,1,1,1,1,1,1,1,1,1,
1,1,1,1,1,1,1,1,1,1,1,1,1,1,1,1,1,1,1,1,1,1,1,1,1,1,1,1,1,1,1,1,1,1,1,1,
1,1,1,1,1,1,1,1,1,1,1,1,1,1,1,1,1,1,1,1,1,1,1,1,1,1,1,1,1,1,1,1,1,1,1,1,
1,1,1,1,1,1,1,1,1,1,1,1,1,1,1,1,1,1,1,1,1,1,1,1,1,1,1,1,1,1,1,1,1,1,1,1,
1,1,1,1,1,1,1,1,1,1,1,1,1,1,1,1,1,1,1,1,1,1,1,1,1,1,1,1,1,1,1,1,1,1,1,1,
1,1,1,1,1,1,1,1,1,1,1,1,1,1,1,1,1,1,1,1,1,1,1,1,1,1,1,1,1,1,1,1,1,1,1,1,
1,1,1,1,1,1,1,1,1,1,1,1,1,1,1,1,1,1,1,1,1,1,1,1,1,1,1,1,1,1,1,1,1,1,1,1,
1,1,1,1,1,1,1,1,1,1,1,1,1,1,1,1,1,1,1,1,1,1,1,1,1,1,1,1,1,1,1,1,1,1,1,1,
1,1,1,1,1,1,1,1,1,1,1,1,1,1,1,1,1,1,1,1,1,1,1,1,1,1,1,1,1,1,1,1,1,1,1,1,
1,1,1,1,1,1,1,1,1,1,1,1,1,1,1,1,1,1,1,1,1,1,1,1,1,1,1,1,1,1,1,1,1,1,1,1,
1,1,1,1,1,1,1,1,1,1,1,1,1,1,1,1,1,1,1,1,1,1,1,1,1,1,1,1,1,1,1,1,1,1,1,1,
1,1,1,1,1,1,1,1,1,1,1,1,1,1,1,1,1,1,1,1,1,1,1,1,1,1,1,1,1,1,1,1,1,1,1,1,
1,1,1,1,1,1,1,1,1,1,1,1,1,1,1,1,1,1,1,1,1,1,1,1,1,1,1,1,1,1,1,1,1,1,1,1,
1,1,1,1,1,1,1,1,1,1,1,1,1,1,1,1,1,1,1,1,1,1,1,1,1,1,1,1,1,1,1,1,1,1,1,1,
1,1,1,1,1,1,1,1,1,1,1,1,1,1,1,1,1,1,1,1,1,1,1,1,1,1,1,1,1,1,1,1,1,1,1,1,
1,1,1,1,1,1,1,1,1,1,1,1,1,1,1,1,1,1,1,1,1,1,1,1,1,1,1,1,1,1,1,1,1,1,1,1,
1,1,1,1,1,1,1,1,1,1,1,1,1,1,1,1,1,1,1,1,1,1,1,1,1,1,1,1,1,1,1,1,1,1,1,1,
1,1,1,1,1,1,1,1,1,1,1,1,1,1,1,1,1,1,1,1,1,1,1,1,1,1,1,1,1,1,1,1,1,1,1,1,
1,1,1,1,1,1,1,1,1,1,1,1,1,1,1,1,1,1,1,1,1,1,1,1,1,1,1,1,1,1,1,1,1,1,1,1,
1,1,1,1,1,1,1,1,1,1,1,1,1,1,1,1,1,1,1,1,1,1,1,1,1,1,1,1,1,1,1,1,1,1,1,1,
1,1,1,1,1,1,1,1,1,1,1,1,1,1,1,1,1,1,1,1,1,1,1,1,1,1,1,1,1,1,1,1,1,1,1,1,
1,1,1,1,1,1,1,1,1,1,1,1,1,1,1,1,1,1,1,1,1,1,1,1,1,1,1,1,1,1,1,1,1,1,1,1,
1,1,1,1,1,1,1,1,1,1,1,1,1,1,1,1,1,1,1,1,1,1,1,1,1,1,1,1,1,1,1,1,1,1,1,1,
1,1,1,1,1,1,1,1,1,1,1,1,1,1,1,1,1,1,1,1,1,1,1,1,1,1,1,1,1,1,1,1,1,1,1,1,
1,1,1,1,1,1,1,1,1,1,1,1,1,1,1,1,1,1,1,1,1,1,1,1,1,1,1,1,1,1,1,1,1,1,1,1,
1,1,1,1,1,1,1,1,1,1,1,1,1,1,1,1,1,1,1,1,1,1,1,1,1,1,1,1,1,1,1,1,1,1,1,1,
1,1,1,1,1,1,1,1,1,1,1,1,1,1,1,1,1,1,1,1,1,1,1,1,1,1,1,1,1,1,1,1,1,1,1,1,
1,1,1,1,1,1,1,1,1,1,1,1,1,1,1,1,1,1,1,1,1,1,1,1,1,1,1,1,1,1,1,1,1,1,1,1,
1,1,1,1,1,1,1,1,1,1,1,1,1,1,1,1,1,1,1,1,1,1,1,1,1,1,1,1,1,1,1,1,1,1,1,1,
1,1,1,1,1,1,1,1,1,1,1,1,1,1,1,1,1,1,1,1,1,1,1,1,1,1,1,1,1,1,1,1,1,1,1,1,
1,1,1,1,1,1,1,1,1,1,1,1,1,1,1,1,1,1,1,1,1,1,1,1,1,1,1,1,1,1,1,1,1,1,1,1,
1,1,1,1,1,1,1,1,1,1,1,1,1,1,1,1,1,1,1,1,1,1,1,1,1,1,1,1,1,1,1,1,1,1,1,1,
1,1,1,1,1,1,1,1,1,1,1,1,1,1,1,1,1,1,1,1,1,1,1,1,1,1,1,1,1,1,1,1,1,1,1,1,
1,1,1,1,1,1,1,1,1,1,1,1,1,1,1,1,1,1,1,1,1,1,1,1,1,1,1,1,1,1,1,1,1,1,1,1,
1,1,1,1,1,1,1,1,1,1,1,1,1,1,1,1,1,1,1,1,1,1,1,1,1,1,1,1,1,1,1,1,1,1,1,1,
1,1,1,1,1,1,1,1,1,1,1,1,1,1,1,1,1,1,1,1,1,1,1,1,1,1,1,1,1,1,1,1,1,1,1,1,
1,1,1,1,1,1,1,1,1,1,1,1,1,1,1,1,1,1,1,1,1,1,1,1,1,1,1,1,1,1,1,1,1,1,1,1,
1,1,1,1,1,1,1,1,1,1,1,1,1,1,1,1,1,1,1,1,1,1,1,1,1,1,1,1,1,1,1,1,1,1,1,1,
1,1,1,1,1,1,1,1,1,1,1,1,1,1,1,1,1,1,1,1,1,1,1,1,1,1,1,1,1,1,1,1,1,1,1,1,
1,1,1,1,1,1,1,1,1,1,1,1,1,1,1,1,1,1,1,1,1,1,1,1,1,1,1,1,1,1,1,1,1,1,1,1,
1,1,1,1,1,1,1,1,1,1,1,1,1,1,1,1,1,1,1,1,1,1,1,1,1,1,1,1,1,1,1,1,1,1,1,1,
1,1,1,1,1,1,1,1,1,1,1,1,1,1,1,1,1,1,1,1,1,1,1,1,1,1,1,1,1,1,1,1,1,1,1,1,
1,1,1,1,1,1,1,1,1,1,1,1,1,1,1,1,1,1,1,1,1,1,1,1,1,1,1,1,1,1,1,1,1,1,1,1,
1,1,1,1,1,1,1,1,1,1,1,1,1,1,1,1,1,1,1,1,1,1,1,1,1,1,1,1,1,1,1,1,1,1,1,1,
1,1,1,1,1,1,1,1,1,1,1,1,1,1,1,1,1,1,1,1,1,1,1,1,1,1,1,1,1,1,1,1,1,1,1,1,
1,1,1,1,4),(2,2),(0.,0.869746702321014,1.7394931589914,2.60923976624962,
3.47983908319159,4.35043840179749,5.22018503077054,6.08993165951504,6.95967828799171,
7.82942491616733,8.69917154401062,9.56891817149224,10.4395174886835,11.3101168056706,
12.179863432132,13.049610058144,13.9193566836854,14.7891033087372,15.6588499332817,
16.5285965573034,17.3991958717975,18.2697951860185,18.7046684974166,19.1395418086746,
19.5744151197912,20.0092884307654,20.4441617415962,20.8790350522825,21.7487816732187,
22.1836549834672,22.6185282935685,23.0534016035221,23.4882749133276,23.9231482229848,
24.3588742245859,24.794600226187,25.2294735355468,26.0992201538203,26.5340934627341,
26.9689667714994,27.4038400801166,27.838713388586,28.2735866969081,28.7084600050832,
29.143333313112,29.5782066209952,30.0130799287334,30.4479532363275,30.8828265437783,
31.3185525442794,31.7542785447804,32.1891518519474,32.6240251589741,33.0588984658616,
33.4937717726112,33.928645079224,34.3635183857014,34.7983916920448,35.2332649982556,
35.6681383043353,36.1030116102854,36.5378849161076,36.9727582218035,37.4076315273749,
37.8425048328235,38.2782308323341,38.7139568318446,39.1488301370532,39.5837034421446,
40.0185767471208,40.4534500519838,40.8883233567357,41.3231966613787,41.7580699659148,
42.1929432703463,42.6278165746754,43.0626898789044,43.4975631830356,43.9324364870714,
44.3673097910142,44.8021830948664,45.2379090935952,45.673635092324,46.1085083960024,
46.5433816995978,46.9782550031127,47.4131283065497,47.8480016099115,48.2828749132006,
48.7177482164198,49.1526215195718,49.5874948226593,50.0223681256851,50.457241428652,
50.8921147315628,51.3269880344203,51.7618613372274,52.197587335454,52.6333133336805,
53.0681866363954,53.5030599390685,53.9379332417027,54.3728065443011,54.8076798468664,
55.2425531494018,55.6774264519101,56.1122997543943,56.5471730568575,56.9820463593026,
57.4169196617326,57.8517929641506,58.2866662665595,58.7215395689624,59.157265567009,
59.5929915650557,60.0278648674556,60.4627381698584,60.8976114722673,61.3324847746853,
61.7673580771153,62.2022313795604,62.6371046820236,63.0719779845079,63.5068512870162,
63.9417245895516,64.376597892117,64.8114711947155,65.2463444973499,65.6812178000231,
66.1169437982275,66.5526697964318,66.9875430991915,67.4224164019987,67.8572897048563,
68.2921630077673,68.7270363107343,69.1619096137603,69.5967829168479,70.0316562200001,
70.4665295232194,70.9014028265087,71.3362761298705,71.7711494333077,72.2060227368227,
72.6408960404182,73.0766220391044,73.5123480377905,73.9472213415547,74.382094645407,
74.8169679493499,75.2518412533859,75.6867145575172,76.1215878617464,76.5564611660756,
76.9913344705072,77.4262077750435,77.8610810796866,78.2959543844386,78.7308276893018,
79.1657009942781,79.6005742993696,80.0363002988208,80.4720262982719,80.9068996035997,
81.3417729090484,81.7766462146199,82.211519520316,82.6463928261383,83.0812661320886,
83.5161394381684,83.9510127443794,84.3858860507229,84.8207593572004,85.2556326638134,
85.6905059705631,86.1253792774507,86.5602525844776,86.995978584908,87.4317045853384,
87.8665778926469,88.3014512000977,88.7363245076919,89.1711978154302,89.6060711233134,
90.0409444313423,90.4758177395175,90.9106910478396,91.345564356309,91.7804376649263,
92.2153109736917,92.6501842826055,93.085057591668,93.5199309008791,93.9556569024059,
94.3913829039327,94.8262562134414,95.2611295230986,95.6960028329042,96.1308761428578,
96.5657494529591,97.0006227632077,97.4354960736028,97.870369384144,98.3052426948304,
98.7401160056612,99.1749893166354,99.6098626277522,100.04473593901,100.915335253024,
101.351061255639,101.785934567313,102.220807879124,102.655681191068,103.090554503145,
103.525427815353,104.395174440154,105.264921065453,105.699794378283,106.134667691232,
106.569541004295,107.004414317471,107.8750136343,108.745612951339,109.615359578629,
110.485106206296,111.354852834309,112.224599462639,113.094346091254,113.964092720119,
114.834692038763,115.705291357499,116.575037986826,117.444784616267,118.314531245777,
119.184277875311,120.054024504821,120.923771134261,121.794370453112,122.66496977189,
123.534716400968,124.404463029834,125.274209658448,126.143956286779,127.013702914792,
127.883449542458,128.754048859798,129.624648176939,130.494394803617,131.364141429857,
132.233888055637,133.103634680937,133.973381305737,134.843127930023,135.71372724472,
136.584326559147,137.019199870684,137.454073182083,137.888946493341,138.323819804458,
139.193566426263,140.063313047491,140.498186357887,140.933059668136,141.367932978237,
141.802806288191,142.237679597997,142.673405599673,143.109131601348,143.544004910857,
143.978878220217,144.413751529429,144.848624838491,145.283498147405,145.718371456171,
146.153244764789,146.588118073258,147.022991381581,147.457864689756,147.892737997785,
148.327611305669,148.762484613407,149.197357921002,149.633083921574,150.068809922147,
150.503683229455,150.938556536623,151.37342984365,151.808303150538,152.243176457288,
152.678049763901,153.112923070379,153.547796376722,153.982669682934,154.417542989014,
154.852416294964,155.287289600787,155.722162906483,156.157036212055,156.592762211626,
157.028488211198,157.463361516526,157.898234821735,158.333108126826,158.767981431803,
159.202854736666,159.637728041419,160.072601346062,160.507474650599,160.94234795503,
161.37722125936,161.812094563589,162.246967867721,162.681841171757,163.1167144757,
163.552440474473,163.988166473247,164.423039777011,164.85791308069,165.292786384286,
165.727659687801,166.162532991238,166.597406294601,167.03227959789,167.46715290111,
167.902026204262,168.33689950735,168.771772810376,169.206646113343,169.641519416254,
170.076392719112,170.512118717363,170.947844715614,171.382718018374,171.817591321089,
172.252464623762,172.687337926397,173.122211228996,173.557084531561,173.991957834097,
174.426831136606,174.86170443909,175.296577741554,175.731451044,176.16632434643,
176.601197648848,177.036070951258,177.471796949306,177.907522947355,178.342396249755,
178.777269552155,179.212142854558,179.647016156968,180.081889459386,180.516762761816,
180.951636064262,181.386509366726,181.82138266921,182.256255971719,182.691129274255,
183.12600257682,183.560875879419,183.995749182054,184.431475180237,184.867201178421,
185.302074481136,185.736947783896,186.171821086704,186.606694389561,187.041567692473,
187.47644099544,187.911314298466,188.346187601554,188.781060904706,189.215934207926,
189.650807511215,190.085680814577,190.520554118015,190.95542742153,191.391153420175,
191.82687941882,192.261752722499,192.696626026263,193.131499330116,193.566372634059,
194.001245938095,194.436119242227,194.870992546456,195.305865850785,195.740739155217,
196.175612459754,196.610485764397,197.045359069149,197.480232374013,197.915105678989,
198.350831678382,198.786557677775,199.221430982984,199.656304288312,200.091177593761,
200.526050899333,200.960924205029,201.395797510852,201.830670816802,202.265544122882,
202.700417429093,203.135290735437,203.570164041915,204.005037348528,204.439910655278,
204.874783962166,205.310509962526,205.746235962887,206.181109270054,206.615982577363,
207.050855884814,207.485729192409,207.920602500147,208.355475808031,208.79034911606,
209.225222424235,209.660095732558,210.094969041027,210.529842349645,210.96471565841,
211.399588967324,211.834462276387,212.27018827784,212.705914279292,213.140787588653,
213.575660898161,214.010534207819,214.880280827579,215.31515413768,215.750027447929,
216.184900758324,216.619774068866,217.054647379553,217.489520690384,218.359267312475,
219.22986662628,219.665592628826,220.100465940363,220.535339252038,220.970212563848,
221.83995918787,222.709705812416,223.579452437468,224.014325750179,224.44919906301,
225.318945689022,226.189545005688,227.060144322571,227.929890949664,228.799637577146,
229.66938420499,230.539130833166,231.408877461643,232.278624090388,233.149223408954,
234.019822727623,234.889569356878,235.759315986267,236.629062615749,237.498809245277,
238.368555874806,239.238302504287,240.108901823183,240.979501142017,241.849247771189,
242.718994400167,243.588741028911,244.458487657389,245.328234285565,246.197980913409,
247.068580230891,247.939179548182,248.80892617507,249.678672801532,250.548419427545,
251.418166053087,252.287912678139,253.157659302684,254.028258617581,254.898857932211,
255.333731243885,255.768604555423,256.203477866821,256.63835117808,257.508097800171,
258.377844421689,258.812717732231,259.247591042627,259.682464352876,260.117337662977,
260.552210972931,260.987936974682,261.858536286089,262.293409595598,262.728282904958,
263.16315621417,263.598029523233,264.032902832147,264.467776140913,264.902649449531,
265.337522758001,265.772396066323,266.207269374499,266.642142682528,267.077015990412,
267.511889298151,267.947615298795,268.383341299439,268.81821460689,269.2530879142,
269.687961221367,270.122834528394,270.557707835282,270.992581142032,271.427454448646,
271.862327755124,272.297201061468,272.732074367679,273.166947673759,273.60182097971,
274.036694285533,274.471567591229,274.907293590862,275.343019590495,275.777892895944,
276.212766201272,276.647639506481,277.082512811573,277.51738611655,277.952259421414,
278.387132726166,278.82200603081,279.256879335346,279.691752639779,280.126625944108,
280.561499248338,280.996372552469,281.431245856506,281.866971855324,282.302697854143,
282.737571157996,283.172444461761,283.60731776544,284.042191069036,284.477064372551,
284.911937675989,285.346810979351,285.781684282641,286.216557585861,286.651430889013,
287.086304192101,287.521177495128,287.956050798095,288.390924101007,288.826650099283,
289.262376097559,289.697249400366,290.132122703127,290.566996005842,291.001869308516,
291.43674261115,291.871615913749,292.306489216315,292.741362518851,293.17623582136,
293.611109123845,294.045982426308,294.480855728754,294.915729031185,295.350602333603,
295.786328331655,296.222054329707,296.65692763211,297.091800934511,297.526674236911,
297.961547539314,298.396420841724,298.831294144142,299.266167446573,299.701040749018,
300.135914051482,300.570787353967,301.005660656476,301.440533959012,301.875407261578,
302.310280564177,302.746006562341,303.181732560506,303.616605863179,304.051479165895,
304.486352468655,304.921225771462,305.35609907432,305.790972377232,306.225845680199,
306.660718983226,307.095592286314,307.530465589466,307.965338892686,308.400212195976,
308.835085499338,309.269958802776,309.705684801381,310.141410799985,310.576284103581,
311.01115740726,311.446030711025,311.880904014878,312.315777318821,312.750650622858,
313.185523926989,313.620397231219,314.055270535549,314.490143839981,314.925017144517,
315.359890449161,315.794763753913,316.229637058777,316.665363058112,317.101089057448,
317.53596236254,317.970835667749,318.405708973077,318.840582278526,319.275455584098,
319.710328889795,320.145202195618,320.580075501568,321.014948807648,321.44982211386,
321.884695420204,322.319568726682,322.754442033295,323.189315340045,323.625041340336,
324.060767340628,324.495640647655,324.930513954822,325.365387262131,325.800260569583,
326.235133877177,326.670007184916,327.1048804928,327.539753800829,327.974627109005,
328.409500417327,328.844373725797,329.279247034415,329.714120343181,330.148993652095,
330.584719653474,331.020445654852,331.455318964064,331.890192273424,332.325065582933,
332.759938892591,333.194812202397,333.629685512351,334.064558822453,334.499432132702,
334.934305443098,335.369178753639,335.804052064326,336.673798686132,337.108671997249,
337.544397999725,337.980124002201,338.4149973136,338.849870625137,339.284743936812,
340.154490560568,341.024237184854,341.459110497191,341.893983809655,342.328857122244,
342.763730434955,343.633477060735,344.504076377234,345.374675693955,346.244422320844,
347.114168948136,347.983915575803,348.853662203817,349.723408832148,350.593155460764,
351.463754779246,352.334354097839,353.204100727012,354.07384735634,354.943593985781,
355.813340615292,356.683087244827,357.552833874338,358.423433193272,359.294032512154,
360.163779141409,361.033525770489,361.903272399355,362.77301902797,363.642765656301,
364.512512284316,365.383111601936,366.253710919371,367.123457546465,367.993204173143,
368.862950799383,369.732697425164,370.602444050463,371.472190675265,372.342789990359,
373.21338930519,373.648262617,374.083135928675,374.952882551611,375.822629173987,
376.257502484962,376.692375795793,377.12724910648,377.562122417021,377.996995727417,
378.431869037666,378.866742347767,379.302468349591,379.738194351416,380.173067661222,
380.607940970879,381.042814280388,381.477687589749,381.91256089896,382.347434208023,
382.782307516937,383.217180825703,383.652054134321,384.086927442791,384.521800751113,
384.956674059289,385.391547367318,385.826420675202,386.262146675918,386.697872676635,
387.13274598423,387.567619291681,388.00249259899,388.437365906157,388.872239213185,
389.307112520073,389.741985826823,390.176859133436,390.611732439914,391.046605746258,
391.48147905247,391.91635235855,392.351225664501,392.786098970323,393.221824970019,
393.657550969714,394.092424275286,394.527297580735,394.962170886063,395.397044191272,
395.831917496364,396.266790801341,396.701664106204,397.136537410957,397.5714107156,
398.006284020137,398.441157324569,398.876030628899,399.310903933128,399.74577723726,
400.181503236126,400.617229234991,401.052102538934,401.486975842787,401.921849146551,
402.356722450231,402.791595753827,403.226469057342,403.66134236078,404.096215664142,
404.531088967432,404.965962270651,405.400835573804,405.835708876892,406.270582179918,
406.705455482886,407.141181481189,407.576907479491,408.01178078235,408.446654085157,
408.881527387917,409.316400690633,409.751273993306,410.186147295941,410.62102059854,
411.055893901106,411.490767203642,411.925640506151,412.360513808636,412.795387111099,
413.230260413545,413.665133715976,414.100859714032,414.536585712088,414.971459014498,
415.406332316901,415.841205619301,416.276078921702,416.710952224105,417.145825526515,
417.580698828933,418.015572131364,418.45044543381,418.885318736273,419.320192038758,
419.755065341267,420.189938643803,420.624811946369,421.060537944515,421.496263942662,
421.931137245297,422.36601054797,422.800883850686,423.235757153446,423.670630456253,
424.105503759112,424.540377062023,424.975250364991,425.410123668017,425.844996971105,
426.279870274258,426.714743577477,427.149616880767,427.584490184129,428.020216182695,
428.455942181261,428.890815484776,429.325688788373,429.760562092052,430.195435395816,
430.630308699669,431.065182003612,431.500055307649,431.93492861178,432.36980191601,
432.80467522034,433.239548524772,433.674421829309,434.109295133952,434.544168438705,
434.979894437984,435.415620437262,435.850493742239,436.285367047331,436.72024035254,
437.155113657869,437.589986963318,438.024860268889,438.459733574586,438.894606880409,
439.32948018636,439.76435349244,440.199226798651,440.634100104995,441.068973411473,
441.503846718087,441.939572718309,442.375298718531,442.810172025419,443.245045332447,
443.679918639614,444.114791946923,444.549665254374,444.984538561969,445.419411869708,
445.854285177591,446.289158485621,446.724031793796,447.158905102119,447.593778410589,
448.028651719207,448.463525027973,448.899251029277,449.334977030581,449.769850339644,
450.639596958216,451.074470267725,451.509343577383,451.944216887189,452.379090197143,
452.813963507244,453.248836817493,453.683710127889,454.118583438431,454.553456749117,
454.988330059949,455.423203370923,455.858929373329,456.294655375734,456.729528686993,
457.164401998391,457.599275309929,458.469021933414,458.90389524536,459.338768557437,
459.773641869646,460.208515181983,460.643388494447,461.078261807036,461.948008432578,
462.818607748906,463.689207065461,464.55895369214,465.428700319234,466.298446946716,
467.16819357456,468.037940202737,468.907686831215,469.778286149605,470.648885468116,
471.518632097196,472.388378726451,473.258125355841,474.127871985322,474.997618614851,
475.86736524438,476.737964563343,477.608563882265,478.478310511593,479.348057140765,
480.217803769743,481.087550398488,481.957297026966,482.827043655142,483.697642972895,
484.568242290469,485.43798891776,486.307735544649,487.177482171112,488.047228797125,
488.916975422667,489.78672204772,490.657321363009,491.09304736596,491.527920678038,
492.397667301793,493.267413925005,494.137160547663,494.57203385878,495.006907169755,
495.441780480586,495.876653791273,496.311527101814,496.74640041221,497.616999724357,
498.052725726255,498.487599036209,498.922472346015,499.357345655673,499.792218965182,
500.227092274542,500.661965583754,501.096838892816,501.531712201731,501.966585510497,
502.401458819114,502.836332127584,503.271205435907,503.706078744082,504.140952052112,
504.576678052901,505.01240405369,505.447277361429,505.882150669023,506.317023976474,
506.751897283783,507.186770590951,507.621643897978,508.056517204866,508.491390511616,
508.92626381823,509.361137124708,509.796010431052,510.230883737263,510.665757043344,
511.100630349294,511.536356349053,511.972082348811,512.406955654506,512.841828960076,
513.276702265523,513.711575570849,514.146448876056,514.581322181146,515.016195486121,
515.451068790983,515.885942095733,516.320815400375,516.75568870491,517.19056200934,
517.625435313668,518.060308617896,518.496034616807,518.931760615718,519.366633919752,
519.801507223694,520.236380527545,520.671253831307,521.106127134985,521.541000438579,
521.975873742092,522.410747045528,522.845620348888,523.280493652176,523.715366955394,
524.150240258545,524.585113561631,525.019986864656,525.455712862985,525.891438861313,
526.326312164223,526.761185467079,527.196058769885,527.630932072643,528.065805375356,
528.500678678029,528.935551980661,529.370425283258,529.805298585822,530.240171888356,
530.675045190863,531.109918493346,531.544791795808,531.979665098252,532.415391096312,
532.851117094373,533.285990396789,533.720863699197,534.155737001598,534.590610303997,
535.025483606395,535.460356908796,535.895230211204,536.330103513621,536.764976816049,
537.199850118493,537.634723420955,538.069596723438,538.504470025945,538.93934332848,
539.375069326608,539.810795324736,540.245668627333,540.680541929966,541.115415232637,
541.550288535351,541.985161838109,542.420035140915,542.854908443771,543.28978174668,
543.724655049646,544.15952835267,544.594401655757,545.029274958907,545.464148262125,
545.899021565413,546.334747563939,546.770473562465,547.205346865901,547.640220169415,
548.075093473009,548.509966776686,548.944840080449,549.3797133843,549.814586688241,
550.249459992276,550.684333296405,551.119206600633,551.554079904961,551.988953209391,
552.423826513926,552.858699818567,553.294425817789,553.73015181701,554.165025121872,
554.599898426846,555.034771731937,555.469645037144,555.90451834247,556.339391647917,
556.774264953487,557.209138259182,557.644011565003,558.078884870951,558.51375817703,
558.948631483239,559.383504789581,559.818378096058,560.254104096209,560.689830096361,
561.12470340311,561.559576709996,561.994450017021,562.429323324187,562.864196631494,
563.299069938943,563.733943246536,564.168816554273,564.603689862154,565.038563170182,
565.473436478355,565.908309786676,566.343183095144,566.77805640376,567.213782404988,
567.649508406216,568.084381715128,568.519255024189,568.954128333399,569.389001642757,
569.823874952264,570.258748261921,570.693621571725,571.128494881677,571.563368191777,
572.433114812417,572.867988122957,573.302861433642,573.737734744471,574.173460746804,
574.609186749136,575.044060060251,575.913806682904,576.783553306113,577.218426617922,
577.653299929865,578.08817324194,578.523046554147,579.392793178944,580.26253980424,
581.13313912039,581.568865123709,582.003738436771,582.87348506323,583.743231690115,
584.612978317402,585.482724945065,586.352471573076,587.222218201403,588.092817519691,
588.963416838109,589.833163467083,590.702910096251,591.572656725575,592.442403355013,
593.31214998452,594.181896614051,595.05249593303,595.92309525198,596.792841881366,
597.662588510618,598.532335139693,599.402081768556,600.271828397167,601.141575025495,
602.012174343369,602.882773661074,603.752520288553,604.622266915642,605.492013542317,
606.361760168553,607.23150679433,608.101253419626,608.971852735101,609.842452050322,
610.71219867434,611.581945297822,612.451691920754,612.886565232011,613.321438543126,
613.756311854099,614.191185164928,615.060931786153,615.931531098516,616.367257100486,
616.802130410586,617.237003720538,617.671877030342,618.106750339998,618.541623649505,
618.976496958863,619.411370268073,619.846243577134,620.281116886046,620.71599019481,
621.150863503426,621.585736811894,622.020610120214,622.455483428388,622.891209429248,
623.326935430108,623.761808737989,624.196682045726,624.631555353319,625.066428660769,
625.501301968075,625.936175275241,626.371048582266,626.805921889153,627.240795195901,
627.675668502512,628.110541808988,628.54541511533,628.98028842154,629.415161727618,
629.850887727438,630.286613727259,630.72148703308,631.156360338774,631.591233644344,
632.026106949791,632.460980255118,632.895853560325,633.330726865415,633.76560017039,
634.200473475251,634.635346780002,635.070220084644,635.505093389179,635.939966693609,
636.374839997937,636.810565996897,637.246291995857,637.681165299986,638.116038604021,
638.550911907962,638.985785211813,639.420658515576,639.855531819253,640.290405122847,
640.725278426361,641.160151729796,641.595025033157,642.029898336444,642.464771639662,
642.899644942813,643.334518245899,643.770244244257,644.205970242616,644.640843545581,
645.075716848491,645.510590151347,645.945463454153,646.380336756911,646.815210059625,
647.250083362296,647.684956664929,648.119829967526,648.55470327009,648.989576572624,
649.424449875131,649.859323177614,650.294196480076,650.729922478144,651.165648476212,
651.600521778641,652.035395081057,652.470268383465,652.905141685866,653.340014988265,
653.774888290663,654.209761593065,654.644634895472,655.079508197889,655.514381500318,
655.949254802762,656.384128105224,656.819001407706,657.253874710213,657.689600708326,
658.12532670644,658.560200009004,658.995073311601,659.429946614234,659.864819916905,
660.299693219619,660.734566522377,661.169439825183,661.604313128039,662.039186430948,
662.474059733914,662.908933036938,663.343806340025,663.778679643175,664.213552946393,
664.649278944883,665.085004943373,665.519878246733,665.954751550169,666.389624853683,
666.824498157277,667.259371460954,667.694244764717,668.129118068568,668.563991372509,
668.998864676544,669.433737980674,669.868611284901,670.303484589229,670.738357893659,
671.173231198194,671.608957197361,672.044683196528,672.479556501278,672.91442980614,
673.349303111115,673.784176416205,674.219049721412,674.653923026738,675.088796332185,
675.523669637755,675.95854294345,676.393416249271,676.82828955522,677.263162861298,
677.698036167508,678.13290947385,678.568635473934,679.004361474018,679.439234780629,
679.874108087377,680.308981394264,680.743854701289,681.178728008455,681.613601315762,
682.048474623211,682.483347930804,682.91822123854,683.353094546422,683.78796785445,
684.222841162623,684.657714470944,685.092587779412,685.528313780566,685.96403978172,
686.398913090483,686.833786399396,687.268659708457,687.703533017666,688.138406327025,
688.573279636532,689.008152946187,689.443026255992,689.877899565944,690.312772876043,
690.74764618629,691.182519496684,691.617392807224,692.052266117909,692.487992120169,
692.92371812243,693.358591433403,694.228338055774,694.663211367171,695.098084678707,
695.532957990379,695.967831302188,696.402704614131,696.837577926207,697.707324550749,
698.577071175797,699.011944488507,699.447670491767,699.883396495028,700.318269807975,
701.188016434211,702.057763060886,702.927509687976,703.797256315454,704.667002943295,
705.536749571467,706.407348889651,707.277948207973,708.147694836835,709.017441465911,
709.887188095163,710.756934724548,711.626681354026,712.496427983551,713.367027302543,
714.237626621516,715.107373250954,715.977119880277,716.846866509446,717.716613138419,
718.586359767161,719.456106395635,720.32670571363,721.197305031464,722.067051659126,
722.936798286414,723.806544913299,724.676291539758,725.546038165767,726.415784791305,
727.286384106969,728.156983422381,729.026730046663,729.896476670415,730.331349982088,
730.766223293624,731.201096605021,731.635969916278,732.505716538366,733.37546315988,
733.81033647042,734.246062472462,734.681788474505,735.116661784752,735.551535094852,
735.986408404804,736.421281714608,736.856155024264,737.291028333771,737.72590164313,
738.160774952339,738.5956482614,739.030521570312,739.465394879076,739.900268187692,
740.33514149616,740.77001480448,741.205740805414,741.641466806347,742.076340114374,
742.511213422256,742.946086729993,743.380960037585,743.815833345035,744.250706652341,
744.685579959507,745.120453266533,745.555326573419,745.990199880167,746.425073186778,
746.859946493254,747.294819799596,747.729693105806,748.165419105691,748.601145105576,
749.036018411525,749.470891717346,749.90576502304,750.34063832861,750.775511634057,
751.210384939384,751.645258244591,752.080131549682,752.515004854656,752.949878159518,
753.384751464269,753.81962476891,754.254498073445,754.689371377875,755.125097376885,
755.560823375895,755.995696680123,756.430569984253,756.865443288287,757.300316592228,
757.735189896079,758.170063199842,758.604936503519,759.039809807113,759.474683110627,
759.909556414062,760.344429717423,760.779303020711,761.214176323929,761.649049627079,
762.084775625469,762.520501623858,762.955374926883,763.390248229848,763.825121532758,
764.259994835614,764.694868138419,765.129741441178,765.564614743891,765.999488046563,
766.434361349196,766.869234651793,767.304107954357,767.738981256891,768.173854559398,
768.608727861881,769.044453859958,769.480179858035,769.915053160479,770.349926462907,
770.784799765324,771.219673067731,771.654546370133,772.089419672531,772.52429297493,
772.959166277331,773.394039579739,773.828912882155,774.263786184584,774.698659487028,
775.13353278949,775.568406091973,776.004132090072,776.439858088172,776.874731390706,
777.30960469327,777.744477995867,778.1793512985,778.614224601171,779.049097903885,
779.483971206643,779.918844509449,780.353717812305,780.788591115215,781.22346441818,
781.658337721205,782.093211024291,782.528084327442,782.963810325897,783.399536324352,
783.834409627639,784.269282931,784.704156234435,785.139029537949,785.573902841543,
786.00877614522,786.443649448983,786.878522752834,787.313396056775,787.74826936081,
788.183142664939,788.618015969167,789.052889273495,789.487762577925,789.923488577038,
790.359214576152,790.794087880793,791.228961185544,791.663834490406,792.098707795381,
792.533581100471,792.968454405678,793.403327711004,793.838201016451,794.273074322021,
794.707947627716,795.142820933537,795.577694239486,796.012567545564,796.447440851774,
796.883166851791,797.318892851808,797.753766158284,798.188639464895,798.623512771643,
799.058386078529,799.493259385555,799.92813269272,800.363006000027,800.797879307477,
801.232752615069,801.667625922806,802.102499230688,802.537372538715,802.972245846889,
803.40711915521,803.84284515629,804.27857115737,804.713444465985,805.148317774749,
805.583191083662,806.018064392723,806.452937701933,806.887811011291,807.322684320798,
808.192430940258,808.62730425021,809.06217756031,809.497050870557,809.931924180951,
810.36679749149,810.802523493679,811.238249495867,811.673122806697,812.542869428785,
812.977742740041,813.412616051438,813.847489362974,814.282362674646,814.717235986455,
815.152109298398,816.021855922681,816.891602547478,817.326475860065,817.762201863265,
818.197927866466,818.632801179295,819.502547805304,820.372294431763,821.242041058648,
822.111787685935,822.981534313598,823.851280941609,824.721880259681,825.5924795779,
826.462226206642,827.331972835616,828.201719464785,829.071466094109,829.941212723546,
830.810959353053,831.681558672047,832.552157991036,833.421904620514,834.2916512499,
835.161397879151,836.031144508226,836.900891137089,837.770637765701,838.641237083811,
839.511836401767,840.381583029608,841.251329657086,842.121076284176,842.990822910851,
843.860569537087,844.730316162863,845.600915478712,846.471514794314,847.341261418855,
848.211008042874,848.645881354683,849.080754666356,849.515627977891,849.950501289288,
850.82024791166,851.689994533462,852.124867844147,852.560593846263,852.996319848379,
853.431193158772,853.866066469019,854.300939779119,855.170686398875,855.605559708531,
856.040433018038,856.475306327397,856.910179636606,857.345052945667,857.77992625458,
858.214799563344,858.64967287196,859.084546180427,859.520272181434,859.95599818244,
860.390871490614,860.825744798641,861.260618106523,861.69549141426,862.130364721852,
862.565238029302,863.000111336609,863.434984643774,863.8698579508,864.304731257686,
864.739604564434,865.174477871045,865.609351177521,866.044224483863,866.479950483814,
866.915676483765,867.350549789843,867.785423095792,868.220296401613,868.655169707307,
869.090043012877,869.524916318325,869.959789623651,870.394662928858,870.829536233948,
871.264409538923,871.699282843785,872.134156148535,872.569029453177,873.003902757712,
873.439628756773,873.875354755834,874.310228060162,874.745101364389,875.179974668519,
875.614847972553,876.049721276495,876.484594580346,876.919467884108,877.354341187786,
877.78921449138,878.224087794893,878.658961098329,879.093834401689,879.528707704977,
879.963581008195,880.399307006616,880.835033005038,881.269906308124,881.704779611148,
882.139652914114,882.574526217024,883.00939951988,883.444272822685,883.879146125444,
884.314019428157,884.748892730829,885.183766033462,885.618639336059,886.053512638623,
886.488385941157,886.923259243664,887.358985241751,887.794711239839,888.2295845423,
888.664457844744,889.099331147173,889.534204449589,889.969077751997,890.403951054398,
890.838824356797,891.273697659195,891.708570961597,892.143444264004,892.578317566421,
893.01319086885,893.448064171293,893.882937473755,894.318663471843,894.75438946993,
895.189262772437,895.624136074971,896.059009377535,896.493882680132,896.928755982765,
897.363629285437,897.798502588151,898.233375890909,898.668249193715,899.103122496571,
899.53799579948,899.972869102446,900.40774240547,900.842615708556,901.278341706978,
901.714067705399,902.148941008617,902.583814311905,903.018687615265,903.453560918701,
903.888434222214,904.323307525808,904.758180829485,905.193054133248,905.627927437099,
906.06280074104,906.497674045075,906.932547349205,907.367420653433,907.80229395776,
908.238019956821,908.673745955883,909.108619260417,909.543492565059,909.978365869809,
910.413239174671,910.848112479646,911.282985784736,911.717859089943,912.152732395269,
912.587605700716,913.022479006287,913.457352311981,913.892225617802,914.327098923751,
914.761972229829,915.19769822978,915.633424229731,916.068297536072,916.503170842548,
916.93804414916,917.372917455908,917.807790762794,918.24266406982,918.677537376985,
919.112410684292,919.547283991742,919.982157299334,920.417030607071,920.851903914953,
921.28677722298,921.721650531154,922.15737653216,922.593102533167,923.027975841635,
923.46284915025,923.897722459014,924.332595767926,924.767469076987,925.202342386197,
925.637215695556,926.072089005063,926.506962314719,926.941835624523,927.376708934475,
927.811582244575,928.246455554822,928.681328865215,929.117054867331,929.987654180132,
930.422527490961,930.857400801934,931.292274113049,931.727147424306,932.162020735703,
932.596894047238,933.46664067072,934.336387294739,934.771260606945,935.20613391928,
935.641007231742,936.076733234882,936.94733255073,937.817079176507,938.686825802743,
939.556572429418,940.426319056508,941.296065683986,942.165812311827,943.036411629783,
943.907010947893,944.776757576505,945.646504205367,946.516250834443,947.385997463694,
948.25574409308,949.125490722558,949.996090041546,950.86668936054,951.736435990048,
952.606182619485,953.475929248809,954.345675877978,955.215422506951,956.085169135693,
956.955768453912,957.826367771985,958.696114399995,959.565861027658,960.435607654946,
961.305354281831,962.175100908289,963.044847534298,963.915446850328,964.786046166116,
965.655792790913,966.525539415195,966.960412727138,967.395286038947,968.265032662155,
969.134779284809,969.569652595924,970.004525906897,970.439399217726,970.875125219914,
971.310851222103,971.745724532643,972.615471153283,973.485217773335,973.920091083139,
974.354964392795,974.789837702302,975.22471101166,975.65958432087,976.094457629931,
976.529330938844,976.964204247608,977.399077556223,977.834803557303,978.270529558383,
978.705402866704,979.140276174877,979.575149482905,980.010022790786,980.444896098523,
980.879769406116,981.314642713565,981.749516020872,982.184389328038,982.619262635063,
983.05413594195,983.489009248698,983.923882555309,984.358755861785,984.794481861802,
985.230207861819,985.665081168029,986.099954474107,986.534827780056,986.969701085877,
987.404574391571,987.839447697141,988.274321002589,988.709194307915,989.144067613122,
989.578940918212,990.013814223187,990.448687528048,990.883560832799,991.31843413744,
991.754160136554,992.189886135667,992.624759440097,993.059632744425,993.494506048653,
993.929379352783,994.364252656817,994.799125960758,995.233999264609,995.668872568372,
996.103745872049,996.538619175643,996.973492479157,997.408365782593,997.843239085953,
998.278112389241,998.713838387696,999.149564386151,999.584437689301,1000.01931099239,
1000.45418429541,1000.88905759838,1001.32393090129,1001.75880420414,1002.19367750695,
1002.62855080971,1003.06342411242,1003.49829741509,1003.93317071773,1004.36804402032,
1004.80291732289,1005.23779062542,1005.67351662352,1006.10924262162,1006.5441159241,
1006.97898922656,1007.41386252901,1007.84873583144,1008.28360913385,1008.71848243626,
1009.15335573866,1009.58822904106,1010.02310234346,1010.45797564586,1010.89284894827,
1011.32772225069,1011.76259555311,1012.19746885556,1012.63319485364,1013.06892085171,
1013.5037941542,1013.9386674567,1014.37354075924,1014.8084140618,1015.2432873644,
1015.67816066703,1016.1130339697,1016.54790727242,1016.98278057517,1017.41765387798,
1017.85252718084,1018.28740048375,1018.72227378671,1019.15714708974,1019.59287308813,
1020.02859908651,1020.46347238967,1020.89834569288,1021.33321899617,1021.76809229953,
1022.20296560297,1022.63783890648,1023.07271221007,1023.50758551375,1023.94245881752,
1024.37733212137,1024.81220542531,1025.24707872935,1025.68195203348,1026.11682533771,
1026.55255133672,1026.98827733573,1027.42315064016,1027.8580239447,1028.29289724934,
1028.72777055409,1029.16264385896,1029.59751716393,1030.03239046902,1030.46726377423,
1030.90213707956,1031.33701038501,1031.77188369058,1032.20675699628,1032.6416303021,
1033.07650360805,1033.51222960793,1033.94795560782,1034.38282891403,1034.81770222038,
1035.25257552685,1035.68744883347,1036.12232214022,1036.5571954471,1036.99206875413,
1037.4269420613,1037.86181536861,1038.29668867606,1038.73156198365,1039.16643529139,
1039.60130859927,1040.0361819073,1040.47190790824,1040.90763390917,1041.34250721749,
1041.77738052596,1042.21225383458,1042.64712714334,1043.08200045226,1043.95174707053,
1044.38662037989,1044.8214936894,1045.25636699906,1045.69124030886,1046.12611361882,
1046.56098692892,1046.99586023917,1047.43158624121,1047.86731224325,1048.3021855538,
1048.73705886448,1049.17193217531,1049.60680548629,1050.0416787974,1050.47655210866,
1050.91142542006,1051.78117204327,1052.21604535508,1052.65091866703,1053.0857919791,
1053.52066529131,1053.95553860365,1054.39126460673,1055.26186392239,1056.13161054793,
1057.00135717395,1057.43623048712,1057.87110380041,1058.7408504273,1059.61059705459,
1060.48034368225,1061.35094300009,1062.22154231809,1063.09128894656,1063.96103557531,
1064.83078220429,1065.70052883346,1066.57027546278,1067.44002209222,1068.3106214112,
1069.18122073019,1070.05096735972,1070.9207139892,1071.79046061859,1072.66020724785,
1073.52995387693,1074.39970050579,1075.27029982411,1076.1408991423,1077.01064577048,
1077.88039239832,1078.7501390258,1079.61988565289,1080.48963227957,1081.35937890581,
1082.22997822202,1083.100577538,1083.97032416305,1084.84007078759,1085.70981741161,
1086.5795640351,1087.44931065803,1087.88418396929,1088.31905728041,1088.75393059138,
1089.18965659365,1089.62538259591,1090.06025590659,1090.93000252753,1091.36487583778,
1091.79974914788,1092.23462245783,1092.66949576764,1093.1043690773,1093.5392423868,
1093.97411569616,1094.40898900538,1094.84386231444,1095.27873562335,1095.71360893212,
1096.14933493327,1096.58506093443,1097.0199342429,1097.45480755122,1097.88968085939,
1098.32455416742,1098.75942747531,1099.19430078305,1099.62917409064,1100.06404739809,
1100.4989207054,1100.93379401257,1101.36866731959,1101.80354062648,1102.23841393323,
1102.67328723984,1103.10901323993,1103.54473924001,1103.97961254636,1104.41448585257,
1104.84935915865,1105.2842324646,1105.71910577042,1106.15397907612,1106.58885238169,
1107.02372568714,1107.45859899246,1107.89347229767,1108.32834560276,1108.76321890774,
1109.1980922126,1109.63296551736,1110.06869151652,1110.50441751569,1110.93929082023,
1111.37416412466,1111.80903742899,1112.24391073322,1112.67878403735,1113.11365734139,
1113.54853064533,1113.98340394918,1114.41827725295,1114.85315055662,1115.28802386022,
1115.72289716374,1116.15777046717,1116.59264377053,1117.02836976903,1117.46409576752,
1117.89896907074,1118.33384237389,1118.76871567698,1119.20358898,1119.63846228297,
1120.07333558588,1120.50820888874,1120.94308219154,1121.3779554943,1121.81282879702,
1122.24770209969,1122.68257540233,1123.11744870492,1123.55232200749,1123.98804800561,
1124.42377400372,1124.85864730623,1125.29352060871,1125.72839391118,1126.16326721362,
1126.59814051605,1127.03301381847,1127.46788712088,1127.90276042328,1128.33763372568,
1128.77250702808,1129.20738033048,1129.64225363289,1130.07712693531,1130.51200023774,
1130.94772623581,1131.38345223388,1131.81832553634,1132.25319883883,1132.68807214134,
1133.12294544387,1133.55781874644,1133.99269204904,1134.42756535167,1134.86243865434,
1135.29731195706,1135.73218525982,1136.16705856263,1136.60193186548,1137.03680516839,
1137.47167847136,1137.90740446972,1138.34313046808,1138.77800377117,1139.21287707432,
1139.64775037754,1140.08262368083,1140.51749698419,1140.95237028763,1141.38724359114,
1141.82211689474,1142.25699019842,1142.69186350218,1143.12673680603,1143.56161010998,
1143.99648341401,1144.43135671814,1144.86708271711,1145.30280871607,1145.7376820204,
1146.17255532483,1146.60742862936,1147.04230193401,1147.47717523876,1147.91204854362,
1148.3469218486,1148.78179515369,1149.2166684589,1149.65154176423,1150.08641506968,
1150.52128837525,1150.95616168094,1151.39103498677,1151.82676098659,1152.26248698641,
1152.69736029249,1153.1322335987,1153.56710690504,1154.00198021152,1154.43685351813,
1154.87172682488,1155.30660013177,1155.7414734388,1156.17634674597,1156.61122005327,
1157.04609336073,1157.48096666832,1157.91583997606,1158.35071328394,1158.7864392848,
1159.22216528566,1159.65703859384,1160.09191190216,1160.52678521063,1160.96165851925,
1161.39653182801,1161.83140513693,1162.26627844599,1162.7011517552,1163.13602506456,
1163.57089837407,1164.00577168373,1164.44064499353,1164.87551830349,1165.74611761556,
1166.18184361753,1166.61671692792,1167.05159023846,1167.48646354915,1167.92133685998,
1168.35621017096,1169.22595679333,1170.09570341627,1170.53057672794,1170.96545003975,
1171.4003233517,1171.83519666377,1172.27006997598,1172.705795979,1173.57639529447,
1174.44614191977,1174.8810152326,1175.31588854555,1176.18563517179,1177.05538179847,
1177.92512842556,1178.79487505304,1179.66547437075,1180.53607368863,1181.40582031696,
1182.27556694557,1183.14531357444,1184.01506020352,1184.88480683277,1185.75455346216,
1186.62515278112,1187.4957521001,1188.36549872963,1189.23524535914,1190.10499198858,
1190.97473861791,1191.84448524708,1192.71423187606,1193.58483119448,1194.45543051277,
1195.3251771411,1196.19492376911,1197.06467039678,1197.93441702407,1198.80416365096,
1199.67391027742,1200.5445095938,1201.41510890996,1202.28485553525,1203.15460216005,
1204.02434878434,1204.89409540809,1205.76384203131,1206.1987153427,1206.63358865396,
1207.06846196508,1207.50418796741,1208.37478728058,1209.2445339018,1209.6794072122,
1210.11428052245,1210.54915383255,1210.9840271425,1211.41890045231,1211.85377376197,
1212.28864707147,1212.72352038083,1213.15839369005,1213.59326699911,1214.02814030802,
1214.46386630925,1214.89959231048,1215.3344656191,1215.76933892757,1216.20421223589,
1216.63908554406,1217.07395885209,1217.50883215998,1217.94370546771,1218.37857877531,
1218.81345208276,1219.24832539007,1219.68319869724,1220.11807200426,1220.55294531115,
1220.9878186179,1221.42354461805,1221.85927061821,1222.29414392468,1222.72901723103,
1223.16389053724,1223.59876384332,1224.03363714927,1224.46851045509,1224.90338376079,
1225.33825706636,1225.77313037181,1226.20800367713,1226.64287698234,1227.07775028743,
1227.51262359241,1227.94749689727,1228.3832228965,1228.81894889572,1229.25382220036,
1229.6886955049,1230.12356880933,1230.55844211366,1230.99331541789,1231.42818872202,
1231.86306202606,1232.29793533,1232.73280863385,1233.16768193762,1233.60255524129,
1234.03742854489,1234.4723018484,1234.90717515184,1235.34290115037,1235.7786271489,
1236.21350045219,1236.64837375541,1237.08324705856,1237.51812036165,1237.95299366467,
1238.38786696764,1238.82274027055,1239.25761357341,1239.69248687621,1240.12736017897,
1240.56223348169,1240.99710678436,1241.431980087,1241.8668533896,1242.30257938773,
1242.73830538585,1243.17317868839,1243.6080519909,1244.04292529338,1244.47779859585,
1244.91267189829,1245.34754520072,1245.78241850314,1246.21729180555,1246.65216510795,
1247.08703841035,1247.52191171275,1247.95678501515,1248.39165831756,1248.82653161998,
1249.26225761804,1249.69798361611,1250.13285691855,1250.56773022101,1251.0026035235,
1251.43747682601,1251.87235012854,1252.30722343111,1252.74209673371,1253.17697003634,
1253.61184333901,1254.04671664173,1254.48158994449,1254.9164632473,1255.35133655015,
1255.78620985306,1256.22193585139,1256.65766184973,1257.09253515275,1257.52740845584,
1257.96228175899,1258.39715506221,1258.8320283655,1259.26690166886,1259.7017749723,
1260.13664827581,1260.57152157941,1261.00639488309,1261.44126818685,1261.8761414907,
1262.31101479465,1262.74588809868,1263.1816140976,1263.61734009651,1264.05221340074,
1264.48708670507,1264.9219600095,1265.35683331403,1265.79170661868,1266.22657992343,
1266.66145322829,1267.09632653327,1267.53119983836,1267.96607314357,1268.4009464489,
1268.83581975434,1269.27069305992,1269.70556636561,1270.14129236537,1270.57701836513,
1271.01189167108,1271.44676497716,1271.88163828337,1272.31651158971,1272.75138489619,
1273.1862582028,1273.62113150955,1274.05600481644,1274.49087812347,1274.92575143063,
1275.36062473794,1275.79549804539,1276.23037135299,1276.66524466073,1277.10097066151,
1277.5366966623,1277.97156997033,1278.40644327851,1278.84131658683,1279.2761898953,
1279.71106320392,1280.14593651268,1280.5808098216,1281.01568313066,1281.45055643987,
1281.88542974923,1282.32030305874,1282.75517636839,1283.1900496782,1283.62492298815,
1284.06064899005,1284.49637499195,1284.9312483022,1285.36612161259,1285.80099492313,
1286.23586823382,1286.67074154465,1287.54048816674,1287.975361478,1288.4102347894,
1288.84510810093,1289.27998141261,1289.71485472442,1290.14972803636,1291.02032735139,
1291.89092666668,1292.32579997914,1292.76067329173,1293.19554660444,1293.63041991727,
1294.50016654328,1295.36991316974,1296.23965979663,1297.10940642392,1297.9800057415,
1298.85060505925,1299.72035168742,1300.5900983159,1301.45984494464,1302.32959157362,
1303.19933820279,1304.06908483212,1304.93968415104,1305.81028347,1306.68003009953,
1307.54977672906,1308.41952335854,1309.28926998793,1310.15901661718,1311.02876324626,
1311.89936256477,1312.76996188316,1313.63970851164,1314.50945513981,1315.37920176765,
1316.24894839514,1317.11869502223,1317.98844164891,1318.85904096546,1319.72964028179,
1320.59938690733,1321.46913353238,1322.33888015692,1323.20862678095,1323.64350009276,
1324.07837340443,1324.51324671597,1324.94812002737,1325.81871934103,1326.68931865441,
1327.12419196524,1327.55906527593,1327.99393858647,1328.42881189686,1328.86368520711,
1329.29855851721,1329.73343182716,1330.16830513697,1330.60317844663,1331.03805175614,
1331.4729250655,1331.90779837471,1332.34267168377,1332.77839768507,1333.21412368638,
1333.64899699514,1334.08387030376,1334.51874361223,1334.95361692055,1335.38849022873,
1335.82336353676,1336.25823684464,1336.69311015238,1337.12798345997,1337.56285676742,
1337.99773007473,1338.4326033819,1338.86747668892,1339.30234999581,1339.73807599603,
1340.17380199625,1340.60867530287,1341.04354860934,1341.47842191569,1341.9132952219,
1342.34816852798,1342.78304183393,1343.21791513975,1343.65278844545,1344.08766175102,
1344.52253505647,1344.95740836179,1345.392281667,1345.82715497209,1346.26202827707,
1346.69775427635,1347.13348027563,1347.56835358038,1348.00322688502,1348.43810018956,
1348.87297349399,1349.30784679832,1349.74272010255,1350.17759340668,1350.61246671072,
1351.04734001466,1351.48221331851,1351.91708662228,1352.35195992595,1352.78683322955,
1353.22170653306,1353.65743253163,1354.09315853019,1354.52803183356,1354.96290513685,
1355.39777844007,1355.83265174322,1356.26752504631,1356.70239834933,1357.1372716523,
1357.57214495521,1358.00701825807,1358.44189156087,1358.87676486363,1359.31163816635,
1359.74651146902,1360.18138477166,1360.6171107698,1361.05283676795,1361.48771007051,
1361.92258337305,1362.35745667556,1362.79232997804,1363.2272032805,1363.66207658295,
1364.09694988538,1364.5318231878,1364.96669649021,1365.40156979261,1365.83644309501,
1366.27131639741,1366.70618969981,1367.14106300222,1367.57678900028,1368.01251499834,
1368.44738830077,1368.88226160321,1369.31713490567,1369.75200820816,1370.18688151067,
1370.6217548132,1371.05662811577,1371.49150141837,1371.926374721,1372.36124802367,
1372.79612132639,1373.23099462915,1373.66586793196,1374.10074123481,1374.53646723311,
1374.97219323142,1375.40706653438,1375.84193983741,1376.2768131405,1376.71168644365,
1377.14655974687,1377.58143305016,1378.01630635352,1378.45117965696,1378.88605296047,
1379.32092626407,1379.75579956775,1380.19067287151,1380.62554617536,1381.06041947931,
1381.49614547817,1381.93187147704,1382.36674478117,1382.8016180854,1383.23649138973,
1383.67136469416,1384.10623799869,1384.54111130334,1384.97598460809,1385.41085791295,
1385.84573121793,1386.28060452302,1386.71547782823,1387.15035113356,1387.585224439,
1388.02009774458,1388.45582374427,1388.89154974397,1389.32642304979,1389.76129635574,
1390.19616966182,1390.63104296803,1391.06591627437,1391.50078958085,1391.93566288746,
1392.37053619421,1392.8054095011,1393.24028280813,1393.6751561153,1394.1100294226,
1394.54490273005,1394.97977603765,1395.41550203836,1395.85122803908,1396.28610134696,
1396.72097465499,1397.15584796317,1397.59072127149,1398.02559457996,1398.46046788858,
1398.89534119734,1399.33021450626,1399.76508781532,1400.19996112453,1400.63483443389,
1401.50458105306,1401.93945436286,1402.37518036469,1402.81090636651,1403.24577967661,
1403.68065298686,1404.11552629725,1404.5503996078,1404.98527291848,1405.85501954029,
1406.2898928514,1406.72476616266,1407.15963947406,1407.5945127856,1408.02938609727,
1408.46425940908,1409.33485872391,1410.205458039,1410.64033135134,1411.07520466381,
1411.51007797639,1411.9449512891,1412.81469791488,1413.68444454112,1414.5541911678,
1415.42393779489,1416.29453711233,1417.16513642995,1418.03488305796,1418.90462968629,
1419.77437631491,1420.64412294377,1421.51386957285,1422.38361620211,1423.25421552099,
1424.12481483992,1424.99456146943,1425.86430809896,1426.73405472847,1427.60380135791,
1428.47354798724,1429.34329461641,1430.21389393501,1431.08449325349,1431.9542398821,
1432.82398651043,1433.69373313844,1434.56347976611,1435.4332263934,1436.30297302029,
1437.17357233701,1438.04417165351,1438.91391827929,1439.78366490459,1440.65341152939,
1441.52315815367,1441.95803146562,1442.39290477743,1442.8277780891,1443.26265140064,
1444.13325071451,1445.00385002811,1445.43872333908,1445.87359664991,1446.3084699606,
1446.74334327114,1447.17821658153,1447.61308989178,1448.48283651184,1448.91770982164,
1449.3525831313,1449.78745644081,1450.22232975017,1450.65720305938,1451.09292906076,
1451.52865506214,1451.96352837105,1452.39840167982,1452.83327498843,1453.2681482969,
1453.70302160522,1454.1378949134,1454.57276822143,1455.00764152931,1455.44251483705,
1455.87738814464,1456.31226145209,1456.7471347594,1457.18200806657,1457.6168813736,
1458.05260737389,1458.48833337418,1458.92320668093,1459.35807998754,1459.79295329402,
1460.22782660036,1460.66269990657,1461.09757321265,1461.5324465186,1461.96731982443,
1462.40219313012,1462.83706643569,1463.27193974114,1463.70681304647,1464.14168635168,
1464.57655965677,1465.0122856561,1465.44801165544,1465.8828849603,1466.31775826505,
1466.7526315697,1467.18750487423,1467.62237817866,1468.05725148299,1468.49212478722,
1468.92699809135,1469.36187139539,1469.79674469933,1470.23161800319,1470.66649130695,
1471.10136461063,1471.53623791422,1471.97196391283,1472.40768991143,1472.84256321487,
1473.27743651823,1473.71230982152,1474.14718312474,1474.58205642789,1475.01692973098,
1475.451803034,1475.88667633697,1476.32154963988,1476.75642294274,1477.19129624555,
1477.62616954831,1478.06104285102,1478.4959161537,1478.93164215186,1479.36736815002,
1479.80224145262,1480.23711475519,1480.67198805772,1481.10686136023,1481.54173466272,
1481.97660796518,1482.41148126762,1482.84635457005,1483.28122787247,1483.71610117488,
1484.15097447728,1484.58584777968,1485.02072108208,1485.45559438449,1485.89132038254,
1486.32704638059,1486.76191968301,1487.19679298544,1487.63166628788,1488.06653959035,
1488.50141289283,1488.93628619534,1489.37115949787,1489.80603280044,1490.24090610304,
1490.67577940567,1491.11065270835,1491.54552601106,1491.98039931382,1492.41527261663,
1492.8509986149,1493.28672461318,1493.72159791609,1494.15647121906,1494.59134452208,
1495.02621782517,1495.46109112832,1495.89596443154,1496.33083773483,1496.76571103819,
1497.20058434163,1497.63545764515,1498.07033094874,1498.50520425242,1498.94007755618,
1499.37495086004,1499.81067685885,1500.24640285767,1500.68127616171,1501.11614946584,
1501.55102277007,1501.9858960744,1502.42076937883,1502.85564268337,1503.29051598801,
1503.72538929276,1504.16026259762,1504.5951359026,1505.03000920769,1505.4648825129,
1505.89975581823,1506.33462912368,1506.77035512331,1507.20608112294,1507.64095442864,
1508.07582773446,1508.51070104041,1508.94557434649,1509.3804476527,1509.81532095904,
1510.25019426552,1510.68506757213,1511.11994087888,1511.55481418577,1511.9896874928,
1512.42456079996,1512.85943410727,1513.29430741472,1513.73003341537,1514.16575941601,
1514.60063272375,1515.03550603163,1515.47037933966,1515.90525264784,1516.34012595616,
1516.77499926463,1517.20987257325,1517.64474588201,1518.07961919093,1518.51449249999,
1518.9493658092,1519.38423911856,1519.81911242807,1520.25398573772,1520.68971173947,
1521.12543774122,1521.56031105118,1521.99518436128,1522.43005767153,1523.29980429246,
1523.73467760315,1524.16955091398,1524.60442422495,1525.03929753607,1525.47417084733,
1525.90904415873,1526.77879078194,1527.64939009657,1528.08511609939,1528.51998941146,
1528.95486272367,1529.38973603601,1530.25948266106,1531.1292292866,1531.99897591261,
1532.86872253907,1533.73846916596,1534.60906848325,1535.47966780073,1536.34941442858,
1537.21916105675,1538.08890768523,1538.95865431398,1539.82840094295,1540.69814757212,
1541.56874689096,1542.43934620985,1543.30909283933,1544.17883946886,1545.04858609839,
1545.91833272787,1546.78807935726,1547.65782598651,1548.52842530518,1549.39902462375,
1550.26877125249,1551.13851788097,1552.00826450914,1552.87801113699,1553.74775776447,
1554.61750439156,1555.48810370844,1556.35870302511,1557.22844965112,1558.09819627666,
1558.96794290171,1559.83768952626,1560.27256283834,1560.70743615028,1561.57718277377,
1562.44778208785,1563.31838140165,1563.75325471277,1564.18812802374,1564.62300133457,
1565.05787464526,1565.9276212662,1566.79736788655,1567.2322411965,1567.66711450631,
1568.10198781596,1568.53686112547,1568.97173443483,1569.40746043628,1569.84318643774,
1570.2780597468,1570.71293305571,1571.14780636448,1571.5826796731,1572.01755298157,
1572.45242628989,1572.88729959806,1573.32217290609,1573.75704621397,1574.19191952171,
1574.62679282931,1575.06166613676,1575.49653944407,1575.93141275123,1576.36713875159,
1576.80286475195,1577.23773805884,1577.67261136559,1578.1074846722,1578.54235797868,
1578.97723128502,1579.41210459124,1579.84697789732,1580.28185120327,1580.71672450909,
1581.15159781478,1581.58647112036,1582.0213444258,1582.45621773113,1582.89109103634,
1583.32681703573,1583.76254303513,1584.1974163401,1584.63228964497,1585.06716294972,
1585.50203625436,1585.9369095589,1586.37178286333,1586.80665616766,1587.24152947189,
1587.67640277602,1588.11127608005,1588.546149384,1588.98102268785,1589.41589599161,
1589.85076929529,1590.28649529394,1590.72222129258,1591.1570945961,1591.59196789953,
1592.0268412029,1592.46171450619,1592.8965878094,1593.33146111256,1593.76633441564,
1594.20120771867,1594.63608102164,1595.07095432455,1595.50582762741,1595.94070093021,
1596.37557423297,1596.81044753569,1597.24617353387,1597.68189953206,1598.11677283469,
1598.55164613729,1598.98651943985,1599.42139274239,1599.8562660449,1600.29113934738,
1600.72601264985,1601.16088595229,1601.59575925472,1602.03063255714,1602.46550585955,
1602.90037916195,1603.33525246435,1603.77012576675,1604.2058517648,1604.64157776285,
1605.07645106526,1605.51132436768,1605.94619767011,1606.38107097255,1606.81594427502,
1607.2508175775,1607.68569088001,1608.12056418254,1608.55543748511,1608.99031078771,
1609.42518409034,1609.86005739302,1610.29493069573,1610.72980399849,1611.16552999674,
1611.60125599499,1612.03612929785,1612.47100260076,1612.90587590373,1613.34074920675,
1613.77562250984,1614.21049581299,1614.64536911621,1615.0802424195,1615.51511572286,
1615.9499890263,1616.38486232981,1616.81973563341,1617.25460893709,1617.68948224085,
1618.12520823963,1618.5609342384,1618.99580754234,1619.43068084638,1619.86555415051,
1620.30042745474,1620.73530075907,1621.1701740635,1621.60504736804,1622.03992067268,
1622.47479397743,1622.90966728229,1623.34454058727,1623.77941389236,1624.21428719757,
1624.6491605029,1625.08488650247,1625.52061250204,1625.95548580761,1626.39035911331,
1626.82523241913,1627.26010572508,1627.69497903116,1628.12985233737,1628.56472564372,
1628.99959895019,1629.43447225681,1629.86934556356,1630.30421887044,1630.73909217747,
1631.17396548464,1631.60883879195,1632.04456479252,1632.48029079309,1632.91516410068,
1633.35003740842,1633.78491071631,1634.21978402433,1634.65465733251,1635.08953064083,
1635.5244039493,1635.95927725792,1636.39415056668,1636.8290238756,1637.26389718466,
1637.69877049387,1638.13364380323,1638.56851711274,1639.00424311442,1639.43996911609,
1639.8748424259,1640.30971573585,1640.74458904595,1641.6143356666,1642.04920897714,
1642.48408228782,1642.91895559865,1643.35382890963,1643.78870222074,1644.223575532,
1645.09332215494,1645.52819546661,1645.96392146936,1646.39964747212,1646.83452078406,
1647.26939409614,1647.70426740834,1648.57401403314,1649.44376065844,1650.31350728422,
1650.74838059729,1651.18325391046,1652.05300053714,1652.92359985428,1653.79419917162,
1654.66394579929,1655.5336924273,1656.40343905563,1657.27318568424,1658.14293231311,
1659.01267894219,1659.88327826096,1660.75387757982,1661.62362420926,1662.49337083877,
1663.3631174683,1664.23286409781,1665.10261072725,1665.97235735658,1666.84295667531,
1667.71355599396,1668.58330262282,1669.45304925143,1670.32279587976,1671.19254250778,
1672.06228913544,1672.93203576273,1673.80263507977,1674.6732343966,1675.54298102284,
1676.41272764862,1677.28247427392,1678.15222089872,1679.021967523,1679.89171414676,
1680.76231346105,1681.19803946366,1681.63291277506,1682.06778608632,1682.50265939743,
1682.93753270841,1683.37240601924,1684.24215264047,1684.67702595086,1685.11189926111,
1685.54677257121,1685.98164588116,1686.41651919097,1686.85139250063,1687.28626581014,
1687.72199181166,1688.15771781319,1688.5925911224,1689.02746443146,1689.46233774038,
1689.89721104914,1690.33208435776,1690.76695766623,1691.20183097455,1691.63670428272,
1692.07157759075,1692.50645089864,1692.94132420637,1693.37619751397,1693.81107082142,
1694.24594412873,1694.68167012916,1695.11739612959,1695.55226943662,1695.9871427435,
1696.42201605025,1696.85688935687,1697.29176266334,1697.72663596969,1698.1615092759,
1698.59638258198,1699.03125588793,1699.46612919375,1699.90100249945,1700.33587580502,
1700.77074911047,1701.20562241579,1701.64134841525,1702.0770744147,1702.51194771979,
1702.94682102476,1703.38169432963,1703.81656763438,1704.25144093902,1704.68631424356,
1705.12118754799,1705.55606085232,1705.99093415655,1706.42580746068,1706.86068076471,
1707.29555406866,1707.73042737251,1708.16530067627,1708.60102667496,1709.03675267365,
1709.47162597724,1709.90649928076,1710.34137258419,1710.77624588756,1711.21111919085,
1711.64599249406,1712.08086579722,1712.5157391003,1712.95061240333,1713.3854857063,
1713.82035900921,1714.25523231207,1714.69010561487,1715.12497891763,1715.56070491584,
1715.99643091404,1716.43130421671,1716.86617751935,1717.30105082195,1717.73592412451,
1718.17079742705,1718.60567072956,1719.04054403204,1719.4754173345,1719.91029063695,
1720.34516393938,1720.7800372418,1721.21491054421,1721.64978384661,1722.08465714901,
1722.52038314706,1722.9561091451,1723.39098244751,1723.82585574992,1724.26072905233,
1724.69560235476,1725.13047565721,1725.56534895967,1726.00022226216,1726.43509556467,
1726.8699688672,1727.30484216977,1727.73971547236,1728.174588775,1728.60946207767,
1729.04433538039,1729.48006137861,1729.91578737684,1730.35066067965,1730.78553398251,
1731.22040728542,1731.65528058838,1732.09015389141,1732.5250271945,1732.95990049765,
1733.39477380087,1733.82964710416,1734.26452040752,1734.69939371096,1735.13426701447,
1735.56914031807,1736.00401362175,1736.43973962048,1736.8754656192,1737.31033892306,
1737.745212227,1738.18008553104,1738.61495883517,1739.0498321394,1739.48470544373,
1739.91957874816,1740.35445205269,1740.78932535734,1741.22419866209,1741.65907196695,
1742.09394527193,1742.52881857702,1742.96369188223,1743.39941788174,1743.83514388125,
1744.2700171867,1744.70489049227,1745.13976379797,1745.57463710379,1746.00951040974,
1746.44438371582,1746.87925702203,1747.31413032837,1747.74900363485,1748.18387694146,
1748.61875024821,1749.0536235551,1749.48849686213,1749.92337016929,1750.3590961698,
1750.7948221703,1751.22969547775,1751.66456878534,1752.09944209308,1752.53431540096,
1752.96918870899,1753.40406201717,1753.83893532549,1754.27380863396,1754.70868194258,
1755.14355525134,1755.57842856026,1756.01330186932,1756.44817517853,1756.88304848789,
1757.31877448949,1757.75450049109,1758.18937380075,1759.05912042051,1759.49399373061,
1759.92886704086,1760.36374035125,1760.79861366179,1761.23348697248,1761.66836028331,
1762.10323359429,1762.5381069054,1763.40785352806,1763.8427268396,1764.27845284228,
1764.71417884496,1765.14905215677,1765.58392546872,1766.0187987808,1766.88854540534,
1767.75829203039,1768.1931653431,1768.62803865593,1769.06291196888,1769.49778528195,
1770.36753190841,1771.2381312254,1772.10873054259,1772.97847717007,1773.84822379791,
1774.71797042609,1775.58771705456,1776.45746368331,1777.32721031228,1778.19780963089,
1779.06840894783,1779.93815555508,1780.80790201176,1781.67764871408),(-1.76619037896906,
-1.18309518948453),.UNSPECIFIED.) ;
#821 = B_SPLINE_SURFACE_WITH_KNOTS('',3,1,((#34258,#34259),(#34260,#34261),
(#34262,#34263),(#34264,#34265),(#34266,#34267),(#34268,#34269),(#34270,
#34271),(#34272,#34273),(#34274,#34275),(#34276,#34277),(#34278,#34279),
(#34280,#34281),(#34282,#34283),(#34284,#34285),(#34286,#34287),(#34288,
#34289),(#34290,#34291),(#34292,#34293),(#34294,#34295),(#34296,#34297),
(#34298,#34299),(#34300,#34301),(#34302,#34303),(#34304,#34305),(#34306,
#34307),(#34308,#34309),(#34310,#34311),(#34312,#34313),(#34314,#34315),
(#34316,#34317),(#34318,#34319),(#34320,#34321),(#34322,#34323),(#34324,
#34325),(#34326,#34327),(#34328,#34329),(#34330,#34331),(#34332,#34333),
(#34334,#34335),(#34336,#34337),(#34338,#34339),(#34340,#34341),(#34342,
#34343),(#34344,#34345),(#34346,#34347),(#34348,#34349),(#34350,#34351),
(#34352,#34353),(#34354,#34355),(#34356,#34357),(#34358,#34359),(#34360,
#34361),(#34362,#34363),(#34364,#34365),(#34366,#34367),(#34368,#34369),
(#34370,#34371),(#34372,#34373),(#34374,#34375),(#34376,#34377),(#34378,
#34379),(#34380,#34381),(#34382,#34383),(#34384,#34385),(#34386,#34387),
(#34388,#34389),(#34390,#34391),(#34392,#34393),(#34394,#34395),(#34396,
#34397),(#34398,#34399),(#34400,#34401),(#34402,#34403),(#34404,#34405),
(#34406,#34407),(#34408,#34409),(#34410,#34411),(#34412,#34413),(#34414,
#34415),(#34416,#34417),(#34418,#34419),(#34420,#34421),(#34422,#34423),
(#34424,#34425),(#34426,#34427),(#34428,#34429),(#34430,#34431),(#34432,
#34433),(#34434,#34435),(#34436,#34437),(#34438,#34439),(#34440,#34441),
(#34442,#34443),(#34444,#34445),(#34446,#34447),(#34448,#34449),(#34450,
#34451),(#34452,#34453),(#34454,#34455),(#34456,#34457),(#34458,#34459),
(#34460,#34461),(#34462,#34463),(#34464,#34465),(#34466,#34467),(#34468,
#34469),(#34470,#34471),(#34472,#34473),(#34474,#34475),(#34476,#34477),
(#34478,#34479),(#34480,#34481),(#34482,#34483),(#34484,#34485),(#34486,
#34487),(#34488,#34489),(#34490,#34491),(#34492,#34493),(#34494,#34495),
(#34496,#34497),(#34498,#34499),(#34500,#34501),(#34502,#34503),(#34504,
#34505),(#34506,#34507),(#34508,#34509),(#34510,#34511),(#34512,#34513),
(#34514,#34515),(#34516,#34517),(#34518,#34519),(#34520,#34521),(#34522,
#34523),(#34524,#34525),(#34526,#34527),(#34528,#34529),(#34530,#34531),
(#34532,#34533),(#34534,#34535),(#34536,#34537),(#34538,#34539),(#34540,
#34541),(#34542,#34543),(#34544,#34545),(#34546,#34547),(#34548,#34549),
(#34550,#34551),(#34552,#34553),(#34554,#34555),(#34556,#34557),(#34558,
#34559),(#34560,#34561),(#34562,#34563),(#34564,#34565),(#34566,#34567),
(#34568,#34569),(#34570,#34571),(#34572,#34573),(#34574,#34575),(#34576,
#34577),(#34578,#34579),(#34580,#34581),(#34582,#34583),(#34584,#34585),
(#34586,#34587),(#34588,#34589),(#34590,#34591),(#34592,#34593),(#34594,
#34595),(#34596,#34597),(#34598,#34599),(#34600,#34601),(#34602,#34603),
(#34604,#34605),(#34606,#34607),(#34608,#34609),(#34610,#34611),(#34612,
#34613),(#34614,#34615),(#34616,#34617),(#34618,#34619),(#34620,#34621),
(#34622,#34623),(#34624,#34625),(#34626,#34627),(#34628,#34629),(#34630,
#34631),(#34632,#34633),(#34634,#34635),(#34636,#34637),(#34638,#34639),
(#34640,#34641),(#34642,#34643),(#34644,#34645),(#34646,#34647),(#34648,
#34649),(#34650,#34651),(#34652,#34653),(#34654,#34655),(#34656,#34657),
(#34658,#34659),(#34660,#34661),(#34662,#34663),(#34664,#34665),(#34666,
#34667),(#34668,#34669),(#34670,#34671),(#34672,#34673),(#34674,#34675),
(#34676,#34677),(#34678,#34679),(#34680,#34681),(#34682,#34683),(#34684,
#34685),(#34686,#34687),(#34688,#34689),(#34690,#34691),(#34692,#34693),
(#34694,#34695),(#34696,#34697),(#34698,#34699),(#34700,#34701),(#34702,
#34703),(#34704,#34705),(#34706,#34707),(#34708,#34709),(#34710,#34711),
(#34712,#34713),(#34714,#34715),(#34716,#34717),(#34718,#34719),(#34720,
#34721),(#34722,#34723),(#34724,#34725),(#34726,#34727),(#34728,#34729),
(#34730,#34731),(#34732,#34733),(#34734,#34735),(#34736,#34737),(#34738,
#34739),(#34740,#34741),(#34742,#34743),(#34744,#34745),(#34746,#34747),
(#34748,#34749),(#34750,#34751),(#34752,#34753),(#34754,#34755),(#34756,
#34757),(#34758,#34759),(#34760,#34761),(#34762,#34763),(#34764,#34765),
(#34766,#34767),(#34768,#34769),(#34770,#34771),(#34772,#34773),(#34774,
#34775),(#34776,#34777),(#34778,#34779),(#34780,#34781),(#34782,#34783),
(#34784,#34785),(#34786,#34787),(#34788,#34789),(#34790,#34791),(#34792,
#34793),(#34794,#34795),(#34796,#34797),(#34798,#34799),(#34800,#34801),
(#34802,#34803),(#34804,#34805),(#34806,#34807),(#34808,#34809),(#34810,
#34811),(#34812,#34813),(#34814,#34815),(#34816,#34817),(#34818,#34819),
(#34820,#34821),(#34822,#34823),(#34824,#34825),(#34826,#34827),(#34828,
#34829),(#34830,#34831),(#34832,#34833),(#34834,#34835),(#34836,#34837),
(#34838,#34839),(#34840,#34841),(#34842,#34843),(#34844,#34845),(#34846,
#34847),(#34848,#34849),(#34850,#34851),(#34852,#34853),(#34854,#34855),
(#34856,#34857),(#34858,#34859),(#34860,#34861),(#34862,#34863),(#34864,
#34865),(#34866,#34867),(#34868,#34869),(#34870,#34871),(#34872,#34873),
(#34874,#34875),(#34876,#34877),(#34878,#34879),(#34880,#34881),(#34882,
#34883),(#34884,#34885),(#34886,#34887),(#34888,#34889),(#34890,#34891),
(#34892,#34893),(#34894,#34895),(#34896,#34897),(#34898,#34899),(#34900,
#34901),(#34902,#34903),(#34904,#34905),(#34906,#34907),(#34908,#34909),
(#34910,#34911),(#34912,#34913),(#34914,#34915),(#34916,#34917),(#34918,
#34919),(#34920,#34921),(#34922,#34923),(#34924,#34925),(#34926,#34927),
(#34928,#34929),(#34930,#34931),(#34932,#34933),(#34934,#34935),(#34936,
#34937),(#34938,#34939),(#34940,#34941),(#34942,#34943),(#34944,#34945),
(#34946,#34947),(#34948,#34949),(#34950,#34951),(#34952,#34953),(#34954,
#34955),(#34956,#34957),(#34958,#34959),(#34960,#34961),(#34962,#34963),
(#34964,#34965),(#34966,#34967),(#34968,#34969),(#34970,#34971),(#34972,
#34973),(#34974,#34975),(#34976,#34977),(#34978,#34979),(#34980,#34981),
(#34982,#34983),(#34984,#34985),(#34986,#34987),(#34988,#34989),(#34990,
#34991),(#34992,#34993),(#34994,#34995),(#34996,#34997),(#34998,#34999),
(#35000,#35001),(#35002,#35003),(#35004,#35005),(#35006,#35007),(#35008,
#35009),(#35010,#35011),(#35012,#35013),(#35014,#35015),(#35016,#35017),
(#35018,#35019),(#35020,#35021),(#35022,#35023),(#35024,#35025),(#35026,
#35027),(#35028,#35029),(#35030,#35031),(#35032,#35033),(#35034,#35035),
(#35036,#35037),(#35038,#35039),(#35040,#35041),(#35042,#35043),(#35044,
#35045),(#35046,#35047),(#35048,#35049),(#35050,#35051),(#35052,#35053),
(#35054,#35055),(#35056,#35057),(#35058,#35059),(#35060,#35061),(#35062,
#35063),(#35064,#35065),(#35066,#35067),(#35068,#35069),(#35070,#35071),
(#35072,#35073),(#35074,#35075),(#35076,#35077),(#35078,#35079),(#35080,
#35081),(#35082,#35083),(#35084,#35085),(#35086,#35087),(#35088,#35089),
(#35090,#35091),(#35092,#35093),(#35094,#35095),(#35096,#35097),(#35098,
#35099),(#35100,#35101),(#35102,#35103),(#35104,#35105),(#35106,#35107),
(#35108,#35109),(#35110,#35111),(#35112,#35113),(#35114,#35115),(#35116,
#35117),(#35118,#35119),(#35120,#35121),(#35122,#35123),(#35124,#35125),
(#35126,#35127),(#35128,#35129),(#35130,#35131),(#35132,#35133),(#35134,
#35135),(#35136,#35137),(#35138,#35139),(#35140,#35141),(#35142,#35143),
(#35144,#35145),(#35146,#35147),(#35148,#35149),(#35150,#35151),(#35152,
#35153),(#35154,#35155),(#35156,#35157),(#35158,#35159),(#35160,#35161),
(#35162,#35163),(#35164,#35165),(#35166,#35167),(#35168,#35169),(#35170,
#35171),(#35172,#35173),(#35174,#35175),(#35176,#35177),(#35178,#35179),
(#35180,#35181),(#35182,#35183),(#35184,#35185),(#35186,#35187),(#35188,
#35189),(#35190,#35191),(#35192,#35193),(#35194,#35195),(#35196,#35197),
(#35198,#35199),(#35200,#35201),(#35202,#35203),(#35204,#35205),(#35206,
#35207),(#35208,#35209),(#35210,#35211),(#35212,#35213),(#35214,#35215),
(#35216,#35217),(#35218,#35219),(#35220,#35221),(#35222,#35223),(#35224,
#35225),(#35226,#35227),(#35228,#35229),(#35230,#35231),(#35232,#35233),
(#35234,#35235),(#35236,#35237),(#35238,#35239),(#35240,#35241),(#35242,
#35243),(#35244,#35245),(#35246,#35247),(#35248,#35249),(#35250,#35251),
(#35252,#35253),(#35254,#35255),(#35256,#35257),(#35258,#35259),(#35260,
#35261),(#35262,#35263),(#35264,#35265),(#35266,#35267),(#35268,#35269),
(#35270,#35271),(#35272,#35273),(#35274,#35275),(#35276,#35277),(#35278,
#35279),(#35280,#35281),(#35282,#35283),(#35284,#35285),(#35286,#35287),
(#35288,#35289),(#35290,#35291),(#35292,#35293),(#35294,#35295),(#35296,
#35297),(#35298,#35299),(#35300,#35301),(#35302,#35303),(#35304,#35305),
(#35306,#35307),(#35308,#35309),(#35310,#35311),(#35312,#35313),(#35314,
#35315),(#35316,#35317),(#35318,#35319),(#35320,#35321),(#35322,#35323),
(#35324,#35325),(#35326,#35327),(#35328,#35329),(#35330,#35331),(#35332,
#35333),(#35334,#35335),(#35336,#35337),(#35338,#35339),(#35340,#35341),
(#35342,#35343),(#35344,#35345),(#35346,#35347),(#35348,#35349),(#35350,
#35351),(#35352,#35353),(#35354,#35355),(#35356,#35357),(#35358,#35359),
(#35360,#35361),(#35362,#35363),(#35364,#35365),(#35366,#35367),(#35368,
#35369),(#35370,#35371),(#35372,#35373),(#35374,#35375),(#35376,#35377),
(#35378,#35379),(#35380,#35381),(#35382,#35383),(#35384,#35385),(#35386,
#35387),(#35388,#35389),(#35390,#35391),(#35392,#35393),(#35394,#35395),
(#35396,#35397),(#35398,#35399),(#35400,#35401),(#35402,#35403),(#35404,
#35405),(#35406,#35407),(#35408,#35409),(#35410,#35411),(#35412,#35413),
(#35414,#35415),(#35416,#35417),(#35418,#35419),(#35420,#35421),(#35422,
#35423),(#35424,#35425),(#35426,#35427),(#35428,#35429),(#35430,#35431),
(#35432,#35433),(#35434,#35435),(#35436,#35437),(#35438,#35439),(#35440,
#35441),(#35442,#35443),(#35444,#35445),(#35446,#35447),(#35448,#35449),
(#35450,#35451),(#35452,#35453),(#35454,#35455),(#35456,#35457),(#35458,
#35459),(#35460,#35461),(#35462,#35463),(#35464,#35465),(#35466,#35467),
(#35468,#35469),(#35470,#35471),(#35472,#35473),(#35474,#35475),(#35476,
#35477),(#35478,#35479),(#35480,#35481),(#35482,#35483),(#35484,#35485),
(#35486,#35487),(#35488,#35489),(#35490,#35491),(#35492,#35493),(#35494,
#35495),(#35496,#35497),(#35498,#35499),(#35500,#35501),(#35502,#35503),
(#35504,#35505),(#35506,#35507),(#35508,#35509),(#35510,#35511),(#35512,
#35513),(#35514,#35515),(#35516,#35517),(#35518,#35519),(#35520,#35521),
(#35522,#35523),(#35524,#35525),(#35526,#35527),(#35528,#35529),(#35530,
#35531),(#35532,#35533),(#35534,#35535),(#35536,#35537),(#35538,#35539),
(#35540,#35541),(#35542,#35543),(#35544,#35545),(#35546,#35547),(#35548,
#35549),(#35550,#35551),(#35552,#35553),(#35554,#35555),(#35556,#35557),
(#35558,#35559),(#35560,#35561),(#35562,#35563),(#35564,#35565),(#35566,
#35567),(#35568,#35569),(#35570,#35571),(#35572,#35573),(#35574,#35575),
(#35576,#35577),(#35578,#35579),(#35580,#35581),(#35582,#35583),(#35584,
#35585),(#35586,#35587),(#35588,#35589),(#35590,#35591),(#35592,#35593),
(#35594,#35595),(#35596,#35597),(#35598,#35599),(#35600,#35601),(#35602,
#35603),(#35604,#35605),(#35606,#35607),(#35608,#35609),(#35610,#35611),
(#35612,#35613),(#35614,#35615),(#35616,#35617),(#35618,#35619),(#35620,
#35621),(#35622,#35623),(#35624,#35625),(#35626,#35627),(#35628,#35629),
(#35630,#35631),(#35632,#35633),(#35634,#35635),(#35636,#35637),(#35638,
#35639),(#35640,#35641),(#35642,#35643),(#35644,#35645),(#35646,#35647),
(#35648,#35649),(#35650,#35651),(#35652,#35653),(#35654,#35655),(#35656,
#35657),(#35658,#35659),(#35660,#35661),(#35662,#35663),(#35664,#35665),
(#35666,#35667),(#35668,#35669),(#35670,#35671),(#35672,#35673),(#35674,
#35675),(#35676,#35677),(#35678,#35679),(#35680,#35681),(#35682,#35683),
(#35684,#35685),(#35686,#35687),(#35688,#35689),(#35690,#35691),(#35692,
#35693),(#35694,#35695),(#35696,#35697),(#35698,#35699),(#35700,#35701),
(#35702,#35703),(#35704,#35705),(#35706,#35707),(#35708,#35709),(#35710,
#35711),(#35712,#35713),(#35714,#35715),(#35716,#35717),(#35718,#35719),
(#35720,#35721),(#35722,#35723),(#35724,#35725),(#35726,#35727),(#35728,
#35729),(#35730,#35731),(#35732,#35733),(#35734,#35735),(#35736,#35737),
(#35738,#35739),(#35740,#35741),(#35742,#35743),(#35744,#35745),(#35746,
#35747),(#35748,#35749),(#35750,#35751),(#35752,#35753),(#35754,#35755),
(#35756,#35757),(#35758,#35759),(#35760,#35761),(#35762,#35763),(#35764,
#35765),(#35766,#35767),(#35768,#35769),(#35770,#35771),(#35772,#35773),
(#35774,#35775),(#35776,#35777),(#35778,#35779),(#35780,#35781),(#35782,
#35783),(#35784,#35785),(#35786,#35787),(#35788,#35789),(#35790,#35791),
(#35792,#35793),(#35794,#35795),(#35796,#35797),(#35798,#35799),(#35800,
#35801),(#35802,#35803),(#35804,#35805),(#35806,#35807),(#35808,#35809),
(#35810,#35811),(#35812,#35813),(#35814,#35815),(#35816,#35817),(#35818,
#35819),(#35820,#35821),(#35822,#35823),(#35824,#35825),(#35826,#35827),
(#35828,#35829),(#35830,#35831),(#35832,#35833),(#35834,#35835),(#35836,
#35837),(#35838,#35839),(#35840,#35841),(#35842,#35843),(#35844,#35845),
(#35846,#35847),(#35848,#35849),(#35850,#35851),(#35852,#35853),(#35854,
#35855),(#35856,#35857),(#35858,#35859),(#35860,#35861),(#35862,#35863),
(#35864,#35865),(#35866,#35867),(#35868,#35869),(#35870,#35871),(#35872,
#35873),(#35874,#35875),(#35876,#35877),(#35878,#35879),(#35880,#35881),
(#35882,#35883),(#35884,#35885),(#35886,#35887),(#35888,#35889),(#35890,
#35891),(#35892,#35893),(#35894,#35895),(#35896,#35897),(#35898,#35899),
(#35900,#35901),(#35902,#35903),(#35904,#35905),(#35906,#35907),(#35908,
#35909),(#35910,#35911),(#35912,#35913),(#35914,#35915),(#35916,#35917),
(#35918,#35919),(#35920,#35921),(#35922,#35923),(#35924,#35925),(#35926,
#35927),(#35928,#35929),(#35930,#35931),(#35932,#35933),(#35934,#35935),
(#35936,#35937),(#35938,#35939),(#35940,#35941),(#35942,#35943),(#35944,
#35945),(#35946,#35947),(#35948,#35949),(#35950,#35951),(#35952,#35953),
(#35954,#35955),(#35956,#35957),(#35958,#35959),(#35960,#35961),(#35962,
#35963),(#35964,#35965),(#35966,#35967),(#35968,#35969),(#35970,#35971),
(#35972,#35973),(#35974,#35975),(#35976,#35977),(#35978,#35979),(#35980,
#35981),(#35982,#35983),(#35984,#35985),(#35986,#35987),(#35988,#35989),
(#35990,#35991),(#35992,#35993),(#35994,#35995),(#35996,#35997),(#35998,
#35999),(#36000,#36001),(#36002,#36003),(#36004,#36005),(#36006,#36007),
(#36008,#36009),(#36010,#36011),(#36012,#36013),(#36014,#36015),(#36016,
#36017),(#36018,#36019),(#36020,#36021),(#36022,#36023),(#36024,#36025),
(#36026,#36027),(#36028,#36029),(#36030,#36031),(#36032,#36033),(#36034,
#36035),(#36036,#36037),(#36038,#36039),(#36040,#36041),(#36042,#36043),
(#36044,#36045),(#36046,#36047),(#36048,#36049),(#36050,#36051),(#36052,
#36053),(#36054,#36055),(#36056,#36057),(#36058,#36059),(#36060,#36061),
(#36062,#36063),(#36064,#36065),(#36066,#36067),(#36068,#36069),(#36070,
#36071),(#36072,#36073),(#36074,#36075),(#36076,#36077),(#36078,#36079),
(#36080,#36081),(#36082,#36083),(#36084,#36085),(#36086,#36087),(#36088,
#36089),(#36090,#36091),(#36092,#36093),(#36094,#36095),(#36096,#36097),
(#36098,#36099),(#36100,#36101),(#36102,#36103),(#36104,#36105),(#36106,
#36107),(#36108,#36109),(#36110,#36111),(#36112,#36113),(#36114,#36115),
(#36116,#36117),(#36118,#36119),(#36120,#36121),(#36122,#36123),(#36124,
#36125),(#36126,#36127),(#36128,#36129),(#36130,#36131),(#36132,#36133),
(#36134,#36135),(#36136,#36137),(#36138,#36139),(#36140,#36141),(#36142,
#36143),(#36144,#36145),(#36146,#36147),(#36148,#36149),(#36150,#36151),
(#36152,#36153),(#36154,#36155),(#36156,#36157),(#36158,#36159),(#36160,
#36161),(#36162,#36163),(#36164,#36165),(#36166,#36167),(#36168,#36169),
(#36170,#36171),(#36172,#36173),(#36174,#36175),(#36176,#36177),(#36178,
#36179),(#36180,#36181),(#36182,#36183),(#36184,#36185),(#36186,#36187),
(#36188,#36189),(#36190,#36191),(#36192,#36193),(#36194,#36195),(#36196,
#36197),(#36198,#36199),(#36200,#36201),(#36202,#36203),(#36204,#36205),
(#36206,#36207),(#36208,#36209),(#36210,#36211),(#36212,#36213),(#36214,
#36215),(#36216,#36217),(#36218,#36219),(#36220,#36221),(#36222,#36223),
(#36224,#36225),(#36226,#36227),(#36228,#36229),(#36230,#36231),(#36232,
#36233),(#36234,#36235),(#36236,#36237),(#36238,#36239),(#36240,#36241),
(#36242,#36243),(#36244,#36245),(#36246,#36247),(#36248,#36249),(#36250,
#36251),(#36252,#36253),(#36254,#36255),(#36256,#36257),(#36258,#36259),
(#36260,#36261),(#36262,#36263),(#36264,#36265),(#36266,#36267),(#36268,
#36269),(#36270,#36271),(#36272,#36273),(#36274,#36275),(#36276,#36277),
(#36278,#36279),(#36280,#36281),(#36282,#36283),(#36284,#36285),(#36286,
#36287),(#36288,#36289),(#36290,#36291),(#36292,#36293),(#36294,#36295),
(#36296,#36297),(#36298,#36299),(#36300,#36301),(#36302,#36303),(#36304,
#36305),(#36306,#36307),(#36308,#36309),(#36310,#36311),(#36312,#36313),
(#36314,#36315),(#36316,#36317),(#36318,#36319),(#36320,#36321),(#36322,
#36323),(#36324,#36325),(#36326,#36327),(#36328,#36329),(#36330,#36331),
(#36332,#36333),(#36334,#36335),(#36336,#36337),(#36338,#36339),(#36340,
#36341),(#36342,#36343),(#36344,#36345),(#36346,#36347),(#36348,#36349),
(#36350,#36351),(#36352,#36353),(#36354,#36355),(#36356,#36357),(#36358,
#36359),(#36360,#36361),(#36362,#36363),(#36364,#36365),(#36366,#36367),
(#36368,#36369),(#36370,#36371),(#36372,#36373),(#36374,#36375),(#36376,
#36377),(#36378,#36379),(#36380,#36381),(#36382,#36383),(#36384,#36385),
(#36386,#36387),(#36388,#36389),(#36390,#36391),(#36392,#36393),(#36394,
#36395),(#36396,#36397),(#36398,#36399),(#36400,#36401),(#36402,#36403),
(#36404,#36405),(#36406,#36407),(#36408,#36409),(#36410,#36411),(#36412,
#36413),(#36414,#36415),(#36416,#36417),(#36418,#36419),(#36420,#36421),
(#36422,#36423),(#36424,#36425),(#36426,#36427),(#36428,#36429),(#36430,
#36431),(#36432,#36433),(#36434,#36435),(#36436,#36437),(#36438,#36439),
(#36440,#36441),(#36442,#36443),(#36444,#36445),(#36446,#36447),(#36448,
#36449),(#36450,#36451),(#36452,#36453),(#36454,#36455),(#36456,#36457),
(#36458,#36459),(#36460,#36461),(#36462,#36463),(#36464,#36465),(#36466,
#36467),(#36468,#36469),(#36470,#36471),(#36472,#36473),(#36474,#36475),
(#36476,#36477),(#36478,#36479),(#36480,#36481),(#36482,#36483),(#36484,
#36485),(#36486,#36487),(#36488,#36489),(#36490,#36491),(#36492,#36493),
(#36494,#36495),(#36496,#36497),(#36498,#36499),(#36500,#36501),(#36502,
#36503),(#36504,#36505),(#36506,#36507),(#36508,#36509),(#36510,#36511),
(#36512,#36513),(#36514,#36515),(#36516,#36517),(#36518,#36519),(#36520,
#36521),(#36522,#36523),(#36524,#36525),(#36526,#36527),(#36528,#36529),
(#36530,#36531),(#36532,#36533),(#36534,#36535),(#36536,#36537),(#36538,
#36539),(#36540,#36541),(#36542,#36543),(#36544,#36545),(#36546,#36547),
(#36548,#36549),(#36550,#36551),(#36552,#36553),(#36554,#36555),(#36556,
#36557),(#36558,#36559),(#36560,#36561),(#36562,#36563),(#36564,#36565),
(#36566,#36567),(#36568,#36569),(#36570,#36571),(#36572,#36573),(#36574,
#36575),(#36576,#36577),(#36578,#36579),(#36580,#36581),(#36582,#36583),
(#36584,#36585),(#36586,#36587),(#36588,#36589),(#36590,#36591),(#36592,
#36593),(#36594,#36595),(#36596,#36597),(#36598,#36599),(#36600,#36601),
(#36602,#36603),(#36604,#36605),(#36606,#36607),(#36608,#36609),(#36610,
#36611),(#36612,#36613),(#36614,#36615),(#36616,#36617),(#36618,#36619),
(#36620,#36621),(#36622,#36623),(#36624,#36625),(#36626,#36627),(#36628,
#36629),(#36630,#36631),(#36632,#36633),(#36634,#36635),(#36636,#36637),
(#36638,#36639),(#36640,#36641),(#36642,#36643),(#36644,#36645),(#36646,
#36647),(#36648,#36649),(#36650,#36651),(#36652,#36653),(#36654,#36655),
(#36656,#36657),(#36658,#36659),(#36660,#36661),(#36662,#36663),(#36664,
#36665),(#36666,#36667),(#36668,#36669),(#36670,#36671),(#36672,#36673),
(#36674,#36675),(#36676,#36677),(#36678,#36679),(#36680,#36681),(#36682,
#36683),(#36684,#36685),(#36686,#36687),(#36688,#36689),(#36690,#36691),
(#36692,#36693),(#36694,#36695),(#36696,#36697),(#36698,#36699),(#36700,
#36701),(#36702,#36703),(#36704,#36705),(#36706,#36707),(#36708,#36709),
(#36710,#36711),(#36712,#36713),(#36714,#36715),(#36716,#36717),(#36718,
#36719),(#36720,#36721),(#36722,#36723),(#36724,#36725),(#36726,#36727),
(#36728,#36729),(#36730,#36731),(#36732,#36733),(#36734,#36735),(#36736,
#36737),(#36738,#36739),(#36740,#36741),(#36742,#36743),(#36744,#36745),
(#36746,#36747),(#36748,#36749),(#36750,#36751),(#36752,#36753),(#36754,
#36755),(#36756,#36757),(#36758,#36759),(#36760,#36761),(#36762,#36763),
(#36764,#36765),(#36766,#36767),(#36768,#36769),(#36770,#36771),(#36772,
#36773),(#36774,#36775),(#36776,#36777),(#36778,#36779),(#36780,#36781),
(#36782,#36783),(#36784,#36785),(#36786,#36787),(#36788,#36789),(#36790,
#36791),(#36792,#36793),(#36794,#36795),(#36796,#36797),(#36798,#36799),
(#36800,#36801),(#36802,#36803),(#36804,#36805),(#36806,#36807),(#36808,
#36809),(#36810,#36811),(#36812,#36813),(#36814,#36815),(#36816,#36817),
(#36818,#36819),(#36820,#36821),(#36822,#36823),(#36824,#36825),(#36826,
#36827),(#36828,#36829),(#36830,#36831),(#36832,#36833),(#36834,#36835),
(#36836,#36837),(#36838,#36839),(#36840,#36841),(#36842,#36843),(#36844,
#36845),(#36846,#36847),(#36848,#36849),(#36850,#36851),(#36852,#36853),
(#36854,#36855),(#36856,#36857),(#36858,#36859),(#36860,#36861),(#36862,
#36863),(#36864,#36865),(#36866,#36867),(#36868,#36869),(#36870,#36871),
(#36872,#36873),(#36874,#36875),(#36876,#36877),(#36878,#36879),(#36880,
#36881),(#36882,#36883),(#36884,#36885),(#36886,#36887),(#36888,#36889),
(#36890,#36891),(#36892,#36893),(#36894,#36895),(#36896,#36897),(#36898,
#36899),(#36900,#36901),(#36902,#36903),(#36904,#36905),(#36906,#36907),
(#36908,#36909),(#36910,#36911),(#36912,#36913),(#36914,#36915),(#36916,
#36917),(#36918,#36919),(#36920,#36921),(#36922,#36923),(#36924,#36925),
(#36926,#36927),(#36928,#36929),(#36930,#36931),(#36932,#36933),(#36934,
#36935),(#36936,#36937),(#36938,#36939),(#36940,#36941),(#36942,#36943),
(#36944,#36945),(#36946,#36947),(#36948,#36949),(#36950,#36951),(#36952,
#36953),(#36954,#36955),(#36956,#36957),(#36958,#36959),(#36960,#36961),
(#36962,#36963),(#36964,#36965),(#36966,#36967),(#36968,#36969),(#36970,
#36971),(#36972,#36973),(#36974,#36975),(#36976,#36977),(#36978,#36979),
(#36980,#36981),(#36982,#36983),(#36984,#36985),(#36986,#36987),(#36988,
#36989),(#36990,#36991),(#36992,#36993),(#36994,#36995),(#36996,#36997),
(#36998,#36999),(#37000,#37001),(#37002,#37003),(#37004,#37005),(#37006,
#37007),(#37008,#37009),(#37010,#37011),(#37012,#37013),(#37014,#37015),
(#37016,#37017),(#37018,#37019),(#37020,#37021),(#37022,#37023),(#37024,
#37025),(#37026,#37027),(#37028,#37029),(#37030,#37031),(#37032,#37033),
(#37034,#37035),(#37036,#37037),(#37038,#37039),(#37040,#37041),(#37042,
#37043),(#37044,#37045),(#37046,#37047),(#37048,#37049),(#37050,#37051),
(#37052,#37053),(#37054,#37055),(#37056,#37057),(#37058,#37059),(#37060,
#37061),(#37062,#37063),(#37064,#37065),(#37066,#37067),(#37068,#37069),
(#37070,#37071),(#37072,#37073),(#37074,#37075),(#37076,#37077),(#37078,
#37079),(#37080,#37081),(#37082,#37083),(#37084,#37085),(#37086,#37087),
(#37088,#37089),(#37090,#37091),(#37092,#37093),(#37094,#37095),(#37096,
#37097),(#37098,#37099),(#37100,#37101),(#37102,#37103),(#37104,#37105),
(#37106,#37107),(#37108,#37109),(#37110,#37111),(#37112,#37113),(#37114,
#37115),(#37116,#37117),(#37118,#37119),(#37120,#37121),(#37122,#37123),
(#37124,#37125),(#37126,#37127),(#37128,#37129),(#37130,#37131),(#37132,
#37133),(#37134,#37135),(#37136,#37137),(#37138,#37139),(#37140,#37141),
(#37142,#37143),(#37144,#37145),(#37146,#37147),(#37148,#37149),(#37150,
#37151),(#37152,#37153),(#37154,#37155),(#37156,#37157),(#37158,#37159),
(#37160,#37161),(#37162,#37163),(#37164,#37165),(#37166,#37167),(#37168,
#37169),(#37170,#37171),(#37172,#37173),(#37174,#37175),(#37176,#37177),
(#37178,#37179),(#37180,#37181),(#37182,#37183),(#37184,#37185),(#37186,
#37187),(#37188,#37189),(#37190,#37191),(#37192,#37193),(#37194,#37195),
(#37196,#37197),(#37198,#37199),(#37200,#37201),(#37202,#37203),(#37204,
#37205),(#37206,#37207),(#37208,#37209),(#37210,#37211),(#37212,#37213),
(#37214,#37215),(#37216,#37217),(#37218,#37219),(#37220,#37221),(#37222,
#37223),(#37224,#37225),(#37226,#37227),(#37228,#37229),(#37230,#37231),
(#37232,#37233),(#37234,#37235),(#37236,#37237),(#37238,#37239),(#37240,
#37241),(#37242,#37243),(#37244,#37245),(#37246,#37247),(#37248,#37249),
(#37250,#37251),(#37252,#37253),(#37254,#37255),(#37256,#37257),(#37258,
#37259),(#37260,#37261),(#37262,#37263),(#37264,#37265),(#37266,#37267),
(#37268,#37269),(#37270,#37271),(#37272,#37273),(#37274,#37275),(#37276,
#37277),(#37278,#37279),(#37280,#37281),(#37282,#37283),(#37284,#37285),
(#37286,#37287),(#37288,#37289),(#37290,#37291),(#37292,#37293),(#37294,
#37295),(#37296,#37297),(#37298,#37299),(#37300,#37301),(#37302,#37303),
(#37304,#37305),(#37306,#37307),(#37308,#37309),(#37310,#37311),(#37312,
#37313),(#37314,#37315),(#37316,#37317),(#37318,#37319),(#37320,#37321),
(#37322,#37323),(#37324,#37325),(#37326,#37327),(#37328,#37329),(#37330,
#37331),(#37332,#37333),(#37334,#37335),(#37336,#37337),(#37338,#37339),
(#37340,#37341),(#37342,#37343),(#37344,#37345),(#37346,#37347),(#37348,
#37349),(#37350,#37351),(#37352,#37353),(#37354,#37355),(#37356,#37357),
(#37358,#37359),(#37360,#37361),(#37362,#37363),(#37364,#37365),(#37366,
#37367),(#37368,#37369),(#37370,#37371),(#37372,#37373),(#37374,#37375),
(#37376,#37377),(#37378,#37379),(#37380,#37381),(#37382,#37383),(#37384,
#37385),(#37386,#37387),(#37388,#37389),(#37390,#37391),(#37392,#37393),
(#37394,#37395),(#37396,#37397),(#37398,#37399),(#37400,#37401),(#37402,
#37403),(#37404,#37405),(#37406,#37407),(#37408,#37409),(#37410,#37411),
(#37412,#37413),(#37414,#37415),(#37416,#37417),(#37418,#37419),(#37420,
#37421),(#37422,#37423),(#37424,#37425),(#37426,#37427),(#37428,#37429),
(#37430,#37431),(#37432,#37433),(#37434,#37435),(#37436,#37437),(#37438,
#37439),(#37440,#37441),(#37442,#37443),(#37444,#37445),(#37446,#37447),
(#37448,#37449),(#37450,#37451),(#37452,#37453),(#37454,#37455),(#37456,
#37457),(#37458,#37459),(#37460,#37461),(#37462,#37463),(#37464,#37465),
(#37466,#37467),(#37468,#37469),(#37470,#37471),(#37472,#37473),(#37474,
#37475),(#37476,#37477),(#37478,#37479),(#37480,#37481),(#37482,#37483),
(#37484,#37485),(#37486,#37487),(#37488,#37489),(#37490,#37491),(#37492,
#37493),(#37494,#37495),(#37496,#37497),(#37498,#37499),(#37500,#37501),
(#37502,#37503),(#37504,#37505),(#37506,#37507),(#37508,#37509),(#37510,
#37511),(#37512,#37513),(#37514,#37515),(#37516,#37517),(#37518,#37519),
(#37520,#37521),(#37522,#37523),(#37524,#37525),(#37526,#37527),(#37528,
#37529),(#37530,#37531),(#37532,#37533),(#37534,#37535),(#37536,#37537),
(#37538,#37539),(#37540,#37541),(#37542,#37543),(#37544,#37545),(#37546,
#37547),(#37548,#37549),(#37550,#37551),(#37552,#37553),(#37554,#37555),
(#37556,#37557),(#37558,#37559),(#37560,#37561),(#37562,#37563),(#37564,
#37565),(#37566,#37567),(#37568,#37569),(#37570,#37571),(#37572,#37573),
(#37574,#37575),(#37576,#37577),(#37578,#37579),(#37580,#37581),(#37582,
#37583),(#37584,#37585),(#37586,#37587),(#37588,#37589),(#37590,#37591),
(#37592,#37593),(#37594,#37595),(#37596,#37597),(#37598,#37599),(#37600,
#37601),(#37602,#37603),(#37604,#37605),(#37606,#37607),(#37608,#37609),
(#37610,#37611),(#37612,#37613),(#37614,#37615),(#37616,#37617),(#37618,
#37619),(#37620,#37621),(#37622,#37623),(#37624,#37625),(#37626,#37627),
(#37628,#37629),(#37630,#37631),(#37632,#37633),(#37634,#37635),(#37636,
#37637),(#37638,#37639),(#37640,#37641),(#37642,#37643),(#37644,#37645),
(#37646,#37647),(#37648,#37649),(#37650,#37651),(#37652,#37653),(#37654,
#37655),(#37656,#37657),(#37658,#37659),(#37660,#37661),(#37662,#37663),
(#37664,#37665),(#37666,#37667),(#37668,#37669),(#37670,#37671),(#37672,
#37673),(#37674,#37675),(#37676,#37677),(#37678,#37679),(#37680,#37681),
(#37682,#37683),(#37684,#37685),(#37686,#37687),(#37688,#37689),(#37690,
#37691),(#37692,#37693),(#37694,#37695),(#37696,#37697),(#37698,#37699),
(#37700,#37701),(#37702,#37703),(#37704,#37705),(#37706,#37707),(#37708,
#37709),(#37710,#37711),(#37712,#37713),(#37714,#37715),(#37716,#37717),
(#37718,#37719),(#37720,#37721),(#37722,#37723),(#37724,#37725),(#37726,
#37727),(#37728,#37729),(#37730,#37731),(#37732,#37733),(#37734,#37735),
(#37736,#37737),(#37738,#37739),(#37740,#37741),(#37742,#37743),(#37744,
#37745),(#37746,#37747),(#37748,#37749),(#37750,#37751),(#37752,#37753),
(#37754,#37755),(#37756,#37757),(#37758,#37759),(#37760,#37761),(#37762,
#37763),(#37764,#37765),(#37766,#37767),(#37768,#37769),(#37770,#37771),
(#37772,#37773),(#37774,#37775),(#37776,#37777),(#37778,#37779),(#37780,
#37781),(#37782,#37783),(#37784,#37785),(#37786,#37787),(#37788,#37789),
(#37790,#37791),(#37792,#37793),(#37794,#37795),(#37796,#37797),(#37798,
#37799),(#37800,#37801),(#37802,#37803),(#37804,#37805),(#37806,#37807),
(#37808,#37809),(#37810,#37811),(#37812,#37813),(#37814,#37815),(#37816,
#37817),(#37818,#37819),(#37820,#37821),(#37822,#37823),(#37824,#37825),
(#37826,#37827),(#37828,#37829),(#37830,#37831),(#37832,#37833),(#37834,
#37835),(#37836,#37837),(#37838,#37839),(#37840,#37841),(#37842,#37843),
(#37844,#37845),(#37846,#37847),(#37848,#37849),(#37850,#37851),(#37852,
#37853),(#37854,#37855),(#37856,#37857),(#37858,#37859),(#37860,#37861),
(#37862,#37863),(#37864,#37865),(#37866,#37867),(#37868,#37869),(#37870,
#37871),(#37872,#37873),(#37874,#37875),(#37876,#37877),(#37878,#37879),
(#37880,#37881),(#37882,#37883),(#37884,#37885),(#37886,#37887),(#37888,
#37889),(#37890,#37891),(#37892,#37893),(#37894,#37895),(#37896,#37897),
(#37898,#37899),(#37900,#37901),(#37902,#37903),(#37904,#37905),(#37906,
#37907),(#37908,#37909),(#37910,#37911),(#37912,#37913),(#37914,#37915),
(#37916,#37917),(#37918,#37919),(#37920,#37921),(#37922,#37923),(#37924,
#37925),(#37926,#37927),(#37928,#37929),(#37930,#37931),(#37932,#37933),
(#37934,#37935),(#37936,#37937),(#37938,#37939),(#37940,#37941),(#37942,
#37943),(#37944,#37945),(#37946,#37947),(#37948,#37949),(#37950,#37951),
(#37952,#37953),(#37954,#37955),(#37956,#37957),(#37958,#37959),(#37960,
#37961),(#37962,#37963),(#37964,#37965),(#37966,#37967),(#37968,#37969),
(#37970,#37971),(#37972,#37973),(#37974,#37975),(#37976,#37977),(#37978,
#37979),(#37980,#37981),(#37982,#37983),(#37984,#37985),(#37986,#37987),
(#37988,#37989),(#37990,#37991),(#37992,#37993),(#37994,#37995),(#37996,
#37997),(#37998,#37999),(#38000,#38001),(#38002,#38003),(#38004,#38005),
(#38006,#38007),(#38008,#38009),(#38010,#38011),(#38012,#38013),(#38014,
#38015),(#38016,#38017),(#38018,#38019),(#38020,#38021),(#38022,#38023),
(#38024,#38025),(#38026,#38027),(#38028,#38029),(#38030,#38031),(#38032,
#38033),(#38034,#38035),(#38036,#38037),(#38038,#38039),(#38040,#38041),
(#38042,#38043),(#38044,#38045),(#38046,#38047),(#38048,#38049),(#38050,
#38051),(#38052,#38053),(#38054,#38055),(#38056,#38057),(#38058,#38059),
(#38060,#38061),(#38062,#38063),(#38064,#38065),(#38066,#38067),(#38068,
#38069),(#38070,#38071),(#38072,#38073),(#38074,#38075),(#38076,#38077),
(#38078,#38079),(#38080,#38081),(#38082,#38083),(#38084,#38085),(#38086,
#38087),(#38088,#38089),(#38090,#38091),(#38092,#38093),(#38094,#38095),
(#38096,#38097),(#38098,#38099),(#38100,#38101),(#38102,#38103),(#38104,
#38105),(#38106,#38107),(#38108,#38109),(#38110,#38111),(#38112,#38113),
(#38114,#38115),(#38116,#38117),(#38118,#38119),(#38120,#38121),(#38122,
#38123),(#38124,#38125),(#38126,#38127),(#38128,#38129),(#38130,#38131),
(#38132,#38133),(#38134,#38135),(#38136,#38137),(#38138,#38139),(#38140,
#38141),(#38142,#38143),(#38144,#38145),(#38146,#38147),(#38148,#38149),
(#38150,#38151),(#38152,#38153),(#38154,#38155),(#38156,#38157),(#38158,
#38159),(#38160,#38161),(#38162,#38163),(#38164,#38165),(#38166,#38167),
(#38168,#38169),(#38170,#38171),(#38172,#38173),(#38174,#38175),(#38176,
#38177),(#38178,#38179),(#38180,#38181),(#38182,#38183),(#38184,#38185),
(#38186,#38187),(#38188,#38189),(#38190,#38191),(#38192,#38193),(#38194,
#38195),(#38196,#38197),(#38198,#38199),(#38200,#38201),(#38202,#38203),
(#38204,#38205),(#38206,#38207),(#38208,#38209),(#38210,#38211),(#38212,
#38213),(#38214,#38215),(#38216,#38217),(#38218,#38219),(#38220,#38221),
(#38222,#38223),(#38224,#38225),(#38226,#38227),(#38228,#38229),(#38230,
#38231),(#38232,#38233),(#38234,#38235),(#38236,#38237),(#38238,#38239),
(#38240,#38241),(#38242,#38243),(#38244,#38245),(#38246,#38247),(#38248,
#38249),(#38250,#38251),(#38252,#38253),(#38254,#38255),(#38256,#38257),
(#38258,#38259),(#38260,#38261),(#38262,#38263),(#38264,#38265),(#38266,
#38267),(#38268,#38269),(#38270,#38271),(#38272,#38273),(#38274,#38275),
(#38276,#38277),(#38278,#38279),(#38280,#38281),(#38282,#38283),(#38284,
#38285),(#38286,#38287),(#38288,#38289),(#38290,#38291),(#38292,#38293),
(#38294,#38295),(#38296,#38297),(#38298,#38299),(#38300,#38301),(#38302,
#38303),(#38304,#38305),(#38306,#38307),(#38308,#38309),(#38310,#38311),
(#38312,#38313),(#38314,#38315),(#38316,#38317),(#38318,#38319),(#38320,
#38321),(#38322,#38323),(#38324,#38325),(#38326,#38327),(#38328,#38329),
(#38330,#38331),(#38332,#38333),(#38334,#38335),(#38336,#38337),(#38338,
#38339),(#38340,#38341),(#38342,#38343),(#38344,#38345),(#38346,#38347),
(#38348,#38349),(#38350,#38351),(#38352,#38353),(#38354,#38355),(#38356,
#38357),(#38358,#38359),(#38360,#38361),(#38362,#38363),(#38364,#38365),
(#38366,#38367),(#38368,#38369),(#38370,#38371),(#38372,#38373),(#38374,
#38375),(#38376,#38377),(#38378,#38379),(#38380,#38381),(#38382,#38383),
(#38384,#38385),(#38386,#38387),(#38388,#38389),(#38390,#38391),(#38392,
#38393),(#38394,#38395),(#38396,#38397),(#38398,#38399),(#38400,#38401),
(#38402,#38403),(#38404,#38405),(#38406,#38407),(#38408,#38409),(#38410,
#38411),(#38412,#38413),(#38414,#38415),(#38416,#38417),(#38418,#38419),
(#38420,#38421),(#38422,#38423),(#38424,#38425),(#38426,#38427),(#38428,
#38429),(#38430,#38431),(#38432,#38433),(#38434,#38435),(#38436,#38437),
(#38438,#38439),(#38440,#38441),(#38442,#38443),(#38444,#38445),(#38446,
#38447),(#38448,#38449),(#38450,#38451),(#38452,#38453),(#38454,#38455),
(#38456,#38457),(#38458,#38459),(#38460,#38461),(#38462,#38463),(#38464,
#38465),(#38466,#38467),(#38468,#38469),(#38470,#38471),(#38472,#38473),
(#38474,#38475),(#38476,#38477),(#38478,#38479),(#38480,#38481),(#38482,
#38483),(#38484,#38485),(#38486,#38487),(#38488,#38489),(#38490,#38491),
(#38492,#38493),(#38494,#38495),(#38496,#38497),(#38498,#38499),(#38500,
#38501),(#38502,#38503),(#38504,#38505),(#38506,#38507),(#38508,#38509),
(#38510,#38511),(#38512,#38513),(#38514,#38515),(#38516,#38517),(#38518,
#38519),(#38520,#38521),(#38522,#38523),(#38524,#38525),(#38526,#38527),
(#38528,#38529),(#38530,#38531),(#38532,#38533),(#38534,#38535),(#38536,
#38537),(#38538,#38539),(#38540,#38541),(#38542,#38543),(#38544,#38545),
(#38546,#38547),(#38548,#38549),(#38550,#38551),(#38552,#38553),(#38554,
#38555),(#38556,#38557),(#38558,#38559),(#38560,#38561),(#38562,#38563),
(#38564,#38565),(#38566,#38567),(#38568,#38569),(#38570,#38571),(#38572,
#38573),(#38574,#38575),(#38576,#38577),(#38578,#38579),(#38580,#38581),
(#38582,#38583),(#38584,#38585),(#38586,#38587),(#38588,#38589),(#38590,
#38591),(#38592,#38593),(#38594,#38595),(#38596,#38597),(#38598,#38599),
(#38600,#38601),(#38602,#38603),(#38604,#38605),(#38606,#38607),(#38608,
#38609),(#38610,#38611),(#38612,#38613),(#38614,#38615),(#38616,#38617),
(#38618,#38619),(#38620,#38621),(#38622,#38623),(#38624,#38625),(#38626,
#38627),(#38628,#38629),(#38630,#38631),(#38632,#38633),(#38634,#38635),
(#38636,#38637),(#38638,#38639),(#38640,#38641),(#38642,#38643),(#38644,
#38645),(#38646,#38647),(#38648,#38649),(#38650,#38651),(#38652,#38653),
(#38654,#38655),(#38656,#38657),(#38658,#38659),(#38660,#38661),(#38662,
#38663),(#38664,#38665),(#38666,#38667),(#38668,#38669),(#38670,#38671),
(#38672,#38673),(#38674,#38675),(#38676,#38677),(#38678,#38679),(#38680,
#38681),(#38682,#38683),(#38684,#38685),(#38686,#38687),(#38688,#38689),
(#38690,#38691),(#38692,#38693),(#38694,#38695),(#38696,#38697),(#38698,
#38699),(#38700,#38701),(#38702,#38703),(#38704,#38705),(#38706,#38707),
(#38708,#38709),(#38710,#38711),(#38712,#38713),(#38714,#38715),(#38716,
#38717),(#38718,#38719),(#38720,#38721),(#38722,#38723),(#38724,#38725),
(#38726,#38727),(#38728,#38729),(#38730,#38731),(#38732,#38733),(#38734,
#38735),(#38736,#38737),(#38738,#38739),(#38740,#38741),(#38742,#38743),
(#38744,#38745),(#38746,#38747),(#38748,#38749),(#38750,#38751),(#38752,
#38753),(#38754,#38755),(#38756,#38757),(#38758,#38759),(#38760,#38761),
(#38762,#38763),(#38764,#38765),(#38766,#38767),(#38768,#38769),(#38770,
#38771),(#38772,#38773),(#38774,#38775),(#38776,#38777),(#38778,#38779),
(#38780,#38781),(#38782,#38783),(#38784,#38785),(#38786,#38787),(#38788,
#38789),(#38790,#38791),(#38792,#38793),(#38794,#38795),(#38796,#38797),
(#38798,#38799),(#38800,#38801),(#38802,#38803),(#38804,#38805),(#38806,
#38807),(#38808,#38809),(#38810,#38811),(#38812,#38813),(#38814,#38815),
(#38816,#38817),(#38818,#38819),(#38820,#38821),(#38822,#38823),(#38824,
#38825),(#38826,#38827),(#38828,#38829),(#38830,#38831),(#38832,#38833),
(#38834,#38835),(#38836,#38837),(#38838,#38839),(#38840,#38841),(#38842,
#38843),(#38844,#38845),(#38846,#38847),(#38848,#38849),(#38850,#38851),
(#38852,#38853),(#38854,#38855),(#38856,#38857),(#38858,#38859),(#38860,
#38861),(#38862,#38863),(#38864,#38865),(#38866,#38867),(#38868,#38869),
(#38870,#38871),(#38872,#38873),(#38874,#38875),(#38876,#38877),(#38878,
#38879),(#38880,#38881),(#38882,#38883),(#38884,#38885),(#38886,#38887),
(#38888,#38889),(#38890,#38891),(#38892,#38893),(#38894,#38895),(#38896,
#38897),(#38898,#38899),(#38900,#38901),(#38902,#38903),(#38904,#38905),
(#38906,#38907),(#38908,#38909),(#38910,#38911),(#38912,#38913),(#38914,
#38915),(#38916,#38917),(#38918,#38919),(#38920,#38921),(#38922,#38923),
(#38924,#38925),(#38926,#38927),(#38928,#38929),(#38930,#38931),(#38932,
#38933),(#38934,#38935),(#38936,#38937),(#38938,#38939),(#38940,#38941),
(#38942,#38943),(#38944,#38945),(#38946,#38947),(#38948,#38949),(#38950,
#38951),(#38952,#38953),(#38954,#38955),(#38956,#38957),(#38958,#38959),
(#38960,#38961),(#38962,#38963),(#38964,#38965),(#38966,#38967),(#38968,
#38969),(#38970,#38971),(#38972,#38973),(#38974,#38975),(#38976,#38977),
(#38978,#38979),(#38980,#38981),(#38982,#38983),(#38984,#38985),(#38986,
#38987),(#38988,#38989),(#38990,#38991),(#38992,#38993),(#38994,#38995),
(#38996,#38997),(#38998,#38999),(#39000,#39001),(#39002,#39003),(#39004,
#39005),(#39006,#39007),(#39008,#39009),(#39010,#39011),(#39012,#39013),
(#39014,#39015),(#39016,#39017),(#39018,#39019),(#39020,#39021),(#39022,
#39023),(#39024,#39025),(#39026,#39027),(#39028,#39029),(#39030,#39031),
(#39032,#39033),(#39034,#39035),(#39036,#39037),(#39038,#39039),(#39040,
#39041),(#39042,#39043),(#39044,#39045),(#39046,#39047),(#39048,#39049),
(#39050,#39051),(#39052,#39053),(#39054,#39055),(#39056,#39057),(#39058,
#39059),(#39060,#39061),(#39062,#39063),(#39064,#39065),(#39066,#39067),
(#39068,#39069),(#39070,#39071),(#39072,#39073),(#39074,#39075),(#39076,
#39077),(#39078,#39079),(#39080,#39081),(#39082,#39083),(#39084,#39085),
(#39086,#39087),(#39088,#39089),(#39090,#39091),(#39092,#39093),(#39094,
#39095),(#39096,#39097),(#39098,#39099),(#39100,#39101),(#39102,#39103),
(#39104,#39105),(#39106,#39107),(#39108,#39109),(#39110,#39111),(#39112,
#39113),(#39114,#39115),(#39116,#39117),(#39118,#39119),(#39120,#39121),
(#39122,#39123),(#39124,#39125),(#39126,#39127),(#39128,#39129),(#39130,
#39131),(#39132,#39133),(#39134,#39135),(#39136,#39137),(#39138,#39139),
(#39140,#39141),(#39142,#39143),(#39144,#39145),(#39146,#39147),(#39148,
#39149),(#39150,#39151),(#39152,#39153),(#39154,#39155),(#39156,#39157),
(#39158,#39159),(#39160,#39161),(#39162,#39163),(#39164,#39165),(#39166,
#39167),(#39168,#39169),(#39170,#39171),(#39172,#39173),(#39174,#39175),
(#39176,#39177),(#39178,#39179),(#39180,#39181),(#39182,#39183),(#39184,
#39185),(#39186,#39187),(#39188,#39189),(#39190,#39191),(#39192,#39193),
(#39194,#39195),(#39196,#39197),(#39198,#39199),(#39200,#39201),(#39202,
#39203),(#39204,#39205),(#39206,#39207),(#39208,#39209),(#39210,#39211),
(#39212,#39213),(#39214,#39215),(#39216,#39217),(#39218,#39219),(#39220,
#39221),(#39222,#39223),(#39224,#39225),(#39226,#39227),(#39228,#39229),
(#39230,#39231),(#39232,#39233),(#39234,#39235),(#39236,#39237),(#39238,
#39239),(#39240,#39241),(#39242,#39243),(#39244,#39245),(#39246,#39247),
(#39248,#39249),(#39250,#39251),(#39252,#39253),(#39254,#39255),(#39256,
#39257),(#39258,#39259),(#39260,#39261),(#39262,#39263),(#39264,#39265),
(#39266,#39267),(#39268,#39269),(#39270,#39271),(#39272,#39273),(#39274,
#39275),(#39276,#39277),(#39278,#39279),(#39280,#39281),(#39282,#39283),
(#39284,#39285),(#39286,#39287),(#39288,#39289),(#39290,#39291),(#39292,
#39293),(#39294,#39295),(#39296,#39297),(#39298,#39299),(#39300,#39301),
(#39302,#39303),(#39304,#39305),(#39306,#39307),(#39308,#39309),(#39310,
#39311),(#39312,#39313),(#39314,#39315),(#39316,#39317),(#39318,#39319),
(#39320,#39321),(#39322,#39323),(#39324,#39325),(#39326,#39327),(#39328,
#39329),(#39330,#39331),(#39332,#39333),(#39334,#39335),(#39336,#39337),
(#39338,#39339),(#39340,#39341),(#39342,#39343),(#39344,#39345),(#39346,
#39347),(#39348,#39349),(#39350,#39351),(#39352,#39353),(#39354,#39355),
(#39356,#39357),(#39358,#39359),(#39360,#39361),(#39362,#39363),(#39364,
#39365),(#39366,#39367),(#39368,#39369),(#39370,#39371),(#39372,#39373),
(#39374,#39375),(#39376,#39377),(#39378,#39379),(#39380,#39381),(#39382,
#39383),(#39384,#39385),(#39386,#39387),(#39388,#39389),(#39390,#39391),
(#39392,#39393),(#39394,#39395),(#39396,#39397),(#39398,#39399),(#39400,
#39401),(#39402,#39403),(#39404,#39405),(#39406,#39407),(#39408,#39409),
(#39410,#39411),(#39412,#39413),(#39414,#39415),(#39416,#39417),(#39418,
#39419),(#39420,#39421),(#39422,#39423),(#39424,#39425),(#39426,#39427),
(#39428,#39429),(#39430,#39431),(#39432,#39433),(#39434,#39435),(#39436,
#39437),(#39438,#39439),(#39440,#39441),(#39442,#39443),(#39444,#39445),
(#39446,#39447),(#39448,#39449),(#39450,#39451),(#39452,#39453),(#39454,
#39455),(#39456,#39457),(#39458,#39459),(#39460,#39461),(#39462,#39463),
(#39464,#39465),(#39466,#39467),(#39468,#39469),(#39470,#39471),(#39472,
#39473),(#39474,#39475),(#39476,#39477),(#39478,#39479),(#39480,#39481),
(#39482,#39483),(#39484,#39485),(#39486,#39487),(#39488,#39489),(#39490,
#39491),(#39492,#39493),(#39494,#39495),(#39496,#39497),(#39498,#39499),
(#39500,#39501),(#39502,#39503),(#39504,#39505),(#39506,#39507),(#39508,
#39509),(#39510,#39511),(#39512,#39513),(#39514,#39515),(#39516,#39517),
(#39518,#39519),(#39520,#39521),(#39522,#39523),(#39524,#39525),(#39526,
#39527),(#39528,#39529),(#39530,#39531),(#39532,#39533),(#39534,#39535),
(#39536,#39537),(#39538,#39539),(#39540,#39541),(#39542,#39543),(#39544,
#39545),(#39546,#39547),(#39548,#39549),(#39550,#39551),(#39552,#39553),
(#39554,#39555),(#39556,#39557),(#39558,#39559),(#39560,#39561),(#39562,
#39563),(#39564,#39565),(#39566,#39567),(#39568,#39569),(#39570,#39571),
(#39572,#39573),(#39574,#39575),(#39576,#39577),(#39578,#39579),(#39580,
#39581),(#39582,#39583),(#39584,#39585),(#39586,#39587),(#39588,#39589),
(#39590,#39591),(#39592,#39593),(#39594,#39595),(#39596,#39597),(#39598,
#39599),(#39600,#39601),(#39602,#39603),(#39604,#39605),(#39606,#39607),
(#39608,#39609),(#39610,#39611),(#39612,#39613),(#39614,#39615),(#39616,
#39617),(#39618,#39619),(#39620,#39621),(#39622,#39623),(#39624,#39625),
(#39626,#39627),(#39628,#39629),(#39630,#39631),(#39632,#39633),(#39634,
#39635),(#39636,#39637),(#39638,#39639),(#39640,#39641),(#39642,#39643),
(#39644,#39645),(#39646,#39647),(#39648,#39649),(#39650,#39651),(#39652,
#39653),(#39654,#39655),(#39656,#39657),(#39658,#39659),(#39660,#39661),
(#39662,#39663),(#39664,#39665),(#39666,#39667),(#39668,#39669),(#39670,
#39671),(#39672,#39673),(#39674,#39675),(#39676,#39677),(#39678,#39679),
(#39680,#39681),(#39682,#39683),(#39684,#39685),(#39686,#39687),(#39688,
#39689),(#39690,#39691),(#39692,#39693),(#39694,#39695),(#39696,#39697),
(#39698,#39699),(#39700,#39701),(#39702,#39703),(#39704,#39705),(#39706,
#39707),(#39708,#39709),(#39710,#39711),(#39712,#39713),(#39714,#39715),
(#39716,#39717),(#39718,#39719),(#39720,#39721),(#39722,#39723),(#39724,
#39725),(#39726,#39727),(#39728,#39729),(#39730,#39731),(#39732,#39733),
(#39734,#39735),(#39736,#39737),(#39738,#39739),(#39740,#39741),(#39742,
#39743),(#39744,#39745),(#39746,#39747),(#39748,#39749),(#39750,#39751),
(#39752,#39753),(#39754,#39755),(#39756,#39757),(#39758,#39759),(#39760,
#39761),(#39762,#39763),(#39764,#39765),(#39766,#39767),(#39768,#39769),
(#39770,#39771),(#39772,#39773),(#39774,#39775),(#39776,#39777),(#39778,
#39779),(#39780,#39781),(#39782,#39783),(#39784,#39785),(#39786,#39787),
(#39788,#39789),(#39790,#39791),(#39792,#39793),(#39794,#39795),(#39796,
#39797),(#39798,#39799),(#39800,#39801),(#39802,#39803),(#39804,#39805),
(#39806,#39807),(#39808,#39809),(#39810,#39811),(#39812,#39813),(#39814,
#39815),(#39816,#39817),(#39818,#39819),(#39820,#39821),(#39822,#39823),
(#39824,#39825),(#39826,#39827),(#39828,#39829),(#39830,#39831),(#39832,
#39833),(#39834,#39835),(#39836,#39837),(#39838,#39839),(#39840,#39841),
(#39842,#39843),(#39844,#39845),(#39846,#39847),(#39848,#39849),(#39850,
#39851),(#39852,#39853),(#39854,#39855),(#39856,#39857),(#39858,#39859),
(#39860,#39861),(#39862,#39863),(#39864,#39865),(#39866,#39867),(#39868,
#39869),(#39870,#39871),(#39872,#39873),(#39874,#39875),(#39876,#39877),
(#39878,#39879),(#39880,#39881),(#39882,#39883),(#39884,#39885),(#39886,
#39887),(#39888,#39889),(#39890,#39891),(#39892,#39893),(#39894,#39895),
(#39896,#39897),(#39898,#39899),(#39900,#39901),(#39902,#39903),(#39904,
#39905),(#39906,#39907),(#39908,#39909),(#39910,#39911),(#39912,#39913),
(#39914,#39915),(#39916,#39917),(#39918,#39919),(#39920,#39921),(#39922,
#39923),(#39924,#39925),(#39926,#39927),(#39928,#39929),(#39930,#39931),
(#39932,#39933),(#39934,#39935),(#39936,#39937),(#39938,#39939),(#39940,
#39941),(#39942,#39943),(#39944,#39945),(#39946,#39947),(#39948,#39949),
(#39950,#39951),(#39952,#39953),(#39954,#39955),(#39956,#39957),(#39958,
#39959),(#39960,#39961),(#39962,#39963),(#39964,#39965),(#39966,#39967),
(#39968,#39969),(#39970,#39971),(#39972,#39973),(#39974,#39975),(#39976,
#39977),(#39978,#39979),(#39980,#39981),(#39982,#39983),(#39984,#39985),
(#39986,#39987),(#39988,#39989),(#39990,#39991),(#39992,#39993),(#39994,
#39995),(#39996,#39997),(#39998,#39999),(#40000,#40001),(#40002,#40003),
(#40004,#40005),(#40006,#40007),(#40008,#40009),(#40010,#40011),(#40012,
#40013),(#40014,#40015),(#40016,#40017),(#40018,#40019),(#40020,#40021),
(#40022,#40023),(#40024,#40025),(#40026,#40027),(#40028,#40029),(#40030,
#40031),(#40032,#40033),(#40034,#40035),(#40036,#40037),(#40038,#40039),
(#40040,#40041),(#40042,#40043),(#40044,#40045),(#40046,#40047),(#40048,
#40049),(#40050,#40051),(#40052,#40053),(#40054,#40055),(#40056,#40057),
(#40058,#40059),(#40060,#40061),(#40062,#40063),(#40064,#40065),(#40066,
#40067),(#40068,#40069),(#40070,#40071),(#40072,#40073),(#40074,#40075),
(#40076,#40077),(#40078,#40079),(#40080,#40081),(#40082,#40083),(#40084,
#40085),(#40086,#40087),(#40088,#40089),(#40090,#40091),(#40092,#40093),
(#40094,#40095),(#40096,#40097),(#40098,#40099),(#40100,#40101),(#40102,
#40103),(#40104,#40105),(#40106,#40107),(#40108,#40109),(#40110,#40111),
(#40112,#40113),(#40114,#40115),(#40116,#40117),(#40118,#40119),(#40120,
#40121),(#40122,#40123),(#40124,#40125),(#40126,#40127),(#40128,#40129),
(#40130,#40131),(#40132,#40133),(#40134,#40135),(#40136,#40137),(#40138,
#40139),(#40140,#40141),(#40142,#40143),(#40144,#40145),(#40146,#40147),
(#40148,#40149),(#40150,#40151),(#40152,#40153),(#40154,#40155),(#40156,
#40157),(#40158,#40159),(#40160,#40161),(#40162,#40163),(#40164,#40165),
(#40166,#40167),(#40168,#40169),(#40170,#40171),(#40172,#40173),(#40174,
#40175),(#40176,#40177),(#40178,#40179),(#40180,#40181),(#40182,#40183),
(#40184,#40185),(#40186,#40187),(#40188,#40189),(#40190,#40191),(#40192,
#40193),(#40194,#40195),(#40196,#40197),(#40198,#40199),(#40200,#40201),
(#40202,#40203),(#40204,#40205),(#40206,#40207),(#40208,#40209),(#40210,
#40211),(#40212,#40213),(#40214,#40215),(#40216,#40217),(#40218,#40219),
(#40220,#40221),(#40222,#40223),(#40224,#40225),(#40226,#40227),(#40228,
#40229),(#40230,#40231),(#40232,#40233),(#40234,#40235),(#40236,#40237),
(#40238,#40239),(#40240,#40241),(#40242,#40243),(#40244,#40245),(#40246,
#40247),(#40248,#40249),(#40250,#40251),(#40252,#40253),(#40254,#40255),
(#40256,#40257),(#40258,#40259),(#40260,#40261),(#40262,#40263),(#40264,
#40265),(#40266,#40267),(#40268,#40269),(#40270,#40271),(#40272,#40273),
(#40274,#40275),(#40276,#40277),(#40278,#40279),(#40280,#40281),(#40282,
#40283),(#40284,#40285),(#40286,#40287),(#40288,#40289),(#40290,#40291),
(#40292,#40293),(#40294,#40295),(#40296,#40297),(#40298,#40299),(#40300,
#40301),(#40302,#40303),(#40304,#40305),(#40306,#40307),(#40308,#40309),
(#40310,#40311),(#40312,#40313),(#40314,#40315),(#40316,#40317),(#40318,
#40319),(#40320,#40321),(#40322,#40323),(#40324,#40325),(#40326,#40327),
(#40328,#40329),(#40330,#40331),(#40332,#40333),(#40334,#40335),(#40336,
#40337),(#40338,#40339),(#40340,#40341),(#40342,#40343),(#40344,#40345),
(#40346,#40347),(#40348,#40349),(#40350,#40351),(#40352,#40353),(#40354,
#40355),(#40356,#40357),(#40358,#40359),(#40360,#40361),(#40362,#40363),
(#40364,#40365),(#40366,#40367),(#40368,#40369),(#40370,#40371),(#40372,
#40373),(#40374,#40375),(#40376,#40377),(#40378,#40379),(#40380,#40381),
(#40382,#40383),(#40384,#40385),(#40386,#40387),(#40388,#40389),(#40390,
#40391),(#40392,#40393),(#40394,#40395),(#40396,#40397),(#40398,#40399),
(#40400,#40401),(#40402,#40403),(#40404,#40405),(#40406,#40407),(#40408,
#40409),(#40410,#40411),(#40412,#40413),(#40414,#40415),(#40416,#40417),
(#40418,#40419),(#40420,#40421),(#40422,#40423),(#40424,#40425),(#40426,
#40427),(#40428,#40429),(#40430,#40431),(#40432,#40433),(#40434,#40435),
(#40436,#40437),(#40438,#40439),(#40440,#40441),(#40442,#40443),(#40444,
#40445),(#40446,#40447),(#40448,#40449),(#40450,#40451),(#40452,#40453),
(#40454,#40455),(#40456,#40457),(#40458,#40459),(#40460,#40461),(#40462,
#40463),(#40464,#40465),(#40466,#40467),(#40468,#40469),(#40470,#40471),
(#40472,#40473),(#40474,#40475),(#40476,#40477),(#40478,#40479),(#40480,
#40481),(#40482,#40483),(#40484,#40485),(#40486,#40487),(#40488,#40489),
(#40490,#40491),(#40492,#40493),(#40494,#40495),(#40496,#40497),(#40498,
#40499),(#40500,#40501),(#40502,#40503),(#40504,#40505),(#40506,#40507),
(#40508,#40509),(#40510,#40511),(#40512,#40513),(#40514,#40515),(#40516,
#40517),(#40518,#40519),(#40520,#40521),(#40522,#40523),(#40524,#40525),
(#40526,#40527),(#40528,#40529),(#40530,#40531),(#40532,#40533),(#40534,
#40535),(#40536,#40537),(#40538,#40539),(#40540,#40541),(#40542,#40543),
(#40544,#40545),(#40546,#40547),(#40548,#40549),(#40550,#40551),(#40552,
#40553),(#40554,#40555),(#40556,#40557),(#40558,#40559),(#40560,#40561),
(#40562,#40563),(#40564,#40565),(#40566,#40567),(#40568,#40569),(#40570,
#40571),(#40572,#40573),(#40574,#40575),(#40576,#40577),(#40578,#40579),
(#40580,#40581),(#40582,#40583),(#40584,#40585),(#40586,#40587),(#40588,
#40589),(#40590,#40591),(#40592,#40593),(#40594,#40595),(#40596,#40597),
(#40598,#40599),(#40600,#40601),(#40602,#40603),(#40604,#40605),(#40606,
#40607),(#40608,#40609),(#40610,#40611),(#40612,#40613),(#40614,#40615),
(#40616,#40617),(#40618,#40619),(#40620,#40621),(#40622,#40623),(#40624,
#40625),(#40626,#40627),(#40628,#40629),(#40630,#40631),(#40632,#40633),
(#40634,#40635),(#40636,#40637),(#40638,#40639),(#40640,#40641),(#40642,
#40643),(#40644,#40645),(#40646,#40647),(#40648,#40649),(#40650,#40651),
(#40652,#40653),(#40654,#40655),(#40656,#40657),(#40658,#40659),(#40660,
#40661),(#40662,#40663),(#40664,#40665),(#40666,#40667),(#40668,#40669),
(#40670,#40671),(#40672,#40673),(#40674,#40675),(#40676,#40677),(#40678,
#40679),(#40680,#40681),(#40682,#40683),(#40684,#40685),(#40686,#40687),
(#40688,#40689),(#40690,#40691),(#40692,#40693),(#40694,#40695),(#40696,
#40697),(#40698,#40699),(#40700,#40701),(#40702,#40703),(#40704,#40705),
(#40706,#40707),(#40708,#40709),(#40710,#40711),(#40712,#40713),(#40714,
#40715),(#40716,#40717),(#40718,#40719),(#40720,#40721),(#40722,#40723),
(#40724,#40725),(#40726,#40727),(#40728,#40729),(#40730,#40731),(#40732,
#40733),(#40734,#40735),(#40736,#40737),(#40738,#40739),(#40740,#40741),
(#40742,#40743),(#40744,#40745),(#40746,#40747),(#40748,#40749),(#40750,
#40751),(#40752,#40753),(#40754,#40755),(#40756,#40757),(#40758,#40759),
(#40760,#40761),(#40762,#40763),(#40764,#40765),(#40766,#40767),(#40768,
#40769),(#40770,#40771),(#40772,#40773),(#40774,#40775),(#40776,#40777),
(#40778,#40779),(#40780,#40781),(#40782,#40783),(#40784,#40785),(#40786,
#40787),(#40788,#40789),(#40790,#40791),(#40792,#40793),(#40794,#40795),
(#40796,#40797),(#40798,#40799),(#40800,#40801),(#40802,#40803),(#40804,
#40805),(#40806,#40807),(#40808,#40809),(#40810,#40811),(#40812,#40813),
(#40814,#40815),(#40816,#40817),(#40818,#40819),(#40820,#40821),(#40822,
#40823),(#40824,#40825),(#40826,#40827),(#40828,#40829),(#40830,#40831),
(#40832,#40833),(#40834,#40835),(#40836,#40837),(#40838,#40839),(#40840,
#40841),(#40842,#40843),(#40844,#40845),(#40846,#40847),(#40848,#40849),
(#40850,#40851),(#40852,#40853),(#40854,#40855),(#40856,#40857),(#40858,
#40859),(#40860,#40861),(#40862,#40863),(#40864,#40865),(#40866,#40867),
(#40868,#40869),(#40870,#40871),(#40872,#40873),(#40874,#40875),(#40876,
#40877),(#40878,#40879),(#40880,#40881),(#40882,#40883),(#40884,#40885),
(#40886,#40887),(#40888,#40889),(#40890,#40891),(#40892,#40893),(#40894,
#40895),(#40896,#40897),(#40898,#40899),(#40900,#40901),(#40902,#40903),
(#40904,#40905),(#40906,#40907),(#40908,#40909),(#40910,#40911),(#40912,
#40913),(#40914,#40915),(#40916,#40917),(#40918,#40919),(#40920,#40921),
(#40922,#40923),(#40924,#40925),(#40926,#40927),(#40928,#40929),(#40930,
#40931),(#40932,#40933),(#40934,#40935),(#40936,#40937),(#40938,#40939),
(#40940,#40941),(#40942,#40943),(#40944,#40945),(#40946,#40947),(#40948,
#40949),(#40950,#40951),(#40952,#40953),(#40954,#40955),(#40956,#40957),
(#40958,#40959),(#40960,#40961),(#40962,#40963),(#40964,#40965),(#40966,
#40967),(#40968,#40969),(#40970,#40971),(#40972,#40973),(#40974,#40975),
(#40976,#40977),(#40978,#40979),(#40980,#40981),(#40982,#40983),(#40984,
#40985),(#40986,#40987),(#40988,#40989),(#40990,#40991),(#40992,#40993),
(#40994,#40995),(#40996,#40997),(#40998,#40999),(#41000,#41001),(#41002,
#41003),(#41004,#41005),(#41006,#41007),(#41008,#41009),(#41010,#41011),
(#41012,#41013),(#41014,#41015),(#41016,#41017),(#41018,#41019),(#41020,
#41021),(#41022,#41023),(#41024,#41025),(#41026,#41027),(#41028,#41029),
(#41030,#41031),(#41032,#41033),(#41034,#41035),(#41036,#41037),(#41038,
#41039),(#41040,#41041),(#41042,#41043),(#41044,#41045),(#41046,#41047),
(#41048,#41049),(#41050,#41051),(#41052,#41053),(#41054,#41055),(#41056,
#41057),(#41058,#41059),(#41060,#41061),(#41062,#41063),(#41064,#41065),
(#41066,#41067),(#41068,#41069),(#41070,#41071),(#41072,#41073),(#41074,
#41075),(#41076,#41077),(#41078,#41079),(#41080,#41081),(#41082,#41083),
(#41084,#41085),(#41086,#41087),(#41088,#41089),(#41090,#41091),(#41092,
#41093),(#41094,#41095),(#41096,#41097),(#41098,#41099),(#41100,#41101),
(#41102,#41103),(#41104,#41105),(#41106,#41107),(#41108,#41109),(#41110,
#41111),(#41112,#41113),(#41114,#41115),(#41116,#41117),(#41118,#41119),
(#41120,#41121),(#41122,#41123),(#41124,#41125),(#41126,#41127),(#41128,
#41129),(#41130,#41131),(#41132,#41133),(#41134,#41135),(#41136,#41137),
(#41138,#41139),(#41140,#41141),(#41142,#41143),(#41144,#41145),(#41146,
#41147),(#41148,#41149),(#41150,#41151),(#41152,#41153),(#41154,#41155),
(#41156,#41157),(#41158,#41159),(#41160,#41161),(#41162,#41163),(#41164,
#41165),(#41166,#41167),(#41168,#41169),(#41170,#41171),(#41172,#41173),
(#41174,#41175),(#41176,#41177),(#41178,#41179),(#41180,#41181),(#41182,
#41183),(#41184,#41185),(#41186,#41187),(#41188,#41189),(#41190,#41191),
(#41192,#41193),(#41194,#41195),(#41196,#41197),(#41198,#41199),(#41200,
#41201),(#41202,#41203),(#41204,#41205),(#41206,#41207),(#41208,#41209),
(#41210,#41211),(#41212,#41213),(#41214,#41215),(#41216,#41217),(#41218,
#41219),(#41220,#41221),(#41222,#41223),(#41224,#41225),(#41226,#41227)),
 .UNSPECIFIED.,.F.,.F.,.F.,(4,1,1,1,1,1,1,1,1,1,1,1,1,1,1,1,1,1,1,1,1,1,
1,1,1,1,1,1,1,1,1,1,1,1,1,1,1,1,1,1,1,1,1,1,1,1,1,1,1,1,1,1,1,1,1,1,1,1,
1,1,1,1,1,1,1,1,1,1,1,1,1,1,1,1,1,1,1,1,1,1,1,1,1,1,1,1,1,1,1,1,1,1,1,1,
1,1,1,1,1,1,1,1,1,1,1,1,1,1,1,1,1,1,1,1,1,1,1,1,1,1,1,1,1,1,1,1,1,1,1,1,
1,1,1,1,1,1,1,1,1,1,1,1,1,1,1,1,1,1,1,1,1,1,1,1,1,1,1,1,1,1,1,1,1,1,1,1,
1,1,1,1,1,1,1,1,1,1,1,1,1,1,1,1,1,1,1,1,1,1,1,1,1,1,1,1,1,1,1,1,1,1,1,1,
1,1,1,1,1,1,1,1,1,1,1,1,1,1,1,1,1,1,1,1,1,1,1,1,1,1,1,1,1,1,1,1,1,1,1,1,
1,1,1,1,1,1,1,1,1,1,1,1,1,1,1,1,1,1,1,1,1,1,1,1,1,1,1,1,1,1,1,1,1,1,1,1,
1,1,1,1,1,1,1,1,1,1,1,1,1,1,1,1,1,1,1,1,1,1,1,1,1,1,1,1,1,1,1,1,1,1,1,1,
1,1,1,1,1,1,1,1,1,1,1,1,1,1,1,1,1,1,1,1,1,1,1,1,1,1,1,1,1,1,1,1,1,1,1,1,
1,1,1,1,1,1,1,1,1,1,1,1,1,1,1,1,1,1,1,1,1,1,1,1,1,1,1,1,1,1,1,1,1,1,1,1,
1,1,1,1,1,1,1,1,1,1,1,1,1,1,1,1,1,1,1,1,1,1,1,1,1,1,1,1,1,1,1,1,1,1,1,1,
1,1,1,1,1,1,1,1,1,1,1,1,1,1,1,1,1,1,1,1,1,1,1,1,1,1,1,1,1,1,1,1,1,1,1,1,
1,1,1,1,1,1,1,1,1,1,1,1,1,1,1,1,1,1,1,1,1,1,1,1,1,1,1,1,1,1,1,1,1,1,1,1,
1,1,1,1,1,1,1,1,1,1,1,1,1,1,1,1,1,1,1,1,1,1,1,1,1,1,1,1,1,1,1,1,1,1,1,1,
1,1,1,1,1,1,1,1,1,1,1,1,1,1,1,1,1,1,1,1,1,1,1,1,1,1,1,1,1,1,1,1,1,1,1,1,
1,1,1,1,1,1,1,1,1,1,1,1,1,1,1,1,1,1,1,1,1,1,1,1,1,1,1,1,1,1,1,1,1,1,1,1,
1,1,1,1,1,1,1,1,1,1,1,1,1,1,1,1,1,1,1,1,1,1,1,1,1,1,1,1,1,1,1,1,1,1,1,1,
1,1,1,1,1,1,1,1,1,1,1,1,1,1,1,1,1,1,1,1,1,1,1,1,1,1,1,1,1,1,1,1,1,1,1,1,
1,1,1,1,1,1,1,1,1,1,1,1,1,1,1,1,1,1,1,1,1,1,1,1,1,1,1,1,1,1,1,1,1,1,1,1,
1,1,1,1,1,1,1,1,1,1,1,1,1,1,1,1,1,1,1,1,1,1,1,1,1,1,1,1,1,1,1,1,1,1,1,1,
1,1,1,1,1,1,1,1,1,1,1,1,1,1,1,1,1,1,1,1,1,1,1,1,1,1,1,1,1,1,1,1,1,1,1,1,
1,1,1,1,1,1,1,1,1,1,1,1,1,1,1,1,1,1,1,1,1,1,1,1,1,1,1,1,1,1,1,1,1,1,1,1,
1,1,1,1,1,1,1,1,1,1,1,1,1,1,1,1,1,1,1,1,1,1,1,1,1,1,1,1,1,1,1,1,1,1,1,1,
1,1,1,1,1,1,1,1,1,1,1,1,1,1,1,1,1,1,1,1,1,1,1,1,1,1,1,1,1,1,1,1,1,1,1,1,
1,1,1,1,1,1,1,1,1,1,1,1,1,1,1,1,1,1,1,1,1,1,1,1,1,1,1,1,1,1,1,1,1,1,1,1,
1,1,1,1,1,1,1,1,1,1,1,1,1,1,1,1,1,1,1,1,1,1,1,1,1,1,1,1,1,1,1,1,1,1,1,1,
1,1,1,1,1,1,1,1,1,1,1,1,1,1,1,1,1,1,1,1,1,1,1,1,1,1,1,1,1,1,1,1,1,1,1,1,
1,1,1,1,1,1,1,1,1,1,1,1,1,1,1,1,1,1,1,1,1,1,1,1,1,1,1,1,1,1,1,1,1,1,1,1,
1,1,1,1,1,1,1,1,1,1,1,1,1,1,1,1,1,1,1,1,1,1,1,1,1,1,1,1,1,1,1,1,1,1,1,1,
1,1,1,1,1,1,1,1,1,1,1,1,1,1,1,1,1,1,1,1,1,1,1,1,1,1,1,1,1,1,1,1,1,1,1,1,
1,1,1,1,1,1,1,1,1,1,1,1,1,1,1,1,1,1,1,1,1,1,1,1,1,1,1,1,1,1,1,1,1,1,1,1,
1,1,1,1,1,1,1,1,1,1,1,1,1,1,1,1,1,1,1,1,1,1,1,1,1,1,1,1,1,1,1,1,1,1,1,1,
1,1,1,1,1,1,1,1,1,1,1,1,1,1,1,1,1,1,1,1,1,1,1,1,1,1,1,1,1,1,1,1,1,1,1,1,
1,1,1,1,1,1,1,1,1,1,1,1,1,1,1,1,1,1,1,1,1,1,1,1,1,1,1,1,1,1,1,1,1,1,1,1,
1,1,1,1,1,1,1,1,1,1,1,1,1,1,1,1,1,1,1,1,1,1,1,1,1,1,1,1,1,1,1,1,1,1,1,1,
1,1,1,1,1,1,1,1,1,1,1,1,1,1,1,1,1,1,1,1,1,1,1,1,1,1,1,1,1,1,1,1,1,1,1,1,
1,1,1,1,1,1,1,1,1,1,1,1,1,1,1,1,1,1,1,1,1,1,1,1,1,1,1,1,1,1,1,1,1,1,1,1,
1,1,1,1,1,1,1,1,1,1,1,1,1,1,1,1,1,1,1,1,1,1,1,1,1,1,1,1,1,1,1,1,1,1,1,1,
1,1,1,1,1,1,1,1,1,1,1,1,1,1,1,1,1,1,1,1,1,1,1,1,1,1,1,1,1,1,1,1,1,1,1,1,
1,1,1,1,1,1,1,1,1,1,1,1,1,1,1,1,1,1,1,1,1,1,1,1,1,1,1,1,1,1,1,1,1,1,1,1,
1,1,1,1,1,1,1,1,1,1,1,1,1,1,1,1,1,1,1,1,1,1,1,1,1,1,1,1,1,1,1,1,1,1,1,1,
1,1,1,1,1,1,1,1,1,1,1,1,1,1,1,1,1,1,1,1,1,1,1,1,1,1,1,1,1,1,1,1,1,1,1,1,
1,1,1,1,1,1,1,1,1,1,1,1,1,1,1,1,1,1,1,1,1,1,1,1,1,1,1,1,1,1,1,1,1,1,1,1,
1,1,1,1,1,1,1,1,1,1,1,1,1,1,1,1,1,1,1,1,1,1,1,1,1,1,1,1,1,1,1,1,1,1,1,1,
1,1,1,1,1,1,1,1,1,1,1,1,1,1,1,1,1,1,1,1,1,1,1,1,1,1,1,1,1,1,1,1,1,1,1,1,
1,1,1,1,1,1,1,1,1,1,1,1,1,1,1,1,1,1,1,1,1,1,1,1,1,1,1,1,1,1,1,1,1,1,1,1,
1,1,1,1,1,1,1,1,1,1,1,1,1,1,1,1,1,1,1,1,1,1,1,1,1,1,1,1,1,1,1,1,1,1,1,1,
1,1,1,1,1,1,1,1,1,1,1,1,1,1,1,1,1,1,1,1,1,1,1,1,1,1,1,1,1,1,1,1,1,1,1,1,
1,1,1,1,1,1,1,1,1,1,1,1,1,1,1,1,1,1,1,1,1,1,1,1,1,1,1,1,1,1,1,1,1,1,1,1,
1,1,1,1,1,1,1,1,1,1,1,1,1,1,1,1,1,1,1,1,1,1,1,1,1,1,1,1,1,1,1,1,1,1,1,1,
1,1,1,1,1,1,1,1,1,1,1,1,1,1,1,1,1,1,1,1,1,1,1,1,1,1,1,1,1,1,1,1,1,1,1,1,
1,1,1,1,1,1,1,1,1,1,1,1,1,1,1,1,1,1,1,1,1,1,1,1,1,1,1,1,1,1,1,1,1,1,1,1,
1,1,1,1,1,1,1,1,1,1,1,1,1,1,1,1,1,1,1,1,1,1,1,1,1,1,1,1,1,1,1,1,1,1,1,1,
1,1,1,1,1,1,1,1,1,1,1,1,1,1,1,1,1,1,1,1,1,1,1,1,1,1,1,1,1,1,1,1,1,1,1,1,
1,1,1,1,1,1,1,1,1,1,1,1,1,1,1,1,1,1,1,1,1,1,1,1,1,1,1,1,1,1,1,1,1,1,1,1,
1,1,1,1,1,1,1,1,1,1,1,1,1,1,1,1,1,1,1,1,1,1,1,1,1,1,1,1,1,1,1,1,1,1,1,1,
1,1,1,1,1,1,1,1,1,1,1,1,1,1,1,1,1,1,1,1,1,1,1,1,1,1,1,1,1,1,1,1,1,1,1,1,
1,1,1,1,1,1,1,1,1,1,1,1,1,1,1,1,1,1,1,1,1,1,1,1,1,1,1,1,1,1,1,1,1,1,1,1,
1,1,1,1,1,1,1,1,1,1,1,1,1,1,1,1,1,1,1,1,1,1,1,1,1,1,1,1,1,1,1,1,1,1,1,1,
1,1,1,1,1,1,1,1,1,1,1,1,1,1,1,1,1,1,1,1,1,1,1,1,1,1,1,1,1,1,1,1,1,1,1,1,
1,1,1,1,1,1,1,1,1,1,1,1,1,1,1,1,1,1,1,1,1,1,1,1,1,1,1,1,1,1,1,1,1,1,1,1,
1,1,1,1,1,1,1,1,1,1,1,1,1,1,1,1,1,1,1,1,1,1,1,1,1,1,1,1,1,1,1,1,1,1,1,1,
1,1,1,1,1,1,1,1,1,1,1,1,1,1,1,1,1,1,1,1,1,1,1,1,1,1,1,1,1,1,1,1,1,1,1,1,
1,1,1,1,1,1,1,1,1,1,1,1,1,1,1,1,1,1,1,1,1,1,1,1,1,1,1,1,1,1,1,1,1,1,1,1,
1,1,1,1,1,1,1,1,1,1,1,1,1,1,1,1,1,1,1,1,1,1,1,1,1,1,1,1,1,1,1,1,1,1,1,1,
1,1,1,1,1,1,1,1,1,1,1,1,1,1,1,1,1,1,1,1,1,1,1,1,1,1,1,1,1,1,1,1,1,1,1,1,
1,1,1,1,1,1,1,1,1,1,1,1,1,1,1,1,1,1,1,1,1,1,1,1,1,1,1,1,1,1,1,1,1,1,1,1,
1,1,1,1,1,1,1,1,1,1,1,1,1,1,1,1,1,1,1,1,1,1,1,1,1,1,1,1,1,1,1,1,1,1,1,1,
1,1,1,1,1,1,1,1,1,1,1,1,1,1,1,1,1,1,1,1,1,1,1,1,1,1,1,1,1,1,1,1,1,1,1,1,
1,1,1,1,1,1,1,1,1,1,1,1,1,1,1,1,1,1,1,1,1,1,1,1,1,1,1,1,1,1,1,1,1,1,1,1,
1,1,1,1,1,1,1,1,1,1,1,1,1,1,1,1,1,1,1,1,1,1,1,1,1,1,1,1,1,1,1,1,1,1,1,1,
1,1,1,1,1,1,1,1,1,1,1,1,1,1,1,1,1,1,1,1,1,1,1,1,1,1,1,1,1,1,1,1,1,1,1,1,
1,1,1,1,1,1,1,1,1,1,1,1,1,1,1,1,1,1,1,1,1,1,1,1,1,1,1,1,1,1,1,1,1,1,1,1,
1,1,1,1,1,1,1,1,1,1,1,1,1,1,1,1,1,1,1,1,1,1,1,1,1,1,1,1,1,1,1,1,1,1,1,1,
1,1,1,1,1,1,1,1,1,1,1,1,1,1,1,1,1,1,1,1,1,1,1,1,1,1,1,1,1,1,1,1,1,1,1,1,
1,1,1,1,1,1,1,1,1,1,1,1,1,1,1,1,1,1,1,1,1,1,1,1,1,1,1,1,1,1,1,1,1,1,1,1,
1,1,1,1,1,1,1,1,1,1,1,1,1,1,1,1,1,1,1,1,1,1,1,1,1,1,1,1,1,1,1,1,1,1,1,1,
1,1,1,1,1,1,1,1,1,1,1,1,1,1,1,1,1,1,1,1,1,1,1,1,1,1,1,1,1,1,1,1,1,1,1,1,
1,1,1,1,1,1,1,1,1,1,1,1,1,1,1,1,1,1,1,1,1,1,1,1,1,1,1,1,1,1,1,1,1,1,1,1,
1,1,1,1,1,1,1,1,1,1,1,1,1,1,1,1,1,1,1,1,1,1,1,1,1,1,1,1,1,1,1,1,1,1,1,1,
1,1,1,1,1,1,1,1,1,1,1,1,1,1,1,1,1,1,1,1,1,1,1,1,1,1,1,1,1,1,1,1,1,1,1,1,
1,1,1,1,1,1,1,1,1,1,1,1,1,1,1,1,1,1,1,1,1,1,1,1,1,1,1,1,1,1,1,1,1,1,1,1,
1,1,1,1,1,1,1,1,1,1,1,1,1,1,1,1,1,1,1,1,1,1,1,1,1,1,1,1,1,1,1,1,1,1,1,1,
1,1,1,1,1,1,1,1,1,1,1,1,1,1,1,1,1,1,1,1,1,1,1,1,1,1,1,1,1,1,1,1,1,1,1,1,
1,1,1,1,1,1,1,1,1,1,1,1,1,1,1,1,1,1,1,1,1,1,1,1,1,1,1,1,1,1,1,1,1,1,1,1,
1,1,1,1,1,1,1,1,1,1,1,1,1,1,1,1,1,1,1,1,1,1,1,1,1,1,1,1,1,1,1,1,1,1,1,1,
1,1,1,1,1,1,1,1,1,1,1,1,1,1,1,1,1,1,1,1,1,1,1,1,1,1,1,1,1,1,1,1,1,1,1,1,
1,1,1,1,1,1,1,1,1,1,1,1,1,1,1,1,1,1,1,1,1,1,1,1,1,1,1,1,1,1,1,1,1,1,1,1,
1,1,1,1,1,1,1,1,1,1,1,1,1,1,1,1,1,1,1,1,1,1,1,1,1,1,1,1,1,1,1,1,1,1,1,1,
1,1,1,1,1,1,1,1,1,1,1,1,1,1,1,1,1,1,1,1,1,1,1,1,1,1,1,1,1,1,1,1,1,1,1,1,
1,1,1,1,1,1,1,1,1,1,1,1,1,1,1,1,1,1,1,1,1,1,1,1,1,1,1,1,1,1,1,1,1,1,1,1,
1,1,1,1,1,1,1,1,1,1,1,1,1,1,1,1,1,1,1,1,1,1,1,1,1,1,1,1,1,1,1,1,1,1,1,1,
1,1,1,1,1,1,1,1,1,1,1,1,1,1,1,1,1,1,1,1,1,1,1,1,1,1,1,1,1,1,1,1,1,1,1,1,
1,1,1,1,1,1,1,1,1,1,1,1,1,1,1,1,1,1,1,1,1,1,1,1,1,1,1,1,1,1,1,1,1,1,1,1,
1,1,1,1,1,1,1,1,1,1,1,1,1,1,1,1,1,1,1,1,1,1,1,1,1,1,1,1,1,1,1,1,1,1,1,1,
1,1,1,1,1,1,1,1,1,1,1,1,1,1,1,1,1,1,1,1,1,1,1,1,1,1,1,1,1,1,1,1,1,1,1,1,
1,1,1,1,4),(2,2),(0.,0.869746702321014,1.7394931589914,2.60923976624962,
3.47983908319159,4.35043840179749,5.22018503077054,6.08993165951504,6.95967828799171,
7.82942491616733,8.69917154401062,9.56891817149224,10.4395174886835,11.3101168056706,
12.179863432132,13.049610058144,13.9193566836854,14.7891033087372,15.6588499332817,
16.5285965573034,17.3991958717975,18.2697951860185,18.7046684974166,19.1395418086746,
19.5744151197912,20.0092884307654,20.4441617415962,20.8790350522825,21.7487816732187,
22.1836549834672,22.6185282935685,23.0534016035221,23.4882749133276,23.9231482229848,
24.3588742245859,24.794600226187,25.2294735355468,26.0992201538203,26.5340934627341,
26.9689667714994,27.4038400801166,27.838713388586,28.2735866969081,28.7084600050832,
29.143333313112,29.5782066209952,30.0130799287334,30.4479532363275,30.8828265437783,
31.3185525442794,31.7542785447804,32.1891518519474,32.6240251589741,33.0588984658616,
33.4937717726112,33.928645079224,34.3635183857014,34.7983916920448,35.2332649982556,
35.6681383043353,36.1030116102854,36.5378849161076,36.9727582218035,37.4076315273749,
37.8425048328235,38.2782308323341,38.7139568318446,39.1488301370532,39.5837034421446,
40.0185767471208,40.4534500519838,40.8883233567357,41.3231966613787,41.7580699659148,
42.1929432703463,42.6278165746754,43.0626898789044,43.4975631830356,43.9324364870714,
44.3673097910142,44.8021830948664,45.2379090935952,45.673635092324,46.1085083960024,
46.5433816995978,46.9782550031127,47.4131283065497,47.8480016099115,48.2828749132006,
48.7177482164198,49.1526215195718,49.5874948226593,50.0223681256851,50.457241428652,
50.8921147315628,51.3269880344203,51.7618613372274,52.197587335454,52.6333133336805,
53.0681866363954,53.5030599390685,53.9379332417027,54.3728065443011,54.8076798468664,
55.2425531494018,55.6774264519101,56.1122997543943,56.5471730568575,56.9820463593026,
57.4169196617326,57.8517929641506,58.2866662665595,58.7215395689624,59.157265567009,
59.5929915650557,60.0278648674556,60.4627381698584,60.8976114722673,61.3324847746853,
61.7673580771153,62.2022313795604,62.6371046820236,63.0719779845079,63.5068512870162,
63.9417245895516,64.376597892117,64.8114711947155,65.2463444973499,65.6812178000231,
66.1169437982275,66.5526697964318,66.9875430991915,67.4224164019987,67.8572897048563,
68.2921630077673,68.7270363107343,69.1619096137603,69.5967829168479,70.0316562200001,
70.4665295232194,70.9014028265087,71.3362761298705,71.7711494333077,72.2060227368227,
72.6408960404182,73.0766220391044,73.5123480377905,73.9472213415547,74.382094645407,
74.8169679493499,75.2518412533859,75.6867145575172,76.1215878617464,76.5564611660756,
76.9913344705072,77.4262077750435,77.8610810796866,78.2959543844386,78.7308276893018,
79.1657009942781,79.6005742993696,80.0363002988208,80.4720262982719,80.9068996035997,
81.3417729090484,81.7766462146199,82.211519520316,82.6463928261383,83.0812661320886,
83.5161394381684,83.9510127443794,84.3858860507229,84.8207593572004,85.2556326638134,
85.6905059705631,86.1253792774507,86.5602525844776,86.995978584908,87.4317045853384,
87.8665778926469,88.3014512000977,88.7363245076919,89.1711978154302,89.6060711233134,
90.0409444313423,90.4758177395175,90.9106910478396,91.345564356309,91.7804376649263,
92.2153109736917,92.6501842826055,93.085057591668,93.5199309008791,93.9556569024059,
94.3913829039327,94.8262562134414,95.2611295230986,95.6960028329042,96.1308761428578,
96.5657494529591,97.0006227632077,97.4354960736028,97.870369384144,98.3052426948304,
98.7401160056612,99.1749893166354,99.6098626277522,100.04473593901,100.915335253024,
101.351061255639,101.785934567313,102.220807879124,102.655681191068,103.090554503145,
103.525427815353,104.395174440154,105.264921065453,105.699794378283,106.134667691232,
106.569541004295,107.004414317471,107.8750136343,108.745612951339,109.615359578629,
110.485106206296,111.354852834309,112.224599462639,113.094346091254,113.964092720119,
114.834692038763,115.705291357499,116.575037986826,117.444784616267,118.314531245777,
119.184277875311,120.054024504821,120.923771134261,121.794370453112,122.66496977189,
123.534716400968,124.404463029834,125.274209658448,126.143956286779,127.013702914792,
127.883449542458,128.754048859798,129.624648176939,130.494394803617,131.364141429857,
132.233888055637,133.103634680937,133.973381305737,134.843127930023,135.71372724472,
136.584326559147,137.019199870684,137.454073182083,137.888946493341,138.323819804458,
139.193566426263,140.063313047491,140.498186357887,140.933059668136,141.367932978237,
141.802806288191,142.237679597997,142.673405599673,143.109131601348,143.544004910857,
143.978878220217,144.413751529429,144.848624838491,145.283498147405,145.718371456171,
146.153244764789,146.588118073258,147.022991381581,147.457864689756,147.892737997785,
148.327611305669,148.762484613407,149.197357921002,149.633083921574,150.068809922147,
150.503683229455,150.938556536623,151.37342984365,151.808303150538,152.243176457288,
152.678049763901,153.112923070379,153.547796376722,153.982669682934,154.417542989014,
154.852416294964,155.287289600787,155.722162906483,156.157036212055,156.592762211626,
157.028488211198,157.463361516526,157.898234821735,158.333108126826,158.767981431803,
159.202854736666,159.637728041419,160.072601346062,160.507474650599,160.94234795503,
161.37722125936,161.812094563589,162.246967867721,162.681841171757,163.1167144757,
163.552440474473,163.988166473247,164.423039777011,164.85791308069,165.292786384286,
165.727659687801,166.162532991238,166.597406294601,167.03227959789,167.46715290111,
167.902026204262,168.33689950735,168.771772810376,169.206646113343,169.641519416254,
170.076392719112,170.512118717363,170.947844715614,171.382718018374,171.817591321089,
172.252464623762,172.687337926397,173.122211228996,173.557084531561,173.991957834097,
174.426831136606,174.86170443909,175.296577741554,175.731451044,176.16632434643,
176.601197648848,177.036070951258,177.471796949306,177.907522947355,178.342396249755,
178.777269552155,179.212142854558,179.647016156968,180.081889459386,180.516762761816,
180.951636064262,181.386509366726,181.82138266921,182.256255971719,182.691129274255,
183.12600257682,183.560875879419,183.995749182054,184.431475180237,184.867201178421,
185.302074481136,185.736947783896,186.171821086704,186.606694389561,187.041567692473,
187.47644099544,187.911314298466,188.346187601554,188.781060904706,189.215934207926,
189.650807511215,190.085680814577,190.520554118015,190.95542742153,191.391153420175,
191.82687941882,192.261752722499,192.696626026263,193.131499330116,193.566372634059,
194.001245938095,194.436119242227,194.870992546456,195.305865850785,195.740739155217,
196.175612459754,196.610485764397,197.045359069149,197.480232374013,197.915105678989,
198.350831678382,198.786557677775,199.221430982984,199.656304288312,200.091177593761,
200.526050899333,200.960924205029,201.395797510852,201.830670816802,202.265544122882,
202.700417429093,203.135290735437,203.570164041915,204.005037348528,204.439910655278,
204.874783962166,205.310509962526,205.746235962887,206.181109270054,206.615982577363,
207.050855884814,207.485729192409,207.920602500147,208.355475808031,208.79034911606,
209.225222424235,209.660095732558,210.094969041027,210.529842349645,210.96471565841,
211.399588967324,211.834462276387,212.27018827784,212.705914279292,213.140787588653,
213.575660898161,214.010534207819,214.880280827579,215.31515413768,215.750027447929,
216.184900758324,216.619774068866,217.054647379553,217.489520690384,218.359267312475,
219.22986662628,219.665592628826,220.100465940363,220.535339252038,220.970212563848,
221.83995918787,222.709705812416,223.579452437468,224.014325750179,224.44919906301,
225.318945689022,226.189545005688,227.060144322571,227.929890949664,228.799637577146,
229.66938420499,230.539130833166,231.408877461643,232.278624090388,233.149223408954,
234.019822727623,234.889569356878,235.759315986267,236.629062615749,237.498809245277,
238.368555874806,239.238302504287,240.108901823183,240.979501142017,241.849247771189,
242.718994400167,243.588741028911,244.458487657389,245.328234285565,246.197980913409,
247.068580230891,247.939179548182,248.80892617507,249.678672801532,250.548419427545,
251.418166053087,252.287912678139,253.157659302684,254.028258617581,254.898857932211,
255.333731243885,255.768604555423,256.203477866821,256.63835117808,257.508097800171,
258.377844421689,258.812717732231,259.247591042627,259.682464352876,260.117337662977,
260.552210972931,260.987936974682,261.858536286089,262.293409595598,262.728282904958,
263.16315621417,263.598029523233,264.032902832147,264.467776140913,264.902649449531,
265.337522758001,265.772396066323,266.207269374499,266.642142682528,267.077015990412,
267.511889298151,267.947615298795,268.383341299439,268.81821460689,269.2530879142,
269.687961221367,270.122834528394,270.557707835282,270.992581142032,271.427454448646,
271.862327755124,272.297201061468,272.732074367679,273.166947673759,273.60182097971,
274.036694285533,274.471567591229,274.907293590862,275.343019590495,275.777892895944,
276.212766201272,276.647639506481,277.082512811573,277.51738611655,277.952259421414,
278.387132726166,278.82200603081,279.256879335346,279.691752639779,280.126625944108,
280.561499248338,280.996372552469,281.431245856506,281.866971855324,282.302697854143,
282.737571157996,283.172444461761,283.60731776544,284.042191069036,284.477064372551,
284.911937675989,285.346810979351,285.781684282641,286.216557585861,286.651430889013,
287.086304192101,287.521177495128,287.956050798095,288.390924101007,288.826650099283,
289.262376097559,289.697249400366,290.132122703127,290.566996005842,291.001869308516,
291.43674261115,291.871615913749,292.306489216315,292.741362518851,293.17623582136,
293.611109123845,294.045982426308,294.480855728754,294.915729031185,295.350602333603,
295.786328331655,296.222054329707,296.65692763211,297.091800934511,297.526674236911,
297.961547539314,298.396420841724,298.831294144142,299.266167446573,299.701040749018,
300.135914051482,300.570787353967,301.005660656476,301.440533959012,301.875407261578,
302.310280564177,302.746006562341,303.181732560506,303.616605863179,304.051479165895,
304.486352468655,304.921225771462,305.35609907432,305.790972377232,306.225845680199,
306.660718983226,307.095592286314,307.530465589466,307.965338892686,308.400212195976,
308.835085499338,309.269958802776,309.705684801381,310.141410799985,310.576284103581,
311.01115740726,311.446030711025,311.880904014878,312.315777318821,312.750650622858,
313.185523926989,313.620397231219,314.055270535549,314.490143839981,314.925017144517,
315.359890449161,315.794763753913,316.229637058777,316.665363058112,317.101089057448,
317.53596236254,317.970835667749,318.405708973077,318.840582278526,319.275455584098,
319.710328889795,320.145202195618,320.580075501568,321.014948807648,321.44982211386,
321.884695420204,322.319568726682,322.754442033295,323.189315340045,323.625041340336,
324.060767340628,324.495640647655,324.930513954822,325.365387262131,325.800260569583,
326.235133877177,326.670007184916,327.1048804928,327.539753800829,327.974627109005,
328.409500417327,328.844373725797,329.279247034415,329.714120343181,330.148993652095,
330.584719653474,331.020445654852,331.455318964064,331.890192273424,332.325065582933,
332.759938892591,333.194812202397,333.629685512351,334.064558822453,334.499432132702,
334.934305443098,335.369178753639,335.804052064326,336.673798686132,337.108671997249,
337.544397999725,337.980124002201,338.4149973136,338.849870625137,339.284743936812,
340.154490560568,341.024237184854,341.459110497191,341.893983809655,342.328857122244,
342.763730434955,343.633477060735,344.504076377234,345.374675693955,346.244422320844,
347.114168948136,347.983915575803,348.853662203817,349.723408832148,350.593155460764,
351.463754779246,352.334354097839,353.204100727012,354.07384735634,354.943593985781,
355.813340615292,356.683087244827,357.552833874338,358.423433193272,359.294032512154,
360.163779141409,361.033525770489,361.903272399355,362.77301902797,363.642765656301,
364.512512284316,365.383111601936,366.253710919371,367.123457546465,367.993204173143,
368.862950799383,369.732697425164,370.602444050463,371.472190675265,372.342789990359,
373.21338930519,373.648262617,374.083135928675,374.952882551611,375.822629173987,
376.257502484962,376.692375795793,377.12724910648,377.562122417021,377.996995727417,
378.431869037666,378.866742347767,379.302468349591,379.738194351416,380.173067661222,
380.607940970879,381.042814280388,381.477687589749,381.91256089896,382.347434208023,
382.782307516937,383.217180825703,383.652054134321,384.086927442791,384.521800751113,
384.956674059289,385.391547367318,385.826420675202,386.262146675918,386.697872676635,
387.13274598423,387.567619291681,388.00249259899,388.437365906157,388.872239213185,
389.307112520073,389.741985826823,390.176859133436,390.611732439914,391.046605746258,
391.48147905247,391.91635235855,392.351225664501,392.786098970323,393.221824970019,
393.657550969714,394.092424275286,394.527297580735,394.962170886063,395.397044191272,
395.831917496364,396.266790801341,396.701664106204,397.136537410957,397.5714107156,
398.006284020137,398.441157324569,398.876030628899,399.310903933128,399.74577723726,
400.181503236126,400.617229234991,401.052102538934,401.486975842787,401.921849146551,
402.356722450231,402.791595753827,403.226469057342,403.66134236078,404.096215664142,
404.531088967432,404.965962270651,405.400835573804,405.835708876892,406.270582179918,
406.705455482886,407.141181481189,407.576907479491,408.01178078235,408.446654085157,
408.881527387917,409.316400690633,409.751273993306,410.186147295941,410.62102059854,
411.055893901106,411.490767203642,411.925640506151,412.360513808636,412.795387111099,
413.230260413545,413.665133715976,414.100859714032,414.536585712088,414.971459014498,
415.406332316901,415.841205619301,416.276078921702,416.710952224105,417.145825526515,
417.580698828933,418.015572131364,418.45044543381,418.885318736273,419.320192038758,
419.755065341267,420.189938643803,420.624811946369,421.060537944515,421.496263942662,
421.931137245297,422.36601054797,422.800883850686,423.235757153446,423.670630456253,
424.105503759112,424.540377062023,424.975250364991,425.410123668017,425.844996971105,
426.279870274258,426.714743577477,427.149616880767,427.584490184129,428.020216182695,
428.455942181261,428.890815484776,429.325688788373,429.760562092052,430.195435395816,
430.630308699669,431.065182003612,431.500055307649,431.93492861178,432.36980191601,
432.80467522034,433.239548524772,433.674421829309,434.109295133952,434.544168438705,
434.979894437984,435.415620437262,435.850493742239,436.285367047331,436.72024035254,
437.155113657869,437.589986963318,438.024860268889,438.459733574586,438.894606880409,
439.32948018636,439.76435349244,440.199226798651,440.634100104995,441.068973411473,
441.503846718087,441.939572718309,442.375298718531,442.810172025419,443.245045332447,
443.679918639614,444.114791946923,444.549665254374,444.984538561969,445.419411869708,
445.854285177591,446.289158485621,446.724031793796,447.158905102119,447.593778410589,
448.028651719207,448.463525027973,448.899251029277,449.334977030581,449.769850339644,
450.639596958216,451.074470267725,451.509343577383,451.944216887189,452.379090197143,
452.813963507244,453.248836817493,453.683710127889,454.118583438431,454.553456749117,
454.988330059949,455.423203370923,455.858929373329,456.294655375734,456.729528686993,
457.164401998391,457.599275309929,458.469021933414,458.90389524536,459.338768557437,
459.773641869646,460.208515181983,460.643388494447,461.078261807036,461.948008432578,
462.818607748906,463.689207065461,464.55895369214,465.428700319234,466.298446946716,
467.16819357456,468.037940202737,468.907686831215,469.778286149605,470.648885468116,
471.518632097196,472.388378726451,473.258125355841,474.127871985322,474.997618614851,
475.86736524438,476.737964563343,477.608563882265,478.478310511593,479.348057140765,
480.217803769743,481.087550398488,481.957297026966,482.827043655142,483.697642972895,
484.568242290469,485.43798891776,486.307735544649,487.177482171112,488.047228797125,
488.916975422667,489.78672204772,490.657321363009,491.09304736596,491.527920678038,
492.397667301793,493.267413925005,494.137160547663,494.57203385878,495.006907169755,
495.441780480586,495.876653791273,496.311527101814,496.74640041221,497.616999724357,
498.052725726255,498.487599036209,498.922472346015,499.357345655673,499.792218965182,
500.227092274542,500.661965583754,501.096838892816,501.531712201731,501.966585510497,
502.401458819114,502.836332127584,503.271205435907,503.706078744082,504.140952052112,
504.576678052901,505.01240405369,505.447277361429,505.882150669023,506.317023976474,
506.751897283783,507.186770590951,507.621643897978,508.056517204866,508.491390511616,
508.92626381823,509.361137124708,509.796010431052,510.230883737263,510.665757043344,
511.100630349294,511.536356349053,511.972082348811,512.406955654506,512.841828960076,
513.276702265523,513.711575570849,514.146448876056,514.581322181146,515.016195486121,
515.451068790983,515.885942095733,516.320815400375,516.75568870491,517.19056200934,
517.625435313668,518.060308617896,518.496034616807,518.931760615718,519.366633919752,
519.801507223694,520.236380527545,520.671253831307,521.106127134985,521.541000438579,
521.975873742092,522.410747045528,522.845620348888,523.280493652176,523.715366955394,
524.150240258545,524.585113561631,525.019986864656,525.455712862985,525.891438861313,
526.326312164223,526.761185467079,527.196058769885,527.630932072643,528.065805375356,
528.500678678029,528.935551980661,529.370425283258,529.805298585822,530.240171888356,
530.675045190863,531.109918493346,531.544791795808,531.979665098252,532.415391096312,
532.851117094373,533.285990396789,533.720863699197,534.155737001598,534.590610303997,
535.025483606395,535.460356908796,535.895230211204,536.330103513621,536.764976816049,
537.199850118493,537.634723420955,538.069596723438,538.504470025945,538.93934332848,
539.375069326608,539.810795324736,540.245668627333,540.680541929966,541.115415232637,
541.550288535351,541.985161838109,542.420035140915,542.854908443771,543.28978174668,
543.724655049646,544.15952835267,544.594401655757,545.029274958907,545.464148262125,
545.899021565413,546.334747563939,546.770473562465,547.205346865901,547.640220169415,
548.075093473009,548.509966776686,548.944840080449,549.3797133843,549.814586688241,
550.249459992276,550.684333296405,551.119206600633,551.554079904961,551.988953209391,
552.423826513926,552.858699818567,553.294425817789,553.73015181701,554.165025121872,
554.599898426846,555.034771731937,555.469645037144,555.90451834247,556.339391647917,
556.774264953487,557.209138259182,557.644011565003,558.078884870951,558.51375817703,
558.948631483239,559.383504789581,559.818378096058,560.254104096209,560.689830096361,
561.12470340311,561.559576709996,561.994450017021,562.429323324187,562.864196631494,
563.299069938943,563.733943246536,564.168816554273,564.603689862154,565.038563170182,
565.473436478355,565.908309786676,566.343183095144,566.77805640376,567.213782404988,
567.649508406216,568.084381715128,568.519255024189,568.954128333399,569.389001642757,
569.823874952264,570.258748261921,570.693621571725,571.128494881677,571.563368191777,
572.433114812417,572.867988122957,573.302861433642,573.737734744471,574.173460746804,
574.609186749136,575.044060060251,575.913806682904,576.783553306113,577.218426617922,
577.653299929865,578.08817324194,578.523046554147,579.392793178944,580.26253980424,
581.13313912039,581.568865123709,582.003738436771,582.87348506323,583.743231690115,
584.612978317402,585.482724945065,586.352471573076,587.222218201403,588.092817519691,
588.963416838109,589.833163467083,590.702910096251,591.572656725575,592.442403355013,
593.31214998452,594.181896614051,595.05249593303,595.92309525198,596.792841881366,
597.662588510618,598.532335139693,599.402081768556,600.271828397167,601.141575025495,
602.012174343369,602.882773661074,603.752520288553,604.622266915642,605.492013542317,
606.361760168553,607.23150679433,608.101253419626,608.971852735101,609.842452050322,
610.71219867434,611.581945297822,612.451691920754,612.886565232011,613.321438543126,
613.756311854099,614.191185164928,615.060931786153,615.931531098516,616.367257100486,
616.802130410586,617.237003720538,617.671877030342,618.106750339998,618.541623649505,
618.976496958863,619.411370268073,619.846243577134,620.281116886046,620.71599019481,
621.150863503426,621.585736811894,622.020610120214,622.455483428388,622.891209429248,
623.326935430108,623.761808737989,624.196682045726,624.631555353319,625.066428660769,
625.501301968075,625.936175275241,626.371048582266,626.805921889153,627.240795195901,
627.675668502512,628.110541808988,628.54541511533,628.98028842154,629.415161727618,
629.850887727438,630.286613727259,630.72148703308,631.156360338774,631.591233644344,
632.026106949791,632.460980255118,632.895853560325,633.330726865415,633.76560017039,
634.200473475251,634.635346780002,635.070220084644,635.505093389179,635.939966693609,
636.374839997937,636.810565996897,637.246291995857,637.681165299986,638.116038604021,
638.550911907962,638.985785211813,639.420658515576,639.855531819253,640.290405122847,
640.725278426361,641.160151729796,641.595025033157,642.029898336444,642.464771639662,
642.899644942813,643.334518245899,643.770244244257,644.205970242616,644.640843545581,
645.075716848491,645.510590151347,645.945463454153,646.380336756911,646.815210059625,
647.250083362296,647.684956664929,648.119829967526,648.55470327009,648.989576572624,
649.424449875131,649.859323177614,650.294196480076,650.729922478144,651.165648476212,
651.600521778641,652.035395081057,652.470268383465,652.905141685866,653.340014988265,
653.774888290663,654.209761593065,654.644634895472,655.079508197889,655.514381500318,
655.949254802762,656.384128105224,656.819001407706,657.253874710213,657.689600708326,
658.12532670644,658.560200009004,658.995073311601,659.429946614234,659.864819916905,
660.299693219619,660.734566522377,661.169439825183,661.604313128039,662.039186430948,
662.474059733914,662.908933036938,663.343806340025,663.778679643175,664.213552946393,
664.649278944883,665.085004943373,665.519878246733,665.954751550169,666.389624853683,
666.824498157277,667.259371460954,667.694244764717,668.129118068568,668.563991372509,
668.998864676544,669.433737980674,669.868611284901,670.303484589229,670.738357893659,
671.173231198194,671.608957197361,672.044683196528,672.479556501278,672.91442980614,
673.349303111115,673.784176416205,674.219049721412,674.653923026738,675.088796332185,
675.523669637755,675.95854294345,676.393416249271,676.82828955522,677.263162861298,
677.698036167508,678.13290947385,678.568635473934,679.004361474018,679.439234780629,
679.874108087377,680.308981394264,680.743854701289,681.178728008455,681.613601315762,
682.048474623211,682.483347930804,682.91822123854,683.353094546422,683.78796785445,
684.222841162623,684.657714470944,685.092587779412,685.528313780566,685.96403978172,
686.398913090483,686.833786399396,687.268659708457,687.703533017666,688.138406327025,
688.573279636532,689.008152946187,689.443026255992,689.877899565944,690.312772876043,
690.74764618629,691.182519496684,691.617392807224,692.052266117909,692.487992120169,
692.92371812243,693.358591433403,694.228338055774,694.663211367171,695.098084678707,
695.532957990379,695.967831302188,696.402704614131,696.837577926207,697.707324550749,
698.577071175797,699.011944488507,699.447670491767,699.883396495028,700.318269807975,
701.188016434211,702.057763060886,702.927509687976,703.797256315454,704.667002943295,
705.536749571467,706.407348889651,707.277948207973,708.147694836835,709.017441465911,
709.887188095163,710.756934724548,711.626681354026,712.496427983551,713.367027302543,
714.237626621516,715.107373250954,715.977119880277,716.846866509446,717.716613138419,
718.586359767161,719.456106395635,720.32670571363,721.197305031464,722.067051659126,
722.936798286414,723.806544913299,724.676291539758,725.546038165767,726.415784791305,
727.286384106969,728.156983422381,729.026730046663,729.896476670415,730.331349982088,
730.766223293624,731.201096605021,731.635969916278,732.505716538366,733.37546315988,
733.81033647042,734.246062472462,734.681788474505,735.116661784752,735.551535094852,
735.986408404804,736.421281714608,736.856155024264,737.291028333771,737.72590164313,
738.160774952339,738.5956482614,739.030521570312,739.465394879076,739.900268187692,
740.33514149616,740.77001480448,741.205740805414,741.641466806347,742.076340114374,
742.511213422256,742.946086729993,743.380960037585,743.815833345035,744.250706652341,
744.685579959507,745.120453266533,745.555326573419,745.990199880167,746.425073186778,
746.859946493254,747.294819799596,747.729693105806,748.165419105691,748.601145105576,
749.036018411525,749.470891717346,749.90576502304,750.34063832861,750.775511634057,
751.210384939384,751.645258244591,752.080131549682,752.515004854656,752.949878159518,
753.384751464269,753.81962476891,754.254498073445,754.689371377875,755.125097376885,
755.560823375895,755.995696680123,756.430569984253,756.865443288287,757.300316592228,
757.735189896079,758.170063199842,758.604936503519,759.039809807113,759.474683110627,
759.909556414062,760.344429717423,760.779303020711,761.214176323929,761.649049627079,
762.084775625469,762.520501623858,762.955374926883,763.390248229848,763.825121532758,
764.259994835614,764.694868138419,765.129741441178,765.564614743891,765.999488046563,
766.434361349196,766.869234651793,767.304107954357,767.738981256891,768.173854559398,
768.608727861881,769.044453859958,769.480179858035,769.915053160479,770.349926462907,
770.784799765324,771.219673067731,771.654546370133,772.089419672531,772.52429297493,
772.959166277331,773.394039579739,773.828912882155,774.263786184584,774.698659487028,
775.13353278949,775.568406091973,776.004132090072,776.439858088172,776.874731390706,
777.30960469327,777.744477995867,778.1793512985,778.614224601171,779.049097903885,
779.483971206643,779.918844509449,780.353717812305,780.788591115215,781.22346441818,
781.658337721205,782.093211024291,782.528084327442,782.963810325897,783.399536324352,
783.834409627639,784.269282931,784.704156234435,785.139029537949,785.573902841543,
786.00877614522,786.443649448983,786.878522752834,787.313396056775,787.74826936081,
788.183142664939,788.618015969167,789.052889273495,789.487762577925,789.923488577038,
790.359214576152,790.794087880793,791.228961185544,791.663834490406,792.098707795381,
792.533581100471,792.968454405678,793.403327711004,793.838201016451,794.273074322021,
794.707947627716,795.142820933537,795.577694239486,796.012567545564,796.447440851774,
796.883166851791,797.318892851808,797.753766158284,798.188639464895,798.623512771643,
799.058386078529,799.493259385555,799.92813269272,800.363006000027,800.797879307477,
801.232752615069,801.667625922806,802.102499230688,802.537372538715,802.972245846889,
803.40711915521,803.84284515629,804.27857115737,804.713444465985,805.148317774749,
805.583191083662,806.018064392723,806.452937701933,806.887811011291,807.322684320798,
808.192430940258,808.62730425021,809.06217756031,809.497050870557,809.931924180951,
810.36679749149,810.802523493679,811.238249495867,811.673122806697,812.542869428785,
812.977742740041,813.412616051438,813.847489362974,814.282362674646,814.717235986455,
815.152109298398,816.021855922681,816.891602547478,817.326475860065,817.762201863265,
818.197927866466,818.632801179295,819.502547805304,820.372294431763,821.242041058648,
822.111787685935,822.981534313598,823.851280941609,824.721880259681,825.5924795779,
826.462226206642,827.331972835616,828.201719464785,829.071466094109,829.941212723546,
830.810959353053,831.681558672047,832.552157991036,833.421904620514,834.2916512499,
835.161397879151,836.031144508226,836.900891137089,837.770637765701,838.641237083811,
839.511836401767,840.381583029608,841.251329657086,842.121076284176,842.990822910851,
843.860569537087,844.730316162863,845.600915478712,846.471514794314,847.341261418855,
848.211008042874,848.645881354683,849.080754666356,849.515627977891,849.950501289288,
850.82024791166,851.689994533462,852.124867844147,852.560593846263,852.996319848379,
853.431193158772,853.866066469019,854.300939779119,855.170686398875,855.605559708531,
856.040433018038,856.475306327397,856.910179636606,857.345052945667,857.77992625458,
858.214799563344,858.64967287196,859.084546180427,859.520272181434,859.95599818244,
860.390871490614,860.825744798641,861.260618106523,861.69549141426,862.130364721852,
862.565238029302,863.000111336609,863.434984643774,863.8698579508,864.304731257686,
864.739604564434,865.174477871045,865.609351177521,866.044224483863,866.479950483814,
866.915676483765,867.350549789843,867.785423095792,868.220296401613,868.655169707307,
869.090043012877,869.524916318325,869.959789623651,870.394662928858,870.829536233948,
871.264409538923,871.699282843785,872.134156148535,872.569029453177,873.003902757712,
873.439628756773,873.875354755834,874.310228060162,874.745101364389,875.179974668519,
875.614847972553,876.049721276495,876.484594580346,876.919467884108,877.354341187786,
877.78921449138,878.224087794893,878.658961098329,879.093834401689,879.528707704977,
879.963581008195,880.399307006616,880.835033005038,881.269906308124,881.704779611148,
882.139652914114,882.574526217024,883.00939951988,883.444272822685,883.879146125444,
884.314019428157,884.748892730829,885.183766033462,885.618639336059,886.053512638623,
886.488385941157,886.923259243664,887.358985241751,887.794711239839,888.2295845423,
888.664457844744,889.099331147173,889.534204449589,889.969077751997,890.403951054398,
890.838824356797,891.273697659195,891.708570961597,892.143444264004,892.578317566421,
893.01319086885,893.448064171293,893.882937473755,894.318663471843,894.75438946993,
895.189262772437,895.624136074971,896.059009377535,896.493882680132,896.928755982765,
897.363629285437,897.798502588151,898.233375890909,898.668249193715,899.103122496571,
899.53799579948,899.972869102446,900.40774240547,900.842615708556,901.278341706978,
901.714067705399,902.148941008617,902.583814311905,903.018687615265,903.453560918701,
903.888434222214,904.323307525808,904.758180829485,905.193054133248,905.627927437099,
906.06280074104,906.497674045075,906.932547349205,907.367420653433,907.80229395776,
908.238019956821,908.673745955883,909.108619260417,909.543492565059,909.978365869809,
910.413239174671,910.848112479646,911.282985784736,911.717859089943,912.152732395269,
912.587605700716,913.022479006287,913.457352311981,913.892225617802,914.327098923751,
914.761972229829,915.19769822978,915.633424229731,916.068297536072,916.503170842548,
916.93804414916,917.372917455908,917.807790762794,918.24266406982,918.677537376985,
919.112410684292,919.547283991742,919.982157299334,920.417030607071,920.851903914953,
921.28677722298,921.721650531154,922.15737653216,922.593102533167,923.027975841635,
923.46284915025,923.897722459014,924.332595767926,924.767469076987,925.202342386197,
925.637215695556,926.072089005063,926.506962314719,926.941835624523,927.376708934475,
927.811582244575,928.246455554822,928.681328865215,929.117054867331,929.987654180132,
930.422527490961,930.857400801934,931.292274113049,931.727147424306,932.162020735703,
932.596894047238,933.46664067072,934.336387294739,934.771260606945,935.20613391928,
935.641007231742,936.076733234882,936.94733255073,937.817079176507,938.686825802743,
939.556572429418,940.426319056508,941.296065683986,942.165812311827,943.036411629783,
943.907010947893,944.776757576505,945.646504205367,946.516250834443,947.385997463694,
948.25574409308,949.125490722558,949.996090041546,950.86668936054,951.736435990048,
952.606182619485,953.475929248809,954.345675877978,955.215422506951,956.085169135693,
956.955768453912,957.826367771985,958.696114399995,959.565861027658,960.435607654946,
961.305354281831,962.175100908289,963.044847534298,963.915446850328,964.786046166116,
965.655792790913,966.525539415195,966.960412727138,967.395286038947,968.265032662155,
969.134779284809,969.569652595924,970.004525906897,970.439399217726,970.875125219914,
971.310851222103,971.745724532643,972.615471153283,973.485217773335,973.920091083139,
974.354964392795,974.789837702302,975.22471101166,975.65958432087,976.094457629931,
976.529330938844,976.964204247608,977.399077556223,977.834803557303,978.270529558383,
978.705402866704,979.140276174877,979.575149482905,980.010022790786,980.444896098523,
980.879769406116,981.314642713565,981.749516020872,982.184389328038,982.619262635063,
983.05413594195,983.489009248698,983.923882555309,984.358755861785,984.794481861802,
985.230207861819,985.665081168029,986.099954474107,986.534827780056,986.969701085877,
987.404574391571,987.839447697141,988.274321002589,988.709194307915,989.144067613122,
989.578940918212,990.013814223187,990.448687528048,990.883560832799,991.31843413744,
991.754160136554,992.189886135667,992.624759440097,993.059632744425,993.494506048653,
993.929379352783,994.364252656817,994.799125960758,995.233999264609,995.668872568372,
996.103745872049,996.538619175643,996.973492479157,997.408365782593,997.843239085953,
998.278112389241,998.713838387696,999.149564386151,999.584437689301,1000.01931099239,
1000.45418429541,1000.88905759838,1001.32393090129,1001.75880420414,1002.19367750695,
1002.62855080971,1003.06342411242,1003.49829741509,1003.93317071773,1004.36804402032,
1004.80291732289,1005.23779062542,1005.67351662352,1006.10924262162,1006.5441159241,
1006.97898922656,1007.41386252901,1007.84873583144,1008.28360913385,1008.71848243626,
1009.15335573866,1009.58822904106,1010.02310234346,1010.45797564586,1010.89284894827,
1011.32772225069,1011.76259555311,1012.19746885556,1012.63319485364,1013.06892085171,
1013.5037941542,1013.9386674567,1014.37354075924,1014.8084140618,1015.2432873644,
1015.67816066703,1016.1130339697,1016.54790727242,1016.98278057517,1017.41765387798,
1017.85252718084,1018.28740048375,1018.72227378671,1019.15714708974,1019.59287308813,
1020.02859908651,1020.46347238967,1020.89834569288,1021.33321899617,1021.76809229953,
1022.20296560297,1022.63783890648,1023.07271221007,1023.50758551375,1023.94245881752,
1024.37733212137,1024.81220542531,1025.24707872935,1025.68195203348,1026.11682533771,
1026.55255133672,1026.98827733573,1027.42315064016,1027.8580239447,1028.29289724934,
1028.72777055409,1029.16264385896,1029.59751716393,1030.03239046902,1030.46726377423,
1030.90213707956,1031.33701038501,1031.77188369058,1032.20675699628,1032.6416303021,
1033.07650360805,1033.51222960793,1033.94795560782,1034.38282891403,1034.81770222038,
1035.25257552685,1035.68744883347,1036.12232214022,1036.5571954471,1036.99206875413,
1037.4269420613,1037.86181536861,1038.29668867606,1038.73156198365,1039.16643529139,
1039.60130859927,1040.0361819073,1040.47190790824,1040.90763390917,1041.34250721749,
1041.77738052596,1042.21225383458,1042.64712714334,1043.08200045226,1043.95174707053,
1044.38662037989,1044.8214936894,1045.25636699906,1045.69124030886,1046.12611361882,
1046.56098692892,1046.99586023917,1047.43158624121,1047.86731224325,1048.3021855538,
1048.73705886448,1049.17193217531,1049.60680548629,1050.0416787974,1050.47655210866,
1050.91142542006,1051.78117204327,1052.21604535508,1052.65091866703,1053.0857919791,
1053.52066529131,1053.95553860365,1054.39126460673,1055.26186392239,1056.13161054793,
1057.00135717395,1057.43623048712,1057.87110380041,1058.7408504273,1059.61059705459,
1060.48034368225,1061.35094300009,1062.22154231809,1063.09128894656,1063.96103557531,
1064.83078220429,1065.70052883346,1066.57027546278,1067.44002209222,1068.3106214112,
1069.18122073019,1070.05096735972,1070.9207139892,1071.79046061859,1072.66020724785,
1073.52995387693,1074.39970050579,1075.27029982411,1076.1408991423,1077.01064577048,
1077.88039239832,1078.7501390258,1079.61988565289,1080.48963227957,1081.35937890581,
1082.22997822202,1083.100577538,1083.97032416305,1084.84007078759,1085.70981741161,
1086.5795640351,1087.44931065803,1087.88418396929,1088.31905728041,1088.75393059138,
1089.18965659365,1089.62538259591,1090.06025590659,1090.93000252753,1091.36487583778,
1091.79974914788,1092.23462245783,1092.66949576764,1093.1043690773,1093.5392423868,
1093.97411569616,1094.40898900538,1094.84386231444,1095.27873562335,1095.71360893212,
1096.14933493327,1096.58506093443,1097.0199342429,1097.45480755122,1097.88968085939,
1098.32455416742,1098.75942747531,1099.19430078305,1099.62917409064,1100.06404739809,
1100.4989207054,1100.93379401257,1101.36866731959,1101.80354062648,1102.23841393323,
1102.67328723984,1103.10901323993,1103.54473924001,1103.97961254636,1104.41448585257,
1104.84935915865,1105.2842324646,1105.71910577042,1106.15397907612,1106.58885238169,
1107.02372568714,1107.45859899246,1107.89347229767,1108.32834560276,1108.76321890774,
1109.1980922126,1109.63296551736,1110.06869151652,1110.50441751569,1110.93929082023,
1111.37416412466,1111.80903742899,1112.24391073322,1112.67878403735,1113.11365734139,
1113.54853064533,1113.98340394918,1114.41827725295,1114.85315055662,1115.28802386022,
1115.72289716374,1116.15777046717,1116.59264377053,1117.02836976903,1117.46409576752,
1117.89896907074,1118.33384237389,1118.76871567698,1119.20358898,1119.63846228297,
1120.07333558588,1120.50820888874,1120.94308219154,1121.3779554943,1121.81282879702,
1122.24770209969,1122.68257540233,1123.11744870492,1123.55232200749,1123.98804800561,
1124.42377400372,1124.85864730623,1125.29352060871,1125.72839391118,1126.16326721362,
1126.59814051605,1127.03301381847,1127.46788712088,1127.90276042328,1128.33763372568,
1128.77250702808,1129.20738033048,1129.64225363289,1130.07712693531,1130.51200023774,
1130.94772623581,1131.38345223388,1131.81832553634,1132.25319883883,1132.68807214134,
1133.12294544387,1133.55781874644,1133.99269204904,1134.42756535167,1134.86243865434,
1135.29731195706,1135.73218525982,1136.16705856263,1136.60193186548,1137.03680516839,
1137.47167847136,1137.90740446972,1138.34313046808,1138.77800377117,1139.21287707432,
1139.64775037754,1140.08262368083,1140.51749698419,1140.95237028763,1141.38724359114,
1141.82211689474,1142.25699019842,1142.69186350218,1143.12673680603,1143.56161010998,
1143.99648341401,1144.43135671814,1144.86708271711,1145.30280871607,1145.7376820204,
1146.17255532483,1146.60742862936,1147.04230193401,1147.47717523876,1147.91204854362,
1148.3469218486,1148.78179515369,1149.2166684589,1149.65154176423,1150.08641506968,
1150.52128837525,1150.95616168094,1151.39103498677,1151.82676098659,1152.26248698641,
1152.69736029249,1153.1322335987,1153.56710690504,1154.00198021152,1154.43685351813,
1154.87172682488,1155.30660013177,1155.7414734388,1156.17634674597,1156.61122005327,
1157.04609336073,1157.48096666832,1157.91583997606,1158.35071328394,1158.7864392848,
1159.22216528566,1159.65703859384,1160.09191190216,1160.52678521063,1160.96165851925,
1161.39653182801,1161.83140513693,1162.26627844599,1162.7011517552,1163.13602506456,
1163.57089837407,1164.00577168373,1164.44064499353,1164.87551830349,1165.74611761556,
1166.18184361753,1166.61671692792,1167.05159023846,1167.48646354915,1167.92133685998,
1168.35621017096,1169.22595679333,1170.09570341627,1170.53057672794,1170.96545003975,
1171.4003233517,1171.83519666377,1172.27006997598,1172.705795979,1173.57639529447,
1174.44614191977,1174.8810152326,1175.31588854555,1176.18563517179,1177.05538179847,
1177.92512842556,1178.79487505304,1179.66547437075,1180.53607368863,1181.40582031696,
1182.27556694557,1183.14531357444,1184.01506020352,1184.88480683277,1185.75455346216,
1186.62515278112,1187.4957521001,1188.36549872963,1189.23524535914,1190.10499198858,
1190.97473861791,1191.84448524708,1192.71423187606,1193.58483119448,1194.45543051277,
1195.3251771411,1196.19492376911,1197.06467039678,1197.93441702407,1198.80416365096,
1199.67391027742,1200.5445095938,1201.41510890996,1202.28485553525,1203.15460216005,
1204.02434878434,1204.89409540809,1205.76384203131,1206.1987153427,1206.63358865396,
1207.06846196508,1207.50418796741,1208.37478728058,1209.2445339018,1209.6794072122,
1210.11428052245,1210.54915383255,1210.9840271425,1211.41890045231,1211.85377376197,
1212.28864707147,1212.72352038083,1213.15839369005,1213.59326699911,1214.02814030802,
1214.46386630925,1214.89959231048,1215.3344656191,1215.76933892757,1216.20421223589,
1216.63908554406,1217.07395885209,1217.50883215998,1217.94370546771,1218.37857877531,
1218.81345208276,1219.24832539007,1219.68319869724,1220.11807200426,1220.55294531115,
1220.9878186179,1221.42354461805,1221.85927061821,1222.29414392468,1222.72901723103,
1223.16389053724,1223.59876384332,1224.03363714927,1224.46851045509,1224.90338376079,
1225.33825706636,1225.77313037181,1226.20800367713,1226.64287698234,1227.07775028743,
1227.51262359241,1227.94749689727,1228.3832228965,1228.81894889572,1229.25382220036,
1229.6886955049,1230.12356880933,1230.55844211366,1230.99331541789,1231.42818872202,
1231.86306202606,1232.29793533,1232.73280863385,1233.16768193762,1233.60255524129,
1234.03742854489,1234.4723018484,1234.90717515184,1235.34290115037,1235.7786271489,
1236.21350045219,1236.64837375541,1237.08324705856,1237.51812036165,1237.95299366467,
1238.38786696764,1238.82274027055,1239.25761357341,1239.69248687621,1240.12736017897,
1240.56223348169,1240.99710678436,1241.431980087,1241.8668533896,1242.30257938773,
1242.73830538585,1243.17317868839,1243.6080519909,1244.04292529338,1244.47779859585,
1244.91267189829,1245.34754520072,1245.78241850314,1246.21729180555,1246.65216510795,
1247.08703841035,1247.52191171275,1247.95678501515,1248.39165831756,1248.82653161998,
1249.26225761804,1249.69798361611,1250.13285691855,1250.56773022101,1251.0026035235,
1251.43747682601,1251.87235012854,1252.30722343111,1252.74209673371,1253.17697003634,
1253.61184333901,1254.04671664173,1254.48158994449,1254.9164632473,1255.35133655015,
1255.78620985306,1256.22193585139,1256.65766184973,1257.09253515275,1257.52740845584,
1257.96228175899,1258.39715506221,1258.8320283655,1259.26690166886,1259.7017749723,
1260.13664827581,1260.57152157941,1261.00639488309,1261.44126818685,1261.8761414907,
1262.31101479465,1262.74588809868,1263.1816140976,1263.61734009651,1264.05221340074,
1264.48708670507,1264.9219600095,1265.35683331403,1265.79170661868,1266.22657992343,
1266.66145322829,1267.09632653327,1267.53119983836,1267.96607314357,1268.4009464489,
1268.83581975434,1269.27069305992,1269.70556636561,1270.14129236537,1270.57701836513,
1271.01189167108,1271.44676497716,1271.88163828337,1272.31651158971,1272.75138489619,
1273.1862582028,1273.62113150955,1274.05600481644,1274.49087812347,1274.92575143063,
1275.36062473794,1275.79549804539,1276.23037135299,1276.66524466073,1277.10097066151,
1277.5366966623,1277.97156997033,1278.40644327851,1278.84131658683,1279.2761898953,
1279.71106320392,1280.14593651268,1280.5808098216,1281.01568313066,1281.45055643987,
1281.88542974923,1282.32030305874,1282.75517636839,1283.1900496782,1283.62492298815,
1284.06064899005,1284.49637499195,1284.9312483022,1285.36612161259,1285.80099492313,
1286.23586823382,1286.67074154465,1287.54048816674,1287.975361478,1288.4102347894,
1288.84510810093,1289.27998141261,1289.71485472442,1290.14972803636,1291.02032735139,
1291.89092666668,1292.32579997914,1292.76067329173,1293.19554660444,1293.63041991727,
1294.50016654328,1295.36991316974,1296.23965979663,1297.10940642392,1297.9800057415,
1298.85060505925,1299.72035168742,1300.5900983159,1301.45984494464,1302.32959157362,
1303.19933820279,1304.06908483212,1304.93968415104,1305.81028347,1306.68003009953,
1307.54977672906,1308.41952335854,1309.28926998793,1310.15901661718,1311.02876324626,
1311.89936256477,1312.76996188316,1313.63970851164,1314.50945513981,1315.37920176765,
1316.24894839514,1317.11869502223,1317.98844164891,1318.85904096546,1319.72964028179,
1320.59938690733,1321.46913353238,1322.33888015692,1323.20862678095,1323.64350009276,
1324.07837340443,1324.51324671597,1324.94812002737,1325.81871934103,1326.68931865441,
1327.12419196524,1327.55906527593,1327.99393858647,1328.42881189686,1328.86368520711,
1329.29855851721,1329.73343182716,1330.16830513697,1330.60317844663,1331.03805175614,
1331.4729250655,1331.90779837471,1332.34267168377,1332.77839768507,1333.21412368638,
1333.64899699514,1334.08387030376,1334.51874361223,1334.95361692055,1335.38849022873,
1335.82336353676,1336.25823684464,1336.69311015238,1337.12798345997,1337.56285676742,
1337.99773007473,1338.4326033819,1338.86747668892,1339.30234999581,1339.73807599603,
1340.17380199625,1340.60867530287,1341.04354860934,1341.47842191569,1341.9132952219,
1342.34816852798,1342.78304183393,1343.21791513975,1343.65278844545,1344.08766175102,
1344.52253505647,1344.95740836179,1345.392281667,1345.82715497209,1346.26202827707,
1346.69775427635,1347.13348027563,1347.56835358038,1348.00322688502,1348.43810018956,
1348.87297349399,1349.30784679832,1349.74272010255,1350.17759340668,1350.61246671072,
1351.04734001466,1351.48221331851,1351.91708662228,1352.35195992595,1352.78683322955,
1353.22170653306,1353.65743253163,1354.09315853019,1354.52803183356,1354.96290513685,
1355.39777844007,1355.83265174322,1356.26752504631,1356.70239834933,1357.1372716523,
1357.57214495521,1358.00701825807,1358.44189156087,1358.87676486363,1359.31163816635,
1359.74651146902,1360.18138477166,1360.6171107698,1361.05283676795,1361.48771007051,
1361.92258337305,1362.35745667556,1362.79232997804,1363.2272032805,1363.66207658295,
1364.09694988538,1364.5318231878,1364.96669649021,1365.40156979261,1365.83644309501,
1366.27131639741,1366.70618969981,1367.14106300222,1367.57678900028,1368.01251499834,
1368.44738830077,1368.88226160321,1369.31713490567,1369.75200820816,1370.18688151067,
1370.6217548132,1371.05662811577,1371.49150141837,1371.926374721,1372.36124802367,
1372.79612132639,1373.23099462915,1373.66586793196,1374.10074123481,1374.53646723311,
1374.97219323142,1375.40706653438,1375.84193983741,1376.2768131405,1376.71168644365,
1377.14655974687,1377.58143305016,1378.01630635352,1378.45117965696,1378.88605296047,
1379.32092626407,1379.75579956775,1380.19067287151,1380.62554617536,1381.06041947931,
1381.49614547817,1381.93187147704,1382.36674478117,1382.8016180854,1383.23649138973,
1383.67136469416,1384.10623799869,1384.54111130334,1384.97598460809,1385.41085791295,
1385.84573121793,1386.28060452302,1386.71547782823,1387.15035113356,1387.585224439,
1388.02009774458,1388.45582374427,1388.89154974397,1389.32642304979,1389.76129635574,
1390.19616966182,1390.63104296803,1391.06591627437,1391.50078958085,1391.93566288746,
1392.37053619421,1392.8054095011,1393.24028280813,1393.6751561153,1394.1100294226,
1394.54490273005,1394.97977603765,1395.41550203836,1395.85122803908,1396.28610134696,
1396.72097465499,1397.15584796317,1397.59072127149,1398.02559457996,1398.46046788858,
1398.89534119734,1399.33021450626,1399.76508781532,1400.19996112453,1400.63483443389,
1401.50458105306,1401.93945436286,1402.37518036469,1402.81090636651,1403.24577967661,
1403.68065298686,1404.11552629725,1404.5503996078,1404.98527291848,1405.85501954029,
1406.2898928514,1406.72476616266,1407.15963947406,1407.5945127856,1408.02938609727,
1408.46425940908,1409.33485872391,1410.205458039,1410.64033135134,1411.07520466381,
1411.51007797639,1411.9449512891,1412.81469791488,1413.68444454112,1414.5541911678,
1415.42393779489,1416.29453711233,1417.16513642995,1418.03488305796,1418.90462968629,
1419.77437631491,1420.64412294377,1421.51386957285,1422.38361620211,1423.25421552099,
1424.12481483992,1424.99456146943,1425.86430809896,1426.73405472847,1427.60380135791,
1428.47354798724,1429.34329461641,1430.21389393501,1431.08449325349,1431.9542398821,
1432.82398651043,1433.69373313844,1434.56347976611,1435.4332263934,1436.30297302029,
1437.17357233701,1438.04417165351,1438.91391827929,1439.78366490459,1440.65341152939,
1441.52315815367,1441.95803146562,1442.39290477743,1442.8277780891,1443.26265140064,
1444.13325071451,1445.00385002811,1445.43872333908,1445.87359664991,1446.3084699606,
1446.74334327114,1447.17821658153,1447.61308989178,1448.48283651184,1448.91770982164,
1449.3525831313,1449.78745644081,1450.22232975017,1450.65720305938,1451.09292906076,
1451.52865506214,1451.96352837105,1452.39840167982,1452.83327498843,1453.2681482969,
1453.70302160522,1454.1378949134,1454.57276822143,1455.00764152931,1455.44251483705,
1455.87738814464,1456.31226145209,1456.7471347594,1457.18200806657,1457.6168813736,
1458.05260737389,1458.48833337418,1458.92320668093,1459.35807998754,1459.79295329402,
1460.22782660036,1460.66269990657,1461.09757321265,1461.5324465186,1461.96731982443,
1462.40219313012,1462.83706643569,1463.27193974114,1463.70681304647,1464.14168635168,
1464.57655965677,1465.0122856561,1465.44801165544,1465.8828849603,1466.31775826505,
1466.7526315697,1467.18750487423,1467.62237817866,1468.05725148299,1468.49212478722,
1468.92699809135,1469.36187139539,1469.79674469933,1470.23161800319,1470.66649130695,
1471.10136461063,1471.53623791422,1471.97196391283,1472.40768991143,1472.84256321487,
1473.27743651823,1473.71230982152,1474.14718312474,1474.58205642789,1475.01692973098,
1475.451803034,1475.88667633697,1476.32154963988,1476.75642294274,1477.19129624555,
1477.62616954831,1478.06104285102,1478.4959161537,1478.93164215186,1479.36736815002,
1479.80224145262,1480.23711475519,1480.67198805772,1481.10686136023,1481.54173466272,
1481.97660796518,1482.41148126762,1482.84635457005,1483.28122787247,1483.71610117488,
1484.15097447728,1484.58584777968,1485.02072108208,1485.45559438449,1485.89132038254,
1486.32704638059,1486.76191968301,1487.19679298544,1487.63166628788,1488.06653959035,
1488.50141289283,1488.93628619534,1489.37115949787,1489.80603280044,1490.24090610304,
1490.67577940567,1491.11065270835,1491.54552601106,1491.98039931382,1492.41527261663,
1492.8509986149,1493.28672461318,1493.72159791609,1494.15647121906,1494.59134452208,
1495.02621782517,1495.46109112832,1495.89596443154,1496.33083773483,1496.76571103819,
1497.20058434163,1497.63545764515,1498.07033094874,1498.50520425242,1498.94007755618,
1499.37495086004,1499.81067685885,1500.24640285767,1500.68127616171,1501.11614946584,
1501.55102277007,1501.9858960744,1502.42076937883,1502.85564268337,1503.29051598801,
1503.72538929276,1504.16026259762,1504.5951359026,1505.03000920769,1505.4648825129,
1505.89975581823,1506.33462912368,1506.77035512331,1507.20608112294,1507.64095442864,
1508.07582773446,1508.51070104041,1508.94557434649,1509.3804476527,1509.81532095904,
1510.25019426552,1510.68506757213,1511.11994087888,1511.55481418577,1511.9896874928,
1512.42456079996,1512.85943410727,1513.29430741472,1513.73003341537,1514.16575941601,
1514.60063272375,1515.03550603163,1515.47037933966,1515.90525264784,1516.34012595616,
1516.77499926463,1517.20987257325,1517.64474588201,1518.07961919093,1518.51449249999,
1518.9493658092,1519.38423911856,1519.81911242807,1520.25398573772,1520.68971173947,
1521.12543774122,1521.56031105118,1521.99518436128,1522.43005767153,1523.29980429246,
1523.73467760315,1524.16955091398,1524.60442422495,1525.03929753607,1525.47417084733,
1525.90904415873,1526.77879078194,1527.64939009657,1528.08511609939,1528.51998941146,
1528.95486272367,1529.38973603601,1530.25948266106,1531.1292292866,1531.99897591261,
1532.86872253907,1533.73846916596,1534.60906848325,1535.47966780073,1536.34941442858,
1537.21916105675,1538.08890768523,1538.95865431398,1539.82840094295,1540.69814757212,
1541.56874689096,1542.43934620985,1543.30909283933,1544.17883946886,1545.04858609839,
1545.91833272787,1546.78807935726,1547.65782598651,1548.52842530518,1549.39902462375,
1550.26877125249,1551.13851788097,1552.00826450914,1552.87801113699,1553.74775776447,
1554.61750439156,1555.48810370844,1556.35870302511,1557.22844965112,1558.09819627666,
1558.96794290171,1559.83768952626,1560.27256283834,1560.70743615028,1561.57718277377,
1562.44778208785,1563.31838140165,1563.75325471277,1564.18812802374,1564.62300133457,
1565.05787464526,1565.9276212662,1566.79736788655,1567.2322411965,1567.66711450631,
1568.10198781596,1568.53686112547,1568.97173443483,1569.40746043628,1569.84318643774,
1570.2780597468,1570.71293305571,1571.14780636448,1571.5826796731,1572.01755298157,
1572.45242628989,1572.88729959806,1573.32217290609,1573.75704621397,1574.19191952171,
1574.62679282931,1575.06166613676,1575.49653944407,1575.93141275123,1576.36713875159,
1576.80286475195,1577.23773805884,1577.67261136559,1578.1074846722,1578.54235797868,
1578.97723128502,1579.41210459124,1579.84697789732,1580.28185120327,1580.71672450909,
1581.15159781478,1581.58647112036,1582.0213444258,1582.45621773113,1582.89109103634,
1583.32681703573,1583.76254303513,1584.1974163401,1584.63228964497,1585.06716294972,
1585.50203625436,1585.9369095589,1586.37178286333,1586.80665616766,1587.24152947189,
1587.67640277602,1588.11127608005,1588.546149384,1588.98102268785,1589.41589599161,
1589.85076929529,1590.28649529394,1590.72222129258,1591.1570945961,1591.59196789953,
1592.0268412029,1592.46171450619,1592.8965878094,1593.33146111256,1593.76633441564,
1594.20120771867,1594.63608102164,1595.07095432455,1595.50582762741,1595.94070093021,
1596.37557423297,1596.81044753569,1597.24617353387,1597.68189953206,1598.11677283469,
1598.55164613729,1598.98651943985,1599.42139274239,1599.8562660449,1600.29113934738,
1600.72601264985,1601.16088595229,1601.59575925472,1602.03063255714,1602.46550585955,
1602.90037916195,1603.33525246435,1603.77012576675,1604.2058517648,1604.64157776285,
1605.07645106526,1605.51132436768,1605.94619767011,1606.38107097255,1606.81594427502,
1607.2508175775,1607.68569088001,1608.12056418254,1608.55543748511,1608.99031078771,
1609.42518409034,1609.86005739302,1610.29493069573,1610.72980399849,1611.16552999674,
1611.60125599499,1612.03612929785,1612.47100260076,1612.90587590373,1613.34074920675,
1613.77562250984,1614.21049581299,1614.64536911621,1615.0802424195,1615.51511572286,
1615.9499890263,1616.38486232981,1616.81973563341,1617.25460893709,1617.68948224085,
1618.12520823963,1618.5609342384,1618.99580754234,1619.43068084638,1619.86555415051,
1620.30042745474,1620.73530075907,1621.1701740635,1621.60504736804,1622.03992067268,
1622.47479397743,1622.90966728229,1623.34454058727,1623.77941389236,1624.21428719757,
1624.6491605029,1625.08488650247,1625.52061250204,1625.95548580761,1626.39035911331,
1626.82523241913,1627.26010572508,1627.69497903116,1628.12985233737,1628.56472564372,
1628.99959895019,1629.43447225681,1629.86934556356,1630.30421887044,1630.73909217747,
1631.17396548464,1631.60883879195,1632.04456479252,1632.48029079309,1632.91516410068,
1633.35003740842,1633.78491071631,1634.21978402433,1634.65465733251,1635.08953064083,
1635.5244039493,1635.95927725792,1636.39415056668,1636.8290238756,1637.26389718466,
1637.69877049387,1638.13364380323,1638.56851711274,1639.00424311442,1639.43996911609,
1639.8748424259,1640.30971573585,1640.74458904595,1641.6143356666,1642.04920897714,
1642.48408228782,1642.91895559865,1643.35382890963,1643.78870222074,1644.223575532,
1645.09332215494,1645.52819546661,1645.96392146936,1646.39964747212,1646.83452078406,
1647.26939409614,1647.70426740834,1648.57401403314,1649.44376065844,1650.31350728422,
1650.74838059729,1651.18325391046,1652.05300053714,1652.92359985428,1653.79419917162,
1654.66394579929,1655.5336924273,1656.40343905563,1657.27318568424,1658.14293231311,
1659.01267894219,1659.88327826096,1660.75387757982,1661.62362420926,1662.49337083877,
1663.3631174683,1664.23286409781,1665.10261072725,1665.97235735658,1666.84295667531,
1667.71355599396,1668.58330262282,1669.45304925143,1670.32279587976,1671.19254250778,
1672.06228913544,1672.93203576273,1673.80263507977,1674.6732343966,1675.54298102284,
1676.41272764862,1677.28247427392,1678.15222089872,1679.021967523,1679.89171414676,
1680.76231346105,1681.19803946366,1681.63291277506,1682.06778608632,1682.50265939743,
1682.93753270841,1683.37240601924,1684.24215264047,1684.67702595086,1685.11189926111,
1685.54677257121,1685.98164588116,1686.41651919097,1686.85139250063,1687.28626581014,
1687.72199181166,1688.15771781319,1688.5925911224,1689.02746443146,1689.46233774038,
1689.89721104914,1690.33208435776,1690.76695766623,1691.20183097455,1691.63670428272,
1692.07157759075,1692.50645089864,1692.94132420637,1693.37619751397,1693.81107082142,
1694.24594412873,1694.68167012916,1695.11739612959,1695.55226943662,1695.9871427435,
1696.42201605025,1696.85688935687,1697.29176266334,1697.72663596969,1698.1615092759,
1698.59638258198,1699.03125588793,1699.46612919375,1699.90100249945,1700.33587580502,
1700.77074911047,1701.20562241579,1701.64134841525,1702.0770744147,1702.51194771979,
1702.94682102476,1703.38169432963,1703.81656763438,1704.25144093902,1704.68631424356,
1705.12118754799,1705.55606085232,1705.99093415655,1706.42580746068,1706.86068076471,
1707.29555406866,1707.73042737251,1708.16530067627,1708.60102667496,1709.03675267365,
1709.47162597724,1709.90649928076,1710.34137258419,1710.77624588756,1711.21111919085,
1711.64599249406,1712.08086579722,1712.5157391003,1712.95061240333,1713.3854857063,
1713.82035900921,1714.25523231207,1714.69010561487,1715.12497891763,1715.56070491584,
1715.99643091404,1716.43130421671,1716.86617751935,1717.30105082195,1717.73592412451,
1718.17079742705,1718.60567072956,1719.04054403204,1719.4754173345,1719.91029063695,
1720.34516393938,1720.7800372418,1721.21491054421,1721.64978384661,1722.08465714901,
1722.52038314706,1722.9561091451,1723.39098244751,1723.82585574992,1724.26072905233,
1724.69560235476,1725.13047565721,1725.56534895967,1726.00022226216,1726.43509556467,
1726.8699688672,1727.30484216977,1727.73971547236,1728.174588775,1728.60946207767,
1729.04433538039,1729.48006137861,1729.91578737684,1730.35066067965,1730.78553398251,
1731.22040728542,1731.65528058838,1732.09015389141,1732.5250271945,1732.95990049765,
1733.39477380087,1733.82964710416,1734.26452040752,1734.69939371096,1735.13426701447,
1735.56914031807,1736.00401362175,1736.43973962048,1736.8754656192,1737.31033892306,
1737.745212227,1738.18008553104,1738.61495883517,1739.0498321394,1739.48470544373,
1739.91957874816,1740.35445205269,1740.78932535734,1741.22419866209,1741.65907196695,
1742.09394527193,1742.52881857702,1742.96369188223,1743.39941788174,1743.83514388125,
1744.2700171867,1744.70489049227,1745.13976379797,1745.57463710379,1746.00951040974,
1746.44438371582,1746.87925702203,1747.31413032837,1747.74900363485,1748.18387694146,
1748.61875024821,1749.0536235551,1749.48849686213,1749.92337016929,1750.3590961698,
1750.7948221703,1751.22969547775,1751.66456878534,1752.09944209308,1752.53431540096,
1752.96918870899,1753.40406201717,1753.83893532549,1754.27380863396,1754.70868194258,
1755.14355525134,1755.57842856026,1756.01330186932,1756.44817517853,1756.88304848789,
1757.31877448949,1757.75450049109,1758.18937380075,1759.05912042051,1759.49399373061,
1759.92886704086,1760.36374035125,1760.79861366179,1761.23348697248,1761.66836028331,
1762.10323359429,1762.5381069054,1763.40785352806,1763.8427268396,1764.27845284228,
1764.71417884496,1765.14905215677,1765.58392546872,1766.0187987808,1766.88854540534,
1767.75829203039,1768.1931653431,1768.62803865593,1769.06291196888,1769.49778528195,
1770.36753190841,1771.2381312254,1772.10873054259,1772.97847717007,1773.84822379791,
1774.71797042609,1775.58771705456,1776.45746368331,1777.32721031228,1778.19780963089,
1779.06840894783,1779.93815555508,1780.80790201176,1781.67764871408),(-0.58309518948453,
1.5208938731769E-10),.UNSPECIFIED.) ;
#822 = B_SPLINE_SURFACE_WITH_KNOTS('',3,1,((#43253,#43254),(#43255,#43256),
(#43257,#43258),(#43259,#43260),(#43261,#43262),(#43263,#43264),(#43265,
#43266),(#43267,#43268),(#43269,#43270),(#43271,#43272),(#43273,#43274),
(#43275,#43276),(#43277,#43278),(#43279,#43280),(#43281,#43282),(#43283,
#43284),(#43285,#43286),(#43287,#43288),(#43289,#43290),(#43291,#43292),
(#43293,#43294),(#43295,#43296),(#43297,#43298),(#43299,#43300),(#43301,
#43302),(#43303,#43304),(#43305,#43306),(#43307,#43308),(#43309,#43310),
(#43311,#43312),(#43313,#43314),(#43315,#43316),(#43317,#43318),(#43319,
#43320),(#43321,#43322),(#43323,#43324),(#43325,#43326),(#43327,#43328),
(#43329,#43330),(#43331,#43332),(#43333,#43334),(#43335,#43336),(#43337,
#43338),(#43339,#43340),(#43341,#43342),(#43343,#43344),(#43345,#43346),
(#43347,#43348),(#43349,#43350),(#43351,#43352),(#43353,#43354),(#43355,
#43356),(#43357,#43358),(#43359,#43360),(#43361,#43362),(#43363,#43364),
(#43365,#43366),(#43367,#43368),(#43369,#43370),(#43371,#43372),(#43373,
#43374),(#43375,#43376),(#43377,#43378),(#43379,#43380),(#43381,#43382),
(#43383,#43384),(#43385,#43386),(#43387,#43388),(#43389,#43390),(#43391,
#43392),(#43393,#43394),(#43395,#43396),(#43397,#43398),(#43399,#43400),
(#43401,#43402),(#43403,#43404),(#43405,#43406),(#43407,#43408),(#43409,
#43410),(#43411,#43412),(#43413,#43414),(#43415,#43416),(#43417,#43418),
(#43419,#43420),(#43421,#43422),(#43423,#43424),(#43425,#43426),(#43427,
#43428),(#43429,#43430),(#43431,#43432),(#43433,#43434),(#43435,#43436),
(#43437,#43438),(#43439,#43440),(#43441,#43442),(#43443,#43444),(#43445,
#43446),(#43447,#43448),(#43449,#43450),(#43451,#43452),(#43453,#43454),
(#43455,#43456),(#43457,#43458),(#43459,#43460),(#43461,#43462),(#43463,
#43464),(#43465,#43466),(#43467,#43468),(#43469,#43470),(#43471,#43472),
(#43473,#43474),(#43475,#43476),(#43477,#43478),(#43479,#43480),(#43481,
#43482),(#43483,#43484),(#43485,#43486),(#43487,#43488),(#43489,#43490),
(#43491,#43492),(#43493,#43494),(#43495,#43496),(#43497,#43498),(#43499,
#43500),(#43501,#43502),(#43503,#43504),(#43505,#43506),(#43507,#43508),
(#43509,#43510),(#43511,#43512),(#43513,#43514),(#43515,#43516),(#43517,
#43518),(#43519,#43520),(#43521,#43522),(#43523,#43524),(#43525,#43526),
(#43527,#43528),(#43529,#43530),(#43531,#43532),(#43533,#43534),(#43535,
#43536),(#43537,#43538),(#43539,#43540),(#43541,#43542),(#43543,#43544),
(#43545,#43546),(#43547,#43548),(#43549,#43550),(#43551,#43552),(#43553,
#43554),(#43555,#43556),(#43557,#43558),(#43559,#43560),(#43561,#43562),
(#43563,#43564),(#43565,#43566),(#43567,#43568),(#43569,#43570),(#43571,
#43572),(#43573,#43574),(#43575,#43576),(#43577,#43578),(#43579,#43580),
(#43581,#43582),(#43583,#43584),(#43585,#43586),(#43587,#43588),(#43589,
#43590),(#43591,#43592),(#43593,#43594),(#43595,#43596),(#43597,#43598),
(#43599,#43600),(#43601,#43602),(#43603,#43604),(#43605,#43606),(#43607,
#43608),(#43609,#43610),(#43611,#43612),(#43613,#43614),(#43615,#43616),
(#43617,#43618),(#43619,#43620),(#43621,#43622),(#43623,#43624),(#43625,
#43626),(#43627,#43628),(#43629,#43630),(#43631,#43632),(#43633,#43634),
(#43635,#43636),(#43637,#43638),(#43639,#43640),(#43641,#43642),(#43643,
#43644),(#43645,#43646),(#43647,#43648),(#43649,#43650),(#43651,#43652),
(#43653,#43654),(#43655,#43656),(#43657,#43658),(#43659,#43660),(#43661,
#43662),(#43663,#43664),(#43665,#43666),(#43667,#43668),(#43669,#43670),
(#43671,#43672),(#43673,#43674),(#43675,#43676),(#43677,#43678),(#43679,
#43680),(#43681,#43682),(#43683,#43684),(#43685,#43686),(#43687,#43688),
(#43689,#43690),(#43691,#43692),(#43693,#43694),(#43695,#43696),(#43697,
#43698),(#43699,#43700),(#43701,#43702),(#43703,#43704),(#43705,#43706),
(#43707,#43708),(#43709,#43710),(#43711,#43712),(#43713,#43714),(#43715,
#43716),(#43717,#43718),(#43719,#43720),(#43721,#43722),(#43723,#43724),
(#43725,#43726),(#43727,#43728),(#43729,#43730),(#43731,#43732),(#43733,
#43734),(#43735,#43736),(#43737,#43738),(#43739,#43740),(#43741,#43742),
(#43743,#43744),(#43745,#43746),(#43747,#43748),(#43749,#43750),(#43751,
#43752),(#43753,#43754),(#43755,#43756),(#43757,#43758),(#43759,#43760),
(#43761,#43762),(#43763,#43764),(#43765,#43766),(#43767,#43768),(#43769,
#43770),(#43771,#43772),(#43773,#43774),(#43775,#43776),(#43777,#43778),
(#43779,#43780),(#43781,#43782),(#43783,#43784),(#43785,#43786),(#43787,
#43788),(#43789,#43790),(#43791,#43792),(#43793,#43794),(#43795,#43796),
(#43797,#43798),(#43799,#43800),(#43801,#43802),(#43803,#43804),(#43805,
#43806),(#43807,#43808),(#43809,#43810),(#43811,#43812),(#43813,#43814),
(#43815,#43816),(#43817,#43818),(#43819,#43820),(#43821,#43822),(#43823,
#43824),(#43825,#43826),(#43827,#43828),(#43829,#43830),(#43831,#43832),
(#43833,#43834),(#43835,#43836),(#43837,#43838),(#43839,#43840),(#43841,
#43842),(#43843,#43844),(#43845,#43846),(#43847,#43848),(#43849,#43850),
(#43851,#43852),(#43853,#43854),(#43855,#43856),(#43857,#43858),(#43859,
#43860),(#43861,#43862),(#43863,#43864),(#43865,#43866),(#43867,#43868),
(#43869,#43870),(#43871,#43872),(#43873,#43874),(#43875,#43876),(#43877,
#43878),(#43879,#43880),(#43881,#43882),(#43883,#43884),(#43885,#43886),
(#43887,#43888),(#43889,#43890),(#43891,#43892),(#43893,#43894),(#43895,
#43896),(#43897,#43898),(#43899,#43900),(#43901,#43902),(#43903,#43904),
(#43905,#43906),(#43907,#43908),(#43909,#43910),(#43911,#43912),(#43913,
#43914),(#43915,#43916),(#43917,#43918),(#43919,#43920),(#43921,#43922),
(#43923,#43924),(#43925,#43926),(#43927,#43928),(#43929,#43930),(#43931,
#43932),(#43933,#43934),(#43935,#43936),(#43937,#43938),(#43939,#43940),
(#43941,#43942),(#43943,#43944),(#43945,#43946),(#43947,#43948),(#43949,
#43950),(#43951,#43952),(#43953,#43954),(#43955,#43956),(#43957,#43958),
(#43959,#43960),(#43961,#43962),(#43963,#43964),(#43965,#43966),(#43967,
#43968),(#43969,#43970),(#43971,#43972),(#43973,#43974),(#43975,#43976),
(#43977,#43978),(#43979,#43980),(#43981,#43982),(#43983,#43984),(#43985,
#43986),(#43987,#43988),(#43989,#43990),(#43991,#43992),(#43993,#43994),
(#43995,#43996),(#43997,#43998),(#43999,#44000),(#44001,#44002),(#44003,
#44004),(#44005,#44006),(#44007,#44008),(#44009,#44010),(#44011,#44012),
(#44013,#44014),(#44015,#44016),(#44017,#44018),(#44019,#44020),(#44021,
#44022),(#44023,#44024),(#44025,#44026),(#44027,#44028),(#44029,#44030),
(#44031,#44032),(#44033,#44034),(#44035,#44036),(#44037,#44038),(#44039,
#44040),(#44041,#44042),(#44043,#44044),(#44045,#44046),(#44047,#44048),
(#44049,#44050),(#44051,#44052),(#44053,#44054),(#44055,#44056),(#44057,
#44058),(#44059,#44060),(#44061,#44062),(#44063,#44064),(#44065,#44066),
(#44067,#44068),(#44069,#44070),(#44071,#44072),(#44073,#44074),(#44075,
#44076),(#44077,#44078),(#44079,#44080),(#44081,#44082),(#44083,#44084),
(#44085,#44086),(#44087,#44088),(#44089,#44090),(#44091,#44092),(#44093,
#44094),(#44095,#44096),(#44097,#44098),(#44099,#44100),(#44101,#44102),
(#44103,#44104),(#44105,#44106),(#44107,#44108),(#44109,#44110),(#44111,
#44112),(#44113,#44114),(#44115,#44116),(#44117,#44118),(#44119,#44120),
(#44121,#44122),(#44123,#44124),(#44125,#44126),(#44127,#44128),(#44129,
#44130),(#44131,#44132),(#44133,#44134),(#44135,#44136),(#44137,#44138),
(#44139,#44140),(#44141,#44142),(#44143,#44144),(#44145,#44146),(#44147,
#44148),(#44149,#44150),(#44151,#44152),(#44153,#44154),(#44155,#44156),
(#44157,#44158),(#44159,#44160),(#44161,#44162),(#44163,#44164),(#44165,
#44166),(#44167,#44168),(#44169,#44170),(#44171,#44172),(#44173,#44174),
(#44175,#44176),(#44177,#44178),(#44179,#44180),(#44181,#44182),(#44183,
#44184),(#44185,#44186),(#44187,#44188),(#44189,#44190),(#44191,#44192),
(#44193,#44194),(#44195,#44196),(#44197,#44198),(#44199,#44200),(#44201,
#44202),(#44203,#44204),(#44205,#44206),(#44207,#44208),(#44209,#44210),
(#44211,#44212),(#44213,#44214),(#44215,#44216),(#44217,#44218),(#44219,
#44220),(#44221,#44222),(#44223,#44224),(#44225,#44226),(#44227,#44228),
(#44229,#44230),(#44231,#44232),(#44233,#44234),(#44235,#44236),(#44237,
#44238),(#44239,#44240),(#44241,#44242),(#44243,#44244),(#44245,#44246),
(#44247,#44248),(#44249,#44250),(#44251,#44252),(#44253,#44254),(#44255,
#44256),(#44257,#44258),(#44259,#44260),(#44261,#44262),(#44263,#44264),
(#44265,#44266),(#44267,#44268),(#44269,#44270),(#44271,#44272),(#44273,
#44274),(#44275,#44276),(#44277,#44278),(#44279,#44280),(#44281,#44282),
(#44283,#44284),(#44285,#44286),(#44287,#44288),(#44289,#44290),(#44291,
#44292),(#44293,#44294),(#44295,#44296),(#44297,#44298),(#44299,#44300),
(#44301,#44302),(#44303,#44304),(#44305,#44306),(#44307,#44308),(#44309,
#44310),(#44311,#44312),(#44313,#44314),(#44315,#44316),(#44317,#44318),
(#44319,#44320),(#44321,#44322),(#44323,#44324),(#44325,#44326),(#44327,
#44328),(#44329,#44330),(#44331,#44332),(#44333,#44334),(#44335,#44336),
(#44337,#44338),(#44339,#44340),(#44341,#44342),(#44343,#44344),(#44345,
#44346),(#44347,#44348),(#44349,#44350),(#44351,#44352),(#44353,#44354),
(#44355,#44356),(#44357,#44358),(#44359,#44360),(#44361,#44362),(#44363,
#44364),(#44365,#44366),(#44367,#44368),(#44369,#44370),(#44371,#44372),
(#44373,#44374),(#44375,#44376),(#44377,#44378),(#44379,#44380),(#44381,
#44382),(#44383,#44384),(#44385,#44386),(#44387,#44388),(#44389,#44390),
(#44391,#44392),(#44393,#44394),(#44395,#44396),(#44397,#44398),(#44399,
#44400),(#44401,#44402),(#44403,#44404),(#44405,#44406),(#44407,#44408),
(#44409,#44410),(#44411,#44412),(#44413,#44414),(#44415,#44416),(#44417,
#44418),(#44419,#44420),(#44421,#44422),(#44423,#44424),(#44425,#44426),
(#44427,#44428),(#44429,#44430),(#44431,#44432),(#44433,#44434),(#44435,
#44436),(#44437,#44438),(#44439,#44440),(#44441,#44442),(#44443,#44444),
(#44445,#44446),(#44447,#44448),(#44449,#44450),(#44451,#44452),(#44453,
#44454),(#44455,#44456),(#44457,#44458),(#44459,#44460),(#44461,#44462),
(#44463,#44464),(#44465,#44466),(#44467,#44468),(#44469,#44470),(#44471,
#44472),(#44473,#44474),(#44475,#44476),(#44477,#44478),(#44479,#44480),
(#44481,#44482),(#44483,#44484),(#44485,#44486),(#44487,#44488),(#44489,
#44490),(#44491,#44492),(#44493,#44494),(#44495,#44496),(#44497,#44498),
(#44499,#44500),(#44501,#44502),(#44503,#44504),(#44505,#44506),(#44507,
#44508),(#44509,#44510),(#44511,#44512),(#44513,#44514),(#44515,#44516),
(#44517,#44518),(#44519,#44520),(#44521,#44522),(#44523,#44524),(#44525,
#44526),(#44527,#44528),(#44529,#44530),(#44531,#44532),(#44533,#44534),
(#44535,#44536),(#44537,#44538),(#44539,#44540),(#44541,#44542),(#44543,
#44544),(#44545,#44546),(#44547,#44548),(#44549,#44550),(#44551,#44552),
(#44553,#44554),(#44555,#44556),(#44557,#44558),(#44559,#44560),(#44561,
#44562),(#44563,#44564),(#44565,#44566),(#44567,#44568),(#44569,#44570),
(#44571,#44572),(#44573,#44574),(#44575,#44576),(#44577,#44578),(#44579,
#44580),(#44581,#44582),(#44583,#44584),(#44585,#44586),(#44587,#44588),
(#44589,#44590),(#44591,#44592),(#44593,#44594),(#44595,#44596),(#44597,
#44598),(#44599,#44600),(#44601,#44602),(#44603,#44604),(#44605,#44606),
(#44607,#44608),(#44609,#44610),(#44611,#44612),(#44613,#44614),(#44615,
#44616),(#44617,#44618),(#44619,#44620),(#44621,#44622),(#44623,#44624),
(#44625,#44626),(#44627,#44628),(#44629,#44630),(#44631,#44632),(#44633,
#44634),(#44635,#44636),(#44637,#44638),(#44639,#44640),(#44641,#44642),
(#44643,#44644),(#44645,#44646),(#44647,#44648),(#44649,#44650),(#44651,
#44652),(#44653,#44654),(#44655,#44656),(#44657,#44658),(#44659,#44660),
(#44661,#44662),(#44663,#44664),(#44665,#44666),(#44667,#44668),(#44669,
#44670),(#44671,#44672),(#44673,#44674),(#44675,#44676),(#44677,#44678),
(#44679,#44680),(#44681,#44682),(#44683,#44684),(#44685,#44686),(#44687,
#44688),(#44689,#44690),(#44691,#44692),(#44693,#44694),(#44695,#44696),
(#44697,#44698),(#44699,#44700),(#44701,#44702),(#44703,#44704),(#44705,
#44706),(#44707,#44708),(#44709,#44710),(#44711,#44712),(#44713,#44714),
(#44715,#44716),(#44717,#44718),(#44719,#44720),(#44721,#44722),(#44723,
#44724),(#44725,#44726),(#44727,#44728),(#44729,#44730),(#44731,#44732),
(#44733,#44734),(#44735,#44736),(#44737,#44738),(#44739,#44740),(#44741,
#44742),(#44743,#44744),(#44745,#44746),(#44747,#44748),(#44749,#44750),
(#44751,#44752),(#44753,#44754),(#44755,#44756),(#44757,#44758),(#44759,
#44760),(#44761,#44762),(#44763,#44764),(#44765,#44766),(#44767,#44768),
(#44769,#44770),(#44771,#44772),(#44773,#44774),(#44775,#44776),(#44777,
#44778),(#44779,#44780),(#44781,#44782),(#44783,#44784),(#44785,#44786),
(#44787,#44788),(#44789,#44790),(#44791,#44792),(#44793,#44794),(#44795,
#44796),(#44797,#44798),(#44799,#44800),(#44801,#44802),(#44803,#44804),
(#44805,#44806),(#44807,#44808),(#44809,#44810),(#44811,#44812),(#44813,
#44814),(#44815,#44816),(#44817,#44818),(#44819,#44820),(#44821,#44822),
(#44823,#44824),(#44825,#44826),(#44827,#44828),(#44829,#44830),(#44831,
#44832),(#44833,#44834),(#44835,#44836),(#44837,#44838),(#44839,#44840),
(#44841,#44842),(#44843,#44844),(#44845,#44846),(#44847,#44848),(#44849,
#44850),(#44851,#44852),(#44853,#44854),(#44855,#44856),(#44857,#44858),
(#44859,#44860),(#44861,#44862),(#44863,#44864),(#44865,#44866),(#44867,
#44868),(#44869,#44870),(#44871,#44872),(#44873,#44874),(#44875,#44876),
(#44877,#44878),(#44879,#44880),(#44881,#44882),(#44883,#44884),(#44885,
#44886),(#44887,#44888),(#44889,#44890),(#44891,#44892),(#44893,#44894),
(#44895,#44896),(#44897,#44898),(#44899,#44900),(#44901,#44902),(#44903,
#44904),(#44905,#44906),(#44907,#44908),(#44909,#44910),(#44911,#44912),
(#44913,#44914),(#44915,#44916),(#44917,#44918),(#44919,#44920),(#44921,
#44922),(#44923,#44924),(#44925,#44926),(#44927,#44928),(#44929,#44930),
(#44931,#44932),(#44933,#44934),(#44935,#44936),(#44937,#44938),(#44939,
#44940),(#44941,#44942),(#44943,#44944),(#44945,#44946),(#44947,#44948),
(#44949,#44950),(#44951,#44952),(#44953,#44954),(#44955,#44956),(#44957,
#44958),(#44959,#44960),(#44961,#44962),(#44963,#44964),(#44965,#44966),
(#44967,#44968),(#44969,#44970),(#44971,#44972),(#44973,#44974),(#44975,
#44976),(#44977,#44978),(#44979,#44980),(#44981,#44982),(#44983,#44984),
(#44985,#44986),(#44987,#44988),(#44989,#44990),(#44991,#44992),(#44993,
#44994),(#44995,#44996),(#44997,#44998),(#44999,#45000),(#45001,#45002),
(#45003,#45004),(#45005,#45006),(#45007,#45008),(#45009,#45010),(#45011,
#45012),(#45013,#45014),(#45015,#45016),(#45017,#45018),(#45019,#45020),
(#45021,#45022),(#45023,#45024),(#45025,#45026),(#45027,#45028),(#45029,
#45030),(#45031,#45032),(#45033,#45034),(#45035,#45036),(#45037,#45038),
(#45039,#45040),(#45041,#45042),(#45043,#45044),(#45045,#45046),(#45047,
#45048),(#45049,#45050),(#45051,#45052),(#45053,#45054),(#45055,#45056),
(#45057,#45058),(#45059,#45060),(#45061,#45062),(#45063,#45064),(#45065,
#45066),(#45067,#45068),(#45069,#45070),(#45071,#45072),(#45073,#45074),
(#45075,#45076),(#45077,#45078),(#45079,#45080),(#45081,#45082),(#45083,
#45084),(#45085,#45086),(#45087,#45088),(#45089,#45090),(#45091,#45092),
(#45093,#45094),(#45095,#45096),(#45097,#45098),(#45099,#45100),(#45101,
#45102),(#45103,#45104),(#45105,#45106),(#45107,#45108),(#45109,#45110),
(#45111,#45112),(#45113,#45114),(#45115,#45116),(#45117,#45118),(#45119,
#45120),(#45121,#45122),(#45123,#45124),(#45125,#45126),(#45127,#45128),
(#45129,#45130),(#45131,#45132),(#45133,#45134),(#45135,#45136),(#45137,
#45138),(#45139,#45140),(#45141,#45142),(#45143,#45144),(#45145,#45146),
(#45147,#45148),(#45149,#45150),(#45151,#45152),(#45153,#45154),(#45155,
#45156),(#45157,#45158),(#45159,#45160),(#45161,#45162),(#45163,#45164),
(#45165,#45166),(#45167,#45168),(#45169,#45170),(#45171,#45172),(#45173,
#45174),(#45175,#45176),(#45177,#45178),(#45179,#45180),(#45181,#45182),
(#45183,#45184),(#45185,#45186),(#45187,#45188),(#45189,#45190),(#45191,
#45192),(#45193,#45194),(#45195,#45196),(#45197,#45198),(#45199,#45200),
(#45201,#45202),(#45203,#45204),(#45205,#45206),(#45207,#45208),(#45209,
#45210),(#45211,#45212),(#45213,#45214),(#45215,#45216),(#45217,#45218),
(#45219,#45220),(#45221,#45222),(#45223,#45224),(#45225,#45226),(#45227,
#45228),(#45229,#45230),(#45231,#45232),(#45233,#45234),(#45235,#45236),
(#45237,#45238),(#45239,#45240),(#45241,#45242),(#45243,#45244),(#45245,
#45246),(#45247,#45248),(#45249,#45250),(#45251,#45252),(#45253,#45254),
(#45255,#45256),(#45257,#45258),(#45259,#45260),(#45261,#45262),(#45263,
#45264),(#45265,#45266),(#45267,#45268),(#45269,#45270),(#45271,#45272),
(#45273,#45274),(#45275,#45276),(#45277,#45278),(#45279,#45280),(#45281,
#45282),(#45283,#45284),(#45285,#45286),(#45287,#45288),(#45289,#45290),
(#45291,#45292),(#45293,#45294),(#45295,#45296),(#45297,#45298),(#45299,
#45300),(#45301,#45302),(#45303,#45304),(#45305,#45306),(#45307,#45308),
(#45309,#45310),(#45311,#45312),(#45313,#45314),(#45315,#45316),(#45317,
#45318),(#45319,#45320),(#45321,#45322),(#45323,#45324),(#45325,#45326),
(#45327,#45328),(#45329,#45330),(#45331,#45332),(#45333,#45334),(#45335,
#45336),(#45337,#45338),(#45339,#45340),(#45341,#45342),(#45343,#45344),
(#45345,#45346),(#45347,#45348),(#45349,#45350),(#45351,#45352),(#45353,
#45354),(#45355,#45356),(#45357,#45358),(#45359,#45360),(#45361,#45362),
(#45363,#45364),(#45365,#45366),(#45367,#45368),(#45369,#45370),(#45371,
#45372),(#45373,#45374),(#45375,#45376),(#45377,#45378),(#45379,#45380),
(#45381,#45382),(#45383,#45384),(#45385,#45386),(#45387,#45388),(#45389,
#45390),(#45391,#45392),(#45393,#45394),(#45395,#45396),(#45397,#45398),
(#45399,#45400),(#45401,#45402),(#45403,#45404),(#45405,#45406),(#45407,
#45408),(#45409,#45410),(#45411,#45412),(#45413,#45414),(#45415,#45416),
(#45417,#45418),(#45419,#45420),(#45421,#45422),(#45423,#45424),(#45425,
#45426),(#45427,#45428),(#45429,#45430),(#45431,#45432),(#45433,#45434),
(#45435,#45436),(#45437,#45438),(#45439,#45440),(#45441,#45442),(#45443,
#45444),(#45445,#45446),(#45447,#45448),(#45449,#45450),(#45451,#45452),
(#45453,#45454),(#45455,#45456),(#45457,#45458),(#45459,#45460),(#45461,
#45462),(#45463,#45464),(#45465,#45466),(#45467,#45468),(#45469,#45470),
(#45471,#45472),(#45473,#45474),(#45475,#45476),(#45477,#45478),(#45479,
#45480),(#45481,#45482),(#45483,#45484),(#45485,#45486),(#45487,#45488),
(#45489,#45490),(#45491,#45492),(#45493,#45494),(#45495,#45496),(#45497,
#45498),(#45499,#45500),(#45501,#45502),(#45503,#45504),(#45505,#45506),
(#45507,#45508),(#45509,#45510),(#45511,#45512),(#45513,#45514),(#45515,
#45516),(#45517,#45518),(#45519,#45520),(#45521,#45522),(#45523,#45524),
(#45525,#45526),(#45527,#45528),(#45529,#45530),(#45531,#45532),(#45533,
#45534),(#45535,#45536),(#45537,#45538),(#45539,#45540),(#45541,#45542),
(#45543,#45544),(#45545,#45546),(#45547,#45548),(#45549,#45550),(#45551,
#45552),(#45553,#45554),(#45555,#45556),(#45557,#45558),(#45559,#45560),
(#45561,#45562),(#45563,#45564),(#45565,#45566),(#45567,#45568),(#45569,
#45570),(#45571,#45572),(#45573,#45574),(#45575,#45576),(#45577,#45578),
(#45579,#45580),(#45581,#45582),(#45583,#45584),(#45585,#45586),(#45587,
#45588),(#45589,#45590),(#45591,#45592),(#45593,#45594),(#45595,#45596),
(#45597,#45598),(#45599,#45600),(#45601,#45602),(#45603,#45604),(#45605,
#45606),(#45607,#45608),(#45609,#45610),(#45611,#45612),(#45613,#45614),
(#45615,#45616),(#45617,#45618),(#45619,#45620),(#45621,#45622),(#45623,
#45624),(#45625,#45626),(#45627,#45628),(#45629,#45630),(#45631,#45632),
(#45633,#45634),(#45635,#45636),(#45637,#45638),(#45639,#45640),(#45641,
#45642),(#45643,#45644),(#45645,#45646),(#45647,#45648),(#45649,#45650),
(#45651,#45652),(#45653,#45654),(#45655,#45656),(#45657,#45658),(#45659,
#45660),(#45661,#45662),(#45663,#45664),(#45665,#45666),(#45667,#45668),
(#45669,#45670),(#45671,#45672),(#45673,#45674),(#45675,#45676),(#45677,
#45678),(#45679,#45680),(#45681,#45682),(#45683,#45684),(#45685,#45686),
(#45687,#45688),(#45689,#45690),(#45691,#45692),(#45693,#45694),(#45695,
#45696),(#45697,#45698),(#45699,#45700),(#45701,#45702),(#45703,#45704),
(#45705,#45706),(#45707,#45708),(#45709,#45710),(#45711,#45712),(#45713,
#45714),(#45715,#45716),(#45717,#45718),(#45719,#45720),(#45721,#45722),
(#45723,#45724),(#45725,#45726),(#45727,#45728),(#45729,#45730),(#45731,
#45732),(#45733,#45734),(#45735,#45736),(#45737,#45738),(#45739,#45740),
(#45741,#45742),(#45743,#45744),(#45745,#45746),(#45747,#45748),(#45749,
#45750),(#45751,#45752),(#45753,#45754),(#45755,#45756),(#45757,#45758),
(#45759,#45760),(#45761,#45762),(#45763,#45764),(#45765,#45766),(#45767,
#45768),(#45769,#45770),(#45771,#45772),(#45773,#45774),(#45775,#45776),
(#45777,#45778),(#45779,#45780),(#45781,#45782),(#45783,#45784),(#45785,
#45786),(#45787,#45788),(#45789,#45790),(#45791,#45792),(#45793,#45794),
(#45795,#45796),(#45797,#45798),(#45799,#45800),(#45801,#45802),(#45803,
#45804),(#45805,#45806),(#45807,#45808),(#45809,#45810),(#45811,#45812),
(#45813,#45814),(#45815,#45816),(#45817,#45818),(#45819,#45820),(#45821,
#45822),(#45823,#45824),(#45825,#45826),(#45827,#45828),(#45829,#45830),
(#45831,#45832),(#45833,#45834),(#45835,#45836),(#45837,#45838),(#45839,
#45840),(#45841,#45842),(#45843,#45844),(#45845,#45846),(#45847,#45848),
(#45849,#45850),(#45851,#45852),(#45853,#45854),(#45855,#45856),(#45857,
#45858),(#45859,#45860),(#45861,#45862),(#45863,#45864),(#45865,#45866),
(#45867,#45868),(#45869,#45870),(#45871,#45872),(#45873,#45874),(#45875,
#45876),(#45877,#45878),(#45879,#45880),(#45881,#45882),(#45883,#45884),
(#45885,#45886),(#45887,#45888),(#45889,#45890),(#45891,#45892),(#45893,
#45894),(#45895,#45896),(#45897,#45898),(#45899,#45900),(#45901,#45902),
(#45903,#45904),(#45905,#45906),(#45907,#45908),(#45909,#45910),(#45911,
#45912),(#45913,#45914),(#45915,#45916),(#45917,#45918),(#45919,#45920),
(#45921,#45922),(#45923,#45924),(#45925,#45926),(#45927,#45928),(#45929,
#45930),(#45931,#45932),(#45933,#45934),(#45935,#45936),(#45937,#45938),
(#45939,#45940),(#45941,#45942),(#45943,#45944),(#45945,#45946),(#45947,
#45948),(#45949,#45950),(#45951,#45952),(#45953,#45954),(#45955,#45956),
(#45957,#45958),(#45959,#45960),(#45961,#45962),(#45963,#45964),(#45965,
#45966),(#45967,#45968),(#45969,#45970),(#45971,#45972),(#45973,#45974),
(#45975,#45976),(#45977,#45978),(#45979,#45980),(#45981,#45982),(#45983,
#45984),(#45985,#45986),(#45987,#45988),(#45989,#45990),(#45991,#45992),
(#45993,#45994),(#45995,#45996),(#45997,#45998),(#45999,#46000),(#46001,
#46002),(#46003,#46004),(#46005,#46006),(#46007,#46008),(#46009,#46010),
(#46011,#46012),(#46013,#46014),(#46015,#46016),(#46017,#46018),(#46019,
#46020),(#46021,#46022),(#46023,#46024),(#46025,#46026),(#46027,#46028),
(#46029,#46030),(#46031,#46032),(#46033,#46034),(#46035,#46036),(#46037,
#46038),(#46039,#46040),(#46041,#46042),(#46043,#46044),(#46045,#46046),
(#46047,#46048),(#46049,#46050),(#46051,#46052),(#46053,#46054),(#46055,
#46056),(#46057,#46058),(#46059,#46060),(#46061,#46062),(#46063,#46064),
(#46065,#46066),(#46067,#46068),(#46069,#46070),(#46071,#46072),(#46073,
#46074),(#46075,#46076),(#46077,#46078),(#46079,#46080),(#46081,#46082),
(#46083,#46084),(#46085,#46086),(#46087,#46088),(#46089,#46090),(#46091,
#46092),(#46093,#46094),(#46095,#46096),(#46097,#46098),(#46099,#46100),
(#46101,#46102),(#46103,#46104),(#46105,#46106),(#46107,#46108),(#46109,
#46110),(#46111,#46112),(#46113,#46114),(#46115,#46116),(#46117,#46118),
(#46119,#46120),(#46121,#46122),(#46123,#46124),(#46125,#46126),(#46127,
#46128),(#46129,#46130),(#46131,#46132),(#46133,#46134),(#46135,#46136),
(#46137,#46138),(#46139,#46140),(#46141,#46142),(#46143,#46144),(#46145,
#46146),(#46147,#46148),(#46149,#46150),(#46151,#46152),(#46153,#46154),
(#46155,#46156),(#46157,#46158),(#46159,#46160),(#46161,#46162),(#46163,
#46164),(#46165,#46166),(#46167,#46168),(#46169,#46170),(#46171,#46172),
(#46173,#46174),(#46175,#46176),(#46177,#46178),(#46179,#46180),(#46181,
#46182),(#46183,#46184),(#46185,#46186),(#46187,#46188),(#46189,#46190),
(#46191,#46192),(#46193,#46194),(#46195,#46196),(#46197,#46198),(#46199,
#46200),(#46201,#46202),(#46203,#46204),(#46205,#46206),(#46207,#46208),
(#46209,#46210),(#46211,#46212),(#46213,#46214),(#46215,#46216),(#46217,
#46218),(#46219,#46220),(#46221,#46222),(#46223,#46224),(#46225,#46226),
(#46227,#46228),(#46229,#46230),(#46231,#46232),(#46233,#46234),(#46235,
#46236),(#46237,#46238),(#46239,#46240),(#46241,#46242),(#46243,#46244),
(#46245,#46246),(#46247,#46248),(#46249,#46250),(#46251,#46252),(#46253,
#46254),(#46255,#46256),(#46257,#46258),(#46259,#46260),(#46261,#46262),
(#46263,#46264),(#46265,#46266),(#46267,#46268),(#46269,#46270),(#46271,
#46272),(#46273,#46274),(#46275,#46276),(#46277,#46278),(#46279,#46280),
(#46281,#46282),(#46283,#46284),(#46285,#46286),(#46287,#46288),(#46289,
#46290),(#46291,#46292),(#46293,#46294),(#46295,#46296),(#46297,#46298),
(#46299,#46300),(#46301,#46302),(#46303,#46304),(#46305,#46306),(#46307,
#46308),(#46309,#46310),(#46311,#46312),(#46313,#46314),(#46315,#46316),
(#46317,#46318),(#46319,#46320),(#46321,#46322),(#46323,#46324),(#46325,
#46326),(#46327,#46328),(#46329,#46330),(#46331,#46332),(#46333,#46334),
(#46335,#46336),(#46337,#46338),(#46339,#46340),(#46341,#46342),(#46343,
#46344),(#46345,#46346),(#46347,#46348),(#46349,#46350),(#46351,#46352),
(#46353,#46354),(#46355,#46356),(#46357,#46358),(#46359,#46360),(#46361,
#46362),(#46363,#46364),(#46365,#46366),(#46367,#46368),(#46369,#46370),
(#46371,#46372),(#46373,#46374),(#46375,#46376),(#46377,#46378),(#46379,
#46380),(#46381,#46382),(#46383,#46384),(#46385,#46386),(#46387,#46388),
(#46389,#46390),(#46391,#46392),(#46393,#46394),(#46395,#46396),(#46397,
#46398),(#46399,#46400),(#46401,#46402),(#46403,#46404),(#46405,#46406),
(#46407,#46408),(#46409,#46410),(#46411,#46412),(#46413,#46414),(#46415,
#46416),(#46417,#46418),(#46419,#46420),(#46421,#46422),(#46423,#46424),
(#46425,#46426),(#46427,#46428),(#46429,#46430),(#46431,#46432),(#46433,
#46434),(#46435,#46436),(#46437,#46438),(#46439,#46440),(#46441,#46442),
(#46443,#46444),(#46445,#46446),(#46447,#46448),(#46449,#46450),(#46451,
#46452),(#46453,#46454),(#46455,#46456),(#46457,#46458),(#46459,#46460),
(#46461,#46462),(#46463,#46464),(#46465,#46466),(#46467,#46468),(#46469,
#46470),(#46471,#46472),(#46473,#46474),(#46475,#46476),(#46477,#46478),
(#46479,#46480),(#46481,#46482),(#46483,#46484),(#46485,#46486),(#46487,
#46488),(#46489,#46490),(#46491,#46492),(#46493,#46494),(#46495,#46496),
(#46497,#46498),(#46499,#46500),(#46501,#46502),(#46503,#46504),(#46505,
#46506),(#46507,#46508),(#46509,#46510),(#46511,#46512),(#46513,#46514),
(#46515,#46516),(#46517,#46518),(#46519,#46520),(#46521,#46522),(#46523,
#46524),(#46525,#46526),(#46527,#46528),(#46529,#46530),(#46531,#46532),
(#46533,#46534),(#46535,#46536),(#46537,#46538),(#46539,#46540),(#46541,
#46542),(#46543,#46544),(#46545,#46546),(#46547,#46548),(#46549,#46550),
(#46551,#46552),(#46553,#46554),(#46555,#46556),(#46557,#46558),(#46559,
#46560),(#46561,#46562),(#46563,#46564),(#46565,#46566),(#46567,#46568),
(#46569,#46570),(#46571,#46572),(#46573,#46574),(#46575,#46576),(#46577,
#46578),(#46579,#46580),(#46581,#46582),(#46583,#46584),(#46585,#46586),
(#46587,#46588),(#46589,#46590),(#46591,#46592),(#46593,#46594),(#46595,
#46596),(#46597,#46598),(#46599,#46600),(#46601,#46602),(#46603,#46604),
(#46605,#46606),(#46607,#46608),(#46609,#46610),(#46611,#46612),(#46613,
#46614),(#46615,#46616),(#46617,#46618),(#46619,#46620),(#46621,#46622),
(#46623,#46624),(#46625,#46626),(#46627,#46628),(#46629,#46630),(#46631,
#46632),(#46633,#46634),(#46635,#46636),(#46637,#46638),(#46639,#46640),
(#46641,#46642),(#46643,#46644),(#46645,#46646),(#46647,#46648),(#46649,
#46650),(#46651,#46652),(#46653,#46654),(#46655,#46656),(#46657,#46658),
(#46659,#46660),(#46661,#46662),(#46663,#46664),(#46665,#46666),(#46667,
#46668),(#46669,#46670),(#46671,#46672),(#46673,#46674),(#46675,#46676),
(#46677,#46678),(#46679,#46680),(#46681,#46682),(#46683,#46684),(#46685,
#46686),(#46687,#46688),(#46689,#46690),(#46691,#46692),(#46693,#46694),
(#46695,#46696),(#46697,#46698),(#46699,#46700),(#46701,#46702),(#46703,
#46704),(#46705,#46706),(#46707,#46708),(#46709,#46710),(#46711,#46712),
(#46713,#46714),(#46715,#46716),(#46717,#46718),(#46719,#46720),(#46721,
#46722),(#46723,#46724),(#46725,#46726),(#46727,#46728),(#46729,#46730),
(#46731,#46732),(#46733,#46734),(#46735,#46736),(#46737,#46738),(#46739,
#46740),(#46741,#46742),(#46743,#46744),(#46745,#46746),(#46747,#46748),
(#46749,#46750),(#46751,#46752),(#46753,#46754),(#46755,#46756),(#46757,
#46758),(#46759,#46760),(#46761,#46762),(#46763,#46764),(#46765,#46766),
(#46767,#46768),(#46769,#46770),(#46771,#46772),(#46773,#46774),(#46775,
#46776),(#46777,#46778),(#46779,#46780),(#46781,#46782),(#46783,#46784),
(#46785,#46786),(#46787,#46788),(#46789,#46790),(#46791,#46792),(#46793,
#46794),(#46795,#46796),(#46797,#46798),(#46799,#46800),(#46801,#46802),
(#46803,#46804),(#46805,#46806),(#46807,#46808),(#46809,#46810),(#46811,
#46812),(#46813,#46814),(#46815,#46816),(#46817,#46818),(#46819,#46820),
(#46821,#46822),(#46823,#46824),(#46825,#46826),(#46827,#46828),(#46829,
#46830),(#46831,#46832),(#46833,#46834),(#46835,#46836),(#46837,#46838),
(#46839,#46840),(#46841,#46842),(#46843,#46844),(#46845,#46846),(#46847,
#46848),(#46849,#46850),(#46851,#46852),(#46853,#46854),(#46855,#46856),
(#46857,#46858),(#46859,#46860),(#46861,#46862),(#46863,#46864),(#46865,
#46866),(#46867,#46868),(#46869,#46870),(#46871,#46872),(#46873,#46874),
(#46875,#46876),(#46877,#46878),(#46879,#46880),(#46881,#46882),(#46883,
#46884),(#46885,#46886),(#46887,#46888),(#46889,#46890),(#46891,#46892),
(#46893,#46894),(#46895,#46896),(#46897,#46898),(#46899,#46900),(#46901,
#46902),(#46903,#46904),(#46905,#46906),(#46907,#46908),(#46909,#46910),
(#46911,#46912),(#46913,#46914),(#46915,#46916),(#46917,#46918),(#46919,
#46920),(#46921,#46922),(#46923,#46924),(#46925,#46926),(#46927,#46928),
(#46929,#46930),(#46931,#46932),(#46933,#46934),(#46935,#46936),(#46937,
#46938),(#46939,#46940),(#46941,#46942),(#46943,#46944),(#46945,#46946),
(#46947,#46948),(#46949,#46950),(#46951,#46952),(#46953,#46954),(#46955,
#46956),(#46957,#46958),(#46959,#46960),(#46961,#46962),(#46963,#46964),
(#46965,#46966),(#46967,#46968),(#46969,#46970),(#46971,#46972),(#46973,
#46974),(#46975,#46976),(#46977,#46978),(#46979,#46980),(#46981,#46982),
(#46983,#46984),(#46985,#46986),(#46987,#46988),(#46989,#46990),(#46991,
#46992),(#46993,#46994),(#46995,#46996),(#46997,#46998),(#46999,#47000),
(#47001,#47002),(#47003,#47004),(#47005,#47006),(#47007,#47008),(#47009,
#47010),(#47011,#47012),(#47013,#47014),(#47015,#47016),(#47017,#47018),
(#47019,#47020),(#47021,#47022),(#47023,#47024),(#47025,#47026),(#47027,
#47028),(#47029,#47030),(#47031,#47032),(#47033,#47034),(#47035,#47036),
(#47037,#47038),(#47039,#47040),(#47041,#47042),(#47043,#47044),(#47045,
#47046),(#47047,#47048),(#47049,#47050),(#47051,#47052),(#47053,#47054),
(#47055,#47056),(#47057,#47058),(#47059,#47060),(#47061,#47062),(#47063,
#47064),(#47065,#47066),(#47067,#47068),(#47069,#47070),(#47071,#47072),
(#47073,#47074),(#47075,#47076),(#47077,#47078),(#47079,#47080),(#47081,
#47082),(#47083,#47084),(#47085,#47086),(#47087,#47088),(#47089,#47090),
(#47091,#47092),(#47093,#47094),(#47095,#47096),(#47097,#47098),(#47099,
#47100),(#47101,#47102),(#47103,#47104),(#47105,#47106),(#47107,#47108),
(#47109,#47110),(#47111,#47112),(#47113,#47114),(#47115,#47116),(#47117,
#47118),(#47119,#47120),(#47121,#47122),(#47123,#47124),(#47125,#47126),
(#47127,#47128),(#47129,#47130),(#47131,#47132),(#47133,#47134),(#47135,
#47136),(#47137,#47138),(#47139,#47140),(#47141,#47142),(#47143,#47144),
(#47145,#47146),(#47147,#47148),(#47149,#47150),(#47151,#47152),(#47153,
#47154),(#47155,#47156),(#47157,#47158),(#47159,#47160),(#47161,#47162),
(#47163,#47164),(#47165,#47166),(#47167,#47168),(#47169,#47170),(#47171,
#47172),(#47173,#47174),(#47175,#47176),(#47177,#47178),(#47179,#47180),
(#47181,#47182),(#47183,#47184),(#47185,#47186),(#47187,#47188),(#47189,
#47190),(#47191,#47192),(#47193,#47194),(#47195,#47196),(#47197,#47198),
(#47199,#47200),(#47201,#47202),(#47203,#47204),(#47205,#47206),(#47207,
#47208),(#47209,#47210),(#47211,#47212),(#47213,#47214),(#47215,#47216),
(#47217,#47218),(#47219,#47220),(#47221,#47222),(#47223,#47224),(#47225,
#47226),(#47227,#47228),(#47229,#47230),(#47231,#47232),(#47233,#47234),
(#47235,#47236),(#47237,#47238),(#47239,#47240),(#47241,#47242),(#47243,
#47244),(#47245,#47246),(#47247,#47248),(#47249,#47250),(#47251,#47252),
(#47253,#47254),(#47255,#47256),(#47257,#47258),(#47259,#47260),(#47261,
#47262),(#47263,#47264),(#47265,#47266),(#47267,#47268),(#47269,#47270),
(#47271,#47272),(#47273,#47274),(#47275,#47276),(#47277,#47278),(#47279,
#47280),(#47281,#47282),(#47283,#47284),(#47285,#47286),(#47287,#47288),
(#47289,#47290),(#47291,#47292),(#47293,#47294),(#47295,#47296),(#47297,
#47298),(#47299,#47300),(#47301,#47302),(#47303,#47304),(#47305,#47306),
(#47307,#47308),(#47309,#47310),(#47311,#47312),(#47313,#47314),(#47315,
#47316),(#47317,#47318),(#47319,#47320),(#47321,#47322),(#47323,#47324),
(#47325,#47326),(#47327,#47328),(#47329,#47330),(#47331,#47332),(#47333,
#47334),(#47335,#47336),(#47337,#47338),(#47339,#47340),(#47341,#47342),
(#47343,#47344),(#47345,#47346),(#47347,#47348),(#47349,#47350),(#47351,
#47352),(#47353,#47354),(#47355,#47356),(#47357,#47358),(#47359,#47360),
(#47361,#47362),(#47363,#47364),(#47365,#47366),(#47367,#47368),(#47369,
#47370),(#47371,#47372),(#47373,#47374),(#47375,#47376),(#47377,#47378),
(#47379,#47380),(#47381,#47382),(#47383,#47384),(#47385,#47386),(#47387,
#47388),(#47389,#47390),(#47391,#47392),(#47393,#47394),(#47395,#47396),
(#47397,#47398),(#47399,#47400),(#47401,#47402),(#47403,#47404),(#47405,
#47406),(#47407,#47408),(#47409,#47410),(#47411,#47412),(#47413,#47414),
(#47415,#47416),(#47417,#47418),(#47419,#47420),(#47421,#47422),(#47423,
#47424),(#47425,#47426),(#47427,#47428),(#47429,#47430),(#47431,#47432),
(#47433,#47434),(#47435,#47436),(#47437,#47438),(#47439,#47440),(#47441,
#47442),(#47443,#47444),(#47445,#47446),(#47447,#47448),(#47449,#47450),
(#47451,#47452),(#47453,#47454),(#47455,#47456),(#47457,#47458),(#47459,
#47460),(#47461,#47462),(#47463,#47464),(#47465,#47466),(#47467,#47468),
(#47469,#47470),(#47471,#47472),(#47473,#47474),(#47475,#47476),(#47477,
#47478),(#47479,#47480),(#47481,#47482),(#47483,#47484),(#47485,#47486),
(#47487,#47488),(#47489,#47490),(#47491,#47492),(#47493,#47494),(#47495,
#47496),(#47497,#47498),(#47499,#47500),(#47501,#47502),(#47503,#47504),
(#47505,#47506),(#47507,#47508),(#47509,#47510),(#47511,#47512),(#47513,
#47514),(#47515,#47516),(#47517,#47518),(#47519,#47520),(#47521,#47522),
(#47523,#47524),(#47525,#47526),(#47527,#47528),(#47529,#47530),(#47531,
#47532),(#47533,#47534),(#47535,#47536),(#47537,#47538),(#47539,#47540),
(#47541,#47542),(#47543,#47544),(#47545,#47546),(#47547,#47548),(#47549,
#47550),(#47551,#47552),(#47553,#47554),(#47555,#47556),(#47557,#47558),
(#47559,#47560),(#47561,#47562),(#47563,#47564),(#47565,#47566),(#47567,
#47568),(#47569,#47570),(#47571,#47572),(#47573,#47574),(#47575,#47576),
(#47577,#47578),(#47579,#47580),(#47581,#47582),(#47583,#47584),(#47585,
#47586),(#47587,#47588),(#47589,#47590),(#47591,#47592),(#47593,#47594),
(#47595,#47596),(#47597,#47598),(#47599,#47600),(#47601,#47602),(#47603,
#47604),(#47605,#47606),(#47607,#47608),(#47609,#47610),(#47611,#47612),
(#47613,#47614),(#47615,#47616),(#47617,#47618),(#47619,#47620),(#47621,
#47622),(#47623,#47624),(#47625,#47626),(#47627,#47628),(#47629,#47630),
(#47631,#47632),(#47633,#47634),(#47635,#47636),(#47637,#47638),(#47639,
#47640),(#47641,#47642),(#47643,#47644),(#47645,#47646),(#47647,#47648),
(#47649,#47650),(#47651,#47652),(#47653,#47654),(#47655,#47656),(#47657,
#47658),(#47659,#47660),(#47661,#47662),(#47663,#47664),(#47665,#47666),
(#47667,#47668),(#47669,#47670),(#47671,#47672),(#47673,#47674),(#47675,
#47676),(#47677,#47678),(#47679,#47680),(#47681,#47682),(#47683,#47684),
(#47685,#47686),(#47687,#47688),(#47689,#47690),(#47691,#47692),(#47693,
#47694),(#47695,#47696),(#47697,#47698),(#47699,#47700),(#47701,#47702),
(#47703,#47704),(#47705,#47706),(#47707,#47708),(#47709,#47710),(#47711,
#47712),(#47713,#47714),(#47715,#47716),(#47717,#47718),(#47719,#47720),
(#47721,#47722),(#47723,#47724),(#47725,#47726),(#47727,#47728),(#47729,
#47730),(#47731,#47732),(#47733,#47734),(#47735,#47736),(#47737,#47738),
(#47739,#47740),(#47741,#47742),(#47743,#47744),(#47745,#47746),(#47747,
#47748),(#47749,#47750),(#47751,#47752),(#47753,#47754),(#47755,#47756),
(#47757,#47758),(#47759,#47760),(#47761,#47762),(#47763,#47764),(#47765,
#47766),(#47767,#47768),(#47769,#47770),(#47771,#47772),(#47773,#47774),
(#47775,#47776),(#47777,#47778),(#47779,#47780),(#47781,#47782),(#47783,
#47784),(#47785,#47786),(#47787,#47788),(#47789,#47790),(#47791,#47792),
(#47793,#47794),(#47795,#47796),(#47797,#47798),(#47799,#47800),(#47801,
#47802),(#47803,#47804),(#47805,#47806),(#47807,#47808),(#47809,#47810),
(#47811,#47812),(#47813,#47814),(#47815,#47816),(#47817,#47818),(#47819,
#47820),(#47821,#47822),(#47823,#47824),(#47825,#47826),(#47827,#47828),
(#47829,#47830),(#47831,#47832),(#47833,#47834),(#47835,#47836),(#47837,
#47838),(#47839,#47840),(#47841,#47842),(#47843,#47844),(#47845,#47846),
(#47847,#47848),(#47849,#47850),(#47851,#47852),(#47853,#47854),(#47855,
#47856),(#47857,#47858),(#47859,#47860),(#47861,#47862),(#47863,#47864),
(#47865,#47866),(#47867,#47868),(#47869,#47870),(#47871,#47872),(#47873,
#47874),(#47875,#47876),(#47877,#47878),(#47879,#47880),(#47881,#47882),
(#47883,#47884),(#47885,#47886),(#47887,#47888),(#47889,#47890),(#47891,
#47892),(#47893,#47894),(#47895,#47896),(#47897,#47898),(#47899,#47900),
(#47901,#47902),(#47903,#47904),(#47905,#47906),(#47907,#47908),(#47909,
#47910),(#47911,#47912),(#47913,#47914),(#47915,#47916),(#47917,#47918),
(#47919,#47920),(#47921,#47922),(#47923,#47924),(#47925,#47926),(#47927,
#47928),(#47929,#47930),(#47931,#47932),(#47933,#47934),(#47935,#47936),
(#47937,#47938),(#47939,#47940),(#47941,#47942),(#47943,#47944),(#47945,
#47946),(#47947,#47948),(#47949,#47950),(#47951,#47952),(#47953,#47954),
(#47955,#47956),(#47957,#47958),(#47959,#47960),(#47961,#47962),(#47963,
#47964),(#47965,#47966),(#47967,#47968),(#47969,#47970),(#47971,#47972),
(#47973,#47974),(#47975,#47976),(#47977,#47978),(#47979,#47980),(#47981,
#47982),(#47983,#47984),(#47985,#47986),(#47987,#47988),(#47989,#47990),
(#47991,#47992),(#47993,#47994),(#47995,#47996),(#47997,#47998),(#47999,
#48000),(#48001,#48002),(#48003,#48004),(#48005,#48006),(#48007,#48008),
(#48009,#48010),(#48011,#48012),(#48013,#48014),(#48015,#48016),(#48017,
#48018),(#48019,#48020),(#48021,#48022),(#48023,#48024),(#48025,#48026),
(#48027,#48028),(#48029,#48030),(#48031,#48032),(#48033,#48034),(#48035,
#48036),(#48037,#48038),(#48039,#48040),(#48041,#48042),(#48043,#48044),
(#48045,#48046),(#48047,#48048),(#48049,#48050),(#48051,#48052),(#48053,
#48054),(#48055,#48056),(#48057,#48058),(#48059,#48060),(#48061,#48062),
(#48063,#48064),(#48065,#48066),(#48067,#48068),(#48069,#48070),(#48071,
#48072),(#48073,#48074),(#48075,#48076),(#48077,#48078),(#48079,#48080),
(#48081,#48082),(#48083,#48084),(#48085,#48086),(#48087,#48088),(#48089,
#48090),(#48091,#48092),(#48093,#48094),(#48095,#48096),(#48097,#48098),
(#48099,#48100),(#48101,#48102),(#48103,#48104),(#48105,#48106),(#48107,
#48108),(#48109,#48110),(#48111,#48112),(#48113,#48114),(#48115,#48116),
(#48117,#48118),(#48119,#48120),(#48121,#48122),(#48123,#48124),(#48125,
#48126),(#48127,#48128),(#48129,#48130),(#48131,#48132),(#48133,#48134),
(#48135,#48136),(#48137,#48138),(#48139,#48140),(#48141,#48142),(#48143,
#48144),(#48145,#48146),(#48147,#48148),(#48149,#48150),(#48151,#48152),
(#48153,#48154),(#48155,#48156),(#48157,#48158),(#48159,#48160),(#48161,
#48162),(#48163,#48164),(#48165,#48166),(#48167,#48168),(#48169,#48170),
(#48171,#48172),(#48173,#48174),(#48175,#48176),(#48177,#48178),(#48179,
#48180),(#48181,#48182),(#48183,#48184),(#48185,#48186),(#48187,#48188),
(#48189,#48190),(#48191,#48192),(#48193,#48194),(#48195,#48196),(#48197,
#48198),(#48199,#48200),(#48201,#48202),(#48203,#48204),(#48205,#48206),
(#48207,#48208),(#48209,#48210),(#48211,#48212),(#48213,#48214),(#48215,
#48216),(#48217,#48218),(#48219,#48220),(#48221,#48222),(#48223,#48224),
(#48225,#48226),(#48227,#48228),(#48229,#48230),(#48231,#48232),(#48233,
#48234),(#48235,#48236),(#48237,#48238),(#48239,#48240),(#48241,#48242),
(#48243,#48244),(#48245,#48246),(#48247,#48248),(#48249,#48250),(#48251,
#48252),(#48253,#48254),(#48255,#48256),(#48257,#48258),(#48259,#48260),
(#48261,#48262),(#48263,#48264),(#48265,#48266),(#48267,#48268),(#48269,
#48270),(#48271,#48272),(#48273,#48274),(#48275,#48276),(#48277,#48278),
(#48279,#48280),(#48281,#48282),(#48283,#48284),(#48285,#48286),(#48287,
#48288),(#48289,#48290),(#48291,#48292),(#48293,#48294),(#48295,#48296),
(#48297,#48298),(#48299,#48300),(#48301,#48302),(#48303,#48304),(#48305,
#48306),(#48307,#48308),(#48309,#48310),(#48311,#48312),(#48313,#48314),
(#48315,#48316),(#48317,#48318),(#48319,#48320),(#48321,#48322),(#48323,
#48324),(#48325,#48326),(#48327,#48328),(#48329,#48330),(#48331,#48332),
(#48333,#48334),(#48335,#48336),(#48337,#48338),(#48339,#48340),(#48341,
#48342),(#48343,#48344),(#48345,#48346),(#48347,#48348),(#48349,#48350),
(#48351,#48352),(#48353,#48354),(#48355,#48356),(#48357,#48358),(#48359,
#48360),(#48361,#48362),(#48363,#48364),(#48365,#48366),(#48367,#48368),
(#48369,#48370),(#48371,#48372),(#48373,#48374),(#48375,#48376),(#48377,
#48378),(#48379,#48380),(#48381,#48382),(#48383,#48384),(#48385,#48386),
(#48387,#48388),(#48389,#48390),(#48391,#48392),(#48393,#48394),(#48395,
#48396),(#48397,#48398),(#48399,#48400),(#48401,#48402),(#48403,#48404),
(#48405,#48406),(#48407,#48408),(#48409,#48410),(#48411,#48412),(#48413,
#48414),(#48415,#48416),(#48417,#48418),(#48419,#48420),(#48421,#48422),
(#48423,#48424),(#48425,#48426),(#48427,#48428),(#48429,#48430),(#48431,
#48432),(#48433,#48434),(#48435,#48436),(#48437,#48438),(#48439,#48440),
(#48441,#48442),(#48443,#48444),(#48445,#48446),(#48447,#48448),(#48449,
#48450),(#48451,#48452),(#48453,#48454),(#48455,#48456),(#48457,#48458),
(#48459,#48460),(#48461,#48462),(#48463,#48464),(#48465,#48466),(#48467,
#48468),(#48469,#48470),(#48471,#48472),(#48473,#48474),(#48475,#48476),
(#48477,#48478),(#48479,#48480),(#48481,#48482),(#48483,#48484),(#48485,
#48486),(#48487,#48488),(#48489,#48490),(#48491,#48492),(#48493,#48494),
(#48495,#48496),(#48497,#48498),(#48499,#48500),(#48501,#48502),(#48503,
#48504),(#48505,#48506),(#48507,#48508),(#48509,#48510),(#48511,#48512),
(#48513,#48514),(#48515,#48516),(#48517,#48518),(#48519,#48520),(#48521,
#48522),(#48523,#48524),(#48525,#48526),(#48527,#48528),(#48529,#48530),
(#48531,#48532),(#48533,#48534),(#48535,#48536),(#48537,#48538),(#48539,
#48540),(#48541,#48542),(#48543,#48544),(#48545,#48546),(#48547,#48548),
(#48549,#48550),(#48551,#48552),(#48553,#48554),(#48555,#48556),(#48557,
#48558),(#48559,#48560),(#48561,#48562),(#48563,#48564),(#48565,#48566),
(#48567,#48568),(#48569,#48570),(#48571,#48572),(#48573,#48574),(#48575,
#48576),(#48577,#48578),(#48579,#48580),(#48581,#48582),(#48583,#48584),
(#48585,#48586),(#48587,#48588),(#48589,#48590),(#48591,#48592),(#48593,
#48594),(#48595,#48596),(#48597,#48598),(#48599,#48600),(#48601,#48602),
(#48603,#48604),(#48605,#48606),(#48607,#48608),(#48609,#48610),(#48611,
#48612),(#48613,#48614),(#48615,#48616),(#48617,#48618),(#48619,#48620),
(#48621,#48622),(#48623,#48624),(#48625,#48626),(#48627,#48628),(#48629,
#48630),(#48631,#48632),(#48633,#48634),(#48635,#48636),(#48637,#48638),
(#48639,#48640),(#48641,#48642),(#48643,#48644),(#48645,#48646),(#48647,
#48648),(#48649,#48650),(#48651,#48652),(#48653,#48654),(#48655,#48656),
(#48657,#48658),(#48659,#48660),(#48661,#48662),(#48663,#48664),(#48665,
#48666),(#48667,#48668),(#48669,#48670),(#48671,#48672),(#48673,#48674),
(#48675,#48676),(#48677,#48678),(#48679,#48680),(#48681,#48682),(#48683,
#48684),(#48685,#48686),(#48687,#48688),(#48689,#48690),(#48691,#48692),
(#48693,#48694),(#48695,#48696),(#48697,#48698),(#48699,#48700),(#48701,
#48702),(#48703,#48704),(#48705,#48706),(#48707,#48708),(#48709,#48710),
(#48711,#48712),(#48713,#48714),(#48715,#48716),(#48717,#48718),(#48719,
#48720),(#48721,#48722),(#48723,#48724),(#48725,#48726),(#48727,#48728),
(#48729,#48730),(#48731,#48732),(#48733,#48734),(#48735,#48736),(#48737,
#48738),(#48739,#48740),(#48741,#48742),(#48743,#48744),(#48745,#48746),
(#48747,#48748),(#48749,#48750),(#48751,#48752),(#48753,#48754),(#48755,
#48756),(#48757,#48758),(#48759,#48760),(#48761,#48762),(#48763,#48764),
(#48765,#48766),(#48767,#48768),(#48769,#48770),(#48771,#48772),(#48773,
#48774),(#48775,#48776),(#48777,#48778),(#48779,#48780),(#48781,#48782),
(#48783,#48784),(#48785,#48786),(#48787,#48788),(#48789,#48790),(#48791,
#48792),(#48793,#48794),(#48795,#48796),(#48797,#48798),(#48799,#48800),
(#48801,#48802),(#48803,#48804),(#48805,#48806),(#48807,#48808),(#48809,
#48810),(#48811,#48812),(#48813,#48814),(#48815,#48816),(#48817,#48818),
(#48819,#48820),(#48821,#48822),(#48823,#48824),(#48825,#48826),(#48827,
#48828),(#48829,#48830),(#48831,#48832),(#48833,#48834),(#48835,#48836),
(#48837,#48838),(#48839,#48840),(#48841,#48842),(#48843,#48844),(#48845,
#48846),(#48847,#48848),(#48849,#48850),(#48851,#48852),(#48853,#48854),
(#48855,#48856),(#48857,#48858),(#48859,#48860),(#48861,#48862),(#48863,
#48864),(#48865,#48866),(#48867,#48868),(#48869,#48870),(#48871,#48872),
(#48873,#48874),(#48875,#48876),(#48877,#48878),(#48879,#48880),(#48881,
#48882),(#48883,#48884),(#48885,#48886),(#48887,#48888),(#48889,#48890),
(#48891,#48892),(#48893,#48894),(#48895,#48896),(#48897,#48898),(#48899,
#48900),(#48901,#48902),(#48903,#48904),(#48905,#48906),(#48907,#48908),
(#48909,#48910),(#48911,#48912),(#48913,#48914),(#48915,#48916),(#48917,
#48918),(#48919,#48920),(#48921,#48922),(#48923,#48924),(#48925,#48926),
(#48927,#48928),(#48929,#48930),(#48931,#48932),(#48933,#48934),(#48935,
#48936),(#48937,#48938),(#48939,#48940),(#48941,#48942),(#48943,#48944),
(#48945,#48946),(#48947,#48948),(#48949,#48950),(#48951,#48952),(#48953,
#48954),(#48955,#48956),(#48957,#48958),(#48959,#48960),(#48961,#48962),
(#48963,#48964),(#48965,#48966),(#48967,#48968),(#48969,#48970),(#48971,
#48972),(#48973,#48974),(#48975,#48976),(#48977,#48978),(#48979,#48980),
(#48981,#48982),(#48983,#48984),(#48985,#48986),(#48987,#48988),(#48989,
#48990),(#48991,#48992),(#48993,#48994),(#48995,#48996),(#48997,#48998),
(#48999,#49000),(#49001,#49002),(#49003,#49004),(#49005,#49006),(#49007,
#49008),(#49009,#49010),(#49011,#49012),(#49013,#49014),(#49015,#49016),
(#49017,#49018),(#49019,#49020),(#49021,#49022),(#49023,#49024),(#49025,
#49026),(#49027,#49028),(#49029,#49030),(#49031,#49032),(#49033,#49034),
(#49035,#49036),(#49037,#49038),(#49039,#49040),(#49041,#49042),(#49043,
#49044),(#49045,#49046),(#49047,#49048),(#49049,#49050),(#49051,#49052),
(#49053,#49054),(#49055,#49056),(#49057,#49058),(#49059,#49060),(#49061,
#49062),(#49063,#49064),(#49065,#49066),(#49067,#49068),(#49069,#49070),
(#49071,#49072),(#49073,#49074),(#49075,#49076),(#49077,#49078),(#49079,
#49080),(#49081,#49082),(#49083,#49084),(#49085,#49086),(#49087,#49088),
(#49089,#49090),(#49091,#49092),(#49093,#49094),(#49095,#49096),(#49097,
#49098),(#49099,#49100),(#49101,#49102),(#49103,#49104),(#49105,#49106),
(#49107,#49108),(#49109,#49110),(#49111,#49112),(#49113,#49114),(#49115,
#49116),(#49117,#49118),(#49119,#49120),(#49121,#49122),(#49123,#49124),
(#49125,#49126),(#49127,#49128),(#49129,#49130),(#49131,#49132),(#49133,
#49134),(#49135,#49136),(#49137,#49138),(#49139,#49140),(#49141,#49142),
(#49143,#49144),(#49145,#49146),(#49147,#49148),(#49149,#49150),(#49151,
#49152),(#49153,#49154),(#49155,#49156),(#49157,#49158),(#49159,#49160),
(#49161,#49162),(#49163,#49164),(#49165,#49166),(#49167,#49168),(#49169,
#49170),(#49171,#49172),(#49173,#49174),(#49175,#49176),(#49177,#49178),
(#49179,#49180),(#49181,#49182),(#49183,#49184),(#49185,#49186),(#49187,
#49188),(#49189,#49190),(#49191,#49192),(#49193,#49194),(#49195,#49196),
(#49197,#49198),(#49199,#49200),(#49201,#49202),(#49203,#49204),(#49205,
#49206),(#49207,#49208),(#49209,#49210),(#49211,#49212),(#49213,#49214),
(#49215,#49216),(#49217,#49218),(#49219,#49220),(#49221,#49222),(#49223,
#49224),(#49225,#49226),(#49227,#49228),(#49229,#49230),(#49231,#49232),
(#49233,#49234),(#49235,#49236),(#49237,#49238),(#49239,#49240),(#49241,
#49242),(#49243,#49244),(#49245,#49246),(#49247,#49248),(#49249,#49250),
(#49251,#49252),(#49253,#49254),(#49255,#49256),(#49257,#49258),(#49259,
#49260),(#49261,#49262),(#49263,#49264),(#49265,#49266),(#49267,#49268),
(#49269,#49270),(#49271,#49272),(#49273,#49274),(#49275,#49276),(#49277,
#49278),(#49279,#49280),(#49281,#49282),(#49283,#49284),(#49285,#49286),
(#49287,#49288),(#49289,#49290),(#49291,#49292),(#49293,#49294),(#49295,
#49296),(#49297,#49298),(#49299,#49300),(#49301,#49302),(#49303,#49304),
(#49305,#49306),(#49307,#49308),(#49309,#49310),(#49311,#49312),(#49313,
#49314),(#49315,#49316),(#49317,#49318),(#49319,#49320),(#49321,#49322),
(#49323,#49324),(#49325,#49326),(#49327,#49328),(#49329,#49330),(#49331,
#49332),(#49333,#49334),(#49335,#49336),(#49337,#49338),(#49339,#49340),
(#49341,#49342),(#49343,#49344),(#49345,#49346),(#49347,#49348),(#49349,
#49350),(#49351,#49352),(#49353,#49354),(#49355,#49356),(#49357,#49358),
(#49359,#49360),(#49361,#49362),(#49363,#49364),(#49365,#49366),(#49367,
#49368),(#49369,#49370),(#49371,#49372),(#49373,#49374),(#49375,#49376),
(#49377,#49378),(#49379,#49380),(#49381,#49382),(#49383,#49384),(#49385,
#49386),(#49387,#49388),(#49389,#49390),(#49391,#49392),(#49393,#49394),
(#49395,#49396),(#49397,#49398),(#49399,#49400),(#49401,#49402),(#49403,
#49404),(#49405,#49406),(#49407,#49408),(#49409,#49410),(#49411,#49412),
(#49413,#49414),(#49415,#49416),(#49417,#49418),(#49419,#49420),(#49421,
#49422),(#49423,#49424),(#49425,#49426),(#49427,#49428),(#49429,#49430),
(#49431,#49432),(#49433,#49434),(#49435,#49436),(#49437,#49438),(#49439,
#49440),(#49441,#49442),(#49443,#49444),(#49445,#49446),(#49447,#49448),
(#49449,#49450),(#49451,#49452),(#49453,#49454),(#49455,#49456),(#49457,
#49458),(#49459,#49460),(#49461,#49462),(#49463,#49464),(#49465,#49466),
(#49467,#49468),(#49469,#49470),(#49471,#49472),(#49473,#49474),(#49475,
#49476),(#49477,#49478),(#49479,#49480),(#49481,#49482),(#49483,#49484),
(#49485,#49486),(#49487,#49488),(#49489,#49490),(#49491,#49492),(#49493,
#49494),(#49495,#49496),(#49497,#49498),(#49499,#49500),(#49501,#49502),
(#49503,#49504),(#49505,#49506),(#49507,#49508),(#49509,#49510),(#49511,
#49512),(#49513,#49514),(#49515,#49516),(#49517,#49518),(#49519,#49520),
(#49521,#49522),(#49523,#49524),(#49525,#49526),(#49527,#49528),(#49529,
#49530),(#49531,#49532),(#49533,#49534),(#49535,#49536),(#49537,#49538),
(#49539,#49540),(#49541,#49542),(#49543,#49544),(#49545,#49546),(#49547,
#49548),(#49549,#49550),(#49551,#49552),(#49553,#49554),(#49555,#49556),
(#49557,#49558),(#49559,#49560),(#49561,#49562),(#49563,#49564),(#49565,
#49566),(#49567,#49568),(#49569,#49570),(#49571,#49572),(#49573,#49574),
(#49575,#49576),(#49577,#49578),(#49579,#49580),(#49581,#49582),(#49583,
#49584),(#49585,#49586),(#49587,#49588),(#49589,#49590),(#49591,#49592),
(#49593,#49594),(#49595,#49596),(#49597,#49598),(#49599,#49600),(#49601,
#49602),(#49603,#49604),(#49605,#49606),(#49607,#49608),(#49609,#49610),
(#49611,#49612),(#49613,#49614),(#49615,#49616),(#49617,#49618),(#49619,
#49620),(#49621,#49622),(#49623,#49624),(#49625,#49626),(#49627,#49628),
(#49629,#49630),(#49631,#49632),(#49633,#49634),(#49635,#49636),(#49637,
#49638),(#49639,#49640),(#49641,#49642),(#49643,#49644),(#49645,#49646),
(#49647,#49648),(#49649,#49650),(#49651,#49652),(#49653,#49654),(#49655,
#49656),(#49657,#49658),(#49659,#49660),(#49661,#49662),(#49663,#49664),
(#49665,#49666),(#49667,#49668),(#49669,#49670),(#49671,#49672),(#49673,
#49674),(#49675,#49676),(#49677,#49678),(#49679,#49680),(#49681,#49682),
(#49683,#49684),(#49685,#49686),(#49687,#49688),(#49689,#49690),(#49691,
#49692),(#49693,#49694),(#49695,#49696),(#49697,#49698),(#49699,#49700),
(#49701,#49702),(#49703,#49704),(#49705,#49706),(#49707,#49708),(#49709,
#49710),(#49711,#49712),(#49713,#49714),(#49715,#49716),(#49717,#49718),
(#49719,#49720),(#49721,#49722),(#49723,#49724),(#49725,#49726),(#49727,
#49728),(#49729,#49730),(#49731,#49732),(#49733,#49734),(#49735,#49736),
(#49737,#49738),(#49739,#49740),(#49741,#49742),(#49743,#49744),(#49745,
#49746),(#49747,#49748),(#49749,#49750),(#49751,#49752),(#49753,#49754),
(#49755,#49756),(#49757,#49758),(#49759,#49760),(#49761,#49762),(#49763,
#49764),(#49765,#49766),(#49767,#49768),(#49769,#49770),(#49771,#49772),
(#49773,#49774),(#49775,#49776),(#49777,#49778),(#49779,#49780),(#49781,
#49782),(#49783,#49784),(#49785,#49786),(#49787,#49788),(#49789,#49790),
(#49791,#49792),(#49793,#49794),(#49795,#49796),(#49797,#49798),(#49799,
#49800),(#49801,#49802),(#49803,#49804),(#49805,#49806),(#49807,#49808),
(#49809,#49810),(#49811,#49812),(#49813,#49814),(#49815,#49816),(#49817,
#49818),(#49819,#49820),(#49821,#49822),(#49823,#49824),(#49825,#49826),
(#49827,#49828),(#49829,#49830),(#49831,#49832),(#49833,#49834),(#49835,
#49836),(#49837,#49838),(#49839,#49840),(#49841,#49842),(#49843,#49844),
(#49845,#49846),(#49847,#49848),(#49849,#49850),(#49851,#49852),(#49853,
#49854),(#49855,#49856),(#49857,#49858),(#49859,#49860),(#49861,#49862),
(#49863,#49864),(#49865,#49866),(#49867,#49868),(#49869,#49870),(#49871,
#49872),(#49873,#49874),(#49875,#49876),(#49877,#49878),(#49879,#49880),
(#49881,#49882),(#49883,#49884),(#49885,#49886),(#49887,#49888),(#49889,
#49890),(#49891,#49892),(#49893,#49894),(#49895,#49896),(#49897,#49898),
(#49899,#49900),(#49901,#49902),(#49903,#49904),(#49905,#49906),(#49907,
#49908),(#49909,#49910),(#49911,#49912),(#49913,#49914),(#49915,#49916),
(#49917,#49918),(#49919,#49920),(#49921,#49922),(#49923,#49924),(#49925,
#49926),(#49927,#49928),(#49929,#49930),(#49931,#49932),(#49933,#49934),
(#49935,#49936),(#49937,#49938),(#49939,#49940),(#49941,#49942),(#49943,
#49944),(#49945,#49946),(#49947,#49948),(#49949,#49950),(#49951,#49952),
(#49953,#49954),(#49955,#49956),(#49957,#49958),(#49959,#49960),(#49961,
#49962),(#49963,#49964),(#49965,#49966),(#49967,#49968),(#49969,#49970),
(#49971,#49972),(#49973,#49974),(#49975,#49976),(#49977,#49978),(#49979,
#49980),(#49981,#49982),(#49983,#49984),(#49985,#49986),(#49987,#49988),
(#49989,#49990),(#49991,#49992),(#49993,#49994),(#49995,#49996),(#49997,
#49998),(#49999,#50000),(#50001,#50002),(#50003,#50004),(#50005,#50006),
(#50007,#50008),(#50009,#50010),(#50011,#50012),(#50013,#50014),(#50015,
#50016),(#50017,#50018),(#50019,#50020),(#50021,#50022),(#50023,#50024),
(#50025,#50026),(#50027,#50028),(#50029,#50030),(#50031,#50032),(#50033,
#50034),(#50035,#50036),(#50037,#50038),(#50039,#50040),(#50041,#50042),
(#50043,#50044),(#50045,#50046),(#50047,#50048),(#50049,#50050),(#50051,
#50052),(#50053,#50054),(#50055,#50056),(#50057,#50058),(#50059,#50060),
(#50061,#50062),(#50063,#50064),(#50065,#50066),(#50067,#50068),(#50069,
#50070),(#50071,#50072),(#50073,#50074),(#50075,#50076),(#50077,#50078),
(#50079,#50080),(#50081,#50082),(#50083,#50084),(#50085,#50086),(#50087,
#50088),(#50089,#50090),(#50091,#50092),(#50093,#50094),(#50095,#50096),
(#50097,#50098),(#50099,#50100),(#50101,#50102),(#50103,#50104),(#50105,
#50106),(#50107,#50108),(#50109,#50110),(#50111,#50112),(#50113,#50114),
(#50115,#50116),(#50117,#50118),(#50119,#50120),(#50121,#50122),(#50123,
#50124),(#50125,#50126),(#50127,#50128),(#50129,#50130),(#50131,#50132),
(#50133,#50134),(#50135,#50136),(#50137,#50138),(#50139,#50140),(#50141,
#50142),(#50143,#50144),(#50145,#50146),(#50147,#50148),(#50149,#50150),
(#50151,#50152),(#50153,#50154),(#50155,#50156),(#50157,#50158),(#50159,
#50160),(#50161,#50162),(#50163,#50164),(#50165,#50166),(#50167,#50168),
(#50169,#50170),(#50171,#50172),(#50173,#50174),(#50175,#50176),(#50177,
#50178),(#50179,#50180),(#50181,#50182),(#50183,#50184),(#50185,#50186),
(#50187,#50188),(#50189,#50190),(#50191,#50192),(#50193,#50194),(#50195,
#50196),(#50197,#50198),(#50199,#50200),(#50201,#50202),(#50203,#50204),
(#50205,#50206),(#50207,#50208),(#50209,#50210),(#50211,#50212),(#50213,
#50214),(#50215,#50216),(#50217,#50218),(#50219,#50220),(#50221,#50222)),
 .UNSPECIFIED.,.F.,.F.,.F.,(4,1,1,1,1,1,1,1,1,1,1,1,1,1,1,1,1,1,1,1,1,1,
1,1,1,1,1,1,1,1,1,1,1,1,1,1,1,1,1,1,1,1,1,1,1,1,1,1,1,1,1,1,1,1,1,1,1,1,
1,1,1,1,1,1,1,1,1,1,1,1,1,1,1,1,1,1,1,1,1,1,1,1,1,1,1,1,1,1,1,1,1,1,1,1,
1,1,1,1,1,1,1,1,1,1,1,1,1,1,1,1,1,1,1,1,1,1,1,1,1,1,1,1,1,1,1,1,1,1,1,1,
1,1,1,1,1,1,1,1,1,1,1,1,1,1,1,1,1,1,1,1,1,1,1,1,1,1,1,1,1,1,1,1,1,1,1,1,
1,1,1,1,1,1,1,1,1,1,1,1,1,1,1,1,1,1,1,1,1,1,1,1,1,1,1,1,1,1,1,1,1,1,1,1,
1,1,1,1,1,1,1,1,1,1,1,1,1,1,1,1,1,1,1,1,1,1,1,1,1,1,1,1,1,1,1,1,1,1,1,1,
1,1,1,1,1,1,1,1,1,1,1,1,1,1,1,1,1,1,1,1,1,1,1,1,1,1,1,1,1,1,1,1,1,1,1,1,
1,1,1,1,1,1,1,1,1,1,1,1,1,1,1,1,1,1,1,1,1,1,1,1,1,1,1,1,1,1,1,1,1,1,1,1,
1,1,1,1,1,1,1,1,1,1,1,1,1,1,1,1,1,1,1,1,1,1,1,1,1,1,1,1,1,1,1,1,1,1,1,1,
1,1,1,1,1,1,1,1,1,1,1,1,1,1,1,1,1,1,1,1,1,1,1,1,1,1,1,1,1,1,1,1,1,1,1,1,
1,1,1,1,1,1,1,1,1,1,1,1,1,1,1,1,1,1,1,1,1,1,1,1,1,1,1,1,1,1,1,1,1,1,1,1,
1,1,1,1,1,1,1,1,1,1,1,1,1,1,1,1,1,1,1,1,1,1,1,1,1,1,1,1,1,1,1,1,1,1,1,1,
1,1,1,1,1,1,1,1,1,1,1,1,1,1,1,1,1,1,1,1,1,1,1,1,1,1,1,1,1,1,1,1,1,1,1,1,
1,1,1,1,1,1,1,1,1,1,1,1,1,1,1,1,1,1,1,1,1,1,1,1,1,1,1,1,1,1,1,1,1,1,1,1,
1,1,1,1,1,1,1,1,1,1,1,1,1,1,1,1,1,1,1,1,1,1,1,1,1,1,1,1,1,1,1,1,1,1,1,1,
1,1,1,1,1,1,1,1,1,1,1,1,1,1,1,1,1,1,1,1,1,1,1,1,1,1,1,1,1,1,1,1,1,1,1,1,
1,1,1,1,1,1,1,1,1,1,1,1,1,1,1,1,1,1,1,1,1,1,1,1,1,1,1,1,1,1,1,1,1,1,1,1,
1,1,1,1,1,1,1,1,1,1,1,1,1,1,1,1,1,1,1,1,1,1,1,1,1,1,1,1,1,1,1,1,1,1,1,1,
1,1,1,1,1,1,1,1,1,1,1,1,1,1,1,1,1,1,1,1,1,1,1,1,1,1,1,1,1,1,1,1,1,1,1,1,
1,1,1,1,1,1,1,1,1,1,1,1,1,1,1,1,1,1,1,1,1,1,1,1,1,1,1,1,1,1,1,1,1,1,1,1,
1,1,1,1,1,1,1,1,1,1,1,1,1,1,1,1,1,1,1,1,1,1,1,1,1,1,1,1,1,1,1,1,1,1,1,1,
1,1,1,1,1,1,1,1,1,1,1,1,1,1,1,1,1,1,1,1,1,1,1,1,1,1,1,1,1,1,1,1,1,1,1,1,
1,1,1,1,1,1,1,1,1,1,1,1,1,1,1,1,1,1,1,1,1,1,1,1,1,1,1,1,1,1,1,1,1,1,1,1,
1,1,1,1,1,1,1,1,1,1,1,1,1,1,1,1,1,1,1,1,1,1,1,1,1,1,1,1,1,1,1,1,1,1,1,1,
1,1,1,1,1,1,1,1,1,1,1,1,1,1,1,1,1,1,1,1,1,1,1,1,1,1,1,1,1,1,1,1,1,1,1,1,
1,1,1,1,1,1,1,1,1,1,1,1,1,1,1,1,1,1,1,1,1,1,1,1,1,1,1,1,1,1,1,1,1,1,1,1,
1,1,1,1,1,1,1,1,1,1,1,1,1,1,1,1,1,1,1,1,1,1,1,1,1,1,1,1,1,1,1,1,1,1,1,1,
1,1,1,1,1,1,1,1,1,1,1,1,1,1,1,1,1,1,1,1,1,1,1,1,1,1,1,1,1,1,1,1,1,1,1,1,
1,1,1,1,1,1,1,1,1,1,1,1,1,1,1,1,1,1,1,1,1,1,1,1,1,1,1,1,1,1,1,1,1,1,1,1,
1,1,1,1,1,1,1,1,1,1,1,1,1,1,1,1,1,1,1,1,1,1,1,1,1,1,1,1,1,1,1,1,1,1,1,1,
1,1,1,1,1,1,1,1,1,1,1,1,1,1,1,1,1,1,1,1,1,1,1,1,1,1,1,1,1,1,1,1,1,1,1,1,
1,1,1,1,1,1,1,1,1,1,1,1,1,1,1,1,1,1,1,1,1,1,1,1,1,1,1,1,1,1,1,1,1,1,1,1,
1,1,1,1,1,1,1,1,1,1,1,1,1,1,1,1,1,1,1,1,1,1,1,1,1,1,1,1,1,1,1,1,1,1,1,1,
1,1,1,1,1,1,1,1,1,1,1,1,1,1,1,1,1,1,1,1,1,1,1,1,1,1,1,1,1,1,1,1,1,1,1,1,
1,1,1,1,1,1,1,1,1,1,1,1,1,1,1,1,1,1,1,1,1,1,1,1,1,1,1,1,1,1,1,1,1,1,1,1,
1,1,1,1,1,1,1,1,1,1,1,1,1,1,1,1,1,1,1,1,1,1,1,1,1,1,1,1,1,1,1,1,1,1,1,1,
1,1,1,1,1,1,1,1,1,1,1,1,1,1,1,1,1,1,1,1,1,1,1,1,1,1,1,1,1,1,1,1,1,1,1,1,
1,1,1,1,1,1,1,1,1,1,1,1,1,1,1,1,1,1,1,1,1,1,1,1,1,1,1,1,1,1,1,1,1,1,1,1,
1,1,1,1,1,1,1,1,1,1,1,1,1,1,1,1,1,1,1,1,1,1,1,1,1,1,1,1,1,1,1,1,1,1,1,1,
1,1,1,1,1,1,1,1,1,1,1,1,1,1,1,1,1,1,1,1,1,1,1,1,1,1,1,1,1,1,1,1,1,1,1,1,
1,1,1,1,1,1,1,1,1,1,1,1,1,1,1,1,1,1,1,1,1,1,1,1,1,1,1,1,1,1,1,1,1,1,1,1,
1,1,1,1,1,1,1,1,1,1,1,1,1,1,1,1,1,1,1,1,1,1,1,1,1,1,1,1,1,1,1,1,1,1,1,1,
1,1,1,1,1,1,1,1,1,1,1,1,1,1,1,1,1,1,1,1,1,1,1,1,1,1,1,1,1,1,1,1,1,1,1,1,
1,1,1,1,1,1,1,1,1,1,1,1,1,1,1,1,1,1,1,1,1,1,1,1,1,1,1,1,1,1,1,1,1,1,1,1,
1,1,1,1,1,1,1,1,1,1,1,1,1,1,1,1,1,1,1,1,1,1,1,1,1,1,1,1,1,1,1,1,1,1,1,1,
1,1,1,1,1,1,1,1,1,1,1,1,1,1,1,1,1,1,1,1,1,1,1,1,1,1,1,1,1,1,1,1,1,1,1,1,
1,1,1,1,1,1,1,1,1,1,1,1,1,1,1,1,1,1,1,1,1,1,1,1,1,1,1,1,1,1,1,1,1,1,1,1,
1,1,1,1,1,1,1,1,1,1,1,1,1,1,1,1,1,1,1,1,1,1,1,1,1,1,1,1,1,1,1,1,1,1,1,1,
1,1,1,1,1,1,1,1,1,1,1,1,1,1,1,1,1,1,1,1,1,1,1,1,1,1,1,1,1,1,1,1,1,1,1,1,
1,1,1,1,1,1,1,1,1,1,1,1,1,1,1,1,1,1,1,1,1,1,1,1,1,1,1,1,1,1,1,1,1,1,1,1,
1,1,1,1,1,1,1,1,1,1,1,1,1,1,1,1,1,1,1,1,1,1,1,1,1,1,1,1,1,1,1,1,1,1,1,1,
1,1,1,1,1,1,1,1,1,1,1,1,1,1,1,1,1,1,1,1,1,1,1,1,1,1,1,1,1,1,1,1,1,1,1,1,
1,1,1,1,1,1,1,1,1,1,1,1,1,1,1,1,1,1,1,1,1,1,1,1,1,1,1,1,1,1,1,1,1,1,1,1,
1,1,1,1,1,1,1,1,1,1,1,1,1,1,1,1,1,1,1,1,1,1,1,1,1,1,1,1,1,1,1,1,1,1,1,1,
1,1,1,1,1,1,1,1,1,1,1,1,1,1,1,1,1,1,1,1,1,1,1,1,1,1,1,1,1,1,1,1,1,1,1,1,
1,1,1,1,1,1,1,1,1,1,1,1,1,1,1,1,1,1,1,1,1,1,1,1,1,1,1,1,1,1,1,1,1,1,1,1,
1,1,1,1,1,1,1,1,1,1,1,1,1,1,1,1,1,1,1,1,1,1,1,1,1,1,1,1,1,1,1,1,1,1,1,1,
1,1,1,1,1,1,1,1,1,1,1,1,1,1,1,1,1,1,1,1,1,1,1,1,1,1,1,1,1,1,1,1,1,1,1,1,
1,1,1,1,1,1,1,1,1,1,1,1,1,1,1,1,1,1,1,1,1,1,1,1,1,1,1,1,1,1,1,1,1,1,1,1,
1,1,1,1,1,1,1,1,1,1,1,1,1,1,1,1,1,1,1,1,1,1,1,1,1,1,1,1,1,1,1,1,1,1,1,1,
1,1,1,1,1,1,1,1,1,1,1,1,1,1,1,1,1,1,1,1,1,1,1,1,1,1,1,1,1,1,1,1,1,1,1,1,
1,1,1,1,1,1,1,1,1,1,1,1,1,1,1,1,1,1,1,1,1,1,1,1,1,1,1,1,1,1,1,1,1,1,1,1,
1,1,1,1,1,1,1,1,1,1,1,1,1,1,1,1,1,1,1,1,1,1,1,1,1,1,1,1,1,1,1,1,1,1,1,1,
1,1,1,1,1,1,1,1,1,1,1,1,1,1,1,1,1,1,1,1,1,1,1,1,1,1,1,1,1,1,1,1,1,1,1,1,
1,1,1,1,1,1,1,1,1,1,1,1,1,1,1,1,1,1,1,1,1,1,1,1,1,1,1,1,1,1,1,1,1,1,1,1,
1,1,1,1,1,1,1,1,1,1,1,1,1,1,1,1,1,1,1,1,1,1,1,1,1,1,1,1,1,1,1,1,1,1,1,1,
1,1,1,1,1,1,1,1,1,1,1,1,1,1,1,1,1,1,1,1,1,1,1,1,1,1,1,1,1,1,1,1,1,1,1,1,
1,1,1,1,1,1,1,1,1,1,1,1,1,1,1,1,1,1,1,1,1,1,1,1,1,1,1,1,1,1,1,1,1,1,1,1,
1,1,1,1,1,1,1,1,1,1,1,1,1,1,1,1,1,1,1,1,1,1,1,1,1,1,1,1,1,1,1,1,1,1,1,1,
1,1,1,1,1,1,1,1,1,1,1,1,1,1,1,1,1,1,1,1,1,1,1,1,1,1,1,1,1,1,1,1,1,1,1,1,
1,1,1,1,1,1,1,1,1,1,1,1,1,1,1,1,1,1,1,1,1,1,1,1,1,1,1,1,1,1,1,1,1,1,1,1,
1,1,1,1,1,1,1,1,1,1,1,1,1,1,1,1,1,1,1,1,1,1,1,1,1,1,1,1,1,1,1,1,1,1,1,1,
1,1,1,1,1,1,1,1,1,1,1,1,1,1,1,1,1,1,1,1,1,1,1,1,1,1,1,1,1,1,1,1,1,1,1,1,
1,1,1,1,1,1,1,1,1,1,1,1,1,1,1,1,1,1,1,1,1,1,1,1,1,1,1,1,1,1,1,1,1,1,1,1,
1,1,1,1,1,1,1,1,1,1,1,1,1,1,1,1,1,1,1,1,1,1,1,1,1,1,1,1,1,1,1,1,1,1,1,1,
1,1,1,1,1,1,1,1,1,1,1,1,1,1,1,1,1,1,1,1,1,1,1,1,1,1,1,1,1,1,1,1,1,1,1,1,
1,1,1,1,1,1,1,1,1,1,1,1,1,1,1,1,1,1,1,1,1,1,1,1,1,1,1,1,1,1,1,1,1,1,1,1,
1,1,1,1,1,1,1,1,1,1,1,1,1,1,1,1,1,1,1,1,1,1,1,1,1,1,1,1,1,1,1,1,1,1,1,1,
1,1,1,1,1,1,1,1,1,1,1,1,1,1,1,1,1,1,1,1,1,1,1,1,1,1,1,1,1,1,1,1,1,1,1,1,
1,1,1,1,1,1,1,1,1,1,1,1,1,1,1,1,1,1,1,1,1,1,1,1,1,1,1,1,1,1,1,1,1,1,1,1,
1,1,1,1,1,1,1,1,1,1,1,1,1,1,1,1,1,1,1,1,1,1,1,1,1,1,1,1,1,1,1,1,1,1,1,1,
1,1,1,1,1,1,1,1,1,1,1,1,1,1,1,1,1,1,1,1,1,1,1,1,1,1,1,1,1,1,1,1,1,1,1,1,
1,1,1,1,1,1,1,1,1,1,1,1,1,1,1,1,1,1,1,1,1,1,1,1,1,1,1,1,1,1,1,1,1,1,1,1,
1,1,1,1,1,1,1,1,1,1,1,1,1,1,1,1,1,1,1,1,1,1,1,1,1,1,1,1,1,1,1,1,1,1,1,1,
1,1,1,1,1,1,1,1,1,1,1,1,1,1,1,1,1,1,1,1,1,1,1,1,1,1,1,1,1,1,1,1,1,1,1,1,
1,1,1,1,1,1,1,1,1,1,1,1,1,1,1,1,1,1,1,1,1,1,1,1,1,1,1,1,1,1,1,1,1,1,1,1,
1,1,1,1,1,1,1,1,1,1,1,1,1,1,1,1,1,1,1,1,1,1,1,1,1,1,1,1,1,1,1,1,1,1,1,1,
1,1,1,1,1,1,1,1,1,1,1,1,1,1,1,1,1,1,1,1,1,1,1,1,1,1,1,1,1,1,1,1,1,1,1,1,
1,1,1,1,1,1,1,1,1,1,1,1,1,1,1,1,1,1,1,1,1,1,1,1,1,1,1,1,1,1,1,1,1,1,1,1,
1,1,1,1,1,1,1,1,1,1,1,1,1,1,1,1,1,1,1,1,1,1,1,1,1,1,1,1,1,1,1,1,1,1,1,1,
1,1,1,1,1,1,1,1,1,1,1,1,1,1,1,1,1,1,1,1,1,1,1,1,1,1,1,1,1,1,1,1,1,1,1,1,
1,1,1,1,1,1,1,1,1,1,1,1,1,1,1,1,1,1,1,1,1,1,1,1,1,1,1,1,1,1,1,1,1,1,1,1,
1,1,1,1,1,1,1,1,1,1,1,1,1,1,1,1,1,1,1,1,1,1,1,1,1,1,1,1,1,1,1,1,1,1,1,1,
1,1,1,1,1,1,1,1,1,1,1,1,1,1,1,1,1,1,1,1,1,1,1,1,1,1,1,1,1,1,1,1,1,1,1,1,
1,1,1,1,1,1,1,1,1,1,1,1,1,1,1,1,1,1,1,1,1,1,1,1,1,1,1,1,1,1,1,1,1,1,1,1,
1,1,1,1,1,1,1,1,1,1,1,1,1,1,1,1,1,1,1,1,1,1,1,1,1,1,1,1,1,1,1,1,1,1,1,1,
1,1,1,1,4),(2,2),(0.,0.869746702321014,1.7394931589914,2.60923976624962,
3.47983908319159,4.35043840179749,5.22018503077054,6.08993165951504,6.95967828799171,
7.82942491616733,8.69917154401062,9.56891817149224,10.4395174886835,11.3101168056706,
12.179863432132,13.049610058144,13.9193566836854,14.7891033087372,15.6588499332817,
16.5285965573034,17.3991958717975,18.2697951860185,18.7046684974166,19.1395418086746,
19.5744151197912,20.0092884307654,20.4441617415962,20.8790350522825,21.7487816732187,
22.1836549834672,22.6185282935685,23.0534016035221,23.4882749133276,23.9231482229848,
24.3588742245859,24.794600226187,25.2294735355468,26.0992201538203,26.5340934627341,
26.9689667714994,27.4038400801166,27.838713388586,28.2735866969081,28.7084600050832,
29.143333313112,29.5782066209952,30.0130799287334,30.4479532363275,30.8828265437783,
31.3185525442794,31.7542785447804,32.1891518519474,32.6240251589741,33.0588984658616,
33.4937717726112,33.928645079224,34.3635183857014,34.7983916920448,35.2332649982556,
35.6681383043353,36.1030116102854,36.5378849161076,36.9727582218035,37.4076315273749,
37.8425048328235,38.2782308323341,38.7139568318446,39.1488301370532,39.5837034421446,
40.0185767471208,40.4534500519838,40.8883233567357,41.3231966613787,41.7580699659148,
42.1929432703463,42.6278165746754,43.0626898789044,43.4975631830356,43.9324364870714,
44.3673097910142,44.8021830948664,45.2379090935952,45.673635092324,46.1085083960024,
46.5433816995978,46.9782550031127,47.4131283065497,47.8480016099115,48.2828749132006,
48.7177482164198,49.1526215195718,49.5874948226593,50.0223681256851,50.457241428652,
50.8921147315628,51.3269880344203,51.7618613372274,52.197587335454,52.6333133336805,
53.0681866363954,53.5030599390685,53.9379332417027,54.3728065443011,54.8076798468664,
55.2425531494018,55.6774264519101,56.1122997543943,56.5471730568575,56.9820463593026,
57.4169196617326,57.8517929641506,58.2866662665595,58.7215395689624,59.157265567009,
59.5929915650557,60.0278648674556,60.4627381698584,60.8976114722673,61.3324847746853,
61.7673580771153,62.2022313795604,62.6371046820236,63.0719779845079,63.5068512870162,
63.9417245895516,64.376597892117,64.8114711947155,65.2463444973499,65.6812178000231,
66.1169437982275,66.5526697964318,66.9875430991915,67.4224164019987,67.8572897048563,
68.2921630077673,68.7270363107343,69.1619096137603,69.5967829168479,70.0316562200001,
70.4665295232194,70.9014028265087,71.3362761298705,71.7711494333077,72.2060227368227,
72.6408960404182,73.0766220391044,73.5123480377905,73.9472213415547,74.382094645407,
74.8169679493499,75.2518412533859,75.6867145575172,76.1215878617464,76.5564611660756,
76.9913344705072,77.4262077750435,77.8610810796866,78.2959543844386,78.7308276893018,
79.1657009942781,79.6005742993696,80.0363002988208,80.4720262982719,80.9068996035997,
81.3417729090484,81.7766462146199,82.211519520316,82.6463928261383,83.0812661320886,
83.5161394381684,83.9510127443794,84.3858860507229,84.8207593572004,85.2556326638134,
85.6905059705631,86.1253792774507,86.5602525844776,86.995978584908,87.4317045853384,
87.8665778926469,88.3014512000977,88.7363245076919,89.1711978154302,89.6060711233134,
90.0409444313423,90.4758177395175,90.9106910478396,91.345564356309,91.7804376649263,
92.2153109736917,92.6501842826055,93.085057591668,93.5199309008791,93.9556569024059,
94.3913829039327,94.8262562134414,95.2611295230986,95.6960028329042,96.1308761428578,
96.5657494529591,97.0006227632077,97.4354960736028,97.870369384144,98.3052426948304,
98.7401160056612,99.1749893166354,99.6098626277522,100.04473593901,100.915335253024,
101.351061255639,101.785934567313,102.220807879124,102.655681191068,103.090554503145,
103.525427815353,104.395174440154,105.264921065453,105.699794378283,106.134667691232,
106.569541004295,107.004414317471,107.8750136343,108.745612951339,109.615359578629,
110.485106206296,111.354852834309,112.224599462639,113.094346091254,113.964092720119,
114.834692038763,115.705291357499,116.575037986826,117.444784616267,118.314531245777,
119.184277875311,120.054024504821,120.923771134261,121.794370453112,122.66496977189,
123.534716400968,124.404463029834,125.274209658448,126.143956286779,127.013702914792,
127.883449542458,128.754048859798,129.624648176939,130.494394803617,131.364141429857,
132.233888055637,133.103634680937,133.973381305737,134.843127930023,135.71372724472,
136.584326559147,137.019199870684,137.454073182083,137.888946493341,138.323819804458,
139.193566426263,140.063313047491,140.498186357887,140.933059668136,141.367932978237,
141.802806288191,142.237679597997,142.673405599673,143.109131601348,143.544004910857,
143.978878220217,144.413751529429,144.848624838491,145.283498147405,145.718371456171,
146.153244764789,146.588118073258,147.022991381581,147.457864689756,147.892737997785,
148.327611305669,148.762484613407,149.197357921002,149.633083921574,150.068809922147,
150.503683229455,150.938556536623,151.37342984365,151.808303150538,152.243176457288,
152.678049763901,153.112923070379,153.547796376722,153.982669682934,154.417542989014,
154.852416294964,155.287289600787,155.722162906483,156.157036212055,156.592762211626,
157.028488211198,157.463361516526,157.898234821735,158.333108126826,158.767981431803,
159.202854736666,159.637728041419,160.072601346062,160.507474650599,160.94234795503,
161.37722125936,161.812094563589,162.246967867721,162.681841171757,163.1167144757,
163.552440474473,163.988166473247,164.423039777011,164.85791308069,165.292786384286,
165.727659687801,166.162532991238,166.597406294601,167.03227959789,167.46715290111,
167.902026204262,168.33689950735,168.771772810376,169.206646113343,169.641519416254,
170.076392719112,170.512118717363,170.947844715614,171.382718018374,171.817591321089,
172.252464623762,172.687337926397,173.122211228996,173.557084531561,173.991957834097,
174.426831136606,174.86170443909,175.296577741554,175.731451044,176.16632434643,
176.601197648848,177.036070951258,177.471796949306,177.907522947355,178.342396249755,
178.777269552155,179.212142854558,179.647016156968,180.081889459386,180.516762761816,
180.951636064262,181.386509366726,181.82138266921,182.256255971719,182.691129274255,
183.12600257682,183.560875879419,183.995749182054,184.431475180237,184.867201178421,
185.302074481136,185.736947783896,186.171821086704,186.606694389561,187.041567692473,
187.47644099544,187.911314298466,188.346187601554,188.781060904706,189.215934207926,
189.650807511215,190.085680814577,190.520554118015,190.95542742153,191.391153420175,
191.82687941882,192.261752722499,192.696626026263,193.131499330116,193.566372634059,
194.001245938095,194.436119242227,194.870992546456,195.305865850785,195.740739155217,
196.175612459754,196.610485764397,197.045359069149,197.480232374013,197.915105678989,
198.350831678382,198.786557677775,199.221430982984,199.656304288312,200.091177593761,
200.526050899333,200.960924205029,201.395797510852,201.830670816802,202.265544122882,
202.700417429093,203.135290735437,203.570164041915,204.005037348528,204.439910655278,
204.874783962166,205.310509962526,205.746235962887,206.181109270054,206.615982577363,
207.050855884814,207.485729192409,207.920602500147,208.355475808031,208.79034911606,
209.225222424235,209.660095732558,210.094969041027,210.529842349645,210.96471565841,
211.399588967324,211.834462276387,212.27018827784,212.705914279292,213.140787588653,
213.575660898161,214.010534207819,214.880280827579,215.31515413768,215.750027447929,
216.184900758324,216.619774068866,217.054647379553,217.489520690384,218.359267312475,
219.22986662628,219.665592628826,220.100465940363,220.535339252038,220.970212563848,
221.83995918787,222.709705812416,223.579452437468,224.014325750179,224.44919906301,
225.318945689022,226.189545005688,227.060144322571,227.929890949664,228.799637577146,
229.66938420499,230.539130833166,231.408877461643,232.278624090388,233.149223408954,
234.019822727623,234.889569356878,235.759315986267,236.629062615749,237.498809245277,
238.368555874806,239.238302504287,240.108901823183,240.979501142017,241.849247771189,
242.718994400167,243.588741028911,244.458487657389,245.328234285565,246.197980913409,
247.068580230891,247.939179548182,248.80892617507,249.678672801532,250.548419427545,
251.418166053087,252.287912678139,253.157659302684,254.028258617581,254.898857932211,
255.333731243885,255.768604555423,256.203477866821,256.63835117808,257.508097800171,
258.377844421689,258.812717732231,259.247591042627,259.682464352876,260.117337662977,
260.552210972931,260.987936974682,261.858536286089,262.293409595598,262.728282904958,
263.16315621417,263.598029523233,264.032902832147,264.467776140913,264.902649449531,
265.337522758001,265.772396066323,266.207269374499,266.642142682528,267.077015990412,
267.511889298151,267.947615298795,268.383341299439,268.81821460689,269.2530879142,
269.687961221367,270.122834528394,270.557707835282,270.992581142032,271.427454448646,
271.862327755124,272.297201061468,272.732074367679,273.166947673759,273.60182097971,
274.036694285533,274.471567591229,274.907293590862,275.343019590495,275.777892895944,
276.212766201272,276.647639506481,277.082512811573,277.51738611655,277.952259421414,
278.387132726166,278.82200603081,279.256879335346,279.691752639779,280.126625944108,
280.561499248338,280.996372552469,281.431245856506,281.866971855324,282.302697854143,
282.737571157996,283.172444461761,283.60731776544,284.042191069036,284.477064372551,
284.911937675989,285.346810979351,285.781684282641,286.216557585861,286.651430889013,
287.086304192101,287.521177495128,287.956050798095,288.390924101007,288.826650099283,
289.262376097559,289.697249400366,290.132122703127,290.566996005842,291.001869308516,
291.43674261115,291.871615913749,292.306489216315,292.741362518851,293.17623582136,
293.611109123845,294.045982426308,294.480855728754,294.915729031185,295.350602333603,
295.786328331655,296.222054329707,296.65692763211,297.091800934511,297.526674236911,
297.961547539314,298.396420841724,298.831294144142,299.266167446573,299.701040749018,
300.135914051482,300.570787353967,301.005660656476,301.440533959012,301.875407261578,
302.310280564177,302.746006562341,303.181732560506,303.616605863179,304.051479165895,
304.486352468655,304.921225771462,305.35609907432,305.790972377232,306.225845680199,
306.660718983226,307.095592286314,307.530465589466,307.965338892686,308.400212195976,
308.835085499338,309.269958802776,309.705684801381,310.141410799985,310.576284103581,
311.01115740726,311.446030711025,311.880904014878,312.315777318821,312.750650622858,
313.185523926989,313.620397231219,314.055270535549,314.490143839981,314.925017144517,
315.359890449161,315.794763753913,316.229637058777,316.665363058112,317.101089057448,
317.53596236254,317.970835667749,318.405708973077,318.840582278526,319.275455584098,
319.710328889795,320.145202195618,320.580075501568,321.014948807648,321.44982211386,
321.884695420204,322.319568726682,322.754442033295,323.189315340045,323.625041340336,
324.060767340628,324.495640647655,324.930513954822,325.365387262131,325.800260569583,
326.235133877177,326.670007184916,327.1048804928,327.539753800829,327.974627109005,
328.409500417327,328.844373725797,329.279247034415,329.714120343181,330.148993652095,
330.584719653474,331.020445654852,331.455318964064,331.890192273424,332.325065582933,
332.759938892591,333.194812202397,333.629685512351,334.064558822453,334.499432132702,
334.934305443098,335.369178753639,335.804052064326,336.673798686132,337.108671997249,
337.544397999725,337.980124002201,338.4149973136,338.849870625137,339.284743936812,
340.154490560568,341.024237184854,341.459110497191,341.893983809655,342.328857122244,
342.763730434955,343.633477060735,344.504076377234,345.374675693955,346.244422320844,
347.114168948136,347.983915575803,348.853662203817,349.723408832148,350.593155460764,
351.463754779246,352.334354097839,353.204100727012,354.07384735634,354.943593985781,
355.813340615292,356.683087244827,357.552833874338,358.423433193272,359.294032512154,
360.163779141409,361.033525770489,361.903272399355,362.77301902797,363.642765656301,
364.512512284316,365.383111601936,366.253710919371,367.123457546465,367.993204173143,
368.862950799383,369.732697425164,370.602444050463,371.472190675265,372.342789990359,
373.21338930519,373.648262617,374.083135928675,374.952882551611,375.822629173987,
376.257502484962,376.692375795793,377.12724910648,377.562122417021,377.996995727417,
378.431869037666,378.866742347767,379.302468349591,379.738194351416,380.173067661222,
380.607940970879,381.042814280388,381.477687589749,381.91256089896,382.347434208023,
382.782307516937,383.217180825703,383.652054134321,384.086927442791,384.521800751113,
384.956674059289,385.391547367318,385.826420675202,386.262146675918,386.697872676635,
387.13274598423,387.567619291681,388.00249259899,388.437365906157,388.872239213185,
389.307112520073,389.741985826823,390.176859133436,390.611732439914,391.046605746258,
391.48147905247,391.91635235855,392.351225664501,392.786098970323,393.221824970019,
393.657550969714,394.092424275286,394.527297580735,394.962170886063,395.397044191272,
395.831917496364,396.266790801341,396.701664106204,397.136537410957,397.5714107156,
398.006284020137,398.441157324569,398.876030628899,399.310903933128,399.74577723726,
400.181503236126,400.617229234991,401.052102538934,401.486975842787,401.921849146551,
402.356722450231,402.791595753827,403.226469057342,403.66134236078,404.096215664142,
404.531088967432,404.965962270651,405.400835573804,405.835708876892,406.270582179918,
406.705455482886,407.141181481189,407.576907479491,408.01178078235,408.446654085157,
408.881527387917,409.316400690633,409.751273993306,410.186147295941,410.62102059854,
411.055893901106,411.490767203642,411.925640506151,412.360513808636,412.795387111099,
413.230260413545,413.665133715976,414.100859714032,414.536585712088,414.971459014498,
415.406332316901,415.841205619301,416.276078921702,416.710952224105,417.145825526515,
417.580698828933,418.015572131364,418.45044543381,418.885318736273,419.320192038758,
419.755065341267,420.189938643803,420.624811946369,421.060537944515,421.496263942662,
421.931137245297,422.36601054797,422.800883850686,423.235757153446,423.670630456253,
424.105503759112,424.540377062023,424.975250364991,425.410123668017,425.844996971105,
426.279870274258,426.714743577477,427.149616880767,427.584490184129,428.020216182695,
428.455942181261,428.890815484776,429.325688788373,429.760562092052,430.195435395816,
430.630308699669,431.065182003612,431.500055307649,431.93492861178,432.36980191601,
432.80467522034,433.239548524772,433.674421829309,434.109295133952,434.544168438705,
434.979894437984,435.415620437262,435.850493742239,436.285367047331,436.72024035254,
437.155113657869,437.589986963318,438.024860268889,438.459733574586,438.894606880409,
439.32948018636,439.76435349244,440.199226798651,440.634100104995,441.068973411473,
441.503846718087,441.939572718309,442.375298718531,442.810172025419,443.245045332447,
443.679918639614,444.114791946923,444.549665254374,444.984538561969,445.419411869708,
445.854285177591,446.289158485621,446.724031793796,447.158905102119,447.593778410589,
448.028651719207,448.463525027973,448.899251029277,449.334977030581,449.769850339644,
450.639596958216,451.074470267725,451.509343577383,451.944216887189,452.379090197143,
452.813963507244,453.248836817493,453.683710127889,454.118583438431,454.553456749117,
454.988330059949,455.423203370923,455.858929373329,456.294655375734,456.729528686993,
457.164401998391,457.599275309929,458.469021933414,458.90389524536,459.338768557437,
459.773641869646,460.208515181983,460.643388494447,461.078261807036,461.948008432578,
462.818607748906,463.689207065461,464.55895369214,465.428700319234,466.298446946716,
467.16819357456,468.037940202737,468.907686831215,469.778286149605,470.648885468116,
471.518632097196,472.388378726451,473.258125355841,474.127871985322,474.997618614851,
475.86736524438,476.737964563343,477.608563882265,478.478310511593,479.348057140765,
480.217803769743,481.087550398488,481.957297026966,482.827043655142,483.697642972895,
484.568242290469,485.43798891776,486.307735544649,487.177482171112,488.047228797125,
488.916975422667,489.78672204772,490.657321363009,491.09304736596,491.527920678038,
492.397667301793,493.267413925005,494.137160547663,494.57203385878,495.006907169755,
495.441780480586,495.876653791273,496.311527101814,496.74640041221,497.616999724357,
498.052725726255,498.487599036209,498.922472346015,499.357345655673,499.792218965182,
500.227092274542,500.661965583754,501.096838892816,501.531712201731,501.966585510497,
502.401458819114,502.836332127584,503.271205435907,503.706078744082,504.140952052112,
504.576678052901,505.01240405369,505.447277361429,505.882150669023,506.317023976474,
506.751897283783,507.186770590951,507.621643897978,508.056517204866,508.491390511616,
508.92626381823,509.361137124708,509.796010431052,510.230883737263,510.665757043344,
511.100630349294,511.536356349053,511.972082348811,512.406955654506,512.841828960076,
513.276702265523,513.711575570849,514.146448876056,514.581322181146,515.016195486121,
515.451068790983,515.885942095733,516.320815400375,516.75568870491,517.19056200934,
517.625435313668,518.060308617896,518.496034616807,518.931760615718,519.366633919752,
519.801507223694,520.236380527545,520.671253831307,521.106127134985,521.541000438579,
521.975873742092,522.410747045528,522.845620348888,523.280493652176,523.715366955394,
524.150240258545,524.585113561631,525.019986864656,525.455712862985,525.891438861313,
526.326312164223,526.761185467079,527.196058769885,527.630932072643,528.065805375356,
528.500678678029,528.935551980661,529.370425283258,529.805298585822,530.240171888356,
530.675045190863,531.109918493346,531.544791795808,531.979665098252,532.415391096312,
532.851117094373,533.285990396789,533.720863699197,534.155737001598,534.590610303997,
535.025483606395,535.460356908796,535.895230211204,536.330103513621,536.764976816049,
537.199850118493,537.634723420955,538.069596723438,538.504470025945,538.93934332848,
539.375069326608,539.810795324736,540.245668627333,540.680541929966,541.115415232637,
541.550288535351,541.985161838109,542.420035140915,542.854908443771,543.28978174668,
543.724655049646,544.15952835267,544.594401655757,545.029274958907,545.464148262125,
545.899021565413,546.334747563939,546.770473562465,547.205346865901,547.640220169415,
548.075093473009,548.509966776686,548.944840080449,549.3797133843,549.814586688241,
550.249459992276,550.684333296405,551.119206600633,551.554079904961,551.988953209391,
552.423826513926,552.858699818567,553.294425817789,553.73015181701,554.165025121872,
554.599898426846,555.034771731937,555.469645037144,555.90451834247,556.339391647917,
556.774264953487,557.209138259182,557.644011565003,558.078884870951,558.51375817703,
558.948631483239,559.383504789581,559.818378096058,560.254104096209,560.689830096361,
561.12470340311,561.559576709996,561.994450017021,562.429323324187,562.864196631494,
563.299069938943,563.733943246536,564.168816554273,564.603689862154,565.038563170182,
565.473436478355,565.908309786676,566.343183095144,566.77805640376,567.213782404988,
567.649508406216,568.084381715128,568.519255024189,568.954128333399,569.389001642757,
569.823874952264,570.258748261921,570.693621571725,571.128494881677,571.563368191777,
572.433114812417,572.867988122957,573.302861433642,573.737734744471,574.173460746804,
574.609186749136,575.044060060251,575.913806682904,576.783553306113,577.218426617922,
577.653299929865,578.08817324194,578.523046554147,579.392793178944,580.26253980424,
581.13313912039,581.568865123709,582.003738436771,582.87348506323,583.743231690115,
584.612978317402,585.482724945065,586.352471573076,587.222218201403,588.092817519691,
588.963416838109,589.833163467083,590.702910096251,591.572656725575,592.442403355013,
593.31214998452,594.181896614051,595.05249593303,595.92309525198,596.792841881366,
597.662588510618,598.532335139693,599.402081768556,600.271828397167,601.141575025495,
602.012174343369,602.882773661074,603.752520288553,604.622266915642,605.492013542317,
606.361760168553,607.23150679433,608.101253419626,608.971852735101,609.842452050322,
610.71219867434,611.581945297822,612.451691920754,612.886565232011,613.321438543126,
613.756311854099,614.191185164928,615.060931786153,615.931531098516,616.367257100486,
616.802130410586,617.237003720538,617.671877030342,618.106750339998,618.541623649505,
618.976496958863,619.411370268073,619.846243577134,620.281116886046,620.71599019481,
621.150863503426,621.585736811894,622.020610120214,622.455483428388,622.891209429248,
623.326935430108,623.761808737989,624.196682045726,624.631555353319,625.066428660769,
625.501301968075,625.936175275241,626.371048582266,626.805921889153,627.240795195901,
627.675668502512,628.110541808988,628.54541511533,628.98028842154,629.415161727618,
629.850887727438,630.286613727259,630.72148703308,631.156360338774,631.591233644344,
632.026106949791,632.460980255118,632.895853560325,633.330726865415,633.76560017039,
634.200473475251,634.635346780002,635.070220084644,635.505093389179,635.939966693609,
636.374839997937,636.810565996897,637.246291995857,637.681165299986,638.116038604021,
638.550911907962,638.985785211813,639.420658515576,639.855531819253,640.290405122847,
640.725278426361,641.160151729796,641.595025033157,642.029898336444,642.464771639662,
642.899644942813,643.334518245899,643.770244244257,644.205970242616,644.640843545581,
645.075716848491,645.510590151347,645.945463454153,646.380336756911,646.815210059625,
647.250083362296,647.684956664929,648.119829967526,648.55470327009,648.989576572624,
649.424449875131,649.859323177614,650.294196480076,650.729922478144,651.165648476212,
651.600521778641,652.035395081057,652.470268383465,652.905141685866,653.340014988265,
653.774888290663,654.209761593065,654.644634895472,655.079508197889,655.514381500318,
655.949254802762,656.384128105224,656.819001407706,657.253874710213,657.689600708326,
658.12532670644,658.560200009004,658.995073311601,659.429946614234,659.864819916905,
660.299693219619,660.734566522377,661.169439825183,661.604313128039,662.039186430948,
662.474059733914,662.908933036938,663.343806340025,663.778679643175,664.213552946393,
664.649278944883,665.085004943373,665.519878246733,665.954751550169,666.389624853683,
666.824498157277,667.259371460954,667.694244764717,668.129118068568,668.563991372509,
668.998864676544,669.433737980674,669.868611284901,670.303484589229,670.738357893659,
671.173231198194,671.608957197361,672.044683196528,672.479556501278,672.91442980614,
673.349303111115,673.784176416205,674.219049721412,674.653923026738,675.088796332185,
675.523669637755,675.95854294345,676.393416249271,676.82828955522,677.263162861298,
677.698036167508,678.13290947385,678.568635473934,679.004361474018,679.439234780629,
679.874108087377,680.308981394264,680.743854701289,681.178728008455,681.613601315762,
682.048474623211,682.483347930804,682.91822123854,683.353094546422,683.78796785445,
684.222841162623,684.657714470944,685.092587779412,685.528313780566,685.96403978172,
686.398913090483,686.833786399396,687.268659708457,687.703533017666,688.138406327025,
688.573279636532,689.008152946187,689.443026255992,689.877899565944,690.312772876043,
690.74764618629,691.182519496684,691.617392807224,692.052266117909,692.487992120169,
692.92371812243,693.358591433403,694.228338055774,694.663211367171,695.098084678707,
695.532957990379,695.967831302188,696.402704614131,696.837577926207,697.707324550749,
698.577071175797,699.011944488507,699.447670491767,699.883396495028,700.318269807975,
701.188016434211,702.057763060886,702.927509687976,703.797256315454,704.667002943295,
705.536749571467,706.407348889651,707.277948207973,708.147694836835,709.017441465911,
709.887188095163,710.756934724548,711.626681354026,712.496427983551,713.367027302543,
714.237626621516,715.107373250954,715.977119880277,716.846866509446,717.716613138419,
718.586359767161,719.456106395635,720.32670571363,721.197305031464,722.067051659126,
722.936798286414,723.806544913299,724.676291539758,725.546038165767,726.415784791305,
727.286384106969,728.156983422381,729.026730046663,729.896476670415,730.331349982088,
730.766223293624,731.201096605021,731.635969916278,732.505716538366,733.37546315988,
733.81033647042,734.246062472462,734.681788474505,735.116661784752,735.551535094852,
735.986408404804,736.421281714608,736.856155024264,737.291028333771,737.72590164313,
738.160774952339,738.5956482614,739.030521570312,739.465394879076,739.900268187692,
740.33514149616,740.77001480448,741.205740805414,741.641466806347,742.076340114374,
742.511213422256,742.946086729993,743.380960037585,743.815833345035,744.250706652341,
744.685579959507,745.120453266533,745.555326573419,745.990199880167,746.425073186778,
746.859946493254,747.294819799596,747.729693105806,748.165419105691,748.601145105576,
749.036018411525,749.470891717346,749.90576502304,750.34063832861,750.775511634057,
751.210384939384,751.645258244591,752.080131549682,752.515004854656,752.949878159518,
753.384751464269,753.81962476891,754.254498073445,754.689371377875,755.125097376885,
755.560823375895,755.995696680123,756.430569984253,756.865443288287,757.300316592228,
757.735189896079,758.170063199842,758.604936503519,759.039809807113,759.474683110627,
759.909556414062,760.344429717423,760.779303020711,761.214176323929,761.649049627079,
762.084775625469,762.520501623858,762.955374926883,763.390248229848,763.825121532758,
764.259994835614,764.694868138419,765.129741441178,765.564614743891,765.999488046563,
766.434361349196,766.869234651793,767.304107954357,767.738981256891,768.173854559398,
768.608727861881,769.044453859958,769.480179858035,769.915053160479,770.349926462907,
770.784799765324,771.219673067731,771.654546370133,772.089419672531,772.52429297493,
772.959166277331,773.394039579739,773.828912882155,774.263786184584,774.698659487028,
775.13353278949,775.568406091973,776.004132090072,776.439858088172,776.874731390706,
777.30960469327,777.744477995867,778.1793512985,778.614224601171,779.049097903885,
779.483971206643,779.918844509449,780.353717812305,780.788591115215,781.22346441818,
781.658337721205,782.093211024291,782.528084327442,782.963810325897,783.399536324352,
783.834409627639,784.269282931,784.704156234435,785.139029537949,785.573902841543,
786.00877614522,786.443649448983,786.878522752834,787.313396056775,787.74826936081,
788.183142664939,788.618015969167,789.052889273495,789.487762577925,789.923488577038,
790.359214576152,790.794087880793,791.228961185544,791.663834490406,792.098707795381,
792.533581100471,792.968454405678,793.403327711004,793.838201016451,794.273074322021,
794.707947627716,795.142820933537,795.577694239486,796.012567545564,796.447440851774,
796.883166851791,797.318892851808,797.753766158284,798.188639464895,798.623512771643,
799.058386078529,799.493259385555,799.92813269272,800.363006000027,800.797879307477,
801.232752615069,801.667625922806,802.102499230688,802.537372538715,802.972245846889,
803.40711915521,803.84284515629,804.27857115737,804.713444465985,805.148317774749,
805.583191083662,806.018064392723,806.452937701933,806.887811011291,807.322684320798,
808.192430940258,808.62730425021,809.06217756031,809.497050870557,809.931924180951,
810.36679749149,810.802523493679,811.238249495867,811.673122806697,812.542869428785,
812.977742740041,813.412616051438,813.847489362974,814.282362674646,814.717235986455,
815.152109298398,816.021855922681,816.891602547478,817.326475860065,817.762201863265,
818.197927866466,818.632801179295,819.502547805304,820.372294431763,821.242041058648,
822.111787685935,822.981534313598,823.851280941609,824.721880259681,825.5924795779,
826.462226206642,827.331972835616,828.201719464785,829.071466094109,829.941212723546,
830.810959353053,831.681558672047,832.552157991036,833.421904620514,834.2916512499,
835.161397879151,836.031144508226,836.900891137089,837.770637765701,838.641237083811,
839.511836401767,840.381583029608,841.251329657086,842.121076284176,842.990822910851,
843.860569537087,844.730316162863,845.600915478712,846.471514794314,847.341261418855,
848.211008042874,848.645881354683,849.080754666356,849.515627977891,849.950501289288,
850.82024791166,851.689994533462,852.124867844147,852.560593846263,852.996319848379,
853.431193158772,853.866066469019,854.300939779119,855.170686398875,855.605559708531,
856.040433018038,856.475306327397,856.910179636606,857.345052945667,857.77992625458,
858.214799563344,858.64967287196,859.084546180427,859.520272181434,859.95599818244,
860.390871490614,860.825744798641,861.260618106523,861.69549141426,862.130364721852,
862.565238029302,863.000111336609,863.434984643774,863.8698579508,864.304731257686,
864.739604564434,865.174477871045,865.609351177521,866.044224483863,866.479950483814,
866.915676483765,867.350549789843,867.785423095792,868.220296401613,868.655169707307,
869.090043012877,869.524916318325,869.959789623651,870.394662928858,870.829536233948,
871.264409538923,871.699282843785,872.134156148535,872.569029453177,873.003902757712,
873.439628756773,873.875354755834,874.310228060162,874.745101364389,875.179974668519,
875.614847972553,876.049721276495,876.484594580346,876.919467884108,877.354341187786,
877.78921449138,878.224087794893,878.658961098329,879.093834401689,879.528707704977,
879.963581008195,880.399307006616,880.835033005038,881.269906308124,881.704779611148,
882.139652914114,882.574526217024,883.00939951988,883.444272822685,883.879146125444,
884.314019428157,884.748892730829,885.183766033462,885.618639336059,886.053512638623,
886.488385941157,886.923259243664,887.358985241751,887.794711239839,888.2295845423,
888.664457844744,889.099331147173,889.534204449589,889.969077751997,890.403951054398,
890.838824356797,891.273697659195,891.708570961597,892.143444264004,892.578317566421,
893.01319086885,893.448064171293,893.882937473755,894.318663471843,894.75438946993,
895.189262772437,895.624136074971,896.059009377535,896.493882680132,896.928755982765,
897.363629285437,897.798502588151,898.233375890909,898.668249193715,899.103122496571,
899.53799579948,899.972869102446,900.40774240547,900.842615708556,901.278341706978,
901.714067705399,902.148941008617,902.583814311905,903.018687615265,903.453560918701,
903.888434222214,904.323307525808,904.758180829485,905.193054133248,905.627927437099,
906.06280074104,906.497674045075,906.932547349205,907.367420653433,907.80229395776,
908.238019956821,908.673745955883,909.108619260417,909.543492565059,909.978365869809,
910.413239174671,910.848112479646,911.282985784736,911.717859089943,912.152732395269,
912.587605700716,913.022479006287,913.457352311981,913.892225617802,914.327098923751,
914.761972229829,915.19769822978,915.633424229731,916.068297536072,916.503170842548,
916.93804414916,917.372917455908,917.807790762794,918.24266406982,918.677537376985,
919.112410684292,919.547283991742,919.982157299334,920.417030607071,920.851903914953,
921.28677722298,921.721650531154,922.15737653216,922.593102533167,923.027975841635,
923.46284915025,923.897722459014,924.332595767926,924.767469076987,925.202342386197,
925.637215695556,926.072089005063,926.506962314719,926.941835624523,927.376708934475,
927.811582244575,928.246455554822,928.681328865215,929.117054867331,929.987654180132,
930.422527490961,930.857400801934,931.292274113049,931.727147424306,932.162020735703,
932.596894047238,933.46664067072,934.336387294739,934.771260606945,935.20613391928,
935.641007231742,936.076733234882,936.94733255073,937.817079176507,938.686825802743,
939.556572429418,940.426319056508,941.296065683986,942.165812311827,943.036411629783,
943.907010947893,944.776757576505,945.646504205367,946.516250834443,947.385997463694,
948.25574409308,949.125490722558,949.996090041546,950.86668936054,951.736435990048,
952.606182619485,953.475929248809,954.345675877978,955.215422506951,956.085169135693,
956.955768453912,957.826367771985,958.696114399995,959.565861027658,960.435607654946,
961.305354281831,962.175100908289,963.044847534298,963.915446850328,964.786046166116,
965.655792790913,966.525539415195,966.960412727138,967.395286038947,968.265032662155,
969.134779284809,969.569652595924,970.004525906897,970.439399217726,970.875125219914,
971.310851222103,971.745724532643,972.615471153283,973.485217773335,973.920091083139,
974.354964392795,974.789837702302,975.22471101166,975.65958432087,976.094457629931,
976.529330938844,976.964204247608,977.399077556223,977.834803557303,978.270529558383,
978.705402866704,979.140276174877,979.575149482905,980.010022790786,980.444896098523,
980.879769406116,981.314642713565,981.749516020872,982.184389328038,982.619262635063,
983.05413594195,983.489009248698,983.923882555309,984.358755861785,984.794481861802,
985.230207861819,985.665081168029,986.099954474107,986.534827780056,986.969701085877,
987.404574391571,987.839447697141,988.274321002589,988.709194307915,989.144067613122,
989.578940918212,990.013814223187,990.448687528048,990.883560832799,991.31843413744,
991.754160136554,992.189886135667,992.624759440097,993.059632744425,993.494506048653,
993.929379352783,994.364252656817,994.799125960758,995.233999264609,995.668872568372,
996.103745872049,996.538619175643,996.973492479157,997.408365782593,997.843239085953,
998.278112389241,998.713838387696,999.149564386151,999.584437689301,1000.01931099239,
1000.45418429541,1000.88905759838,1001.32393090129,1001.75880420414,1002.19367750695,
1002.62855080971,1003.06342411242,1003.49829741509,1003.93317071773,1004.36804402032,
1004.80291732289,1005.23779062542,1005.67351662352,1006.10924262162,1006.5441159241,
1006.97898922656,1007.41386252901,1007.84873583144,1008.28360913385,1008.71848243626,
1009.15335573866,1009.58822904106,1010.02310234346,1010.45797564586,1010.89284894827,
1011.32772225069,1011.76259555311,1012.19746885556,1012.63319485364,1013.06892085171,
1013.5037941542,1013.9386674567,1014.37354075924,1014.8084140618,1015.2432873644,
1015.67816066703,1016.1130339697,1016.54790727242,1016.98278057517,1017.41765387798,
1017.85252718084,1018.28740048375,1018.72227378671,1019.15714708974,1019.59287308813,
1020.02859908651,1020.46347238967,1020.89834569288,1021.33321899617,1021.76809229953,
1022.20296560297,1022.63783890648,1023.07271221007,1023.50758551375,1023.94245881752,
1024.37733212137,1024.81220542531,1025.24707872935,1025.68195203348,1026.11682533771,
1026.55255133672,1026.98827733573,1027.42315064016,1027.8580239447,1028.29289724934,
1028.72777055409,1029.16264385896,1029.59751716393,1030.03239046902,1030.46726377423,
1030.90213707956,1031.33701038501,1031.77188369058,1032.20675699628,1032.6416303021,
1033.07650360805,1033.51222960793,1033.94795560782,1034.38282891403,1034.81770222038,
1035.25257552685,1035.68744883347,1036.12232214022,1036.5571954471,1036.99206875413,
1037.4269420613,1037.86181536861,1038.29668867606,1038.73156198365,1039.16643529139,
1039.60130859927,1040.0361819073,1040.47190790824,1040.90763390917,1041.34250721749,
1041.77738052596,1042.21225383458,1042.64712714334,1043.08200045226,1043.95174707053,
1044.38662037989,1044.8214936894,1045.25636699906,1045.69124030886,1046.12611361882,
1046.56098692892,1046.99586023917,1047.43158624121,1047.86731224325,1048.3021855538,
1048.73705886448,1049.17193217531,1049.60680548629,1050.0416787974,1050.47655210866,
1050.91142542006,1051.78117204327,1052.21604535508,1052.65091866703,1053.0857919791,
1053.52066529131,1053.95553860365,1054.39126460673,1055.26186392239,1056.13161054793,
1057.00135717395,1057.43623048712,1057.87110380041,1058.7408504273,1059.61059705459,
1060.48034368225,1061.35094300009,1062.22154231809,1063.09128894656,1063.96103557531,
1064.83078220429,1065.70052883346,1066.57027546278,1067.44002209222,1068.3106214112,
1069.18122073019,1070.05096735972,1070.9207139892,1071.79046061859,1072.66020724785,
1073.52995387693,1074.39970050579,1075.27029982411,1076.1408991423,1077.01064577048,
1077.88039239832,1078.7501390258,1079.61988565289,1080.48963227957,1081.35937890581,
1082.22997822202,1083.100577538,1083.97032416305,1084.84007078759,1085.70981741161,
1086.5795640351,1087.44931065803,1087.88418396929,1088.31905728041,1088.75393059138,
1089.18965659365,1089.62538259591,1090.06025590659,1090.93000252753,1091.36487583778,
1091.79974914788,1092.23462245783,1092.66949576764,1093.1043690773,1093.5392423868,
1093.97411569616,1094.40898900538,1094.84386231444,1095.27873562335,1095.71360893212,
1096.14933493327,1096.58506093443,1097.0199342429,1097.45480755122,1097.88968085939,
1098.32455416742,1098.75942747531,1099.19430078305,1099.62917409064,1100.06404739809,
1100.4989207054,1100.93379401257,1101.36866731959,1101.80354062648,1102.23841393323,
1102.67328723984,1103.10901323993,1103.54473924001,1103.97961254636,1104.41448585257,
1104.84935915865,1105.2842324646,1105.71910577042,1106.15397907612,1106.58885238169,
1107.02372568714,1107.45859899246,1107.89347229767,1108.32834560276,1108.76321890774,
1109.1980922126,1109.63296551736,1110.06869151652,1110.50441751569,1110.93929082023,
1111.37416412466,1111.80903742899,1112.24391073322,1112.67878403735,1113.11365734139,
1113.54853064533,1113.98340394918,1114.41827725295,1114.85315055662,1115.28802386022,
1115.72289716374,1116.15777046717,1116.59264377053,1117.02836976903,1117.46409576752,
1117.89896907074,1118.33384237389,1118.76871567698,1119.20358898,1119.63846228297,
1120.07333558588,1120.50820888874,1120.94308219154,1121.3779554943,1121.81282879702,
1122.24770209969,1122.68257540233,1123.11744870492,1123.55232200749,1123.98804800561,
1124.42377400372,1124.85864730623,1125.29352060871,1125.72839391118,1126.16326721362,
1126.59814051605,1127.03301381847,1127.46788712088,1127.90276042328,1128.33763372568,
1128.77250702808,1129.20738033048,1129.64225363289,1130.07712693531,1130.51200023774,
1130.94772623581,1131.38345223388,1131.81832553634,1132.25319883883,1132.68807214134,
1133.12294544387,1133.55781874644,1133.99269204904,1134.42756535167,1134.86243865434,
1135.29731195706,1135.73218525982,1136.16705856263,1136.60193186548,1137.03680516839,
1137.47167847136,1137.90740446972,1138.34313046808,1138.77800377117,1139.21287707432,
1139.64775037754,1140.08262368083,1140.51749698419,1140.95237028763,1141.38724359114,
1141.82211689474,1142.25699019842,1142.69186350218,1143.12673680603,1143.56161010998,
1143.99648341401,1144.43135671814,1144.86708271711,1145.30280871607,1145.7376820204,
1146.17255532483,1146.60742862936,1147.04230193401,1147.47717523876,1147.91204854362,
1148.3469218486,1148.78179515369,1149.2166684589,1149.65154176423,1150.08641506968,
1150.52128837525,1150.95616168094,1151.39103498677,1151.82676098659,1152.26248698641,
1152.69736029249,1153.1322335987,1153.56710690504,1154.00198021152,1154.43685351813,
1154.87172682488,1155.30660013177,1155.7414734388,1156.17634674597,1156.61122005327,
1157.04609336073,1157.48096666832,1157.91583997606,1158.35071328394,1158.7864392848,
1159.22216528566,1159.65703859384,1160.09191190216,1160.52678521063,1160.96165851925,
1161.39653182801,1161.83140513693,1162.26627844599,1162.7011517552,1163.13602506456,
1163.57089837407,1164.00577168373,1164.44064499353,1164.87551830349,1165.74611761556,
1166.18184361753,1166.61671692792,1167.05159023846,1167.48646354915,1167.92133685998,
1168.35621017096,1169.22595679333,1170.09570341627,1170.53057672794,1170.96545003975,
1171.4003233517,1171.83519666377,1172.27006997598,1172.705795979,1173.57639529447,
1174.44614191977,1174.8810152326,1175.31588854555,1176.18563517179,1177.05538179847,
1177.92512842556,1178.79487505304,1179.66547437075,1180.53607368863,1181.40582031696,
1182.27556694557,1183.14531357444,1184.01506020352,1184.88480683277,1185.75455346216,
1186.62515278112,1187.4957521001,1188.36549872963,1189.23524535914,1190.10499198858,
1190.97473861791,1191.84448524708,1192.71423187606,1193.58483119448,1194.45543051277,
1195.3251771411,1196.19492376911,1197.06467039678,1197.93441702407,1198.80416365096,
1199.67391027742,1200.5445095938,1201.41510890996,1202.28485553525,1203.15460216005,
1204.02434878434,1204.89409540809,1205.76384203131,1206.1987153427,1206.63358865396,
1207.06846196508,1207.50418796741,1208.37478728058,1209.2445339018,1209.6794072122,
1210.11428052245,1210.54915383255,1210.9840271425,1211.41890045231,1211.85377376197,
1212.28864707147,1212.72352038083,1213.15839369005,1213.59326699911,1214.02814030802,
1214.46386630925,1214.89959231048,1215.3344656191,1215.76933892757,1216.20421223589,
1216.63908554406,1217.07395885209,1217.50883215998,1217.94370546771,1218.37857877531,
1218.81345208276,1219.24832539007,1219.68319869724,1220.11807200426,1220.55294531115,
1220.9878186179,1221.42354461805,1221.85927061821,1222.29414392468,1222.72901723103,
1223.16389053724,1223.59876384332,1224.03363714927,1224.46851045509,1224.90338376079,
1225.33825706636,1225.77313037181,1226.20800367713,1226.64287698234,1227.07775028743,
1227.51262359241,1227.94749689727,1228.3832228965,1228.81894889572,1229.25382220036,
1229.6886955049,1230.12356880933,1230.55844211366,1230.99331541789,1231.42818872202,
1231.86306202606,1232.29793533,1232.73280863385,1233.16768193762,1233.60255524129,
1234.03742854489,1234.4723018484,1234.90717515184,1235.34290115037,1235.7786271489,
1236.21350045219,1236.64837375541,1237.08324705856,1237.51812036165,1237.95299366467,
1238.38786696764,1238.82274027055,1239.25761357341,1239.69248687621,1240.12736017897,
1240.56223348169,1240.99710678436,1241.431980087,1241.8668533896,1242.30257938773,
1242.73830538585,1243.17317868839,1243.6080519909,1244.04292529338,1244.47779859585,
1244.91267189829,1245.34754520072,1245.78241850314,1246.21729180555,1246.65216510795,
1247.08703841035,1247.52191171275,1247.95678501515,1248.39165831756,1248.82653161998,
1249.26225761804,1249.69798361611,1250.13285691855,1250.56773022101,1251.0026035235,
1251.43747682601,1251.87235012854,1252.30722343111,1252.74209673371,1253.17697003634,
1253.61184333901,1254.04671664173,1254.48158994449,1254.9164632473,1255.35133655015,
1255.78620985306,1256.22193585139,1256.65766184973,1257.09253515275,1257.52740845584,
1257.96228175899,1258.39715506221,1258.8320283655,1259.26690166886,1259.7017749723,
1260.13664827581,1260.57152157941,1261.00639488309,1261.44126818685,1261.8761414907,
1262.31101479465,1262.74588809868,1263.1816140976,1263.61734009651,1264.05221340074,
1264.48708670507,1264.9219600095,1265.35683331403,1265.79170661868,1266.22657992343,
1266.66145322829,1267.09632653327,1267.53119983836,1267.96607314357,1268.4009464489,
1268.83581975434,1269.27069305992,1269.70556636561,1270.14129236537,1270.57701836513,
1271.01189167108,1271.44676497716,1271.88163828337,1272.31651158971,1272.75138489619,
1273.1862582028,1273.62113150955,1274.05600481644,1274.49087812347,1274.92575143063,
1275.36062473794,1275.79549804539,1276.23037135299,1276.66524466073,1277.10097066151,
1277.5366966623,1277.97156997033,1278.40644327851,1278.84131658683,1279.2761898953,
1279.71106320392,1280.14593651268,1280.5808098216,1281.01568313066,1281.45055643987,
1281.88542974923,1282.32030305874,1282.75517636839,1283.1900496782,1283.62492298815,
1284.06064899005,1284.49637499195,1284.9312483022,1285.36612161259,1285.80099492313,
1286.23586823382,1286.67074154465,1287.54048816674,1287.975361478,1288.4102347894,
1288.84510810093,1289.27998141261,1289.71485472442,1290.14972803636,1291.02032735139,
1291.89092666668,1292.32579997914,1292.76067329173,1293.19554660444,1293.63041991727,
1294.50016654328,1295.36991316974,1296.23965979663,1297.10940642392,1297.9800057415,
1298.85060505925,1299.72035168742,1300.5900983159,1301.45984494464,1302.32959157362,
1303.19933820279,1304.06908483212,1304.93968415104,1305.81028347,1306.68003009953,
1307.54977672906,1308.41952335854,1309.28926998793,1310.15901661718,1311.02876324626,
1311.89936256477,1312.76996188316,1313.63970851164,1314.50945513981,1315.37920176765,
1316.24894839514,1317.11869502223,1317.98844164891,1318.85904096546,1319.72964028179,
1320.59938690733,1321.46913353238,1322.33888015692,1323.20862678095,1323.64350009276,
1324.07837340443,1324.51324671597,1324.94812002737,1325.81871934103,1326.68931865441,
1327.12419196524,1327.55906527593,1327.99393858647,1328.42881189686,1328.86368520711,
1329.29855851721,1329.73343182716,1330.16830513697,1330.60317844663,1331.03805175614,
1331.4729250655,1331.90779837471,1332.34267168377,1332.77839768507,1333.21412368638,
1333.64899699514,1334.08387030376,1334.51874361223,1334.95361692055,1335.38849022873,
1335.82336353676,1336.25823684464,1336.69311015238,1337.12798345997,1337.56285676742,
1337.99773007473,1338.4326033819,1338.86747668892,1339.30234999581,1339.73807599603,
1340.17380199625,1340.60867530287,1341.04354860934,1341.47842191569,1341.9132952219,
1342.34816852798,1342.78304183393,1343.21791513975,1343.65278844545,1344.08766175102,
1344.52253505647,1344.95740836179,1345.392281667,1345.82715497209,1346.26202827707,
1346.69775427635,1347.13348027563,1347.56835358038,1348.00322688502,1348.43810018956,
1348.87297349399,1349.30784679832,1349.74272010255,1350.17759340668,1350.61246671072,
1351.04734001466,1351.48221331851,1351.91708662228,1352.35195992595,1352.78683322955,
1353.22170653306,1353.65743253163,1354.09315853019,1354.52803183356,1354.96290513685,
1355.39777844007,1355.83265174322,1356.26752504631,1356.70239834933,1357.1372716523,
1357.57214495521,1358.00701825807,1358.44189156087,1358.87676486363,1359.31163816635,
1359.74651146902,1360.18138477166,1360.6171107698,1361.05283676795,1361.48771007051,
1361.92258337305,1362.35745667556,1362.79232997804,1363.2272032805,1363.66207658295,
1364.09694988538,1364.5318231878,1364.96669649021,1365.40156979261,1365.83644309501,
1366.27131639741,1366.70618969981,1367.14106300222,1367.57678900028,1368.01251499834,
1368.44738830077,1368.88226160321,1369.31713490567,1369.75200820816,1370.18688151067,
1370.6217548132,1371.05662811577,1371.49150141837,1371.926374721,1372.36124802367,
1372.79612132639,1373.23099462915,1373.66586793196,1374.10074123481,1374.53646723311,
1374.97219323142,1375.40706653438,1375.84193983741,1376.2768131405,1376.71168644365,
1377.14655974687,1377.58143305016,1378.01630635352,1378.45117965696,1378.88605296047,
1379.32092626407,1379.75579956775,1380.19067287151,1380.62554617536,1381.06041947931,
1381.49614547817,1381.93187147704,1382.36674478117,1382.8016180854,1383.23649138973,
1383.67136469416,1384.10623799869,1384.54111130334,1384.97598460809,1385.41085791295,
1385.84573121793,1386.28060452302,1386.71547782823,1387.15035113356,1387.585224439,
1388.02009774458,1388.45582374427,1388.89154974397,1389.32642304979,1389.76129635574,
1390.19616966182,1390.63104296803,1391.06591627437,1391.50078958085,1391.93566288746,
1392.37053619421,1392.8054095011,1393.24028280813,1393.6751561153,1394.1100294226,
1394.54490273005,1394.97977603765,1395.41550203836,1395.85122803908,1396.28610134696,
1396.72097465499,1397.15584796317,1397.59072127149,1398.02559457996,1398.46046788858,
1398.89534119734,1399.33021450626,1399.76508781532,1400.19996112453,1400.63483443389,
1401.50458105306,1401.93945436286,1402.37518036469,1402.81090636651,1403.24577967661,
1403.68065298686,1404.11552629725,1404.5503996078,1404.98527291848,1405.85501954029,
1406.2898928514,1406.72476616266,1407.15963947406,1407.5945127856,1408.02938609727,
1408.46425940908,1409.33485872391,1410.205458039,1410.64033135134,1411.07520466381,
1411.51007797639,1411.9449512891,1412.81469791488,1413.68444454112,1414.5541911678,
1415.42393779489,1416.29453711233,1417.16513642995,1418.03488305796,1418.90462968629,
1419.77437631491,1420.64412294377,1421.51386957285,1422.38361620211,1423.25421552099,
1424.12481483992,1424.99456146943,1425.86430809896,1426.73405472847,1427.60380135791,
1428.47354798724,1429.34329461641,1430.21389393501,1431.08449325349,1431.9542398821,
1432.82398651043,1433.69373313844,1434.56347976611,1435.4332263934,1436.30297302029,
1437.17357233701,1438.04417165351,1438.91391827929,1439.78366490459,1440.65341152939,
1441.52315815367,1441.95803146562,1442.39290477743,1442.8277780891,1443.26265140064,
1444.13325071451,1445.00385002811,1445.43872333908,1445.87359664991,1446.3084699606,
1446.74334327114,1447.17821658153,1447.61308989178,1448.48283651184,1448.91770982164,
1449.3525831313,1449.78745644081,1450.22232975017,1450.65720305938,1451.09292906076,
1451.52865506214,1451.96352837105,1452.39840167982,1452.83327498843,1453.2681482969,
1453.70302160522,1454.1378949134,1454.57276822143,1455.00764152931,1455.44251483705,
1455.87738814464,1456.31226145209,1456.7471347594,1457.18200806657,1457.6168813736,
1458.05260737389,1458.48833337418,1458.92320668093,1459.35807998754,1459.79295329402,
1460.22782660036,1460.66269990657,1461.09757321265,1461.5324465186,1461.96731982443,
1462.40219313012,1462.83706643569,1463.27193974114,1463.70681304647,1464.14168635168,
1464.57655965677,1465.0122856561,1465.44801165544,1465.8828849603,1466.31775826505,
1466.7526315697,1467.18750487423,1467.62237817866,1468.05725148299,1468.49212478722,
1468.92699809135,1469.36187139539,1469.79674469933,1470.23161800319,1470.66649130695,
1471.10136461063,1471.53623791422,1471.97196391283,1472.40768991143,1472.84256321487,
1473.27743651823,1473.71230982152,1474.14718312474,1474.58205642789,1475.01692973098,
1475.451803034,1475.88667633697,1476.32154963988,1476.75642294274,1477.19129624555,
1477.62616954831,1478.06104285102,1478.4959161537,1478.93164215186,1479.36736815002,
1479.80224145262,1480.23711475519,1480.67198805772,1481.10686136023,1481.54173466272,
1481.97660796518,1482.41148126762,1482.84635457005,1483.28122787247,1483.71610117488,
1484.15097447728,1484.58584777968,1485.02072108208,1485.45559438449,1485.89132038254,
1486.32704638059,1486.76191968301,1487.19679298544,1487.63166628788,1488.06653959035,
1488.50141289283,1488.93628619534,1489.37115949787,1489.80603280044,1490.24090610304,
1490.67577940567,1491.11065270835,1491.54552601106,1491.98039931382,1492.41527261663,
1492.8509986149,1493.28672461318,1493.72159791609,1494.15647121906,1494.59134452208,
1495.02621782517,1495.46109112832,1495.89596443154,1496.33083773483,1496.76571103819,
1497.20058434163,1497.63545764515,1498.07033094874,1498.50520425242,1498.94007755618,
1499.37495086004,1499.81067685885,1500.24640285767,1500.68127616171,1501.11614946584,
1501.55102277007,1501.9858960744,1502.42076937883,1502.85564268337,1503.29051598801,
1503.72538929276,1504.16026259762,1504.5951359026,1505.03000920769,1505.4648825129,
1505.89975581823,1506.33462912368,1506.77035512331,1507.20608112294,1507.64095442864,
1508.07582773446,1508.51070104041,1508.94557434649,1509.3804476527,1509.81532095904,
1510.25019426552,1510.68506757213,1511.11994087888,1511.55481418577,1511.9896874928,
1512.42456079996,1512.85943410727,1513.29430741472,1513.73003341537,1514.16575941601,
1514.60063272375,1515.03550603163,1515.47037933966,1515.90525264784,1516.34012595616,
1516.77499926463,1517.20987257325,1517.64474588201,1518.07961919093,1518.51449249999,
1518.9493658092,1519.38423911856,1519.81911242807,1520.25398573772,1520.68971173947,
1521.12543774122,1521.56031105118,1521.99518436128,1522.43005767153,1523.29980429246,
1523.73467760315,1524.16955091398,1524.60442422495,1525.03929753607,1525.47417084733,
1525.90904415873,1526.77879078194,1527.64939009657,1528.08511609939,1528.51998941146,
1528.95486272367,1529.38973603601,1530.25948266106,1531.1292292866,1531.99897591261,
1532.86872253907,1533.73846916596,1534.60906848325,1535.47966780073,1536.34941442858,
1537.21916105675,1538.08890768523,1538.95865431398,1539.82840094295,1540.69814757212,
1541.56874689096,1542.43934620985,1543.30909283933,1544.17883946886,1545.04858609839,
1545.91833272787,1546.78807935726,1547.65782598651,1548.52842530518,1549.39902462375,
1550.26877125249,1551.13851788097,1552.00826450914,1552.87801113699,1553.74775776447,
1554.61750439156,1555.48810370844,1556.35870302511,1557.22844965112,1558.09819627666,
1558.96794290171,1559.83768952626,1560.27256283834,1560.70743615028,1561.57718277377,
1562.44778208785,1563.31838140165,1563.75325471277,1564.18812802374,1564.62300133457,
1565.05787464526,1565.9276212662,1566.79736788655,1567.2322411965,1567.66711450631,
1568.10198781596,1568.53686112547,1568.97173443483,1569.40746043628,1569.84318643774,
1570.2780597468,1570.71293305571,1571.14780636448,1571.5826796731,1572.01755298157,
1572.45242628989,1572.88729959806,1573.32217290609,1573.75704621397,1574.19191952171,
1574.62679282931,1575.06166613676,1575.49653944407,1575.93141275123,1576.36713875159,
1576.80286475195,1577.23773805884,1577.67261136559,1578.1074846722,1578.54235797868,
1578.97723128502,1579.41210459124,1579.84697789732,1580.28185120327,1580.71672450909,
1581.15159781478,1581.58647112036,1582.0213444258,1582.45621773113,1582.89109103634,
1583.32681703573,1583.76254303513,1584.1974163401,1584.63228964497,1585.06716294972,
1585.50203625436,1585.9369095589,1586.37178286333,1586.80665616766,1587.24152947189,
1587.67640277602,1588.11127608005,1588.546149384,1588.98102268785,1589.41589599161,
1589.85076929529,1590.28649529394,1590.72222129258,1591.1570945961,1591.59196789953,
1592.0268412029,1592.46171450619,1592.8965878094,1593.33146111256,1593.76633441564,
1594.20120771867,1594.63608102164,1595.07095432455,1595.50582762741,1595.94070093021,
1596.37557423297,1596.81044753569,1597.24617353387,1597.68189953206,1598.11677283469,
1598.55164613729,1598.98651943985,1599.42139274239,1599.8562660449,1600.29113934738,
1600.72601264985,1601.16088595229,1601.59575925472,1602.03063255714,1602.46550585955,
1602.90037916195,1603.33525246435,1603.77012576675,1604.2058517648,1604.64157776285,
1605.07645106526,1605.51132436768,1605.94619767011,1606.38107097255,1606.81594427502,
1607.2508175775,1607.68569088001,1608.12056418254,1608.55543748511,1608.99031078771,
1609.42518409034,1609.86005739302,1610.29493069573,1610.72980399849,1611.16552999674,
1611.60125599499,1612.03612929785,1612.47100260076,1612.90587590373,1613.34074920675,
1613.77562250984,1614.21049581299,1614.64536911621,1615.0802424195,1615.51511572286,
1615.9499890263,1616.38486232981,1616.81973563341,1617.25460893709,1617.68948224085,
1618.12520823963,1618.5609342384,1618.99580754234,1619.43068084638,1619.86555415051,
1620.30042745474,1620.73530075907,1621.1701740635,1621.60504736804,1622.03992067268,
1622.47479397743,1622.90966728229,1623.34454058727,1623.77941389236,1624.21428719757,
1624.6491605029,1625.08488650247,1625.52061250204,1625.95548580761,1626.39035911331,
1626.82523241913,1627.26010572508,1627.69497903116,1628.12985233737,1628.56472564372,
1628.99959895019,1629.43447225681,1629.86934556356,1630.30421887044,1630.73909217747,
1631.17396548464,1631.60883879195,1632.04456479252,1632.48029079309,1632.91516410068,
1633.35003740842,1633.78491071631,1634.21978402433,1634.65465733251,1635.08953064083,
1635.5244039493,1635.95927725792,1636.39415056668,1636.8290238756,1637.26389718466,
1637.69877049387,1638.13364380323,1638.56851711274,1639.00424311442,1639.43996911609,
1639.8748424259,1640.30971573585,1640.74458904595,1641.6143356666,1642.04920897714,
1642.48408228782,1642.91895559865,1643.35382890963,1643.78870222074,1644.223575532,
1645.09332215494,1645.52819546661,1645.96392146936,1646.39964747212,1646.83452078406,
1647.26939409614,1647.70426740834,1648.57401403314,1649.44376065844,1650.31350728422,
1650.74838059729,1651.18325391046,1652.05300053714,1652.92359985428,1653.79419917162,
1654.66394579929,1655.5336924273,1656.40343905563,1657.27318568424,1658.14293231311,
1659.01267894219,1659.88327826096,1660.75387757982,1661.62362420926,1662.49337083877,
1663.3631174683,1664.23286409781,1665.10261072725,1665.97235735658,1666.84295667531,
1667.71355599396,1668.58330262282,1669.45304925143,1670.32279587976,1671.19254250778,
1672.06228913544,1672.93203576273,1673.80263507977,1674.6732343966,1675.54298102284,
1676.41272764862,1677.28247427392,1678.15222089872,1679.021967523,1679.89171414676,
1680.76231346105,1681.19803946366,1681.63291277506,1682.06778608632,1682.50265939743,
1682.93753270841,1683.37240601924,1684.24215264047,1684.67702595086,1685.11189926111,
1685.54677257121,1685.98164588116,1686.41651919097,1686.85139250063,1687.28626581014,
1687.72199181166,1688.15771781319,1688.5925911224,1689.02746443146,1689.46233774038,
1689.89721104914,1690.33208435776,1690.76695766623,1691.20183097455,1691.63670428272,
1692.07157759075,1692.50645089864,1692.94132420637,1693.37619751397,1693.81107082142,
1694.24594412873,1694.68167012916,1695.11739612959,1695.55226943662,1695.9871427435,
1696.42201605025,1696.85688935687,1697.29176266334,1697.72663596969,1698.1615092759,
1698.59638258198,1699.03125588793,1699.46612919375,1699.90100249945,1700.33587580502,
1700.77074911047,1701.20562241579,1701.64134841525,1702.0770744147,1702.51194771979,
1702.94682102476,1703.38169432963,1703.81656763438,1704.25144093902,1704.68631424356,
1705.12118754799,1705.55606085232,1705.99093415655,1706.42580746068,1706.86068076471,
1707.29555406866,1707.73042737251,1708.16530067627,1708.60102667496,1709.03675267365,
1709.47162597724,1709.90649928076,1710.34137258419,1710.77624588756,1711.21111919085,
1711.64599249406,1712.08086579722,1712.5157391003,1712.95061240333,1713.3854857063,
1713.82035900921,1714.25523231207,1714.69010561487,1715.12497891763,1715.56070491584,
1715.99643091404,1716.43130421671,1716.86617751935,1717.30105082195,1717.73592412451,
1718.17079742705,1718.60567072956,1719.04054403204,1719.4754173345,1719.91029063695,
1720.34516393938,1720.7800372418,1721.21491054421,1721.64978384661,1722.08465714901,
1722.52038314706,1722.9561091451,1723.39098244751,1723.82585574992,1724.26072905233,
1724.69560235476,1725.13047565721,1725.56534895967,1726.00022226216,1726.43509556467,
1726.8699688672,1727.30484216977,1727.73971547236,1728.174588775,1728.60946207767,
1729.04433538039,1729.48006137861,1729.91578737684,1730.35066067965,1730.78553398251,
1731.22040728542,1731.65528058838,1732.09015389141,1732.5250271945,1732.95990049765,
1733.39477380087,1733.82964710416,1734.26452040752,1734.69939371096,1735.13426701447,
1735.56914031807,1736.00401362175,1736.43973962048,1736.8754656192,1737.31033892306,
1737.745212227,1738.18008553104,1738.61495883517,1739.0498321394,1739.48470544373,
1739.91957874816,1740.35445205269,1740.78932535734,1741.22419866209,1741.65907196695,
1742.09394527193,1742.52881857702,1742.96369188223,1743.39941788174,1743.83514388125,
1744.2700171867,1744.70489049227,1745.13976379797,1745.57463710379,1746.00951040974,
1746.44438371582,1746.87925702203,1747.31413032837,1747.74900363485,1748.18387694146,
1748.61875024821,1749.0536235551,1749.48849686213,1749.92337016929,1750.3590961698,
1750.7948221703,1751.22969547775,1751.66456878534,1752.09944209308,1752.53431540096,
1752.96918870899,1753.40406201717,1753.83893532549,1754.27380863396,1754.70868194258,
1755.14355525134,1755.57842856026,1756.01330186932,1756.44817517853,1756.88304848789,
1757.31877448949,1757.75450049109,1758.18937380075,1759.05912042051,1759.49399373061,
1759.92886704086,1760.36374035125,1760.79861366179,1761.23348697248,1761.66836028331,
1762.10323359429,1762.5381069054,1763.40785352806,1763.8427268396,1764.27845284228,
1764.71417884496,1765.14905215677,1765.58392546872,1766.0187987808,1766.88854540534,
1767.75829203039,1768.1931653431,1768.62803865593,1769.06291196888,1769.49778528195,
1770.36753190841,1771.2381312254,1772.10873054259,1772.97847717007,1773.84822379791,
1774.71797042609,1775.58771705456,1776.45746368331,1777.32721031228,1778.19780963089,
1779.06840894783,1779.93815555508,1780.80790201176,1781.67764871408),(-0.58309518948453,
0.),.UNSPECIFIED.) ;
#823 = B_SPLINE_SURFACE_WITH_KNOTS('',3,1,((#50304,#50305),(#50306,#50307),
(#50308,#50309),(#50310,#50311),(#50312,#50313),(#50314,#50315),(#50316,
#50317),(#50318,#50319),(#50320,#50321),(#50322,#50323),(#50324,#50325),
(#50326,#50327),(#50328,#50329),(#50330,#50331),(#50332,#50333),(#50334,
#50335),(#50336,#50337),(#50338,#50339),(#50340,#50341),(#50342,#50343),
(#50344,#50345),(#50346,#50347),(#50348,#50349),(#50350,#50351),(#50352,
#50353),(#50354,#50355),(#50356,#50357),(#50358,#50359),(#50360,#50361),
(#50362,#50363),(#50364,#50365),(#50366,#50367),(#50368,#50369),(#50370,
#50371),(#50372,#50373),(#50374,#50375),(#50376,#50377),(#50378,#50379),
(#50380,#50381),(#50382,#50383),(#50384,#50385),(#50386,#50387),(#50388,
#50389),(#50390,#50391),(#50392,#50393),(#50394,#50395),(#50396,#50397),
(#50398,#50399),(#50400,#50401),(#50402,#50403),(#50404,#50405),(#50406,
#50407),(#50408,#50409),(#50410,#50411),(#50412,#50413),(#50414,#50415),
(#50416,#50417),(#50418,#50419),(#50420,#50421),(#50422,#50423),(#50424,
#50425),(#50426,#50427),(#50428,#50429),(#50430,#50431),(#50432,#50433),
(#50434,#50435),(#50436,#50437),(#50438,#50439),(#50440,#50441),(#50442,
#50443),(#50444,#50445),(#50446,#50447),(#50448,#50449),(#50450,#50451),
(#50452,#50453),(#50454,#50455),(#50456,#50457),(#50458,#50459),(#50460,
#50461),(#50462,#50463),(#50464,#50465),(#50466,#50467),(#50468,#50469),
(#50470,#50471),(#50472,#50473),(#50474,#50475),(#50476,#50477),(#50478,
#50479),(#50480,#50481),(#50482,#50483),(#50484,#50485),(#50486,#50487),
(#50488,#50489),(#50490,#50491),(#50492,#50493),(#50494,#50495),(#50496,
#50497),(#50498,#50499),(#50500,#50501),(#50502,#50503),(#50504,#50505),
(#50506,#50507),(#50508,#50509),(#50510,#50511),(#50512,#50513),(#50514,
#50515),(#50516,#50517),(#50518,#50519),(#50520,#50521),(#50522,#50523),
(#50524,#50525),(#50526,#50527),(#50528,#50529),(#50530,#50531),(#50532,
#50533),(#50534,#50535),(#50536,#50537),(#50538,#50539),(#50540,#50541),
(#50542,#50543),(#50544,#50545),(#50546,#50547),(#50548,#50549),(#50550,
#50551),(#50552,#50553),(#50554,#50555),(#50556,#50557),(#50558,#50559),
(#50560,#50561),(#50562,#50563),(#50564,#50565),(#50566,#50567),(#50568,
#50569),(#50570,#50571),(#50572,#50573),(#50574,#50575),(#50576,#50577),
(#50578,#50579),(#50580,#50581),(#50582,#50583),(#50584,#50585),(#50586,
#50587),(#50588,#50589),(#50590,#50591),(#50592,#50593),(#50594,#50595),
(#50596,#50597),(#50598,#50599),(#50600,#50601),(#50602,#50603),(#50604,
#50605),(#50606,#50607),(#50608,#50609),(#50610,#50611),(#50612,#50613),
(#50614,#50615),(#50616,#50617),(#50618,#50619),(#50620,#50621),(#50622,
#50623),(#50624,#50625),(#50626,#50627),(#50628,#50629),(#50630,#50631),
(#50632,#50633),(#50634,#50635),(#50636,#50637),(#50638,#50639),(#50640,
#50641),(#50642,#50643),(#50644,#50645),(#50646,#50647),(#50648,#50649),
(#50650,#50651),(#50652,#50653),(#50654,#50655),(#50656,#50657),(#50658,
#50659),(#50660,#50661),(#50662,#50663),(#50664,#50665),(#50666,#50667),
(#50668,#50669),(#50670,#50671),(#50672,#50673),(#50674,#50675),(#50676,
#50677),(#50678,#50679),(#50680,#50681),(#50682,#50683),(#50684,#50685),
(#50686,#50687),(#50688,#50689),(#50690,#50691),(#50692,#50693),(#50694,
#50695),(#50696,#50697),(#50698,#50699),(#50700,#50701),(#50702,#50703),
(#50704,#50705),(#50706,#50707),(#50708,#50709),(#50710,#50711),(#50712,
#50713),(#50714,#50715),(#50716,#50717),(#50718,#50719),(#50720,#50721),
(#50722,#50723),(#50724,#50725),(#50726,#50727),(#50728,#50729),(#50730,
#50731),(#50732,#50733),(#50734,#50735),(#50736,#50737),(#50738,#50739),
(#50740,#50741),(#50742,#50743),(#50744,#50745),(#50746,#50747),(#50748,
#50749),(#50750,#50751),(#50752,#50753),(#50754,#50755),(#50756,#50757),
(#50758,#50759),(#50760,#50761),(#50762,#50763),(#50764,#50765),(#50766,
#50767),(#50768,#50769),(#50770,#50771),(#50772,#50773),(#50774,#50775),
(#50776,#50777),(#50778,#50779),(#50780,#50781),(#50782,#50783),(#50784,
#50785),(#50786,#50787),(#50788,#50789),(#50790,#50791),(#50792,#50793),
(#50794,#50795),(#50796,#50797),(#50798,#50799),(#50800,#50801),(#50802,
#50803),(#50804,#50805),(#50806,#50807),(#50808,#50809),(#50810,#50811),
(#50812,#50813),(#50814,#50815),(#50816,#50817),(#50818,#50819),(#50820,
#50821),(#50822,#50823),(#50824,#50825),(#50826,#50827),(#50828,#50829),
(#50830,#50831),(#50832,#50833),(#50834,#50835),(#50836,#50837),(#50838,
#50839),(#50840,#50841),(#50842,#50843),(#50844,#50845),(#50846,#50847),
(#50848,#50849),(#50850,#50851),(#50852,#50853),(#50854,#50855),(#50856,
#50857),(#50858,#50859),(#50860,#50861),(#50862,#50863),(#50864,#50865),
(#50866,#50867),(#50868,#50869),(#50870,#50871),(#50872,#50873),(#50874,
#50875),(#50876,#50877),(#50878,#50879),(#50880,#50881),(#50882,#50883),
(#50884,#50885),(#50886,#50887),(#50888,#50889),(#50890,#50891),(#50892,
#50893),(#50894,#50895),(#50896,#50897),(#50898,#50899),(#50900,#50901),
(#50902,#50903),(#50904,#50905),(#50906,#50907),(#50908,#50909),(#50910,
#50911),(#50912,#50913),(#50914,#50915),(#50916,#50917),(#50918,#50919),
(#50920,#50921),(#50922,#50923),(#50924,#50925),(#50926,#50927),(#50928,
#50929),(#50930,#50931),(#50932,#50933),(#50934,#50935),(#50936,#50937),
(#50938,#50939),(#50940,#50941),(#50942,#50943),(#50944,#50945),(#50946,
#50947),(#50948,#50949),(#50950,#50951),(#50952,#50953),(#50954,#50955),
(#50956,#50957),(#50958,#50959),(#50960,#50961),(#50962,#50963),(#50964,
#50965),(#50966,#50967),(#50968,#50969),(#50970,#50971),(#50972,#50973),
(#50974,#50975),(#50976,#50977),(#50978,#50979),(#50980,#50981),(#50982,
#50983),(#50984,#50985),(#50986,#50987),(#50988,#50989),(#50990,#50991),
(#50992,#50993),(#50994,#50995),(#50996,#50997),(#50998,#50999),(#51000,
#51001),(#51002,#51003),(#51004,#51005),(#51006,#51007),(#51008,#51009),
(#51010,#51011),(#51012,#51013),(#51014,#51015),(#51016,#51017),(#51018,
#51019),(#51020,#51021),(#51022,#51023),(#51024,#51025),(#51026,#51027),
(#51028,#51029),(#51030,#51031),(#51032,#51033),(#51034,#51035),(#51036,
#51037),(#51038,#51039),(#51040,#51041),(#51042,#51043),(#51044,#51045),
(#51046,#51047),(#51048,#51049),(#51050,#51051),(#51052,#51053),(#51054,
#51055),(#51056,#51057),(#51058,#51059),(#51060,#51061),(#51062,#51063),
(#51064,#51065),(#51066,#51067),(#51068,#51069),(#51070,#51071),(#51072,
#51073),(#51074,#51075),(#51076,#51077),(#51078,#51079),(#51080,#51081),
(#51082,#51083),(#51084,#51085),(#51086,#51087),(#51088,#51089),(#51090,
#51091),(#51092,#51093),(#51094,#51095),(#51096,#51097),(#51098,#51099),
(#51100,#51101),(#51102,#51103),(#51104,#51105),(#51106,#51107),(#51108,
#51109),(#51110,#51111),(#51112,#51113),(#51114,#51115),(#51116,#51117),
(#51118,#51119),(#51120,#51121),(#51122,#51123),(#51124,#51125),(#51126,
#51127),(#51128,#51129),(#51130,#51131),(#51132,#51133),(#51134,#51135),
(#51136,#51137),(#51138,#51139),(#51140,#51141),(#51142,#51143),(#51144,
#51145),(#51146,#51147),(#51148,#51149),(#51150,#51151),(#51152,#51153),
(#51154,#51155),(#51156,#51157),(#51158,#51159),(#51160,#51161),(#51162,
#51163),(#51164,#51165),(#51166,#51167),(#51168,#51169),(#51170,#51171),
(#51172,#51173),(#51174,#51175),(#51176,#51177),(#51178,#51179),(#51180,
#51181),(#51182,#51183),(#51184,#51185),(#51186,#51187),(#51188,#51189),
(#51190,#51191),(#51192,#51193),(#51194,#51195),(#51196,#51197),(#51198,
#51199),(#51200,#51201),(#51202,#51203),(#51204,#51205),(#51206,#51207),
(#51208,#51209),(#51210,#51211),(#51212,#51213),(#51214,#51215),(#51216,
#51217),(#51218,#51219),(#51220,#51221),(#51222,#51223),(#51224,#51225),
(#51226,#51227),(#51228,#51229),(#51230,#51231),(#51232,#51233),(#51234,
#51235),(#51236,#51237),(#51238,#51239),(#51240,#51241),(#51242,#51243),
(#51244,#51245),(#51246,#51247),(#51248,#51249),(#51250,#51251),(#51252,
#51253),(#51254,#51255),(#51256,#51257),(#51258,#51259),(#51260,#51261),
(#51262,#51263),(#51264,#51265),(#51266,#51267),(#51268,#51269),(#51270,
#51271),(#51272,#51273),(#51274,#51275),(#51276,#51277),(#51278,#51279),
(#51280,#51281),(#51282,#51283),(#51284,#51285),(#51286,#51287),(#51288,
#51289),(#51290,#51291),(#51292,#51293),(#51294,#51295),(#51296,#51297),
(#51298,#51299),(#51300,#51301),(#51302,#51303),(#51304,#51305),(#51306,
#51307),(#51308,#51309),(#51310,#51311),(#51312,#51313),(#51314,#51315),
(#51316,#51317),(#51318,#51319),(#51320,#51321),(#51322,#51323),(#51324,
#51325),(#51326,#51327),(#51328,#51329),(#51330,#51331),(#51332,#51333),
(#51334,#51335),(#51336,#51337),(#51338,#51339),(#51340,#51341),(#51342,
#51343),(#51344,#51345),(#51346,#51347),(#51348,#51349),(#51350,#51351),
(#51352,#51353),(#51354,#51355),(#51356,#51357),(#51358,#51359),(#51360,
#51361),(#51362,#51363),(#51364,#51365),(#51366,#51367),(#51368,#51369),
(#51370,#51371),(#51372,#51373),(#51374,#51375),(#51376,#51377),(#51378,
#51379),(#51380,#51381),(#51382,#51383),(#51384,#51385),(#51386,#51387),
(#51388,#51389),(#51390,#51391),(#51392,#51393),(#51394,#51395),(#51396,
#51397),(#51398,#51399),(#51400,#51401),(#51402,#51403),(#51404,#51405),
(#51406,#51407),(#51408,#51409),(#51410,#51411),(#51412,#51413),(#51414,
#51415),(#51416,#51417),(#51418,#51419),(#51420,#51421),(#51422,#51423),
(#51424,#51425),(#51426,#51427),(#51428,#51429),(#51430,#51431),(#51432,
#51433),(#51434,#51435),(#51436,#51437),(#51438,#51439),(#51440,#51441),
(#51442,#51443),(#51444,#51445),(#51446,#51447),(#51448,#51449),(#51450,
#51451),(#51452,#51453),(#51454,#51455),(#51456,#51457),(#51458,#51459),
(#51460,#51461),(#51462,#51463),(#51464,#51465),(#51466,#51467),(#51468,
#51469),(#51470,#51471),(#51472,#51473),(#51474,#51475),(#51476,#51477),
(#51478,#51479),(#51480,#51481),(#51482,#51483),(#51484,#51485),(#51486,
#51487),(#51488,#51489),(#51490,#51491),(#51492,#51493),(#51494,#51495),
(#51496,#51497),(#51498,#51499),(#51500,#51501),(#51502,#51503),(#51504,
#51505),(#51506,#51507),(#51508,#51509),(#51510,#51511),(#51512,#51513),
(#51514,#51515),(#51516,#51517),(#51518,#51519),(#51520,#51521),(#51522,
#51523),(#51524,#51525),(#51526,#51527),(#51528,#51529),(#51530,#51531),
(#51532,#51533),(#51534,#51535),(#51536,#51537),(#51538,#51539),(#51540,
#51541),(#51542,#51543),(#51544,#51545),(#51546,#51547),(#51548,#51549),
(#51550,#51551),(#51552,#51553),(#51554,#51555),(#51556,#51557),(#51558,
#51559),(#51560,#51561),(#51562,#51563),(#51564,#51565),(#51566,#51567),
(#51568,#51569),(#51570,#51571),(#51572,#51573),(#51574,#51575),(#51576,
#51577),(#51578,#51579),(#51580,#51581),(#51582,#51583),(#51584,#51585),
(#51586,#51587),(#51588,#51589),(#51590,#51591),(#51592,#51593),(#51594,
#51595),(#51596,#51597),(#51598,#51599),(#51600,#51601),(#51602,#51603),
(#51604,#51605),(#51606,#51607),(#51608,#51609),(#51610,#51611),(#51612,
#51613),(#51614,#51615),(#51616,#51617),(#51618,#51619),(#51620,#51621),
(#51622,#51623),(#51624,#51625),(#51626,#51627),(#51628,#51629),(#51630,
#51631),(#51632,#51633),(#51634,#51635),(#51636,#51637),(#51638,#51639),
(#51640,#51641),(#51642,#51643),(#51644,#51645),(#51646,#51647),(#51648,
#51649),(#51650,#51651),(#51652,#51653),(#51654,#51655),(#51656,#51657),
(#51658,#51659),(#51660,#51661),(#51662,#51663),(#51664,#51665),(#51666,
#51667),(#51668,#51669),(#51670,#51671),(#51672,#51673),(#51674,#51675),
(#51676,#51677),(#51678,#51679),(#51680,#51681),(#51682,#51683),(#51684,
#51685),(#51686,#51687),(#51688,#51689),(#51690,#51691),(#51692,#51693),
(#51694,#51695),(#51696,#51697),(#51698,#51699),(#51700,#51701),(#51702,
#51703),(#51704,#51705),(#51706,#51707),(#51708,#51709),(#51710,#51711),
(#51712,#51713),(#51714,#51715),(#51716,#51717),(#51718,#51719),(#51720,
#51721),(#51722,#51723),(#51724,#51725),(#51726,#51727),(#51728,#51729),
(#51730,#51731),(#51732,#51733),(#51734,#51735),(#51736,#51737),(#51738,
#51739),(#51740,#51741),(#51742,#51743),(#51744,#51745),(#51746,#51747),
(#51748,#51749),(#51750,#51751),(#51752,#51753),(#51754,#51755),(#51756,
#51757),(#51758,#51759),(#51760,#51761),(#51762,#51763),(#51764,#51765),
(#51766,#51767),(#51768,#51769),(#51770,#51771),(#51772,#51773),(#51774,
#51775),(#51776,#51777),(#51778,#51779),(#51780,#51781),(#51782,#51783),
(#51784,#51785),(#51786,#51787),(#51788,#51789),(#51790,#51791),(#51792,
#51793),(#51794,#51795),(#51796,#51797),(#51798,#51799),(#51800,#51801),
(#51802,#51803),(#51804,#51805),(#51806,#51807),(#51808,#51809),(#51810,
#51811),(#51812,#51813),(#51814,#51815),(#51816,#51817),(#51818,#51819),
(#51820,#51821),(#51822,#51823),(#51824,#51825),(#51826,#51827),(#51828,
#51829),(#51830,#51831),(#51832,#51833),(#51834,#51835),(#51836,#51837),
(#51838,#51839),(#51840,#51841),(#51842,#51843),(#51844,#51845),(#51846,
#51847),(#51848,#51849),(#51850,#51851),(#51852,#51853),(#51854,#51855),
(#51856,#51857),(#51858,#51859),(#51860,#51861),(#51862,#51863),(#51864,
#51865),(#51866,#51867),(#51868,#51869),(#51870,#51871),(#51872,#51873),
(#51874,#51875),(#51876,#51877),(#51878,#51879),(#51880,#51881),(#51882,
#51883),(#51884,#51885),(#51886,#51887),(#51888,#51889),(#51890,#51891),
(#51892,#51893),(#51894,#51895),(#51896,#51897),(#51898,#51899),(#51900,
#51901),(#51902,#51903),(#51904,#51905),(#51906,#51907),(#51908,#51909),
(#51910,#51911),(#51912,#51913),(#51914,#51915),(#51916,#51917),(#51918,
#51919),(#51920,#51921),(#51922,#51923),(#51924,#51925),(#51926,#51927),
(#51928,#51929),(#51930,#51931),(#51932,#51933),(#51934,#51935),(#51936,
#51937),(#51938,#51939),(#51940,#51941),(#51942,#51943),(#51944,#51945),
(#51946,#51947),(#51948,#51949),(#51950,#51951),(#51952,#51953),(#51954,
#51955),(#51956,#51957),(#51958,#51959),(#51960,#51961),(#51962,#51963),
(#51964,#51965),(#51966,#51967),(#51968,#51969),(#51970,#51971),(#51972,
#51973),(#51974,#51975),(#51976,#51977),(#51978,#51979),(#51980,#51981),
(#51982,#51983),(#51984,#51985),(#51986,#51987),(#51988,#51989),(#51990,
#51991),(#51992,#51993),(#51994,#51995),(#51996,#51997),(#51998,#51999),
(#52000,#52001),(#52002,#52003),(#52004,#52005),(#52006,#52007),(#52008,
#52009),(#52010,#52011),(#52012,#52013),(#52014,#52015),(#52016,#52017),
(#52018,#52019),(#52020,#52021),(#52022,#52023),(#52024,#52025),(#52026,
#52027),(#52028,#52029),(#52030,#52031),(#52032,#52033),(#52034,#52035),
(#52036,#52037),(#52038,#52039),(#52040,#52041),(#52042,#52043),(#52044,
#52045),(#52046,#52047),(#52048,#52049),(#52050,#52051),(#52052,#52053),
(#52054,#52055),(#52056,#52057),(#52058,#52059),(#52060,#52061),(#52062,
#52063),(#52064,#52065),(#52066,#52067),(#52068,#52069),(#52070,#52071),
(#52072,#52073),(#52074,#52075),(#52076,#52077),(#52078,#52079),(#52080,
#52081),(#52082,#52083),(#52084,#52085),(#52086,#52087),(#52088,#52089),
(#52090,#52091),(#52092,#52093),(#52094,#52095),(#52096,#52097),(#52098,
#52099),(#52100,#52101),(#52102,#52103),(#52104,#52105),(#52106,#52107),
(#52108,#52109),(#52110,#52111),(#52112,#52113),(#52114,#52115),(#52116,
#52117),(#52118,#52119),(#52120,#52121),(#52122,#52123),(#52124,#52125),
(#52126,#52127),(#52128,#52129),(#52130,#52131),(#52132,#52133),(#52134,
#52135),(#52136,#52137),(#52138,#52139),(#52140,#52141),(#52142,#52143),
(#52144,#52145),(#52146,#52147),(#52148,#52149),(#52150,#52151),(#52152,
#52153),(#52154,#52155),(#52156,#52157),(#52158,#52159),(#52160,#52161),
(#52162,#52163),(#52164,#52165),(#52166,#52167),(#52168,#52169),(#52170,
#52171),(#52172,#52173),(#52174,#52175),(#52176,#52177),(#52178,#52179),
(#52180,#52181),(#52182,#52183),(#52184,#52185),(#52186,#52187),(#52188,
#52189),(#52190,#52191),(#52192,#52193),(#52194,#52195),(#52196,#52197),
(#52198,#52199),(#52200,#52201),(#52202,#52203),(#52204,#52205),(#52206,
#52207),(#52208,#52209),(#52210,#52211),(#52212,#52213),(#52214,#52215),
(#52216,#52217),(#52218,#52219),(#52220,#52221),(#52222,#52223),(#52224,
#52225),(#52226,#52227),(#52228,#52229),(#52230,#52231),(#52232,#52233),
(#52234,#52235),(#52236,#52237),(#52238,#52239),(#52240,#52241),(#52242,
#52243),(#52244,#52245),(#52246,#52247),(#52248,#52249),(#52250,#52251),
(#52252,#52253),(#52254,#52255),(#52256,#52257),(#52258,#52259),(#52260,
#52261),(#52262,#52263),(#52264,#52265),(#52266,#52267),(#52268,#52269),
(#52270,#52271),(#52272,#52273),(#52274,#52275),(#52276,#52277),(#52278,
#52279),(#52280,#52281),(#52282,#52283),(#52284,#52285),(#52286,#52287),
(#52288,#52289),(#52290,#52291),(#52292,#52293),(#52294,#52295),(#52296,
#52297),(#52298,#52299),(#52300,#52301),(#52302,#52303),(#52304,#52305),
(#52306,#52307),(#52308,#52309),(#52310,#52311),(#52312,#52313),(#52314,
#52315),(#52316,#52317),(#52318,#52319),(#52320,#52321),(#52322,#52323),
(#52324,#52325),(#52326,#52327),(#52328,#52329),(#52330,#52331),(#52332,
#52333),(#52334,#52335),(#52336,#52337),(#52338,#52339),(#52340,#52341),
(#52342,#52343),(#52344,#52345),(#52346,#52347),(#52348,#52349),(#52350,
#52351),(#52352,#52353),(#52354,#52355),(#52356,#52357),(#52358,#52359),
(#52360,#52361),(#52362,#52363),(#52364,#52365),(#52366,#52367),(#52368,
#52369),(#52370,#52371),(#52372,#52373),(#52374,#52375),(#52376,#52377),
(#52378,#52379),(#52380,#52381),(#52382,#52383),(#52384,#52385),(#52386,
#52387),(#52388,#52389),(#52390,#52391),(#52392,#52393),(#52394,#52395),
(#52396,#52397),(#52398,#52399),(#52400,#52401),(#52402,#52403),(#52404,
#52405),(#52406,#52407),(#52408,#52409),(#52410,#52411),(#52412,#52413),
(#52414,#52415),(#52416,#52417),(#52418,#52419),(#52420,#52421),(#52422,
#52423),(#52424,#52425),(#52426,#52427),(#52428,#52429),(#52430,#52431),
(#52432,#52433),(#52434,#52435),(#52436,#52437),(#52438,#52439),(#52440,
#52441),(#52442,#52443),(#52444,#52445),(#52446,#52447),(#52448,#52449),
(#52450,#52451),(#52452,#52453),(#52454,#52455),(#52456,#52457),(#52458,
#52459),(#52460,#52461),(#52462,#52463),(#52464,#52465),(#52466,#52467),
(#52468,#52469),(#52470,#52471),(#52472,#52473),(#52474,#52475),(#52476,
#52477),(#52478,#52479),(#52480,#52481),(#52482,#52483),(#52484,#52485),
(#52486,#52487),(#52488,#52489),(#52490,#52491),(#52492,#52493),(#52494,
#52495),(#52496,#52497),(#52498,#52499),(#52500,#52501),(#52502,#52503),
(#52504,#52505),(#52506,#52507),(#52508,#52509),(#52510,#52511),(#52512,
#52513),(#52514,#52515),(#52516,#52517),(#52518,#52519),(#52520,#52521),
(#52522,#52523),(#52524,#52525),(#52526,#52527),(#52528,#52529),(#52530,
#52531),(#52532,#52533),(#52534,#52535),(#52536,#52537),(#52538,#52539),
(#52540,#52541),(#52542,#52543),(#52544,#52545),(#52546,#52547),(#52548,
#52549),(#52550,#52551),(#52552,#52553),(#52554,#52555),(#52556,#52557),
(#52558,#52559),(#52560,#52561),(#52562,#52563),(#52564,#52565),(#52566,
#52567),(#52568,#52569),(#52570,#52571),(#52572,#52573),(#52574,#52575),
(#52576,#52577),(#52578,#52579),(#52580,#52581),(#52582,#52583),(#52584,
#52585),(#52586,#52587),(#52588,#52589),(#52590,#52591),(#52592,#52593),
(#52594,#52595),(#52596,#52597),(#52598,#52599),(#52600,#52601),(#52602,
#52603),(#52604,#52605),(#52606,#52607),(#52608,#52609),(#52610,#52611),
(#52612,#52613),(#52614,#52615),(#52616,#52617),(#52618,#52619),(#52620,
#52621),(#52622,#52623),(#52624,#52625),(#52626,#52627),(#52628,#52629),
(#52630,#52631),(#52632,#52633),(#52634,#52635),(#52636,#52637),(#52638,
#52639),(#52640,#52641),(#52642,#52643),(#52644,#52645),(#52646,#52647),
(#52648,#52649),(#52650,#52651),(#52652,#52653),(#52654,#52655),(#52656,
#52657),(#52658,#52659),(#52660,#52661),(#52662,#52663),(#52664,#52665),
(#52666,#52667),(#52668,#52669),(#52670,#52671),(#52672,#52673),(#52674,
#52675),(#52676,#52677),(#52678,#52679),(#52680,#52681),(#52682,#52683),
(#52684,#52685),(#52686,#52687),(#52688,#52689),(#52690,#52691),(#52692,
#52693),(#52694,#52695),(#52696,#52697),(#52698,#52699),(#52700,#52701),
(#52702,#52703),(#52704,#52705),(#52706,#52707),(#52708,#52709),(#52710,
#52711),(#52712,#52713),(#52714,#52715),(#52716,#52717),(#52718,#52719),
(#52720,#52721),(#52722,#52723),(#52724,#52725),(#52726,#52727),(#52728,
#52729),(#52730,#52731),(#52732,#52733),(#52734,#52735),(#52736,#52737),
(#52738,#52739),(#52740,#52741),(#52742,#52743),(#52744,#52745),(#52746,
#52747),(#52748,#52749),(#52750,#52751),(#52752,#52753),(#52754,#52755),
(#52756,#52757),(#52758,#52759),(#52760,#52761),(#52762,#52763),(#52764,
#52765),(#52766,#52767),(#52768,#52769),(#52770,#52771),(#52772,#52773),
(#52774,#52775),(#52776,#52777),(#52778,#52779),(#52780,#52781),(#52782,
#52783),(#52784,#52785),(#52786,#52787),(#52788,#52789),(#52790,#52791),
(#52792,#52793),(#52794,#52795),(#52796,#52797),(#52798,#52799),(#52800,
#52801),(#52802,#52803),(#52804,#52805),(#52806,#52807),(#52808,#52809),
(#52810,#52811),(#52812,#52813),(#52814,#52815),(#52816,#52817),(#52818,
#52819),(#52820,#52821),(#52822,#52823),(#52824,#52825),(#52826,#52827),
(#52828,#52829),(#52830,#52831),(#52832,#52833),(#52834,#52835),(#52836,
#52837),(#52838,#52839),(#52840,#52841),(#52842,#52843),(#52844,#52845),
(#52846,#52847),(#52848,#52849),(#52850,#52851),(#52852,#52853),(#52854,
#52855),(#52856,#52857),(#52858,#52859),(#52860,#52861),(#52862,#52863),
(#52864,#52865),(#52866,#52867),(#52868,#52869),(#52870,#52871),(#52872,
#52873),(#52874,#52875),(#52876,#52877),(#52878,#52879),(#52880,#52881),
(#52882,#52883),(#52884,#52885),(#52886,#52887),(#52888,#52889),(#52890,
#52891),(#52892,#52893),(#52894,#52895),(#52896,#52897),(#52898,#52899),
(#52900,#52901),(#52902,#52903),(#52904,#52905),(#52906,#52907),(#52908,
#52909),(#52910,#52911),(#52912,#52913),(#52914,#52915),(#52916,#52917),
(#52918,#52919),(#52920,#52921),(#52922,#52923),(#52924,#52925),(#52926,
#52927),(#52928,#52929),(#52930,#52931),(#52932,#52933),(#52934,#52935),
(#52936,#52937),(#52938,#52939),(#52940,#52941),(#52942,#52943),(#52944,
#52945),(#52946,#52947),(#52948,#52949),(#52950,#52951),(#52952,#52953),
(#52954,#52955),(#52956,#52957),(#52958,#52959),(#52960,#52961),(#52962,
#52963),(#52964,#52965),(#52966,#52967),(#52968,#52969),(#52970,#52971),
(#52972,#52973),(#52974,#52975),(#52976,#52977),(#52978,#52979),(#52980,
#52981),(#52982,#52983),(#52984,#52985),(#52986,#52987),(#52988,#52989),
(#52990,#52991),(#52992,#52993),(#52994,#52995),(#52996,#52997),(#52998,
#52999),(#53000,#53001),(#53002,#53003),(#53004,#53005),(#53006,#53007),
(#53008,#53009),(#53010,#53011),(#53012,#53013),(#53014,#53015),(#53016,
#53017),(#53018,#53019),(#53020,#53021),(#53022,#53023),(#53024,#53025),
(#53026,#53027),(#53028,#53029),(#53030,#53031),(#53032,#53033),(#53034,
#53035),(#53036,#53037),(#53038,#53039),(#53040,#53041),(#53042,#53043),
(#53044,#53045),(#53046,#53047),(#53048,#53049),(#53050,#53051),(#53052,
#53053),(#53054,#53055),(#53056,#53057),(#53058,#53059),(#53060,#53061),
(#53062,#53063),(#53064,#53065),(#53066,#53067),(#53068,#53069),(#53070,
#53071),(#53072,#53073),(#53074,#53075),(#53076,#53077),(#53078,#53079),
(#53080,#53081),(#53082,#53083),(#53084,#53085),(#53086,#53087),(#53088,
#53089),(#53090,#53091),(#53092,#53093),(#53094,#53095),(#53096,#53097),
(#53098,#53099),(#53100,#53101),(#53102,#53103),(#53104,#53105),(#53106,
#53107),(#53108,#53109),(#53110,#53111),(#53112,#53113),(#53114,#53115),
(#53116,#53117),(#53118,#53119),(#53120,#53121),(#53122,#53123),(#53124,
#53125),(#53126,#53127),(#53128,#53129),(#53130,#53131),(#53132,#53133),
(#53134,#53135),(#53136,#53137),(#53138,#53139),(#53140,#53141),(#53142,
#53143),(#53144,#53145),(#53146,#53147),(#53148,#53149),(#53150,#53151),
(#53152,#53153),(#53154,#53155),(#53156,#53157),(#53158,#53159),(#53160,
#53161),(#53162,#53163),(#53164,#53165),(#53166,#53167),(#53168,#53169),
(#53170,#53171),(#53172,#53173),(#53174,#53175),(#53176,#53177),(#53178,
#53179),(#53180,#53181),(#53182,#53183),(#53184,#53185),(#53186,#53187),
(#53188,#53189),(#53190,#53191),(#53192,#53193),(#53194,#53195),(#53196,
#53197),(#53198,#53199),(#53200,#53201),(#53202,#53203),(#53204,#53205),
(#53206,#53207),(#53208,#53209),(#53210,#53211),(#53212,#53213),(#53214,
#53215),(#53216,#53217),(#53218,#53219),(#53220,#53221),(#53222,#53223),
(#53224,#53225),(#53226,#53227),(#53228,#53229),(#53230,#53231),(#53232,
#53233),(#53234,#53235),(#53236,#53237),(#53238,#53239),(#53240,#53241),
(#53242,#53243),(#53244,#53245),(#53246,#53247),(#53248,#53249),(#53250,
#53251),(#53252,#53253),(#53254,#53255),(#53256,#53257),(#53258,#53259),
(#53260,#53261),(#53262,#53263),(#53264,#53265),(#53266,#53267),(#53268,
#53269),(#53270,#53271),(#53272,#53273),(#53274,#53275),(#53276,#53277),
(#53278,#53279),(#53280,#53281),(#53282,#53283),(#53284,#53285),(#53286,
#53287),(#53288,#53289),(#53290,#53291),(#53292,#53293),(#53294,#53295),
(#53296,#53297),(#53298,#53299),(#53300,#53301),(#53302,#53303),(#53304,
#53305),(#53306,#53307),(#53308,#53309),(#53310,#53311),(#53312,#53313),
(#53314,#53315),(#53316,#53317),(#53318,#53319),(#53320,#53321),(#53322,
#53323),(#53324,#53325),(#53326,#53327),(#53328,#53329),(#53330,#53331),
(#53332,#53333),(#53334,#53335),(#53336,#53337),(#53338,#53339),(#53340,
#53341),(#53342,#53343),(#53344,#53345),(#53346,#53347),(#53348,#53349),
(#53350,#53351),(#53352,#53353),(#53354,#53355),(#53356,#53357),(#53358,
#53359),(#53360,#53361),(#53362,#53363),(#53364,#53365),(#53366,#53367),
(#53368,#53369),(#53370,#53371),(#53372,#53373),(#53374,#53375),(#53376,
#53377),(#53378,#53379),(#53380,#53381),(#53382,#53383),(#53384,#53385),
(#53386,#53387),(#53388,#53389),(#53390,#53391),(#53392,#53393),(#53394,
#53395),(#53396,#53397),(#53398,#53399),(#53400,#53401),(#53402,#53403),
(#53404,#53405),(#53406,#53407),(#53408,#53409),(#53410,#53411),(#53412,
#53413),(#53414,#53415),(#53416,#53417),(#53418,#53419),(#53420,#53421),
(#53422,#53423),(#53424,#53425),(#53426,#53427),(#53428,#53429),(#53430,
#53431),(#53432,#53433),(#53434,#53435),(#53436,#53437),(#53438,#53439),
(#53440,#53441),(#53442,#53443),(#53444,#53445),(#53446,#53447),(#53448,
#53449),(#53450,#53451),(#53452,#53453),(#53454,#53455),(#53456,#53457),
(#53458,#53459),(#53460,#53461),(#53462,#53463),(#53464,#53465),(#53466,
#53467),(#53468,#53469),(#53470,#53471),(#53472,#53473),(#53474,#53475),
(#53476,#53477),(#53478,#53479),(#53480,#53481),(#53482,#53483),(#53484,
#53485),(#53486,#53487),(#53488,#53489),(#53490,#53491),(#53492,#53493),
(#53494,#53495),(#53496,#53497),(#53498,#53499),(#53500,#53501),(#53502,
#53503),(#53504,#53505),(#53506,#53507),(#53508,#53509),(#53510,#53511),
(#53512,#53513),(#53514,#53515),(#53516,#53517),(#53518,#53519),(#53520,
#53521),(#53522,#53523),(#53524,#53525),(#53526,#53527),(#53528,#53529),
(#53530,#53531),(#53532,#53533),(#53534,#53535),(#53536,#53537),(#53538,
#53539),(#53540,#53541),(#53542,#53543),(#53544,#53545),(#53546,#53547),
(#53548,#53549),(#53550,#53551),(#53552,#53553),(#53554,#53555),(#53556,
#53557),(#53558,#53559),(#53560,#53561),(#53562,#53563),(#53564,#53565),
(#53566,#53567),(#53568,#53569),(#53570,#53571),(#53572,#53573),(#53574,
#53575),(#53576,#53577),(#53578,#53579),(#53580,#53581),(#53582,#53583),
(#53584,#53585),(#53586,#53587),(#53588,#53589),(#53590,#53591),(#53592,
#53593),(#53594,#53595),(#53596,#53597),(#53598,#53599),(#53600,#53601),
(#53602,#53603),(#53604,#53605),(#53606,#53607),(#53608,#53609),(#53610,
#53611),(#53612,#53613),(#53614,#53615),(#53616,#53617),(#53618,#53619),
(#53620,#53621),(#53622,#53623),(#53624,#53625),(#53626,#53627),(#53628,
#53629),(#53630,#53631),(#53632,#53633),(#53634,#53635),(#53636,#53637),
(#53638,#53639),(#53640,#53641),(#53642,#53643),(#53644,#53645),(#53646,
#53647),(#53648,#53649),(#53650,#53651),(#53652,#53653),(#53654,#53655),
(#53656,#53657),(#53658,#53659),(#53660,#53661),(#53662,#53663),(#53664,
#53665),(#53666,#53667),(#53668,#53669),(#53670,#53671),(#53672,#53673),
(#53674,#53675),(#53676,#53677),(#53678,#53679),(#53680,#53681),(#53682,
#53683),(#53684,#53685),(#53686,#53687),(#53688,#53689),(#53690,#53691),
(#53692,#53693),(#53694,#53695),(#53696,#53697),(#53698,#53699),(#53700,
#53701),(#53702,#53703),(#53704,#53705),(#53706,#53707),(#53708,#53709),
(#53710,#53711),(#53712,#53713),(#53714,#53715),(#53716,#53717),(#53718,
#53719),(#53720,#53721),(#53722,#53723),(#53724,#53725),(#53726,#53727),
(#53728,#53729),(#53730,#53731),(#53732,#53733),(#53734,#53735),(#53736,
#53737),(#53738,#53739),(#53740,#53741),(#53742,#53743),(#53744,#53745),
(#53746,#53747),(#53748,#53749),(#53750,#53751),(#53752,#53753),(#53754,
#53755),(#53756,#53757),(#53758,#53759),(#53760,#53761),(#53762,#53763),
(#53764,#53765),(#53766,#53767),(#53768,#53769),(#53770,#53771),(#53772,
#53773),(#53774,#53775),(#53776,#53777),(#53778,#53779),(#53780,#53781),
(#53782,#53783),(#53784,#53785),(#53786,#53787),(#53788,#53789),(#53790,
#53791),(#53792,#53793),(#53794,#53795),(#53796,#53797),(#53798,#53799),
(#53800,#53801),(#53802,#53803),(#53804,#53805),(#53806,#53807),(#53808,
#53809),(#53810,#53811),(#53812,#53813),(#53814,#53815),(#53816,#53817),
(#53818,#53819),(#53820,#53821),(#53822,#53823),(#53824,#53825),(#53826,
#53827),(#53828,#53829),(#53830,#53831),(#53832,#53833),(#53834,#53835),
(#53836,#53837),(#53838,#53839),(#53840,#53841),(#53842,#53843),(#53844,
#53845),(#53846,#53847),(#53848,#53849),(#53850,#53851),(#53852,#53853),
(#53854,#53855),(#53856,#53857),(#53858,#53859),(#53860,#53861),(#53862,
#53863),(#53864,#53865),(#53866,#53867),(#53868,#53869),(#53870,#53871),
(#53872,#53873),(#53874,#53875),(#53876,#53877),(#53878,#53879),(#53880,
#53881),(#53882,#53883),(#53884,#53885),(#53886,#53887),(#53888,#53889),
(#53890,#53891),(#53892,#53893),(#53894,#53895),(#53896,#53897),(#53898,
#53899),(#53900,#53901),(#53902,#53903),(#53904,#53905),(#53906,#53907),
(#53908,#53909),(#53910,#53911),(#53912,#53913),(#53914,#53915),(#53916,
#53917),(#53918,#53919),(#53920,#53921),(#53922,#53923),(#53924,#53925),
(#53926,#53927),(#53928,#53929),(#53930,#53931),(#53932,#53933),(#53934,
#53935),(#53936,#53937),(#53938,#53939),(#53940,#53941),(#53942,#53943),
(#53944,#53945),(#53946,#53947),(#53948,#53949),(#53950,#53951),(#53952,
#53953),(#53954,#53955),(#53956,#53957),(#53958,#53959),(#53960,#53961),
(#53962,#53963),(#53964,#53965),(#53966,#53967),(#53968,#53969),(#53970,
#53971),(#53972,#53973),(#53974,#53975),(#53976,#53977),(#53978,#53979),
(#53980,#53981),(#53982,#53983),(#53984,#53985),(#53986,#53987),(#53988,
#53989),(#53990,#53991),(#53992,#53993),(#53994,#53995),(#53996,#53997),
(#53998,#53999),(#54000,#54001),(#54002,#54003),(#54004,#54005),(#54006,
#54007),(#54008,#54009),(#54010,#54011),(#54012,#54013),(#54014,#54015),
(#54016,#54017),(#54018,#54019),(#54020,#54021),(#54022,#54023),(#54024,
#54025),(#54026,#54027),(#54028,#54029),(#54030,#54031),(#54032,#54033),
(#54034,#54035),(#54036,#54037),(#54038,#54039),(#54040,#54041),(#54042,
#54043),(#54044,#54045),(#54046,#54047),(#54048,#54049),(#54050,#54051),
(#54052,#54053),(#54054,#54055),(#54056,#54057),(#54058,#54059),(#54060,
#54061),(#54062,#54063),(#54064,#54065),(#54066,#54067),(#54068,#54069),
(#54070,#54071),(#54072,#54073),(#54074,#54075),(#54076,#54077),(#54078,
#54079),(#54080,#54081),(#54082,#54083),(#54084,#54085),(#54086,#54087),
(#54088,#54089),(#54090,#54091),(#54092,#54093),(#54094,#54095),(#54096,
#54097),(#54098,#54099),(#54100,#54101),(#54102,#54103),(#54104,#54105),
(#54106,#54107),(#54108,#54109),(#54110,#54111),(#54112,#54113),(#54114,
#54115),(#54116,#54117),(#54118,#54119),(#54120,#54121),(#54122,#54123),
(#54124,#54125),(#54126,#54127),(#54128,#54129),(#54130,#54131),(#54132,
#54133),(#54134,#54135),(#54136,#54137),(#54138,#54139),(#54140,#54141),
(#54142,#54143),(#54144,#54145),(#54146,#54147),(#54148,#54149),(#54150,
#54151),(#54152,#54153),(#54154,#54155),(#54156,#54157),(#54158,#54159),
(#54160,#54161),(#54162,#54163),(#54164,#54165),(#54166,#54167),(#54168,
#54169),(#54170,#54171),(#54172,#54173),(#54174,#54175),(#54176,#54177),
(#54178,#54179),(#54180,#54181),(#54182,#54183),(#54184,#54185),(#54186,
#54187),(#54188,#54189),(#54190,#54191),(#54192,#54193),(#54194,#54195),
(#54196,#54197),(#54198,#54199),(#54200,#54201),(#54202,#54203),(#54204,
#54205),(#54206,#54207),(#54208,#54209),(#54210,#54211),(#54212,#54213),
(#54214,#54215),(#54216,#54217),(#54218,#54219),(#54220,#54221),(#54222,
#54223),(#54224,#54225),(#54226,#54227),(#54228,#54229),(#54230,#54231),
(#54232,#54233),(#54234,#54235),(#54236,#54237),(#54238,#54239),(#54240,
#54241),(#54242,#54243),(#54244,#54245),(#54246,#54247),(#54248,#54249),
(#54250,#54251),(#54252,#54253),(#54254,#54255),(#54256,#54257),(#54258,
#54259),(#54260,#54261),(#54262,#54263),(#54264,#54265),(#54266,#54267),
(#54268,#54269),(#54270,#54271),(#54272,#54273),(#54274,#54275),(#54276,
#54277),(#54278,#54279),(#54280,#54281),(#54282,#54283),(#54284,#54285),
(#54286,#54287),(#54288,#54289),(#54290,#54291),(#54292,#54293),(#54294,
#54295),(#54296,#54297),(#54298,#54299),(#54300,#54301),(#54302,#54303),
(#54304,#54305),(#54306,#54307),(#54308,#54309),(#54310,#54311),(#54312,
#54313),(#54314,#54315),(#54316,#54317),(#54318,#54319),(#54320,#54321),
(#54322,#54323),(#54324,#54325),(#54326,#54327),(#54328,#54329),(#54330,
#54331),(#54332,#54333),(#54334,#54335),(#54336,#54337),(#54338,#54339),
(#54340,#54341),(#54342,#54343),(#54344,#54345),(#54346,#54347),(#54348,
#54349),(#54350,#54351),(#54352,#54353),(#54354,#54355),(#54356,#54357),
(#54358,#54359),(#54360,#54361),(#54362,#54363),(#54364,#54365),(#54366,
#54367),(#54368,#54369),(#54370,#54371),(#54372,#54373),(#54374,#54375),
(#54376,#54377),(#54378,#54379),(#54380,#54381),(#54382,#54383),(#54384,
#54385),(#54386,#54387),(#54388,#54389),(#54390,#54391),(#54392,#54393),
(#54394,#54395),(#54396,#54397),(#54398,#54399),(#54400,#54401),(#54402,
#54403),(#54404,#54405),(#54406,#54407),(#54408,#54409),(#54410,#54411),
(#54412,#54413),(#54414,#54415),(#54416,#54417),(#54418,#54419),(#54420,
#54421),(#54422,#54423),(#54424,#54425),(#54426,#54427),(#54428,#54429),
(#54430,#54431),(#54432,#54433),(#54434,#54435),(#54436,#54437),(#54438,
#54439),(#54440,#54441),(#54442,#54443),(#54444,#54445),(#54446,#54447),
(#54448,#54449),(#54450,#54451),(#54452,#54453),(#54454,#54455),(#54456,
#54457),(#54458,#54459),(#54460,#54461),(#54462,#54463),(#54464,#54465),
(#54466,#54467),(#54468,#54469),(#54470,#54471),(#54472,#54473),(#54474,
#54475),(#54476,#54477),(#54478,#54479),(#54480,#54481),(#54482,#54483),
(#54484,#54485),(#54486,#54487),(#54488,#54489),(#54490,#54491),(#54492,
#54493),(#54494,#54495),(#54496,#54497),(#54498,#54499),(#54500,#54501),
(#54502,#54503),(#54504,#54505),(#54506,#54507),(#54508,#54509),(#54510,
#54511),(#54512,#54513),(#54514,#54515),(#54516,#54517),(#54518,#54519),
(#54520,#54521),(#54522,#54523),(#54524,#54525),(#54526,#54527),(#54528,
#54529),(#54530,#54531),(#54532,#54533),(#54534,#54535),(#54536,#54537),
(#54538,#54539),(#54540,#54541),(#54542,#54543),(#54544,#54545),(#54546,
#54547),(#54548,#54549),(#54550,#54551),(#54552,#54553),(#54554,#54555),
(#54556,#54557),(#54558,#54559),(#54560,#54561),(#54562,#54563),(#54564,
#54565),(#54566,#54567),(#54568,#54569),(#54570,#54571),(#54572,#54573),
(#54574,#54575),(#54576,#54577),(#54578,#54579),(#54580,#54581),(#54582,
#54583),(#54584,#54585),(#54586,#54587),(#54588,#54589),(#54590,#54591),
(#54592,#54593),(#54594,#54595),(#54596,#54597),(#54598,#54599),(#54600,
#54601),(#54602,#54603),(#54604,#54605),(#54606,#54607),(#54608,#54609),
(#54610,#54611),(#54612,#54613),(#54614,#54615),(#54616,#54617),(#54618,
#54619),(#54620,#54621),(#54622,#54623),(#54624,#54625),(#54626,#54627),
(#54628,#54629),(#54630,#54631),(#54632,#54633),(#54634,#54635),(#54636,
#54637),(#54638,#54639),(#54640,#54641),(#54642,#54643),(#54644,#54645),
(#54646,#54647),(#54648,#54649),(#54650,#54651),(#54652,#54653),(#54654,
#54655),(#54656,#54657),(#54658,#54659),(#54660,#54661),(#54662,#54663),
(#54664,#54665),(#54666,#54667),(#54668,#54669),(#54670,#54671),(#54672,
#54673),(#54674,#54675),(#54676,#54677),(#54678,#54679),(#54680,#54681),
(#54682,#54683),(#54684,#54685),(#54686,#54687),(#54688,#54689),(#54690,
#54691),(#54692,#54693),(#54694,#54695),(#54696,#54697),(#54698,#54699),
(#54700,#54701),(#54702,#54703),(#54704,#54705),(#54706,#54707),(#54708,
#54709),(#54710,#54711),(#54712,#54713),(#54714,#54715),(#54716,#54717),
(#54718,#54719),(#54720,#54721),(#54722,#54723),(#54724,#54725),(#54726,
#54727),(#54728,#54729),(#54730,#54731),(#54732,#54733),(#54734,#54735),
(#54736,#54737),(#54738,#54739),(#54740,#54741),(#54742,#54743),(#54744,
#54745),(#54746,#54747),(#54748,#54749),(#54750,#54751),(#54752,#54753),
(#54754,#54755),(#54756,#54757),(#54758,#54759),(#54760,#54761),(#54762,
#54763),(#54764,#54765),(#54766,#54767),(#54768,#54769),(#54770,#54771),
(#54772,#54773),(#54774,#54775),(#54776,#54777),(#54778,#54779),(#54780,
#54781),(#54782,#54783),(#54784,#54785),(#54786,#54787),(#54788,#54789),
(#54790,#54791),(#54792,#54793),(#54794,#54795),(#54796,#54797),(#54798,
#54799),(#54800,#54801),(#54802,#54803),(#54804,#54805),(#54806,#54807),
(#54808,#54809),(#54810,#54811),(#54812,#54813),(#54814,#54815),(#54816,
#54817),(#54818,#54819),(#54820,#54821),(#54822,#54823),(#54824,#54825),
(#54826,#54827),(#54828,#54829),(#54830,#54831),(#54832,#54833),(#54834,
#54835),(#54836,#54837),(#54838,#54839),(#54840,#54841),(#54842,#54843),
(#54844,#54845),(#54846,#54847),(#54848,#54849),(#54850,#54851),(#54852,
#54853),(#54854,#54855),(#54856,#54857),(#54858,#54859),(#54860,#54861),
(#54862,#54863),(#54864,#54865),(#54866,#54867),(#54868,#54869),(#54870,
#54871),(#54872,#54873),(#54874,#54875),(#54876,#54877),(#54878,#54879),
(#54880,#54881),(#54882,#54883),(#54884,#54885),(#54886,#54887),(#54888,
#54889),(#54890,#54891),(#54892,#54893),(#54894,#54895),(#54896,#54897),
(#54898,#54899),(#54900,#54901),(#54902,#54903),(#54904,#54905),(#54906,
#54907),(#54908,#54909),(#54910,#54911),(#54912,#54913),(#54914,#54915),
(#54916,#54917),(#54918,#54919),(#54920,#54921),(#54922,#54923),(#54924,
#54925),(#54926,#54927),(#54928,#54929),(#54930,#54931),(#54932,#54933),
(#54934,#54935),(#54936,#54937),(#54938,#54939),(#54940,#54941),(#54942,
#54943),(#54944,#54945),(#54946,#54947),(#54948,#54949),(#54950,#54951),
(#54952,#54953),(#54954,#54955),(#54956,#54957),(#54958,#54959),(#54960,
#54961),(#54962,#54963),(#54964,#54965),(#54966,#54967),(#54968,#54969),
(#54970,#54971),(#54972,#54973),(#54974,#54975),(#54976,#54977),(#54978,
#54979),(#54980,#54981),(#54982,#54983),(#54984,#54985),(#54986,#54987),
(#54988,#54989),(#54990,#54991),(#54992,#54993),(#54994,#54995),(#54996,
#54997),(#54998,#54999),(#55000,#55001),(#55002,#55003),(#55004,#55005),
(#55006,#55007),(#55008,#55009),(#55010,#55011),(#55012,#55013),(#55014,
#55015),(#55016,#55017),(#55018,#55019),(#55020,#55021),(#55022,#55023),
(#55024,#55025),(#55026,#55027),(#55028,#55029),(#55030,#55031),(#55032,
#55033),(#55034,#55035),(#55036,#55037),(#55038,#55039),(#55040,#55041),
(#55042,#55043),(#55044,#55045),(#55046,#55047),(#55048,#55049),(#55050,
#55051),(#55052,#55053),(#55054,#55055),(#55056,#55057),(#55058,#55059),
(#55060,#55061),(#55062,#55063),(#55064,#55065),(#55066,#55067),(#55068,
#55069),(#55070,#55071),(#55072,#55073),(#55074,#55075),(#55076,#55077),
(#55078,#55079),(#55080,#55081),(#55082,#55083),(#55084,#55085),(#55086,
#55087),(#55088,#55089),(#55090,#55091),(#55092,#55093),(#55094,#55095),
(#55096,#55097),(#55098,#55099),(#55100,#55101),(#55102,#55103),(#55104,
#55105),(#55106,#55107),(#55108,#55109),(#55110,#55111),(#55112,#55113),
(#55114,#55115),(#55116,#55117),(#55118,#55119),(#55120,#55121),(#55122,
#55123),(#55124,#55125),(#55126,#55127),(#55128,#55129),(#55130,#55131),
(#55132,#55133),(#55134,#55135),(#55136,#55137),(#55138,#55139),(#55140,
#55141),(#55142,#55143),(#55144,#55145),(#55146,#55147),(#55148,#55149),
(#55150,#55151),(#55152,#55153),(#55154,#55155),(#55156,#55157),(#55158,
#55159),(#55160,#55161),(#55162,#55163),(#55164,#55165),(#55166,#55167),
(#55168,#55169),(#55170,#55171),(#55172,#55173),(#55174,#55175),(#55176,
#55177),(#55178,#55179),(#55180,#55181),(#55182,#55183),(#55184,#55185),
(#55186,#55187),(#55188,#55189),(#55190,#55191),(#55192,#55193),(#55194,
#55195),(#55196,#55197),(#55198,#55199),(#55200,#55201),(#55202,#55203),
(#55204,#55205),(#55206,#55207),(#55208,#55209),(#55210,#55211),(#55212,
#55213),(#55214,#55215),(#55216,#55217),(#55218,#55219),(#55220,#55221),
(#55222,#55223),(#55224,#55225),(#55226,#55227),(#55228,#55229),(#55230,
#55231),(#55232,#55233),(#55234,#55235),(#55236,#55237),(#55238,#55239),
(#55240,#55241),(#55242,#55243),(#55244,#55245),(#55246,#55247),(#55248,
#55249),(#55250,#55251),(#55252,#55253),(#55254,#55255),(#55256,#55257),
(#55258,#55259),(#55260,#55261),(#55262,#55263),(#55264,#55265),(#55266,
#55267),(#55268,#55269),(#55270,#55271),(#55272,#55273),(#55274,#55275),
(#55276,#55277),(#55278,#55279),(#55280,#55281),(#55282,#55283),(#55284,
#55285),(#55286,#55287),(#55288,#55289),(#55290,#55291),(#55292,#55293),
(#55294,#55295),(#55296,#55297),(#55298,#55299),(#55300,#55301),(#55302,
#55303),(#55304,#55305),(#55306,#55307),(#55308,#55309),(#55310,#55311),
(#55312,#55313),(#55314,#55315),(#55316,#55317),(#55318,#55319),(#55320,
#55321),(#55322,#55323),(#55324,#55325),(#55326,#55327),(#55328,#55329),
(#55330,#55331),(#55332,#55333),(#55334,#55335),(#55336,#55337),(#55338,
#55339),(#55340,#55341),(#55342,#55343),(#55344,#55345),(#55346,#55347),
(#55348,#55349),(#55350,#55351),(#55352,#55353),(#55354,#55355),(#55356,
#55357),(#55358,#55359),(#55360,#55361),(#55362,#55363),(#55364,#55365),
(#55366,#55367),(#55368,#55369),(#55370,#55371),(#55372,#55373),(#55374,
#55375),(#55376,#55377),(#55378,#55379),(#55380,#55381),(#55382,#55383),
(#55384,#55385),(#55386,#55387),(#55388,#55389),(#55390,#55391),(#55392,
#55393),(#55394,#55395),(#55396,#55397),(#55398,#55399),(#55400,#55401),
(#55402,#55403),(#55404,#55405),(#55406,#55407),(#55408,#55409),(#55410,
#55411),(#55412,#55413),(#55414,#55415),(#55416,#55417),(#55418,#55419),
(#55420,#55421),(#55422,#55423),(#55424,#55425),(#55426,#55427),(#55428,
#55429),(#55430,#55431),(#55432,#55433),(#55434,#55435),(#55436,#55437),
(#55438,#55439),(#55440,#55441),(#55442,#55443),(#55444,#55445),(#55446,
#55447),(#55448,#55449),(#55450,#55451),(#55452,#55453),(#55454,#55455),
(#55456,#55457),(#55458,#55459),(#55460,#55461),(#55462,#55463),(#55464,
#55465),(#55466,#55467),(#55468,#55469),(#55470,#55471),(#55472,#55473),
(#55474,#55475),(#55476,#55477),(#55478,#55479),(#55480,#55481),(#55482,
#55483),(#55484,#55485),(#55486,#55487),(#55488,#55489),(#55490,#55491),
(#55492,#55493),(#55494,#55495),(#55496,#55497),(#55498,#55499),(#55500,
#55501),(#55502,#55503),(#55504,#55505),(#55506,#55507),(#55508,#55509),
(#55510,#55511),(#55512,#55513),(#55514,#55515),(#55516,#55517),(#55518,
#55519),(#55520,#55521),(#55522,#55523),(#55524,#55525),(#55526,#55527),
(#55528,#55529),(#55530,#55531),(#55532,#55533),(#55534,#55535),(#55536,
#55537),(#55538,#55539),(#55540,#55541),(#55542,#55543),(#55544,#55545),
(#55546,#55547),(#55548,#55549),(#55550,#55551),(#55552,#55553),(#55554,
#55555),(#55556,#55557),(#55558,#55559),(#55560,#55561),(#55562,#55563),
(#55564,#55565),(#55566,#55567),(#55568,#55569),(#55570,#55571),(#55572,
#55573),(#55574,#55575),(#55576,#55577),(#55578,#55579),(#55580,#55581),
(#55582,#55583),(#55584,#55585),(#55586,#55587),(#55588,#55589),(#55590,
#55591),(#55592,#55593),(#55594,#55595),(#55596,#55597),(#55598,#55599),
(#55600,#55601),(#55602,#55603),(#55604,#55605),(#55606,#55607),(#55608,
#55609),(#55610,#55611),(#55612,#55613),(#55614,#55615),(#55616,#55617),
(#55618,#55619),(#55620,#55621),(#55622,#55623),(#55624,#55625),(#55626,
#55627),(#55628,#55629),(#55630,#55631),(#55632,#55633),(#55634,#55635),
(#55636,#55637),(#55638,#55639),(#55640,#55641),(#55642,#55643),(#55644,
#55645),(#55646,#55647),(#55648,#55649),(#55650,#55651),(#55652,#55653),
(#55654,#55655),(#55656,#55657),(#55658,#55659),(#55660,#55661),(#55662,
#55663),(#55664,#55665),(#55666,#55667),(#55668,#55669),(#55670,#55671),
(#55672,#55673),(#55674,#55675),(#55676,#55677),(#55678,#55679),(#55680,
#55681),(#55682,#55683),(#55684,#55685),(#55686,#55687),(#55688,#55689),
(#55690,#55691),(#55692,#55693),(#55694,#55695),(#55696,#55697),(#55698,
#55699),(#55700,#55701),(#55702,#55703),(#55704,#55705),(#55706,#55707),
(#55708,#55709),(#55710,#55711),(#55712,#55713),(#55714,#55715),(#55716,
#55717),(#55718,#55719),(#55720,#55721),(#55722,#55723),(#55724,#55725),
(#55726,#55727),(#55728,#55729),(#55730,#55731),(#55732,#55733),(#55734,
#55735),(#55736,#55737),(#55738,#55739),(#55740,#55741),(#55742,#55743),
(#55744,#55745),(#55746,#55747),(#55748,#55749),(#55750,#55751),(#55752,
#55753),(#55754,#55755),(#55756,#55757),(#55758,#55759),(#55760,#55761),
(#55762,#55763),(#55764,#55765),(#55766,#55767),(#55768,#55769),(#55770,
#55771),(#55772,#55773),(#55774,#55775),(#55776,#55777),(#55778,#55779),
(#55780,#55781),(#55782,#55783),(#55784,#55785),(#55786,#55787),(#55788,
#55789),(#55790,#55791),(#55792,#55793),(#55794,#55795),(#55796,#55797),
(#55798,#55799),(#55800,#55801),(#55802,#55803),(#55804,#55805),(#55806,
#55807),(#55808,#55809),(#55810,#55811),(#55812,#55813),(#55814,#55815),
(#55816,#55817),(#55818,#55819),(#55820,#55821),(#55822,#55823),(#55824,
#55825),(#55826,#55827),(#55828,#55829),(#55830,#55831),(#55832,#55833),
(#55834,#55835),(#55836,#55837),(#55838,#55839),(#55840,#55841),(#55842,
#55843),(#55844,#55845),(#55846,#55847),(#55848,#55849),(#55850,#55851),
(#55852,#55853),(#55854,#55855),(#55856,#55857),(#55858,#55859),(#55860,
#55861),(#55862,#55863),(#55864,#55865),(#55866,#55867),(#55868,#55869),
(#55870,#55871),(#55872,#55873),(#55874,#55875),(#55876,#55877),(#55878,
#55879),(#55880,#55881),(#55882,#55883),(#55884,#55885),(#55886,#55887),
(#55888,#55889),(#55890,#55891),(#55892,#55893),(#55894,#55895),(#55896,
#55897),(#55898,#55899),(#55900,#55901),(#55902,#55903),(#55904,#55905),
(#55906,#55907),(#55908,#55909),(#55910,#55911),(#55912,#55913),(#55914,
#55915),(#55916,#55917),(#55918,#55919),(#55920,#55921),(#55922,#55923),
(#55924,#55925),(#55926,#55927),(#55928,#55929),(#55930,#55931),(#55932,
#55933),(#55934,#55935),(#55936,#55937),(#55938,#55939),(#55940,#55941),
(#55942,#55943),(#55944,#55945),(#55946,#55947),(#55948,#55949),(#55950,
#55951),(#55952,#55953),(#55954,#55955),(#55956,#55957),(#55958,#55959),
(#55960,#55961),(#55962,#55963),(#55964,#55965),(#55966,#55967),(#55968,
#55969),(#55970,#55971),(#55972,#55973),(#55974,#55975),(#55976,#55977),
(#55978,#55979),(#55980,#55981),(#55982,#55983),(#55984,#55985),(#55986,
#55987),(#55988,#55989),(#55990,#55991),(#55992,#55993),(#55994,#55995),
(#55996,#55997),(#55998,#55999),(#56000,#56001),(#56002,#56003),(#56004,
#56005),(#56006,#56007),(#56008,#56009),(#56010,#56011),(#56012,#56013),
(#56014,#56015),(#56016,#56017),(#56018,#56019),(#56020,#56021),(#56022,
#56023),(#56024,#56025),(#56026,#56027),(#56028,#56029),(#56030,#56031),
(#56032,#56033),(#56034,#56035),(#56036,#56037),(#56038,#56039),(#56040,
#56041),(#56042,#56043),(#56044,#56045),(#56046,#56047),(#56048,#56049),
(#56050,#56051),(#56052,#56053),(#56054,#56055),(#56056,#56057),(#56058,
#56059),(#56060,#56061),(#56062,#56063),(#56064,#56065),(#56066,#56067),
(#56068,#56069),(#56070,#56071),(#56072,#56073),(#56074,#56075),(#56076,
#56077),(#56078,#56079),(#56080,#56081),(#56082,#56083),(#56084,#56085),
(#56086,#56087),(#56088,#56089),(#56090,#56091),(#56092,#56093),(#56094,
#56095),(#56096,#56097),(#56098,#56099),(#56100,#56101),(#56102,#56103),
(#56104,#56105),(#56106,#56107),(#56108,#56109),(#56110,#56111),(#56112,
#56113),(#56114,#56115),(#56116,#56117),(#56118,#56119),(#56120,#56121),
(#56122,#56123),(#56124,#56125),(#56126,#56127),(#56128,#56129),(#56130,
#56131),(#56132,#56133),(#56134,#56135),(#56136,#56137),(#56138,#56139),
(#56140,#56141),(#56142,#56143),(#56144,#56145),(#56146,#56147),(#56148,
#56149),(#56150,#56151),(#56152,#56153),(#56154,#56155),(#56156,#56157),
(#56158,#56159),(#56160,#56161),(#56162,#56163),(#56164,#56165),(#56166,
#56167),(#56168,#56169),(#56170,#56171),(#56172,#56173),(#56174,#56175),
(#56176,#56177),(#56178,#56179),(#56180,#56181),(#56182,#56183),(#56184,
#56185),(#56186,#56187),(#56188,#56189),(#56190,#56191),(#56192,#56193),
(#56194,#56195),(#56196,#56197),(#56198,#56199),(#56200,#56201),(#56202,
#56203),(#56204,#56205),(#56206,#56207),(#56208,#56209),(#56210,#56211),
(#56212,#56213),(#56214,#56215),(#56216,#56217),(#56218,#56219),(#56220,
#56221),(#56222,#56223),(#56224,#56225),(#56226,#56227),(#56228,#56229),
(#56230,#56231),(#56232,#56233),(#56234,#56235),(#56236,#56237),(#56238,
#56239),(#56240,#56241),(#56242,#56243),(#56244,#56245),(#56246,#56247),
(#56248,#56249),(#56250,#56251),(#56252,#56253),(#56254,#56255),(#56256,
#56257),(#56258,#56259),(#56260,#56261),(#56262,#56263),(#56264,#56265),
(#56266,#56267),(#56268,#56269),(#56270,#56271),(#56272,#56273),(#56274,
#56275),(#56276,#56277),(#56278,#56279),(#56280,#56281),(#56282,#56283),
(#56284,#56285),(#56286,#56287),(#56288,#56289),(#56290,#56291),(#56292,
#56293),(#56294,#56295),(#56296,#56297),(#56298,#56299),(#56300,#56301),
(#56302,#56303),(#56304,#56305),(#56306,#56307),(#56308,#56309),(#56310,
#56311),(#56312,#56313),(#56314,#56315),(#56316,#56317),(#56318,#56319),
(#56320,#56321),(#56322,#56323),(#56324,#56325),(#56326,#56327),(#56328,
#56329),(#56330,#56331),(#56332,#56333),(#56334,#56335),(#56336,#56337),
(#56338,#56339),(#56340,#56341),(#56342,#56343),(#56344,#56345),(#56346,
#56347),(#56348,#56349),(#56350,#56351),(#56352,#56353),(#56354,#56355),
(#56356,#56357),(#56358,#56359),(#56360,#56361),(#56362,#56363),(#56364,
#56365),(#56366,#56367),(#56368,#56369),(#56370,#56371),(#56372,#56373),
(#56374,#56375),(#56376,#56377),(#56378,#56379),(#56380,#56381),(#56382,
#56383),(#56384,#56385),(#56386,#56387),(#56388,#56389),(#56390,#56391),
(#56392,#56393),(#56394,#56395),(#56396,#56397),(#56398,#56399),(#56400,
#56401),(#56402,#56403),(#56404,#56405),(#56406,#56407),(#56408,#56409),
(#56410,#56411),(#56412,#56413),(#56414,#56415),(#56416,#56417),(#56418,
#56419),(#56420,#56421),(#56422,#56423),(#56424,#56425),(#56426,#56427),
(#56428,#56429),(#56430,#56431),(#56432,#56433),(#56434,#56435),(#56436,
#56437),(#56438,#56439),(#56440,#56441),(#56442,#56443),(#56444,#56445),
(#56446,#56447),(#56448,#56449),(#56450,#56451),(#56452,#56453),(#56454,
#56455),(#56456,#56457),(#56458,#56459),(#56460,#56461),(#56462,#56463),
(#56464,#56465),(#56466,#56467),(#56468,#56469),(#56470,#56471),(#56472,
#56473),(#56474,#56475),(#56476,#56477),(#56478,#56479),(#56480,#56481),
(#56482,#56483),(#56484,#56485),(#56486,#56487),(#56488,#56489),(#56490,
#56491),(#56492,#56493),(#56494,#56495),(#56496,#56497),(#56498,#56499),
(#56500,#56501),(#56502,#56503),(#56504,#56505),(#56506,#56507),(#56508,
#56509),(#56510,#56511),(#56512,#56513),(#56514,#56515),(#56516,#56517),
(#56518,#56519),(#56520,#56521),(#56522,#56523),(#56524,#56525),(#56526,
#56527),(#56528,#56529),(#56530,#56531),(#56532,#56533),(#56534,#56535),
(#56536,#56537),(#56538,#56539),(#56540,#56541),(#56542,#56543),(#56544,
#56545),(#56546,#56547),(#56548,#56549),(#56550,#56551),(#56552,#56553),
(#56554,#56555),(#56556,#56557),(#56558,#56559),(#56560,#56561),(#56562,
#56563),(#56564,#56565),(#56566,#56567),(#56568,#56569),(#56570,#56571),
(#56572,#56573),(#56574,#56575),(#56576,#56577),(#56578,#56579),(#56580,
#56581),(#56582,#56583),(#56584,#56585),(#56586,#56587),(#56588,#56589),
(#56590,#56591),(#56592,#56593),(#56594,#56595),(#56596,#56597),(#56598,
#56599),(#56600,#56601),(#56602,#56603),(#56604,#56605),(#56606,#56607),
(#56608,#56609),(#56610,#56611),(#56612,#56613),(#56614,#56615),(#56616,
#56617),(#56618,#56619),(#56620,#56621),(#56622,#56623),(#56624,#56625),
(#56626,#56627),(#56628,#56629),(#56630,#56631),(#56632,#56633),(#56634,
#56635),(#56636,#56637),(#56638,#56639),(#56640,#56641),(#56642,#56643),
(#56644,#56645),(#56646,#56647),(#56648,#56649),(#56650,#56651),(#56652,
#56653),(#56654,#56655),(#56656,#56657),(#56658,#56659),(#56660,#56661),
(#56662,#56663),(#56664,#56665),(#56666,#56667),(#56668,#56669),(#56670,
#56671),(#56672,#56673),(#56674,#56675),(#56676,#56677),(#56678,#56679),
(#56680,#56681),(#56682,#56683),(#56684,#56685),(#56686,#56687),(#56688,
#56689),(#56690,#56691),(#56692,#56693),(#56694,#56695),(#56696,#56697),
(#56698,#56699),(#56700,#56701),(#56702,#56703),(#56704,#56705),(#56706,
#56707),(#56708,#56709),(#56710,#56711),(#56712,#56713),(#56714,#56715),
(#56716,#56717),(#56718,#56719),(#56720,#56721),(#56722,#56723),(#56724,
#56725),(#56726,#56727),(#56728,#56729),(#56730,#56731),(#56732,#56733),
(#56734,#56735),(#56736,#56737),(#56738,#56739),(#56740,#56741),(#56742,
#56743),(#56744,#56745),(#56746,#56747),(#56748,#56749),(#56750,#56751),
(#56752,#56753),(#56754,#56755),(#56756,#56757),(#56758,#56759),(#56760,
#56761),(#56762,#56763),(#56764,#56765),(#56766,#56767),(#56768,#56769),
(#56770,#56771),(#56772,#56773),(#56774,#56775),(#56776,#56777),(#56778,
#56779),(#56780,#56781),(#56782,#56783),(#56784,#56785),(#56786,#56787),
(#56788,#56789),(#56790,#56791),(#56792,#56793),(#56794,#56795),(#56796,
#56797),(#56798,#56799),(#56800,#56801),(#56802,#56803),(#56804,#56805),
(#56806,#56807),(#56808,#56809),(#56810,#56811),(#56812,#56813),(#56814,
#56815),(#56816,#56817),(#56818,#56819),(#56820,#56821),(#56822,#56823),
(#56824,#56825),(#56826,#56827),(#56828,#56829),(#56830,#56831),(#56832,
#56833),(#56834,#56835),(#56836,#56837),(#56838,#56839),(#56840,#56841),
(#56842,#56843),(#56844,#56845),(#56846,#56847),(#56848,#56849),(#56850,
#56851),(#56852,#56853),(#56854,#56855),(#56856,#56857),(#56858,#56859),
(#56860,#56861),(#56862,#56863),(#56864,#56865),(#56866,#56867),(#56868,
#56869),(#56870,#56871),(#56872,#56873),(#56874,#56875),(#56876,#56877),
(#56878,#56879),(#56880,#56881),(#56882,#56883),(#56884,#56885),(#56886,
#56887),(#56888,#56889),(#56890,#56891),(#56892,#56893),(#56894,#56895),
(#56896,#56897),(#56898,#56899),(#56900,#56901),(#56902,#56903),(#56904,
#56905),(#56906,#56907),(#56908,#56909),(#56910,#56911),(#56912,#56913),
(#56914,#56915),(#56916,#56917),(#56918,#56919),(#56920,#56921),(#56922,
#56923),(#56924,#56925),(#56926,#56927),(#56928,#56929),(#56930,#56931),
(#56932,#56933),(#56934,#56935),(#56936,#56937),(#56938,#56939),(#56940,
#56941),(#56942,#56943),(#56944,#56945),(#56946,#56947),(#56948,#56949),
(#56950,#56951),(#56952,#56953),(#56954,#56955),(#56956,#56957),(#56958,
#56959),(#56960,#56961),(#56962,#56963),(#56964,#56965),(#56966,#56967),
(#56968,#56969),(#56970,#56971),(#56972,#56973),(#56974,#56975),(#56976,
#56977),(#56978,#56979),(#56980,#56981),(#56982,#56983),(#56984,#56985),
(#56986,#56987),(#56988,#56989),(#56990,#56991),(#56992,#56993),(#56994,
#56995),(#56996,#56997),(#56998,#56999),(#57000,#57001),(#57002,#57003),
(#57004,#57005),(#57006,#57007),(#57008,#57009),(#57010,#57011),(#57012,
#57013),(#57014,#57015),(#57016,#57017),(#57018,#57019),(#57020,#57021),
(#57022,#57023),(#57024,#57025),(#57026,#57027),(#57028,#57029),(#57030,
#57031),(#57032,#57033),(#57034,#57035),(#57036,#57037),(#57038,#57039),
(#57040,#57041),(#57042,#57043),(#57044,#57045),(#57046,#57047),(#57048,
#57049),(#57050,#57051),(#57052,#57053),(#57054,#57055),(#57056,#57057),
(#57058,#57059),(#57060,#57061),(#57062,#57063),(#57064,#57065),(#57066,
#57067),(#57068,#57069),(#57070,#57071),(#57072,#57073),(#57074,#57075),
(#57076,#57077),(#57078,#57079),(#57080,#57081),(#57082,#57083),(#57084,
#57085),(#57086,#57087),(#57088,#57089),(#57090,#57091),(#57092,#57093),
(#57094,#57095),(#57096,#57097),(#57098,#57099),(#57100,#57101),(#57102,
#57103),(#57104,#57105),(#57106,#57107),(#57108,#57109),(#57110,#57111),
(#57112,#57113),(#57114,#57115),(#57116,#57117),(#57118,#57119),(#57120,
#57121),(#57122,#57123),(#57124,#57125),(#57126,#57127),(#57128,#57129),
(#57130,#57131),(#57132,#57133),(#57134,#57135),(#57136,#57137),(#57138,
#57139),(#57140,#57141),(#57142,#57143),(#57144,#57145),(#57146,#57147),
(#57148,#57149),(#57150,#57151),(#57152,#57153),(#57154,#57155),(#57156,
#57157),(#57158,#57159),(#57160,#57161),(#57162,#57163),(#57164,#57165),
(#57166,#57167),(#57168,#57169),(#57170,#57171),(#57172,#57173),(#57174,
#57175),(#57176,#57177),(#57178,#57179),(#57180,#57181),(#57182,#57183),
(#57184,#57185),(#57186,#57187),(#57188,#57189),(#57190,#57191),(#57192,
#57193),(#57194,#57195),(#57196,#57197),(#57198,#57199),(#57200,#57201),
(#57202,#57203),(#57204,#57205),(#57206,#57207),(#57208,#57209),(#57210,
#57211),(#57212,#57213),(#57214,#57215),(#57216,#57217),(#57218,#57219),
(#57220,#57221),(#57222,#57223),(#57224,#57225),(#57226,#57227),(#57228,
#57229),(#57230,#57231),(#57232,#57233),(#57234,#57235),(#57236,#57237),
(#57238,#57239),(#57240,#57241),(#57242,#57243),(#57244,#57245),(#57246,
#57247),(#57248,#57249),(#57250,#57251),(#57252,#57253),(#57254,#57255),
(#57256,#57257),(#57258,#57259),(#57260,#57261),(#57262,#57263),(#57264,
#57265),(#57266,#57267),(#57268,#57269),(#57270,#57271),(#57272,#57273)),
 .UNSPECIFIED.,.F.,.F.,.F.,(4,1,1,1,1,1,1,1,1,1,1,1,1,1,1,1,1,1,1,1,1,1,
1,1,1,1,1,1,1,1,1,1,1,1,1,1,1,1,1,1,1,1,1,1,1,1,1,1,1,1,1,1,1,1,1,1,1,1,
1,1,1,1,1,1,1,1,1,1,1,1,1,1,1,1,1,1,1,1,1,1,1,1,1,1,1,1,1,1,1,1,1,1,1,1,
1,1,1,1,1,1,1,1,1,1,1,1,1,1,1,1,1,1,1,1,1,1,1,1,1,1,1,1,1,1,1,1,1,1,1,1,
1,1,1,1,1,1,1,1,1,1,1,1,1,1,1,1,1,1,1,1,1,1,1,1,1,1,1,1,1,1,1,1,1,1,1,1,
1,1,1,1,1,1,1,1,1,1,1,1,1,1,1,1,1,1,1,1,1,1,1,1,1,1,1,1,1,1,1,1,1,1,1,1,
1,1,1,1,1,1,1,1,1,1,1,1,1,1,1,1,1,1,1,1,1,1,1,1,1,1,1,1,1,1,1,1,1,1,1,1,
1,1,1,1,1,1,1,1,1,1,1,1,1,1,1,1,1,1,1,1,1,1,1,1,1,1,1,1,1,1,1,1,1,1,1,1,
1,1,1,1,1,1,1,1,1,1,1,1,1,1,1,1,1,1,1,1,1,1,1,1,1,1,1,1,1,1,1,1,1,1,1,1,
1,1,1,1,1,1,1,1,1,1,1,1,1,1,1,1,1,1,1,1,1,1,1,1,1,1,1,1,1,1,1,1,1,1,1,1,
1,1,1,1,1,1,1,1,1,1,1,1,1,1,1,1,1,1,1,1,1,1,1,1,1,1,1,1,1,1,1,1,1,1,1,1,
1,1,1,1,1,1,1,1,1,1,1,1,1,1,1,1,1,1,1,1,1,1,1,1,1,1,1,1,1,1,1,1,1,1,1,1,
1,1,1,1,1,1,1,1,1,1,1,1,1,1,1,1,1,1,1,1,1,1,1,1,1,1,1,1,1,1,1,1,1,1,1,1,
1,1,1,1,1,1,1,1,1,1,1,1,1,1,1,1,1,1,1,1,1,1,1,1,1,1,1,1,1,1,1,1,1,1,1,1,
1,1,1,1,1,1,1,1,1,1,1,1,1,1,1,1,1,1,1,1,1,1,1,1,1,1,1,1,1,1,1,1,1,1,1,1,
1,1,1,1,1,1,1,1,1,1,1,1,1,1,1,1,1,1,1,1,1,1,1,1,1,1,1,1,1,1,1,1,1,1,1,1,
1,1,1,1,1,1,1,1,1,1,1,1,1,1,1,1,1,1,1,1,1,1,1,1,1,1,1,1,1,1,1,1,1,1,1,1,
1,1,1,1,1,1,1,1,1,1,1,1,1,1,1,1,1,1,1,1,1,1,1,1,1,1,1,1,1,1,1,1,1,1,1,1,
1,1,1,1,1,1,1,1,1,1,1,1,1,1,1,1,1,1,1,1,1,1,1,1,1,1,1,1,1,1,1,1,1,1,1,1,
1,1,1,1,1,1,1,1,1,1,1,1,1,1,1,1,1,1,1,1,1,1,1,1,1,1,1,1,1,1,1,1,1,1,1,1,
1,1,1,1,1,1,1,1,1,1,1,1,1,1,1,1,1,1,1,1,1,1,1,1,1,1,1,1,1,1,1,1,1,1,1,1,
1,1,1,1,1,1,1,1,1,1,1,1,1,1,1,1,1,1,1,1,1,1,1,1,1,1,1,1,1,1,1,1,1,1,1,1,
1,1,1,1,1,1,1,1,1,1,1,1,1,1,1,1,1,1,1,1,1,1,1,1,1,1,1,1,1,1,1,1,1,1,1,1,
1,1,1,1,1,1,1,1,1,1,1,1,1,1,1,1,1,1,1,1,1,1,1,1,1,1,1,1,1,1,1,1,1,1,1,1,
1,1,1,1,1,1,1,1,1,1,1,1,1,1,1,1,1,1,1,1,1,1,1,1,1,1,1,1,1,1,1,1,1,1,1,1,
1,1,1,1,1,1,1,1,1,1,1,1,1,1,1,1,1,1,1,1,1,1,1,1,1,1,1,1,1,1,1,1,1,1,1,1,
1,1,1,1,1,1,1,1,1,1,1,1,1,1,1,1,1,1,1,1,1,1,1,1,1,1,1,1,1,1,1,1,1,1,1,1,
1,1,1,1,1,1,1,1,1,1,1,1,1,1,1,1,1,1,1,1,1,1,1,1,1,1,1,1,1,1,1,1,1,1,1,1,
1,1,1,1,1,1,1,1,1,1,1,1,1,1,1,1,1,1,1,1,1,1,1,1,1,1,1,1,1,1,1,1,1,1,1,1,
1,1,1,1,1,1,1,1,1,1,1,1,1,1,1,1,1,1,1,1,1,1,1,1,1,1,1,1,1,1,1,1,1,1,1,1,
1,1,1,1,1,1,1,1,1,1,1,1,1,1,1,1,1,1,1,1,1,1,1,1,1,1,1,1,1,1,1,1,1,1,1,1,
1,1,1,1,1,1,1,1,1,1,1,1,1,1,1,1,1,1,1,1,1,1,1,1,1,1,1,1,1,1,1,1,1,1,1,1,
1,1,1,1,1,1,1,1,1,1,1,1,1,1,1,1,1,1,1,1,1,1,1,1,1,1,1,1,1,1,1,1,1,1,1,1,
1,1,1,1,1,1,1,1,1,1,1,1,1,1,1,1,1,1,1,1,1,1,1,1,1,1,1,1,1,1,1,1,1,1,1,1,
1,1,1,1,1,1,1,1,1,1,1,1,1,1,1,1,1,1,1,1,1,1,1,1,1,1,1,1,1,1,1,1,1,1,1,1,
1,1,1,1,1,1,1,1,1,1,1,1,1,1,1,1,1,1,1,1,1,1,1,1,1,1,1,1,1,1,1,1,1,1,1,1,
1,1,1,1,1,1,1,1,1,1,1,1,1,1,1,1,1,1,1,1,1,1,1,1,1,1,1,1,1,1,1,1,1,1,1,1,
1,1,1,1,1,1,1,1,1,1,1,1,1,1,1,1,1,1,1,1,1,1,1,1,1,1,1,1,1,1,1,1,1,1,1,1,
1,1,1,1,1,1,1,1,1,1,1,1,1,1,1,1,1,1,1,1,1,1,1,1,1,1,1,1,1,1,1,1,1,1,1,1,
1,1,1,1,1,1,1,1,1,1,1,1,1,1,1,1,1,1,1,1,1,1,1,1,1,1,1,1,1,1,1,1,1,1,1,1,
1,1,1,1,1,1,1,1,1,1,1,1,1,1,1,1,1,1,1,1,1,1,1,1,1,1,1,1,1,1,1,1,1,1,1,1,
1,1,1,1,1,1,1,1,1,1,1,1,1,1,1,1,1,1,1,1,1,1,1,1,1,1,1,1,1,1,1,1,1,1,1,1,
1,1,1,1,1,1,1,1,1,1,1,1,1,1,1,1,1,1,1,1,1,1,1,1,1,1,1,1,1,1,1,1,1,1,1,1,
1,1,1,1,1,1,1,1,1,1,1,1,1,1,1,1,1,1,1,1,1,1,1,1,1,1,1,1,1,1,1,1,1,1,1,1,
1,1,1,1,1,1,1,1,1,1,1,1,1,1,1,1,1,1,1,1,1,1,1,1,1,1,1,1,1,1,1,1,1,1,1,1,
1,1,1,1,1,1,1,1,1,1,1,1,1,1,1,1,1,1,1,1,1,1,1,1,1,1,1,1,1,1,1,1,1,1,1,1,
1,1,1,1,1,1,1,1,1,1,1,1,1,1,1,1,1,1,1,1,1,1,1,1,1,1,1,1,1,1,1,1,1,1,1,1,
1,1,1,1,1,1,1,1,1,1,1,1,1,1,1,1,1,1,1,1,1,1,1,1,1,1,1,1,1,1,1,1,1,1,1,1,
1,1,1,1,1,1,1,1,1,1,1,1,1,1,1,1,1,1,1,1,1,1,1,1,1,1,1,1,1,1,1,1,1,1,1,1,
1,1,1,1,1,1,1,1,1,1,1,1,1,1,1,1,1,1,1,1,1,1,1,1,1,1,1,1,1,1,1,1,1,1,1,1,
1,1,1,1,1,1,1,1,1,1,1,1,1,1,1,1,1,1,1,1,1,1,1,1,1,1,1,1,1,1,1,1,1,1,1,1,
1,1,1,1,1,1,1,1,1,1,1,1,1,1,1,1,1,1,1,1,1,1,1,1,1,1,1,1,1,1,1,1,1,1,1,1,
1,1,1,1,1,1,1,1,1,1,1,1,1,1,1,1,1,1,1,1,1,1,1,1,1,1,1,1,1,1,1,1,1,1,1,1,
1,1,1,1,1,1,1,1,1,1,1,1,1,1,1,1,1,1,1,1,1,1,1,1,1,1,1,1,1,1,1,1,1,1,1,1,
1,1,1,1,1,1,1,1,1,1,1,1,1,1,1,1,1,1,1,1,1,1,1,1,1,1,1,1,1,1,1,1,1,1,1,1,
1,1,1,1,1,1,1,1,1,1,1,1,1,1,1,1,1,1,1,1,1,1,1,1,1,1,1,1,1,1,1,1,1,1,1,1,
1,1,1,1,1,1,1,1,1,1,1,1,1,1,1,1,1,1,1,1,1,1,1,1,1,1,1,1,1,1,1,1,1,1,1,1,
1,1,1,1,1,1,1,1,1,1,1,1,1,1,1,1,1,1,1,1,1,1,1,1,1,1,1,1,1,1,1,1,1,1,1,1,
1,1,1,1,1,1,1,1,1,1,1,1,1,1,1,1,1,1,1,1,1,1,1,1,1,1,1,1,1,1,1,1,1,1,1,1,
1,1,1,1,1,1,1,1,1,1,1,1,1,1,1,1,1,1,1,1,1,1,1,1,1,1,1,1,1,1,1,1,1,1,1,1,
1,1,1,1,1,1,1,1,1,1,1,1,1,1,1,1,1,1,1,1,1,1,1,1,1,1,1,1,1,1,1,1,1,1,1,1,
1,1,1,1,1,1,1,1,1,1,1,1,1,1,1,1,1,1,1,1,1,1,1,1,1,1,1,1,1,1,1,1,1,1,1,1,
1,1,1,1,1,1,1,1,1,1,1,1,1,1,1,1,1,1,1,1,1,1,1,1,1,1,1,1,1,1,1,1,1,1,1,1,
1,1,1,1,1,1,1,1,1,1,1,1,1,1,1,1,1,1,1,1,1,1,1,1,1,1,1,1,1,1,1,1,1,1,1,1,
1,1,1,1,1,1,1,1,1,1,1,1,1,1,1,1,1,1,1,1,1,1,1,1,1,1,1,1,1,1,1,1,1,1,1,1,
1,1,1,1,1,1,1,1,1,1,1,1,1,1,1,1,1,1,1,1,1,1,1,1,1,1,1,1,1,1,1,1,1,1,1,1,
1,1,1,1,1,1,1,1,1,1,1,1,1,1,1,1,1,1,1,1,1,1,1,1,1,1,1,1,1,1,1,1,1,1,1,1,
1,1,1,1,1,1,1,1,1,1,1,1,1,1,1,1,1,1,1,1,1,1,1,1,1,1,1,1,1,1,1,1,1,1,1,1,
1,1,1,1,1,1,1,1,1,1,1,1,1,1,1,1,1,1,1,1,1,1,1,1,1,1,1,1,1,1,1,1,1,1,1,1,
1,1,1,1,1,1,1,1,1,1,1,1,1,1,1,1,1,1,1,1,1,1,1,1,1,1,1,1,1,1,1,1,1,1,1,1,
1,1,1,1,1,1,1,1,1,1,1,1,1,1,1,1,1,1,1,1,1,1,1,1,1,1,1,1,1,1,1,1,1,1,1,1,
1,1,1,1,1,1,1,1,1,1,1,1,1,1,1,1,1,1,1,1,1,1,1,1,1,1,1,1,1,1,1,1,1,1,1,1,
1,1,1,1,1,1,1,1,1,1,1,1,1,1,1,1,1,1,1,1,1,1,1,1,1,1,1,1,1,1,1,1,1,1,1,1,
1,1,1,1,1,1,1,1,1,1,1,1,1,1,1,1,1,1,1,1,1,1,1,1,1,1,1,1,1,1,1,1,1,1,1,1,
1,1,1,1,1,1,1,1,1,1,1,1,1,1,1,1,1,1,1,1,1,1,1,1,1,1,1,1,1,1,1,1,1,1,1,1,
1,1,1,1,1,1,1,1,1,1,1,1,1,1,1,1,1,1,1,1,1,1,1,1,1,1,1,1,1,1,1,1,1,1,1,1,
1,1,1,1,1,1,1,1,1,1,1,1,1,1,1,1,1,1,1,1,1,1,1,1,1,1,1,1,1,1,1,1,1,1,1,1,
1,1,1,1,1,1,1,1,1,1,1,1,1,1,1,1,1,1,1,1,1,1,1,1,1,1,1,1,1,1,1,1,1,1,1,1,
1,1,1,1,1,1,1,1,1,1,1,1,1,1,1,1,1,1,1,1,1,1,1,1,1,1,1,1,1,1,1,1,1,1,1,1,
1,1,1,1,1,1,1,1,1,1,1,1,1,1,1,1,1,1,1,1,1,1,1,1,1,1,1,1,1,1,1,1,1,1,1,1,
1,1,1,1,1,1,1,1,1,1,1,1,1,1,1,1,1,1,1,1,1,1,1,1,1,1,1,1,1,1,1,1,1,1,1,1,
1,1,1,1,1,1,1,1,1,1,1,1,1,1,1,1,1,1,1,1,1,1,1,1,1,1,1,1,1,1,1,1,1,1,1,1,
1,1,1,1,1,1,1,1,1,1,1,1,1,1,1,1,1,1,1,1,1,1,1,1,1,1,1,1,1,1,1,1,1,1,1,1,
1,1,1,1,1,1,1,1,1,1,1,1,1,1,1,1,1,1,1,1,1,1,1,1,1,1,1,1,1,1,1,1,1,1,1,1,
1,1,1,1,1,1,1,1,1,1,1,1,1,1,1,1,1,1,1,1,1,1,1,1,1,1,1,1,1,1,1,1,1,1,1,1,
1,1,1,1,1,1,1,1,1,1,1,1,1,1,1,1,1,1,1,1,1,1,1,1,1,1,1,1,1,1,1,1,1,1,1,1,
1,1,1,1,1,1,1,1,1,1,1,1,1,1,1,1,1,1,1,1,1,1,1,1,1,1,1,1,1,1,1,1,1,1,1,1,
1,1,1,1,1,1,1,1,1,1,1,1,1,1,1,1,1,1,1,1,1,1,1,1,1,1,1,1,1,1,1,1,1,1,1,1,
1,1,1,1,1,1,1,1,1,1,1,1,1,1,1,1,1,1,1,1,1,1,1,1,1,1,1,1,1,1,1,1,1,1,1,1,
1,1,1,1,1,1,1,1,1,1,1,1,1,1,1,1,1,1,1,1,1,1,1,1,1,1,1,1,1,1,1,1,1,1,1,1,
1,1,1,1,1,1,1,1,1,1,1,1,1,1,1,1,1,1,1,1,1,1,1,1,1,1,1,1,1,1,1,1,1,1,1,1,
1,1,1,1,1,1,1,1,1,1,1,1,1,1,1,1,1,1,1,1,1,1,1,1,1,1,1,1,1,1,1,1,1,1,1,1,
1,1,1,1,1,1,1,1,1,1,1,1,1,1,1,1,1,1,1,1,1,1,1,1,1,1,1,1,1,1,1,1,1,1,1,1,
1,1,1,1,1,1,1,1,1,1,1,1,1,1,1,1,1,1,1,1,1,1,1,1,1,1,1,1,1,1,1,1,1,1,1,1,
1,1,1,1,1,1,1,1,1,1,1,1,1,1,1,1,1,1,1,1,1,1,1,1,1,1,1,1,1,1,1,1,1,1,1,1,
1,1,1,1,1,1,1,1,1,1,1,1,1,1,1,1,1,1,1,1,1,1,1,1,1,1,1,1,1,1,1,1,1,1,1,1,
1,1,1,1,1,1,1,1,1,1,1,1,1,1,1,1,1,1,1,1,1,1,1,1,1,1,1,1,1,1,1,1,1,1,1,1,
1,1,1,1,4),(2,2),(0.,0.869746702321014,1.7394931589914,2.60923976624962,
3.47983908319159,4.35043840179749,5.22018503077054,6.08993165951504,6.95967828799171,
7.82942491616733,8.69917154401062,9.56891817149224,10.4395174886835,11.3101168056706,
12.179863432132,13.049610058144,13.9193566836854,14.7891033087372,15.6588499332817,
16.5285965573034,17.3991958717975,18.2697951860185,18.7046684974166,19.1395418086746,
19.5744151197912,20.0092884307654,20.4441617415962,20.8790350522825,21.7487816732187,
22.1836549834672,22.6185282935685,23.0534016035221,23.4882749133276,23.9231482229848,
24.3588742245859,24.794600226187,25.2294735355468,26.0992201538203,26.5340934627341,
26.9689667714994,27.4038400801166,27.838713388586,28.2735866969081,28.7084600050832,
29.143333313112,29.5782066209952,30.0130799287334,30.4479532363275,30.8828265437783,
31.3185525442794,31.7542785447804,32.1891518519474,32.6240251589741,33.0588984658616,
33.4937717726112,33.928645079224,34.3635183857014,34.7983916920448,35.2332649982556,
35.6681383043353,36.1030116102854,36.5378849161076,36.9727582218035,37.4076315273749,
37.8425048328235,38.2782308323341,38.7139568318446,39.1488301370532,39.5837034421446,
40.0185767471208,40.4534500519838,40.8883233567357,41.3231966613787,41.7580699659148,
42.1929432703463,42.6278165746754,43.0626898789044,43.4975631830356,43.9324364870714,
44.3673097910142,44.8021830948664,45.2379090935952,45.673635092324,46.1085083960024,
46.5433816995978,46.9782550031127,47.4131283065497,47.8480016099115,48.2828749132006,
48.7177482164198,49.1526215195718,49.5874948226593,50.0223681256851,50.457241428652,
50.8921147315628,51.3269880344203,51.7618613372274,52.197587335454,52.6333133336805,
53.0681866363954,53.5030599390685,53.9379332417027,54.3728065443011,54.8076798468664,
55.2425531494018,55.6774264519101,56.1122997543943,56.5471730568575,56.9820463593026,
57.4169196617326,57.8517929641506,58.2866662665595,58.7215395689624,59.157265567009,
59.5929915650557,60.0278648674556,60.4627381698584,60.8976114722673,61.3324847746853,
61.7673580771153,62.2022313795604,62.6371046820236,63.0719779845079,63.5068512870162,
63.9417245895516,64.376597892117,64.8114711947155,65.2463444973499,65.6812178000231,
66.1169437982275,66.5526697964318,66.9875430991915,67.4224164019987,67.8572897048563,
68.2921630077673,68.7270363107343,69.1619096137603,69.5967829168479,70.0316562200001,
70.4665295232194,70.9014028265087,71.3362761298705,71.7711494333077,72.2060227368227,
72.6408960404182,73.0766220391044,73.5123480377905,73.9472213415547,74.382094645407,
74.8169679493499,75.2518412533859,75.6867145575172,76.1215878617464,76.5564611660756,
76.9913344705072,77.4262077750435,77.8610810796866,78.2959543844386,78.7308276893018,
79.1657009942781,79.6005742993696,80.0363002988208,80.4720262982719,80.9068996035997,
81.3417729090484,81.7766462146199,82.211519520316,82.6463928261383,83.0812661320886,
83.5161394381684,83.9510127443794,84.3858860507229,84.8207593572004,85.2556326638134,
85.6905059705631,86.1253792774507,86.5602525844776,86.995978584908,87.4317045853384,
87.8665778926469,88.3014512000977,88.7363245076919,89.1711978154302,89.6060711233134,
90.0409444313423,90.4758177395175,90.9106910478396,91.345564356309,91.7804376649263,
92.2153109736917,92.6501842826055,93.085057591668,93.5199309008791,93.9556569024059,
94.3913829039327,94.8262562134414,95.2611295230986,95.6960028329042,96.1308761428578,
96.5657494529591,97.0006227632077,97.4354960736028,97.870369384144,98.3052426948304,
98.7401160056612,99.1749893166354,99.6098626277522,100.04473593901,100.915335253024,
101.351061255639,101.785934567313,102.220807879124,102.655681191068,103.090554503145,
103.525427815353,104.395174440154,105.264921065453,105.699794378283,106.134667691232,
106.569541004295,107.004414317471,107.8750136343,108.745612951339,109.615359578629,
110.485106206296,111.354852834309,112.224599462639,113.094346091254,113.964092720119,
114.834692038763,115.705291357499,116.575037986826,117.444784616267,118.314531245777,
119.184277875311,120.054024504821,120.923771134261,121.794370453112,122.66496977189,
123.534716400968,124.404463029834,125.274209658448,126.143956286779,127.013702914792,
127.883449542458,128.754048859798,129.624648176939,130.494394803617,131.364141429857,
132.233888055637,133.103634680937,133.973381305737,134.843127930023,135.71372724472,
136.584326559147,137.019199870684,137.454073182083,137.888946493341,138.323819804458,
139.193566426263,140.063313047491,140.498186357887,140.933059668136,141.367932978237,
141.802806288191,142.237679597997,142.673405599673,143.109131601348,143.544004910857,
143.978878220217,144.413751529429,144.848624838491,145.283498147405,145.718371456171,
146.153244764789,146.588118073258,147.022991381581,147.457864689756,147.892737997785,
148.327611305669,148.762484613407,149.197357921002,149.633083921574,150.068809922147,
150.503683229455,150.938556536623,151.37342984365,151.808303150538,152.243176457288,
152.678049763901,153.112923070379,153.547796376722,153.982669682934,154.417542989014,
154.852416294964,155.287289600787,155.722162906483,156.157036212055,156.592762211626,
157.028488211198,157.463361516526,157.898234821735,158.333108126826,158.767981431803,
159.202854736666,159.637728041419,160.072601346062,160.507474650599,160.94234795503,
161.37722125936,161.812094563589,162.246967867721,162.681841171757,163.1167144757,
163.552440474473,163.988166473247,164.423039777011,164.85791308069,165.292786384286,
165.727659687801,166.162532991238,166.597406294601,167.03227959789,167.46715290111,
167.902026204262,168.33689950735,168.771772810376,169.206646113343,169.641519416254,
170.076392719112,170.512118717363,170.947844715614,171.382718018374,171.817591321089,
172.252464623762,172.687337926397,173.122211228996,173.557084531561,173.991957834097,
174.426831136606,174.86170443909,175.296577741554,175.731451044,176.16632434643,
176.601197648848,177.036070951258,177.471796949306,177.907522947355,178.342396249755,
178.777269552155,179.212142854558,179.647016156968,180.081889459386,180.516762761816,
180.951636064262,181.386509366726,181.82138266921,182.256255971719,182.691129274255,
183.12600257682,183.560875879419,183.995749182054,184.431475180237,184.867201178421,
185.302074481136,185.736947783896,186.171821086704,186.606694389561,187.041567692473,
187.47644099544,187.911314298466,188.346187601554,188.781060904706,189.215934207926,
189.650807511215,190.085680814577,190.520554118015,190.95542742153,191.391153420175,
191.82687941882,192.261752722499,192.696626026263,193.131499330116,193.566372634059,
194.001245938095,194.436119242227,194.870992546456,195.305865850785,195.740739155217,
196.175612459754,196.610485764397,197.045359069149,197.480232374013,197.915105678989,
198.350831678382,198.786557677775,199.221430982984,199.656304288312,200.091177593761,
200.526050899333,200.960924205029,201.395797510852,201.830670816802,202.265544122882,
202.700417429093,203.135290735437,203.570164041915,204.005037348528,204.439910655278,
204.874783962166,205.310509962526,205.746235962887,206.181109270054,206.615982577363,
207.050855884814,207.485729192409,207.920602500147,208.355475808031,208.79034911606,
209.225222424235,209.660095732558,210.094969041027,210.529842349645,210.96471565841,
211.399588967324,211.834462276387,212.27018827784,212.705914279292,213.140787588653,
213.575660898161,214.010534207819,214.880280827579,215.31515413768,215.750027447929,
216.184900758324,216.619774068866,217.054647379553,217.489520690384,218.359267312475,
219.22986662628,219.665592628826,220.100465940363,220.535339252038,220.970212563848,
221.83995918787,222.709705812416,223.579452437468,224.014325750179,224.44919906301,
225.318945689022,226.189545005688,227.060144322571,227.929890949664,228.799637577146,
229.66938420499,230.539130833166,231.408877461643,232.278624090388,233.149223408954,
234.019822727623,234.889569356878,235.759315986267,236.629062615749,237.498809245277,
238.368555874806,239.238302504287,240.108901823183,240.979501142017,241.849247771189,
242.718994400167,243.588741028911,244.458487657389,245.328234285565,246.197980913409,
247.068580230891,247.939179548182,248.80892617507,249.678672801532,250.548419427545,
251.418166053087,252.287912678139,253.157659302684,254.028258617581,254.898857932211,
255.333731243885,255.768604555423,256.203477866821,256.63835117808,257.508097800171,
258.377844421689,258.812717732231,259.247591042627,259.682464352876,260.117337662977,
260.552210972931,260.987936974682,261.858536286089,262.293409595598,262.728282904958,
263.16315621417,263.598029523233,264.032902832147,264.467776140913,264.902649449531,
265.337522758001,265.772396066323,266.207269374499,266.642142682528,267.077015990412,
267.511889298151,267.947615298795,268.383341299439,268.81821460689,269.2530879142,
269.687961221367,270.122834528394,270.557707835282,270.992581142032,271.427454448646,
271.862327755124,272.297201061468,272.732074367679,273.166947673759,273.60182097971,
274.036694285533,274.471567591229,274.907293590862,275.343019590495,275.777892895944,
276.212766201272,276.647639506481,277.082512811573,277.51738611655,277.952259421414,
278.387132726166,278.82200603081,279.256879335346,279.691752639779,280.126625944108,
280.561499248338,280.996372552469,281.431245856506,281.866971855324,282.302697854143,
282.737571157996,283.172444461761,283.60731776544,284.042191069036,284.477064372551,
284.911937675989,285.346810979351,285.781684282641,286.216557585861,286.651430889013,
287.086304192101,287.521177495128,287.956050798095,288.390924101007,288.826650099283,
289.262376097559,289.697249400366,290.132122703127,290.566996005842,291.001869308516,
291.43674261115,291.871615913749,292.306489216315,292.741362518851,293.17623582136,
293.611109123845,294.045982426308,294.480855728754,294.915729031185,295.350602333603,
295.786328331655,296.222054329707,296.65692763211,297.091800934511,297.526674236911,
297.961547539314,298.396420841724,298.831294144142,299.266167446573,299.701040749018,
300.135914051482,300.570787353967,301.005660656476,301.440533959012,301.875407261578,
302.310280564177,302.746006562341,303.181732560506,303.616605863179,304.051479165895,
304.486352468655,304.921225771462,305.35609907432,305.790972377232,306.225845680199,
306.660718983226,307.095592286314,307.530465589466,307.965338892686,308.400212195976,
308.835085499338,309.269958802776,309.705684801381,310.141410799985,310.576284103581,
311.01115740726,311.446030711025,311.880904014878,312.315777318821,312.750650622858,
313.185523926989,313.620397231219,314.055270535549,314.490143839981,314.925017144517,
315.359890449161,315.794763753913,316.229637058777,316.665363058112,317.101089057448,
317.53596236254,317.970835667749,318.405708973077,318.840582278526,319.275455584098,
319.710328889795,320.145202195618,320.580075501568,321.014948807648,321.44982211386,
321.884695420204,322.319568726682,322.754442033295,323.189315340045,323.625041340336,
324.060767340628,324.495640647655,324.930513954822,325.365387262131,325.800260569583,
326.235133877177,326.670007184916,327.1048804928,327.539753800829,327.974627109005,
328.409500417327,328.844373725797,329.279247034415,329.714120343181,330.148993652095,
330.584719653474,331.020445654852,331.455318964064,331.890192273424,332.325065582933,
332.759938892591,333.194812202397,333.629685512351,334.064558822453,334.499432132702,
334.934305443098,335.369178753639,335.804052064326,336.673798686132,337.108671997249,
337.544397999725,337.980124002201,338.4149973136,338.849870625137,339.284743936812,
340.154490560568,341.024237184854,341.459110497191,341.893983809655,342.328857122244,
342.763730434955,343.633477060735,344.504076377234,345.374675693955,346.244422320844,
347.114168948136,347.983915575803,348.853662203817,349.723408832148,350.593155460764,
351.463754779246,352.334354097839,353.204100727012,354.07384735634,354.943593985781,
355.813340615292,356.683087244827,357.552833874338,358.423433193272,359.294032512154,
360.163779141409,361.033525770489,361.903272399355,362.77301902797,363.642765656301,
364.512512284316,365.383111601936,366.253710919371,367.123457546465,367.993204173143,
368.862950799383,369.732697425164,370.602444050463,371.472190675265,372.342789990359,
373.21338930519,373.648262617,374.083135928675,374.952882551611,375.822629173987,
376.257502484962,376.692375795793,377.12724910648,377.562122417021,377.996995727417,
378.431869037666,378.866742347767,379.302468349591,379.738194351416,380.173067661222,
380.607940970879,381.042814280388,381.477687589749,381.91256089896,382.347434208023,
382.782307516937,383.217180825703,383.652054134321,384.086927442791,384.521800751113,
384.956674059289,385.391547367318,385.826420675202,386.262146675918,386.697872676635,
387.13274598423,387.567619291681,388.00249259899,388.437365906157,388.872239213185,
389.307112520073,389.741985826823,390.176859133436,390.611732439914,391.046605746258,
391.48147905247,391.91635235855,392.351225664501,392.786098970323,393.221824970019,
393.657550969714,394.092424275286,394.527297580735,394.962170886063,395.397044191272,
395.831917496364,396.266790801341,396.701664106204,397.136537410957,397.5714107156,
398.006284020137,398.441157324569,398.876030628899,399.310903933128,399.74577723726,
400.181503236126,400.617229234991,401.052102538934,401.486975842787,401.921849146551,
402.356722450231,402.791595753827,403.226469057342,403.66134236078,404.096215664142,
404.531088967432,404.965962270651,405.400835573804,405.835708876892,406.270582179918,
406.705455482886,407.141181481189,407.576907479491,408.01178078235,408.446654085157,
408.881527387917,409.316400690633,409.751273993306,410.186147295941,410.62102059854,
411.055893901106,411.490767203642,411.925640506151,412.360513808636,412.795387111099,
413.230260413545,413.665133715976,414.100859714032,414.536585712088,414.971459014498,
415.406332316901,415.841205619301,416.276078921702,416.710952224105,417.145825526515,
417.580698828933,418.015572131364,418.45044543381,418.885318736273,419.320192038758,
419.755065341267,420.189938643803,420.624811946369,421.060537944515,421.496263942662,
421.931137245297,422.36601054797,422.800883850686,423.235757153446,423.670630456253,
424.105503759112,424.540377062023,424.975250364991,425.410123668017,425.844996971105,
426.279870274258,426.714743577477,427.149616880767,427.584490184129,428.020216182695,
428.455942181261,428.890815484776,429.325688788373,429.760562092052,430.195435395816,
430.630308699669,431.065182003612,431.500055307649,431.93492861178,432.36980191601,
432.80467522034,433.239548524772,433.674421829309,434.109295133952,434.544168438705,
434.979894437984,435.415620437262,435.850493742239,436.285367047331,436.72024035254,
437.155113657869,437.589986963318,438.024860268889,438.459733574586,438.894606880409,
439.32948018636,439.76435349244,440.199226798651,440.634100104995,441.068973411473,
441.503846718087,441.939572718309,442.375298718531,442.810172025419,443.245045332447,
443.679918639614,444.114791946923,444.549665254374,444.984538561969,445.419411869708,
445.854285177591,446.289158485621,446.724031793796,447.158905102119,447.593778410589,
448.028651719207,448.463525027973,448.899251029277,449.334977030581,449.769850339644,
450.639596958216,451.074470267725,451.509343577383,451.944216887189,452.379090197143,
452.813963507244,453.248836817493,453.683710127889,454.118583438431,454.553456749117,
454.988330059949,455.423203370923,455.858929373329,456.294655375734,456.729528686993,
457.164401998391,457.599275309929,458.469021933414,458.90389524536,459.338768557437,
459.773641869646,460.208515181983,460.643388494447,461.078261807036,461.948008432578,
462.818607748906,463.689207065461,464.55895369214,465.428700319234,466.298446946716,
467.16819357456,468.037940202737,468.907686831215,469.778286149605,470.648885468116,
471.518632097196,472.388378726451,473.258125355841,474.127871985322,474.997618614851,
475.86736524438,476.737964563343,477.608563882265,478.478310511593,479.348057140765,
480.217803769743,481.087550398488,481.957297026966,482.827043655142,483.697642972895,
484.568242290469,485.43798891776,486.307735544649,487.177482171112,488.047228797125,
488.916975422667,489.78672204772,490.657321363009,491.09304736596,491.527920678038,
492.397667301793,493.267413925005,494.137160547663,494.57203385878,495.006907169755,
495.441780480586,495.876653791273,496.311527101814,496.74640041221,497.616999724357,
498.052725726255,498.487599036209,498.922472346015,499.357345655673,499.792218965182,
500.227092274542,500.661965583754,501.096838892816,501.531712201731,501.966585510497,
502.401458819114,502.836332127584,503.271205435907,503.706078744082,504.140952052112,
504.576678052901,505.01240405369,505.447277361429,505.882150669023,506.317023976474,
506.751897283783,507.186770590951,507.621643897978,508.056517204866,508.491390511616,
508.92626381823,509.361137124708,509.796010431052,510.230883737263,510.665757043344,
511.100630349294,511.536356349053,511.972082348811,512.406955654506,512.841828960076,
513.276702265523,513.711575570849,514.146448876056,514.581322181146,515.016195486121,
515.451068790983,515.885942095733,516.320815400375,516.75568870491,517.19056200934,
517.625435313668,518.060308617896,518.496034616807,518.931760615718,519.366633919752,
519.801507223694,520.236380527545,520.671253831307,521.106127134985,521.541000438579,
521.975873742092,522.410747045528,522.845620348888,523.280493652176,523.715366955394,
524.150240258545,524.585113561631,525.019986864656,525.455712862985,525.891438861313,
526.326312164223,526.761185467079,527.196058769885,527.630932072643,528.065805375356,
528.500678678029,528.935551980661,529.370425283258,529.805298585822,530.240171888356,
530.675045190863,531.109918493346,531.544791795808,531.979665098252,532.415391096312,
532.851117094373,533.285990396789,533.720863699197,534.155737001598,534.590610303997,
535.025483606395,535.460356908796,535.895230211204,536.330103513621,536.764976816049,
537.199850118493,537.634723420955,538.069596723438,538.504470025945,538.93934332848,
539.375069326608,539.810795324736,540.245668627333,540.680541929966,541.115415232637,
541.550288535351,541.985161838109,542.420035140915,542.854908443771,543.28978174668,
543.724655049646,544.15952835267,544.594401655757,545.029274958907,545.464148262125,
545.899021565413,546.334747563939,546.770473562465,547.205346865901,547.640220169415,
548.075093473009,548.509966776686,548.944840080449,549.3797133843,549.814586688241,
550.249459992276,550.684333296405,551.119206600633,551.554079904961,551.988953209391,
552.423826513926,552.858699818567,553.294425817789,553.73015181701,554.165025121872,
554.599898426846,555.034771731937,555.469645037144,555.90451834247,556.339391647917,
556.774264953487,557.209138259182,557.644011565003,558.078884870951,558.51375817703,
558.948631483239,559.383504789581,559.818378096058,560.254104096209,560.689830096361,
561.12470340311,561.559576709996,561.994450017021,562.429323324187,562.864196631494,
563.299069938943,563.733943246536,564.168816554273,564.603689862154,565.038563170182,
565.473436478355,565.908309786676,566.343183095144,566.77805640376,567.213782404988,
567.649508406216,568.084381715128,568.519255024189,568.954128333399,569.389001642757,
569.823874952264,570.258748261921,570.693621571725,571.128494881677,571.563368191777,
572.433114812417,572.867988122957,573.302861433642,573.737734744471,574.173460746804,
574.609186749136,575.044060060251,575.913806682904,576.783553306113,577.218426617922,
577.653299929865,578.08817324194,578.523046554147,579.392793178944,580.26253980424,
581.13313912039,581.568865123709,582.003738436771,582.87348506323,583.743231690115,
584.612978317402,585.482724945065,586.352471573076,587.222218201403,588.092817519691,
588.963416838109,589.833163467083,590.702910096251,591.572656725575,592.442403355013,
593.31214998452,594.181896614051,595.05249593303,595.92309525198,596.792841881366,
597.662588510618,598.532335139693,599.402081768556,600.271828397167,601.141575025495,
602.012174343369,602.882773661074,603.752520288553,604.622266915642,605.492013542317,
606.361760168553,607.23150679433,608.101253419626,608.971852735101,609.842452050322,
610.71219867434,611.581945297822,612.451691920754,612.886565232011,613.321438543126,
613.756311854099,614.191185164928,615.060931786153,615.931531098516,616.367257100486,
616.802130410586,617.237003720538,617.671877030342,618.106750339998,618.541623649505,
618.976496958863,619.411370268073,619.846243577134,620.281116886046,620.71599019481,
621.150863503426,621.585736811894,622.020610120214,622.455483428388,622.891209429248,
623.326935430108,623.761808737989,624.196682045726,624.631555353319,625.066428660769,
625.501301968075,625.936175275241,626.371048582266,626.805921889153,627.240795195901,
627.675668502512,628.110541808988,628.54541511533,628.98028842154,629.415161727618,
629.850887727438,630.286613727259,630.72148703308,631.156360338774,631.591233644344,
632.026106949791,632.460980255118,632.895853560325,633.330726865415,633.76560017039,
634.200473475251,634.635346780002,635.070220084644,635.505093389179,635.939966693609,
636.374839997937,636.810565996897,637.246291995857,637.681165299986,638.116038604021,
638.550911907962,638.985785211813,639.420658515576,639.855531819253,640.290405122847,
640.725278426361,641.160151729796,641.595025033157,642.029898336444,642.464771639662,
642.899644942813,643.334518245899,643.770244244257,644.205970242616,644.640843545581,
645.075716848491,645.510590151347,645.945463454153,646.380336756911,646.815210059625,
647.250083362296,647.684956664929,648.119829967526,648.55470327009,648.989576572624,
649.424449875131,649.859323177614,650.294196480076,650.729922478144,651.165648476212,
651.600521778641,652.035395081057,652.470268383465,652.905141685866,653.340014988265,
653.774888290663,654.209761593065,654.644634895472,655.079508197889,655.514381500318,
655.949254802762,656.384128105224,656.819001407706,657.253874710213,657.689600708326,
658.12532670644,658.560200009004,658.995073311601,659.429946614234,659.864819916905,
660.299693219619,660.734566522377,661.169439825183,661.604313128039,662.039186430948,
662.474059733914,662.908933036938,663.343806340025,663.778679643175,664.213552946393,
664.649278944883,665.085004943373,665.519878246733,665.954751550169,666.389624853683,
666.824498157277,667.259371460954,667.694244764717,668.129118068568,668.563991372509,
668.998864676544,669.433737980674,669.868611284901,670.303484589229,670.738357893659,
671.173231198194,671.608957197361,672.044683196528,672.479556501278,672.91442980614,
673.349303111115,673.784176416205,674.219049721412,674.653923026738,675.088796332185,
675.523669637755,675.95854294345,676.393416249271,676.82828955522,677.263162861298,
677.698036167508,678.13290947385,678.568635473934,679.004361474018,679.439234780629,
679.874108087377,680.308981394264,680.743854701289,681.178728008455,681.613601315762,
682.048474623211,682.483347930804,682.91822123854,683.353094546422,683.78796785445,
684.222841162623,684.657714470944,685.092587779412,685.528313780566,685.96403978172,
686.398913090483,686.833786399396,687.268659708457,687.703533017666,688.138406327025,
688.573279636532,689.008152946187,689.443026255992,689.877899565944,690.312772876043,
690.74764618629,691.182519496684,691.617392807224,692.052266117909,692.487992120169,
692.92371812243,693.358591433403,694.228338055774,694.663211367171,695.098084678707,
695.532957990379,695.967831302188,696.402704614131,696.837577926207,697.707324550749,
698.577071175797,699.011944488507,699.447670491767,699.883396495028,700.318269807975,
701.188016434211,702.057763060886,702.927509687976,703.797256315454,704.667002943295,
705.536749571467,706.407348889651,707.277948207973,708.147694836835,709.017441465911,
709.887188095163,710.756934724548,711.626681354026,712.496427983551,713.367027302543,
714.237626621516,715.107373250954,715.977119880277,716.846866509446,717.716613138419,
718.586359767161,719.456106395635,720.32670571363,721.197305031464,722.067051659126,
722.936798286414,723.806544913299,724.676291539758,725.546038165767,726.415784791305,
727.286384106969,728.156983422381,729.026730046663,729.896476670415,730.331349982088,
730.766223293624,731.201096605021,731.635969916278,732.505716538366,733.37546315988,
733.81033647042,734.246062472462,734.681788474505,735.116661784752,735.551535094852,
735.986408404804,736.421281714608,736.856155024264,737.291028333771,737.72590164313,
738.160774952339,738.5956482614,739.030521570312,739.465394879076,739.900268187692,
740.33514149616,740.77001480448,741.205740805414,741.641466806347,742.076340114374,
742.511213422256,742.946086729993,743.380960037585,743.815833345035,744.250706652341,
744.685579959507,745.120453266533,745.555326573419,745.990199880167,746.425073186778,
746.859946493254,747.294819799596,747.729693105806,748.165419105691,748.601145105576,
749.036018411525,749.470891717346,749.90576502304,750.34063832861,750.775511634057,
751.210384939384,751.645258244591,752.080131549682,752.515004854656,752.949878159518,
753.384751464269,753.81962476891,754.254498073445,754.689371377875,755.125097376885,
755.560823375895,755.995696680123,756.430569984253,756.865443288287,757.300316592228,
757.735189896079,758.170063199842,758.604936503519,759.039809807113,759.474683110627,
759.909556414062,760.344429717423,760.779303020711,761.214176323929,761.649049627079,
762.084775625469,762.520501623858,762.955374926883,763.390248229848,763.825121532758,
764.259994835614,764.694868138419,765.129741441178,765.564614743891,765.999488046563,
766.434361349196,766.869234651793,767.304107954357,767.738981256891,768.173854559398,
768.608727861881,769.044453859958,769.480179858035,769.915053160479,770.349926462907,
770.784799765324,771.219673067731,771.654546370133,772.089419672531,772.52429297493,
772.959166277331,773.394039579739,773.828912882155,774.263786184584,774.698659487028,
775.13353278949,775.568406091973,776.004132090072,776.439858088172,776.874731390706,
777.30960469327,777.744477995867,778.1793512985,778.614224601171,779.049097903885,
779.483971206643,779.918844509449,780.353717812305,780.788591115215,781.22346441818,
781.658337721205,782.093211024291,782.528084327442,782.963810325897,783.399536324352,
783.834409627639,784.269282931,784.704156234435,785.139029537949,785.573902841543,
786.00877614522,786.443649448983,786.878522752834,787.313396056775,787.74826936081,
788.183142664939,788.618015969167,789.052889273495,789.487762577925,789.923488577038,
790.359214576152,790.794087880793,791.228961185544,791.663834490406,792.098707795381,
792.533581100471,792.968454405678,793.403327711004,793.838201016451,794.273074322021,
794.707947627716,795.142820933537,795.577694239486,796.012567545564,796.447440851774,
796.883166851791,797.318892851808,797.753766158284,798.188639464895,798.623512771643,
799.058386078529,799.493259385555,799.92813269272,800.363006000027,800.797879307477,
801.232752615069,801.667625922806,802.102499230688,802.537372538715,802.972245846889,
803.40711915521,803.84284515629,804.27857115737,804.713444465985,805.148317774749,
805.583191083662,806.018064392723,806.452937701933,806.887811011291,807.322684320798,
808.192430940258,808.62730425021,809.06217756031,809.497050870557,809.931924180951,
810.36679749149,810.802523493679,811.238249495867,811.673122806697,812.542869428785,
812.977742740041,813.412616051438,813.847489362974,814.282362674646,814.717235986455,
815.152109298398,816.021855922681,816.891602547478,817.326475860065,817.762201863265,
818.197927866466,818.632801179295,819.502547805304,820.372294431763,821.242041058648,
822.111787685935,822.981534313598,823.851280941609,824.721880259681,825.5924795779,
826.462226206642,827.331972835616,828.201719464785,829.071466094109,829.941212723546,
830.810959353053,831.681558672047,832.552157991036,833.421904620514,834.2916512499,
835.161397879151,836.031144508226,836.900891137089,837.770637765701,838.641237083811,
839.511836401767,840.381583029608,841.251329657086,842.121076284176,842.990822910851,
843.860569537087,844.730316162863,845.600915478712,846.471514794314,847.341261418855,
848.211008042874,848.645881354683,849.080754666356,849.515627977891,849.950501289288,
850.82024791166,851.689994533462,852.124867844147,852.560593846263,852.996319848379,
853.431193158772,853.866066469019,854.300939779119,855.170686398875,855.605559708531,
856.040433018038,856.475306327397,856.910179636606,857.345052945667,857.77992625458,
858.214799563344,858.64967287196,859.084546180427,859.520272181434,859.95599818244,
860.390871490614,860.825744798641,861.260618106523,861.69549141426,862.130364721852,
862.565238029302,863.000111336609,863.434984643774,863.8698579508,864.304731257686,
864.739604564434,865.174477871045,865.609351177521,866.044224483863,866.479950483814,
866.915676483765,867.350549789843,867.785423095792,868.220296401613,868.655169707307,
869.090043012877,869.524916318325,869.959789623651,870.394662928858,870.829536233948,
871.264409538923,871.699282843785,872.134156148535,872.569029453177,873.003902757712,
873.439628756773,873.875354755834,874.310228060162,874.745101364389,875.179974668519,
875.614847972553,876.049721276495,876.484594580346,876.919467884108,877.354341187786,
877.78921449138,878.224087794893,878.658961098329,879.093834401689,879.528707704977,
879.963581008195,880.399307006616,880.835033005038,881.269906308124,881.704779611148,
882.139652914114,882.574526217024,883.00939951988,883.444272822685,883.879146125444,
884.314019428157,884.748892730829,885.183766033462,885.618639336059,886.053512638623,
886.488385941157,886.923259243664,887.358985241751,887.794711239839,888.2295845423,
888.664457844744,889.099331147173,889.534204449589,889.969077751997,890.403951054398,
890.838824356797,891.273697659195,891.708570961597,892.143444264004,892.578317566421,
893.01319086885,893.448064171293,893.882937473755,894.318663471843,894.75438946993,
895.189262772437,895.624136074971,896.059009377535,896.493882680132,896.928755982765,
897.363629285437,897.798502588151,898.233375890909,898.668249193715,899.103122496571,
899.53799579948,899.972869102446,900.40774240547,900.842615708556,901.278341706978,
901.714067705399,902.148941008617,902.583814311905,903.018687615265,903.453560918701,
903.888434222214,904.323307525808,904.758180829485,905.193054133248,905.627927437099,
906.06280074104,906.497674045075,906.932547349205,907.367420653433,907.80229395776,
908.238019956821,908.673745955883,909.108619260417,909.543492565059,909.978365869809,
910.413239174671,910.848112479646,911.282985784736,911.717859089943,912.152732395269,
912.587605700716,913.022479006287,913.457352311981,913.892225617802,914.327098923751,
914.761972229829,915.19769822978,915.633424229731,916.068297536072,916.503170842548,
916.93804414916,917.372917455908,917.807790762794,918.24266406982,918.677537376985,
919.112410684292,919.547283991742,919.982157299334,920.417030607071,920.851903914953,
921.28677722298,921.721650531154,922.15737653216,922.593102533167,923.027975841635,
923.46284915025,923.897722459014,924.332595767926,924.767469076987,925.202342386197,
925.637215695556,926.072089005063,926.506962314719,926.941835624523,927.376708934475,
927.811582244575,928.246455554822,928.681328865215,929.117054867331,929.987654180132,
930.422527490961,930.857400801934,931.292274113049,931.727147424306,932.162020735703,
932.596894047238,933.46664067072,934.336387294739,934.771260606945,935.20613391928,
935.641007231742,936.076733234882,936.94733255073,937.817079176507,938.686825802743,
939.556572429418,940.426319056508,941.296065683986,942.165812311827,943.036411629783,
943.907010947893,944.776757576505,945.646504205367,946.516250834443,947.385997463694,
948.25574409308,949.125490722558,949.996090041546,950.86668936054,951.736435990048,
952.606182619485,953.475929248809,954.345675877978,955.215422506951,956.085169135693,
956.955768453912,957.826367771985,958.696114399995,959.565861027658,960.435607654946,
961.305354281831,962.175100908289,963.044847534298,963.915446850328,964.786046166116,
965.655792790913,966.525539415195,966.960412727138,967.395286038947,968.265032662155,
969.134779284809,969.569652595924,970.004525906897,970.439399217726,970.875125219914,
971.310851222103,971.745724532643,972.615471153283,973.485217773335,973.920091083139,
974.354964392795,974.789837702302,975.22471101166,975.65958432087,976.094457629931,
976.529330938844,976.964204247608,977.399077556223,977.834803557303,978.270529558383,
978.705402866704,979.140276174877,979.575149482905,980.010022790786,980.444896098523,
980.879769406116,981.314642713565,981.749516020872,982.184389328038,982.619262635063,
983.05413594195,983.489009248698,983.923882555309,984.358755861785,984.794481861802,
985.230207861819,985.665081168029,986.099954474107,986.534827780056,986.969701085877,
987.404574391571,987.839447697141,988.274321002589,988.709194307915,989.144067613122,
989.578940918212,990.013814223187,990.448687528048,990.883560832799,991.31843413744,
991.754160136554,992.189886135667,992.624759440097,993.059632744425,993.494506048653,
993.929379352783,994.364252656817,994.799125960758,995.233999264609,995.668872568372,
996.103745872049,996.538619175643,996.973492479157,997.408365782593,997.843239085953,
998.278112389241,998.713838387696,999.149564386151,999.584437689301,1000.01931099239,
1000.45418429541,1000.88905759838,1001.32393090129,1001.75880420414,1002.19367750695,
1002.62855080971,1003.06342411242,1003.49829741509,1003.93317071773,1004.36804402032,
1004.80291732289,1005.23779062542,1005.67351662352,1006.10924262162,1006.5441159241,
1006.97898922656,1007.41386252901,1007.84873583144,1008.28360913385,1008.71848243626,
1009.15335573866,1009.58822904106,1010.02310234346,1010.45797564586,1010.89284894827,
1011.32772225069,1011.76259555311,1012.19746885556,1012.63319485364,1013.06892085171,
1013.5037941542,1013.9386674567,1014.37354075924,1014.8084140618,1015.2432873644,
1015.67816066703,1016.1130339697,1016.54790727242,1016.98278057517,1017.41765387798,
1017.85252718084,1018.28740048375,1018.72227378671,1019.15714708974,1019.59287308813,
1020.02859908651,1020.46347238967,1020.89834569288,1021.33321899617,1021.76809229953,
1022.20296560297,1022.63783890648,1023.07271221007,1023.50758551375,1023.94245881752,
1024.37733212137,1024.81220542531,1025.24707872935,1025.68195203348,1026.11682533771,
1026.55255133672,1026.98827733573,1027.42315064016,1027.8580239447,1028.29289724934,
1028.72777055409,1029.16264385896,1029.59751716393,1030.03239046902,1030.46726377423,
1030.90213707956,1031.33701038501,1031.77188369058,1032.20675699628,1032.6416303021,
1033.07650360805,1033.51222960793,1033.94795560782,1034.38282891403,1034.81770222038,
1035.25257552685,1035.68744883347,1036.12232214022,1036.5571954471,1036.99206875413,
1037.4269420613,1037.86181536861,1038.29668867606,1038.73156198365,1039.16643529139,
1039.60130859927,1040.0361819073,1040.47190790824,1040.90763390917,1041.34250721749,
1041.77738052596,1042.21225383458,1042.64712714334,1043.08200045226,1043.95174707053,
1044.38662037989,1044.8214936894,1045.25636699906,1045.69124030886,1046.12611361882,
1046.56098692892,1046.99586023917,1047.43158624121,1047.86731224325,1048.3021855538,
1048.73705886448,1049.17193217531,1049.60680548629,1050.0416787974,1050.47655210866,
1050.91142542006,1051.78117204327,1052.21604535508,1052.65091866703,1053.0857919791,
1053.52066529131,1053.95553860365,1054.39126460673,1055.26186392239,1056.13161054793,
1057.00135717395,1057.43623048712,1057.87110380041,1058.7408504273,1059.61059705459,
1060.48034368225,1061.35094300009,1062.22154231809,1063.09128894656,1063.96103557531,
1064.83078220429,1065.70052883346,1066.57027546278,1067.44002209222,1068.3106214112,
1069.18122073019,1070.05096735972,1070.9207139892,1071.79046061859,1072.66020724785,
1073.52995387693,1074.39970050579,1075.27029982411,1076.1408991423,1077.01064577048,
1077.88039239832,1078.7501390258,1079.61988565289,1080.48963227957,1081.35937890581,
1082.22997822202,1083.100577538,1083.97032416305,1084.84007078759,1085.70981741161,
1086.5795640351,1087.44931065803,1087.88418396929,1088.31905728041,1088.75393059138,
1089.18965659365,1089.62538259591,1090.06025590659,1090.93000252753,1091.36487583778,
1091.79974914788,1092.23462245783,1092.66949576764,1093.1043690773,1093.5392423868,
1093.97411569616,1094.40898900538,1094.84386231444,1095.27873562335,1095.71360893212,
1096.14933493327,1096.58506093443,1097.0199342429,1097.45480755122,1097.88968085939,
1098.32455416742,1098.75942747531,1099.19430078305,1099.62917409064,1100.06404739809,
1100.4989207054,1100.93379401257,1101.36866731959,1101.80354062648,1102.23841393323,
1102.67328723984,1103.10901323993,1103.54473924001,1103.97961254636,1104.41448585257,
1104.84935915865,1105.2842324646,1105.71910577042,1106.15397907612,1106.58885238169,
1107.02372568714,1107.45859899246,1107.89347229767,1108.32834560276,1108.76321890774,
1109.1980922126,1109.63296551736,1110.06869151652,1110.50441751569,1110.93929082023,
1111.37416412466,1111.80903742899,1112.24391073322,1112.67878403735,1113.11365734139,
1113.54853064533,1113.98340394918,1114.41827725295,1114.85315055662,1115.28802386022,
1115.72289716374,1116.15777046717,1116.59264377053,1117.02836976903,1117.46409576752,
1117.89896907074,1118.33384237389,1118.76871567698,1119.20358898,1119.63846228297,
1120.07333558588,1120.50820888874,1120.94308219154,1121.3779554943,1121.81282879702,
1122.24770209969,1122.68257540233,1123.11744870492,1123.55232200749,1123.98804800561,
1124.42377400372,1124.85864730623,1125.29352060871,1125.72839391118,1126.16326721362,
1126.59814051605,1127.03301381847,1127.46788712088,1127.90276042328,1128.33763372568,
1128.77250702808,1129.20738033048,1129.64225363289,1130.07712693531,1130.51200023774,
1130.94772623581,1131.38345223388,1131.81832553634,1132.25319883883,1132.68807214134,
1133.12294544387,1133.55781874644,1133.99269204904,1134.42756535167,1134.86243865434,
1135.29731195706,1135.73218525982,1136.16705856263,1136.60193186548,1137.03680516839,
1137.47167847136,1137.90740446972,1138.34313046808,1138.77800377117,1139.21287707432,
1139.64775037754,1140.08262368083,1140.51749698419,1140.95237028763,1141.38724359114,
1141.82211689474,1142.25699019842,1142.69186350218,1143.12673680603,1143.56161010998,
1143.99648341401,1144.43135671814,1144.86708271711,1145.30280871607,1145.7376820204,
1146.17255532483,1146.60742862936,1147.04230193401,1147.47717523876,1147.91204854362,
1148.3469218486,1148.78179515369,1149.2166684589,1149.65154176423,1150.08641506968,
1150.52128837525,1150.95616168094,1151.39103498677,1151.82676098659,1152.26248698641,
1152.69736029249,1153.1322335987,1153.56710690504,1154.00198021152,1154.43685351813,
1154.87172682488,1155.30660013177,1155.7414734388,1156.17634674597,1156.61122005327,
1157.04609336073,1157.48096666832,1157.91583997606,1158.35071328394,1158.7864392848,
1159.22216528566,1159.65703859384,1160.09191190216,1160.52678521063,1160.96165851925,
1161.39653182801,1161.83140513693,1162.26627844599,1162.7011517552,1163.13602506456,
1163.57089837407,1164.00577168373,1164.44064499353,1164.87551830349,1165.74611761556,
1166.18184361753,1166.61671692792,1167.05159023846,1167.48646354915,1167.92133685998,
1168.35621017096,1169.22595679333,1170.09570341627,1170.53057672794,1170.96545003975,
1171.4003233517,1171.83519666377,1172.27006997598,1172.705795979,1173.57639529447,
1174.44614191977,1174.8810152326,1175.31588854555,1176.18563517179,1177.05538179847,
1177.92512842556,1178.79487505304,1179.66547437075,1180.53607368863,1181.40582031696,
1182.27556694557,1183.14531357444,1184.01506020352,1184.88480683277,1185.75455346216,
1186.62515278112,1187.4957521001,1188.36549872963,1189.23524535914,1190.10499198858,
1190.97473861791,1191.84448524708,1192.71423187606,1193.58483119448,1194.45543051277,
1195.3251771411,1196.19492376911,1197.06467039678,1197.93441702407,1198.80416365096,
1199.67391027742,1200.5445095938,1201.41510890996,1202.28485553525,1203.15460216005,
1204.02434878434,1204.89409540809,1205.76384203131,1206.1987153427,1206.63358865396,
1207.06846196508,1207.50418796741,1208.37478728058,1209.2445339018,1209.6794072122,
1210.11428052245,1210.54915383255,1210.9840271425,1211.41890045231,1211.85377376197,
1212.28864707147,1212.72352038083,1213.15839369005,1213.59326699911,1214.02814030802,
1214.46386630925,1214.89959231048,1215.3344656191,1215.76933892757,1216.20421223589,
1216.63908554406,1217.07395885209,1217.50883215998,1217.94370546771,1218.37857877531,
1218.81345208276,1219.24832539007,1219.68319869724,1220.11807200426,1220.55294531115,
1220.9878186179,1221.42354461805,1221.85927061821,1222.29414392468,1222.72901723103,
1223.16389053724,1223.59876384332,1224.03363714927,1224.46851045509,1224.90338376079,
1225.33825706636,1225.77313037181,1226.20800367713,1226.64287698234,1227.07775028743,
1227.51262359241,1227.94749689727,1228.3832228965,1228.81894889572,1229.25382220036,
1229.6886955049,1230.12356880933,1230.55844211366,1230.99331541789,1231.42818872202,
1231.86306202606,1232.29793533,1232.73280863385,1233.16768193762,1233.60255524129,
1234.03742854489,1234.4723018484,1234.90717515184,1235.34290115037,1235.7786271489,
1236.21350045219,1236.64837375541,1237.08324705856,1237.51812036165,1237.95299366467,
1238.38786696764,1238.82274027055,1239.25761357341,1239.69248687621,1240.12736017897,
1240.56223348169,1240.99710678436,1241.431980087,1241.8668533896,1242.30257938773,
1242.73830538585,1243.17317868839,1243.6080519909,1244.04292529338,1244.47779859585,
1244.91267189829,1245.34754520072,1245.78241850314,1246.21729180555,1246.65216510795,
1247.08703841035,1247.52191171275,1247.95678501515,1248.39165831756,1248.82653161998,
1249.26225761804,1249.69798361611,1250.13285691855,1250.56773022101,1251.0026035235,
1251.43747682601,1251.87235012854,1252.30722343111,1252.74209673371,1253.17697003634,
1253.61184333901,1254.04671664173,1254.48158994449,1254.9164632473,1255.35133655015,
1255.78620985306,1256.22193585139,1256.65766184973,1257.09253515275,1257.52740845584,
1257.96228175899,1258.39715506221,1258.8320283655,1259.26690166886,1259.7017749723,
1260.13664827581,1260.57152157941,1261.00639488309,1261.44126818685,1261.8761414907,
1262.31101479465,1262.74588809868,1263.1816140976,1263.61734009651,1264.05221340074,
1264.48708670507,1264.9219600095,1265.35683331403,1265.79170661868,1266.22657992343,
1266.66145322829,1267.09632653327,1267.53119983836,1267.96607314357,1268.4009464489,
1268.83581975434,1269.27069305992,1269.70556636561,1270.14129236537,1270.57701836513,
1271.01189167108,1271.44676497716,1271.88163828337,1272.31651158971,1272.75138489619,
1273.1862582028,1273.62113150955,1274.05600481644,1274.49087812347,1274.92575143063,
1275.36062473794,1275.79549804539,1276.23037135299,1276.66524466073,1277.10097066151,
1277.5366966623,1277.97156997033,1278.40644327851,1278.84131658683,1279.2761898953,
1279.71106320392,1280.14593651268,1280.5808098216,1281.01568313066,1281.45055643987,
1281.88542974923,1282.32030305874,1282.75517636839,1283.1900496782,1283.62492298815,
1284.06064899005,1284.49637499195,1284.9312483022,1285.36612161259,1285.80099492313,
1286.23586823382,1286.67074154465,1287.54048816674,1287.975361478,1288.4102347894,
1288.84510810093,1289.27998141261,1289.71485472442,1290.14972803636,1291.02032735139,
1291.89092666668,1292.32579997914,1292.76067329173,1293.19554660444,1293.63041991727,
1294.50016654328,1295.36991316974,1296.23965979663,1297.10940642392,1297.9800057415,
1298.85060505925,1299.72035168742,1300.5900983159,1301.45984494464,1302.32959157362,
1303.19933820279,1304.06908483212,1304.93968415104,1305.81028347,1306.68003009953,
1307.54977672906,1308.41952335854,1309.28926998793,1310.15901661718,1311.02876324626,
1311.89936256477,1312.76996188316,1313.63970851164,1314.50945513981,1315.37920176765,
1316.24894839514,1317.11869502223,1317.98844164891,1318.85904096546,1319.72964028179,
1320.59938690733,1321.46913353238,1322.33888015692,1323.20862678095,1323.64350009276,
1324.07837340443,1324.51324671597,1324.94812002737,1325.81871934103,1326.68931865441,
1327.12419196524,1327.55906527593,1327.99393858647,1328.42881189686,1328.86368520711,
1329.29855851721,1329.73343182716,1330.16830513697,1330.60317844663,1331.03805175614,
1331.4729250655,1331.90779837471,1332.34267168377,1332.77839768507,1333.21412368638,
1333.64899699514,1334.08387030376,1334.51874361223,1334.95361692055,1335.38849022873,
1335.82336353676,1336.25823684464,1336.69311015238,1337.12798345997,1337.56285676742,
1337.99773007473,1338.4326033819,1338.86747668892,1339.30234999581,1339.73807599603,
1340.17380199625,1340.60867530287,1341.04354860934,1341.47842191569,1341.9132952219,
1342.34816852798,1342.78304183393,1343.21791513975,1343.65278844545,1344.08766175102,
1344.52253505647,1344.95740836179,1345.392281667,1345.82715497209,1346.26202827707,
1346.69775427635,1347.13348027563,1347.56835358038,1348.00322688502,1348.43810018956,
1348.87297349399,1349.30784679832,1349.74272010255,1350.17759340668,1350.61246671072,
1351.04734001466,1351.48221331851,1351.91708662228,1352.35195992595,1352.78683322955,
1353.22170653306,1353.65743253163,1354.09315853019,1354.52803183356,1354.96290513685,
1355.39777844007,1355.83265174322,1356.26752504631,1356.70239834933,1357.1372716523,
1357.57214495521,1358.00701825807,1358.44189156087,1358.87676486363,1359.31163816635,
1359.74651146902,1360.18138477166,1360.6171107698,1361.05283676795,1361.48771007051,
1361.92258337305,1362.35745667556,1362.79232997804,1363.2272032805,1363.66207658295,
1364.09694988538,1364.5318231878,1364.96669649021,1365.40156979261,1365.83644309501,
1366.27131639741,1366.70618969981,1367.14106300222,1367.57678900028,1368.01251499834,
1368.44738830077,1368.88226160321,1369.31713490567,1369.75200820816,1370.18688151067,
1370.6217548132,1371.05662811577,1371.49150141837,1371.926374721,1372.36124802367,
1372.79612132639,1373.23099462915,1373.66586793196,1374.10074123481,1374.53646723311,
1374.97219323142,1375.40706653438,1375.84193983741,1376.2768131405,1376.71168644365,
1377.14655974687,1377.58143305016,1378.01630635352,1378.45117965696,1378.88605296047,
1379.32092626407,1379.75579956775,1380.19067287151,1380.62554617536,1381.06041947931,
1381.49614547817,1381.93187147704,1382.36674478117,1382.8016180854,1383.23649138973,
1383.67136469416,1384.10623799869,1384.54111130334,1384.97598460809,1385.41085791295,
1385.84573121793,1386.28060452302,1386.71547782823,1387.15035113356,1387.585224439,
1388.02009774458,1388.45582374427,1388.89154974397,1389.32642304979,1389.76129635574,
1390.19616966182,1390.63104296803,1391.06591627437,1391.50078958085,1391.93566288746,
1392.37053619421,1392.8054095011,1393.24028280813,1393.6751561153,1394.1100294226,
1394.54490273005,1394.97977603765,1395.41550203836,1395.85122803908,1396.28610134696,
1396.72097465499,1397.15584796317,1397.59072127149,1398.02559457996,1398.46046788858,
1398.89534119734,1399.33021450626,1399.76508781532,1400.19996112453,1400.63483443389,
1401.50458105306,1401.93945436286,1402.37518036469,1402.81090636651,1403.24577967661,
1403.68065298686,1404.11552629725,1404.5503996078,1404.98527291848,1405.85501954029,
1406.2898928514,1406.72476616266,1407.15963947406,1407.5945127856,1408.02938609727,
1408.46425940908,1409.33485872391,1410.205458039,1410.64033135134,1411.07520466381,
1411.51007797639,1411.9449512891,1412.81469791488,1413.68444454112,1414.5541911678,
1415.42393779489,1416.29453711233,1417.16513642995,1418.03488305796,1418.90462968629,
1419.77437631491,1420.64412294377,1421.51386957285,1422.38361620211,1423.25421552099,
1424.12481483992,1424.99456146943,1425.86430809896,1426.73405472847,1427.60380135791,
1428.47354798724,1429.34329461641,1430.21389393501,1431.08449325349,1431.9542398821,
1432.82398651043,1433.69373313844,1434.56347976611,1435.4332263934,1436.30297302029,
1437.17357233701,1438.04417165351,1438.91391827929,1439.78366490459,1440.65341152939,
1441.52315815367,1441.95803146562,1442.39290477743,1442.8277780891,1443.26265140064,
1444.13325071451,1445.00385002811,1445.43872333908,1445.87359664991,1446.3084699606,
1446.74334327114,1447.17821658153,1447.61308989178,1448.48283651184,1448.91770982164,
1449.3525831313,1449.78745644081,1450.22232975017,1450.65720305938,1451.09292906076,
1451.52865506214,1451.96352837105,1452.39840167982,1452.83327498843,1453.2681482969,
1453.70302160522,1454.1378949134,1454.57276822143,1455.00764152931,1455.44251483705,
1455.87738814464,1456.31226145209,1456.7471347594,1457.18200806657,1457.6168813736,
1458.05260737389,1458.48833337418,1458.92320668093,1459.35807998754,1459.79295329402,
1460.22782660036,1460.66269990657,1461.09757321265,1461.5324465186,1461.96731982443,
1462.40219313012,1462.83706643569,1463.27193974114,1463.70681304647,1464.14168635168,
1464.57655965677,1465.0122856561,1465.44801165544,1465.8828849603,1466.31775826505,
1466.7526315697,1467.18750487423,1467.62237817866,1468.05725148299,1468.49212478722,
1468.92699809135,1469.36187139539,1469.79674469933,1470.23161800319,1470.66649130695,
1471.10136461063,1471.53623791422,1471.97196391283,1472.40768991143,1472.84256321487,
1473.27743651823,1473.71230982152,1474.14718312474,1474.58205642789,1475.01692973098,
1475.451803034,1475.88667633697,1476.32154963988,1476.75642294274,1477.19129624555,
1477.62616954831,1478.06104285102,1478.4959161537,1478.93164215186,1479.36736815002,
1479.80224145262,1480.23711475519,1480.67198805772,1481.10686136023,1481.54173466272,
1481.97660796518,1482.41148126762,1482.84635457005,1483.28122787247,1483.71610117488,
1484.15097447728,1484.58584777968,1485.02072108208,1485.45559438449,1485.89132038254,
1486.32704638059,1486.76191968301,1487.19679298544,1487.63166628788,1488.06653959035,
1488.50141289283,1488.93628619534,1489.37115949787,1489.80603280044,1490.24090610304,
1490.67577940567,1491.11065270835,1491.54552601106,1491.98039931382,1492.41527261663,
1492.8509986149,1493.28672461318,1493.72159791609,1494.15647121906,1494.59134452208,
1495.02621782517,1495.46109112832,1495.89596443154,1496.33083773483,1496.76571103819,
1497.20058434163,1497.63545764515,1498.07033094874,1498.50520425242,1498.94007755618,
1499.37495086004,1499.81067685885,1500.24640285767,1500.68127616171,1501.11614946584,
1501.55102277007,1501.9858960744,1502.42076937883,1502.85564268337,1503.29051598801,
1503.72538929276,1504.16026259762,1504.5951359026,1505.03000920769,1505.4648825129,
1505.89975581823,1506.33462912368,1506.77035512331,1507.20608112294,1507.64095442864,
1508.07582773446,1508.51070104041,1508.94557434649,1509.3804476527,1509.81532095904,
1510.25019426552,1510.68506757213,1511.11994087888,1511.55481418577,1511.9896874928,
1512.42456079996,1512.85943410727,1513.29430741472,1513.73003341537,1514.16575941601,
1514.60063272375,1515.03550603163,1515.47037933966,1515.90525264784,1516.34012595616,
1516.77499926463,1517.20987257325,1517.64474588201,1518.07961919093,1518.51449249999,
1518.9493658092,1519.38423911856,1519.81911242807,1520.25398573772,1520.68971173947,
1521.12543774122,1521.56031105118,1521.99518436128,1522.43005767153,1523.29980429246,
1523.73467760315,1524.16955091398,1524.60442422495,1525.03929753607,1525.47417084733,
1525.90904415873,1526.77879078194,1527.64939009657,1528.08511609939,1528.51998941146,
1528.95486272367,1529.38973603601,1530.25948266106,1531.1292292866,1531.99897591261,
1532.86872253907,1533.73846916596,1534.60906848325,1535.47966780073,1536.34941442858,
1537.21916105675,1538.08890768523,1538.95865431398,1539.82840094295,1540.69814757212,
1541.56874689096,1542.43934620985,1543.30909283933,1544.17883946886,1545.04858609839,
1545.91833272787,1546.78807935726,1547.65782598651,1548.52842530518,1549.39902462375,
1550.26877125249,1551.13851788097,1552.00826450914,1552.87801113699,1553.74775776447,
1554.61750439156,1555.48810370844,1556.35870302511,1557.22844965112,1558.09819627666,
1558.96794290171,1559.83768952626,1560.27256283834,1560.70743615028,1561.57718277377,
1562.44778208785,1563.31838140165,1563.75325471277,1564.18812802374,1564.62300133457,
1565.05787464526,1565.9276212662,1566.79736788655,1567.2322411965,1567.66711450631,
1568.10198781596,1568.53686112547,1568.97173443483,1569.40746043628,1569.84318643774,
1570.2780597468,1570.71293305571,1571.14780636448,1571.5826796731,1572.01755298157,
1572.45242628989,1572.88729959806,1573.32217290609,1573.75704621397,1574.19191952171,
1574.62679282931,1575.06166613676,1575.49653944407,1575.93141275123,1576.36713875159,
1576.80286475195,1577.23773805884,1577.67261136559,1578.1074846722,1578.54235797868,
1578.97723128502,1579.41210459124,1579.84697789732,1580.28185120327,1580.71672450909,
1581.15159781478,1581.58647112036,1582.0213444258,1582.45621773113,1582.89109103634,
1583.32681703573,1583.76254303513,1584.1974163401,1584.63228964497,1585.06716294972,
1585.50203625436,1585.9369095589,1586.37178286333,1586.80665616766,1587.24152947189,
1587.67640277602,1588.11127608005,1588.546149384,1588.98102268785,1589.41589599161,
1589.85076929529,1590.28649529394,1590.72222129258,1591.1570945961,1591.59196789953,
1592.0268412029,1592.46171450619,1592.8965878094,1593.33146111256,1593.76633441564,
1594.20120771867,1594.63608102164,1595.07095432455,1595.50582762741,1595.94070093021,
1596.37557423297,1596.81044753569,1597.24617353387,1597.68189953206,1598.11677283469,
1598.55164613729,1598.98651943985,1599.42139274239,1599.8562660449,1600.29113934738,
1600.72601264985,1601.16088595229,1601.59575925472,1602.03063255714,1602.46550585955,
1602.90037916195,1603.33525246435,1603.77012576675,1604.2058517648,1604.64157776285,
1605.07645106526,1605.51132436768,1605.94619767011,1606.38107097255,1606.81594427502,
1607.2508175775,1607.68569088001,1608.12056418254,1608.55543748511,1608.99031078771,
1609.42518409034,1609.86005739302,1610.29493069573,1610.72980399849,1611.16552999674,
1611.60125599499,1612.03612929785,1612.47100260076,1612.90587590373,1613.34074920675,
1613.77562250984,1614.21049581299,1614.64536911621,1615.0802424195,1615.51511572286,
1615.9499890263,1616.38486232981,1616.81973563341,1617.25460893709,1617.68948224085,
1618.12520823963,1618.5609342384,1618.99580754234,1619.43068084638,1619.86555415051,
1620.30042745474,1620.73530075907,1621.1701740635,1621.60504736804,1622.03992067268,
1622.47479397743,1622.90966728229,1623.34454058727,1623.77941389236,1624.21428719757,
1624.6491605029,1625.08488650247,1625.52061250204,1625.95548580761,1626.39035911331,
1626.82523241913,1627.26010572508,1627.69497903116,1628.12985233737,1628.56472564372,
1628.99959895019,1629.43447225681,1629.86934556356,1630.30421887044,1630.73909217747,
1631.17396548464,1631.60883879195,1632.04456479252,1632.48029079309,1632.91516410068,
1633.35003740842,1633.78491071631,1634.21978402433,1634.65465733251,1635.08953064083,
1635.5244039493,1635.95927725792,1636.39415056668,1636.8290238756,1637.26389718466,
1637.69877049387,1638.13364380323,1638.56851711274,1639.00424311442,1639.43996911609,
1639.8748424259,1640.30971573585,1640.74458904595,1641.6143356666,1642.04920897714,
1642.48408228782,1642.91895559865,1643.35382890963,1643.78870222074,1644.223575532,
1645.09332215494,1645.52819546661,1645.96392146936,1646.39964747212,1646.83452078406,
1647.26939409614,1647.70426740834,1648.57401403314,1649.44376065844,1650.31350728422,
1650.74838059729,1651.18325391046,1652.05300053714,1652.92359985428,1653.79419917162,
1654.66394579929,1655.5336924273,1656.40343905563,1657.27318568424,1658.14293231311,
1659.01267894219,1659.88327826096,1660.75387757982,1661.62362420926,1662.49337083877,
1663.3631174683,1664.23286409781,1665.10261072725,1665.97235735658,1666.84295667531,
1667.71355599396,1668.58330262282,1669.45304925143,1670.32279587976,1671.19254250778,
1672.06228913544,1672.93203576273,1673.80263507977,1674.6732343966,1675.54298102284,
1676.41272764862,1677.28247427392,1678.15222089872,1679.021967523,1679.89171414676,
1680.76231346105,1681.19803946366,1681.63291277506,1682.06778608632,1682.50265939743,
1682.93753270841,1683.37240601924,1684.24215264047,1684.67702595086,1685.11189926111,
1685.54677257121,1685.98164588116,1686.41651919097,1686.85139250063,1687.28626581014,
1687.72199181166,1688.15771781319,1688.5925911224,1689.02746443146,1689.46233774038,
1689.89721104914,1690.33208435776,1690.76695766623,1691.20183097455,1691.63670428272,
1692.07157759075,1692.50645089864,1692.94132420637,1693.37619751397,1693.81107082142,
1694.24594412873,1694.68167012916,1695.11739612959,1695.55226943662,1695.9871427435,
1696.42201605025,1696.85688935687,1697.29176266334,1697.72663596969,1698.1615092759,
1698.59638258198,1699.03125588793,1699.46612919375,1699.90100249945,1700.33587580502,
1700.77074911047,1701.20562241579,1701.64134841525,1702.0770744147,1702.51194771979,
1702.94682102476,1703.38169432963,1703.81656763438,1704.25144093902,1704.68631424356,
1705.12118754799,1705.55606085232,1705.99093415655,1706.42580746068,1706.86068076471,
1707.29555406866,1707.73042737251,1708.16530067627,1708.60102667496,1709.03675267365,
1709.47162597724,1709.90649928076,1710.34137258419,1710.77624588756,1711.21111919085,
1711.64599249406,1712.08086579722,1712.5157391003,1712.95061240333,1713.3854857063,
1713.82035900921,1714.25523231207,1714.69010561487,1715.12497891763,1715.56070491584,
1715.99643091404,1716.43130421671,1716.86617751935,1717.30105082195,1717.73592412451,
1718.17079742705,1718.60567072956,1719.04054403204,1719.4754173345,1719.91029063695,
1720.34516393938,1720.7800372418,1721.21491054421,1721.64978384661,1722.08465714901,
1722.52038314706,1722.9561091451,1723.39098244751,1723.82585574992,1724.26072905233,
1724.69560235476,1725.13047565721,1725.56534895967,1726.00022226216,1726.43509556467,
1726.8699688672,1727.30484216977,1727.73971547236,1728.174588775,1728.60946207767,
1729.04433538039,1729.48006137861,1729.91578737684,1730.35066067965,1730.78553398251,
1731.22040728542,1731.65528058838,1732.09015389141,1732.5250271945,1732.95990049765,
1733.39477380087,1733.82964710416,1734.26452040752,1734.69939371096,1735.13426701447,
1735.56914031807,1736.00401362175,1736.43973962048,1736.8754656192,1737.31033892306,
1737.745212227,1738.18008553104,1738.61495883517,1739.0498321394,1739.48470544373,
1739.91957874816,1740.35445205269,1740.78932535734,1741.22419866209,1741.65907196695,
1742.09394527193,1742.52881857702,1742.96369188223,1743.39941788174,1743.83514388125,
1744.2700171867,1744.70489049227,1745.13976379797,1745.57463710379,1746.00951040974,
1746.44438371582,1746.87925702203,1747.31413032837,1747.74900363485,1748.18387694146,
1748.61875024821,1749.0536235551,1749.48849686213,1749.92337016929,1750.3590961698,
1750.7948221703,1751.22969547775,1751.66456878534,1752.09944209308,1752.53431540096,
1752.96918870899,1753.40406201717,1753.83893532549,1754.27380863396,1754.70868194258,
1755.14355525134,1755.57842856026,1756.01330186932,1756.44817517853,1756.88304848789,
1757.31877448949,1757.75450049109,1758.18937380075,1759.05912042051,1759.49399373061,
1759.92886704086,1760.36374035125,1760.79861366179,1761.23348697248,1761.66836028331,
1762.10323359429,1762.5381069054,1763.40785352806,1763.8427268396,1764.27845284228,
1764.71417884496,1765.14905215677,1765.58392546872,1766.0187987808,1766.88854540534,
1767.75829203039,1768.1931653431,1768.62803865593,1769.06291196888,1769.49778528195,
1770.36753190841,1771.2381312254,1772.10873054259,1772.97847717007,1773.84822379791,
1774.71797042609,1775.58771705456,1776.45746368331,1777.32721031228,1778.19780963089,
1779.06840894783,1779.93815555508,1780.80790201176,1781.67764871408),(-0.58309518948453,
3.80976832182013E-10),.UNSPECIFIED.) ;
#824 = B_SPLINE_SURFACE_WITH_KNOTS('',3,1,((#57502,#57503),(#57504,#57505),
(#57506,#57507),(#57508,#57509),(#57510,#57511),(#57512,#57513),(#57514,
#57515),(#57516,#57517),(#57518,#57519),(#57520,#57521),(#57522,#57523),
(#57524,#57525),(#57526,#57527),(#57528,#57529),(#57530,#57531),(#57532,
#57533),(#57534,#57535),(#57536,#57537),(#57538,#57539),(#57540,#57541),
(#57542,#57543),(#57544,#57545),(#57546,#57547),(#57548,#57549),(#57550,
#57551),(#57552,#57553),(#57554,#57555),(#57556,#57557),(#57558,#57559),
(#57560,#57561),(#57562,#57563),(#57564,#57565),(#57566,#57567),(#57568,
#57569),(#57570,#57571),(#57572,#57573),(#57574,#57575),(#57576,#57577),
(#57578,#57579),(#57580,#57581),(#57582,#57583),(#57584,#57585),(#57586,
#57587),(#57588,#57589),(#57590,#57591),(#57592,#57593),(#57594,#57595),
(#57596,#57597),(#57598,#57599),(#57600,#57601),(#57602,#57603),(#57604,
#57605),(#57606,#57607),(#57608,#57609),(#57610,#57611),(#57612,#57613),
(#57614,#57615),(#57616,#57617),(#57618,#57619),(#57620,#57621),(#57622,
#57623),(#57624,#57625),(#57626,#57627),(#57628,#57629),(#57630,#57631),
(#57632,#57633),(#57634,#57635),(#57636,#57637),(#57638,#57639),(#57640,
#57641),(#57642,#57643),(#57644,#57645),(#57646,#57647),(#57648,#57649),
(#57650,#57651),(#57652,#57653),(#57654,#57655),(#57656,#57657),(#57658,
#57659),(#57660,#57661),(#57662,#57663),(#57664,#57665),(#57666,#57667),
(#57668,#57669),(#57670,#57671),(#57672,#57673),(#57674,#57675),(#57676,
#57677),(#57678,#57679),(#57680,#57681),(#57682,#57683),(#57684,#57685),
(#57686,#57687),(#57688,#57689),(#57690,#57691),(#57692,#57693),(#57694,
#57695),(#57696,#57697),(#57698,#57699),(#57700,#57701),(#57702,#57703),
(#57704,#57705),(#57706,#57707),(#57708,#57709),(#57710,#57711),(#57712,
#57713),(#57714,#57715),(#57716,#57717),(#57718,#57719),(#57720,#57721),
(#57722,#57723),(#57724,#57725),(#57726,#57727),(#57728,#57729),(#57730,
#57731),(#57732,#57733),(#57734,#57735),(#57736,#57737),(#57738,#57739),
(#57740,#57741),(#57742,#57743),(#57744,#57745),(#57746,#57747),(#57748,
#57749),(#57750,#57751),(#57752,#57753),(#57754,#57755),(#57756,#57757),
(#57758,#57759),(#57760,#57761),(#57762,#57763),(#57764,#57765),(#57766,
#57767),(#57768,#57769),(#57770,#57771),(#57772,#57773),(#57774,#57775),
(#57776,#57777),(#57778,#57779),(#57780,#57781),(#57782,#57783),(#57784,
#57785),(#57786,#57787),(#57788,#57789),(#57790,#57791),(#57792,#57793),
(#57794,#57795),(#57796,#57797),(#57798,#57799),(#57800,#57801),(#57802,
#57803),(#57804,#57805),(#57806,#57807),(#57808,#57809),(#57810,#57811),
(#57812,#57813),(#57814,#57815),(#57816,#57817),(#57818,#57819),(#57820,
#57821),(#57822,#57823),(#57824,#57825),(#57826,#57827),(#57828,#57829),
(#57830,#57831),(#57832,#57833),(#57834,#57835),(#57836,#57837),(#57838,
#57839),(#57840,#57841),(#57842,#57843),(#57844,#57845),(#57846,#57847),
(#57848,#57849),(#57850,#57851),(#57852,#57853),(#57854,#57855),(#57856,
#57857),(#57858,#57859),(#57860,#57861),(#57862,#57863),(#57864,#57865),
(#57866,#57867),(#57868,#57869),(#57870,#57871),(#57872,#57873),(#57874,
#57875),(#57876,#57877),(#57878,#57879),(#57880,#57881),(#57882,#57883),
(#57884,#57885),(#57886,#57887),(#57888,#57889),(#57890,#57891),(#57892,
#57893),(#57894,#57895),(#57896,#57897),(#57898,#57899),(#57900,#57901),
(#57902,#57903),(#57904,#57905),(#57906,#57907),(#57908,#57909),(#57910,
#57911),(#57912,#57913),(#57914,#57915),(#57916,#57917),(#57918,#57919),
(#57920,#57921),(#57922,#57923),(#57924,#57925),(#57926,#57927),(#57928,
#57929),(#57930,#57931),(#57932,#57933),(#57934,#57935),(#57936,#57937),
(#57938,#57939),(#57940,#57941),(#57942,#57943),(#57944,#57945),(#57946,
#57947),(#57948,#57949),(#57950,#57951),(#57952,#57953),(#57954,#57955),
(#57956,#57957),(#57958,#57959),(#57960,#57961),(#57962,#57963),(#57964,
#57965),(#57966,#57967),(#57968,#57969),(#57970,#57971),(#57972,#57973),
(#57974,#57975),(#57976,#57977),(#57978,#57979),(#57980,#57981),(#57982,
#57983),(#57984,#57985),(#57986,#57987),(#57988,#57989),(#57990,#57991),
(#57992,#57993),(#57994,#57995),(#57996,#57997),(#57998,#57999),(#58000,
#58001),(#58002,#58003),(#58004,#58005),(#58006,#58007),(#58008,#58009),
(#58010,#58011),(#58012,#58013),(#58014,#58015),(#58016,#58017),(#58018,
#58019),(#58020,#58021),(#58022,#58023),(#58024,#58025),(#58026,#58027),
(#58028,#58029),(#58030,#58031),(#58032,#58033),(#58034,#58035),(#58036,
#58037),(#58038,#58039),(#58040,#58041),(#58042,#58043),(#58044,#58045),
(#58046,#58047),(#58048,#58049),(#58050,#58051),(#58052,#58053),(#58054,
#58055),(#58056,#58057),(#58058,#58059),(#58060,#58061),(#58062,#58063),
(#58064,#58065),(#58066,#58067),(#58068,#58069),(#58070,#58071),(#58072,
#58073),(#58074,#58075),(#58076,#58077),(#58078,#58079),(#58080,#58081),
(#58082,#58083),(#58084,#58085),(#58086,#58087),(#58088,#58089),(#58090,
#58091),(#58092,#58093),(#58094,#58095),(#58096,#58097),(#58098,#58099),
(#58100,#58101),(#58102,#58103),(#58104,#58105),(#58106,#58107),(#58108,
#58109),(#58110,#58111),(#58112,#58113),(#58114,#58115),(#58116,#58117),
(#58118,#58119),(#58120,#58121),(#58122,#58123),(#58124,#58125),(#58126,
#58127),(#58128,#58129),(#58130,#58131),(#58132,#58133),(#58134,#58135),
(#58136,#58137),(#58138,#58139),(#58140,#58141),(#58142,#58143),(#58144,
#58145),(#58146,#58147),(#58148,#58149),(#58150,#58151),(#58152,#58153),
(#58154,#58155),(#58156,#58157),(#58158,#58159),(#58160,#58161),(#58162,
#58163),(#58164,#58165),(#58166,#58167),(#58168,#58169),(#58170,#58171),
(#58172,#58173),(#58174,#58175),(#58176,#58177),(#58178,#58179),(#58180,
#58181),(#58182,#58183),(#58184,#58185),(#58186,#58187),(#58188,#58189),
(#58190,#58191),(#58192,#58193),(#58194,#58195),(#58196,#58197),(#58198,
#58199),(#58200,#58201),(#58202,#58203),(#58204,#58205),(#58206,#58207),
(#58208,#58209),(#58210,#58211),(#58212,#58213),(#58214,#58215),(#58216,
#58217),(#58218,#58219),(#58220,#58221),(#58222,#58223),(#58224,#58225),
(#58226,#58227),(#58228,#58229),(#58230,#58231),(#58232,#58233),(#58234,
#58235),(#58236,#58237),(#58238,#58239),(#58240,#58241),(#58242,#58243),
(#58244,#58245),(#58246,#58247),(#58248,#58249),(#58250,#58251),(#58252,
#58253),(#58254,#58255),(#58256,#58257),(#58258,#58259),(#58260,#58261),
(#58262,#58263),(#58264,#58265),(#58266,#58267),(#58268,#58269),(#58270,
#58271),(#58272,#58273),(#58274,#58275),(#58276,#58277),(#58278,#58279),
(#58280,#58281),(#58282,#58283),(#58284,#58285),(#58286,#58287),(#58288,
#58289),(#58290,#58291),(#58292,#58293),(#58294,#58295),(#58296,#58297),
(#58298,#58299),(#58300,#58301),(#58302,#58303),(#58304,#58305),(#58306,
#58307),(#58308,#58309),(#58310,#58311),(#58312,#58313),(#58314,#58315),
(#58316,#58317),(#58318,#58319),(#58320,#58321),(#58322,#58323),(#58324,
#58325),(#58326,#58327),(#58328,#58329),(#58330,#58331),(#58332,#58333),
(#58334,#58335),(#58336,#58337),(#58338,#58339),(#58340,#58341),(#58342,
#58343),(#58344,#58345),(#58346,#58347),(#58348,#58349),(#58350,#58351),
(#58352,#58353),(#58354,#58355),(#58356,#58357),(#58358,#58359),(#58360,
#58361),(#58362,#58363),(#58364,#58365),(#58366,#58367),(#58368,#58369),
(#58370,#58371),(#58372,#58373),(#58374,#58375),(#58376,#58377),(#58378,
#58379),(#58380,#58381),(#58382,#58383),(#58384,#58385),(#58386,#58387),
(#58388,#58389),(#58390,#58391),(#58392,#58393),(#58394,#58395),(#58396,
#58397),(#58398,#58399),(#58400,#58401),(#58402,#58403),(#58404,#58405),
(#58406,#58407),(#58408,#58409),(#58410,#58411),(#58412,#58413),(#58414,
#58415),(#58416,#58417),(#58418,#58419),(#58420,#58421),(#58422,#58423),
(#58424,#58425),(#58426,#58427),(#58428,#58429),(#58430,#58431),(#58432,
#58433),(#58434,#58435),(#58436,#58437),(#58438,#58439),(#58440,#58441),
(#58442,#58443),(#58444,#58445),(#58446,#58447),(#58448,#58449),(#58450,
#58451),(#58452,#58453),(#58454,#58455),(#58456,#58457),(#58458,#58459),
(#58460,#58461),(#58462,#58463),(#58464,#58465),(#58466,#58467),(#58468,
#58469),(#58470,#58471),(#58472,#58473),(#58474,#58475),(#58476,#58477),
(#58478,#58479),(#58480,#58481),(#58482,#58483),(#58484,#58485),(#58486,
#58487),(#58488,#58489),(#58490,#58491),(#58492,#58493),(#58494,#58495),
(#58496,#58497),(#58498,#58499),(#58500,#58501),(#58502,#58503),(#58504,
#58505),(#58506,#58507),(#58508,#58509),(#58510,#58511),(#58512,#58513),
(#58514,#58515),(#58516,#58517),(#58518,#58519),(#58520,#58521),(#58522,
#58523),(#58524,#58525),(#58526,#58527),(#58528,#58529),(#58530,#58531),
(#58532,#58533),(#58534,#58535),(#58536,#58537),(#58538,#58539),(#58540,
#58541),(#58542,#58543),(#58544,#58545),(#58546,#58547),(#58548,#58549),
(#58550,#58551),(#58552,#58553),(#58554,#58555),(#58556,#58557),(#58558,
#58559),(#58560,#58561),(#58562,#58563),(#58564,#58565),(#58566,#58567),
(#58568,#58569),(#58570,#58571),(#58572,#58573),(#58574,#58575),(#58576,
#58577),(#58578,#58579),(#58580,#58581),(#58582,#58583),(#58584,#58585),
(#58586,#58587),(#58588,#58589),(#58590,#58591),(#58592,#58593),(#58594,
#58595),(#58596,#58597),(#58598,#58599),(#58600,#58601),(#58602,#58603),
(#58604,#58605),(#58606,#58607),(#58608,#58609),(#58610,#58611),(#58612,
#58613),(#58614,#58615),(#58616,#58617),(#58618,#58619),(#58620,#58621),
(#58622,#58623),(#58624,#58625),(#58626,#58627),(#58628,#58629),(#58630,
#58631),(#58632,#58633),(#58634,#58635),(#58636,#58637),(#58638,#58639),
(#58640,#58641),(#58642,#58643),(#58644,#58645),(#58646,#58647),(#58648,
#58649),(#58650,#58651),(#58652,#58653),(#58654,#58655),(#58656,#58657),
(#58658,#58659),(#58660,#58661),(#58662,#58663),(#58664,#58665),(#58666,
#58667),(#58668,#58669),(#58670,#58671),(#58672,#58673),(#58674,#58675),
(#58676,#58677),(#58678,#58679),(#58680,#58681),(#58682,#58683),(#58684,
#58685),(#58686,#58687),(#58688,#58689),(#58690,#58691),(#58692,#58693),
(#58694,#58695),(#58696,#58697),(#58698,#58699),(#58700,#58701),(#58702,
#58703),(#58704,#58705),(#58706,#58707),(#58708,#58709),(#58710,#58711),
(#58712,#58713),(#58714,#58715),(#58716,#58717),(#58718,#58719),(#58720,
#58721),(#58722,#58723),(#58724,#58725),(#58726,#58727),(#58728,#58729),
(#58730,#58731),(#58732,#58733),(#58734,#58735),(#58736,#58737),(#58738,
#58739),(#58740,#58741),(#58742,#58743),(#58744,#58745),(#58746,#58747),
(#58748,#58749),(#58750,#58751),(#58752,#58753),(#58754,#58755),(#58756,
#58757),(#58758,#58759),(#58760,#58761),(#58762,#58763),(#58764,#58765),
(#58766,#58767),(#58768,#58769),(#58770,#58771),(#58772,#58773),(#58774,
#58775),(#58776,#58777),(#58778,#58779),(#58780,#58781),(#58782,#58783),
(#58784,#58785),(#58786,#58787),(#58788,#58789),(#58790,#58791),(#58792,
#58793),(#58794,#58795),(#58796,#58797),(#58798,#58799),(#58800,#58801),
(#58802,#58803),(#58804,#58805),(#58806,#58807),(#58808,#58809),(#58810,
#58811),(#58812,#58813),(#58814,#58815),(#58816,#58817),(#58818,#58819),
(#58820,#58821),(#58822,#58823),(#58824,#58825),(#58826,#58827),(#58828,
#58829),(#58830,#58831),(#58832,#58833),(#58834,#58835),(#58836,#58837),
(#58838,#58839),(#58840,#58841),(#58842,#58843),(#58844,#58845),(#58846,
#58847),(#58848,#58849),(#58850,#58851),(#58852,#58853),(#58854,#58855),
(#58856,#58857),(#58858,#58859),(#58860,#58861),(#58862,#58863),(#58864,
#58865),(#58866,#58867),(#58868,#58869),(#58870,#58871),(#58872,#58873),
(#58874,#58875),(#58876,#58877),(#58878,#58879),(#58880,#58881),(#58882,
#58883),(#58884,#58885),(#58886,#58887),(#58888,#58889),(#58890,#58891),
(#58892,#58893),(#58894,#58895),(#58896,#58897),(#58898,#58899),(#58900,
#58901),(#58902,#58903),(#58904,#58905),(#58906,#58907),(#58908,#58909),
(#58910,#58911),(#58912,#58913),(#58914,#58915),(#58916,#58917),(#58918,
#58919),(#58920,#58921),(#58922,#58923),(#58924,#58925),(#58926,#58927),
(#58928,#58929),(#58930,#58931),(#58932,#58933),(#58934,#58935),(#58936,
#58937),(#58938,#58939),(#58940,#58941),(#58942,#58943),(#58944,#58945),
(#58946,#58947),(#58948,#58949),(#58950,#58951),(#58952,#58953),(#58954,
#58955),(#58956,#58957),(#58958,#58959),(#58960,#58961),(#58962,#58963),
(#58964,#58965),(#58966,#58967),(#58968,#58969),(#58970,#58971),(#58972,
#58973),(#58974,#58975),(#58976,#58977),(#58978,#58979),(#58980,#58981),
(#58982,#58983),(#58984,#58985),(#58986,#58987),(#58988,#58989),(#58990,
#58991),(#58992,#58993),(#58994,#58995),(#58996,#58997),(#58998,#58999),
(#59000,#59001),(#59002,#59003),(#59004,#59005),(#59006,#59007),(#59008,
#59009),(#59010,#59011),(#59012,#59013),(#59014,#59015),(#59016,#59017),
(#59018,#59019),(#59020,#59021),(#59022,#59023),(#59024,#59025),(#59026,
#59027),(#59028,#59029),(#59030,#59031),(#59032,#59033),(#59034,#59035),
(#59036,#59037),(#59038,#59039),(#59040,#59041),(#59042,#59043),(#59044,
#59045),(#59046,#59047),(#59048,#59049),(#59050,#59051),(#59052,#59053),
(#59054,#59055),(#59056,#59057),(#59058,#59059),(#59060,#59061),(#59062,
#59063),(#59064,#59065),(#59066,#59067),(#59068,#59069),(#59070,#59071),
(#59072,#59073),(#59074,#59075),(#59076,#59077),(#59078,#59079),(#59080,
#59081),(#59082,#59083),(#59084,#59085),(#59086,#59087),(#59088,#59089),
(#59090,#59091),(#59092,#59093),(#59094,#59095),(#59096,#59097),(#59098,
#59099),(#59100,#59101),(#59102,#59103),(#59104,#59105),(#59106,#59107),
(#59108,#59109),(#59110,#59111),(#59112,#59113),(#59114,#59115),(#59116,
#59117),(#59118,#59119),(#59120,#59121),(#59122,#59123),(#59124,#59125),
(#59126,#59127),(#59128,#59129),(#59130,#59131),(#59132,#59133),(#59134,
#59135),(#59136,#59137),(#59138,#59139),(#59140,#59141),(#59142,#59143),
(#59144,#59145),(#59146,#59147),(#59148,#59149),(#59150,#59151),(#59152,
#59153),(#59154,#59155),(#59156,#59157),(#59158,#59159),(#59160,#59161),
(#59162,#59163),(#59164,#59165),(#59166,#59167),(#59168,#59169),(#59170,
#59171),(#59172,#59173),(#59174,#59175),(#59176,#59177),(#59178,#59179),
(#59180,#59181),(#59182,#59183),(#59184,#59185),(#59186,#59187),(#59188,
#59189),(#59190,#59191),(#59192,#59193),(#59194,#59195),(#59196,#59197),
(#59198,#59199),(#59200,#59201),(#59202,#59203),(#59204,#59205),(#59206,
#59207),(#59208,#59209),(#59210,#59211),(#59212,#59213),(#59214,#59215),
(#59216,#59217),(#59218,#59219),(#59220,#59221),(#59222,#59223),(#59224,
#59225),(#59226,#59227),(#59228,#59229),(#59230,#59231),(#59232,#59233),
(#59234,#59235),(#59236,#59237),(#59238,#59239),(#59240,#59241),(#59242,
#59243),(#59244,#59245),(#59246,#59247),(#59248,#59249),(#59250,#59251),
(#59252,#59253),(#59254,#59255),(#59256,#59257),(#59258,#59259),(#59260,
#59261),(#59262,#59263),(#59264,#59265),(#59266,#59267),(#59268,#59269),
(#59270,#59271),(#59272,#59273),(#59274,#59275),(#59276,#59277),(#59278,
#59279),(#59280,#59281),(#59282,#59283),(#59284,#59285),(#59286,#59287),
(#59288,#59289),(#59290,#59291),(#59292,#59293),(#59294,#59295),(#59296,
#59297),(#59298,#59299),(#59300,#59301),(#59302,#59303),(#59304,#59305),
(#59306,#59307),(#59308,#59309),(#59310,#59311),(#59312,#59313),(#59314,
#59315),(#59316,#59317),(#59318,#59319),(#59320,#59321),(#59322,#59323),
(#59324,#59325),(#59326,#59327),(#59328,#59329),(#59330,#59331),(#59332,
#59333),(#59334,#59335),(#59336,#59337),(#59338,#59339),(#59340,#59341),
(#59342,#59343),(#59344,#59345),(#59346,#59347),(#59348,#59349),(#59350,
#59351),(#59352,#59353),(#59354,#59355),(#59356,#59357),(#59358,#59359),
(#59360,#59361),(#59362,#59363),(#59364,#59365),(#59366,#59367),(#59368,
#59369),(#59370,#59371),(#59372,#59373),(#59374,#59375),(#59376,#59377),
(#59378,#59379),(#59380,#59381),(#59382,#59383),(#59384,#59385),(#59386,
#59387),(#59388,#59389),(#59390,#59391),(#59392,#59393),(#59394,#59395),
(#59396,#59397),(#59398,#59399),(#59400,#59401),(#59402,#59403),(#59404,
#59405),(#59406,#59407),(#59408,#59409),(#59410,#59411),(#59412,#59413),
(#59414,#59415),(#59416,#59417),(#59418,#59419),(#59420,#59421),(#59422,
#59423),(#59424,#59425),(#59426,#59427),(#59428,#59429),(#59430,#59431),
(#59432,#59433),(#59434,#59435),(#59436,#59437),(#59438,#59439),(#59440,
#59441),(#59442,#59443),(#59444,#59445),(#59446,#59447),(#59448,#59449),
(#59450,#59451),(#59452,#59453),(#59454,#59455),(#59456,#59457),(#59458,
#59459),(#59460,#59461),(#59462,#59463),(#59464,#59465),(#59466,#59467),
(#59468,#59469),(#59470,#59471),(#59472,#59473),(#59474,#59475),(#59476,
#59477),(#59478,#59479),(#59480,#59481),(#59482,#59483),(#59484,#59485),
(#59486,#59487),(#59488,#59489),(#59490,#59491),(#59492,#59493),(#59494,
#59495),(#59496,#59497),(#59498,#59499),(#59500,#59501),(#59502,#59503),
(#59504,#59505),(#59506,#59507),(#59508,#59509),(#59510,#59511),(#59512,
#59513),(#59514,#59515),(#59516,#59517),(#59518,#59519),(#59520,#59521),
(#59522,#59523),(#59524,#59525),(#59526,#59527),(#59528,#59529),(#59530,
#59531),(#59532,#59533),(#59534,#59535),(#59536,#59537),(#59538,#59539),
(#59540,#59541),(#59542,#59543),(#59544,#59545),(#59546,#59547),(#59548,
#59549),(#59550,#59551),(#59552,#59553),(#59554,#59555),(#59556,#59557),
(#59558,#59559),(#59560,#59561),(#59562,#59563),(#59564,#59565),(#59566,
#59567),(#59568,#59569),(#59570,#59571),(#59572,#59573),(#59574,#59575),
(#59576,#59577),(#59578,#59579),(#59580,#59581),(#59582,#59583),(#59584,
#59585),(#59586,#59587),(#59588,#59589),(#59590,#59591),(#59592,#59593),
(#59594,#59595),(#59596,#59597),(#59598,#59599),(#59600,#59601),(#59602,
#59603),(#59604,#59605),(#59606,#59607),(#59608,#59609),(#59610,#59611),
(#59612,#59613),(#59614,#59615),(#59616,#59617),(#59618,#59619),(#59620,
#59621),(#59622,#59623),(#59624,#59625),(#59626,#59627),(#59628,#59629),
(#59630,#59631),(#59632,#59633),(#59634,#59635),(#59636,#59637),(#59638,
#59639),(#59640,#59641),(#59642,#59643),(#59644,#59645),(#59646,#59647),
(#59648,#59649),(#59650,#59651),(#59652,#59653),(#59654,#59655),(#59656,
#59657),(#59658,#59659),(#59660,#59661),(#59662,#59663),(#59664,#59665),
(#59666,#59667),(#59668,#59669),(#59670,#59671),(#59672,#59673),(#59674,
#59675),(#59676,#59677),(#59678,#59679),(#59680,#59681),(#59682,#59683),
(#59684,#59685),(#59686,#59687),(#59688,#59689),(#59690,#59691),(#59692,
#59693),(#59694,#59695),(#59696,#59697),(#59698,#59699),(#59700,#59701),
(#59702,#59703),(#59704,#59705),(#59706,#59707),(#59708,#59709),(#59710,
#59711),(#59712,#59713),(#59714,#59715),(#59716,#59717),(#59718,#59719),
(#59720,#59721),(#59722,#59723),(#59724,#59725),(#59726,#59727),(#59728,
#59729),(#59730,#59731),(#59732,#59733),(#59734,#59735),(#59736,#59737),
(#59738,#59739),(#59740,#59741),(#59742,#59743),(#59744,#59745),(#59746,
#59747),(#59748,#59749),(#59750,#59751),(#59752,#59753),(#59754,#59755),
(#59756,#59757),(#59758,#59759),(#59760,#59761),(#59762,#59763),(#59764,
#59765),(#59766,#59767),(#59768,#59769),(#59770,#59771),(#59772,#59773),
(#59774,#59775),(#59776,#59777),(#59778,#59779),(#59780,#59781),(#59782,
#59783),(#59784,#59785),(#59786,#59787),(#59788,#59789),(#59790,#59791),
(#59792,#59793),(#59794,#59795),(#59796,#59797),(#59798,#59799),(#59800,
#59801),(#59802,#59803),(#59804,#59805),(#59806,#59807),(#59808,#59809),
(#59810,#59811),(#59812,#59813),(#59814,#59815),(#59816,#59817),(#59818,
#59819),(#59820,#59821),(#59822,#59823),(#59824,#59825),(#59826,#59827),
(#59828,#59829),(#59830,#59831),(#59832,#59833),(#59834,#59835),(#59836,
#59837),(#59838,#59839),(#59840,#59841),(#59842,#59843),(#59844,#59845),
(#59846,#59847),(#59848,#59849),(#59850,#59851),(#59852,#59853),(#59854,
#59855),(#59856,#59857),(#59858,#59859),(#59860,#59861),(#59862,#59863),
(#59864,#59865),(#59866,#59867),(#59868,#59869),(#59870,#59871),(#59872,
#59873),(#59874,#59875),(#59876,#59877),(#59878,#59879),(#59880,#59881),
(#59882,#59883),(#59884,#59885),(#59886,#59887),(#59888,#59889),(#59890,
#59891),(#59892,#59893),(#59894,#59895),(#59896,#59897),(#59898,#59899),
(#59900,#59901),(#59902,#59903),(#59904,#59905),(#59906,#59907),(#59908,
#59909),(#59910,#59911),(#59912,#59913),(#59914,#59915),(#59916,#59917),
(#59918,#59919),(#59920,#59921),(#59922,#59923),(#59924,#59925),(#59926,
#59927),(#59928,#59929),(#59930,#59931),(#59932,#59933),(#59934,#59935),
(#59936,#59937),(#59938,#59939),(#59940,#59941),(#59942,#59943),(#59944,
#59945),(#59946,#59947),(#59948,#59949),(#59950,#59951),(#59952,#59953),
(#59954,#59955),(#59956,#59957),(#59958,#59959),(#59960,#59961),(#59962,
#59963),(#59964,#59965),(#59966,#59967),(#59968,#59969),(#59970,#59971),
(#59972,#59973),(#59974,#59975),(#59976,#59977),(#59978,#59979),(#59980,
#59981),(#59982,#59983),(#59984,#59985),(#59986,#59987),(#59988,#59989),
(#59990,#59991),(#59992,#59993),(#59994,#59995),(#59996,#59997),(#59998,
#59999),(#60000,#60001),(#60002,#60003),(#60004,#60005),(#60006,#60007),
(#60008,#60009),(#60010,#60011),(#60012,#60013),(#60014,#60015),(#60016,
#60017),(#60018,#60019),(#60020,#60021),(#60022,#60023),(#60024,#60025),
(#60026,#60027),(#60028,#60029),(#60030,#60031),(#60032,#60033),(#60034,
#60035),(#60036,#60037),(#60038,#60039),(#60040,#60041),(#60042,#60043),
(#60044,#60045),(#60046,#60047),(#60048,#60049),(#60050,#60051),(#60052,
#60053),(#60054,#60055),(#60056,#60057),(#60058,#60059),(#60060,#60061),
(#60062,#60063),(#60064,#60065),(#60066,#60067),(#60068,#60069),(#60070,
#60071),(#60072,#60073),(#60074,#60075),(#60076,#60077),(#60078,#60079),
(#60080,#60081),(#60082,#60083),(#60084,#60085),(#60086,#60087),(#60088,
#60089),(#60090,#60091),(#60092,#60093),(#60094,#60095),(#60096,#60097),
(#60098,#60099),(#60100,#60101),(#60102,#60103),(#60104,#60105),(#60106,
#60107),(#60108,#60109),(#60110,#60111),(#60112,#60113),(#60114,#60115),
(#60116,#60117),(#60118,#60119),(#60120,#60121),(#60122,#60123),(#60124,
#60125),(#60126,#60127),(#60128,#60129),(#60130,#60131),(#60132,#60133),
(#60134,#60135),(#60136,#60137),(#60138,#60139),(#60140,#60141),(#60142,
#60143),(#60144,#60145),(#60146,#60147),(#60148,#60149),(#60150,#60151),
(#60152,#60153),(#60154,#60155),(#60156,#60157),(#60158,#60159),(#60160,
#60161),(#60162,#60163),(#60164,#60165),(#60166,#60167),(#60168,#60169),
(#60170,#60171),(#60172,#60173),(#60174,#60175),(#60176,#60177),(#60178,
#60179),(#60180,#60181),(#60182,#60183),(#60184,#60185),(#60186,#60187),
(#60188,#60189),(#60190,#60191),(#60192,#60193),(#60194,#60195),(#60196,
#60197),(#60198,#60199),(#60200,#60201),(#60202,#60203),(#60204,#60205),
(#60206,#60207),(#60208,#60209),(#60210,#60211),(#60212,#60213),(#60214,
#60215),(#60216,#60217),(#60218,#60219),(#60220,#60221),(#60222,#60223),
(#60224,#60225),(#60226,#60227),(#60228,#60229),(#60230,#60231),(#60232,
#60233),(#60234,#60235),(#60236,#60237),(#60238,#60239),(#60240,#60241),
(#60242,#60243),(#60244,#60245),(#60246,#60247),(#60248,#60249),(#60250,
#60251),(#60252,#60253),(#60254,#60255),(#60256,#60257),(#60258,#60259),
(#60260,#60261),(#60262,#60263),(#60264,#60265),(#60266,#60267),(#60268,
#60269),(#60270,#60271),(#60272,#60273),(#60274,#60275),(#60276,#60277),
(#60278,#60279),(#60280,#60281),(#60282,#60283),(#60284,#60285),(#60286,
#60287),(#60288,#60289),(#60290,#60291),(#60292,#60293),(#60294,#60295),
(#60296,#60297),(#60298,#60299),(#60300,#60301),(#60302,#60303),(#60304,
#60305),(#60306,#60307),(#60308,#60309),(#60310,#60311),(#60312,#60313),
(#60314,#60315),(#60316,#60317),(#60318,#60319),(#60320,#60321),(#60322,
#60323),(#60324,#60325),(#60326,#60327),(#60328,#60329),(#60330,#60331),
(#60332,#60333),(#60334,#60335),(#60336,#60337),(#60338,#60339),(#60340,
#60341),(#60342,#60343),(#60344,#60345),(#60346,#60347),(#60348,#60349),
(#60350,#60351),(#60352,#60353),(#60354,#60355),(#60356,#60357),(#60358,
#60359),(#60360,#60361),(#60362,#60363),(#60364,#60365),(#60366,#60367),
(#60368,#60369),(#60370,#60371),(#60372,#60373),(#60374,#60375),(#60376,
#60377),(#60378,#60379),(#60380,#60381),(#60382,#60383),(#60384,#60385),
(#60386,#60387),(#60388,#60389),(#60390,#60391),(#60392,#60393),(#60394,
#60395),(#60396,#60397),(#60398,#60399),(#60400,#60401),(#60402,#60403),
(#60404,#60405),(#60406,#60407),(#60408,#60409),(#60410,#60411),(#60412,
#60413),(#60414,#60415),(#60416,#60417),(#60418,#60419),(#60420,#60421),
(#60422,#60423),(#60424,#60425),(#60426,#60427),(#60428,#60429),(#60430,
#60431),(#60432,#60433),(#60434,#60435),(#60436,#60437),(#60438,#60439),
(#60440,#60441),(#60442,#60443),(#60444,#60445),(#60446,#60447),(#60448,
#60449),(#60450,#60451),(#60452,#60453),(#60454,#60455),(#60456,#60457),
(#60458,#60459),(#60460,#60461),(#60462,#60463),(#60464,#60465),(#60466,
#60467),(#60468,#60469),(#60470,#60471),(#60472,#60473),(#60474,#60475),
(#60476,#60477),(#60478,#60479),(#60480,#60481),(#60482,#60483),(#60484,
#60485),(#60486,#60487),(#60488,#60489),(#60490,#60491),(#60492,#60493),
(#60494,#60495),(#60496,#60497),(#60498,#60499),(#60500,#60501),(#60502,
#60503),(#60504,#60505),(#60506,#60507),(#60508,#60509),(#60510,#60511),
(#60512,#60513),(#60514,#60515),(#60516,#60517),(#60518,#60519),(#60520,
#60521),(#60522,#60523),(#60524,#60525),(#60526,#60527),(#60528,#60529),
(#60530,#60531),(#60532,#60533),(#60534,#60535),(#60536,#60537),(#60538,
#60539),(#60540,#60541),(#60542,#60543),(#60544,#60545),(#60546,#60547),
(#60548,#60549),(#60550,#60551),(#60552,#60553),(#60554,#60555),(#60556,
#60557),(#60558,#60559),(#60560,#60561),(#60562,#60563),(#60564,#60565),
(#60566,#60567),(#60568,#60569),(#60570,#60571),(#60572,#60573),(#60574,
#60575),(#60576,#60577),(#60578,#60579),(#60580,#60581),(#60582,#60583),
(#60584,#60585),(#60586,#60587),(#60588,#60589),(#60590,#60591),(#60592,
#60593),(#60594,#60595),(#60596,#60597),(#60598,#60599),(#60600,#60601),
(#60602,#60603),(#60604,#60605),(#60606,#60607),(#60608,#60609),(#60610,
#60611),(#60612,#60613),(#60614,#60615),(#60616,#60617),(#60618,#60619),
(#60620,#60621),(#60622,#60623),(#60624,#60625),(#60626,#60627),(#60628,
#60629),(#60630,#60631),(#60632,#60633),(#60634,#60635),(#60636,#60637),
(#60638,#60639),(#60640,#60641),(#60642,#60643),(#60644,#60645),(#60646,
#60647),(#60648,#60649),(#60650,#60651),(#60652,#60653),(#60654,#60655),
(#60656,#60657),(#60658,#60659),(#60660,#60661),(#60662,#60663),(#60664,
#60665),(#60666,#60667),(#60668,#60669),(#60670,#60671),(#60672,#60673),
(#60674,#60675),(#60676,#60677),(#60678,#60679),(#60680,#60681),(#60682,
#60683),(#60684,#60685),(#60686,#60687),(#60688,#60689),(#60690,#60691),
(#60692,#60693),(#60694,#60695),(#60696,#60697),(#60698,#60699),(#60700,
#60701),(#60702,#60703),(#60704,#60705),(#60706,#60707),(#60708,#60709),
(#60710,#60711),(#60712,#60713),(#60714,#60715),(#60716,#60717),(#60718,
#60719),(#60720,#60721),(#60722,#60723),(#60724,#60725),(#60726,#60727),
(#60728,#60729),(#60730,#60731),(#60732,#60733),(#60734,#60735),(#60736,
#60737),(#60738,#60739),(#60740,#60741),(#60742,#60743),(#60744,#60745),
(#60746,#60747),(#60748,#60749),(#60750,#60751),(#60752,#60753),(#60754,
#60755),(#60756,#60757),(#60758,#60759),(#60760,#60761),(#60762,#60763),
(#60764,#60765),(#60766,#60767),(#60768,#60769),(#60770,#60771),(#60772,
#60773),(#60774,#60775),(#60776,#60777),(#60778,#60779),(#60780,#60781),
(#60782,#60783),(#60784,#60785),(#60786,#60787),(#60788,#60789),(#60790,
#60791),(#60792,#60793),(#60794,#60795),(#60796,#60797),(#60798,#60799),
(#60800,#60801),(#60802,#60803),(#60804,#60805),(#60806,#60807),(#60808,
#60809),(#60810,#60811),(#60812,#60813),(#60814,#60815),(#60816,#60817),
(#60818,#60819),(#60820,#60821),(#60822,#60823),(#60824,#60825),(#60826,
#60827),(#60828,#60829),(#60830,#60831),(#60832,#60833),(#60834,#60835),
(#60836,#60837),(#60838,#60839),(#60840,#60841),(#60842,#60843),(#60844,
#60845),(#60846,#60847),(#60848,#60849),(#60850,#60851),(#60852,#60853),
(#60854,#60855),(#60856,#60857),(#60858,#60859),(#60860,#60861),(#60862,
#60863),(#60864,#60865),(#60866,#60867),(#60868,#60869),(#60870,#60871),
(#60872,#60873),(#60874,#60875),(#60876,#60877),(#60878,#60879),(#60880,
#60881),(#60882,#60883),(#60884,#60885),(#60886,#60887),(#60888,#60889),
(#60890,#60891),(#60892,#60893),(#60894,#60895),(#60896,#60897),(#60898,
#60899),(#60900,#60901),(#60902,#60903),(#60904,#60905),(#60906,#60907),
(#60908,#60909),(#60910,#60911),(#60912,#60913),(#60914,#60915),(#60916,
#60917),(#60918,#60919),(#60920,#60921),(#60922,#60923),(#60924,#60925),
(#60926,#60927),(#60928,#60929),(#60930,#60931),(#60932,#60933),(#60934,
#60935),(#60936,#60937),(#60938,#60939),(#60940,#60941),(#60942,#60943),
(#60944,#60945),(#60946,#60947),(#60948,#60949),(#60950,#60951),(#60952,
#60953),(#60954,#60955),(#60956,#60957),(#60958,#60959),(#60960,#60961),
(#60962,#60963),(#60964,#60965),(#60966,#60967),(#60968,#60969),(#60970,
#60971),(#60972,#60973),(#60974,#60975),(#60976,#60977),(#60978,#60979),
(#60980,#60981),(#60982,#60983),(#60984,#60985),(#60986,#60987),(#60988,
#60989),(#60990,#60991),(#60992,#60993),(#60994,#60995),(#60996,#60997),
(#60998,#60999),(#61000,#61001),(#61002,#61003),(#61004,#61005),(#61006,
#61007),(#61008,#61009),(#61010,#61011),(#61012,#61013),(#61014,#61015),
(#61016,#61017),(#61018,#61019),(#61020,#61021),(#61022,#61023),(#61024,
#61025),(#61026,#61027),(#61028,#61029),(#61030,#61031),(#61032,#61033),
(#61034,#61035),(#61036,#61037),(#61038,#61039),(#61040,#61041),(#61042,
#61043),(#61044,#61045),(#61046,#61047),(#61048,#61049),(#61050,#61051),
(#61052,#61053),(#61054,#61055),(#61056,#61057),(#61058,#61059),(#61060,
#61061),(#61062,#61063),(#61064,#61065),(#61066,#61067),(#61068,#61069),
(#61070,#61071),(#61072,#61073),(#61074,#61075),(#61076,#61077),(#61078,
#61079),(#61080,#61081),(#61082,#61083),(#61084,#61085),(#61086,#61087),
(#61088,#61089),(#61090,#61091),(#61092,#61093),(#61094,#61095),(#61096,
#61097),(#61098,#61099),(#61100,#61101),(#61102,#61103),(#61104,#61105),
(#61106,#61107),(#61108,#61109),(#61110,#61111),(#61112,#61113),(#61114,
#61115),(#61116,#61117),(#61118,#61119),(#61120,#61121),(#61122,#61123),
(#61124,#61125),(#61126,#61127),(#61128,#61129),(#61130,#61131),(#61132,
#61133),(#61134,#61135),(#61136,#61137),(#61138,#61139),(#61140,#61141),
(#61142,#61143),(#61144,#61145),(#61146,#61147),(#61148,#61149),(#61150,
#61151),(#61152,#61153),(#61154,#61155),(#61156,#61157),(#61158,#61159),
(#61160,#61161),(#61162,#61163),(#61164,#61165),(#61166,#61167),(#61168,
#61169),(#61170,#61171),(#61172,#61173),(#61174,#61175),(#61176,#61177),
(#61178,#61179),(#61180,#61181),(#61182,#61183),(#61184,#61185),(#61186,
#61187),(#61188,#61189),(#61190,#61191),(#61192,#61193),(#61194,#61195),
(#61196,#61197),(#61198,#61199),(#61200,#61201),(#61202,#61203),(#61204,
#61205),(#61206,#61207),(#61208,#61209),(#61210,#61211),(#61212,#61213),
(#61214,#61215),(#61216,#61217),(#61218,#61219),(#61220,#61221),(#61222,
#61223),(#61224,#61225),(#61226,#61227),(#61228,#61229),(#61230,#61231),
(#61232,#61233),(#61234,#61235),(#61236,#61237),(#61238,#61239),(#61240,
#61241),(#61242,#61243),(#61244,#61245),(#61246,#61247),(#61248,#61249),
(#61250,#61251),(#61252,#61253),(#61254,#61255),(#61256,#61257),(#61258,
#61259),(#61260,#61261),(#61262,#61263),(#61264,#61265),(#61266,#61267),
(#61268,#61269),(#61270,#61271),(#61272,#61273),(#61274,#61275),(#61276,
#61277),(#61278,#61279),(#61280,#61281),(#61282,#61283),(#61284,#61285),
(#61286,#61287),(#61288,#61289),(#61290,#61291),(#61292,#61293),(#61294,
#61295),(#61296,#61297),(#61298,#61299),(#61300,#61301),(#61302,#61303),
(#61304,#61305),(#61306,#61307),(#61308,#61309),(#61310,#61311),(#61312,
#61313),(#61314,#61315),(#61316,#61317),(#61318,#61319),(#61320,#61321),
(#61322,#61323),(#61324,#61325),(#61326,#61327),(#61328,#61329),(#61330,
#61331),(#61332,#61333),(#61334,#61335),(#61336,#61337),(#61338,#61339),
(#61340,#61341),(#61342,#61343),(#61344,#61345),(#61346,#61347),(#61348,
#61349),(#61350,#61351),(#61352,#61353),(#61354,#61355),(#61356,#61357),
(#61358,#61359),(#61360,#61361),(#61362,#61363),(#61364,#61365),(#61366,
#61367),(#61368,#61369),(#61370,#61371),(#61372,#61373),(#61374,#61375),
(#61376,#61377),(#61378,#61379),(#61380,#61381),(#61382,#61383),(#61384,
#61385),(#61386,#61387),(#61388,#61389),(#61390,#61391),(#61392,#61393),
(#61394,#61395),(#61396,#61397),(#61398,#61399),(#61400,#61401),(#61402,
#61403),(#61404,#61405),(#61406,#61407),(#61408,#61409),(#61410,#61411),
(#61412,#61413),(#61414,#61415),(#61416,#61417),(#61418,#61419),(#61420,
#61421),(#61422,#61423),(#61424,#61425),(#61426,#61427),(#61428,#61429),
(#61430,#61431),(#61432,#61433),(#61434,#61435),(#61436,#61437),(#61438,
#61439),(#61440,#61441),(#61442,#61443),(#61444,#61445),(#61446,#61447),
(#61448,#61449),(#61450,#61451),(#61452,#61453),(#61454,#61455),(#61456,
#61457),(#61458,#61459),(#61460,#61461),(#61462,#61463),(#61464,#61465),
(#61466,#61467),(#61468,#61469),(#61470,#61471),(#61472,#61473),(#61474,
#61475),(#61476,#61477),(#61478,#61479),(#61480,#61481),(#61482,#61483),
(#61484,#61485),(#61486,#61487),(#61488,#61489),(#61490,#61491),(#61492,
#61493),(#61494,#61495),(#61496,#61497),(#61498,#61499),(#61500,#61501),
(#61502,#61503),(#61504,#61505),(#61506,#61507),(#61508,#61509),(#61510,
#61511),(#61512,#61513),(#61514,#61515),(#61516,#61517),(#61518,#61519),
(#61520,#61521),(#61522,#61523),(#61524,#61525),(#61526,#61527),(#61528,
#61529),(#61530,#61531),(#61532,#61533),(#61534,#61535),(#61536,#61537),
(#61538,#61539),(#61540,#61541),(#61542,#61543),(#61544,#61545),(#61546,
#61547),(#61548,#61549),(#61550,#61551),(#61552,#61553),(#61554,#61555),
(#61556,#61557),(#61558,#61559),(#61560,#61561),(#61562,#61563),(#61564,
#61565),(#61566,#61567),(#61568,#61569),(#61570,#61571),(#61572,#61573),
(#61574,#61575),(#61576,#61577),(#61578,#61579),(#61580,#61581),(#61582,
#61583),(#61584,#61585),(#61586,#61587),(#61588,#61589),(#61590,#61591),
(#61592,#61593),(#61594,#61595),(#61596,#61597),(#61598,#61599),(#61600,
#61601),(#61602,#61603),(#61604,#61605),(#61606,#61607),(#61608,#61609),
(#61610,#61611),(#61612,#61613),(#61614,#61615),(#61616,#61617),(#61618,
#61619),(#61620,#61621),(#61622,#61623),(#61624,#61625),(#61626,#61627),
(#61628,#61629),(#61630,#61631),(#61632,#61633),(#61634,#61635),(#61636,
#61637),(#61638,#61639),(#61640,#61641),(#61642,#61643),(#61644,#61645),
(#61646,#61647),(#61648,#61649),(#61650,#61651),(#61652,#61653),(#61654,
#61655),(#61656,#61657),(#61658,#61659),(#61660,#61661),(#61662,#61663),
(#61664,#61665),(#61666,#61667),(#61668,#61669),(#61670,#61671),(#61672,
#61673),(#61674,#61675),(#61676,#61677),(#61678,#61679),(#61680,#61681),
(#61682,#61683),(#61684,#61685),(#61686,#61687),(#61688,#61689),(#61690,
#61691),(#61692,#61693),(#61694,#61695),(#61696,#61697),(#61698,#61699),
(#61700,#61701),(#61702,#61703),(#61704,#61705),(#61706,#61707),(#61708,
#61709),(#61710,#61711),(#61712,#61713),(#61714,#61715),(#61716,#61717),
(#61718,#61719),(#61720,#61721),(#61722,#61723),(#61724,#61725),(#61726,
#61727),(#61728,#61729),(#61730,#61731),(#61732,#61733),(#61734,#61735),
(#61736,#61737),(#61738,#61739),(#61740,#61741),(#61742,#61743),(#61744,
#61745),(#61746,#61747),(#61748,#61749),(#61750,#61751),(#61752,#61753),
(#61754,#61755),(#61756,#61757),(#61758,#61759),(#61760,#61761),(#61762,
#61763),(#61764,#61765),(#61766,#61767),(#61768,#61769),(#61770,#61771),
(#61772,#61773),(#61774,#61775),(#61776,#61777),(#61778,#61779),(#61780,
#61781),(#61782,#61783),(#61784,#61785),(#61786,#61787),(#61788,#61789),
(#61790,#61791),(#61792,#61793),(#61794,#61795),(#61796,#61797),(#61798,
#61799),(#61800,#61801),(#61802,#61803),(#61804,#61805),(#61806,#61807),
(#61808,#61809),(#61810,#61811),(#61812,#61813),(#61814,#61815),(#61816,
#61817),(#61818,#61819),(#61820,#61821),(#61822,#61823),(#61824,#61825),
(#61826,#61827),(#61828,#61829),(#61830,#61831),(#61832,#61833),(#61834,
#61835),(#61836,#61837),(#61838,#61839),(#61840,#61841),(#61842,#61843),
(#61844,#61845),(#61846,#61847),(#61848,#61849),(#61850,#61851),(#61852,
#61853),(#61854,#61855),(#61856,#61857),(#61858,#61859),(#61860,#61861),
(#61862,#61863),(#61864,#61865),(#61866,#61867),(#61868,#61869),(#61870,
#61871),(#61872,#61873),(#61874,#61875),(#61876,#61877),(#61878,#61879),
(#61880,#61881),(#61882,#61883),(#61884,#61885),(#61886,#61887),(#61888,
#61889),(#61890,#61891),(#61892,#61893),(#61894,#61895),(#61896,#61897),
(#61898,#61899),(#61900,#61901),(#61902,#61903),(#61904,#61905),(#61906,
#61907),(#61908,#61909),(#61910,#61911),(#61912,#61913),(#61914,#61915),
(#61916,#61917),(#61918,#61919),(#61920,#61921),(#61922,#61923),(#61924,
#61925),(#61926,#61927),(#61928,#61929),(#61930,#61931),(#61932,#61933),
(#61934,#61935),(#61936,#61937),(#61938,#61939),(#61940,#61941),(#61942,
#61943),(#61944,#61945),(#61946,#61947),(#61948,#61949),(#61950,#61951),
(#61952,#61953),(#61954,#61955),(#61956,#61957),(#61958,#61959),(#61960,
#61961),(#61962,#61963),(#61964,#61965),(#61966,#61967),(#61968,#61969),
(#61970,#61971),(#61972,#61973),(#61974,#61975),(#61976,#61977),(#61978,
#61979),(#61980,#61981),(#61982,#61983),(#61984,#61985),(#61986,#61987),
(#61988,#61989),(#61990,#61991),(#61992,#61993),(#61994,#61995),(#61996,
#61997),(#61998,#61999),(#62000,#62001),(#62002,#62003),(#62004,#62005),
(#62006,#62007),(#62008,#62009),(#62010,#62011),(#62012,#62013),(#62014,
#62015),(#62016,#62017),(#62018,#62019),(#62020,#62021),(#62022,#62023),
(#62024,#62025),(#62026,#62027),(#62028,#62029),(#62030,#62031),(#62032,
#62033),(#62034,#62035),(#62036,#62037),(#62038,#62039),(#62040,#62041),
(#62042,#62043),(#62044,#62045),(#62046,#62047),(#62048,#62049),(#62050,
#62051),(#62052,#62053),(#62054,#62055),(#62056,#62057),(#62058,#62059),
(#62060,#62061),(#62062,#62063),(#62064,#62065),(#62066,#62067),(#62068,
#62069),(#62070,#62071),(#62072,#62073),(#62074,#62075),(#62076,#62077),
(#62078,#62079),(#62080,#62081),(#62082,#62083),(#62084,#62085),(#62086,
#62087),(#62088,#62089),(#62090,#62091),(#62092,#62093),(#62094,#62095),
(#62096,#62097),(#62098,#62099),(#62100,#62101),(#62102,#62103),(#62104,
#62105),(#62106,#62107),(#62108,#62109),(#62110,#62111),(#62112,#62113),
(#62114,#62115),(#62116,#62117),(#62118,#62119),(#62120,#62121),(#62122,
#62123),(#62124,#62125),(#62126,#62127),(#62128,#62129),(#62130,#62131),
(#62132,#62133),(#62134,#62135),(#62136,#62137),(#62138,#62139),(#62140,
#62141),(#62142,#62143),(#62144,#62145),(#62146,#62147),(#62148,#62149),
(#62150,#62151),(#62152,#62153),(#62154,#62155),(#62156,#62157),(#62158,
#62159),(#62160,#62161),(#62162,#62163),(#62164,#62165),(#62166,#62167),
(#62168,#62169),(#62170,#62171),(#62172,#62173),(#62174,#62175),(#62176,
#62177),(#62178,#62179),(#62180,#62181),(#62182,#62183),(#62184,#62185),
(#62186,#62187),(#62188,#62189),(#62190,#62191),(#62192,#62193),(#62194,
#62195),(#62196,#62197),(#62198,#62199),(#62200,#62201),(#62202,#62203),
(#62204,#62205),(#62206,#62207),(#62208,#62209),(#62210,#62211),(#62212,
#62213),(#62214,#62215),(#62216,#62217),(#62218,#62219),(#62220,#62221),
(#62222,#62223),(#62224,#62225),(#62226,#62227),(#62228,#62229),(#62230,
#62231),(#62232,#62233),(#62234,#62235),(#62236,#62237),(#62238,#62239),
(#62240,#62241),(#62242,#62243),(#62244,#62245),(#62246,#62247),(#62248,
#62249),(#62250,#62251),(#62252,#62253),(#62254,#62255),(#62256,#62257),
(#62258,#62259),(#62260,#62261),(#62262,#62263),(#62264,#62265),(#62266,
#62267),(#62268,#62269),(#62270,#62271),(#62272,#62273),(#62274,#62275),
(#62276,#62277),(#62278,#62279),(#62280,#62281),(#62282,#62283),(#62284,
#62285),(#62286,#62287),(#62288,#62289),(#62290,#62291),(#62292,#62293),
(#62294,#62295),(#62296,#62297),(#62298,#62299),(#62300,#62301),(#62302,
#62303),(#62304,#62305),(#62306,#62307),(#62308,#62309),(#62310,#62311),
(#62312,#62313),(#62314,#62315),(#62316,#62317),(#62318,#62319),(#62320,
#62321),(#62322,#62323),(#62324,#62325),(#62326,#62327),(#62328,#62329),
(#62330,#62331),(#62332,#62333),(#62334,#62335),(#62336,#62337),(#62338,
#62339),(#62340,#62341),(#62342,#62343),(#62344,#62345),(#62346,#62347),
(#62348,#62349),(#62350,#62351),(#62352,#62353),(#62354,#62355),(#62356,
#62357),(#62358,#62359),(#62360,#62361),(#62362,#62363),(#62364,#62365),
(#62366,#62367),(#62368,#62369),(#62370,#62371),(#62372,#62373),(#62374,
#62375),(#62376,#62377),(#62378,#62379),(#62380,#62381),(#62382,#62383),
(#62384,#62385),(#62386,#62387),(#62388,#62389),(#62390,#62391),(#62392,
#62393),(#62394,#62395),(#62396,#62397),(#62398,#62399),(#62400,#62401),
(#62402,#62403),(#62404,#62405),(#62406,#62407),(#62408,#62409),(#62410,
#62411),(#62412,#62413),(#62414,#62415),(#62416,#62417),(#62418,#62419),
(#62420,#62421),(#62422,#62423),(#62424,#62425),(#62426,#62427),(#62428,
#62429),(#62430,#62431),(#62432,#62433),(#62434,#62435),(#62436,#62437),
(#62438,#62439),(#62440,#62441),(#62442,#62443),(#62444,#62445),(#62446,
#62447),(#62448,#62449),(#62450,#62451),(#62452,#62453),(#62454,#62455),
(#62456,#62457),(#62458,#62459),(#62460,#62461),(#62462,#62463),(#62464,
#62465),(#62466,#62467),(#62468,#62469),(#62470,#62471),(#62472,#62473),
(#62474,#62475),(#62476,#62477),(#62478,#62479),(#62480,#62481),(#62482,
#62483),(#62484,#62485),(#62486,#62487),(#62488,#62489),(#62490,#62491),
(#62492,#62493),(#62494,#62495),(#62496,#62497),(#62498,#62499),(#62500,
#62501),(#62502,#62503),(#62504,#62505),(#62506,#62507),(#62508,#62509),
(#62510,#62511),(#62512,#62513),(#62514,#62515),(#62516,#62517),(#62518,
#62519),(#62520,#62521),(#62522,#62523),(#62524,#62525),(#62526,#62527),
(#62528,#62529),(#62530,#62531),(#62532,#62533),(#62534,#62535),(#62536,
#62537),(#62538,#62539),(#62540,#62541),(#62542,#62543),(#62544,#62545),
(#62546,#62547),(#62548,#62549),(#62550,#62551),(#62552,#62553),(#62554,
#62555),(#62556,#62557),(#62558,#62559),(#62560,#62561),(#62562,#62563),
(#62564,#62565),(#62566,#62567),(#62568,#62569),(#62570,#62571),(#62572,
#62573),(#62574,#62575),(#62576,#62577),(#62578,#62579),(#62580,#62581),
(#62582,#62583),(#62584,#62585),(#62586,#62587),(#62588,#62589),(#62590,
#62591),(#62592,#62593),(#62594,#62595),(#62596,#62597),(#62598,#62599),
(#62600,#62601),(#62602,#62603),(#62604,#62605),(#62606,#62607),(#62608,
#62609),(#62610,#62611),(#62612,#62613),(#62614,#62615),(#62616,#62617),
(#62618,#62619),(#62620,#62621),(#62622,#62623),(#62624,#62625),(#62626,
#62627),(#62628,#62629),(#62630,#62631),(#62632,#62633),(#62634,#62635),
(#62636,#62637),(#62638,#62639),(#62640,#62641),(#62642,#62643),(#62644,
#62645),(#62646,#62647),(#62648,#62649),(#62650,#62651),(#62652,#62653),
(#62654,#62655),(#62656,#62657),(#62658,#62659),(#62660,#62661),(#62662,
#62663),(#62664,#62665),(#62666,#62667),(#62668,#62669),(#62670,#62671),
(#62672,#62673),(#62674,#62675),(#62676,#62677),(#62678,#62679),(#62680,
#62681),(#62682,#62683),(#62684,#62685),(#62686,#62687),(#62688,#62689),
(#62690,#62691),(#62692,#62693),(#62694,#62695),(#62696,#62697),(#62698,
#62699),(#62700,#62701),(#62702,#62703),(#62704,#62705),(#62706,#62707),
(#62708,#62709),(#62710,#62711),(#62712,#62713),(#62714,#62715),(#62716,
#62717),(#62718,#62719),(#62720,#62721),(#62722,#62723),(#62724,#62725),
(#62726,#62727),(#62728,#62729),(#62730,#62731),(#62732,#62733),(#62734,
#62735),(#62736,#62737),(#62738,#62739),(#62740,#62741),(#62742,#62743),
(#62744,#62745),(#62746,#62747),(#62748,#62749),(#62750,#62751),(#62752,
#62753),(#62754,#62755),(#62756,#62757),(#62758,#62759),(#62760,#62761),
(#62762,#62763),(#62764,#62765),(#62766,#62767),(#62768,#62769),(#62770,
#62771),(#62772,#62773),(#62774,#62775),(#62776,#62777),(#62778,#62779),
(#62780,#62781),(#62782,#62783),(#62784,#62785),(#62786,#62787),(#62788,
#62789),(#62790,#62791),(#62792,#62793),(#62794,#62795),(#62796,#62797),
(#62798,#62799),(#62800,#62801),(#62802,#62803),(#62804,#62805),(#62806,
#62807),(#62808,#62809),(#62810,#62811),(#62812,#62813),(#62814,#62815),
(#62816,#62817),(#62818,#62819),(#62820,#62821),(#62822,#62823),(#62824,
#62825),(#62826,#62827),(#62828,#62829),(#62830,#62831),(#62832,#62833),
(#62834,#62835),(#62836,#62837),(#62838,#62839),(#62840,#62841),(#62842,
#62843),(#62844,#62845),(#62846,#62847),(#62848,#62849),(#62850,#62851),
(#62852,#62853),(#62854,#62855),(#62856,#62857),(#62858,#62859),(#62860,
#62861),(#62862,#62863),(#62864,#62865),(#62866,#62867),(#62868,#62869),
(#62870,#62871),(#62872,#62873),(#62874,#62875),(#62876,#62877),(#62878,
#62879),(#62880,#62881),(#62882,#62883),(#62884,#62885),(#62886,#62887),
(#62888,#62889),(#62890,#62891),(#62892,#62893),(#62894,#62895),(#62896,
#62897),(#62898,#62899),(#62900,#62901),(#62902,#62903),(#62904,#62905),
(#62906,#62907),(#62908,#62909),(#62910,#62911),(#62912,#62913),(#62914,
#62915),(#62916,#62917),(#62918,#62919),(#62920,#62921),(#62922,#62923),
(#62924,#62925),(#62926,#62927),(#62928,#62929),(#62930,#62931),(#62932,
#62933),(#62934,#62935),(#62936,#62937),(#62938,#62939),(#62940,#62941),
(#62942,#62943),(#62944,#62945),(#62946,#62947),(#62948,#62949),(#62950,
#62951),(#62952,#62953),(#62954,#62955),(#62956,#62957),(#62958,#62959),
(#62960,#62961),(#62962,#62963),(#62964,#62965),(#62966,#62967),(#62968,
#62969),(#62970,#62971),(#62972,#62973),(#62974,#62975),(#62976,#62977),
(#62978,#62979),(#62980,#62981),(#62982,#62983),(#62984,#62985),(#62986,
#62987),(#62988,#62989),(#62990,#62991),(#62992,#62993),(#62994,#62995),
(#62996,#62997),(#62998,#62999),(#63000,#63001),(#63002,#63003),(#63004,
#63005),(#63006,#63007),(#63008,#63009),(#63010,#63011),(#63012,#63013),
(#63014,#63015),(#63016,#63017),(#63018,#63019),(#63020,#63021),(#63022,
#63023),(#63024,#63025),(#63026,#63027),(#63028,#63029),(#63030,#63031),
(#63032,#63033),(#63034,#63035),(#63036,#63037),(#63038,#63039),(#63040,
#63041),(#63042,#63043),(#63044,#63045),(#63046,#63047),(#63048,#63049),
(#63050,#63051),(#63052,#63053),(#63054,#63055),(#63056,#63057),(#63058,
#63059),(#63060,#63061),(#63062,#63063),(#63064,#63065),(#63066,#63067),
(#63068,#63069),(#63070,#63071),(#63072,#63073),(#63074,#63075),(#63076,
#63077),(#63078,#63079),(#63080,#63081),(#63082,#63083),(#63084,#63085),
(#63086,#63087),(#63088,#63089),(#63090,#63091),(#63092,#63093),(#63094,
#63095),(#63096,#63097),(#63098,#63099),(#63100,#63101),(#63102,#63103),
(#63104,#63105),(#63106,#63107),(#63108,#63109),(#63110,#63111),(#63112,
#63113),(#63114,#63115),(#63116,#63117),(#63118,#63119),(#63120,#63121),
(#63122,#63123),(#63124,#63125),(#63126,#63127),(#63128,#63129),(#63130,
#63131),(#63132,#63133),(#63134,#63135),(#63136,#63137),(#63138,#63139),
(#63140,#63141),(#63142,#63143),(#63144,#63145),(#63146,#63147),(#63148,
#63149),(#63150,#63151),(#63152,#63153),(#63154,#63155),(#63156,#63157),
(#63158,#63159),(#63160,#63161),(#63162,#63163),(#63164,#63165),(#63166,
#63167),(#63168,#63169),(#63170,#63171),(#63172,#63173),(#63174,#63175),
(#63176,#63177),(#63178,#63179),(#63180,#63181),(#63182,#63183),(#63184,
#63185),(#63186,#63187),(#63188,#63189),(#63190,#63191),(#63192,#63193),
(#63194,#63195),(#63196,#63197),(#63198,#63199),(#63200,#63201),(#63202,
#63203),(#63204,#63205),(#63206,#63207),(#63208,#63209),(#63210,#63211),
(#63212,#63213),(#63214,#63215),(#63216,#63217),(#63218,#63219),(#63220,
#63221),(#63222,#63223),(#63224,#63225),(#63226,#63227),(#63228,#63229),
(#63230,#63231),(#63232,#63233),(#63234,#63235),(#63236,#63237),(#63238,
#63239),(#63240,#63241),(#63242,#63243),(#63244,#63245),(#63246,#63247),
(#63248,#63249),(#63250,#63251),(#63252,#63253),(#63254,#63255),(#63256,
#63257),(#63258,#63259),(#63260,#63261),(#63262,#63263),(#63264,#63265),
(#63266,#63267),(#63268,#63269),(#63270,#63271),(#63272,#63273),(#63274,
#63275),(#63276,#63277),(#63278,#63279),(#63280,#63281),(#63282,#63283),
(#63284,#63285),(#63286,#63287),(#63288,#63289),(#63290,#63291),(#63292,
#63293),(#63294,#63295),(#63296,#63297),(#63298,#63299),(#63300,#63301),
(#63302,#63303),(#63304,#63305),(#63306,#63307),(#63308,#63309),(#63310,
#63311),(#63312,#63313),(#63314,#63315),(#63316,#63317),(#63318,#63319),
(#63320,#63321),(#63322,#63323),(#63324,#63325),(#63326,#63327),(#63328,
#63329),(#63330,#63331),(#63332,#63333),(#63334,#63335),(#63336,#63337),
(#63338,#63339),(#63340,#63341),(#63342,#63343),(#63344,#63345),(#63346,
#63347),(#63348,#63349),(#63350,#63351),(#63352,#63353),(#63354,#63355),
(#63356,#63357),(#63358,#63359),(#63360,#63361),(#63362,#63363),(#63364,
#63365),(#63366,#63367),(#63368,#63369),(#63370,#63371),(#63372,#63373),
(#63374,#63375),(#63376,#63377),(#63378,#63379),(#63380,#63381),(#63382,
#63383),(#63384,#63385),(#63386,#63387),(#63388,#63389),(#63390,#63391),
(#63392,#63393),(#63394,#63395),(#63396,#63397),(#63398,#63399),(#63400,
#63401),(#63402,#63403),(#63404,#63405),(#63406,#63407),(#63408,#63409),
(#63410,#63411),(#63412,#63413),(#63414,#63415),(#63416,#63417),(#63418,
#63419),(#63420,#63421),(#63422,#63423),(#63424,#63425),(#63426,#63427),
(#63428,#63429),(#63430,#63431),(#63432,#63433),(#63434,#63435),(#63436,
#63437),(#63438,#63439),(#63440,#63441),(#63442,#63443),(#63444,#63445),
(#63446,#63447),(#63448,#63449),(#63450,#63451),(#63452,#63453),(#63454,
#63455),(#63456,#63457),(#63458,#63459),(#63460,#63461),(#63462,#63463),
(#63464,#63465),(#63466,#63467),(#63468,#63469),(#63470,#63471),(#63472,
#63473),(#63474,#63475),(#63476,#63477),(#63478,#63479),(#63480,#63481),
(#63482,#63483),(#63484,#63485),(#63486,#63487),(#63488,#63489),(#63490,
#63491),(#63492,#63493),(#63494,#63495),(#63496,#63497),(#63498,#63499),
(#63500,#63501),(#63502,#63503),(#63504,#63505),(#63506,#63507),(#63508,
#63509),(#63510,#63511),(#63512,#63513),(#63514,#63515),(#63516,#63517),
(#63518,#63519),(#63520,#63521),(#63522,#63523),(#63524,#63525),(#63526,
#63527),(#63528,#63529),(#63530,#63531),(#63532,#63533),(#63534,#63535),
(#63536,#63537),(#63538,#63539),(#63540,#63541),(#63542,#63543),(#63544,
#63545),(#63546,#63547),(#63548,#63549),(#63550,#63551),(#63552,#63553),
(#63554,#63555),(#63556,#63557),(#63558,#63559),(#63560,#63561),(#63562,
#63563),(#63564,#63565),(#63566,#63567),(#63568,#63569),(#63570,#63571),
(#63572,#63573),(#63574,#63575),(#63576,#63577),(#63578,#63579),(#63580,
#63581),(#63582,#63583),(#63584,#63585),(#63586,#63587),(#63588,#63589),
(#63590,#63591),(#63592,#63593),(#63594,#63595),(#63596,#63597),(#63598,
#63599),(#63600,#63601),(#63602,#63603),(#63604,#63605),(#63606,#63607),
(#63608,#63609),(#63610,#63611),(#63612,#63613),(#63614,#63615),(#63616,
#63617),(#63618,#63619),(#63620,#63621),(#63622,#63623),(#63624,#63625),
(#63626,#63627),(#63628,#63629),(#63630,#63631),(#63632,#63633),(#63634,
#63635),(#63636,#63637),(#63638,#63639),(#63640,#63641),(#63642,#63643),
(#63644,#63645),(#63646,#63647),(#63648,#63649),(#63650,#63651),(#63652,
#63653),(#63654,#63655),(#63656,#63657),(#63658,#63659),(#63660,#63661),
(#63662,#63663),(#63664,#63665),(#63666,#63667),(#63668,#63669),(#63670,
#63671),(#63672,#63673),(#63674,#63675),(#63676,#63677),(#63678,#63679),
(#63680,#63681),(#63682,#63683),(#63684,#63685),(#63686,#63687),(#63688,
#63689),(#63690,#63691),(#63692,#63693),(#63694,#63695),(#63696,#63697),
(#63698,#63699),(#63700,#63701),(#63702,#63703),(#63704,#63705),(#63706,
#63707),(#63708,#63709),(#63710,#63711),(#63712,#63713),(#63714,#63715),
(#63716,#63717),(#63718,#63719),(#63720,#63721),(#63722,#63723),(#63724,
#63725),(#63726,#63727),(#63728,#63729),(#63730,#63731),(#63732,#63733),
(#63734,#63735),(#63736,#63737),(#63738,#63739),(#63740,#63741),(#63742,
#63743),(#63744,#63745),(#63746,#63747),(#63748,#63749),(#63750,#63751),
(#63752,#63753),(#63754,#63755),(#63756,#63757),(#63758,#63759),(#63760,
#63761),(#63762,#63763),(#63764,#63765),(#63766,#63767),(#63768,#63769),
(#63770,#63771),(#63772,#63773),(#63774,#63775),(#63776,#63777),(#63778,
#63779),(#63780,#63781),(#63782,#63783),(#63784,#63785),(#63786,#63787),
(#63788,#63789),(#63790,#63791),(#63792,#63793),(#63794,#63795),(#63796,
#63797),(#63798,#63799),(#63800,#63801),(#63802,#63803),(#63804,#63805),
(#63806,#63807),(#63808,#63809),(#63810,#63811),(#63812,#63813),(#63814,
#63815),(#63816,#63817),(#63818,#63819),(#63820,#63821),(#63822,#63823),
(#63824,#63825),(#63826,#63827),(#63828,#63829),(#63830,#63831),(#63832,
#63833),(#63834,#63835),(#63836,#63837),(#63838,#63839),(#63840,#63841),
(#63842,#63843),(#63844,#63845),(#63846,#63847),(#63848,#63849),(#63850,
#63851),(#63852,#63853),(#63854,#63855),(#63856,#63857),(#63858,#63859),
(#63860,#63861),(#63862,#63863),(#63864,#63865),(#63866,#63867),(#63868,
#63869),(#63870,#63871),(#63872,#63873),(#63874,#63875),(#63876,#63877),
(#63878,#63879),(#63880,#63881),(#63882,#63883),(#63884,#63885),(#63886,
#63887),(#63888,#63889),(#63890,#63891),(#63892,#63893),(#63894,#63895),
(#63896,#63897),(#63898,#63899),(#63900,#63901),(#63902,#63903),(#63904,
#63905),(#63906,#63907),(#63908,#63909),(#63910,#63911),(#63912,#63913),
(#63914,#63915),(#63916,#63917),(#63918,#63919),(#63920,#63921),(#63922,
#63923),(#63924,#63925),(#63926,#63927),(#63928,#63929),(#63930,#63931),
(#63932,#63933),(#63934,#63935),(#63936,#63937),(#63938,#63939),(#63940,
#63941),(#63942,#63943),(#63944,#63945),(#63946,#63947),(#63948,#63949),
(#63950,#63951),(#63952,#63953),(#63954,#63955),(#63956,#63957),(#63958,
#63959),(#63960,#63961),(#63962,#63963),(#63964,#63965),(#63966,#63967),
(#63968,#63969),(#63970,#63971),(#63972,#63973),(#63974,#63975),(#63976,
#63977),(#63978,#63979),(#63980,#63981),(#63982,#63983),(#63984,#63985),
(#63986,#63987),(#63988,#63989),(#63990,#63991),(#63992,#63993),(#63994,
#63995),(#63996,#63997),(#63998,#63999),(#64000,#64001),(#64002,#64003),
(#64004,#64005),(#64006,#64007),(#64008,#64009),(#64010,#64011),(#64012,
#64013),(#64014,#64015),(#64016,#64017),(#64018,#64019),(#64020,#64021),
(#64022,#64023),(#64024,#64025),(#64026,#64027),(#64028,#64029),(#64030,
#64031),(#64032,#64033),(#64034,#64035),(#64036,#64037),(#64038,#64039),
(#64040,#64041),(#64042,#64043),(#64044,#64045),(#64046,#64047),(#64048,
#64049),(#64050,#64051),(#64052,#64053),(#64054,#64055),(#64056,#64057),
(#64058,#64059),(#64060,#64061),(#64062,#64063),(#64064,#64065),(#64066,
#64067),(#64068,#64069),(#64070,#64071),(#64072,#64073),(#64074,#64075),
(#64076,#64077),(#64078,#64079),(#64080,#64081),(#64082,#64083),(#64084,
#64085),(#64086,#64087),(#64088,#64089),(#64090,#64091),(#64092,#64093),
(#64094,#64095),(#64096,#64097),(#64098,#64099),(#64100,#64101),(#64102,
#64103),(#64104,#64105),(#64106,#64107),(#64108,#64109),(#64110,#64111),
(#64112,#64113),(#64114,#64115),(#64116,#64117),(#64118,#64119),(#64120,
#64121),(#64122,#64123),(#64124,#64125),(#64126,#64127),(#64128,#64129),
(#64130,#64131),(#64132,#64133),(#64134,#64135),(#64136,#64137),(#64138,
#64139),(#64140,#64141),(#64142,#64143),(#64144,#64145),(#64146,#64147),
(#64148,#64149),(#64150,#64151),(#64152,#64153),(#64154,#64155),(#64156,
#64157),(#64158,#64159),(#64160,#64161),(#64162,#64163),(#64164,#64165),
(#64166,#64167),(#64168,#64169),(#64170,#64171),(#64172,#64173),(#64174,
#64175),(#64176,#64177),(#64178,#64179),(#64180,#64181),(#64182,#64183),
(#64184,#64185),(#64186,#64187),(#64188,#64189),(#64190,#64191),(#64192,
#64193),(#64194,#64195),(#64196,#64197),(#64198,#64199),(#64200,#64201),
(#64202,#64203),(#64204,#64205),(#64206,#64207),(#64208,#64209),(#64210,
#64211),(#64212,#64213),(#64214,#64215),(#64216,#64217),(#64218,#64219),
(#64220,#64221),(#64222,#64223),(#64224,#64225),(#64226,#64227),(#64228,
#64229),(#64230,#64231),(#64232,#64233),(#64234,#64235),(#64236,#64237),
(#64238,#64239),(#64240,#64241),(#64242,#64243),(#64244,#64245),(#64246,
#64247),(#64248,#64249),(#64250,#64251),(#64252,#64253),(#64254,#64255),
(#64256,#64257),(#64258,#64259),(#64260,#64261),(#64262,#64263),(#64264,
#64265),(#64266,#64267),(#64268,#64269),(#64270,#64271),(#64272,#64273),
(#64274,#64275),(#64276,#64277),(#64278,#64279),(#64280,#64281),(#64282,
#64283),(#64284,#64285),(#64286,#64287),(#64288,#64289),(#64290,#64291),
(#64292,#64293),(#64294,#64295),(#64296,#64297),(#64298,#64299),(#64300,
#64301),(#64302,#64303),(#64304,#64305),(#64306,#64307),(#64308,#64309),
(#64310,#64311),(#64312,#64313),(#64314,#64315),(#64316,#64317),(#64318,
#64319),(#64320,#64321),(#64322,#64323),(#64324,#64325),(#64326,#64327),
(#64328,#64329),(#64330,#64331),(#64332,#64333),(#64334,#64335),(#64336,
#64337),(#64338,#64339),(#64340,#64341),(#64342,#64343),(#64344,#64345),
(#64346,#64347),(#64348,#64349),(#64350,#64351),(#64352,#64353),(#64354,
#64355),(#64356,#64357),(#64358,#64359),(#64360,#64361),(#64362,#64363),
(#64364,#64365),(#64366,#64367),(#64368,#64369),(#64370,#64371),(#64372,
#64373),(#64374,#64375),(#64376,#64377),(#64378,#64379),(#64380,#64381),
(#64382,#64383),(#64384,#64385),(#64386,#64387),(#64388,#64389),(#64390,
#64391),(#64392,#64393),(#64394,#64395),(#64396,#64397),(#64398,#64399),
(#64400,#64401),(#64402,#64403),(#64404,#64405),(#64406,#64407),(#64408,
#64409),(#64410,#64411),(#64412,#64413),(#64414,#64415),(#64416,#64417),
(#64418,#64419),(#64420,#64421),(#64422,#64423),(#64424,#64425),(#64426,
#64427),(#64428,#64429),(#64430,#64431),(#64432,#64433),(#64434,#64435),
(#64436,#64437),(#64438,#64439),(#64440,#64441),(#64442,#64443),(#64444,
#64445),(#64446,#64447),(#64448,#64449),(#64450,#64451),(#64452,#64453),
(#64454,#64455),(#64456,#64457),(#64458,#64459),(#64460,#64461),(#64462,
#64463),(#64464,#64465),(#64466,#64467),(#64468,#64469),(#64470,#64471)),
 .UNSPECIFIED.,.F.,.F.,.F.,(4,1,1,1,1,1,1,1,1,1,1,1,1,1,1,1,1,1,1,1,1,1,
1,1,1,1,1,1,1,1,1,1,1,1,1,1,1,1,1,1,1,1,1,1,1,1,1,1,1,1,1,1,1,1,1,1,1,1,
1,1,1,1,1,1,1,1,1,1,1,1,1,1,1,1,1,1,1,1,1,1,1,1,1,1,1,1,1,1,1,1,1,1,1,1,
1,1,1,1,1,1,1,1,1,1,1,1,1,1,1,1,1,1,1,1,1,1,1,1,1,1,1,1,1,1,1,1,1,1,1,1,
1,1,1,1,1,1,1,1,1,1,1,1,1,1,1,1,1,1,1,1,1,1,1,1,1,1,1,1,1,1,1,1,1,1,1,1,
1,1,1,1,1,1,1,1,1,1,1,1,1,1,1,1,1,1,1,1,1,1,1,1,1,1,1,1,1,1,1,1,1,1,1,1,
1,1,1,1,1,1,1,1,1,1,1,1,1,1,1,1,1,1,1,1,1,1,1,1,1,1,1,1,1,1,1,1,1,1,1,1,
1,1,1,1,1,1,1,1,1,1,1,1,1,1,1,1,1,1,1,1,1,1,1,1,1,1,1,1,1,1,1,1,1,1,1,1,
1,1,1,1,1,1,1,1,1,1,1,1,1,1,1,1,1,1,1,1,1,1,1,1,1,1,1,1,1,1,1,1,1,1,1,1,
1,1,1,1,1,1,1,1,1,1,1,1,1,1,1,1,1,1,1,1,1,1,1,1,1,1,1,1,1,1,1,1,1,1,1,1,
1,1,1,1,1,1,1,1,1,1,1,1,1,1,1,1,1,1,1,1,1,1,1,1,1,1,1,1,1,1,1,1,1,1,1,1,
1,1,1,1,1,1,1,1,1,1,1,1,1,1,1,1,1,1,1,1,1,1,1,1,1,1,1,1,1,1,1,1,1,1,1,1,
1,1,1,1,1,1,1,1,1,1,1,1,1,1,1,1,1,1,1,1,1,1,1,1,1,1,1,1,1,1,1,1,1,1,1,1,
1,1,1,1,1,1,1,1,1,1,1,1,1,1,1,1,1,1,1,1,1,1,1,1,1,1,1,1,1,1,1,1,1,1,1,1,
1,1,1,1,1,1,1,1,1,1,1,1,1,1,1,1,1,1,1,1,1,1,1,1,1,1,1,1,1,1,1,1,1,1,1,1,
1,1,1,1,1,1,1,1,1,1,1,1,1,1,1,1,1,1,1,1,1,1,1,1,1,1,1,1,1,1,1,1,1,1,1,1,
1,1,1,1,1,1,1,1,1,1,1,1,1,1,1,1,1,1,1,1,1,1,1,1,1,1,1,1,1,1,1,1,1,1,1,1,
1,1,1,1,1,1,1,1,1,1,1,1,1,1,1,1,1,1,1,1,1,1,1,1,1,1,1,1,1,1,1,1,1,1,1,1,
1,1,1,1,1,1,1,1,1,1,1,1,1,1,1,1,1,1,1,1,1,1,1,1,1,1,1,1,1,1,1,1,1,1,1,1,
1,1,1,1,1,1,1,1,1,1,1,1,1,1,1,1,1,1,1,1,1,1,1,1,1,1,1,1,1,1,1,1,1,1,1,1,
1,1,1,1,1,1,1,1,1,1,1,1,1,1,1,1,1,1,1,1,1,1,1,1,1,1,1,1,1,1,1,1,1,1,1,1,
1,1,1,1,1,1,1,1,1,1,1,1,1,1,1,1,1,1,1,1,1,1,1,1,1,1,1,1,1,1,1,1,1,1,1,1,
1,1,1,1,1,1,1,1,1,1,1,1,1,1,1,1,1,1,1,1,1,1,1,1,1,1,1,1,1,1,1,1,1,1,1,1,
1,1,1,1,1,1,1,1,1,1,1,1,1,1,1,1,1,1,1,1,1,1,1,1,1,1,1,1,1,1,1,1,1,1,1,1,
1,1,1,1,1,1,1,1,1,1,1,1,1,1,1,1,1,1,1,1,1,1,1,1,1,1,1,1,1,1,1,1,1,1,1,1,
1,1,1,1,1,1,1,1,1,1,1,1,1,1,1,1,1,1,1,1,1,1,1,1,1,1,1,1,1,1,1,1,1,1,1,1,
1,1,1,1,1,1,1,1,1,1,1,1,1,1,1,1,1,1,1,1,1,1,1,1,1,1,1,1,1,1,1,1,1,1,1,1,
1,1,1,1,1,1,1,1,1,1,1,1,1,1,1,1,1,1,1,1,1,1,1,1,1,1,1,1,1,1,1,1,1,1,1,1,
1,1,1,1,1,1,1,1,1,1,1,1,1,1,1,1,1,1,1,1,1,1,1,1,1,1,1,1,1,1,1,1,1,1,1,1,
1,1,1,1,1,1,1,1,1,1,1,1,1,1,1,1,1,1,1,1,1,1,1,1,1,1,1,1,1,1,1,1,1,1,1,1,
1,1,1,1,1,1,1,1,1,1,1,1,1,1,1,1,1,1,1,1,1,1,1,1,1,1,1,1,1,1,1,1,1,1,1,1,
1,1,1,1,1,1,1,1,1,1,1,1,1,1,1,1,1,1,1,1,1,1,1,1,1,1,1,1,1,1,1,1,1,1,1,1,
1,1,1,1,1,1,1,1,1,1,1,1,1,1,1,1,1,1,1,1,1,1,1,1,1,1,1,1,1,1,1,1,1,1,1,1,
1,1,1,1,1,1,1,1,1,1,1,1,1,1,1,1,1,1,1,1,1,1,1,1,1,1,1,1,1,1,1,1,1,1,1,1,
1,1,1,1,1,1,1,1,1,1,1,1,1,1,1,1,1,1,1,1,1,1,1,1,1,1,1,1,1,1,1,1,1,1,1,1,
1,1,1,1,1,1,1,1,1,1,1,1,1,1,1,1,1,1,1,1,1,1,1,1,1,1,1,1,1,1,1,1,1,1,1,1,
1,1,1,1,1,1,1,1,1,1,1,1,1,1,1,1,1,1,1,1,1,1,1,1,1,1,1,1,1,1,1,1,1,1,1,1,
1,1,1,1,1,1,1,1,1,1,1,1,1,1,1,1,1,1,1,1,1,1,1,1,1,1,1,1,1,1,1,1,1,1,1,1,
1,1,1,1,1,1,1,1,1,1,1,1,1,1,1,1,1,1,1,1,1,1,1,1,1,1,1,1,1,1,1,1,1,1,1,1,
1,1,1,1,1,1,1,1,1,1,1,1,1,1,1,1,1,1,1,1,1,1,1,1,1,1,1,1,1,1,1,1,1,1,1,1,
1,1,1,1,1,1,1,1,1,1,1,1,1,1,1,1,1,1,1,1,1,1,1,1,1,1,1,1,1,1,1,1,1,1,1,1,
1,1,1,1,1,1,1,1,1,1,1,1,1,1,1,1,1,1,1,1,1,1,1,1,1,1,1,1,1,1,1,1,1,1,1,1,
1,1,1,1,1,1,1,1,1,1,1,1,1,1,1,1,1,1,1,1,1,1,1,1,1,1,1,1,1,1,1,1,1,1,1,1,
1,1,1,1,1,1,1,1,1,1,1,1,1,1,1,1,1,1,1,1,1,1,1,1,1,1,1,1,1,1,1,1,1,1,1,1,
1,1,1,1,1,1,1,1,1,1,1,1,1,1,1,1,1,1,1,1,1,1,1,1,1,1,1,1,1,1,1,1,1,1,1,1,
1,1,1,1,1,1,1,1,1,1,1,1,1,1,1,1,1,1,1,1,1,1,1,1,1,1,1,1,1,1,1,1,1,1,1,1,
1,1,1,1,1,1,1,1,1,1,1,1,1,1,1,1,1,1,1,1,1,1,1,1,1,1,1,1,1,1,1,1,1,1,1,1,
1,1,1,1,1,1,1,1,1,1,1,1,1,1,1,1,1,1,1,1,1,1,1,1,1,1,1,1,1,1,1,1,1,1,1,1,
1,1,1,1,1,1,1,1,1,1,1,1,1,1,1,1,1,1,1,1,1,1,1,1,1,1,1,1,1,1,1,1,1,1,1,1,
1,1,1,1,1,1,1,1,1,1,1,1,1,1,1,1,1,1,1,1,1,1,1,1,1,1,1,1,1,1,1,1,1,1,1,1,
1,1,1,1,1,1,1,1,1,1,1,1,1,1,1,1,1,1,1,1,1,1,1,1,1,1,1,1,1,1,1,1,1,1,1,1,
1,1,1,1,1,1,1,1,1,1,1,1,1,1,1,1,1,1,1,1,1,1,1,1,1,1,1,1,1,1,1,1,1,1,1,1,
1,1,1,1,1,1,1,1,1,1,1,1,1,1,1,1,1,1,1,1,1,1,1,1,1,1,1,1,1,1,1,1,1,1,1,1,
1,1,1,1,1,1,1,1,1,1,1,1,1,1,1,1,1,1,1,1,1,1,1,1,1,1,1,1,1,1,1,1,1,1,1,1,
1,1,1,1,1,1,1,1,1,1,1,1,1,1,1,1,1,1,1,1,1,1,1,1,1,1,1,1,1,1,1,1,1,1,1,1,
1,1,1,1,1,1,1,1,1,1,1,1,1,1,1,1,1,1,1,1,1,1,1,1,1,1,1,1,1,1,1,1,1,1,1,1,
1,1,1,1,1,1,1,1,1,1,1,1,1,1,1,1,1,1,1,1,1,1,1,1,1,1,1,1,1,1,1,1,1,1,1,1,
1,1,1,1,1,1,1,1,1,1,1,1,1,1,1,1,1,1,1,1,1,1,1,1,1,1,1,1,1,1,1,1,1,1,1,1,
1,1,1,1,1,1,1,1,1,1,1,1,1,1,1,1,1,1,1,1,1,1,1,1,1,1,1,1,1,1,1,1,1,1,1,1,
1,1,1,1,1,1,1,1,1,1,1,1,1,1,1,1,1,1,1,1,1,1,1,1,1,1,1,1,1,1,1,1,1,1,1,1,
1,1,1,1,1,1,1,1,1,1,1,1,1,1,1,1,1,1,1,1,1,1,1,1,1,1,1,1,1,1,1,1,1,1,1,1,
1,1,1,1,1,1,1,1,1,1,1,1,1,1,1,1,1,1,1,1,1,1,1,1,1,1,1,1,1,1,1,1,1,1,1,1,
1,1,1,1,1,1,1,1,1,1,1,1,1,1,1,1,1,1,1,1,1,1,1,1,1,1,1,1,1,1,1,1,1,1,1,1,
1,1,1,1,1,1,1,1,1,1,1,1,1,1,1,1,1,1,1,1,1,1,1,1,1,1,1,1,1,1,1,1,1,1,1,1,
1,1,1,1,1,1,1,1,1,1,1,1,1,1,1,1,1,1,1,1,1,1,1,1,1,1,1,1,1,1,1,1,1,1,1,1,
1,1,1,1,1,1,1,1,1,1,1,1,1,1,1,1,1,1,1,1,1,1,1,1,1,1,1,1,1,1,1,1,1,1,1,1,
1,1,1,1,1,1,1,1,1,1,1,1,1,1,1,1,1,1,1,1,1,1,1,1,1,1,1,1,1,1,1,1,1,1,1,1,
1,1,1,1,1,1,1,1,1,1,1,1,1,1,1,1,1,1,1,1,1,1,1,1,1,1,1,1,1,1,1,1,1,1,1,1,
1,1,1,1,1,1,1,1,1,1,1,1,1,1,1,1,1,1,1,1,1,1,1,1,1,1,1,1,1,1,1,1,1,1,1,1,
1,1,1,1,1,1,1,1,1,1,1,1,1,1,1,1,1,1,1,1,1,1,1,1,1,1,1,1,1,1,1,1,1,1,1,1,
1,1,1,1,1,1,1,1,1,1,1,1,1,1,1,1,1,1,1,1,1,1,1,1,1,1,1,1,1,1,1,1,1,1,1,1,
1,1,1,1,1,1,1,1,1,1,1,1,1,1,1,1,1,1,1,1,1,1,1,1,1,1,1,1,1,1,1,1,1,1,1,1,
1,1,1,1,1,1,1,1,1,1,1,1,1,1,1,1,1,1,1,1,1,1,1,1,1,1,1,1,1,1,1,1,1,1,1,1,
1,1,1,1,1,1,1,1,1,1,1,1,1,1,1,1,1,1,1,1,1,1,1,1,1,1,1,1,1,1,1,1,1,1,1,1,
1,1,1,1,1,1,1,1,1,1,1,1,1,1,1,1,1,1,1,1,1,1,1,1,1,1,1,1,1,1,1,1,1,1,1,1,
1,1,1,1,1,1,1,1,1,1,1,1,1,1,1,1,1,1,1,1,1,1,1,1,1,1,1,1,1,1,1,1,1,1,1,1,
1,1,1,1,1,1,1,1,1,1,1,1,1,1,1,1,1,1,1,1,1,1,1,1,1,1,1,1,1,1,1,1,1,1,1,1,
1,1,1,1,1,1,1,1,1,1,1,1,1,1,1,1,1,1,1,1,1,1,1,1,1,1,1,1,1,1,1,1,1,1,1,1,
1,1,1,1,1,1,1,1,1,1,1,1,1,1,1,1,1,1,1,1,1,1,1,1,1,1,1,1,1,1,1,1,1,1,1,1,
1,1,1,1,1,1,1,1,1,1,1,1,1,1,1,1,1,1,1,1,1,1,1,1,1,1,1,1,1,1,1,1,1,1,1,1,
1,1,1,1,1,1,1,1,1,1,1,1,1,1,1,1,1,1,1,1,1,1,1,1,1,1,1,1,1,1,1,1,1,1,1,1,
1,1,1,1,1,1,1,1,1,1,1,1,1,1,1,1,1,1,1,1,1,1,1,1,1,1,1,1,1,1,1,1,1,1,1,1,
1,1,1,1,1,1,1,1,1,1,1,1,1,1,1,1,1,1,1,1,1,1,1,1,1,1,1,1,1,1,1,1,1,1,1,1,
1,1,1,1,1,1,1,1,1,1,1,1,1,1,1,1,1,1,1,1,1,1,1,1,1,1,1,1,1,1,1,1,1,1,1,1,
1,1,1,1,1,1,1,1,1,1,1,1,1,1,1,1,1,1,1,1,1,1,1,1,1,1,1,1,1,1,1,1,1,1,1,1,
1,1,1,1,1,1,1,1,1,1,1,1,1,1,1,1,1,1,1,1,1,1,1,1,1,1,1,1,1,1,1,1,1,1,1,1,
1,1,1,1,1,1,1,1,1,1,1,1,1,1,1,1,1,1,1,1,1,1,1,1,1,1,1,1,1,1,1,1,1,1,1,1,
1,1,1,1,1,1,1,1,1,1,1,1,1,1,1,1,1,1,1,1,1,1,1,1,1,1,1,1,1,1,1,1,1,1,1,1,
1,1,1,1,1,1,1,1,1,1,1,1,1,1,1,1,1,1,1,1,1,1,1,1,1,1,1,1,1,1,1,1,1,1,1,1,
1,1,1,1,1,1,1,1,1,1,1,1,1,1,1,1,1,1,1,1,1,1,1,1,1,1,1,1,1,1,1,1,1,1,1,1,
1,1,1,1,1,1,1,1,1,1,1,1,1,1,1,1,1,1,1,1,1,1,1,1,1,1,1,1,1,1,1,1,1,1,1,1,
1,1,1,1,1,1,1,1,1,1,1,1,1,1,1,1,1,1,1,1,1,1,1,1,1,1,1,1,1,1,1,1,1,1,1,1,
1,1,1,1,1,1,1,1,1,1,1,1,1,1,1,1,1,1,1,1,1,1,1,1,1,1,1,1,1,1,1,1,1,1,1,1,
1,1,1,1,1,1,1,1,1,1,1,1,1,1,1,1,1,1,1,1,1,1,1,1,1,1,1,1,1,1,1,1,1,1,1,1,
1,1,1,1,1,1,1,1,1,1,1,1,1,1,1,1,1,1,1,1,1,1,1,1,1,1,1,1,1,1,1,1,1,1,1,1,
1,1,1,1,1,1,1,1,1,1,1,1,1,1,1,1,1,1,1,1,1,1,1,1,1,1,1,1,1,1,1,1,1,1,1,1,
1,1,1,1,1,1,1,1,1,1,1,1,1,1,1,1,1,1,1,1,1,1,1,1,1,1,1,1,1,1,1,1,1,1,1,1,
1,1,1,1,4),(2,2),(0.,0.869746702321014,1.7394931589914,2.60923976624962,
3.47983908319159,4.35043840179749,5.22018503077054,6.08993165951504,6.95967828799171,
7.82942491616733,8.69917154401062,9.56891817149224,10.4395174886835,11.3101168056706,
12.179863432132,13.049610058144,13.9193566836854,14.7891033087372,15.6588499332817,
16.5285965573034,17.3991958717975,18.2697951860185,18.7046684974166,19.1395418086746,
19.5744151197912,20.0092884307654,20.4441617415962,20.8790350522825,21.7487816732187,
22.1836549834672,22.6185282935685,23.0534016035221,23.4882749133276,23.9231482229848,
24.3588742245859,24.794600226187,25.2294735355468,26.0992201538203,26.5340934627341,
26.9689667714994,27.4038400801166,27.838713388586,28.2735866969081,28.7084600050832,
29.143333313112,29.5782066209952,30.0130799287334,30.4479532363275,30.8828265437783,
31.3185525442794,31.7542785447804,32.1891518519474,32.6240251589741,33.0588984658616,
33.4937717726112,33.928645079224,34.3635183857014,34.7983916920448,35.2332649982556,
35.6681383043353,36.1030116102854,36.5378849161076,36.9727582218035,37.4076315273749,
37.8425048328235,38.2782308323341,38.7139568318446,39.1488301370532,39.5837034421446,
40.0185767471208,40.4534500519838,40.8883233567357,41.3231966613787,41.7580699659148,
42.1929432703463,42.6278165746754,43.0626898789044,43.4975631830356,43.9324364870714,
44.3673097910142,44.8021830948664,45.2379090935952,45.673635092324,46.1085083960024,
46.5433816995978,46.9782550031127,47.4131283065497,47.8480016099115,48.2828749132006,
48.7177482164198,49.1526215195718,49.5874948226593,50.0223681256851,50.457241428652,
50.8921147315628,51.3269880344203,51.7618613372274,52.197587335454,52.6333133336805,
53.0681866363954,53.5030599390685,53.9379332417027,54.3728065443011,54.8076798468664,
55.2425531494018,55.6774264519101,56.1122997543943,56.5471730568575,56.9820463593026,
57.4169196617326,57.8517929641506,58.2866662665595,58.7215395689624,59.157265567009,
59.5929915650557,60.0278648674556,60.4627381698584,60.8976114722673,61.3324847746853,
61.7673580771153,62.2022313795604,62.6371046820236,63.0719779845079,63.5068512870162,
63.9417245895516,64.376597892117,64.8114711947155,65.2463444973499,65.6812178000231,
66.1169437982275,66.5526697964318,66.9875430991915,67.4224164019987,67.8572897048563,
68.2921630077673,68.7270363107343,69.1619096137603,69.5967829168479,70.0316562200001,
70.4665295232194,70.9014028265087,71.3362761298705,71.7711494333077,72.2060227368227,
72.6408960404182,73.0766220391044,73.5123480377905,73.9472213415547,74.382094645407,
74.8169679493499,75.2518412533859,75.6867145575172,76.1215878617464,76.5564611660756,
76.9913344705072,77.4262077750435,77.8610810796866,78.2959543844386,78.7308276893018,
79.1657009942781,79.6005742993696,80.0363002988208,80.4720262982719,80.9068996035997,
81.3417729090484,81.7766462146199,82.211519520316,82.6463928261383,83.0812661320886,
83.5161394381684,83.9510127443794,84.3858860507229,84.8207593572004,85.2556326638134,
85.6905059705631,86.1253792774507,86.5602525844776,86.995978584908,87.4317045853384,
87.8665778926469,88.3014512000977,88.7363245076919,89.1711978154302,89.6060711233134,
90.0409444313423,90.4758177395175,90.9106910478396,91.345564356309,91.7804376649263,
92.2153109736917,92.6501842826055,93.085057591668,93.5199309008791,93.9556569024059,
94.3913829039327,94.8262562134414,95.2611295230986,95.6960028329042,96.1308761428578,
96.5657494529591,97.0006227632077,97.4354960736028,97.870369384144,98.3052426948304,
98.7401160056612,99.1749893166354,99.6098626277522,100.04473593901,100.915335253024,
101.351061255639,101.785934567313,102.220807879124,102.655681191068,103.090554503145,
103.525427815353,104.395174440154,105.264921065453,105.699794378283,106.134667691232,
106.569541004295,107.004414317471,107.8750136343,108.745612951339,109.615359578629,
110.485106206296,111.354852834309,112.224599462639,113.094346091254,113.964092720119,
114.834692038763,115.705291357499,116.575037986826,117.444784616267,118.314531245777,
119.184277875311,120.054024504821,120.923771134261,121.794370453112,122.66496977189,
123.534716400968,124.404463029834,125.274209658448,126.143956286779,127.013702914792,
127.883449542458,128.754048859798,129.624648176939,130.494394803617,131.364141429857,
132.233888055637,133.103634680937,133.973381305737,134.843127930023,135.71372724472,
136.584326559147,137.019199870684,137.454073182083,137.888946493341,138.323819804458,
139.193566426263,140.063313047491,140.498186357887,140.933059668136,141.367932978237,
141.802806288191,142.237679597997,142.673405599673,143.109131601348,143.544004910857,
143.978878220217,144.413751529429,144.848624838491,145.283498147405,145.718371456171,
146.153244764789,146.588118073258,147.022991381581,147.457864689756,147.892737997785,
148.327611305669,148.762484613407,149.197357921002,149.633083921574,150.068809922147,
150.503683229455,150.938556536623,151.37342984365,151.808303150538,152.243176457288,
152.678049763901,153.112923070379,153.547796376722,153.982669682934,154.417542989014,
154.852416294964,155.287289600787,155.722162906483,156.157036212055,156.592762211626,
157.028488211198,157.463361516526,157.898234821735,158.333108126826,158.767981431803,
159.202854736666,159.637728041419,160.072601346062,160.507474650599,160.94234795503,
161.37722125936,161.812094563589,162.246967867721,162.681841171757,163.1167144757,
163.552440474473,163.988166473247,164.423039777011,164.85791308069,165.292786384286,
165.727659687801,166.162532991238,166.597406294601,167.03227959789,167.46715290111,
167.902026204262,168.33689950735,168.771772810376,169.206646113343,169.641519416254,
170.076392719112,170.512118717363,170.947844715614,171.382718018374,171.817591321089,
172.252464623762,172.687337926397,173.122211228996,173.557084531561,173.991957834097,
174.426831136606,174.86170443909,175.296577741554,175.731451044,176.16632434643,
176.601197648848,177.036070951258,177.471796949306,177.907522947355,178.342396249755,
178.777269552155,179.212142854558,179.647016156968,180.081889459386,180.516762761816,
180.951636064262,181.386509366726,181.82138266921,182.256255971719,182.691129274255,
183.12600257682,183.560875879419,183.995749182054,184.431475180237,184.867201178421,
185.302074481136,185.736947783896,186.171821086704,186.606694389561,187.041567692473,
187.47644099544,187.911314298466,188.346187601554,188.781060904706,189.215934207926,
189.650807511215,190.085680814577,190.520554118015,190.95542742153,191.391153420175,
191.82687941882,192.261752722499,192.696626026263,193.131499330116,193.566372634059,
194.001245938095,194.436119242227,194.870992546456,195.305865850785,195.740739155217,
196.175612459754,196.610485764397,197.045359069149,197.480232374013,197.915105678989,
198.350831678382,198.786557677775,199.221430982984,199.656304288312,200.091177593761,
200.526050899333,200.960924205029,201.395797510852,201.830670816802,202.265544122882,
202.700417429093,203.135290735437,203.570164041915,204.005037348528,204.439910655278,
204.874783962166,205.310509962526,205.746235962887,206.181109270054,206.615982577363,
207.050855884814,207.485729192409,207.920602500147,208.355475808031,208.79034911606,
209.225222424235,209.660095732558,210.094969041027,210.529842349645,210.96471565841,
211.399588967324,211.834462276387,212.27018827784,212.705914279292,213.140787588653,
213.575660898161,214.010534207819,214.880280827579,215.31515413768,215.750027447929,
216.184900758324,216.619774068866,217.054647379553,217.489520690384,218.359267312475,
219.22986662628,219.665592628826,220.100465940363,220.535339252038,220.970212563848,
221.83995918787,222.709705812416,223.579452437468,224.014325750179,224.44919906301,
225.318945689022,226.189545005688,227.060144322571,227.929890949664,228.799637577146,
229.66938420499,230.539130833166,231.408877461643,232.278624090388,233.149223408954,
234.019822727623,234.889569356878,235.759315986267,236.629062615749,237.498809245277,
238.368555874806,239.238302504287,240.108901823183,240.979501142017,241.849247771189,
242.718994400167,243.588741028911,244.458487657389,245.328234285565,246.197980913409,
247.068580230891,247.939179548182,248.80892617507,249.678672801532,250.548419427545,
251.418166053087,252.287912678139,253.157659302684,254.028258617581,254.898857932211,
255.333731243885,255.768604555423,256.203477866821,256.63835117808,257.508097800171,
258.377844421689,258.812717732231,259.247591042627,259.682464352876,260.117337662977,
260.552210972931,260.987936974682,261.858536286089,262.293409595598,262.728282904958,
263.16315621417,263.598029523233,264.032902832147,264.467776140913,264.902649449531,
265.337522758001,265.772396066323,266.207269374499,266.642142682528,267.077015990412,
267.511889298151,267.947615298795,268.383341299439,268.81821460689,269.2530879142,
269.687961221367,270.122834528394,270.557707835282,270.992581142032,271.427454448646,
271.862327755124,272.297201061468,272.732074367679,273.166947673759,273.60182097971,
274.036694285533,274.471567591229,274.907293590862,275.343019590495,275.777892895944,
276.212766201272,276.647639506481,277.082512811573,277.51738611655,277.952259421414,
278.387132726166,278.82200603081,279.256879335346,279.691752639779,280.126625944108,
280.561499248338,280.996372552469,281.431245856506,281.866971855324,282.302697854143,
282.737571157996,283.172444461761,283.60731776544,284.042191069036,284.477064372551,
284.911937675989,285.346810979351,285.781684282641,286.216557585861,286.651430889013,
287.086304192101,287.521177495128,287.956050798095,288.390924101007,288.826650099283,
289.262376097559,289.697249400366,290.132122703127,290.566996005842,291.001869308516,
291.43674261115,291.871615913749,292.306489216315,292.741362518851,293.17623582136,
293.611109123845,294.045982426308,294.480855728754,294.915729031185,295.350602333603,
295.786328331655,296.222054329707,296.65692763211,297.091800934511,297.526674236911,
297.961547539314,298.396420841724,298.831294144142,299.266167446573,299.701040749018,
300.135914051482,300.570787353967,301.005660656476,301.440533959012,301.875407261578,
302.310280564177,302.746006562341,303.181732560506,303.616605863179,304.051479165895,
304.486352468655,304.921225771462,305.35609907432,305.790972377232,306.225845680199,
306.660718983226,307.095592286314,307.530465589466,307.965338892686,308.400212195976,
308.835085499338,309.269958802776,309.705684801381,310.141410799985,310.576284103581,
311.01115740726,311.446030711025,311.880904014878,312.315777318821,312.750650622858,
313.185523926989,313.620397231219,314.055270535549,314.490143839981,314.925017144517,
315.359890449161,315.794763753913,316.229637058777,316.665363058112,317.101089057448,
317.53596236254,317.970835667749,318.405708973077,318.840582278526,319.275455584098,
319.710328889795,320.145202195618,320.580075501568,321.014948807648,321.44982211386,
321.884695420204,322.319568726682,322.754442033295,323.189315340045,323.625041340336,
324.060767340628,324.495640647655,324.930513954822,325.365387262131,325.800260569583,
326.235133877177,326.670007184916,327.1048804928,327.539753800829,327.974627109005,
328.409500417327,328.844373725797,329.279247034415,329.714120343181,330.148993652095,
330.584719653474,331.020445654852,331.455318964064,331.890192273424,332.325065582933,
332.759938892591,333.194812202397,333.629685512351,334.064558822453,334.499432132702,
334.934305443098,335.369178753639,335.804052064326,336.673798686132,337.108671997249,
337.544397999725,337.980124002201,338.4149973136,338.849870625137,339.284743936812,
340.154490560568,341.024237184854,341.459110497191,341.893983809655,342.328857122244,
342.763730434955,343.633477060735,344.504076377234,345.374675693955,346.244422320844,
347.114168948136,347.983915575803,348.853662203817,349.723408832148,350.593155460764,
351.463754779246,352.334354097839,353.204100727012,354.07384735634,354.943593985781,
355.813340615292,356.683087244827,357.552833874338,358.423433193272,359.294032512154,
360.163779141409,361.033525770489,361.903272399355,362.77301902797,363.642765656301,
364.512512284316,365.383111601936,366.253710919371,367.123457546465,367.993204173143,
368.862950799383,369.732697425164,370.602444050463,371.472190675265,372.342789990359,
373.21338930519,373.648262617,374.083135928675,374.952882551611,375.822629173987,
376.257502484962,376.692375795793,377.12724910648,377.562122417021,377.996995727417,
378.431869037666,378.866742347767,379.302468349591,379.738194351416,380.173067661222,
380.607940970879,381.042814280388,381.477687589749,381.91256089896,382.347434208023,
382.782307516937,383.217180825703,383.652054134321,384.086927442791,384.521800751113,
384.956674059289,385.391547367318,385.826420675202,386.262146675918,386.697872676635,
387.13274598423,387.567619291681,388.00249259899,388.437365906157,388.872239213185,
389.307112520073,389.741985826823,390.176859133436,390.611732439914,391.046605746258,
391.48147905247,391.91635235855,392.351225664501,392.786098970323,393.221824970019,
393.657550969714,394.092424275286,394.527297580735,394.962170886063,395.397044191272,
395.831917496364,396.266790801341,396.701664106204,397.136537410957,397.5714107156,
398.006284020137,398.441157324569,398.876030628899,399.310903933128,399.74577723726,
400.181503236126,400.617229234991,401.052102538934,401.486975842787,401.921849146551,
402.356722450231,402.791595753827,403.226469057342,403.66134236078,404.096215664142,
404.531088967432,404.965962270651,405.400835573804,405.835708876892,406.270582179918,
406.705455482886,407.141181481189,407.576907479491,408.01178078235,408.446654085157,
408.881527387917,409.316400690633,409.751273993306,410.186147295941,410.62102059854,
411.055893901106,411.490767203642,411.925640506151,412.360513808636,412.795387111099,
413.230260413545,413.665133715976,414.100859714032,414.536585712088,414.971459014498,
415.406332316901,415.841205619301,416.276078921702,416.710952224105,417.145825526515,
417.580698828933,418.015572131364,418.45044543381,418.885318736273,419.320192038758,
419.755065341267,420.189938643803,420.624811946369,421.060537944515,421.496263942662,
421.931137245297,422.36601054797,422.800883850686,423.235757153446,423.670630456253,
424.105503759112,424.540377062023,424.975250364991,425.410123668017,425.844996971105,
426.279870274258,426.714743577477,427.149616880767,427.584490184129,428.020216182695,
428.455942181261,428.890815484776,429.325688788373,429.760562092052,430.195435395816,
430.630308699669,431.065182003612,431.500055307649,431.93492861178,432.36980191601,
432.80467522034,433.239548524772,433.674421829309,434.109295133952,434.544168438705,
434.979894437984,435.415620437262,435.850493742239,436.285367047331,436.72024035254,
437.155113657869,437.589986963318,438.024860268889,438.459733574586,438.894606880409,
439.32948018636,439.76435349244,440.199226798651,440.634100104995,441.068973411473,
441.503846718087,441.939572718309,442.375298718531,442.810172025419,443.245045332447,
443.679918639614,444.114791946923,444.549665254374,444.984538561969,445.419411869708,
445.854285177591,446.289158485621,446.724031793796,447.158905102119,447.593778410589,
448.028651719207,448.463525027973,448.899251029277,449.334977030581,449.769850339644,
450.639596958216,451.074470267725,451.509343577383,451.944216887189,452.379090197143,
452.813963507244,453.248836817493,453.683710127889,454.118583438431,454.553456749117,
454.988330059949,455.423203370923,455.858929373329,456.294655375734,456.729528686993,
457.164401998391,457.599275309929,458.469021933414,458.90389524536,459.338768557437,
459.773641869646,460.208515181983,460.643388494447,461.078261807036,461.948008432578,
462.818607748906,463.689207065461,464.55895369214,465.428700319234,466.298446946716,
467.16819357456,468.037940202737,468.907686831215,469.778286149605,470.648885468116,
471.518632097196,472.388378726451,473.258125355841,474.127871985322,474.997618614851,
475.86736524438,476.737964563343,477.608563882265,478.478310511593,479.348057140765,
480.217803769743,481.087550398488,481.957297026966,482.827043655142,483.697642972895,
484.568242290469,485.43798891776,486.307735544649,487.177482171112,488.047228797125,
488.916975422667,489.78672204772,490.657321363009,491.09304736596,491.527920678038,
492.397667301793,493.267413925005,494.137160547663,494.57203385878,495.006907169755,
495.441780480586,495.876653791273,496.311527101814,496.74640041221,497.616999724357,
498.052725726255,498.487599036209,498.922472346015,499.357345655673,499.792218965182,
500.227092274542,500.661965583754,501.096838892816,501.531712201731,501.966585510497,
502.401458819114,502.836332127584,503.271205435907,503.706078744082,504.140952052112,
504.576678052901,505.01240405369,505.447277361429,505.882150669023,506.317023976474,
506.751897283783,507.186770590951,507.621643897978,508.056517204866,508.491390511616,
508.92626381823,509.361137124708,509.796010431052,510.230883737263,510.665757043344,
511.100630349294,511.536356349053,511.972082348811,512.406955654506,512.841828960076,
513.276702265523,513.711575570849,514.146448876056,514.581322181146,515.016195486121,
515.451068790983,515.885942095733,516.320815400375,516.75568870491,517.19056200934,
517.625435313668,518.060308617896,518.496034616807,518.931760615718,519.366633919752,
519.801507223694,520.236380527545,520.671253831307,521.106127134985,521.541000438579,
521.975873742092,522.410747045528,522.845620348888,523.280493652176,523.715366955394,
524.150240258545,524.585113561631,525.019986864656,525.455712862985,525.891438861313,
526.326312164223,526.761185467079,527.196058769885,527.630932072643,528.065805375356,
528.500678678029,528.935551980661,529.370425283258,529.805298585822,530.240171888356,
530.675045190863,531.109918493346,531.544791795808,531.979665098252,532.415391096312,
532.851117094373,533.285990396789,533.720863699197,534.155737001598,534.590610303997,
535.025483606395,535.460356908796,535.895230211204,536.330103513621,536.764976816049,
537.199850118493,537.634723420955,538.069596723438,538.504470025945,538.93934332848,
539.375069326608,539.810795324736,540.245668627333,540.680541929966,541.115415232637,
541.550288535351,541.985161838109,542.420035140915,542.854908443771,543.28978174668,
543.724655049646,544.15952835267,544.594401655757,545.029274958907,545.464148262125,
545.899021565413,546.334747563939,546.770473562465,547.205346865901,547.640220169415,
548.075093473009,548.509966776686,548.944840080449,549.3797133843,549.814586688241,
550.249459992276,550.684333296405,551.119206600633,551.554079904961,551.988953209391,
552.423826513926,552.858699818567,553.294425817789,553.73015181701,554.165025121872,
554.599898426846,555.034771731937,555.469645037144,555.90451834247,556.339391647917,
556.774264953487,557.209138259182,557.644011565003,558.078884870951,558.51375817703,
558.948631483239,559.383504789581,559.818378096058,560.254104096209,560.689830096361,
561.12470340311,561.559576709996,561.994450017021,562.429323324187,562.864196631494,
563.299069938943,563.733943246536,564.168816554273,564.603689862154,565.038563170182,
565.473436478355,565.908309786676,566.343183095144,566.77805640376,567.213782404988,
567.649508406216,568.084381715128,568.519255024189,568.954128333399,569.389001642757,
569.823874952264,570.258748261921,570.693621571725,571.128494881677,571.563368191777,
572.433114812417,572.867988122957,573.302861433642,573.737734744471,574.173460746804,
574.609186749136,575.044060060251,575.913806682904,576.783553306113,577.218426617922,
577.653299929865,578.08817324194,578.523046554147,579.392793178944,580.26253980424,
581.13313912039,581.568865123709,582.003738436771,582.87348506323,583.743231690115,
584.612978317402,585.482724945065,586.352471573076,587.222218201403,588.092817519691,
588.963416838109,589.833163467083,590.702910096251,591.572656725575,592.442403355013,
593.31214998452,594.181896614051,595.05249593303,595.92309525198,596.792841881366,
597.662588510618,598.532335139693,599.402081768556,600.271828397167,601.141575025495,
602.012174343369,602.882773661074,603.752520288553,604.622266915642,605.492013542317,
606.361760168553,607.23150679433,608.101253419626,608.971852735101,609.842452050322,
610.71219867434,611.581945297822,612.451691920754,612.886565232011,613.321438543126,
613.756311854099,614.191185164928,615.060931786153,615.931531098516,616.367257100486,
616.802130410586,617.237003720538,617.671877030342,618.106750339998,618.541623649505,
618.976496958863,619.411370268073,619.846243577134,620.281116886046,620.71599019481,
621.150863503426,621.585736811894,622.020610120214,622.455483428388,622.891209429248,
623.326935430108,623.761808737989,624.196682045726,624.631555353319,625.066428660769,
625.501301968075,625.936175275241,626.371048582266,626.805921889153,627.240795195901,
627.675668502512,628.110541808988,628.54541511533,628.98028842154,629.415161727618,
629.850887727438,630.286613727259,630.72148703308,631.156360338774,631.591233644344,
632.026106949791,632.460980255118,632.895853560325,633.330726865415,633.76560017039,
634.200473475251,634.635346780002,635.070220084644,635.505093389179,635.939966693609,
636.374839997937,636.810565996897,637.246291995857,637.681165299986,638.116038604021,
638.550911907962,638.985785211813,639.420658515576,639.855531819253,640.290405122847,
640.725278426361,641.160151729796,641.595025033157,642.029898336444,642.464771639662,
642.899644942813,643.334518245899,643.770244244257,644.205970242616,644.640843545581,
645.075716848491,645.510590151347,645.945463454153,646.380336756911,646.815210059625,
647.250083362296,647.684956664929,648.119829967526,648.55470327009,648.989576572624,
649.424449875131,649.859323177614,650.294196480076,650.729922478144,651.165648476212,
651.600521778641,652.035395081057,652.470268383465,652.905141685866,653.340014988265,
653.774888290663,654.209761593065,654.644634895472,655.079508197889,655.514381500318,
655.949254802762,656.384128105224,656.819001407706,657.253874710213,657.689600708326,
658.12532670644,658.560200009004,658.995073311601,659.429946614234,659.864819916905,
660.299693219619,660.734566522377,661.169439825183,661.604313128039,662.039186430948,
662.474059733914,662.908933036938,663.343806340025,663.778679643175,664.213552946393,
664.649278944883,665.085004943373,665.519878246733,665.954751550169,666.389624853683,
666.824498157277,667.259371460954,667.694244764717,668.129118068568,668.563991372509,
668.998864676544,669.433737980674,669.868611284901,670.303484589229,670.738357893659,
671.173231198194,671.608957197361,672.044683196528,672.479556501278,672.91442980614,
673.349303111115,673.784176416205,674.219049721412,674.653923026738,675.088796332185,
675.523669637755,675.95854294345,676.393416249271,676.82828955522,677.263162861298,
677.698036167508,678.13290947385,678.568635473934,679.004361474018,679.439234780629,
679.874108087377,680.308981394264,680.743854701289,681.178728008455,681.613601315762,
682.048474623211,682.483347930804,682.91822123854,683.353094546422,683.78796785445,
684.222841162623,684.657714470944,685.092587779412,685.528313780566,685.96403978172,
686.398913090483,686.833786399396,687.268659708457,687.703533017666,688.138406327025,
688.573279636532,689.008152946187,689.443026255992,689.877899565944,690.312772876043,
690.74764618629,691.182519496684,691.617392807224,692.052266117909,692.487992120169,
692.92371812243,693.358591433403,694.228338055774,694.663211367171,695.098084678707,
695.532957990379,695.967831302188,696.402704614131,696.837577926207,697.707324550749,
698.577071175797,699.011944488507,699.447670491767,699.883396495028,700.318269807975,
701.188016434211,702.057763060886,702.927509687976,703.797256315454,704.667002943295,
705.536749571467,706.407348889651,707.277948207973,708.147694836835,709.017441465911,
709.887188095163,710.756934724548,711.626681354026,712.496427983551,713.367027302543,
714.237626621516,715.107373250954,715.977119880277,716.846866509446,717.716613138419,
718.586359767161,719.456106395635,720.32670571363,721.197305031464,722.067051659126,
722.936798286414,723.806544913299,724.676291539758,725.546038165767,726.415784791305,
727.286384106969,728.156983422381,729.026730046663,729.896476670415,730.331349982088,
730.766223293624,731.201096605021,731.635969916278,732.505716538366,733.37546315988,
733.81033647042,734.246062472462,734.681788474505,735.116661784752,735.551535094852,
735.986408404804,736.421281714608,736.856155024264,737.291028333771,737.72590164313,
738.160774952339,738.5956482614,739.030521570312,739.465394879076,739.900268187692,
740.33514149616,740.77001480448,741.205740805414,741.641466806347,742.076340114374,
742.511213422256,742.946086729993,743.380960037585,743.815833345035,744.250706652341,
744.685579959507,745.120453266533,745.555326573419,745.990199880167,746.425073186778,
746.859946493254,747.294819799596,747.729693105806,748.165419105691,748.601145105576,
749.036018411525,749.470891717346,749.90576502304,750.34063832861,750.775511634057,
751.210384939384,751.645258244591,752.080131549682,752.515004854656,752.949878159518,
753.384751464269,753.81962476891,754.254498073445,754.689371377875,755.125097376885,
755.560823375895,755.995696680123,756.430569984253,756.865443288287,757.300316592228,
757.735189896079,758.170063199842,758.604936503519,759.039809807113,759.474683110627,
759.909556414062,760.344429717423,760.779303020711,761.214176323929,761.649049627079,
762.084775625469,762.520501623858,762.955374926883,763.390248229848,763.825121532758,
764.259994835614,764.694868138419,765.129741441178,765.564614743891,765.999488046563,
766.434361349196,766.869234651793,767.304107954357,767.738981256891,768.173854559398,
768.608727861881,769.044453859958,769.480179858035,769.915053160479,770.349926462907,
770.784799765324,771.219673067731,771.654546370133,772.089419672531,772.52429297493,
772.959166277331,773.394039579739,773.828912882155,774.263786184584,774.698659487028,
775.13353278949,775.568406091973,776.004132090072,776.439858088172,776.874731390706,
777.30960469327,777.744477995867,778.1793512985,778.614224601171,779.049097903885,
779.483971206643,779.918844509449,780.353717812305,780.788591115215,781.22346441818,
781.658337721205,782.093211024291,782.528084327442,782.963810325897,783.399536324352,
783.834409627639,784.269282931,784.704156234435,785.139029537949,785.573902841543,
786.00877614522,786.443649448983,786.878522752834,787.313396056775,787.74826936081,
788.183142664939,788.618015969167,789.052889273495,789.487762577925,789.923488577038,
790.359214576152,790.794087880793,791.228961185544,791.663834490406,792.098707795381,
792.533581100471,792.968454405678,793.403327711004,793.838201016451,794.273074322021,
794.707947627716,795.142820933537,795.577694239486,796.012567545564,796.447440851774,
796.883166851791,797.318892851808,797.753766158284,798.188639464895,798.623512771643,
799.058386078529,799.493259385555,799.92813269272,800.363006000027,800.797879307477,
801.232752615069,801.667625922806,802.102499230688,802.537372538715,802.972245846889,
803.40711915521,803.84284515629,804.27857115737,804.713444465985,805.148317774749,
805.583191083662,806.018064392723,806.452937701933,806.887811011291,807.322684320798,
808.192430940258,808.62730425021,809.06217756031,809.497050870557,809.931924180951,
810.36679749149,810.802523493679,811.238249495867,811.673122806697,812.542869428785,
812.977742740041,813.412616051438,813.847489362974,814.282362674646,814.717235986455,
815.152109298398,816.021855922681,816.891602547478,817.326475860065,817.762201863265,
818.197927866466,818.632801179295,819.502547805304,820.372294431763,821.242041058648,
822.111787685935,822.981534313598,823.851280941609,824.721880259681,825.5924795779,
826.462226206642,827.331972835616,828.201719464785,829.071466094109,829.941212723546,
830.810959353053,831.681558672047,832.552157991036,833.421904620514,834.2916512499,
835.161397879151,836.031144508226,836.900891137089,837.770637765701,838.641237083811,
839.511836401767,840.381583029608,841.251329657086,842.121076284176,842.990822910851,
843.860569537087,844.730316162863,845.600915478712,846.471514794314,847.341261418855,
848.211008042874,848.645881354683,849.080754666356,849.515627977891,849.950501289288,
850.82024791166,851.689994533462,852.124867844147,852.560593846263,852.996319848379,
853.431193158772,853.866066469019,854.300939779119,855.170686398875,855.605559708531,
856.040433018038,856.475306327397,856.910179636606,857.345052945667,857.77992625458,
858.214799563344,858.64967287196,859.084546180427,859.520272181434,859.95599818244,
860.390871490614,860.825744798641,861.260618106523,861.69549141426,862.130364721852,
862.565238029302,863.000111336609,863.434984643774,863.8698579508,864.304731257686,
864.739604564434,865.174477871045,865.609351177521,866.044224483863,866.479950483814,
866.915676483765,867.350549789843,867.785423095792,868.220296401613,868.655169707307,
869.090043012877,869.524916318325,869.959789623651,870.394662928858,870.829536233948,
871.264409538923,871.699282843785,872.134156148535,872.569029453177,873.003902757712,
873.439628756773,873.875354755834,874.310228060162,874.745101364389,875.179974668519,
875.614847972553,876.049721276495,876.484594580346,876.919467884108,877.354341187786,
877.78921449138,878.224087794893,878.658961098329,879.093834401689,879.528707704977,
879.963581008195,880.399307006616,880.835033005038,881.269906308124,881.704779611148,
882.139652914114,882.574526217024,883.00939951988,883.444272822685,883.879146125444,
884.314019428157,884.748892730829,885.183766033462,885.618639336059,886.053512638623,
886.488385941157,886.923259243664,887.358985241751,887.794711239839,888.2295845423,
888.664457844744,889.099331147173,889.534204449589,889.969077751997,890.403951054398,
890.838824356797,891.273697659195,891.708570961597,892.143444264004,892.578317566421,
893.01319086885,893.448064171293,893.882937473755,894.318663471843,894.75438946993,
895.189262772437,895.624136074971,896.059009377535,896.493882680132,896.928755982765,
897.363629285437,897.798502588151,898.233375890909,898.668249193715,899.103122496571,
899.53799579948,899.972869102446,900.40774240547,900.842615708556,901.278341706978,
901.714067705399,902.148941008617,902.583814311905,903.018687615265,903.453560918701,
903.888434222214,904.323307525808,904.758180829485,905.193054133248,905.627927437099,
906.06280074104,906.497674045075,906.932547349205,907.367420653433,907.80229395776,
908.238019956821,908.673745955883,909.108619260417,909.543492565059,909.978365869809,
910.413239174671,910.848112479646,911.282985784736,911.717859089943,912.152732395269,
912.587605700716,913.022479006287,913.457352311981,913.892225617802,914.327098923751,
914.761972229829,915.19769822978,915.633424229731,916.068297536072,916.503170842548,
916.93804414916,917.372917455908,917.807790762794,918.24266406982,918.677537376985,
919.112410684292,919.547283991742,919.982157299334,920.417030607071,920.851903914953,
921.28677722298,921.721650531154,922.15737653216,922.593102533167,923.027975841635,
923.46284915025,923.897722459014,924.332595767926,924.767469076987,925.202342386197,
925.637215695556,926.072089005063,926.506962314719,926.941835624523,927.376708934475,
927.811582244575,928.246455554822,928.681328865215,929.117054867331,929.987654180132,
930.422527490961,930.857400801934,931.292274113049,931.727147424306,932.162020735703,
932.596894047238,933.46664067072,934.336387294739,934.771260606945,935.20613391928,
935.641007231742,936.076733234882,936.94733255073,937.817079176507,938.686825802743,
939.556572429418,940.426319056508,941.296065683986,942.165812311827,943.036411629783,
943.907010947893,944.776757576505,945.646504205367,946.516250834443,947.385997463694,
948.25574409308,949.125490722558,949.996090041546,950.86668936054,951.736435990048,
952.606182619485,953.475929248809,954.345675877978,955.215422506951,956.085169135693,
956.955768453912,957.826367771985,958.696114399995,959.565861027658,960.435607654946,
961.305354281831,962.175100908289,963.044847534298,963.915446850328,964.786046166116,
965.655792790913,966.525539415195,966.960412727138,967.395286038947,968.265032662155,
969.134779284809,969.569652595924,970.004525906897,970.439399217726,970.875125219914,
971.310851222103,971.745724532643,972.615471153283,973.485217773335,973.920091083139,
974.354964392795,974.789837702302,975.22471101166,975.65958432087,976.094457629931,
976.529330938844,976.964204247608,977.399077556223,977.834803557303,978.270529558383,
978.705402866704,979.140276174877,979.575149482905,980.010022790786,980.444896098523,
980.879769406116,981.314642713565,981.749516020872,982.184389328038,982.619262635063,
983.05413594195,983.489009248698,983.923882555309,984.358755861785,984.794481861802,
985.230207861819,985.665081168029,986.099954474107,986.534827780056,986.969701085877,
987.404574391571,987.839447697141,988.274321002589,988.709194307915,989.144067613122,
989.578940918212,990.013814223187,990.448687528048,990.883560832799,991.31843413744,
991.754160136554,992.189886135667,992.624759440097,993.059632744425,993.494506048653,
993.929379352783,994.364252656817,994.799125960758,995.233999264609,995.668872568372,
996.103745872049,996.538619175643,996.973492479157,997.408365782593,997.843239085953,
998.278112389241,998.713838387696,999.149564386151,999.584437689301,1000.01931099239,
1000.45418429541,1000.88905759838,1001.32393090129,1001.75880420414,1002.19367750695,
1002.62855080971,1003.06342411242,1003.49829741509,1003.93317071773,1004.36804402032,
1004.80291732289,1005.23779062542,1005.67351662352,1006.10924262162,1006.5441159241,
1006.97898922656,1007.41386252901,1007.84873583144,1008.28360913385,1008.71848243626,
1009.15335573866,1009.58822904106,1010.02310234346,1010.45797564586,1010.89284894827,
1011.32772225069,1011.76259555311,1012.19746885556,1012.63319485364,1013.06892085171,
1013.5037941542,1013.9386674567,1014.37354075924,1014.8084140618,1015.2432873644,
1015.67816066703,1016.1130339697,1016.54790727242,1016.98278057517,1017.41765387798,
1017.85252718084,1018.28740048375,1018.72227378671,1019.15714708974,1019.59287308813,
1020.02859908651,1020.46347238967,1020.89834569288,1021.33321899617,1021.76809229953,
1022.20296560297,1022.63783890648,1023.07271221007,1023.50758551375,1023.94245881752,
1024.37733212137,1024.81220542531,1025.24707872935,1025.68195203348,1026.11682533771,
1026.55255133672,1026.98827733573,1027.42315064016,1027.8580239447,1028.29289724934,
1028.72777055409,1029.16264385896,1029.59751716393,1030.03239046902,1030.46726377423,
1030.90213707956,1031.33701038501,1031.77188369058,1032.20675699628,1032.6416303021,
1033.07650360805,1033.51222960793,1033.94795560782,1034.38282891403,1034.81770222038,
1035.25257552685,1035.68744883347,1036.12232214022,1036.5571954471,1036.99206875413,
1037.4269420613,1037.86181536861,1038.29668867606,1038.73156198365,1039.16643529139,
1039.60130859927,1040.0361819073,1040.47190790824,1040.90763390917,1041.34250721749,
1041.77738052596,1042.21225383458,1042.64712714334,1043.08200045226,1043.95174707053,
1044.38662037989,1044.8214936894,1045.25636699906,1045.69124030886,1046.12611361882,
1046.56098692892,1046.99586023917,1047.43158624121,1047.86731224325,1048.3021855538,
1048.73705886448,1049.17193217531,1049.60680548629,1050.0416787974,1050.47655210866,
1050.91142542006,1051.78117204327,1052.21604535508,1052.65091866703,1053.0857919791,
1053.52066529131,1053.95553860365,1054.39126460673,1055.26186392239,1056.13161054793,
1057.00135717395,1057.43623048712,1057.87110380041,1058.7408504273,1059.61059705459,
1060.48034368225,1061.35094300009,1062.22154231809,1063.09128894656,1063.96103557531,
1064.83078220429,1065.70052883346,1066.57027546278,1067.44002209222,1068.3106214112,
1069.18122073019,1070.05096735972,1070.9207139892,1071.79046061859,1072.66020724785,
1073.52995387693,1074.39970050579,1075.27029982411,1076.1408991423,1077.01064577048,
1077.88039239832,1078.7501390258,1079.61988565289,1080.48963227957,1081.35937890581,
1082.22997822202,1083.100577538,1083.97032416305,1084.84007078759,1085.70981741161,
1086.5795640351,1087.44931065803,1087.88418396929,1088.31905728041,1088.75393059138,
1089.18965659365,1089.62538259591,1090.06025590659,1090.93000252753,1091.36487583778,
1091.79974914788,1092.23462245783,1092.66949576764,1093.1043690773,1093.5392423868,
1093.97411569616,1094.40898900538,1094.84386231444,1095.27873562335,1095.71360893212,
1096.14933493327,1096.58506093443,1097.0199342429,1097.45480755122,1097.88968085939,
1098.32455416742,1098.75942747531,1099.19430078305,1099.62917409064,1100.06404739809,
1100.4989207054,1100.93379401257,1101.36866731959,1101.80354062648,1102.23841393323,
1102.67328723984,1103.10901323993,1103.54473924001,1103.97961254636,1104.41448585257,
1104.84935915865,1105.2842324646,1105.71910577042,1106.15397907612,1106.58885238169,
1107.02372568714,1107.45859899246,1107.89347229767,1108.32834560276,1108.76321890774,
1109.1980922126,1109.63296551736,1110.06869151652,1110.50441751569,1110.93929082023,
1111.37416412466,1111.80903742899,1112.24391073322,1112.67878403735,1113.11365734139,
1113.54853064533,1113.98340394918,1114.41827725295,1114.85315055662,1115.28802386022,
1115.72289716374,1116.15777046717,1116.59264377053,1117.02836976903,1117.46409576752,
1117.89896907074,1118.33384237389,1118.76871567698,1119.20358898,1119.63846228297,
1120.07333558588,1120.50820888874,1120.94308219154,1121.3779554943,1121.81282879702,
1122.24770209969,1122.68257540233,1123.11744870492,1123.55232200749,1123.98804800561,
1124.42377400372,1124.85864730623,1125.29352060871,1125.72839391118,1126.16326721362,
1126.59814051605,1127.03301381847,1127.46788712088,1127.90276042328,1128.33763372568,
1128.77250702808,1129.20738033048,1129.64225363289,1130.07712693531,1130.51200023774,
1130.94772623581,1131.38345223388,1131.81832553634,1132.25319883883,1132.68807214134,
1133.12294544387,1133.55781874644,1133.99269204904,1134.42756535167,1134.86243865434,
1135.29731195706,1135.73218525982,1136.16705856263,1136.60193186548,1137.03680516839,
1137.47167847136,1137.90740446972,1138.34313046808,1138.77800377117,1139.21287707432,
1139.64775037754,1140.08262368083,1140.51749698419,1140.95237028763,1141.38724359114,
1141.82211689474,1142.25699019842,1142.69186350218,1143.12673680603,1143.56161010998,
1143.99648341401,1144.43135671814,1144.86708271711,1145.30280871607,1145.7376820204,
1146.17255532483,1146.60742862936,1147.04230193401,1147.47717523876,1147.91204854362,
1148.3469218486,1148.78179515369,1149.2166684589,1149.65154176423,1150.08641506968,
1150.52128837525,1150.95616168094,1151.39103498677,1151.82676098659,1152.26248698641,
1152.69736029249,1153.1322335987,1153.56710690504,1154.00198021152,1154.43685351813,
1154.87172682488,1155.30660013177,1155.7414734388,1156.17634674597,1156.61122005327,
1157.04609336073,1157.48096666832,1157.91583997606,1158.35071328394,1158.7864392848,
1159.22216528566,1159.65703859384,1160.09191190216,1160.52678521063,1160.96165851925,
1161.39653182801,1161.83140513693,1162.26627844599,1162.7011517552,1163.13602506456,
1163.57089837407,1164.00577168373,1164.44064499353,1164.87551830349,1165.74611761556,
1166.18184361753,1166.61671692792,1167.05159023846,1167.48646354915,1167.92133685998,
1168.35621017096,1169.22595679333,1170.09570341627,1170.53057672794,1170.96545003975,
1171.4003233517,1171.83519666377,1172.27006997598,1172.705795979,1173.57639529447,
1174.44614191977,1174.8810152326,1175.31588854555,1176.18563517179,1177.05538179847,
1177.92512842556,1178.79487505304,1179.66547437075,1180.53607368863,1181.40582031696,
1182.27556694557,1183.14531357444,1184.01506020352,1184.88480683277,1185.75455346216,
1186.62515278112,1187.4957521001,1188.36549872963,1189.23524535914,1190.10499198858,
1190.97473861791,1191.84448524708,1192.71423187606,1193.58483119448,1194.45543051277,
1195.3251771411,1196.19492376911,1197.06467039678,1197.93441702407,1198.80416365096,
1199.67391027742,1200.5445095938,1201.41510890996,1202.28485553525,1203.15460216005,
1204.02434878434,1204.89409540809,1205.76384203131,1206.1987153427,1206.63358865396,
1207.06846196508,1207.50418796741,1208.37478728058,1209.2445339018,1209.6794072122,
1210.11428052245,1210.54915383255,1210.9840271425,1211.41890045231,1211.85377376197,
1212.28864707147,1212.72352038083,1213.15839369005,1213.59326699911,1214.02814030802,
1214.46386630925,1214.89959231048,1215.3344656191,1215.76933892757,1216.20421223589,
1216.63908554406,1217.07395885209,1217.50883215998,1217.94370546771,1218.37857877531,
1218.81345208276,1219.24832539007,1219.68319869724,1220.11807200426,1220.55294531115,
1220.9878186179,1221.42354461805,1221.85927061821,1222.29414392468,1222.72901723103,
1223.16389053724,1223.59876384332,1224.03363714927,1224.46851045509,1224.90338376079,
1225.33825706636,1225.77313037181,1226.20800367713,1226.64287698234,1227.07775028743,
1227.51262359241,1227.94749689727,1228.3832228965,1228.81894889572,1229.25382220036,
1229.6886955049,1230.12356880933,1230.55844211366,1230.99331541789,1231.42818872202,
1231.86306202606,1232.29793533,1232.73280863385,1233.16768193762,1233.60255524129,
1234.03742854489,1234.4723018484,1234.90717515184,1235.34290115037,1235.7786271489,
1236.21350045219,1236.64837375541,1237.08324705856,1237.51812036165,1237.95299366467,
1238.38786696764,1238.82274027055,1239.25761357341,1239.69248687621,1240.12736017897,
1240.56223348169,1240.99710678436,1241.431980087,1241.8668533896,1242.30257938773,
1242.73830538585,1243.17317868839,1243.6080519909,1244.04292529338,1244.47779859585,
1244.91267189829,1245.34754520072,1245.78241850314,1246.21729180555,1246.65216510795,
1247.08703841035,1247.52191171275,1247.95678501515,1248.39165831756,1248.82653161998,
1249.26225761804,1249.69798361611,1250.13285691855,1250.56773022101,1251.0026035235,
1251.43747682601,1251.87235012854,1252.30722343111,1252.74209673371,1253.17697003634,
1253.61184333901,1254.04671664173,1254.48158994449,1254.9164632473,1255.35133655015,
1255.78620985306,1256.22193585139,1256.65766184973,1257.09253515275,1257.52740845584,
1257.96228175899,1258.39715506221,1258.8320283655,1259.26690166886,1259.7017749723,
1260.13664827581,1260.57152157941,1261.00639488309,1261.44126818685,1261.8761414907,
1262.31101479465,1262.74588809868,1263.1816140976,1263.61734009651,1264.05221340074,
1264.48708670507,1264.9219600095,1265.35683331403,1265.79170661868,1266.22657992343,
1266.66145322829,1267.09632653327,1267.53119983836,1267.96607314357,1268.4009464489,
1268.83581975434,1269.27069305992,1269.70556636561,1270.14129236537,1270.57701836513,
1271.01189167108,1271.44676497716,1271.88163828337,1272.31651158971,1272.75138489619,
1273.1862582028,1273.62113150955,1274.05600481644,1274.49087812347,1274.92575143063,
1275.36062473794,1275.79549804539,1276.23037135299,1276.66524466073,1277.10097066151,
1277.5366966623,1277.97156997033,1278.40644327851,1278.84131658683,1279.2761898953,
1279.71106320392,1280.14593651268,1280.5808098216,1281.01568313066,1281.45055643987,
1281.88542974923,1282.32030305874,1282.75517636839,1283.1900496782,1283.62492298815,
1284.06064899005,1284.49637499195,1284.9312483022,1285.36612161259,1285.80099492313,
1286.23586823382,1286.67074154465,1287.54048816674,1287.975361478,1288.4102347894,
1288.84510810093,1289.27998141261,1289.71485472442,1290.14972803636,1291.02032735139,
1291.89092666668,1292.32579997914,1292.76067329173,1293.19554660444,1293.63041991727,
1294.50016654328,1295.36991316974,1296.23965979663,1297.10940642392,1297.9800057415,
1298.85060505925,1299.72035168742,1300.5900983159,1301.45984494464,1302.32959157362,
1303.19933820279,1304.06908483212,1304.93968415104,1305.81028347,1306.68003009953,
1307.54977672906,1308.41952335854,1309.28926998793,1310.15901661718,1311.02876324626,
1311.89936256477,1312.76996188316,1313.63970851164,1314.50945513981,1315.37920176765,
1316.24894839514,1317.11869502223,1317.98844164891,1318.85904096546,1319.72964028179,
1320.59938690733,1321.46913353238,1322.33888015692,1323.20862678095,1323.64350009276,
1324.07837340443,1324.51324671597,1324.94812002737,1325.81871934103,1326.68931865441,
1327.12419196524,1327.55906527593,1327.99393858647,1328.42881189686,1328.86368520711,
1329.29855851721,1329.73343182716,1330.16830513697,1330.60317844663,1331.03805175614,
1331.4729250655,1331.90779837471,1332.34267168377,1332.77839768507,1333.21412368638,
1333.64899699514,1334.08387030376,1334.51874361223,1334.95361692055,1335.38849022873,
1335.82336353676,1336.25823684464,1336.69311015238,1337.12798345997,1337.56285676742,
1337.99773007473,1338.4326033819,1338.86747668892,1339.30234999581,1339.73807599603,
1340.17380199625,1340.60867530287,1341.04354860934,1341.47842191569,1341.9132952219,
1342.34816852798,1342.78304183393,1343.21791513975,1343.65278844545,1344.08766175102,
1344.52253505647,1344.95740836179,1345.392281667,1345.82715497209,1346.26202827707,
1346.69775427635,1347.13348027563,1347.56835358038,1348.00322688502,1348.43810018956,
1348.87297349399,1349.30784679832,1349.74272010255,1350.17759340668,1350.61246671072,
1351.04734001466,1351.48221331851,1351.91708662228,1352.35195992595,1352.78683322955,
1353.22170653306,1353.65743253163,1354.09315853019,1354.52803183356,1354.96290513685,
1355.39777844007,1355.83265174322,1356.26752504631,1356.70239834933,1357.1372716523,
1357.57214495521,1358.00701825807,1358.44189156087,1358.87676486363,1359.31163816635,
1359.74651146902,1360.18138477166,1360.6171107698,1361.05283676795,1361.48771007051,
1361.92258337305,1362.35745667556,1362.79232997804,1363.2272032805,1363.66207658295,
1364.09694988538,1364.5318231878,1364.96669649021,1365.40156979261,1365.83644309501,
1366.27131639741,1366.70618969981,1367.14106300222,1367.57678900028,1368.01251499834,
1368.44738830077,1368.88226160321,1369.31713490567,1369.75200820816,1370.18688151067,
1370.6217548132,1371.05662811577,1371.49150141837,1371.926374721,1372.36124802367,
1372.79612132639,1373.23099462915,1373.66586793196,1374.10074123481,1374.53646723311,
1374.97219323142,1375.40706653438,1375.84193983741,1376.2768131405,1376.71168644365,
1377.14655974687,1377.58143305016,1378.01630635352,1378.45117965696,1378.88605296047,
1379.32092626407,1379.75579956775,1380.19067287151,1380.62554617536,1381.06041947931,
1381.49614547817,1381.93187147704,1382.36674478117,1382.8016180854,1383.23649138973,
1383.67136469416,1384.10623799869,1384.54111130334,1384.97598460809,1385.41085791295,
1385.84573121793,1386.28060452302,1386.71547782823,1387.15035113356,1387.585224439,
1388.02009774458,1388.45582374427,1388.89154974397,1389.32642304979,1389.76129635574,
1390.19616966182,1390.63104296803,1391.06591627437,1391.50078958085,1391.93566288746,
1392.37053619421,1392.8054095011,1393.24028280813,1393.6751561153,1394.1100294226,
1394.54490273005,1394.97977603765,1395.41550203836,1395.85122803908,1396.28610134696,
1396.72097465499,1397.15584796317,1397.59072127149,1398.02559457996,1398.46046788858,
1398.89534119734,1399.33021450626,1399.76508781532,1400.19996112453,1400.63483443389,
1401.50458105306,1401.93945436286,1402.37518036469,1402.81090636651,1403.24577967661,
1403.68065298686,1404.11552629725,1404.5503996078,1404.98527291848,1405.85501954029,
1406.2898928514,1406.72476616266,1407.15963947406,1407.5945127856,1408.02938609727,
1408.46425940908,1409.33485872391,1410.205458039,1410.64033135134,1411.07520466381,
1411.51007797639,1411.9449512891,1412.81469791488,1413.68444454112,1414.5541911678,
1415.42393779489,1416.29453711233,1417.16513642995,1418.03488305796,1418.90462968629,
1419.77437631491,1420.64412294377,1421.51386957285,1422.38361620211,1423.25421552099,
1424.12481483992,1424.99456146943,1425.86430809896,1426.73405472847,1427.60380135791,
1428.47354798724,1429.34329461641,1430.21389393501,1431.08449325349,1431.9542398821,
1432.82398651043,1433.69373313844,1434.56347976611,1435.4332263934,1436.30297302029,
1437.17357233701,1438.04417165351,1438.91391827929,1439.78366490459,1440.65341152939,
1441.52315815367,1441.95803146562,1442.39290477743,1442.8277780891,1443.26265140064,
1444.13325071451,1445.00385002811,1445.43872333908,1445.87359664991,1446.3084699606,
1446.74334327114,1447.17821658153,1447.61308989178,1448.48283651184,1448.91770982164,
1449.3525831313,1449.78745644081,1450.22232975017,1450.65720305938,1451.09292906076,
1451.52865506214,1451.96352837105,1452.39840167982,1452.83327498843,1453.2681482969,
1453.70302160522,1454.1378949134,1454.57276822143,1455.00764152931,1455.44251483705,
1455.87738814464,1456.31226145209,1456.7471347594,1457.18200806657,1457.6168813736,
1458.05260737389,1458.48833337418,1458.92320668093,1459.35807998754,1459.79295329402,
1460.22782660036,1460.66269990657,1461.09757321265,1461.5324465186,1461.96731982443,
1462.40219313012,1462.83706643569,1463.27193974114,1463.70681304647,1464.14168635168,
1464.57655965677,1465.0122856561,1465.44801165544,1465.8828849603,1466.31775826505,
1466.7526315697,1467.18750487423,1467.62237817866,1468.05725148299,1468.49212478722,
1468.92699809135,1469.36187139539,1469.79674469933,1470.23161800319,1470.66649130695,
1471.10136461063,1471.53623791422,1471.97196391283,1472.40768991143,1472.84256321487,
1473.27743651823,1473.71230982152,1474.14718312474,1474.58205642789,1475.01692973098,
1475.451803034,1475.88667633697,1476.32154963988,1476.75642294274,1477.19129624555,
1477.62616954831,1478.06104285102,1478.4959161537,1478.93164215186,1479.36736815002,
1479.80224145262,1480.23711475519,1480.67198805772,1481.10686136023,1481.54173466272,
1481.97660796518,1482.41148126762,1482.84635457005,1483.28122787247,1483.71610117488,
1484.15097447728,1484.58584777968,1485.02072108208,1485.45559438449,1485.89132038254,
1486.32704638059,1486.76191968301,1487.19679298544,1487.63166628788,1488.06653959035,
1488.50141289283,1488.93628619534,1489.37115949787,1489.80603280044,1490.24090610304,
1490.67577940567,1491.11065270835,1491.54552601106,1491.98039931382,1492.41527261663,
1492.8509986149,1493.28672461318,1493.72159791609,1494.15647121906,1494.59134452208,
1495.02621782517,1495.46109112832,1495.89596443154,1496.33083773483,1496.76571103819,
1497.20058434163,1497.63545764515,1498.07033094874,1498.50520425242,1498.94007755618,
1499.37495086004,1499.81067685885,1500.24640285767,1500.68127616171,1501.11614946584,
1501.55102277007,1501.9858960744,1502.42076937883,1502.85564268337,1503.29051598801,
1503.72538929276,1504.16026259762,1504.5951359026,1505.03000920769,1505.4648825129,
1505.89975581823,1506.33462912368,1506.77035512331,1507.20608112294,1507.64095442864,
1508.07582773446,1508.51070104041,1508.94557434649,1509.3804476527,1509.81532095904,
1510.25019426552,1510.68506757213,1511.11994087888,1511.55481418577,1511.9896874928,
1512.42456079996,1512.85943410727,1513.29430741472,1513.73003341537,1514.16575941601,
1514.60063272375,1515.03550603163,1515.47037933966,1515.90525264784,1516.34012595616,
1516.77499926463,1517.20987257325,1517.64474588201,1518.07961919093,1518.51449249999,
1518.9493658092,1519.38423911856,1519.81911242807,1520.25398573772,1520.68971173947,
1521.12543774122,1521.56031105118,1521.99518436128,1522.43005767153,1523.29980429246,
1523.73467760315,1524.16955091398,1524.60442422495,1525.03929753607,1525.47417084733,
1525.90904415873,1526.77879078194,1527.64939009657,1528.08511609939,1528.51998941146,
1528.95486272367,1529.38973603601,1530.25948266106,1531.1292292866,1531.99897591261,
1532.86872253907,1533.73846916596,1534.60906848325,1535.47966780073,1536.34941442858,
1537.21916105675,1538.08890768523,1538.95865431398,1539.82840094295,1540.69814757212,
1541.56874689096,1542.43934620985,1543.30909283933,1544.17883946886,1545.04858609839,
1545.91833272787,1546.78807935726,1547.65782598651,1548.52842530518,1549.39902462375,
1550.26877125249,1551.13851788097,1552.00826450914,1552.87801113699,1553.74775776447,
1554.61750439156,1555.48810370844,1556.35870302511,1557.22844965112,1558.09819627666,
1558.96794290171,1559.83768952626,1560.27256283834,1560.70743615028,1561.57718277377,
1562.44778208785,1563.31838140165,1563.75325471277,1564.18812802374,1564.62300133457,
1565.05787464526,1565.9276212662,1566.79736788655,1567.2322411965,1567.66711450631,
1568.10198781596,1568.53686112547,1568.97173443483,1569.40746043628,1569.84318643774,
1570.2780597468,1570.71293305571,1571.14780636448,1571.5826796731,1572.01755298157,
1572.45242628989,1572.88729959806,1573.32217290609,1573.75704621397,1574.19191952171,
1574.62679282931,1575.06166613676,1575.49653944407,1575.93141275123,1576.36713875159,
1576.80286475195,1577.23773805884,1577.67261136559,1578.1074846722,1578.54235797868,
1578.97723128502,1579.41210459124,1579.84697789732,1580.28185120327,1580.71672450909,
1581.15159781478,1581.58647112036,1582.0213444258,1582.45621773113,1582.89109103634,
1583.32681703573,1583.76254303513,1584.1974163401,1584.63228964497,1585.06716294972,
1585.50203625436,1585.9369095589,1586.37178286333,1586.80665616766,1587.24152947189,
1587.67640277602,1588.11127608005,1588.546149384,1588.98102268785,1589.41589599161,
1589.85076929529,1590.28649529394,1590.72222129258,1591.1570945961,1591.59196789953,
1592.0268412029,1592.46171450619,1592.8965878094,1593.33146111256,1593.76633441564,
1594.20120771867,1594.63608102164,1595.07095432455,1595.50582762741,1595.94070093021,
1596.37557423297,1596.81044753569,1597.24617353387,1597.68189953206,1598.11677283469,
1598.55164613729,1598.98651943985,1599.42139274239,1599.8562660449,1600.29113934738,
1600.72601264985,1601.16088595229,1601.59575925472,1602.03063255714,1602.46550585955,
1602.90037916195,1603.33525246435,1603.77012576675,1604.2058517648,1604.64157776285,
1605.07645106526,1605.51132436768,1605.94619767011,1606.38107097255,1606.81594427502,
1607.2508175775,1607.68569088001,1608.12056418254,1608.55543748511,1608.99031078771,
1609.42518409034,1609.86005739302,1610.29493069573,1610.72980399849,1611.16552999674,
1611.60125599499,1612.03612929785,1612.47100260076,1612.90587590373,1613.34074920675,
1613.77562250984,1614.21049581299,1614.64536911621,1615.0802424195,1615.51511572286,
1615.9499890263,1616.38486232981,1616.81973563341,1617.25460893709,1617.68948224085,
1618.12520823963,1618.5609342384,1618.99580754234,1619.43068084638,1619.86555415051,
1620.30042745474,1620.73530075907,1621.1701740635,1621.60504736804,1622.03992067268,
1622.47479397743,1622.90966728229,1623.34454058727,1623.77941389236,1624.21428719757,
1624.6491605029,1625.08488650247,1625.52061250204,1625.95548580761,1626.39035911331,
1626.82523241913,1627.26010572508,1627.69497903116,1628.12985233737,1628.56472564372,
1628.99959895019,1629.43447225681,1629.86934556356,1630.30421887044,1630.73909217747,
1631.17396548464,1631.60883879195,1632.04456479252,1632.48029079309,1632.91516410068,
1633.35003740842,1633.78491071631,1634.21978402433,1634.65465733251,1635.08953064083,
1635.5244039493,1635.95927725792,1636.39415056668,1636.8290238756,1637.26389718466,
1637.69877049387,1638.13364380323,1638.56851711274,1639.00424311442,1639.43996911609,
1639.8748424259,1640.30971573585,1640.74458904595,1641.6143356666,1642.04920897714,
1642.48408228782,1642.91895559865,1643.35382890963,1643.78870222074,1644.223575532,
1645.09332215494,1645.52819546661,1645.96392146936,1646.39964747212,1646.83452078406,
1647.26939409614,1647.70426740834,1648.57401403314,1649.44376065844,1650.31350728422,
1650.74838059729,1651.18325391046,1652.05300053714,1652.92359985428,1653.79419917162,
1654.66394579929,1655.5336924273,1656.40343905563,1657.27318568424,1658.14293231311,
1659.01267894219,1659.88327826096,1660.75387757982,1661.62362420926,1662.49337083877,
1663.3631174683,1664.23286409781,1665.10261072725,1665.97235735658,1666.84295667531,
1667.71355599396,1668.58330262282,1669.45304925143,1670.32279587976,1671.19254250778,
1672.06228913544,1672.93203576273,1673.80263507977,1674.6732343966,1675.54298102284,
1676.41272764862,1677.28247427392,1678.15222089872,1679.021967523,1679.89171414676,
1680.76231346105,1681.19803946366,1681.63291277506,1682.06778608632,1682.50265939743,
1682.93753270841,1683.37240601924,1684.24215264047,1684.67702595086,1685.11189926111,
1685.54677257121,1685.98164588116,1686.41651919097,1686.85139250063,1687.28626581014,
1687.72199181166,1688.15771781319,1688.5925911224,1689.02746443146,1689.46233774038,
1689.89721104914,1690.33208435776,1690.76695766623,1691.20183097455,1691.63670428272,
1692.07157759075,1692.50645089864,1692.94132420637,1693.37619751397,1693.81107082142,
1694.24594412873,1694.68167012916,1695.11739612959,1695.55226943662,1695.9871427435,
1696.42201605025,1696.85688935687,1697.29176266334,1697.72663596969,1698.1615092759,
1698.59638258198,1699.03125588793,1699.46612919375,1699.90100249945,1700.33587580502,
1700.77074911047,1701.20562241579,1701.64134841525,1702.0770744147,1702.51194771979,
1702.94682102476,1703.38169432963,1703.81656763438,1704.25144093902,1704.68631424356,
1705.12118754799,1705.55606085232,1705.99093415655,1706.42580746068,1706.86068076471,
1707.29555406866,1707.73042737251,1708.16530067627,1708.60102667496,1709.03675267365,
1709.47162597724,1709.90649928076,1710.34137258419,1710.77624588756,1711.21111919085,
1711.64599249406,1712.08086579722,1712.5157391003,1712.95061240333,1713.3854857063,
1713.82035900921,1714.25523231207,1714.69010561487,1715.12497891763,1715.56070491584,
1715.99643091404,1716.43130421671,1716.86617751935,1717.30105082195,1717.73592412451,
1718.17079742705,1718.60567072956,1719.04054403204,1719.4754173345,1719.91029063695,
1720.34516393938,1720.7800372418,1721.21491054421,1721.64978384661,1722.08465714901,
1722.52038314706,1722.9561091451,1723.39098244751,1723.82585574992,1724.26072905233,
1724.69560235476,1725.13047565721,1725.56534895967,1726.00022226216,1726.43509556467,
1726.8699688672,1727.30484216977,1727.73971547236,1728.174588775,1728.60946207767,
1729.04433538039,1729.48006137861,1729.91578737684,1730.35066067965,1730.78553398251,
1731.22040728542,1731.65528058838,1732.09015389141,1732.5250271945,1732.95990049765,
1733.39477380087,1733.82964710416,1734.26452040752,1734.69939371096,1735.13426701447,
1735.56914031807,1736.00401362175,1736.43973962048,1736.8754656192,1737.31033892306,
1737.745212227,1738.18008553104,1738.61495883517,1739.0498321394,1739.48470544373,
1739.91957874816,1740.35445205269,1740.78932535734,1741.22419866209,1741.65907196695,
1742.09394527193,1742.52881857702,1742.96369188223,1743.39941788174,1743.83514388125,
1744.2700171867,1744.70489049227,1745.13976379797,1745.57463710379,1746.00951040974,
1746.44438371582,1746.87925702203,1747.31413032837,1747.74900363485,1748.18387694146,
1748.61875024821,1749.0536235551,1749.48849686213,1749.92337016929,1750.3590961698,
1750.7948221703,1751.22969547775,1751.66456878534,1752.09944209308,1752.53431540096,
1752.96918870899,1753.40406201717,1753.83893532549,1754.27380863396,1754.70868194258,
1755.14355525134,1755.57842856026,1756.01330186932,1756.44817517853,1756.88304848789,
1757.31877448949,1757.75450049109,1758.18937380075,1759.05912042051,1759.49399373061,
1759.92886704086,1760.36374035125,1760.79861366179,1761.23348697248,1761.66836028331,
1762.10323359429,1762.5381069054,1763.40785352806,1763.8427268396,1764.27845284228,
1764.71417884496,1765.14905215677,1765.58392546872,1766.0187987808,1766.88854540534,
1767.75829203039,1768.1931653431,1768.62803865593,1769.06291196888,1769.49778528195,
1770.36753190841,1771.2381312254,1772.10873054259,1772.97847717007,1773.84822379791,
1774.71797042609,1775.58771705456,1776.45746368331,1777.32721031228,1778.19780963089,
1779.06840894783,1779.93815555508,1780.80790201176,1781.67764871408),(-1.76619037896906,
-1.18309518948453),.UNSPECIFIED.) ;
#825 = B_SPLINE_SURFACE_WITH_KNOTS('',3,1,((#64564,#64565),(#64566,#64567),
(#64568,#64569),(#64570,#64571),(#64572,#64573),(#64574,#64575),(#64576,
#64577),(#64578,#64579),(#64580,#64581),(#64582,#64583),(#64584,#64585),
(#64586,#64587),(#64588,#64589),(#64590,#64591),(#64592,#64593),(#64594,
#64595),(#64596,#64597),(#64598,#64599),(#64600,#64601),(#64602,#64603),
(#64604,#64605),(#64606,#64607),(#64608,#64609),(#64610,#64611),(#64612,
#64613),(#64614,#64615),(#64616,#64617),(#64618,#64619),(#64620,#64621),
(#64622,#64623),(#64624,#64625),(#64626,#64627),(#64628,#64629),(#64630,
#64631),(#64632,#64633),(#64634,#64635),(#64636,#64637),(#64638,#64639),
(#64640,#64641),(#64642,#64643),(#64644,#64645),(#64646,#64647),(#64648,
#64649),(#64650,#64651),(#64652,#64653),(#64654,#64655),(#64656,#64657),
(#64658,#64659),(#64660,#64661),(#64662,#64663),(#64664,#64665),(#64666,
#64667),(#64668,#64669),(#64670,#64671),(#64672,#64673),(#64674,#64675),
(#64676,#64677),(#64678,#64679),(#64680,#64681),(#64682,#64683),(#64684,
#64685),(#64686,#64687),(#64688,#64689),(#64690,#64691),(#64692,#64693),
(#64694,#64695),(#64696,#64697),(#64698,#64699),(#64700,#64701),(#64702,
#64703),(#64704,#64705),(#64706,#64707),(#64708,#64709),(#64710,#64711),
(#64712,#64713),(#64714,#64715),(#64716,#64717),(#64718,#64719),(#64720,
#64721),(#64722,#64723),(#64724,#64725),(#64726,#64727),(#64728,#64729),
(#64730,#64731),(#64732,#64733),(#64734,#64735),(#64736,#64737),(#64738,
#64739),(#64740,#64741),(#64742,#64743),(#64744,#64745),(#64746,#64747),
(#64748,#64749),(#64750,#64751),(#64752,#64753),(#64754,#64755),(#64756,
#64757),(#64758,#64759),(#64760,#64761),(#64762,#64763),(#64764,#64765),
(#64766,#64767),(#64768,#64769),(#64770,#64771),(#64772,#64773),(#64774,
#64775),(#64776,#64777),(#64778,#64779),(#64780,#64781),(#64782,#64783),
(#64784,#64785),(#64786,#64787),(#64788,#64789),(#64790,#64791),(#64792,
#64793),(#64794,#64795),(#64796,#64797),(#64798,#64799),(#64800,#64801),
(#64802,#64803),(#64804,#64805),(#64806,#64807),(#64808,#64809),(#64810,
#64811),(#64812,#64813),(#64814,#64815),(#64816,#64817),(#64818,#64819),
(#64820,#64821),(#64822,#64823),(#64824,#64825),(#64826,#64827),(#64828,
#64829),(#64830,#64831),(#64832,#64833),(#64834,#64835),(#64836,#64837),
(#64838,#64839),(#64840,#64841),(#64842,#64843),(#64844,#64845),(#64846,
#64847),(#64848,#64849),(#64850,#64851),(#64852,#64853),(#64854,#64855),
(#64856,#64857),(#64858,#64859),(#64860,#64861),(#64862,#64863),(#64864,
#64865),(#64866,#64867),(#64868,#64869),(#64870,#64871),(#64872,#64873),
(#64874,#64875),(#64876,#64877),(#64878,#64879),(#64880,#64881),(#64882,
#64883),(#64884,#64885),(#64886,#64887),(#64888,#64889),(#64890,#64891),
(#64892,#64893),(#64894,#64895),(#64896,#64897),(#64898,#64899),(#64900,
#64901),(#64902,#64903),(#64904,#64905),(#64906,#64907),(#64908,#64909),
(#64910,#64911),(#64912,#64913),(#64914,#64915),(#64916,#64917),(#64918,
#64919),(#64920,#64921),(#64922,#64923),(#64924,#64925),(#64926,#64927),
(#64928,#64929),(#64930,#64931),(#64932,#64933),(#64934,#64935),(#64936,
#64937),(#64938,#64939),(#64940,#64941),(#64942,#64943),(#64944,#64945),
(#64946,#64947),(#64948,#64949),(#64950,#64951),(#64952,#64953),(#64954,
#64955),(#64956,#64957),(#64958,#64959),(#64960,#64961),(#64962,#64963),
(#64964,#64965),(#64966,#64967),(#64968,#64969),(#64970,#64971),(#64972,
#64973),(#64974,#64975),(#64976,#64977),(#64978,#64979),(#64980,#64981),
(#64982,#64983),(#64984,#64985),(#64986,#64987),(#64988,#64989),(#64990,
#64991),(#64992,#64993),(#64994,#64995),(#64996,#64997),(#64998,#64999),
(#65000,#65001),(#65002,#65003),(#65004,#65005),(#65006,#65007),(#65008,
#65009),(#65010,#65011),(#65012,#65013),(#65014,#65015),(#65016,#65017),
(#65018,#65019),(#65020,#65021),(#65022,#65023),(#65024,#65025),(#65026,
#65027),(#65028,#65029),(#65030,#65031),(#65032,#65033),(#65034,#65035),
(#65036,#65037),(#65038,#65039),(#65040,#65041),(#65042,#65043),(#65044,
#65045),(#65046,#65047),(#65048,#65049),(#65050,#65051),(#65052,#65053),
(#65054,#65055),(#65056,#65057),(#65058,#65059),(#65060,#65061),(#65062,
#65063),(#65064,#65065),(#65066,#65067),(#65068,#65069),(#65070,#65071),
(#65072,#65073),(#65074,#65075),(#65076,#65077),(#65078,#65079),(#65080,
#65081),(#65082,#65083),(#65084,#65085),(#65086,#65087),(#65088,#65089),
(#65090,#65091),(#65092,#65093),(#65094,#65095),(#65096,#65097),(#65098,
#65099),(#65100,#65101),(#65102,#65103),(#65104,#65105),(#65106,#65107),
(#65108,#65109),(#65110,#65111),(#65112,#65113),(#65114,#65115),(#65116,
#65117),(#65118,#65119),(#65120,#65121),(#65122,#65123),(#65124,#65125),
(#65126,#65127),(#65128,#65129),(#65130,#65131),(#65132,#65133),(#65134,
#65135),(#65136,#65137),(#65138,#65139),(#65140,#65141),(#65142,#65143),
(#65144,#65145),(#65146,#65147),(#65148,#65149),(#65150,#65151),(#65152,
#65153),(#65154,#65155),(#65156,#65157),(#65158,#65159),(#65160,#65161),
(#65162,#65163),(#65164,#65165),(#65166,#65167),(#65168,#65169),(#65170,
#65171),(#65172,#65173),(#65174,#65175),(#65176,#65177),(#65178,#65179),
(#65180,#65181),(#65182,#65183),(#65184,#65185),(#65186,#65187),(#65188,
#65189),(#65190,#65191),(#65192,#65193),(#65194,#65195),(#65196,#65197),
(#65198,#65199),(#65200,#65201),(#65202,#65203),(#65204,#65205),(#65206,
#65207),(#65208,#65209),(#65210,#65211),(#65212,#65213),(#65214,#65215),
(#65216,#65217),(#65218,#65219),(#65220,#65221),(#65222,#65223),(#65224,
#65225),(#65226,#65227),(#65228,#65229),(#65230,#65231),(#65232,#65233),
(#65234,#65235),(#65236,#65237),(#65238,#65239),(#65240,#65241),(#65242,
#65243),(#65244,#65245),(#65246,#65247),(#65248,#65249),(#65250,#65251),
(#65252,#65253),(#65254,#65255),(#65256,#65257),(#65258,#65259),(#65260,
#65261),(#65262,#65263),(#65264,#65265),(#65266,#65267),(#65268,#65269),
(#65270,#65271),(#65272,#65273),(#65274,#65275),(#65276,#65277),(#65278,
#65279),(#65280,#65281),(#65282,#65283),(#65284,#65285),(#65286,#65287),
(#65288,#65289),(#65290,#65291),(#65292,#65293),(#65294,#65295),(#65296,
#65297),(#65298,#65299),(#65300,#65301),(#65302,#65303),(#65304,#65305),
(#65306,#65307),(#65308,#65309),(#65310,#65311),(#65312,#65313),(#65314,
#65315),(#65316,#65317),(#65318,#65319),(#65320,#65321),(#65322,#65323),
(#65324,#65325),(#65326,#65327),(#65328,#65329),(#65330,#65331),(#65332,
#65333),(#65334,#65335),(#65336,#65337),(#65338,#65339),(#65340,#65341),
(#65342,#65343),(#65344,#65345),(#65346,#65347),(#65348,#65349),(#65350,
#65351),(#65352,#65353),(#65354,#65355),(#65356,#65357),(#65358,#65359),
(#65360,#65361),(#65362,#65363),(#65364,#65365),(#65366,#65367),(#65368,
#65369),(#65370,#65371),(#65372,#65373),(#65374,#65375),(#65376,#65377),
(#65378,#65379),(#65380,#65381),(#65382,#65383),(#65384,#65385),(#65386,
#65387),(#65388,#65389),(#65390,#65391),(#65392,#65393),(#65394,#65395),
(#65396,#65397),(#65398,#65399),(#65400,#65401),(#65402,#65403),(#65404,
#65405),(#65406,#65407),(#65408,#65409),(#65410,#65411),(#65412,#65413),
(#65414,#65415),(#65416,#65417),(#65418,#65419),(#65420,#65421),(#65422,
#65423),(#65424,#65425),(#65426,#65427),(#65428,#65429),(#65430,#65431),
(#65432,#65433),(#65434,#65435),(#65436,#65437),(#65438,#65439),(#65440,
#65441),(#65442,#65443),(#65444,#65445),(#65446,#65447),(#65448,#65449),
(#65450,#65451),(#65452,#65453),(#65454,#65455),(#65456,#65457),(#65458,
#65459),(#65460,#65461),(#65462,#65463),(#65464,#65465),(#65466,#65467),
(#65468,#65469),(#65470,#65471),(#65472,#65473),(#65474,#65475),(#65476,
#65477),(#65478,#65479),(#65480,#65481),(#65482,#65483),(#65484,#65485),
(#65486,#65487),(#65488,#65489),(#65490,#65491),(#65492,#65493),(#65494,
#65495),(#65496,#65497),(#65498,#65499),(#65500,#65501),(#65502,#65503),
(#65504,#65505),(#65506,#65507),(#65508,#65509),(#65510,#65511),(#65512,
#65513),(#65514,#65515),(#65516,#65517),(#65518,#65519),(#65520,#65521),
(#65522,#65523),(#65524,#65525),(#65526,#65527),(#65528,#65529),(#65530,
#65531),(#65532,#65533),(#65534,#65535),(#65536,#65537),(#65538,#65539),
(#65540,#65541),(#65542,#65543),(#65544,#65545),(#65546,#65547),(#65548,
#65549),(#65550,#65551),(#65552,#65553),(#65554,#65555),(#65556,#65557),
(#65558,#65559),(#65560,#65561),(#65562,#65563),(#65564,#65565),(#65566,
#65567),(#65568,#65569),(#65570,#65571),(#65572,#65573),(#65574,#65575),
(#65576,#65577),(#65578,#65579),(#65580,#65581),(#65582,#65583),(#65584,
#65585),(#65586,#65587),(#65588,#65589),(#65590,#65591),(#65592,#65593),
(#65594,#65595),(#65596,#65597),(#65598,#65599),(#65600,#65601),(#65602,
#65603),(#65604,#65605),(#65606,#65607),(#65608,#65609),(#65610,#65611),
(#65612,#65613),(#65614,#65615),(#65616,#65617),(#65618,#65619),(#65620,
#65621),(#65622,#65623),(#65624,#65625),(#65626,#65627),(#65628,#65629),
(#65630,#65631),(#65632,#65633),(#65634,#65635),(#65636,#65637),(#65638,
#65639),(#65640,#65641),(#65642,#65643),(#65644,#65645),(#65646,#65647),
(#65648,#65649),(#65650,#65651),(#65652,#65653),(#65654,#65655),(#65656,
#65657),(#65658,#65659),(#65660,#65661),(#65662,#65663),(#65664,#65665),
(#65666,#65667),(#65668,#65669),(#65670,#65671),(#65672,#65673),(#65674,
#65675),(#65676,#65677),(#65678,#65679),(#65680,#65681),(#65682,#65683),
(#65684,#65685),(#65686,#65687),(#65688,#65689),(#65690,#65691),(#65692,
#65693),(#65694,#65695),(#65696,#65697),(#65698,#65699),(#65700,#65701),
(#65702,#65703),(#65704,#65705),(#65706,#65707),(#65708,#65709),(#65710,
#65711),(#65712,#65713),(#65714,#65715),(#65716,#65717),(#65718,#65719),
(#65720,#65721),(#65722,#65723),(#65724,#65725),(#65726,#65727),(#65728,
#65729),(#65730,#65731),(#65732,#65733),(#65734,#65735),(#65736,#65737),
(#65738,#65739),(#65740,#65741),(#65742,#65743),(#65744,#65745),(#65746,
#65747),(#65748,#65749),(#65750,#65751),(#65752,#65753),(#65754,#65755),
(#65756,#65757),(#65758,#65759),(#65760,#65761),(#65762,#65763),(#65764,
#65765),(#65766,#65767),(#65768,#65769),(#65770,#65771),(#65772,#65773),
(#65774,#65775),(#65776,#65777),(#65778,#65779),(#65780,#65781),(#65782,
#65783),(#65784,#65785),(#65786,#65787),(#65788,#65789),(#65790,#65791),
(#65792,#65793),(#65794,#65795),(#65796,#65797),(#65798,#65799),(#65800,
#65801),(#65802,#65803),(#65804,#65805),(#65806,#65807),(#65808,#65809),
(#65810,#65811),(#65812,#65813),(#65814,#65815),(#65816,#65817),(#65818,
#65819),(#65820,#65821),(#65822,#65823),(#65824,#65825),(#65826,#65827),
(#65828,#65829),(#65830,#65831),(#65832,#65833),(#65834,#65835),(#65836,
#65837),(#65838,#65839),(#65840,#65841),(#65842,#65843),(#65844,#65845),
(#65846,#65847),(#65848,#65849),(#65850,#65851),(#65852,#65853),(#65854,
#65855),(#65856,#65857),(#65858,#65859),(#65860,#65861),(#65862,#65863),
(#65864,#65865),(#65866,#65867),(#65868,#65869),(#65870,#65871),(#65872,
#65873),(#65874,#65875),(#65876,#65877),(#65878,#65879),(#65880,#65881),
(#65882,#65883),(#65884,#65885),(#65886,#65887),(#65888,#65889),(#65890,
#65891),(#65892,#65893),(#65894,#65895),(#65896,#65897),(#65898,#65899),
(#65900,#65901),(#65902,#65903),(#65904,#65905),(#65906,#65907),(#65908,
#65909),(#65910,#65911),(#65912,#65913),(#65914,#65915),(#65916,#65917),
(#65918,#65919),(#65920,#65921),(#65922,#65923),(#65924,#65925),(#65926,
#65927),(#65928,#65929),(#65930,#65931),(#65932,#65933),(#65934,#65935),
(#65936,#65937),(#65938,#65939),(#65940,#65941),(#65942,#65943),(#65944,
#65945),(#65946,#65947),(#65948,#65949),(#65950,#65951),(#65952,#65953),
(#65954,#65955),(#65956,#65957),(#65958,#65959),(#65960,#65961),(#65962,
#65963),(#65964,#65965),(#65966,#65967),(#65968,#65969),(#65970,#65971),
(#65972,#65973),(#65974,#65975),(#65976,#65977),(#65978,#65979),(#65980,
#65981),(#65982,#65983),(#65984,#65985),(#65986,#65987),(#65988,#65989),
(#65990,#65991),(#65992,#65993),(#65994,#65995),(#65996,#65997),(#65998,
#65999),(#66000,#66001),(#66002,#66003),(#66004,#66005),(#66006,#66007),
(#66008,#66009),(#66010,#66011),(#66012,#66013),(#66014,#66015),(#66016,
#66017),(#66018,#66019),(#66020,#66021),(#66022,#66023),(#66024,#66025),
(#66026,#66027),(#66028,#66029),(#66030,#66031),(#66032,#66033),(#66034,
#66035),(#66036,#66037),(#66038,#66039),(#66040,#66041),(#66042,#66043),
(#66044,#66045),(#66046,#66047),(#66048,#66049),(#66050,#66051),(#66052,
#66053),(#66054,#66055),(#66056,#66057),(#66058,#66059),(#66060,#66061),
(#66062,#66063),(#66064,#66065),(#66066,#66067),(#66068,#66069),(#66070,
#66071),(#66072,#66073),(#66074,#66075),(#66076,#66077),(#66078,#66079),
(#66080,#66081),(#66082,#66083),(#66084,#66085),(#66086,#66087),(#66088,
#66089),(#66090,#66091),(#66092,#66093),(#66094,#66095),(#66096,#66097),
(#66098,#66099),(#66100,#66101),(#66102,#66103),(#66104,#66105),(#66106,
#66107),(#66108,#66109),(#66110,#66111),(#66112,#66113),(#66114,#66115),
(#66116,#66117),(#66118,#66119),(#66120,#66121),(#66122,#66123),(#66124,
#66125),(#66126,#66127),(#66128,#66129),(#66130,#66131),(#66132,#66133),
(#66134,#66135),(#66136,#66137),(#66138,#66139),(#66140,#66141),(#66142,
#66143),(#66144,#66145),(#66146,#66147),(#66148,#66149),(#66150,#66151),
(#66152,#66153),(#66154,#66155),(#66156,#66157),(#66158,#66159),(#66160,
#66161),(#66162,#66163),(#66164,#66165),(#66166,#66167),(#66168,#66169),
(#66170,#66171),(#66172,#66173),(#66174,#66175),(#66176,#66177),(#66178,
#66179),(#66180,#66181),(#66182,#66183),(#66184,#66185),(#66186,#66187),
(#66188,#66189),(#66190,#66191),(#66192,#66193),(#66194,#66195),(#66196,
#66197),(#66198,#66199),(#66200,#66201),(#66202,#66203),(#66204,#66205),
(#66206,#66207),(#66208,#66209),(#66210,#66211),(#66212,#66213),(#66214,
#66215),(#66216,#66217),(#66218,#66219),(#66220,#66221),(#66222,#66223),
(#66224,#66225),(#66226,#66227),(#66228,#66229),(#66230,#66231),(#66232,
#66233),(#66234,#66235),(#66236,#66237),(#66238,#66239),(#66240,#66241),
(#66242,#66243),(#66244,#66245),(#66246,#66247),(#66248,#66249),(#66250,
#66251),(#66252,#66253),(#66254,#66255),(#66256,#66257),(#66258,#66259),
(#66260,#66261),(#66262,#66263),(#66264,#66265),(#66266,#66267),(#66268,
#66269),(#66270,#66271),(#66272,#66273),(#66274,#66275),(#66276,#66277),
(#66278,#66279),(#66280,#66281),(#66282,#66283),(#66284,#66285),(#66286,
#66287),(#66288,#66289),(#66290,#66291),(#66292,#66293),(#66294,#66295),
(#66296,#66297),(#66298,#66299),(#66300,#66301),(#66302,#66303),(#66304,
#66305),(#66306,#66307),(#66308,#66309),(#66310,#66311),(#66312,#66313),
(#66314,#66315),(#66316,#66317),(#66318,#66319),(#66320,#66321),(#66322,
#66323),(#66324,#66325),(#66326,#66327),(#66328,#66329),(#66330,#66331),
(#66332,#66333),(#66334,#66335),(#66336,#66337),(#66338,#66339),(#66340,
#66341),(#66342,#66343),(#66344,#66345),(#66346,#66347),(#66348,#66349),
(#66350,#66351),(#66352,#66353),(#66354,#66355),(#66356,#66357),(#66358,
#66359),(#66360,#66361),(#66362,#66363),(#66364,#66365),(#66366,#66367),
(#66368,#66369),(#66370,#66371),(#66372,#66373),(#66374,#66375),(#66376,
#66377),(#66378,#66379),(#66380,#66381),(#66382,#66383),(#66384,#66385),
(#66386,#66387),(#66388,#66389),(#66390,#66391),(#66392,#66393),(#66394,
#66395),(#66396,#66397),(#66398,#66399),(#66400,#66401),(#66402,#66403),
(#66404,#66405),(#66406,#66407),(#66408,#66409),(#66410,#66411),(#66412,
#66413),(#66414,#66415),(#66416,#66417),(#66418,#66419),(#66420,#66421),
(#66422,#66423),(#66424,#66425),(#66426,#66427),(#66428,#66429),(#66430,
#66431),(#66432,#66433),(#66434,#66435),(#66436,#66437),(#66438,#66439),
(#66440,#66441),(#66442,#66443),(#66444,#66445),(#66446,#66447),(#66448,
#66449),(#66450,#66451),(#66452,#66453),(#66454,#66455),(#66456,#66457),
(#66458,#66459),(#66460,#66461),(#66462,#66463),(#66464,#66465),(#66466,
#66467),(#66468,#66469),(#66470,#66471),(#66472,#66473),(#66474,#66475),
(#66476,#66477),(#66478,#66479),(#66480,#66481),(#66482,#66483),(#66484,
#66485),(#66486,#66487),(#66488,#66489),(#66490,#66491),(#66492,#66493),
(#66494,#66495),(#66496,#66497),(#66498,#66499),(#66500,#66501),(#66502,
#66503),(#66504,#66505),(#66506,#66507),(#66508,#66509),(#66510,#66511),
(#66512,#66513),(#66514,#66515),(#66516,#66517),(#66518,#66519),(#66520,
#66521),(#66522,#66523),(#66524,#66525),(#66526,#66527),(#66528,#66529),
(#66530,#66531),(#66532,#66533),(#66534,#66535),(#66536,#66537),(#66538,
#66539),(#66540,#66541),(#66542,#66543),(#66544,#66545),(#66546,#66547),
(#66548,#66549),(#66550,#66551),(#66552,#66553),(#66554,#66555),(#66556,
#66557),(#66558,#66559),(#66560,#66561),(#66562,#66563),(#66564,#66565),
(#66566,#66567),(#66568,#66569),(#66570,#66571),(#66572,#66573),(#66574,
#66575),(#66576,#66577),(#66578,#66579),(#66580,#66581),(#66582,#66583),
(#66584,#66585),(#66586,#66587),(#66588,#66589),(#66590,#66591),(#66592,
#66593),(#66594,#66595),(#66596,#66597),(#66598,#66599),(#66600,#66601),
(#66602,#66603),(#66604,#66605),(#66606,#66607),(#66608,#66609),(#66610,
#66611),(#66612,#66613),(#66614,#66615),(#66616,#66617),(#66618,#66619),
(#66620,#66621),(#66622,#66623),(#66624,#66625),(#66626,#66627),(#66628,
#66629),(#66630,#66631),(#66632,#66633),(#66634,#66635),(#66636,#66637),
(#66638,#66639),(#66640,#66641),(#66642,#66643),(#66644,#66645),(#66646,
#66647),(#66648,#66649),(#66650,#66651),(#66652,#66653),(#66654,#66655),
(#66656,#66657),(#66658,#66659),(#66660,#66661),(#66662,#66663),(#66664,
#66665),(#66666,#66667),(#66668,#66669),(#66670,#66671),(#66672,#66673),
(#66674,#66675),(#66676,#66677),(#66678,#66679),(#66680,#66681),(#66682,
#66683),(#66684,#66685),(#66686,#66687),(#66688,#66689),(#66690,#66691),
(#66692,#66693),(#66694,#66695),(#66696,#66697),(#66698,#66699),(#66700,
#66701),(#66702,#66703),(#66704,#66705),(#66706,#66707),(#66708,#66709),
(#66710,#66711),(#66712,#66713),(#66714,#66715),(#66716,#66717),(#66718,
#66719),(#66720,#66721),(#66722,#66723),(#66724,#66725),(#66726,#66727),
(#66728,#66729),(#66730,#66731),(#66732,#66733),(#66734,#66735),(#66736,
#66737),(#66738,#66739),(#66740,#66741),(#66742,#66743),(#66744,#66745),
(#66746,#66747),(#66748,#66749),(#66750,#66751),(#66752,#66753),(#66754,
#66755),(#66756,#66757),(#66758,#66759),(#66760,#66761),(#66762,#66763),
(#66764,#66765),(#66766,#66767),(#66768,#66769),(#66770,#66771),(#66772,
#66773),(#66774,#66775),(#66776,#66777),(#66778,#66779),(#66780,#66781),
(#66782,#66783),(#66784,#66785),(#66786,#66787),(#66788,#66789),(#66790,
#66791),(#66792,#66793),(#66794,#66795),(#66796,#66797),(#66798,#66799),
(#66800,#66801),(#66802,#66803),(#66804,#66805),(#66806,#66807),(#66808,
#66809),(#66810,#66811),(#66812,#66813),(#66814,#66815),(#66816,#66817),
(#66818,#66819),(#66820,#66821),(#66822,#66823),(#66824,#66825),(#66826,
#66827),(#66828,#66829),(#66830,#66831),(#66832,#66833),(#66834,#66835),
(#66836,#66837),(#66838,#66839),(#66840,#66841),(#66842,#66843),(#66844,
#66845),(#66846,#66847),(#66848,#66849),(#66850,#66851),(#66852,#66853),
(#66854,#66855),(#66856,#66857),(#66858,#66859),(#66860,#66861),(#66862,
#66863),(#66864,#66865),(#66866,#66867),(#66868,#66869),(#66870,#66871),
(#66872,#66873),(#66874,#66875),(#66876,#66877),(#66878,#66879),(#66880,
#66881),(#66882,#66883),(#66884,#66885),(#66886,#66887),(#66888,#66889),
(#66890,#66891),(#66892,#66893),(#66894,#66895),(#66896,#66897),(#66898,
#66899),(#66900,#66901),(#66902,#66903),(#66904,#66905),(#66906,#66907),
(#66908,#66909),(#66910,#66911),(#66912,#66913),(#66914,#66915),(#66916,
#66917),(#66918,#66919),(#66920,#66921),(#66922,#66923),(#66924,#66925),
(#66926,#66927),(#66928,#66929),(#66930,#66931),(#66932,#66933),(#66934,
#66935),(#66936,#66937),(#66938,#66939),(#66940,#66941),(#66942,#66943),
(#66944,#66945),(#66946,#66947),(#66948,#66949),(#66950,#66951),(#66952,
#66953),(#66954,#66955),(#66956,#66957),(#66958,#66959),(#66960,#66961),
(#66962,#66963),(#66964,#66965),(#66966,#66967),(#66968,#66969),(#66970,
#66971),(#66972,#66973),(#66974,#66975),(#66976,#66977),(#66978,#66979),
(#66980,#66981),(#66982,#66983),(#66984,#66985),(#66986,#66987),(#66988,
#66989),(#66990,#66991),(#66992,#66993),(#66994,#66995),(#66996,#66997),
(#66998,#66999),(#67000,#67001),(#67002,#67003),(#67004,#67005),(#67006,
#67007),(#67008,#67009),(#67010,#67011),(#67012,#67013),(#67014,#67015),
(#67016,#67017),(#67018,#67019),(#67020,#67021),(#67022,#67023),(#67024,
#67025),(#67026,#67027),(#67028,#67029),(#67030,#67031),(#67032,#67033),
(#67034,#67035),(#67036,#67037),(#67038,#67039),(#67040,#67041),(#67042,
#67043),(#67044,#67045),(#67046,#67047),(#67048,#67049),(#67050,#67051),
(#67052,#67053),(#67054,#67055),(#67056,#67057),(#67058,#67059),(#67060,
#67061),(#67062,#67063),(#67064,#67065),(#67066,#67067),(#67068,#67069),
(#67070,#67071),(#67072,#67073),(#67074,#67075),(#67076,#67077),(#67078,
#67079),(#67080,#67081),(#67082,#67083),(#67084,#67085),(#67086,#67087),
(#67088,#67089),(#67090,#67091),(#67092,#67093),(#67094,#67095),(#67096,
#67097),(#67098,#67099),(#67100,#67101),(#67102,#67103),(#67104,#67105),
(#67106,#67107),(#67108,#67109),(#67110,#67111),(#67112,#67113),(#67114,
#67115),(#67116,#67117),(#67118,#67119),(#67120,#67121),(#67122,#67123),
(#67124,#67125),(#67126,#67127),(#67128,#67129),(#67130,#67131),(#67132,
#67133),(#67134,#67135),(#67136,#67137),(#67138,#67139),(#67140,#67141),
(#67142,#67143),(#67144,#67145),(#67146,#67147),(#67148,#67149),(#67150,
#67151),(#67152,#67153),(#67154,#67155),(#67156,#67157),(#67158,#67159),
(#67160,#67161),(#67162,#67163),(#67164,#67165),(#67166,#67167),(#67168,
#67169),(#67170,#67171),(#67172,#67173),(#67174,#67175),(#67176,#67177),
(#67178,#67179),(#67180,#67181),(#67182,#67183),(#67184,#67185),(#67186,
#67187),(#67188,#67189),(#67190,#67191),(#67192,#67193),(#67194,#67195),
(#67196,#67197),(#67198,#67199),(#67200,#67201),(#67202,#67203),(#67204,
#67205),(#67206,#67207),(#67208,#67209),(#67210,#67211),(#67212,#67213),
(#67214,#67215),(#67216,#67217),(#67218,#67219),(#67220,#67221),(#67222,
#67223),(#67224,#67225),(#67226,#67227),(#67228,#67229),(#67230,#67231),
(#67232,#67233),(#67234,#67235),(#67236,#67237),(#67238,#67239),(#67240,
#67241),(#67242,#67243),(#67244,#67245),(#67246,#67247),(#67248,#67249),
(#67250,#67251),(#67252,#67253),(#67254,#67255),(#67256,#67257),(#67258,
#67259),(#67260,#67261),(#67262,#67263),(#67264,#67265),(#67266,#67267),
(#67268,#67269),(#67270,#67271),(#67272,#67273),(#67274,#67275),(#67276,
#67277),(#67278,#67279),(#67280,#67281),(#67282,#67283),(#67284,#67285),
(#67286,#67287),(#67288,#67289),(#67290,#67291),(#67292,#67293),(#67294,
#67295),(#67296,#67297),(#67298,#67299),(#67300,#67301),(#67302,#67303),
(#67304,#67305),(#67306,#67307),(#67308,#67309),(#67310,#67311),(#67312,
#67313),(#67314,#67315),(#67316,#67317),(#67318,#67319),(#67320,#67321),
(#67322,#67323),(#67324,#67325),(#67326,#67327),(#67328,#67329),(#67330,
#67331),(#67332,#67333),(#67334,#67335),(#67336,#67337),(#67338,#67339),
(#67340,#67341),(#67342,#67343),(#67344,#67345),(#67346,#67347),(#67348,
#67349),(#67350,#67351),(#67352,#67353),(#67354,#67355),(#67356,#67357),
(#67358,#67359),(#67360,#67361),(#67362,#67363),(#67364,#67365),(#67366,
#67367),(#67368,#67369),(#67370,#67371),(#67372,#67373),(#67374,#67375),
(#67376,#67377),(#67378,#67379),(#67380,#67381),(#67382,#67383),(#67384,
#67385),(#67386,#67387),(#67388,#67389),(#67390,#67391),(#67392,#67393),
(#67394,#67395),(#67396,#67397),(#67398,#67399),(#67400,#67401),(#67402,
#67403),(#67404,#67405),(#67406,#67407),(#67408,#67409),(#67410,#67411),
(#67412,#67413),(#67414,#67415),(#67416,#67417),(#67418,#67419),(#67420,
#67421),(#67422,#67423),(#67424,#67425),(#67426,#67427),(#67428,#67429),
(#67430,#67431),(#67432,#67433),(#67434,#67435),(#67436,#67437),(#67438,
#67439),(#67440,#67441),(#67442,#67443),(#67444,#67445),(#67446,#67447),
(#67448,#67449),(#67450,#67451),(#67452,#67453),(#67454,#67455),(#67456,
#67457),(#67458,#67459),(#67460,#67461),(#67462,#67463),(#67464,#67465),
(#67466,#67467),(#67468,#67469),(#67470,#67471),(#67472,#67473),(#67474,
#67475),(#67476,#67477),(#67478,#67479),(#67480,#67481),(#67482,#67483),
(#67484,#67485),(#67486,#67487),(#67488,#67489),(#67490,#67491),(#67492,
#67493),(#67494,#67495),(#67496,#67497),(#67498,#67499),(#67500,#67501),
(#67502,#67503),(#67504,#67505),(#67506,#67507),(#67508,#67509),(#67510,
#67511),(#67512,#67513),(#67514,#67515),(#67516,#67517),(#67518,#67519),
(#67520,#67521),(#67522,#67523),(#67524,#67525),(#67526,#67527),(#67528,
#67529),(#67530,#67531),(#67532,#67533),(#67534,#67535),(#67536,#67537),
(#67538,#67539),(#67540,#67541),(#67542,#67543),(#67544,#67545),(#67546,
#67547),(#67548,#67549),(#67550,#67551),(#67552,#67553),(#67554,#67555),
(#67556,#67557),(#67558,#67559),(#67560,#67561),(#67562,#67563),(#67564,
#67565),(#67566,#67567),(#67568,#67569),(#67570,#67571),(#67572,#67573),
(#67574,#67575),(#67576,#67577),(#67578,#67579),(#67580,#67581),(#67582,
#67583),(#67584,#67585),(#67586,#67587),(#67588,#67589),(#67590,#67591),
(#67592,#67593),(#67594,#67595),(#67596,#67597),(#67598,#67599),(#67600,
#67601),(#67602,#67603),(#67604,#67605),(#67606,#67607),(#67608,#67609),
(#67610,#67611),(#67612,#67613),(#67614,#67615),(#67616,#67617),(#67618,
#67619),(#67620,#67621),(#67622,#67623),(#67624,#67625),(#67626,#67627),
(#67628,#67629),(#67630,#67631),(#67632,#67633),(#67634,#67635),(#67636,
#67637),(#67638,#67639),(#67640,#67641),(#67642,#67643),(#67644,#67645),
(#67646,#67647),(#67648,#67649),(#67650,#67651),(#67652,#67653),(#67654,
#67655),(#67656,#67657),(#67658,#67659),(#67660,#67661),(#67662,#67663),
(#67664,#67665),(#67666,#67667),(#67668,#67669),(#67670,#67671),(#67672,
#67673),(#67674,#67675),(#67676,#67677),(#67678,#67679),(#67680,#67681),
(#67682,#67683),(#67684,#67685),(#67686,#67687),(#67688,#67689),(#67690,
#67691),(#67692,#67693),(#67694,#67695),(#67696,#67697),(#67698,#67699),
(#67700,#67701),(#67702,#67703),(#67704,#67705),(#67706,#67707),(#67708,
#67709),(#67710,#67711),(#67712,#67713),(#67714,#67715),(#67716,#67717),
(#67718,#67719),(#67720,#67721),(#67722,#67723),(#67724,#67725),(#67726,
#67727),(#67728,#67729),(#67730,#67731),(#67732,#67733),(#67734,#67735),
(#67736,#67737),(#67738,#67739),(#67740,#67741),(#67742,#67743),(#67744,
#67745),(#67746,#67747),(#67748,#67749),(#67750,#67751),(#67752,#67753),
(#67754,#67755),(#67756,#67757),(#67758,#67759),(#67760,#67761),(#67762,
#67763),(#67764,#67765),(#67766,#67767),(#67768,#67769),(#67770,#67771),
(#67772,#67773),(#67774,#67775),(#67776,#67777),(#67778,#67779),(#67780,
#67781),(#67782,#67783),(#67784,#67785),(#67786,#67787),(#67788,#67789),
(#67790,#67791),(#67792,#67793),(#67794,#67795),(#67796,#67797),(#67798,
#67799),(#67800,#67801),(#67802,#67803),(#67804,#67805),(#67806,#67807),
(#67808,#67809),(#67810,#67811),(#67812,#67813),(#67814,#67815),(#67816,
#67817),(#67818,#67819),(#67820,#67821),(#67822,#67823),(#67824,#67825),
(#67826,#67827),(#67828,#67829),(#67830,#67831),(#67832,#67833),(#67834,
#67835),(#67836,#67837),(#67838,#67839),(#67840,#67841),(#67842,#67843),
(#67844,#67845),(#67846,#67847),(#67848,#67849),(#67850,#67851),(#67852,
#67853),(#67854,#67855),(#67856,#67857),(#67858,#67859),(#67860,#67861),
(#67862,#67863),(#67864,#67865),(#67866,#67867),(#67868,#67869),(#67870,
#67871),(#67872,#67873),(#67874,#67875),(#67876,#67877),(#67878,#67879),
(#67880,#67881),(#67882,#67883),(#67884,#67885),(#67886,#67887),(#67888,
#67889),(#67890,#67891),(#67892,#67893),(#67894,#67895),(#67896,#67897),
(#67898,#67899),(#67900,#67901),(#67902,#67903),(#67904,#67905),(#67906,
#67907),(#67908,#67909),(#67910,#67911),(#67912,#67913),(#67914,#67915),
(#67916,#67917),(#67918,#67919),(#67920,#67921),(#67922,#67923),(#67924,
#67925),(#67926,#67927),(#67928,#67929),(#67930,#67931),(#67932,#67933),
(#67934,#67935),(#67936,#67937),(#67938,#67939),(#67940,#67941),(#67942,
#67943),(#67944,#67945),(#67946,#67947),(#67948,#67949),(#67950,#67951),
(#67952,#67953),(#67954,#67955),(#67956,#67957),(#67958,#67959),(#67960,
#67961),(#67962,#67963),(#67964,#67965),(#67966,#67967),(#67968,#67969),
(#67970,#67971),(#67972,#67973),(#67974,#67975),(#67976,#67977),(#67978,
#67979),(#67980,#67981),(#67982,#67983),(#67984,#67985),(#67986,#67987),
(#67988,#67989),(#67990,#67991),(#67992,#67993),(#67994,#67995),(#67996,
#67997),(#67998,#67999),(#68000,#68001),(#68002,#68003),(#68004,#68005),
(#68006,#68007),(#68008,#68009),(#68010,#68011),(#68012,#68013),(#68014,
#68015),(#68016,#68017),(#68018,#68019),(#68020,#68021),(#68022,#68023),
(#68024,#68025),(#68026,#68027),(#68028,#68029),(#68030,#68031),(#68032,
#68033),(#68034,#68035),(#68036,#68037),(#68038,#68039),(#68040,#68041),
(#68042,#68043),(#68044,#68045),(#68046,#68047),(#68048,#68049),(#68050,
#68051),(#68052,#68053),(#68054,#68055),(#68056,#68057),(#68058,#68059),
(#68060,#68061),(#68062,#68063),(#68064,#68065),(#68066,#68067),(#68068,
#68069),(#68070,#68071),(#68072,#68073),(#68074,#68075),(#68076,#68077),
(#68078,#68079),(#68080,#68081),(#68082,#68083),(#68084,#68085),(#68086,
#68087),(#68088,#68089),(#68090,#68091),(#68092,#68093),(#68094,#68095),
(#68096,#68097),(#68098,#68099),(#68100,#68101),(#68102,#68103),(#68104,
#68105),(#68106,#68107),(#68108,#68109),(#68110,#68111),(#68112,#68113),
(#68114,#68115),(#68116,#68117),(#68118,#68119),(#68120,#68121),(#68122,
#68123),(#68124,#68125),(#68126,#68127),(#68128,#68129),(#68130,#68131),
(#68132,#68133),(#68134,#68135),(#68136,#68137),(#68138,#68139),(#68140,
#68141),(#68142,#68143),(#68144,#68145),(#68146,#68147),(#68148,#68149),
(#68150,#68151),(#68152,#68153),(#68154,#68155),(#68156,#68157),(#68158,
#68159),(#68160,#68161),(#68162,#68163),(#68164,#68165),(#68166,#68167),
(#68168,#68169),(#68170,#68171),(#68172,#68173),(#68174,#68175),(#68176,
#68177),(#68178,#68179),(#68180,#68181),(#68182,#68183),(#68184,#68185),
(#68186,#68187),(#68188,#68189),(#68190,#68191),(#68192,#68193),(#68194,
#68195),(#68196,#68197),(#68198,#68199),(#68200,#68201),(#68202,#68203),
(#68204,#68205),(#68206,#68207),(#68208,#68209),(#68210,#68211),(#68212,
#68213),(#68214,#68215),(#68216,#68217),(#68218,#68219),(#68220,#68221),
(#68222,#68223),(#68224,#68225),(#68226,#68227),(#68228,#68229),(#68230,
#68231),(#68232,#68233),(#68234,#68235),(#68236,#68237),(#68238,#68239),
(#68240,#68241),(#68242,#68243),(#68244,#68245),(#68246,#68247),(#68248,
#68249),(#68250,#68251),(#68252,#68253),(#68254,#68255),(#68256,#68257),
(#68258,#68259),(#68260,#68261),(#68262,#68263),(#68264,#68265),(#68266,
#68267),(#68268,#68269),(#68270,#68271),(#68272,#68273),(#68274,#68275),
(#68276,#68277),(#68278,#68279),(#68280,#68281),(#68282,#68283),(#68284,
#68285),(#68286,#68287),(#68288,#68289),(#68290,#68291),(#68292,#68293),
(#68294,#68295),(#68296,#68297),(#68298,#68299),(#68300,#68301),(#68302,
#68303),(#68304,#68305),(#68306,#68307),(#68308,#68309),(#68310,#68311),
(#68312,#68313),(#68314,#68315),(#68316,#68317),(#68318,#68319),(#68320,
#68321),(#68322,#68323),(#68324,#68325),(#68326,#68327),(#68328,#68329),
(#68330,#68331),(#68332,#68333),(#68334,#68335),(#68336,#68337),(#68338,
#68339),(#68340,#68341),(#68342,#68343),(#68344,#68345),(#68346,#68347),
(#68348,#68349),(#68350,#68351),(#68352,#68353),(#68354,#68355),(#68356,
#68357),(#68358,#68359),(#68360,#68361),(#68362,#68363),(#68364,#68365),
(#68366,#68367),(#68368,#68369),(#68370,#68371),(#68372,#68373),(#68374,
#68375),(#68376,#68377),(#68378,#68379),(#68380,#68381),(#68382,#68383),
(#68384,#68385),(#68386,#68387),(#68388,#68389),(#68390,#68391),(#68392,
#68393),(#68394,#68395),(#68396,#68397),(#68398,#68399),(#68400,#68401),
(#68402,#68403),(#68404,#68405),(#68406,#68407),(#68408,#68409),(#68410,
#68411),(#68412,#68413),(#68414,#68415),(#68416,#68417),(#68418,#68419),
(#68420,#68421),(#68422,#68423),(#68424,#68425),(#68426,#68427),(#68428,
#68429),(#68430,#68431),(#68432,#68433),(#68434,#68435),(#68436,#68437),
(#68438,#68439),(#68440,#68441),(#68442,#68443),(#68444,#68445),(#68446,
#68447),(#68448,#68449),(#68450,#68451),(#68452,#68453),(#68454,#68455),
(#68456,#68457),(#68458,#68459),(#68460,#68461),(#68462,#68463),(#68464,
#68465),(#68466,#68467),(#68468,#68469),(#68470,#68471),(#68472,#68473),
(#68474,#68475),(#68476,#68477),(#68478,#68479),(#68480,#68481),(#68482,
#68483),(#68484,#68485),(#68486,#68487),(#68488,#68489),(#68490,#68491),
(#68492,#68493),(#68494,#68495),(#68496,#68497),(#68498,#68499),(#68500,
#68501),(#68502,#68503),(#68504,#68505),(#68506,#68507),(#68508,#68509),
(#68510,#68511),(#68512,#68513),(#68514,#68515),(#68516,#68517),(#68518,
#68519),(#68520,#68521),(#68522,#68523),(#68524,#68525),(#68526,#68527),
(#68528,#68529),(#68530,#68531),(#68532,#68533),(#68534,#68535),(#68536,
#68537),(#68538,#68539),(#68540,#68541),(#68542,#68543),(#68544,#68545),
(#68546,#68547),(#68548,#68549),(#68550,#68551),(#68552,#68553),(#68554,
#68555),(#68556,#68557),(#68558,#68559),(#68560,#68561),(#68562,#68563),
(#68564,#68565),(#68566,#68567),(#68568,#68569),(#68570,#68571),(#68572,
#68573),(#68574,#68575),(#68576,#68577),(#68578,#68579),(#68580,#68581),
(#68582,#68583),(#68584,#68585),(#68586,#68587),(#68588,#68589),(#68590,
#68591),(#68592,#68593),(#68594,#68595),(#68596,#68597),(#68598,#68599),
(#68600,#68601),(#68602,#68603),(#68604,#68605),(#68606,#68607),(#68608,
#68609),(#68610,#68611),(#68612,#68613),(#68614,#68615),(#68616,#68617),
(#68618,#68619),(#68620,#68621),(#68622,#68623),(#68624,#68625),(#68626,
#68627),(#68628,#68629),(#68630,#68631),(#68632,#68633),(#68634,#68635),
(#68636,#68637),(#68638,#68639),(#68640,#68641),(#68642,#68643),(#68644,
#68645),(#68646,#68647),(#68648,#68649),(#68650,#68651),(#68652,#68653),
(#68654,#68655),(#68656,#68657),(#68658,#68659),(#68660,#68661),(#68662,
#68663),(#68664,#68665),(#68666,#68667),(#68668,#68669),(#68670,#68671),
(#68672,#68673),(#68674,#68675),(#68676,#68677),(#68678,#68679),(#68680,
#68681),(#68682,#68683),(#68684,#68685),(#68686,#68687),(#68688,#68689),
(#68690,#68691),(#68692,#68693),(#68694,#68695),(#68696,#68697),(#68698,
#68699),(#68700,#68701),(#68702,#68703),(#68704,#68705),(#68706,#68707),
(#68708,#68709),(#68710,#68711),(#68712,#68713),(#68714,#68715),(#68716,
#68717),(#68718,#68719),(#68720,#68721),(#68722,#68723),(#68724,#68725),
(#68726,#68727),(#68728,#68729),(#68730,#68731),(#68732,#68733),(#68734,
#68735),(#68736,#68737),(#68738,#68739),(#68740,#68741),(#68742,#68743),
(#68744,#68745),(#68746,#68747),(#68748,#68749),(#68750,#68751),(#68752,
#68753),(#68754,#68755),(#68756,#68757),(#68758,#68759),(#68760,#68761),
(#68762,#68763),(#68764,#68765),(#68766,#68767),(#68768,#68769),(#68770,
#68771),(#68772,#68773),(#68774,#68775),(#68776,#68777),(#68778,#68779),
(#68780,#68781),(#68782,#68783),(#68784,#68785),(#68786,#68787),(#68788,
#68789),(#68790,#68791),(#68792,#68793),(#68794,#68795),(#68796,#68797),
(#68798,#68799),(#68800,#68801),(#68802,#68803),(#68804,#68805),(#68806,
#68807),(#68808,#68809),(#68810,#68811),(#68812,#68813),(#68814,#68815),
(#68816,#68817),(#68818,#68819),(#68820,#68821),(#68822,#68823),(#68824,
#68825),(#68826,#68827),(#68828,#68829),(#68830,#68831),(#68832,#68833),
(#68834,#68835),(#68836,#68837),(#68838,#68839),(#68840,#68841),(#68842,
#68843),(#68844,#68845),(#68846,#68847),(#68848,#68849),(#68850,#68851),
(#68852,#68853),(#68854,#68855),(#68856,#68857),(#68858,#68859),(#68860,
#68861),(#68862,#68863),(#68864,#68865),(#68866,#68867),(#68868,#68869),
(#68870,#68871),(#68872,#68873),(#68874,#68875),(#68876,#68877),(#68878,
#68879),(#68880,#68881),(#68882,#68883),(#68884,#68885),(#68886,#68887),
(#68888,#68889),(#68890,#68891),(#68892,#68893),(#68894,#68895),(#68896,
#68897),(#68898,#68899),(#68900,#68901),(#68902,#68903),(#68904,#68905),
(#68906,#68907),(#68908,#68909),(#68910,#68911),(#68912,#68913),(#68914,
#68915),(#68916,#68917),(#68918,#68919),(#68920,#68921),(#68922,#68923),
(#68924,#68925),(#68926,#68927),(#68928,#68929),(#68930,#68931),(#68932,
#68933),(#68934,#68935),(#68936,#68937),(#68938,#68939),(#68940,#68941),
(#68942,#68943),(#68944,#68945),(#68946,#68947),(#68948,#68949),(#68950,
#68951),(#68952,#68953),(#68954,#68955),(#68956,#68957),(#68958,#68959),
(#68960,#68961),(#68962,#68963),(#68964,#68965),(#68966,#68967),(#68968,
#68969),(#68970,#68971),(#68972,#68973),(#68974,#68975),(#68976,#68977),
(#68978,#68979),(#68980,#68981),(#68982,#68983),(#68984,#68985),(#68986,
#68987),(#68988,#68989),(#68990,#68991),(#68992,#68993),(#68994,#68995),
(#68996,#68997),(#68998,#68999),(#69000,#69001),(#69002,#69003),(#69004,
#69005),(#69006,#69007),(#69008,#69009),(#69010,#69011),(#69012,#69013),
(#69014,#69015),(#69016,#69017),(#69018,#69019),(#69020,#69021),(#69022,
#69023),(#69024,#69025),(#69026,#69027),(#69028,#69029),(#69030,#69031),
(#69032,#69033),(#69034,#69035),(#69036,#69037),(#69038,#69039),(#69040,
#69041),(#69042,#69043),(#69044,#69045),(#69046,#69047),(#69048,#69049),
(#69050,#69051),(#69052,#69053),(#69054,#69055),(#69056,#69057),(#69058,
#69059),(#69060,#69061),(#69062,#69063),(#69064,#69065),(#69066,#69067),
(#69068,#69069),(#69070,#69071),(#69072,#69073),(#69074,#69075),(#69076,
#69077),(#69078,#69079),(#69080,#69081),(#69082,#69083),(#69084,#69085),
(#69086,#69087),(#69088,#69089),(#69090,#69091),(#69092,#69093),(#69094,
#69095),(#69096,#69097),(#69098,#69099),(#69100,#69101),(#69102,#69103),
(#69104,#69105),(#69106,#69107),(#69108,#69109),(#69110,#69111),(#69112,
#69113),(#69114,#69115),(#69116,#69117),(#69118,#69119),(#69120,#69121),
(#69122,#69123),(#69124,#69125),(#69126,#69127),(#69128,#69129),(#69130,
#69131),(#69132,#69133),(#69134,#69135),(#69136,#69137),(#69138,#69139),
(#69140,#69141),(#69142,#69143),(#69144,#69145),(#69146,#69147),(#69148,
#69149),(#69150,#69151),(#69152,#69153),(#69154,#69155),(#69156,#69157),
(#69158,#69159),(#69160,#69161),(#69162,#69163),(#69164,#69165),(#69166,
#69167),(#69168,#69169),(#69170,#69171),(#69172,#69173),(#69174,#69175),
(#69176,#69177),(#69178,#69179),(#69180,#69181),(#69182,#69183),(#69184,
#69185),(#69186,#69187),(#69188,#69189),(#69190,#69191),(#69192,#69193),
(#69194,#69195),(#69196,#69197),(#69198,#69199),(#69200,#69201),(#69202,
#69203),(#69204,#69205),(#69206,#69207),(#69208,#69209),(#69210,#69211),
(#69212,#69213),(#69214,#69215),(#69216,#69217),(#69218,#69219),(#69220,
#69221),(#69222,#69223),(#69224,#69225),(#69226,#69227),(#69228,#69229),
(#69230,#69231),(#69232,#69233),(#69234,#69235),(#69236,#69237),(#69238,
#69239),(#69240,#69241),(#69242,#69243),(#69244,#69245),(#69246,#69247),
(#69248,#69249),(#69250,#69251),(#69252,#69253),(#69254,#69255),(#69256,
#69257),(#69258,#69259),(#69260,#69261),(#69262,#69263),(#69264,#69265),
(#69266,#69267),(#69268,#69269),(#69270,#69271),(#69272,#69273),(#69274,
#69275),(#69276,#69277),(#69278,#69279),(#69280,#69281),(#69282,#69283),
(#69284,#69285),(#69286,#69287),(#69288,#69289),(#69290,#69291),(#69292,
#69293),(#69294,#69295),(#69296,#69297),(#69298,#69299),(#69300,#69301),
(#69302,#69303),(#69304,#69305),(#69306,#69307),(#69308,#69309),(#69310,
#69311),(#69312,#69313),(#69314,#69315),(#69316,#69317),(#69318,#69319),
(#69320,#69321),(#69322,#69323),(#69324,#69325),(#69326,#69327),(#69328,
#69329),(#69330,#69331),(#69332,#69333),(#69334,#69335),(#69336,#69337),
(#69338,#69339),(#69340,#69341),(#69342,#69343),(#69344,#69345),(#69346,
#69347),(#69348,#69349),(#69350,#69351),(#69352,#69353),(#69354,#69355),
(#69356,#69357),(#69358,#69359),(#69360,#69361),(#69362,#69363),(#69364,
#69365),(#69366,#69367),(#69368,#69369),(#69370,#69371),(#69372,#69373),
(#69374,#69375),(#69376,#69377),(#69378,#69379),(#69380,#69381),(#69382,
#69383),(#69384,#69385),(#69386,#69387),(#69388,#69389),(#69390,#69391),
(#69392,#69393),(#69394,#69395),(#69396,#69397),(#69398,#69399),(#69400,
#69401),(#69402,#69403),(#69404,#69405),(#69406,#69407),(#69408,#69409),
(#69410,#69411),(#69412,#69413),(#69414,#69415),(#69416,#69417),(#69418,
#69419),(#69420,#69421),(#69422,#69423),(#69424,#69425),(#69426,#69427),
(#69428,#69429),(#69430,#69431),(#69432,#69433),(#69434,#69435),(#69436,
#69437),(#69438,#69439),(#69440,#69441),(#69442,#69443),(#69444,#69445),
(#69446,#69447),(#69448,#69449),(#69450,#69451),(#69452,#69453),(#69454,
#69455),(#69456,#69457),(#69458,#69459),(#69460,#69461),(#69462,#69463),
(#69464,#69465),(#69466,#69467),(#69468,#69469),(#69470,#69471),(#69472,
#69473),(#69474,#69475),(#69476,#69477),(#69478,#69479),(#69480,#69481),
(#69482,#69483),(#69484,#69485),(#69486,#69487),(#69488,#69489),(#69490,
#69491),(#69492,#69493),(#69494,#69495),(#69496,#69497),(#69498,#69499),
(#69500,#69501),(#69502,#69503),(#69504,#69505),(#69506,#69507),(#69508,
#69509),(#69510,#69511),(#69512,#69513),(#69514,#69515),(#69516,#69517),
(#69518,#69519),(#69520,#69521),(#69522,#69523),(#69524,#69525),(#69526,
#69527),(#69528,#69529),(#69530,#69531),(#69532,#69533),(#69534,#69535),
(#69536,#69537),(#69538,#69539),(#69540,#69541),(#69542,#69543),(#69544,
#69545),(#69546,#69547),(#69548,#69549),(#69550,#69551),(#69552,#69553),
(#69554,#69555),(#69556,#69557),(#69558,#69559),(#69560,#69561),(#69562,
#69563),(#69564,#69565),(#69566,#69567),(#69568,#69569),(#69570,#69571),
(#69572,#69573),(#69574,#69575),(#69576,#69577),(#69578,#69579),(#69580,
#69581),(#69582,#69583),(#69584,#69585),(#69586,#69587),(#69588,#69589),
(#69590,#69591),(#69592,#69593),(#69594,#69595),(#69596,#69597),(#69598,
#69599),(#69600,#69601),(#69602,#69603),(#69604,#69605),(#69606,#69607),
(#69608,#69609),(#69610,#69611),(#69612,#69613),(#69614,#69615),(#69616,
#69617),(#69618,#69619),(#69620,#69621),(#69622,#69623),(#69624,#69625),
(#69626,#69627),(#69628,#69629),(#69630,#69631),(#69632,#69633),(#69634,
#69635),(#69636,#69637),(#69638,#69639),(#69640,#69641),(#69642,#69643),
(#69644,#69645),(#69646,#69647),(#69648,#69649),(#69650,#69651),(#69652,
#69653),(#69654,#69655),(#69656,#69657),(#69658,#69659),(#69660,#69661),
(#69662,#69663),(#69664,#69665),(#69666,#69667),(#69668,#69669),(#69670,
#69671),(#69672,#69673),(#69674,#69675),(#69676,#69677),(#69678,#69679),
(#69680,#69681),(#69682,#69683),(#69684,#69685),(#69686,#69687),(#69688,
#69689),(#69690,#69691),(#69692,#69693),(#69694,#69695),(#69696,#69697),
(#69698,#69699),(#69700,#69701),(#69702,#69703),(#69704,#69705),(#69706,
#69707),(#69708,#69709),(#69710,#69711),(#69712,#69713),(#69714,#69715),
(#69716,#69717),(#69718,#69719),(#69720,#69721),(#69722,#69723),(#69724,
#69725),(#69726,#69727),(#69728,#69729),(#69730,#69731),(#69732,#69733),
(#69734,#69735),(#69736,#69737),(#69738,#69739),(#69740,#69741),(#69742,
#69743),(#69744,#69745),(#69746,#69747),(#69748,#69749),(#69750,#69751),
(#69752,#69753),(#69754,#69755),(#69756,#69757),(#69758,#69759),(#69760,
#69761),(#69762,#69763),(#69764,#69765),(#69766,#69767),(#69768,#69769),
(#69770,#69771),(#69772,#69773),(#69774,#69775),(#69776,#69777),(#69778,
#69779),(#69780,#69781),(#69782,#69783),(#69784,#69785),(#69786,#69787),
(#69788,#69789),(#69790,#69791),(#69792,#69793),(#69794,#69795),(#69796,
#69797),(#69798,#69799),(#69800,#69801),(#69802,#69803),(#69804,#69805),
(#69806,#69807),(#69808,#69809),(#69810,#69811),(#69812,#69813),(#69814,
#69815),(#69816,#69817),(#69818,#69819),(#69820,#69821),(#69822,#69823),
(#69824,#69825),(#69826,#69827),(#69828,#69829),(#69830,#69831),(#69832,
#69833),(#69834,#69835),(#69836,#69837),(#69838,#69839),(#69840,#69841),
(#69842,#69843),(#69844,#69845),(#69846,#69847),(#69848,#69849),(#69850,
#69851),(#69852,#69853),(#69854,#69855),(#69856,#69857),(#69858,#69859),
(#69860,#69861),(#69862,#69863),(#69864,#69865),(#69866,#69867),(#69868,
#69869),(#69870,#69871),(#69872,#69873),(#69874,#69875),(#69876,#69877),
(#69878,#69879),(#69880,#69881),(#69882,#69883),(#69884,#69885),(#69886,
#69887),(#69888,#69889),(#69890,#69891),(#69892,#69893),(#69894,#69895),
(#69896,#69897),(#69898,#69899),(#69900,#69901),(#69902,#69903),(#69904,
#69905),(#69906,#69907),(#69908,#69909),(#69910,#69911),(#69912,#69913),
(#69914,#69915),(#69916,#69917),(#69918,#69919),(#69920,#69921),(#69922,
#69923),(#69924,#69925),(#69926,#69927),(#69928,#69929),(#69930,#69931),
(#69932,#69933),(#69934,#69935),(#69936,#69937),(#69938,#69939),(#69940,
#69941),(#69942,#69943),(#69944,#69945),(#69946,#69947),(#69948,#69949),
(#69950,#69951),(#69952,#69953),(#69954,#69955),(#69956,#69957),(#69958,
#69959),(#69960,#69961),(#69962,#69963),(#69964,#69965),(#69966,#69967),
(#69968,#69969),(#69970,#69971),(#69972,#69973),(#69974,#69975),(#69976,
#69977),(#69978,#69979),(#69980,#69981),(#69982,#69983),(#69984,#69985),
(#69986,#69987),(#69988,#69989),(#69990,#69991),(#69992,#69993),(#69994,
#69995),(#69996,#69997),(#69998,#69999),(#70000,#70001),(#70002,#70003),
(#70004,#70005),(#70006,#70007),(#70008,#70009),(#70010,#70011),(#70012,
#70013),(#70014,#70015),(#70016,#70017),(#70018,#70019),(#70020,#70021),
(#70022,#70023),(#70024,#70025),(#70026,#70027),(#70028,#70029),(#70030,
#70031),(#70032,#70033),(#70034,#70035),(#70036,#70037),(#70038,#70039),
(#70040,#70041),(#70042,#70043),(#70044,#70045),(#70046,#70047),(#70048,
#70049),(#70050,#70051),(#70052,#70053),(#70054,#70055),(#70056,#70057),
(#70058,#70059),(#70060,#70061),(#70062,#70063),(#70064,#70065),(#70066,
#70067),(#70068,#70069),(#70070,#70071),(#70072,#70073),(#70074,#70075),
(#70076,#70077),(#70078,#70079),(#70080,#70081),(#70082,#70083),(#70084,
#70085),(#70086,#70087),(#70088,#70089),(#70090,#70091),(#70092,#70093),
(#70094,#70095),(#70096,#70097),(#70098,#70099),(#70100,#70101),(#70102,
#70103),(#70104,#70105),(#70106,#70107),(#70108,#70109),(#70110,#70111),
(#70112,#70113),(#70114,#70115),(#70116,#70117),(#70118,#70119),(#70120,
#70121),(#70122,#70123),(#70124,#70125),(#70126,#70127),(#70128,#70129),
(#70130,#70131),(#70132,#70133),(#70134,#70135),(#70136,#70137),(#70138,
#70139),(#70140,#70141),(#70142,#70143),(#70144,#70145),(#70146,#70147),
(#70148,#70149),(#70150,#70151),(#70152,#70153),(#70154,#70155),(#70156,
#70157),(#70158,#70159),(#70160,#70161),(#70162,#70163),(#70164,#70165),
(#70166,#70167),(#70168,#70169),(#70170,#70171),(#70172,#70173),(#70174,
#70175),(#70176,#70177),(#70178,#70179),(#70180,#70181),(#70182,#70183),
(#70184,#70185),(#70186,#70187),(#70188,#70189),(#70190,#70191),(#70192,
#70193),(#70194,#70195),(#70196,#70197),(#70198,#70199),(#70200,#70201),
(#70202,#70203),(#70204,#70205),(#70206,#70207),(#70208,#70209),(#70210,
#70211),(#70212,#70213),(#70214,#70215),(#70216,#70217),(#70218,#70219),
(#70220,#70221),(#70222,#70223),(#70224,#70225),(#70226,#70227),(#70228,
#70229),(#70230,#70231),(#70232,#70233),(#70234,#70235),(#70236,#70237),
(#70238,#70239),(#70240,#70241),(#70242,#70243),(#70244,#70245),(#70246,
#70247),(#70248,#70249),(#70250,#70251),(#70252,#70253),(#70254,#70255),
(#70256,#70257),(#70258,#70259),(#70260,#70261),(#70262,#70263),(#70264,
#70265),(#70266,#70267),(#70268,#70269),(#70270,#70271),(#70272,#70273),
(#70274,#70275),(#70276,#70277),(#70278,#70279),(#70280,#70281),(#70282,
#70283),(#70284,#70285),(#70286,#70287),(#70288,#70289),(#70290,#70291),
(#70292,#70293),(#70294,#70295),(#70296,#70297),(#70298,#70299),(#70300,
#70301),(#70302,#70303),(#70304,#70305),(#70306,#70307),(#70308,#70309),
(#70310,#70311),(#70312,#70313),(#70314,#70315),(#70316,#70317),(#70318,
#70319),(#70320,#70321),(#70322,#70323),(#70324,#70325),(#70326,#70327),
(#70328,#70329),(#70330,#70331),(#70332,#70333),(#70334,#70335),(#70336,
#70337),(#70338,#70339),(#70340,#70341),(#70342,#70343),(#70344,#70345),
(#70346,#70347),(#70348,#70349),(#70350,#70351),(#70352,#70353),(#70354,
#70355),(#70356,#70357),(#70358,#70359),(#70360,#70361),(#70362,#70363),
(#70364,#70365),(#70366,#70367),(#70368,#70369),(#70370,#70371),(#70372,
#70373),(#70374,#70375),(#70376,#70377),(#70378,#70379),(#70380,#70381),
(#70382,#70383),(#70384,#70385),(#70386,#70387),(#70388,#70389),(#70390,
#70391),(#70392,#70393),(#70394,#70395),(#70396,#70397),(#70398,#70399),
(#70400,#70401),(#70402,#70403),(#70404,#70405),(#70406,#70407),(#70408,
#70409),(#70410,#70411),(#70412,#70413),(#70414,#70415),(#70416,#70417),
(#70418,#70419),(#70420,#70421),(#70422,#70423),(#70424,#70425),(#70426,
#70427),(#70428,#70429),(#70430,#70431),(#70432,#70433),(#70434,#70435),
(#70436,#70437),(#70438,#70439),(#70440,#70441),(#70442,#70443),(#70444,
#70445),(#70446,#70447),(#70448,#70449),(#70450,#70451),(#70452,#70453),
(#70454,#70455),(#70456,#70457),(#70458,#70459),(#70460,#70461),(#70462,
#70463),(#70464,#70465),(#70466,#70467),(#70468,#70469),(#70470,#70471),
(#70472,#70473),(#70474,#70475),(#70476,#70477),(#70478,#70479),(#70480,
#70481),(#70482,#70483),(#70484,#70485),(#70486,#70487),(#70488,#70489),
(#70490,#70491),(#70492,#70493),(#70494,#70495),(#70496,#70497),(#70498,
#70499),(#70500,#70501),(#70502,#70503),(#70504,#70505),(#70506,#70507),
(#70508,#70509),(#70510,#70511),(#70512,#70513),(#70514,#70515),(#70516,
#70517),(#70518,#70519),(#70520,#70521),(#70522,#70523),(#70524,#70525),
(#70526,#70527),(#70528,#70529),(#70530,#70531),(#70532,#70533),(#70534,
#70535),(#70536,#70537),(#70538,#70539),(#70540,#70541),(#70542,#70543),
(#70544,#70545),(#70546,#70547),(#70548,#70549),(#70550,#70551),(#70552,
#70553),(#70554,#70555),(#70556,#70557),(#70558,#70559),(#70560,#70561),
(#70562,#70563),(#70564,#70565),(#70566,#70567),(#70568,#70569),(#70570,
#70571),(#70572,#70573),(#70574,#70575),(#70576,#70577),(#70578,#70579),
(#70580,#70581),(#70582,#70583),(#70584,#70585),(#70586,#70587),(#70588,
#70589),(#70590,#70591),(#70592,#70593),(#70594,#70595),(#70596,#70597),
(#70598,#70599),(#70600,#70601),(#70602,#70603),(#70604,#70605),(#70606,
#70607),(#70608,#70609),(#70610,#70611),(#70612,#70613),(#70614,#70615),
(#70616,#70617),(#70618,#70619),(#70620,#70621),(#70622,#70623),(#70624,
#70625),(#70626,#70627),(#70628,#70629),(#70630,#70631),(#70632,#70633),
(#70634,#70635),(#70636,#70637),(#70638,#70639),(#70640,#70641),(#70642,
#70643),(#70644,#70645),(#70646,#70647),(#70648,#70649),(#70650,#70651),
(#70652,#70653),(#70654,#70655),(#70656,#70657),(#70658,#70659),(#70660,
#70661),(#70662,#70663),(#70664,#70665),(#70666,#70667),(#70668,#70669),
(#70670,#70671),(#70672,#70673),(#70674,#70675),(#70676,#70677),(#70678,
#70679),(#70680,#70681),(#70682,#70683),(#70684,#70685),(#70686,#70687),
(#70688,#70689),(#70690,#70691),(#70692,#70693),(#70694,#70695),(#70696,
#70697),(#70698,#70699),(#70700,#70701),(#70702,#70703),(#70704,#70705),
(#70706,#70707),(#70708,#70709),(#70710,#70711),(#70712,#70713),(#70714,
#70715),(#70716,#70717),(#70718,#70719),(#70720,#70721),(#70722,#70723),
(#70724,#70725),(#70726,#70727),(#70728,#70729),(#70730,#70731),(#70732,
#70733),(#70734,#70735),(#70736,#70737),(#70738,#70739),(#70740,#70741),
(#70742,#70743),(#70744,#70745),(#70746,#70747),(#70748,#70749),(#70750,
#70751),(#70752,#70753),(#70754,#70755),(#70756,#70757),(#70758,#70759),
(#70760,#70761),(#70762,#70763),(#70764,#70765),(#70766,#70767),(#70768,
#70769),(#70770,#70771),(#70772,#70773),(#70774,#70775),(#70776,#70777),
(#70778,#70779),(#70780,#70781),(#70782,#70783),(#70784,#70785),(#70786,
#70787),(#70788,#70789),(#70790,#70791),(#70792,#70793),(#70794,#70795),
(#70796,#70797),(#70798,#70799),(#70800,#70801),(#70802,#70803),(#70804,
#70805),(#70806,#70807),(#70808,#70809),(#70810,#70811),(#70812,#70813),
(#70814,#70815),(#70816,#70817),(#70818,#70819),(#70820,#70821),(#70822,
#70823),(#70824,#70825),(#70826,#70827),(#70828,#70829),(#70830,#70831),
(#70832,#70833),(#70834,#70835),(#70836,#70837),(#70838,#70839),(#70840,
#70841),(#70842,#70843),(#70844,#70845),(#70846,#70847),(#70848,#70849),
(#70850,#70851),(#70852,#70853),(#70854,#70855),(#70856,#70857),(#70858,
#70859),(#70860,#70861),(#70862,#70863),(#70864,#70865),(#70866,#70867),
(#70868,#70869),(#70870,#70871),(#70872,#70873),(#70874,#70875),(#70876,
#70877),(#70878,#70879),(#70880,#70881),(#70882,#70883),(#70884,#70885),
(#70886,#70887),(#70888,#70889),(#70890,#70891),(#70892,#70893),(#70894,
#70895),(#70896,#70897),(#70898,#70899),(#70900,#70901),(#70902,#70903),
(#70904,#70905),(#70906,#70907),(#70908,#70909),(#70910,#70911),(#70912,
#70913),(#70914,#70915),(#70916,#70917),(#70918,#70919),(#70920,#70921),
(#70922,#70923),(#70924,#70925),(#70926,#70927),(#70928,#70929),(#70930,
#70931),(#70932,#70933),(#70934,#70935),(#70936,#70937),(#70938,#70939),
(#70940,#70941),(#70942,#70943),(#70944,#70945),(#70946,#70947),(#70948,
#70949),(#70950,#70951),(#70952,#70953),(#70954,#70955),(#70956,#70957),
(#70958,#70959),(#70960,#70961),(#70962,#70963),(#70964,#70965),(#70966,
#70967),(#70968,#70969),(#70970,#70971),(#70972,#70973),(#70974,#70975),
(#70976,#70977),(#70978,#70979),(#70980,#70981),(#70982,#70983),(#70984,
#70985),(#70986,#70987),(#70988,#70989),(#70990,#70991),(#70992,#70993),
(#70994,#70995),(#70996,#70997),(#70998,#70999),(#71000,#71001),(#71002,
#71003),(#71004,#71005),(#71006,#71007),(#71008,#71009),(#71010,#71011),
(#71012,#71013),(#71014,#71015),(#71016,#71017),(#71018,#71019),(#71020,
#71021),(#71022,#71023),(#71024,#71025),(#71026,#71027),(#71028,#71029),
(#71030,#71031),(#71032,#71033),(#71034,#71035),(#71036,#71037),(#71038,
#71039),(#71040,#71041),(#71042,#71043),(#71044,#71045),(#71046,#71047),
(#71048,#71049),(#71050,#71051),(#71052,#71053),(#71054,#71055),(#71056,
#71057),(#71058,#71059),(#71060,#71061),(#71062,#71063),(#71064,#71065),
(#71066,#71067),(#71068,#71069),(#71070,#71071),(#71072,#71073),(#71074,
#71075),(#71076,#71077),(#71078,#71079),(#71080,#71081),(#71082,#71083),
(#71084,#71085),(#71086,#71087),(#71088,#71089),(#71090,#71091),(#71092,
#71093),(#71094,#71095),(#71096,#71097),(#71098,#71099),(#71100,#71101),
(#71102,#71103),(#71104,#71105),(#71106,#71107),(#71108,#71109),(#71110,
#71111),(#71112,#71113),(#71114,#71115),(#71116,#71117),(#71118,#71119),
(#71120,#71121),(#71122,#71123),(#71124,#71125),(#71126,#71127),(#71128,
#71129),(#71130,#71131),(#71132,#71133),(#71134,#71135),(#71136,#71137),
(#71138,#71139),(#71140,#71141),(#71142,#71143),(#71144,#71145),(#71146,
#71147),(#71148,#71149),(#71150,#71151),(#71152,#71153),(#71154,#71155),
(#71156,#71157),(#71158,#71159),(#71160,#71161),(#71162,#71163),(#71164,
#71165),(#71166,#71167),(#71168,#71169),(#71170,#71171),(#71172,#71173),
(#71174,#71175),(#71176,#71177),(#71178,#71179),(#71180,#71181),(#71182,
#71183),(#71184,#71185),(#71186,#71187),(#71188,#71189),(#71190,#71191),
(#71192,#71193),(#71194,#71195),(#71196,#71197),(#71198,#71199),(#71200,
#71201),(#71202,#71203),(#71204,#71205),(#71206,#71207),(#71208,#71209),
(#71210,#71211),(#71212,#71213),(#71214,#71215),(#71216,#71217),(#71218,
#71219),(#71220,#71221),(#71222,#71223),(#71224,#71225),(#71226,#71227),
(#71228,#71229),(#71230,#71231),(#71232,#71233),(#71234,#71235),(#71236,
#71237),(#71238,#71239),(#71240,#71241),(#71242,#71243),(#71244,#71245),
(#71246,#71247),(#71248,#71249),(#71250,#71251),(#71252,#71253),(#71254,
#71255),(#71256,#71257),(#71258,#71259),(#71260,#71261),(#71262,#71263),
(#71264,#71265),(#71266,#71267),(#71268,#71269),(#71270,#71271),(#71272,
#71273),(#71274,#71275),(#71276,#71277),(#71278,#71279),(#71280,#71281),
(#71282,#71283),(#71284,#71285),(#71286,#71287),(#71288,#71289),(#71290,
#71291),(#71292,#71293),(#71294,#71295),(#71296,#71297),(#71298,#71299),
(#71300,#71301),(#71302,#71303),(#71304,#71305),(#71306,#71307),(#71308,
#71309),(#71310,#71311),(#71312,#71313),(#71314,#71315),(#71316,#71317),
(#71318,#71319),(#71320,#71321),(#71322,#71323),(#71324,#71325),(#71326,
#71327),(#71328,#71329),(#71330,#71331),(#71332,#71333),(#71334,#71335),
(#71336,#71337),(#71338,#71339),(#71340,#71341),(#71342,#71343),(#71344,
#71345),(#71346,#71347),(#71348,#71349),(#71350,#71351),(#71352,#71353),
(#71354,#71355),(#71356,#71357),(#71358,#71359),(#71360,#71361),(#71362,
#71363),(#71364,#71365),(#71366,#71367),(#71368,#71369),(#71370,#71371),
(#71372,#71373),(#71374,#71375),(#71376,#71377),(#71378,#71379),(#71380,
#71381),(#71382,#71383),(#71384,#71385),(#71386,#71387),(#71388,#71389),
(#71390,#71391),(#71392,#71393),(#71394,#71395),(#71396,#71397),(#71398,
#71399),(#71400,#71401),(#71402,#71403),(#71404,#71405),(#71406,#71407),
(#71408,#71409),(#71410,#71411),(#71412,#71413),(#71414,#71415),(#71416,
#71417),(#71418,#71419),(#71420,#71421),(#71422,#71423),(#71424,#71425),
(#71426,#71427),(#71428,#71429),(#71430,#71431),(#71432,#71433),(#71434,
#71435),(#71436,#71437),(#71438,#71439),(#71440,#71441),(#71442,#71443),
(#71444,#71445),(#71446,#71447),(#71448,#71449),(#71450,#71451),(#71452,
#71453),(#71454,#71455),(#71456,#71457),(#71458,#71459),(#71460,#71461),
(#71462,#71463),(#71464,#71465),(#71466,#71467),(#71468,#71469),(#71470,
#71471),(#71472,#71473),(#71474,#71475),(#71476,#71477),(#71478,#71479),
(#71480,#71481),(#71482,#71483),(#71484,#71485),(#71486,#71487),(#71488,
#71489),(#71490,#71491),(#71492,#71493),(#71494,#71495),(#71496,#71497),
(#71498,#71499),(#71500,#71501),(#71502,#71503),(#71504,#71505),(#71506,
#71507),(#71508,#71509),(#71510,#71511),(#71512,#71513),(#71514,#71515),
(#71516,#71517),(#71518,#71519),(#71520,#71521),(#71522,#71523),(#71524,
#71525),(#71526,#71527),(#71528,#71529),(#71530,#71531),(#71532,#71533)),
 .UNSPECIFIED.,.F.,.F.,.F.,(4,1,1,1,1,1,1,1,1,1,1,1,1,1,1,1,1,1,1,1,1,1,
1,1,1,1,1,1,1,1,1,1,1,1,1,1,1,1,1,1,1,1,1,1,1,1,1,1,1,1,1,1,1,1,1,1,1,1,
1,1,1,1,1,1,1,1,1,1,1,1,1,1,1,1,1,1,1,1,1,1,1,1,1,1,1,1,1,1,1,1,1,1,1,1,
1,1,1,1,1,1,1,1,1,1,1,1,1,1,1,1,1,1,1,1,1,1,1,1,1,1,1,1,1,1,1,1,1,1,1,1,
1,1,1,1,1,1,1,1,1,1,1,1,1,1,1,1,1,1,1,1,1,1,1,1,1,1,1,1,1,1,1,1,1,1,1,1,
1,1,1,1,1,1,1,1,1,1,1,1,1,1,1,1,1,1,1,1,1,1,1,1,1,1,1,1,1,1,1,1,1,1,1,1,
1,1,1,1,1,1,1,1,1,1,1,1,1,1,1,1,1,1,1,1,1,1,1,1,1,1,1,1,1,1,1,1,1,1,1,1,
1,1,1,1,1,1,1,1,1,1,1,1,1,1,1,1,1,1,1,1,1,1,1,1,1,1,1,1,1,1,1,1,1,1,1,1,
1,1,1,1,1,1,1,1,1,1,1,1,1,1,1,1,1,1,1,1,1,1,1,1,1,1,1,1,1,1,1,1,1,1,1,1,
1,1,1,1,1,1,1,1,1,1,1,1,1,1,1,1,1,1,1,1,1,1,1,1,1,1,1,1,1,1,1,1,1,1,1,1,
1,1,1,1,1,1,1,1,1,1,1,1,1,1,1,1,1,1,1,1,1,1,1,1,1,1,1,1,1,1,1,1,1,1,1,1,
1,1,1,1,1,1,1,1,1,1,1,1,1,1,1,1,1,1,1,1,1,1,1,1,1,1,1,1,1,1,1,1,1,1,1,1,
1,1,1,1,1,1,1,1,1,1,1,1,1,1,1,1,1,1,1,1,1,1,1,1,1,1,1,1,1,1,1,1,1,1,1,1,
1,1,1,1,1,1,1,1,1,1,1,1,1,1,1,1,1,1,1,1,1,1,1,1,1,1,1,1,1,1,1,1,1,1,1,1,
1,1,1,1,1,1,1,1,1,1,1,1,1,1,1,1,1,1,1,1,1,1,1,1,1,1,1,1,1,1,1,1,1,1,1,1,
1,1,1,1,1,1,1,1,1,1,1,1,1,1,1,1,1,1,1,1,1,1,1,1,1,1,1,1,1,1,1,1,1,1,1,1,
1,1,1,1,1,1,1,1,1,1,1,1,1,1,1,1,1,1,1,1,1,1,1,1,1,1,1,1,1,1,1,1,1,1,1,1,
1,1,1,1,1,1,1,1,1,1,1,1,1,1,1,1,1,1,1,1,1,1,1,1,1,1,1,1,1,1,1,1,1,1,1,1,
1,1,1,1,1,1,1,1,1,1,1,1,1,1,1,1,1,1,1,1,1,1,1,1,1,1,1,1,1,1,1,1,1,1,1,1,
1,1,1,1,1,1,1,1,1,1,1,1,1,1,1,1,1,1,1,1,1,1,1,1,1,1,1,1,1,1,1,1,1,1,1,1,
1,1,1,1,1,1,1,1,1,1,1,1,1,1,1,1,1,1,1,1,1,1,1,1,1,1,1,1,1,1,1,1,1,1,1,1,
1,1,1,1,1,1,1,1,1,1,1,1,1,1,1,1,1,1,1,1,1,1,1,1,1,1,1,1,1,1,1,1,1,1,1,1,
1,1,1,1,1,1,1,1,1,1,1,1,1,1,1,1,1,1,1,1,1,1,1,1,1,1,1,1,1,1,1,1,1,1,1,1,
1,1,1,1,1,1,1,1,1,1,1,1,1,1,1,1,1,1,1,1,1,1,1,1,1,1,1,1,1,1,1,1,1,1,1,1,
1,1,1,1,1,1,1,1,1,1,1,1,1,1,1,1,1,1,1,1,1,1,1,1,1,1,1,1,1,1,1,1,1,1,1,1,
1,1,1,1,1,1,1,1,1,1,1,1,1,1,1,1,1,1,1,1,1,1,1,1,1,1,1,1,1,1,1,1,1,1,1,1,
1,1,1,1,1,1,1,1,1,1,1,1,1,1,1,1,1,1,1,1,1,1,1,1,1,1,1,1,1,1,1,1,1,1,1,1,
1,1,1,1,1,1,1,1,1,1,1,1,1,1,1,1,1,1,1,1,1,1,1,1,1,1,1,1,1,1,1,1,1,1,1,1,
1,1,1,1,1,1,1,1,1,1,1,1,1,1,1,1,1,1,1,1,1,1,1,1,1,1,1,1,1,1,1,1,1,1,1,1,
1,1,1,1,1,1,1,1,1,1,1,1,1,1,1,1,1,1,1,1,1,1,1,1,1,1,1,1,1,1,1,1,1,1,1,1,
1,1,1,1,1,1,1,1,1,1,1,1,1,1,1,1,1,1,1,1,1,1,1,1,1,1,1,1,1,1,1,1,1,1,1,1,
1,1,1,1,1,1,1,1,1,1,1,1,1,1,1,1,1,1,1,1,1,1,1,1,1,1,1,1,1,1,1,1,1,1,1,1,
1,1,1,1,1,1,1,1,1,1,1,1,1,1,1,1,1,1,1,1,1,1,1,1,1,1,1,1,1,1,1,1,1,1,1,1,
1,1,1,1,1,1,1,1,1,1,1,1,1,1,1,1,1,1,1,1,1,1,1,1,1,1,1,1,1,1,1,1,1,1,1,1,
1,1,1,1,1,1,1,1,1,1,1,1,1,1,1,1,1,1,1,1,1,1,1,1,1,1,1,1,1,1,1,1,1,1,1,1,
1,1,1,1,1,1,1,1,1,1,1,1,1,1,1,1,1,1,1,1,1,1,1,1,1,1,1,1,1,1,1,1,1,1,1,1,
1,1,1,1,1,1,1,1,1,1,1,1,1,1,1,1,1,1,1,1,1,1,1,1,1,1,1,1,1,1,1,1,1,1,1,1,
1,1,1,1,1,1,1,1,1,1,1,1,1,1,1,1,1,1,1,1,1,1,1,1,1,1,1,1,1,1,1,1,1,1,1,1,
1,1,1,1,1,1,1,1,1,1,1,1,1,1,1,1,1,1,1,1,1,1,1,1,1,1,1,1,1,1,1,1,1,1,1,1,
1,1,1,1,1,1,1,1,1,1,1,1,1,1,1,1,1,1,1,1,1,1,1,1,1,1,1,1,1,1,1,1,1,1,1,1,
1,1,1,1,1,1,1,1,1,1,1,1,1,1,1,1,1,1,1,1,1,1,1,1,1,1,1,1,1,1,1,1,1,1,1,1,
1,1,1,1,1,1,1,1,1,1,1,1,1,1,1,1,1,1,1,1,1,1,1,1,1,1,1,1,1,1,1,1,1,1,1,1,
1,1,1,1,1,1,1,1,1,1,1,1,1,1,1,1,1,1,1,1,1,1,1,1,1,1,1,1,1,1,1,1,1,1,1,1,
1,1,1,1,1,1,1,1,1,1,1,1,1,1,1,1,1,1,1,1,1,1,1,1,1,1,1,1,1,1,1,1,1,1,1,1,
1,1,1,1,1,1,1,1,1,1,1,1,1,1,1,1,1,1,1,1,1,1,1,1,1,1,1,1,1,1,1,1,1,1,1,1,
1,1,1,1,1,1,1,1,1,1,1,1,1,1,1,1,1,1,1,1,1,1,1,1,1,1,1,1,1,1,1,1,1,1,1,1,
1,1,1,1,1,1,1,1,1,1,1,1,1,1,1,1,1,1,1,1,1,1,1,1,1,1,1,1,1,1,1,1,1,1,1,1,
1,1,1,1,1,1,1,1,1,1,1,1,1,1,1,1,1,1,1,1,1,1,1,1,1,1,1,1,1,1,1,1,1,1,1,1,
1,1,1,1,1,1,1,1,1,1,1,1,1,1,1,1,1,1,1,1,1,1,1,1,1,1,1,1,1,1,1,1,1,1,1,1,
1,1,1,1,1,1,1,1,1,1,1,1,1,1,1,1,1,1,1,1,1,1,1,1,1,1,1,1,1,1,1,1,1,1,1,1,
1,1,1,1,1,1,1,1,1,1,1,1,1,1,1,1,1,1,1,1,1,1,1,1,1,1,1,1,1,1,1,1,1,1,1,1,
1,1,1,1,1,1,1,1,1,1,1,1,1,1,1,1,1,1,1,1,1,1,1,1,1,1,1,1,1,1,1,1,1,1,1,1,
1,1,1,1,1,1,1,1,1,1,1,1,1,1,1,1,1,1,1,1,1,1,1,1,1,1,1,1,1,1,1,1,1,1,1,1,
1,1,1,1,1,1,1,1,1,1,1,1,1,1,1,1,1,1,1,1,1,1,1,1,1,1,1,1,1,1,1,1,1,1,1,1,
1,1,1,1,1,1,1,1,1,1,1,1,1,1,1,1,1,1,1,1,1,1,1,1,1,1,1,1,1,1,1,1,1,1,1,1,
1,1,1,1,1,1,1,1,1,1,1,1,1,1,1,1,1,1,1,1,1,1,1,1,1,1,1,1,1,1,1,1,1,1,1,1,
1,1,1,1,1,1,1,1,1,1,1,1,1,1,1,1,1,1,1,1,1,1,1,1,1,1,1,1,1,1,1,1,1,1,1,1,
1,1,1,1,1,1,1,1,1,1,1,1,1,1,1,1,1,1,1,1,1,1,1,1,1,1,1,1,1,1,1,1,1,1,1,1,
1,1,1,1,1,1,1,1,1,1,1,1,1,1,1,1,1,1,1,1,1,1,1,1,1,1,1,1,1,1,1,1,1,1,1,1,
1,1,1,1,1,1,1,1,1,1,1,1,1,1,1,1,1,1,1,1,1,1,1,1,1,1,1,1,1,1,1,1,1,1,1,1,
1,1,1,1,1,1,1,1,1,1,1,1,1,1,1,1,1,1,1,1,1,1,1,1,1,1,1,1,1,1,1,1,1,1,1,1,
1,1,1,1,1,1,1,1,1,1,1,1,1,1,1,1,1,1,1,1,1,1,1,1,1,1,1,1,1,1,1,1,1,1,1,1,
1,1,1,1,1,1,1,1,1,1,1,1,1,1,1,1,1,1,1,1,1,1,1,1,1,1,1,1,1,1,1,1,1,1,1,1,
1,1,1,1,1,1,1,1,1,1,1,1,1,1,1,1,1,1,1,1,1,1,1,1,1,1,1,1,1,1,1,1,1,1,1,1,
1,1,1,1,1,1,1,1,1,1,1,1,1,1,1,1,1,1,1,1,1,1,1,1,1,1,1,1,1,1,1,1,1,1,1,1,
1,1,1,1,1,1,1,1,1,1,1,1,1,1,1,1,1,1,1,1,1,1,1,1,1,1,1,1,1,1,1,1,1,1,1,1,
1,1,1,1,1,1,1,1,1,1,1,1,1,1,1,1,1,1,1,1,1,1,1,1,1,1,1,1,1,1,1,1,1,1,1,1,
1,1,1,1,1,1,1,1,1,1,1,1,1,1,1,1,1,1,1,1,1,1,1,1,1,1,1,1,1,1,1,1,1,1,1,1,
1,1,1,1,1,1,1,1,1,1,1,1,1,1,1,1,1,1,1,1,1,1,1,1,1,1,1,1,1,1,1,1,1,1,1,1,
1,1,1,1,1,1,1,1,1,1,1,1,1,1,1,1,1,1,1,1,1,1,1,1,1,1,1,1,1,1,1,1,1,1,1,1,
1,1,1,1,1,1,1,1,1,1,1,1,1,1,1,1,1,1,1,1,1,1,1,1,1,1,1,1,1,1,1,1,1,1,1,1,
1,1,1,1,1,1,1,1,1,1,1,1,1,1,1,1,1,1,1,1,1,1,1,1,1,1,1,1,1,1,1,1,1,1,1,1,
1,1,1,1,1,1,1,1,1,1,1,1,1,1,1,1,1,1,1,1,1,1,1,1,1,1,1,1,1,1,1,1,1,1,1,1,
1,1,1,1,1,1,1,1,1,1,1,1,1,1,1,1,1,1,1,1,1,1,1,1,1,1,1,1,1,1,1,1,1,1,1,1,
1,1,1,1,1,1,1,1,1,1,1,1,1,1,1,1,1,1,1,1,1,1,1,1,1,1,1,1,1,1,1,1,1,1,1,1,
1,1,1,1,1,1,1,1,1,1,1,1,1,1,1,1,1,1,1,1,1,1,1,1,1,1,1,1,1,1,1,1,1,1,1,1,
1,1,1,1,1,1,1,1,1,1,1,1,1,1,1,1,1,1,1,1,1,1,1,1,1,1,1,1,1,1,1,1,1,1,1,1,
1,1,1,1,1,1,1,1,1,1,1,1,1,1,1,1,1,1,1,1,1,1,1,1,1,1,1,1,1,1,1,1,1,1,1,1,
1,1,1,1,1,1,1,1,1,1,1,1,1,1,1,1,1,1,1,1,1,1,1,1,1,1,1,1,1,1,1,1,1,1,1,1,
1,1,1,1,1,1,1,1,1,1,1,1,1,1,1,1,1,1,1,1,1,1,1,1,1,1,1,1,1,1,1,1,1,1,1,1,
1,1,1,1,1,1,1,1,1,1,1,1,1,1,1,1,1,1,1,1,1,1,1,1,1,1,1,1,1,1,1,1,1,1,1,1,
1,1,1,1,1,1,1,1,1,1,1,1,1,1,1,1,1,1,1,1,1,1,1,1,1,1,1,1,1,1,1,1,1,1,1,1,
1,1,1,1,1,1,1,1,1,1,1,1,1,1,1,1,1,1,1,1,1,1,1,1,1,1,1,1,1,1,1,1,1,1,1,1,
1,1,1,1,1,1,1,1,1,1,1,1,1,1,1,1,1,1,1,1,1,1,1,1,1,1,1,1,1,1,1,1,1,1,1,1,
1,1,1,1,1,1,1,1,1,1,1,1,1,1,1,1,1,1,1,1,1,1,1,1,1,1,1,1,1,1,1,1,1,1,1,1,
1,1,1,1,1,1,1,1,1,1,1,1,1,1,1,1,1,1,1,1,1,1,1,1,1,1,1,1,1,1,1,1,1,1,1,1,
1,1,1,1,1,1,1,1,1,1,1,1,1,1,1,1,1,1,1,1,1,1,1,1,1,1,1,1,1,1,1,1,1,1,1,1,
1,1,1,1,1,1,1,1,1,1,1,1,1,1,1,1,1,1,1,1,1,1,1,1,1,1,1,1,1,1,1,1,1,1,1,1,
1,1,1,1,1,1,1,1,1,1,1,1,1,1,1,1,1,1,1,1,1,1,1,1,1,1,1,1,1,1,1,1,1,1,1,1,
1,1,1,1,1,1,1,1,1,1,1,1,1,1,1,1,1,1,1,1,1,1,1,1,1,1,1,1,1,1,1,1,1,1,1,1,
1,1,1,1,1,1,1,1,1,1,1,1,1,1,1,1,1,1,1,1,1,1,1,1,1,1,1,1,1,1,1,1,1,1,1,1,
1,1,1,1,1,1,1,1,1,1,1,1,1,1,1,1,1,1,1,1,1,1,1,1,1,1,1,1,1,1,1,1,1,1,1,1,
1,1,1,1,1,1,1,1,1,1,1,1,1,1,1,1,1,1,1,1,1,1,1,1,1,1,1,1,1,1,1,1,1,1,1,1,
1,1,1,1,1,1,1,1,1,1,1,1,1,1,1,1,1,1,1,1,1,1,1,1,1,1,1,1,1,1,1,1,1,1,1,1,
1,1,1,1,1,1,1,1,1,1,1,1,1,1,1,1,1,1,1,1,1,1,1,1,1,1,1,1,1,1,1,1,1,1,1,1,
1,1,1,1,1,1,1,1,1,1,1,1,1,1,1,1,1,1,1,1,1,1,1,1,1,1,1,1,1,1,1,1,1,1,1,1,
1,1,1,1,1,1,1,1,1,1,1,1,1,1,1,1,1,1,1,1,1,1,1,1,1,1,1,1,1,1,1,1,1,1,1,1,
1,1,1,1,4),(2,2),(0.,0.869746702321014,1.7394931589914,2.60923976624962,
3.47983908319159,4.35043840179749,5.22018503077054,6.08993165951504,6.95967828799171,
7.82942491616733,8.69917154401062,9.56891817149224,10.4395174886835,11.3101168056706,
12.179863432132,13.049610058144,13.9193566836854,14.7891033087372,15.6588499332817,
16.5285965573034,17.3991958717975,18.2697951860185,18.7046684974166,19.1395418086746,
19.5744151197912,20.0092884307654,20.4441617415962,20.8790350522825,21.7487816732187,
22.1836549834672,22.6185282935685,23.0534016035221,23.4882749133276,23.9231482229848,
24.3588742245859,24.794600226187,25.2294735355468,26.0992201538203,26.5340934627341,
26.9689667714994,27.4038400801166,27.838713388586,28.2735866969081,28.7084600050832,
29.143333313112,29.5782066209952,30.0130799287334,30.4479532363275,30.8828265437783,
31.3185525442794,31.7542785447804,32.1891518519474,32.6240251589741,33.0588984658616,
33.4937717726112,33.928645079224,34.3635183857014,34.7983916920448,35.2332649982556,
35.6681383043353,36.1030116102854,36.5378849161076,36.9727582218035,37.4076315273749,
37.8425048328235,38.2782308323341,38.7139568318446,39.1488301370532,39.5837034421446,
40.0185767471208,40.4534500519838,40.8883233567357,41.3231966613787,41.7580699659148,
42.1929432703463,42.6278165746754,43.0626898789044,43.4975631830356,43.9324364870714,
44.3673097910142,44.8021830948664,45.2379090935952,45.673635092324,46.1085083960024,
46.5433816995978,46.9782550031127,47.4131283065497,47.8480016099115,48.2828749132006,
48.7177482164198,49.1526215195718,49.5874948226593,50.0223681256851,50.457241428652,
50.8921147315628,51.3269880344203,51.7618613372274,52.197587335454,52.6333133336805,
53.0681866363954,53.5030599390685,53.9379332417027,54.3728065443011,54.8076798468664,
55.2425531494018,55.6774264519101,56.1122997543943,56.5471730568575,56.9820463593026,
57.4169196617326,57.8517929641506,58.2866662665595,58.7215395689624,59.157265567009,
59.5929915650557,60.0278648674556,60.4627381698584,60.8976114722673,61.3324847746853,
61.7673580771153,62.2022313795604,62.6371046820236,63.0719779845079,63.5068512870162,
63.9417245895516,64.376597892117,64.8114711947155,65.2463444973499,65.6812178000231,
66.1169437982275,66.5526697964318,66.9875430991915,67.4224164019987,67.8572897048563,
68.2921630077673,68.7270363107343,69.1619096137603,69.5967829168479,70.0316562200001,
70.4665295232194,70.9014028265087,71.3362761298705,71.7711494333077,72.2060227368227,
72.6408960404182,73.0766220391044,73.5123480377905,73.9472213415547,74.382094645407,
74.8169679493499,75.2518412533859,75.6867145575172,76.1215878617464,76.5564611660756,
76.9913344705072,77.4262077750435,77.8610810796866,78.2959543844386,78.7308276893018,
79.1657009942781,79.6005742993696,80.0363002988208,80.4720262982719,80.9068996035997,
81.3417729090484,81.7766462146199,82.211519520316,82.6463928261383,83.0812661320886,
83.5161394381684,83.9510127443794,84.3858860507229,84.8207593572004,85.2556326638134,
85.6905059705631,86.1253792774507,86.5602525844776,86.995978584908,87.4317045853384,
87.8665778926469,88.3014512000977,88.7363245076919,89.1711978154302,89.6060711233134,
90.0409444313423,90.4758177395175,90.9106910478396,91.345564356309,91.7804376649263,
92.2153109736917,92.6501842826055,93.085057591668,93.5199309008791,93.9556569024059,
94.3913829039327,94.8262562134414,95.2611295230986,95.6960028329042,96.1308761428578,
96.5657494529591,97.0006227632077,97.4354960736028,97.870369384144,98.3052426948304,
98.7401160056612,99.1749893166354,99.6098626277522,100.04473593901,100.915335253024,
101.351061255639,101.785934567313,102.220807879124,102.655681191068,103.090554503145,
103.525427815353,104.395174440154,105.264921065453,105.699794378283,106.134667691232,
106.569541004295,107.004414317471,107.8750136343,108.745612951339,109.615359578629,
110.485106206296,111.354852834309,112.224599462639,113.094346091254,113.964092720119,
114.834692038763,115.705291357499,116.575037986826,117.444784616267,118.314531245777,
119.184277875311,120.054024504821,120.923771134261,121.794370453112,122.66496977189,
123.534716400968,124.404463029834,125.274209658448,126.143956286779,127.013702914792,
127.883449542458,128.754048859798,129.624648176939,130.494394803617,131.364141429857,
132.233888055637,133.103634680937,133.973381305737,134.843127930023,135.71372724472,
136.584326559147,137.019199870684,137.454073182083,137.888946493341,138.323819804458,
139.193566426263,140.063313047491,140.498186357887,140.933059668136,141.367932978237,
141.802806288191,142.237679597997,142.673405599673,143.109131601348,143.544004910857,
143.978878220217,144.413751529429,144.848624838491,145.283498147405,145.718371456171,
146.153244764789,146.588118073258,147.022991381581,147.457864689756,147.892737997785,
148.327611305669,148.762484613407,149.197357921002,149.633083921574,150.068809922147,
150.503683229455,150.938556536623,151.37342984365,151.808303150538,152.243176457288,
152.678049763901,153.112923070379,153.547796376722,153.982669682934,154.417542989014,
154.852416294964,155.287289600787,155.722162906483,156.157036212055,156.592762211626,
157.028488211198,157.463361516526,157.898234821735,158.333108126826,158.767981431803,
159.202854736666,159.637728041419,160.072601346062,160.507474650599,160.94234795503,
161.37722125936,161.812094563589,162.246967867721,162.681841171757,163.1167144757,
163.552440474473,163.988166473247,164.423039777011,164.85791308069,165.292786384286,
165.727659687801,166.162532991238,166.597406294601,167.03227959789,167.46715290111,
167.902026204262,168.33689950735,168.771772810376,169.206646113343,169.641519416254,
170.076392719112,170.512118717363,170.947844715614,171.382718018374,171.817591321089,
172.252464623762,172.687337926397,173.122211228996,173.557084531561,173.991957834097,
174.426831136606,174.86170443909,175.296577741554,175.731451044,176.16632434643,
176.601197648848,177.036070951258,177.471796949306,177.907522947355,178.342396249755,
178.777269552155,179.212142854558,179.647016156968,180.081889459386,180.516762761816,
180.951636064262,181.386509366726,181.82138266921,182.256255971719,182.691129274255,
183.12600257682,183.560875879419,183.995749182054,184.431475180237,184.867201178421,
185.302074481136,185.736947783896,186.171821086704,186.606694389561,187.041567692473,
187.47644099544,187.911314298466,188.346187601554,188.781060904706,189.215934207926,
189.650807511215,190.085680814577,190.520554118015,190.95542742153,191.391153420175,
191.82687941882,192.261752722499,192.696626026263,193.131499330116,193.566372634059,
194.001245938095,194.436119242227,194.870992546456,195.305865850785,195.740739155217,
196.175612459754,196.610485764397,197.045359069149,197.480232374013,197.915105678989,
198.350831678382,198.786557677775,199.221430982984,199.656304288312,200.091177593761,
200.526050899333,200.960924205029,201.395797510852,201.830670816802,202.265544122882,
202.700417429093,203.135290735437,203.570164041915,204.005037348528,204.439910655278,
204.874783962166,205.310509962526,205.746235962887,206.181109270054,206.615982577363,
207.050855884814,207.485729192409,207.920602500147,208.355475808031,208.79034911606,
209.225222424235,209.660095732558,210.094969041027,210.529842349645,210.96471565841,
211.399588967324,211.834462276387,212.27018827784,212.705914279292,213.140787588653,
213.575660898161,214.010534207819,214.880280827579,215.31515413768,215.750027447929,
216.184900758324,216.619774068866,217.054647379553,217.489520690384,218.359267312475,
219.22986662628,219.665592628826,220.100465940363,220.535339252038,220.970212563848,
221.83995918787,222.709705812416,223.579452437468,224.014325750179,224.44919906301,
225.318945689022,226.189545005688,227.060144322571,227.929890949664,228.799637577146,
229.66938420499,230.539130833166,231.408877461643,232.278624090388,233.149223408954,
234.019822727623,234.889569356878,235.759315986267,236.629062615749,237.498809245277,
238.368555874806,239.238302504287,240.108901823183,240.979501142017,241.849247771189,
242.718994400167,243.588741028911,244.458487657389,245.328234285565,246.197980913409,
247.068580230891,247.939179548182,248.80892617507,249.678672801532,250.548419427545,
251.418166053087,252.287912678139,253.157659302684,254.028258617581,254.898857932211,
255.333731243885,255.768604555423,256.203477866821,256.63835117808,257.508097800171,
258.377844421689,258.812717732231,259.247591042627,259.682464352876,260.117337662977,
260.552210972931,260.987936974682,261.858536286089,262.293409595598,262.728282904958,
263.16315621417,263.598029523233,264.032902832147,264.467776140913,264.902649449531,
265.337522758001,265.772396066323,266.207269374499,266.642142682528,267.077015990412,
267.511889298151,267.947615298795,268.383341299439,268.81821460689,269.2530879142,
269.687961221367,270.122834528394,270.557707835282,270.992581142032,271.427454448646,
271.862327755124,272.297201061468,272.732074367679,273.166947673759,273.60182097971,
274.036694285533,274.471567591229,274.907293590862,275.343019590495,275.777892895944,
276.212766201272,276.647639506481,277.082512811573,277.51738611655,277.952259421414,
278.387132726166,278.82200603081,279.256879335346,279.691752639779,280.126625944108,
280.561499248338,280.996372552469,281.431245856506,281.866971855324,282.302697854143,
282.737571157996,283.172444461761,283.60731776544,284.042191069036,284.477064372551,
284.911937675989,285.346810979351,285.781684282641,286.216557585861,286.651430889013,
287.086304192101,287.521177495128,287.956050798095,288.390924101007,288.826650099283,
289.262376097559,289.697249400366,290.132122703127,290.566996005842,291.001869308516,
291.43674261115,291.871615913749,292.306489216315,292.741362518851,293.17623582136,
293.611109123845,294.045982426308,294.480855728754,294.915729031185,295.350602333603,
295.786328331655,296.222054329707,296.65692763211,297.091800934511,297.526674236911,
297.961547539314,298.396420841724,298.831294144142,299.266167446573,299.701040749018,
300.135914051482,300.570787353967,301.005660656476,301.440533959012,301.875407261578,
302.310280564177,302.746006562341,303.181732560506,303.616605863179,304.051479165895,
304.486352468655,304.921225771462,305.35609907432,305.790972377232,306.225845680199,
306.660718983226,307.095592286314,307.530465589466,307.965338892686,308.400212195976,
308.835085499338,309.269958802776,309.705684801381,310.141410799985,310.576284103581,
311.01115740726,311.446030711025,311.880904014878,312.315777318821,312.750650622858,
313.185523926989,313.620397231219,314.055270535549,314.490143839981,314.925017144517,
315.359890449161,315.794763753913,316.229637058777,316.665363058112,317.101089057448,
317.53596236254,317.970835667749,318.405708973077,318.840582278526,319.275455584098,
319.710328889795,320.145202195618,320.580075501568,321.014948807648,321.44982211386,
321.884695420204,322.319568726682,322.754442033295,323.189315340045,323.625041340336,
324.060767340628,324.495640647655,324.930513954822,325.365387262131,325.800260569583,
326.235133877177,326.670007184916,327.1048804928,327.539753800829,327.974627109005,
328.409500417327,328.844373725797,329.279247034415,329.714120343181,330.148993652095,
330.584719653474,331.020445654852,331.455318964064,331.890192273424,332.325065582933,
332.759938892591,333.194812202397,333.629685512351,334.064558822453,334.499432132702,
334.934305443098,335.369178753639,335.804052064326,336.673798686132,337.108671997249,
337.544397999725,337.980124002201,338.4149973136,338.849870625137,339.284743936812,
340.154490560568,341.024237184854,341.459110497191,341.893983809655,342.328857122244,
342.763730434955,343.633477060735,344.504076377234,345.374675693955,346.244422320844,
347.114168948136,347.983915575803,348.853662203817,349.723408832148,350.593155460764,
351.463754779246,352.334354097839,353.204100727012,354.07384735634,354.943593985781,
355.813340615292,356.683087244827,357.552833874338,358.423433193272,359.294032512154,
360.163779141409,361.033525770489,361.903272399355,362.77301902797,363.642765656301,
364.512512284316,365.383111601936,366.253710919371,367.123457546465,367.993204173143,
368.862950799383,369.732697425164,370.602444050463,371.472190675265,372.342789990359,
373.21338930519,373.648262617,374.083135928675,374.952882551611,375.822629173987,
376.257502484962,376.692375795793,377.12724910648,377.562122417021,377.996995727417,
378.431869037666,378.866742347767,379.302468349591,379.738194351416,380.173067661222,
380.607940970879,381.042814280388,381.477687589749,381.91256089896,382.347434208023,
382.782307516937,383.217180825703,383.652054134321,384.086927442791,384.521800751113,
384.956674059289,385.391547367318,385.826420675202,386.262146675918,386.697872676635,
387.13274598423,387.567619291681,388.00249259899,388.437365906157,388.872239213185,
389.307112520073,389.741985826823,390.176859133436,390.611732439914,391.046605746258,
391.48147905247,391.91635235855,392.351225664501,392.786098970323,393.221824970019,
393.657550969714,394.092424275286,394.527297580735,394.962170886063,395.397044191272,
395.831917496364,396.266790801341,396.701664106204,397.136537410957,397.5714107156,
398.006284020137,398.441157324569,398.876030628899,399.310903933128,399.74577723726,
400.181503236126,400.617229234991,401.052102538934,401.486975842787,401.921849146551,
402.356722450231,402.791595753827,403.226469057342,403.66134236078,404.096215664142,
404.531088967432,404.965962270651,405.400835573804,405.835708876892,406.270582179918,
406.705455482886,407.141181481189,407.576907479491,408.01178078235,408.446654085157,
408.881527387917,409.316400690633,409.751273993306,410.186147295941,410.62102059854,
411.055893901106,411.490767203642,411.925640506151,412.360513808636,412.795387111099,
413.230260413545,413.665133715976,414.100859714032,414.536585712088,414.971459014498,
415.406332316901,415.841205619301,416.276078921702,416.710952224105,417.145825526515,
417.580698828933,418.015572131364,418.45044543381,418.885318736273,419.320192038758,
419.755065341267,420.189938643803,420.624811946369,421.060537944515,421.496263942662,
421.931137245297,422.36601054797,422.800883850686,423.235757153446,423.670630456253,
424.105503759112,424.540377062023,424.975250364991,425.410123668017,425.844996971105,
426.279870274258,426.714743577477,427.149616880767,427.584490184129,428.020216182695,
428.455942181261,428.890815484776,429.325688788373,429.760562092052,430.195435395816,
430.630308699669,431.065182003612,431.500055307649,431.93492861178,432.36980191601,
432.80467522034,433.239548524772,433.674421829309,434.109295133952,434.544168438705,
434.979894437984,435.415620437262,435.850493742239,436.285367047331,436.72024035254,
437.155113657869,437.589986963318,438.024860268889,438.459733574586,438.894606880409,
439.32948018636,439.76435349244,440.199226798651,440.634100104995,441.068973411473,
441.503846718087,441.939572718309,442.375298718531,442.810172025419,443.245045332447,
443.679918639614,444.114791946923,444.549665254374,444.984538561969,445.419411869708,
445.854285177591,446.289158485621,446.724031793796,447.158905102119,447.593778410589,
448.028651719207,448.463525027973,448.899251029277,449.334977030581,449.769850339644,
450.639596958216,451.074470267725,451.509343577383,451.944216887189,452.379090197143,
452.813963507244,453.248836817493,453.683710127889,454.118583438431,454.553456749117,
454.988330059949,455.423203370923,455.858929373329,456.294655375734,456.729528686993,
457.164401998391,457.599275309929,458.469021933414,458.90389524536,459.338768557437,
459.773641869646,460.208515181983,460.643388494447,461.078261807036,461.948008432578,
462.818607748906,463.689207065461,464.55895369214,465.428700319234,466.298446946716,
467.16819357456,468.037940202737,468.907686831215,469.778286149605,470.648885468116,
471.518632097196,472.388378726451,473.258125355841,474.127871985322,474.997618614851,
475.86736524438,476.737964563343,477.608563882265,478.478310511593,479.348057140765,
480.217803769743,481.087550398488,481.957297026966,482.827043655142,483.697642972895,
484.568242290469,485.43798891776,486.307735544649,487.177482171112,488.047228797125,
488.916975422667,489.78672204772,490.657321363009,491.09304736596,491.527920678038,
492.397667301793,493.267413925005,494.137160547663,494.57203385878,495.006907169755,
495.441780480586,495.876653791273,496.311527101814,496.74640041221,497.616999724357,
498.052725726255,498.487599036209,498.922472346015,499.357345655673,499.792218965182,
500.227092274542,500.661965583754,501.096838892816,501.531712201731,501.966585510497,
502.401458819114,502.836332127584,503.271205435907,503.706078744082,504.140952052112,
504.576678052901,505.01240405369,505.447277361429,505.882150669023,506.317023976474,
506.751897283783,507.186770590951,507.621643897978,508.056517204866,508.491390511616,
508.92626381823,509.361137124708,509.796010431052,510.230883737263,510.665757043344,
511.100630349294,511.536356349053,511.972082348811,512.406955654506,512.841828960076,
513.276702265523,513.711575570849,514.146448876056,514.581322181146,515.016195486121,
515.451068790983,515.885942095733,516.320815400375,516.75568870491,517.19056200934,
517.625435313668,518.060308617896,518.496034616807,518.931760615718,519.366633919752,
519.801507223694,520.236380527545,520.671253831307,521.106127134985,521.541000438579,
521.975873742092,522.410747045528,522.845620348888,523.280493652176,523.715366955394,
524.150240258545,524.585113561631,525.019986864656,525.455712862985,525.891438861313,
526.326312164223,526.761185467079,527.196058769885,527.630932072643,528.065805375356,
528.500678678029,528.935551980661,529.370425283258,529.805298585822,530.240171888356,
530.675045190863,531.109918493346,531.544791795808,531.979665098252,532.415391096312,
532.851117094373,533.285990396789,533.720863699197,534.155737001598,534.590610303997,
535.025483606395,535.460356908796,535.895230211204,536.330103513621,536.764976816049,
537.199850118493,537.634723420955,538.069596723438,538.504470025945,538.93934332848,
539.375069326608,539.810795324736,540.245668627333,540.680541929966,541.115415232637,
541.550288535351,541.985161838109,542.420035140915,542.854908443771,543.28978174668,
543.724655049646,544.15952835267,544.594401655757,545.029274958907,545.464148262125,
545.899021565413,546.334747563939,546.770473562465,547.205346865901,547.640220169415,
548.075093473009,548.509966776686,548.944840080449,549.3797133843,549.814586688241,
550.249459992276,550.684333296405,551.119206600633,551.554079904961,551.988953209391,
552.423826513926,552.858699818567,553.294425817789,553.73015181701,554.165025121872,
554.599898426846,555.034771731937,555.469645037144,555.90451834247,556.339391647917,
556.774264953487,557.209138259182,557.644011565003,558.078884870951,558.51375817703,
558.948631483239,559.383504789581,559.818378096058,560.254104096209,560.689830096361,
561.12470340311,561.559576709996,561.994450017021,562.429323324187,562.864196631494,
563.299069938943,563.733943246536,564.168816554273,564.603689862154,565.038563170182,
565.473436478355,565.908309786676,566.343183095144,566.77805640376,567.213782404988,
567.649508406216,568.084381715128,568.519255024189,568.954128333399,569.389001642757,
569.823874952264,570.258748261921,570.693621571725,571.128494881677,571.563368191777,
572.433114812417,572.867988122957,573.302861433642,573.737734744471,574.173460746804,
574.609186749136,575.044060060251,575.913806682904,576.783553306113,577.218426617922,
577.653299929865,578.08817324194,578.523046554147,579.392793178944,580.26253980424,
581.13313912039,581.568865123709,582.003738436771,582.87348506323,583.743231690115,
584.612978317402,585.482724945065,586.352471573076,587.222218201403,588.092817519691,
588.963416838109,589.833163467083,590.702910096251,591.572656725575,592.442403355013,
593.31214998452,594.181896614051,595.05249593303,595.92309525198,596.792841881366,
597.662588510618,598.532335139693,599.402081768556,600.271828397167,601.141575025495,
602.012174343369,602.882773661074,603.752520288553,604.622266915642,605.492013542317,
606.361760168553,607.23150679433,608.101253419626,608.971852735101,609.842452050322,
610.71219867434,611.581945297822,612.451691920754,612.886565232011,613.321438543126,
613.756311854099,614.191185164928,615.060931786153,615.931531098516,616.367257100486,
616.802130410586,617.237003720538,617.671877030342,618.106750339998,618.541623649505,
618.976496958863,619.411370268073,619.846243577134,620.281116886046,620.71599019481,
621.150863503426,621.585736811894,622.020610120214,622.455483428388,622.891209429248,
623.326935430108,623.761808737989,624.196682045726,624.631555353319,625.066428660769,
625.501301968075,625.936175275241,626.371048582266,626.805921889153,627.240795195901,
627.675668502512,628.110541808988,628.54541511533,628.98028842154,629.415161727618,
629.850887727438,630.286613727259,630.72148703308,631.156360338774,631.591233644344,
632.026106949791,632.460980255118,632.895853560325,633.330726865415,633.76560017039,
634.200473475251,634.635346780002,635.070220084644,635.505093389179,635.939966693609,
636.374839997937,636.810565996897,637.246291995857,637.681165299986,638.116038604021,
638.550911907962,638.985785211813,639.420658515576,639.855531819253,640.290405122847,
640.725278426361,641.160151729796,641.595025033157,642.029898336444,642.464771639662,
642.899644942813,643.334518245899,643.770244244257,644.205970242616,644.640843545581,
645.075716848491,645.510590151347,645.945463454153,646.380336756911,646.815210059625,
647.250083362296,647.684956664929,648.119829967526,648.55470327009,648.989576572624,
649.424449875131,649.859323177614,650.294196480076,650.729922478144,651.165648476212,
651.600521778641,652.035395081057,652.470268383465,652.905141685866,653.340014988265,
653.774888290663,654.209761593065,654.644634895472,655.079508197889,655.514381500318,
655.949254802762,656.384128105224,656.819001407706,657.253874710213,657.689600708326,
658.12532670644,658.560200009004,658.995073311601,659.429946614234,659.864819916905,
660.299693219619,660.734566522377,661.169439825183,661.604313128039,662.039186430948,
662.474059733914,662.908933036938,663.343806340025,663.778679643175,664.213552946393,
664.649278944883,665.085004943373,665.519878246733,665.954751550169,666.389624853683,
666.824498157277,667.259371460954,667.694244764717,668.129118068568,668.563991372509,
668.998864676544,669.433737980674,669.868611284901,670.303484589229,670.738357893659,
671.173231198194,671.608957197361,672.044683196528,672.479556501278,672.91442980614,
673.349303111115,673.784176416205,674.219049721412,674.653923026738,675.088796332185,
675.523669637755,675.95854294345,676.393416249271,676.82828955522,677.263162861298,
677.698036167508,678.13290947385,678.568635473934,679.004361474018,679.439234780629,
679.874108087377,680.308981394264,680.743854701289,681.178728008455,681.613601315762,
682.048474623211,682.483347930804,682.91822123854,683.353094546422,683.78796785445,
684.222841162623,684.657714470944,685.092587779412,685.528313780566,685.96403978172,
686.398913090483,686.833786399396,687.268659708457,687.703533017666,688.138406327025,
688.573279636532,689.008152946187,689.443026255992,689.877899565944,690.312772876043,
690.74764618629,691.182519496684,691.617392807224,692.052266117909,692.487992120169,
692.92371812243,693.358591433403,694.228338055774,694.663211367171,695.098084678707,
695.532957990379,695.967831302188,696.402704614131,696.837577926207,697.707324550749,
698.577071175797,699.011944488507,699.447670491767,699.883396495028,700.318269807975,
701.188016434211,702.057763060886,702.927509687976,703.797256315454,704.667002943295,
705.536749571467,706.407348889651,707.277948207973,708.147694836835,709.017441465911,
709.887188095163,710.756934724548,711.626681354026,712.496427983551,713.367027302543,
714.237626621516,715.107373250954,715.977119880277,716.846866509446,717.716613138419,
718.586359767161,719.456106395635,720.32670571363,721.197305031464,722.067051659126,
722.936798286414,723.806544913299,724.676291539758,725.546038165767,726.415784791305,
727.286384106969,728.156983422381,729.026730046663,729.896476670415,730.331349982088,
730.766223293624,731.201096605021,731.635969916278,732.505716538366,733.37546315988,
733.81033647042,734.246062472462,734.681788474505,735.116661784752,735.551535094852,
735.986408404804,736.421281714608,736.856155024264,737.291028333771,737.72590164313,
738.160774952339,738.5956482614,739.030521570312,739.465394879076,739.900268187692,
740.33514149616,740.77001480448,741.205740805414,741.641466806347,742.076340114374,
742.511213422256,742.946086729993,743.380960037585,743.815833345035,744.250706652341,
744.685579959507,745.120453266533,745.555326573419,745.990199880167,746.425073186778,
746.859946493254,747.294819799596,747.729693105806,748.165419105691,748.601145105576,
749.036018411525,749.470891717346,749.90576502304,750.34063832861,750.775511634057,
751.210384939384,751.645258244591,752.080131549682,752.515004854656,752.949878159518,
753.384751464269,753.81962476891,754.254498073445,754.689371377875,755.125097376885,
755.560823375895,755.995696680123,756.430569984253,756.865443288287,757.300316592228,
757.735189896079,758.170063199842,758.604936503519,759.039809807113,759.474683110627,
759.909556414062,760.344429717423,760.779303020711,761.214176323929,761.649049627079,
762.084775625469,762.520501623858,762.955374926883,763.390248229848,763.825121532758,
764.259994835614,764.694868138419,765.129741441178,765.564614743891,765.999488046563,
766.434361349196,766.869234651793,767.304107954357,767.738981256891,768.173854559398,
768.608727861881,769.044453859958,769.480179858035,769.915053160479,770.349926462907,
770.784799765324,771.219673067731,771.654546370133,772.089419672531,772.52429297493,
772.959166277331,773.394039579739,773.828912882155,774.263786184584,774.698659487028,
775.13353278949,775.568406091973,776.004132090072,776.439858088172,776.874731390706,
777.30960469327,777.744477995867,778.1793512985,778.614224601171,779.049097903885,
779.483971206643,779.918844509449,780.353717812305,780.788591115215,781.22346441818,
781.658337721205,782.093211024291,782.528084327442,782.963810325897,783.399536324352,
783.834409627639,784.269282931,784.704156234435,785.139029537949,785.573902841543,
786.00877614522,786.443649448983,786.878522752834,787.313396056775,787.74826936081,
788.183142664939,788.618015969167,789.052889273495,789.487762577925,789.923488577038,
790.359214576152,790.794087880793,791.228961185544,791.663834490406,792.098707795381,
792.533581100471,792.968454405678,793.403327711004,793.838201016451,794.273074322021,
794.707947627716,795.142820933537,795.577694239486,796.012567545564,796.447440851774,
796.883166851791,797.318892851808,797.753766158284,798.188639464895,798.623512771643,
799.058386078529,799.493259385555,799.92813269272,800.363006000027,800.797879307477,
801.232752615069,801.667625922806,802.102499230688,802.537372538715,802.972245846889,
803.40711915521,803.84284515629,804.27857115737,804.713444465985,805.148317774749,
805.583191083662,806.018064392723,806.452937701933,806.887811011291,807.322684320798,
808.192430940258,808.62730425021,809.06217756031,809.497050870557,809.931924180951,
810.36679749149,810.802523493679,811.238249495867,811.673122806697,812.542869428785,
812.977742740041,813.412616051438,813.847489362974,814.282362674646,814.717235986455,
815.152109298398,816.021855922681,816.891602547478,817.326475860065,817.762201863265,
818.197927866466,818.632801179295,819.502547805304,820.372294431763,821.242041058648,
822.111787685935,822.981534313598,823.851280941609,824.721880259681,825.5924795779,
826.462226206642,827.331972835616,828.201719464785,829.071466094109,829.941212723546,
830.810959353053,831.681558672047,832.552157991036,833.421904620514,834.2916512499,
835.161397879151,836.031144508226,836.900891137089,837.770637765701,838.641237083811,
839.511836401767,840.381583029608,841.251329657086,842.121076284176,842.990822910851,
843.860569537087,844.730316162863,845.600915478712,846.471514794314,847.341261418855,
848.211008042874,848.645881354683,849.080754666356,849.515627977891,849.950501289288,
850.82024791166,851.689994533462,852.124867844147,852.560593846263,852.996319848379,
853.431193158772,853.866066469019,854.300939779119,855.170686398875,855.605559708531,
856.040433018038,856.475306327397,856.910179636606,857.345052945667,857.77992625458,
858.214799563344,858.64967287196,859.084546180427,859.520272181434,859.95599818244,
860.390871490614,860.825744798641,861.260618106523,861.69549141426,862.130364721852,
862.565238029302,863.000111336609,863.434984643774,863.8698579508,864.304731257686,
864.739604564434,865.174477871045,865.609351177521,866.044224483863,866.479950483814,
866.915676483765,867.350549789843,867.785423095792,868.220296401613,868.655169707307,
869.090043012877,869.524916318325,869.959789623651,870.394662928858,870.829536233948,
871.264409538923,871.699282843785,872.134156148535,872.569029453177,873.003902757712,
873.439628756773,873.875354755834,874.310228060162,874.745101364389,875.179974668519,
875.614847972553,876.049721276495,876.484594580346,876.919467884108,877.354341187786,
877.78921449138,878.224087794893,878.658961098329,879.093834401689,879.528707704977,
879.963581008195,880.399307006616,880.835033005038,881.269906308124,881.704779611148,
882.139652914114,882.574526217024,883.00939951988,883.444272822685,883.879146125444,
884.314019428157,884.748892730829,885.183766033462,885.618639336059,886.053512638623,
886.488385941157,886.923259243664,887.358985241751,887.794711239839,888.2295845423,
888.664457844744,889.099331147173,889.534204449589,889.969077751997,890.403951054398,
890.838824356797,891.273697659195,891.708570961597,892.143444264004,892.578317566421,
893.01319086885,893.448064171293,893.882937473755,894.318663471843,894.75438946993,
895.189262772437,895.624136074971,896.059009377535,896.493882680132,896.928755982765,
897.363629285437,897.798502588151,898.233375890909,898.668249193715,899.103122496571,
899.53799579948,899.972869102446,900.40774240547,900.842615708556,901.278341706978,
901.714067705399,902.148941008617,902.583814311905,903.018687615265,903.453560918701,
903.888434222214,904.323307525808,904.758180829485,905.193054133248,905.627927437099,
906.06280074104,906.497674045075,906.932547349205,907.367420653433,907.80229395776,
908.238019956821,908.673745955883,909.108619260417,909.543492565059,909.978365869809,
910.413239174671,910.848112479646,911.282985784736,911.717859089943,912.152732395269,
912.587605700716,913.022479006287,913.457352311981,913.892225617802,914.327098923751,
914.761972229829,915.19769822978,915.633424229731,916.068297536072,916.503170842548,
916.93804414916,917.372917455908,917.807790762794,918.24266406982,918.677537376985,
919.112410684292,919.547283991742,919.982157299334,920.417030607071,920.851903914953,
921.28677722298,921.721650531154,922.15737653216,922.593102533167,923.027975841635,
923.46284915025,923.897722459014,924.332595767926,924.767469076987,925.202342386197,
925.637215695556,926.072089005063,926.506962314719,926.941835624523,927.376708934475,
927.811582244575,928.246455554822,928.681328865215,929.117054867331,929.987654180132,
930.422527490961,930.857400801934,931.292274113049,931.727147424306,932.162020735703,
932.596894047238,933.46664067072,934.336387294739,934.771260606945,935.20613391928,
935.641007231742,936.076733234882,936.94733255073,937.817079176507,938.686825802743,
939.556572429418,940.426319056508,941.296065683986,942.165812311827,943.036411629783,
943.907010947893,944.776757576505,945.646504205367,946.516250834443,947.385997463694,
948.25574409308,949.125490722558,949.996090041546,950.86668936054,951.736435990048,
952.606182619485,953.475929248809,954.345675877978,955.215422506951,956.085169135693,
956.955768453912,957.826367771985,958.696114399995,959.565861027658,960.435607654946,
961.305354281831,962.175100908289,963.044847534298,963.915446850328,964.786046166116,
965.655792790913,966.525539415195,966.960412727138,967.395286038947,968.265032662155,
969.134779284809,969.569652595924,970.004525906897,970.439399217726,970.875125219914,
971.310851222103,971.745724532643,972.615471153283,973.485217773335,973.920091083139,
974.354964392795,974.789837702302,975.22471101166,975.65958432087,976.094457629931,
976.529330938844,976.964204247608,977.399077556223,977.834803557303,978.270529558383,
978.705402866704,979.140276174877,979.575149482905,980.010022790786,980.444896098523,
980.879769406116,981.314642713565,981.749516020872,982.184389328038,982.619262635063,
983.05413594195,983.489009248698,983.923882555309,984.358755861785,984.794481861802,
985.230207861819,985.665081168029,986.099954474107,986.534827780056,986.969701085877,
987.404574391571,987.839447697141,988.274321002589,988.709194307915,989.144067613122,
989.578940918212,990.013814223187,990.448687528048,990.883560832799,991.31843413744,
991.754160136554,992.189886135667,992.624759440097,993.059632744425,993.494506048653,
993.929379352783,994.364252656817,994.799125960758,995.233999264609,995.668872568372,
996.103745872049,996.538619175643,996.973492479157,997.408365782593,997.843239085953,
998.278112389241,998.713838387696,999.149564386151,999.584437689301,1000.01931099239,
1000.45418429541,1000.88905759838,1001.32393090129,1001.75880420414,1002.19367750695,
1002.62855080971,1003.06342411242,1003.49829741509,1003.93317071773,1004.36804402032,
1004.80291732289,1005.23779062542,1005.67351662352,1006.10924262162,1006.5441159241,
1006.97898922656,1007.41386252901,1007.84873583144,1008.28360913385,1008.71848243626,
1009.15335573866,1009.58822904106,1010.02310234346,1010.45797564586,1010.89284894827,
1011.32772225069,1011.76259555311,1012.19746885556,1012.63319485364,1013.06892085171,
1013.5037941542,1013.9386674567,1014.37354075924,1014.8084140618,1015.2432873644,
1015.67816066703,1016.1130339697,1016.54790727242,1016.98278057517,1017.41765387798,
1017.85252718084,1018.28740048375,1018.72227378671,1019.15714708974,1019.59287308813,
1020.02859908651,1020.46347238967,1020.89834569288,1021.33321899617,1021.76809229953,
1022.20296560297,1022.63783890648,1023.07271221007,1023.50758551375,1023.94245881752,
1024.37733212137,1024.81220542531,1025.24707872935,1025.68195203348,1026.11682533771,
1026.55255133672,1026.98827733573,1027.42315064016,1027.8580239447,1028.29289724934,
1028.72777055409,1029.16264385896,1029.59751716393,1030.03239046902,1030.46726377423,
1030.90213707956,1031.33701038501,1031.77188369058,1032.20675699628,1032.6416303021,
1033.07650360805,1033.51222960793,1033.94795560782,1034.38282891403,1034.81770222038,
1035.25257552685,1035.68744883347,1036.12232214022,1036.5571954471,1036.99206875413,
1037.4269420613,1037.86181536861,1038.29668867606,1038.73156198365,1039.16643529139,
1039.60130859927,1040.0361819073,1040.47190790824,1040.90763390917,1041.34250721749,
1041.77738052596,1042.21225383458,1042.64712714334,1043.08200045226,1043.95174707053,
1044.38662037989,1044.8214936894,1045.25636699906,1045.69124030886,1046.12611361882,
1046.56098692892,1046.99586023917,1047.43158624121,1047.86731224325,1048.3021855538,
1048.73705886448,1049.17193217531,1049.60680548629,1050.0416787974,1050.47655210866,
1050.91142542006,1051.78117204327,1052.21604535508,1052.65091866703,1053.0857919791,
1053.52066529131,1053.95553860365,1054.39126460673,1055.26186392239,1056.13161054793,
1057.00135717395,1057.43623048712,1057.87110380041,1058.7408504273,1059.61059705459,
1060.48034368225,1061.35094300009,1062.22154231809,1063.09128894656,1063.96103557531,
1064.83078220429,1065.70052883346,1066.57027546278,1067.44002209222,1068.3106214112,
1069.18122073019,1070.05096735972,1070.9207139892,1071.79046061859,1072.66020724785,
1073.52995387693,1074.39970050579,1075.27029982411,1076.1408991423,1077.01064577048,
1077.88039239832,1078.7501390258,1079.61988565289,1080.48963227957,1081.35937890581,
1082.22997822202,1083.100577538,1083.97032416305,1084.84007078759,1085.70981741161,
1086.5795640351,1087.44931065803,1087.88418396929,1088.31905728041,1088.75393059138,
1089.18965659365,1089.62538259591,1090.06025590659,1090.93000252753,1091.36487583778,
1091.79974914788,1092.23462245783,1092.66949576764,1093.1043690773,1093.5392423868,
1093.97411569616,1094.40898900538,1094.84386231444,1095.27873562335,1095.71360893212,
1096.14933493327,1096.58506093443,1097.0199342429,1097.45480755122,1097.88968085939,
1098.32455416742,1098.75942747531,1099.19430078305,1099.62917409064,1100.06404739809,
1100.4989207054,1100.93379401257,1101.36866731959,1101.80354062648,1102.23841393323,
1102.67328723984,1103.10901323993,1103.54473924001,1103.97961254636,1104.41448585257,
1104.84935915865,1105.2842324646,1105.71910577042,1106.15397907612,1106.58885238169,
1107.02372568714,1107.45859899246,1107.89347229767,1108.32834560276,1108.76321890774,
1109.1980922126,1109.63296551736,1110.06869151652,1110.50441751569,1110.93929082023,
1111.37416412466,1111.80903742899,1112.24391073322,1112.67878403735,1113.11365734139,
1113.54853064533,1113.98340394918,1114.41827725295,1114.85315055662,1115.28802386022,
1115.72289716374,1116.15777046717,1116.59264377053,1117.02836976903,1117.46409576752,
1117.89896907074,1118.33384237389,1118.76871567698,1119.20358898,1119.63846228297,
1120.07333558588,1120.50820888874,1120.94308219154,1121.3779554943,1121.81282879702,
1122.24770209969,1122.68257540233,1123.11744870492,1123.55232200749,1123.98804800561,
1124.42377400372,1124.85864730623,1125.29352060871,1125.72839391118,1126.16326721362,
1126.59814051605,1127.03301381847,1127.46788712088,1127.90276042328,1128.33763372568,
1128.77250702808,1129.20738033048,1129.64225363289,1130.07712693531,1130.51200023774,
1130.94772623581,1131.38345223388,1131.81832553634,1132.25319883883,1132.68807214134,
1133.12294544387,1133.55781874644,1133.99269204904,1134.42756535167,1134.86243865434,
1135.29731195706,1135.73218525982,1136.16705856263,1136.60193186548,1137.03680516839,
1137.47167847136,1137.90740446972,1138.34313046808,1138.77800377117,1139.21287707432,
1139.64775037754,1140.08262368083,1140.51749698419,1140.95237028763,1141.38724359114,
1141.82211689474,1142.25699019842,1142.69186350218,1143.12673680603,1143.56161010998,
1143.99648341401,1144.43135671814,1144.86708271711,1145.30280871607,1145.7376820204,
1146.17255532483,1146.60742862936,1147.04230193401,1147.47717523876,1147.91204854362,
1148.3469218486,1148.78179515369,1149.2166684589,1149.65154176423,1150.08641506968,
1150.52128837525,1150.95616168094,1151.39103498677,1151.82676098659,1152.26248698641,
1152.69736029249,1153.1322335987,1153.56710690504,1154.00198021152,1154.43685351813,
1154.87172682488,1155.30660013177,1155.7414734388,1156.17634674597,1156.61122005327,
1157.04609336073,1157.48096666832,1157.91583997606,1158.35071328394,1158.7864392848,
1159.22216528566,1159.65703859384,1160.09191190216,1160.52678521063,1160.96165851925,
1161.39653182801,1161.83140513693,1162.26627844599,1162.7011517552,1163.13602506456,
1163.57089837407,1164.00577168373,1164.44064499353,1164.87551830349,1165.74611761556,
1166.18184361753,1166.61671692792,1167.05159023846,1167.48646354915,1167.92133685998,
1168.35621017096,1169.22595679333,1170.09570341627,1170.53057672794,1170.96545003975,
1171.4003233517,1171.83519666377,1172.27006997598,1172.705795979,1173.57639529447,
1174.44614191977,1174.8810152326,1175.31588854555,1176.18563517179,1177.05538179847,
1177.92512842556,1178.79487505304,1179.66547437075,1180.53607368863,1181.40582031696,
1182.27556694557,1183.14531357444,1184.01506020352,1184.88480683277,1185.75455346216,
1186.62515278112,1187.4957521001,1188.36549872963,1189.23524535914,1190.10499198858,
1190.97473861791,1191.84448524708,1192.71423187606,1193.58483119448,1194.45543051277,
1195.3251771411,1196.19492376911,1197.06467039678,1197.93441702407,1198.80416365096,
1199.67391027742,1200.5445095938,1201.41510890996,1202.28485553525,1203.15460216005,
1204.02434878434,1204.89409540809,1205.76384203131,1206.1987153427,1206.63358865396,
1207.06846196508,1207.50418796741,1208.37478728058,1209.2445339018,1209.6794072122,
1210.11428052245,1210.54915383255,1210.9840271425,1211.41890045231,1211.85377376197,
1212.28864707147,1212.72352038083,1213.15839369005,1213.59326699911,1214.02814030802,
1214.46386630925,1214.89959231048,1215.3344656191,1215.76933892757,1216.20421223589,
1216.63908554406,1217.07395885209,1217.50883215998,1217.94370546771,1218.37857877531,
1218.81345208276,1219.24832539007,1219.68319869724,1220.11807200426,1220.55294531115,
1220.9878186179,1221.42354461805,1221.85927061821,1222.29414392468,1222.72901723103,
1223.16389053724,1223.59876384332,1224.03363714927,1224.46851045509,1224.90338376079,
1225.33825706636,1225.77313037181,1226.20800367713,1226.64287698234,1227.07775028743,
1227.51262359241,1227.94749689727,1228.3832228965,1228.81894889572,1229.25382220036,
1229.6886955049,1230.12356880933,1230.55844211366,1230.99331541789,1231.42818872202,
1231.86306202606,1232.29793533,1232.73280863385,1233.16768193762,1233.60255524129,
1234.03742854489,1234.4723018484,1234.90717515184,1235.34290115037,1235.7786271489,
1236.21350045219,1236.64837375541,1237.08324705856,1237.51812036165,1237.95299366467,
1238.38786696764,1238.82274027055,1239.25761357341,1239.69248687621,1240.12736017897,
1240.56223348169,1240.99710678436,1241.431980087,1241.8668533896,1242.30257938773,
1242.73830538585,1243.17317868839,1243.6080519909,1244.04292529338,1244.47779859585,
1244.91267189829,1245.34754520072,1245.78241850314,1246.21729180555,1246.65216510795,
1247.08703841035,1247.52191171275,1247.95678501515,1248.39165831756,1248.82653161998,
1249.26225761804,1249.69798361611,1250.13285691855,1250.56773022101,1251.0026035235,
1251.43747682601,1251.87235012854,1252.30722343111,1252.74209673371,1253.17697003634,
1253.61184333901,1254.04671664173,1254.48158994449,1254.9164632473,1255.35133655015,
1255.78620985306,1256.22193585139,1256.65766184973,1257.09253515275,1257.52740845584,
1257.96228175899,1258.39715506221,1258.8320283655,1259.26690166886,1259.7017749723,
1260.13664827581,1260.57152157941,1261.00639488309,1261.44126818685,1261.8761414907,
1262.31101479465,1262.74588809868,1263.1816140976,1263.61734009651,1264.05221340074,
1264.48708670507,1264.9219600095,1265.35683331403,1265.79170661868,1266.22657992343,
1266.66145322829,1267.09632653327,1267.53119983836,1267.96607314357,1268.4009464489,
1268.83581975434,1269.27069305992,1269.70556636561,1270.14129236537,1270.57701836513,
1271.01189167108,1271.44676497716,1271.88163828337,1272.31651158971,1272.75138489619,
1273.1862582028,1273.62113150955,1274.05600481644,1274.49087812347,1274.92575143063,
1275.36062473794,1275.79549804539,1276.23037135299,1276.66524466073,1277.10097066151,
1277.5366966623,1277.97156997033,1278.40644327851,1278.84131658683,1279.2761898953,
1279.71106320392,1280.14593651268,1280.5808098216,1281.01568313066,1281.45055643987,
1281.88542974923,1282.32030305874,1282.75517636839,1283.1900496782,1283.62492298815,
1284.06064899005,1284.49637499195,1284.9312483022,1285.36612161259,1285.80099492313,
1286.23586823382,1286.67074154465,1287.54048816674,1287.975361478,1288.4102347894,
1288.84510810093,1289.27998141261,1289.71485472442,1290.14972803636,1291.02032735139,
1291.89092666668,1292.32579997914,1292.76067329173,1293.19554660444,1293.63041991727,
1294.50016654328,1295.36991316974,1296.23965979663,1297.10940642392,1297.9800057415,
1298.85060505925,1299.72035168742,1300.5900983159,1301.45984494464,1302.32959157362,
1303.19933820279,1304.06908483212,1304.93968415104,1305.81028347,1306.68003009953,
1307.54977672906,1308.41952335854,1309.28926998793,1310.15901661718,1311.02876324626,
1311.89936256477,1312.76996188316,1313.63970851164,1314.50945513981,1315.37920176765,
1316.24894839514,1317.11869502223,1317.98844164891,1318.85904096546,1319.72964028179,
1320.59938690733,1321.46913353238,1322.33888015692,1323.20862678095,1323.64350009276,
1324.07837340443,1324.51324671597,1324.94812002737,1325.81871934103,1326.68931865441,
1327.12419196524,1327.55906527593,1327.99393858647,1328.42881189686,1328.86368520711,
1329.29855851721,1329.73343182716,1330.16830513697,1330.60317844663,1331.03805175614,
1331.4729250655,1331.90779837471,1332.34267168377,1332.77839768507,1333.21412368638,
1333.64899699514,1334.08387030376,1334.51874361223,1334.95361692055,1335.38849022873,
1335.82336353676,1336.25823684464,1336.69311015238,1337.12798345997,1337.56285676742,
1337.99773007473,1338.4326033819,1338.86747668892,1339.30234999581,1339.73807599603,
1340.17380199625,1340.60867530287,1341.04354860934,1341.47842191569,1341.9132952219,
1342.34816852798,1342.78304183393,1343.21791513975,1343.65278844545,1344.08766175102,
1344.52253505647,1344.95740836179,1345.392281667,1345.82715497209,1346.26202827707,
1346.69775427635,1347.13348027563,1347.56835358038,1348.00322688502,1348.43810018956,
1348.87297349399,1349.30784679832,1349.74272010255,1350.17759340668,1350.61246671072,
1351.04734001466,1351.48221331851,1351.91708662228,1352.35195992595,1352.78683322955,
1353.22170653306,1353.65743253163,1354.09315853019,1354.52803183356,1354.96290513685,
1355.39777844007,1355.83265174322,1356.26752504631,1356.70239834933,1357.1372716523,
1357.57214495521,1358.00701825807,1358.44189156087,1358.87676486363,1359.31163816635,
1359.74651146902,1360.18138477166,1360.6171107698,1361.05283676795,1361.48771007051,
1361.92258337305,1362.35745667556,1362.79232997804,1363.2272032805,1363.66207658295,
1364.09694988538,1364.5318231878,1364.96669649021,1365.40156979261,1365.83644309501,
1366.27131639741,1366.70618969981,1367.14106300222,1367.57678900028,1368.01251499834,
1368.44738830077,1368.88226160321,1369.31713490567,1369.75200820816,1370.18688151067,
1370.6217548132,1371.05662811577,1371.49150141837,1371.926374721,1372.36124802367,
1372.79612132639,1373.23099462915,1373.66586793196,1374.10074123481,1374.53646723311,
1374.97219323142,1375.40706653438,1375.84193983741,1376.2768131405,1376.71168644365,
1377.14655974687,1377.58143305016,1378.01630635352,1378.45117965696,1378.88605296047,
1379.32092626407,1379.75579956775,1380.19067287151,1380.62554617536,1381.06041947931,
1381.49614547817,1381.93187147704,1382.36674478117,1382.8016180854,1383.23649138973,
1383.67136469416,1384.10623799869,1384.54111130334,1384.97598460809,1385.41085791295,
1385.84573121793,1386.28060452302,1386.71547782823,1387.15035113356,1387.585224439,
1388.02009774458,1388.45582374427,1388.89154974397,1389.32642304979,1389.76129635574,
1390.19616966182,1390.63104296803,1391.06591627437,1391.50078958085,1391.93566288746,
1392.37053619421,1392.8054095011,1393.24028280813,1393.6751561153,1394.1100294226,
1394.54490273005,1394.97977603765,1395.41550203836,1395.85122803908,1396.28610134696,
1396.72097465499,1397.15584796317,1397.59072127149,1398.02559457996,1398.46046788858,
1398.89534119734,1399.33021450626,1399.76508781532,1400.19996112453,1400.63483443389,
1401.50458105306,1401.93945436286,1402.37518036469,1402.81090636651,1403.24577967661,
1403.68065298686,1404.11552629725,1404.5503996078,1404.98527291848,1405.85501954029,
1406.2898928514,1406.72476616266,1407.15963947406,1407.5945127856,1408.02938609727,
1408.46425940908,1409.33485872391,1410.205458039,1410.64033135134,1411.07520466381,
1411.51007797639,1411.9449512891,1412.81469791488,1413.68444454112,1414.5541911678,
1415.42393779489,1416.29453711233,1417.16513642995,1418.03488305796,1418.90462968629,
1419.77437631491,1420.64412294377,1421.51386957285,1422.38361620211,1423.25421552099,
1424.12481483992,1424.99456146943,1425.86430809896,1426.73405472847,1427.60380135791,
1428.47354798724,1429.34329461641,1430.21389393501,1431.08449325349,1431.9542398821,
1432.82398651043,1433.69373313844,1434.56347976611,1435.4332263934,1436.30297302029,
1437.17357233701,1438.04417165351,1438.91391827929,1439.78366490459,1440.65341152939,
1441.52315815367,1441.95803146562,1442.39290477743,1442.8277780891,1443.26265140064,
1444.13325071451,1445.00385002811,1445.43872333908,1445.87359664991,1446.3084699606,
1446.74334327114,1447.17821658153,1447.61308989178,1448.48283651184,1448.91770982164,
1449.3525831313,1449.78745644081,1450.22232975017,1450.65720305938,1451.09292906076,
1451.52865506214,1451.96352837105,1452.39840167982,1452.83327498843,1453.2681482969,
1453.70302160522,1454.1378949134,1454.57276822143,1455.00764152931,1455.44251483705,
1455.87738814464,1456.31226145209,1456.7471347594,1457.18200806657,1457.6168813736,
1458.05260737389,1458.48833337418,1458.92320668093,1459.35807998754,1459.79295329402,
1460.22782660036,1460.66269990657,1461.09757321265,1461.5324465186,1461.96731982443,
1462.40219313012,1462.83706643569,1463.27193974114,1463.70681304647,1464.14168635168,
1464.57655965677,1465.0122856561,1465.44801165544,1465.8828849603,1466.31775826505,
1466.7526315697,1467.18750487423,1467.62237817866,1468.05725148299,1468.49212478722,
1468.92699809135,1469.36187139539,1469.79674469933,1470.23161800319,1470.66649130695,
1471.10136461063,1471.53623791422,1471.97196391283,1472.40768991143,1472.84256321487,
1473.27743651823,1473.71230982152,1474.14718312474,1474.58205642789,1475.01692973098,
1475.451803034,1475.88667633697,1476.32154963988,1476.75642294274,1477.19129624555,
1477.62616954831,1478.06104285102,1478.4959161537,1478.93164215186,1479.36736815002,
1479.80224145262,1480.23711475519,1480.67198805772,1481.10686136023,1481.54173466272,
1481.97660796518,1482.41148126762,1482.84635457005,1483.28122787247,1483.71610117488,
1484.15097447728,1484.58584777968,1485.02072108208,1485.45559438449,1485.89132038254,
1486.32704638059,1486.76191968301,1487.19679298544,1487.63166628788,1488.06653959035,
1488.50141289283,1488.93628619534,1489.37115949787,1489.80603280044,1490.24090610304,
1490.67577940567,1491.11065270835,1491.54552601106,1491.98039931382,1492.41527261663,
1492.8509986149,1493.28672461318,1493.72159791609,1494.15647121906,1494.59134452208,
1495.02621782517,1495.46109112832,1495.89596443154,1496.33083773483,1496.76571103819,
1497.20058434163,1497.63545764515,1498.07033094874,1498.50520425242,1498.94007755618,
1499.37495086004,1499.81067685885,1500.24640285767,1500.68127616171,1501.11614946584,
1501.55102277007,1501.9858960744,1502.42076937883,1502.85564268337,1503.29051598801,
1503.72538929276,1504.16026259762,1504.5951359026,1505.03000920769,1505.4648825129,
1505.89975581823,1506.33462912368,1506.77035512331,1507.20608112294,1507.64095442864,
1508.07582773446,1508.51070104041,1508.94557434649,1509.3804476527,1509.81532095904,
1510.25019426552,1510.68506757213,1511.11994087888,1511.55481418577,1511.9896874928,
1512.42456079996,1512.85943410727,1513.29430741472,1513.73003341537,1514.16575941601,
1514.60063272375,1515.03550603163,1515.47037933966,1515.90525264784,1516.34012595616,
1516.77499926463,1517.20987257325,1517.64474588201,1518.07961919093,1518.51449249999,
1518.9493658092,1519.38423911856,1519.81911242807,1520.25398573772,1520.68971173947,
1521.12543774122,1521.56031105118,1521.99518436128,1522.43005767153,1523.29980429246,
1523.73467760315,1524.16955091398,1524.60442422495,1525.03929753607,1525.47417084733,
1525.90904415873,1526.77879078194,1527.64939009657,1528.08511609939,1528.51998941146,
1528.95486272367,1529.38973603601,1530.25948266106,1531.1292292866,1531.99897591261,
1532.86872253907,1533.73846916596,1534.60906848325,1535.47966780073,1536.34941442858,
1537.21916105675,1538.08890768523,1538.95865431398,1539.82840094295,1540.69814757212,
1541.56874689096,1542.43934620985,1543.30909283933,1544.17883946886,1545.04858609839,
1545.91833272787,1546.78807935726,1547.65782598651,1548.52842530518,1549.39902462375,
1550.26877125249,1551.13851788097,1552.00826450914,1552.87801113699,1553.74775776447,
1554.61750439156,1555.48810370844,1556.35870302511,1557.22844965112,1558.09819627666,
1558.96794290171,1559.83768952626,1560.27256283834,1560.70743615028,1561.57718277377,
1562.44778208785,1563.31838140165,1563.75325471277,1564.18812802374,1564.62300133457,
1565.05787464526,1565.9276212662,1566.79736788655,1567.2322411965,1567.66711450631,
1568.10198781596,1568.53686112547,1568.97173443483,1569.40746043628,1569.84318643774,
1570.2780597468,1570.71293305571,1571.14780636448,1571.5826796731,1572.01755298157,
1572.45242628989,1572.88729959806,1573.32217290609,1573.75704621397,1574.19191952171,
1574.62679282931,1575.06166613676,1575.49653944407,1575.93141275123,1576.36713875159,
1576.80286475195,1577.23773805884,1577.67261136559,1578.1074846722,1578.54235797868,
1578.97723128502,1579.41210459124,1579.84697789732,1580.28185120327,1580.71672450909,
1581.15159781478,1581.58647112036,1582.0213444258,1582.45621773113,1582.89109103634,
1583.32681703573,1583.76254303513,1584.1974163401,1584.63228964497,1585.06716294972,
1585.50203625436,1585.9369095589,1586.37178286333,1586.80665616766,1587.24152947189,
1587.67640277602,1588.11127608005,1588.546149384,1588.98102268785,1589.41589599161,
1589.85076929529,1590.28649529394,1590.72222129258,1591.1570945961,1591.59196789953,
1592.0268412029,1592.46171450619,1592.8965878094,1593.33146111256,1593.76633441564,
1594.20120771867,1594.63608102164,1595.07095432455,1595.50582762741,1595.94070093021,
1596.37557423297,1596.81044753569,1597.24617353387,1597.68189953206,1598.11677283469,
1598.55164613729,1598.98651943985,1599.42139274239,1599.8562660449,1600.29113934738,
1600.72601264985,1601.16088595229,1601.59575925472,1602.03063255714,1602.46550585955,
1602.90037916195,1603.33525246435,1603.77012576675,1604.2058517648,1604.64157776285,
1605.07645106526,1605.51132436768,1605.94619767011,1606.38107097255,1606.81594427502,
1607.2508175775,1607.68569088001,1608.12056418254,1608.55543748511,1608.99031078771,
1609.42518409034,1609.86005739302,1610.29493069573,1610.72980399849,1611.16552999674,
1611.60125599499,1612.03612929785,1612.47100260076,1612.90587590373,1613.34074920675,
1613.77562250984,1614.21049581299,1614.64536911621,1615.0802424195,1615.51511572286,
1615.9499890263,1616.38486232981,1616.81973563341,1617.25460893709,1617.68948224085,
1618.12520823963,1618.5609342384,1618.99580754234,1619.43068084638,1619.86555415051,
1620.30042745474,1620.73530075907,1621.1701740635,1621.60504736804,1622.03992067268,
1622.47479397743,1622.90966728229,1623.34454058727,1623.77941389236,1624.21428719757,
1624.6491605029,1625.08488650247,1625.52061250204,1625.95548580761,1626.39035911331,
1626.82523241913,1627.26010572508,1627.69497903116,1628.12985233737,1628.56472564372,
1628.99959895019,1629.43447225681,1629.86934556356,1630.30421887044,1630.73909217747,
1631.17396548464,1631.60883879195,1632.04456479252,1632.48029079309,1632.91516410068,
1633.35003740842,1633.78491071631,1634.21978402433,1634.65465733251,1635.08953064083,
1635.5244039493,1635.95927725792,1636.39415056668,1636.8290238756,1637.26389718466,
1637.69877049387,1638.13364380323,1638.56851711274,1639.00424311442,1639.43996911609,
1639.8748424259,1640.30971573585,1640.74458904595,1641.6143356666,1642.04920897714,
1642.48408228782,1642.91895559865,1643.35382890963,1643.78870222074,1644.223575532,
1645.09332215494,1645.52819546661,1645.96392146936,1646.39964747212,1646.83452078406,
1647.26939409614,1647.70426740834,1648.57401403314,1649.44376065844,1650.31350728422,
1650.74838059729,1651.18325391046,1652.05300053714,1652.92359985428,1653.79419917162,
1654.66394579929,1655.5336924273,1656.40343905563,1657.27318568424,1658.14293231311,
1659.01267894219,1659.88327826096,1660.75387757982,1661.62362420926,1662.49337083877,
1663.3631174683,1664.23286409781,1665.10261072725,1665.97235735658,1666.84295667531,
1667.71355599396,1668.58330262282,1669.45304925143,1670.32279587976,1671.19254250778,
1672.06228913544,1672.93203576273,1673.80263507977,1674.6732343966,1675.54298102284,
1676.41272764862,1677.28247427392,1678.15222089872,1679.021967523,1679.89171414676,
1680.76231346105,1681.19803946366,1681.63291277506,1682.06778608632,1682.50265939743,
1682.93753270841,1683.37240601924,1684.24215264047,1684.67702595086,1685.11189926111,
1685.54677257121,1685.98164588116,1686.41651919097,1686.85139250063,1687.28626581014,
1687.72199181166,1688.15771781319,1688.5925911224,1689.02746443146,1689.46233774038,
1689.89721104914,1690.33208435776,1690.76695766623,1691.20183097455,1691.63670428272,
1692.07157759075,1692.50645089864,1692.94132420637,1693.37619751397,1693.81107082142,
1694.24594412873,1694.68167012916,1695.11739612959,1695.55226943662,1695.9871427435,
1696.42201605025,1696.85688935687,1697.29176266334,1697.72663596969,1698.1615092759,
1698.59638258198,1699.03125588793,1699.46612919375,1699.90100249945,1700.33587580502,
1700.77074911047,1701.20562241579,1701.64134841525,1702.0770744147,1702.51194771979,
1702.94682102476,1703.38169432963,1703.81656763438,1704.25144093902,1704.68631424356,
1705.12118754799,1705.55606085232,1705.99093415655,1706.42580746068,1706.86068076471,
1707.29555406866,1707.73042737251,1708.16530067627,1708.60102667496,1709.03675267365,
1709.47162597724,1709.90649928076,1710.34137258419,1710.77624588756,1711.21111919085,
1711.64599249406,1712.08086579722,1712.5157391003,1712.95061240333,1713.3854857063,
1713.82035900921,1714.25523231207,1714.69010561487,1715.12497891763,1715.56070491584,
1715.99643091404,1716.43130421671,1716.86617751935,1717.30105082195,1717.73592412451,
1718.17079742705,1718.60567072956,1719.04054403204,1719.4754173345,1719.91029063695,
1720.34516393938,1720.7800372418,1721.21491054421,1721.64978384661,1722.08465714901,
1722.52038314706,1722.9561091451,1723.39098244751,1723.82585574992,1724.26072905233,
1724.69560235476,1725.13047565721,1725.56534895967,1726.00022226216,1726.43509556467,
1726.8699688672,1727.30484216977,1727.73971547236,1728.174588775,1728.60946207767,
1729.04433538039,1729.48006137861,1729.91578737684,1730.35066067965,1730.78553398251,
1731.22040728542,1731.65528058838,1732.09015389141,1732.5250271945,1732.95990049765,
1733.39477380087,1733.82964710416,1734.26452040752,1734.69939371096,1735.13426701447,
1735.56914031807,1736.00401362175,1736.43973962048,1736.8754656192,1737.31033892306,
1737.745212227,1738.18008553104,1738.61495883517,1739.0498321394,1739.48470544373,
1739.91957874816,1740.35445205269,1740.78932535734,1741.22419866209,1741.65907196695,
1742.09394527193,1742.52881857702,1742.96369188223,1743.39941788174,1743.83514388125,
1744.2700171867,1744.70489049227,1745.13976379797,1745.57463710379,1746.00951040974,
1746.44438371582,1746.87925702203,1747.31413032837,1747.74900363485,1748.18387694146,
1748.61875024821,1749.0536235551,1749.48849686213,1749.92337016929,1750.3590961698,
1750.7948221703,1751.22969547775,1751.66456878534,1752.09944209308,1752.53431540096,
1752.96918870899,1753.40406201717,1753.83893532549,1754.27380863396,1754.70868194258,
1755.14355525134,1755.57842856026,1756.01330186932,1756.44817517853,1756.88304848789,
1757.31877448949,1757.75450049109,1758.18937380075,1759.05912042051,1759.49399373061,
1759.92886704086,1760.36374035125,1760.79861366179,1761.23348697248,1761.66836028331,
1762.10323359429,1762.5381069054,1763.40785352806,1763.8427268396,1764.27845284228,
1764.71417884496,1765.14905215677,1765.58392546872,1766.0187987808,1766.88854540534,
1767.75829203039,1768.1931653431,1768.62803865593,1769.06291196888,1769.49778528195,
1770.36753190841,1771.2381312254,1772.10873054259,1772.97847717007,1773.84822379791,
1774.71797042609,1775.58771705456,1776.45746368331,1777.32721031228,1778.19780963089,
1779.06840894783,1779.93815555508,1780.80790201176,1781.67764871408),(-1.76619037896906,
-1.18309518948453),.UNSPECIFIED.) ;
#826 = B_SPLINE_SURFACE_WITH_KNOTS('',3,1,((#72010,#72011),(#72012,#72013),
(#72014,#72015),(#72016,#72017),(#72018,#72019),(#72020,#72021),(#72022,
#72023),(#72024,#72025),(#72026,#72027),(#72028,#72029),(#72030,#72031),
(#72032,#72033),(#72034,#72035),(#72036,#72037),(#72038,#72039),(#72040,
#72041),(#72042,#72043),(#72044,#72045),(#72046,#72047),(#72048,#72049),
(#72050,#72051),(#72052,#72053),(#72054,#72055),(#72056,#72057),(#72058,
#72059),(#72060,#72061),(#72062,#72063),(#72064,#72065),(#72066,#72067),
(#72068,#72069),(#72070,#72071),(#72072,#72073),(#72074,#72075),(#72076,
#72077),(#72078,#72079),(#72080,#72081),(#72082,#72083),(#72084,#72085),
(#72086,#72087),(#72088,#72089),(#72090,#72091),(#72092,#72093),(#72094,
#72095),(#72096,#72097),(#72098,#72099),(#72100,#72101),(#72102,#72103),
(#72104,#72105),(#72106,#72107),(#72108,#72109),(#72110,#72111),(#72112,
#72113),(#72114,#72115),(#72116,#72117),(#72118,#72119),(#72120,#72121),
(#72122,#72123),(#72124,#72125),(#72126,#72127),(#72128,#72129),(#72130,
#72131),(#72132,#72133),(#72134,#72135),(#72136,#72137),(#72138,#72139),
(#72140,#72141),(#72142,#72143),(#72144,#72145),(#72146,#72147),(#72148,
#72149),(#72150,#72151),(#72152,#72153),(#72154,#72155),(#72156,#72157),
(#72158,#72159),(#72160,#72161),(#72162,#72163),(#72164,#72165),(#72166,
#72167),(#72168,#72169),(#72170,#72171),(#72172,#72173),(#72174,#72175),
(#72176,#72177),(#72178,#72179),(#72180,#72181),(#72182,#72183),(#72184,
#72185),(#72186,#72187),(#72188,#72189),(#72190,#72191),(#72192,#72193),
(#72194,#72195),(#72196,#72197),(#72198,#72199),(#72200,#72201),(#72202,
#72203),(#72204,#72205),(#72206,#72207),(#72208,#72209),(#72210,#72211),
(#72212,#72213),(#72214,#72215),(#72216,#72217),(#72218,#72219),(#72220,
#72221),(#72222,#72223),(#72224,#72225),(#72226,#72227),(#72228,#72229),
(#72230,#72231),(#72232,#72233),(#72234,#72235),(#72236,#72237),(#72238,
#72239),(#72240,#72241),(#72242,#72243),(#72244,#72245),(#72246,#72247),
(#72248,#72249),(#72250,#72251),(#72252,#72253),(#72254,#72255),(#72256,
#72257),(#72258,#72259),(#72260,#72261),(#72262,#72263),(#72264,#72265),
(#72266,#72267),(#72268,#72269),(#72270,#72271),(#72272,#72273),(#72274,
#72275),(#72276,#72277),(#72278,#72279),(#72280,#72281),(#72282,#72283),
(#72284,#72285),(#72286,#72287),(#72288,#72289),(#72290,#72291),(#72292,
#72293),(#72294,#72295),(#72296,#72297),(#72298,#72299),(#72300,#72301),
(#72302,#72303),(#72304,#72305),(#72306,#72307),(#72308,#72309),(#72310,
#72311),(#72312,#72313),(#72314,#72315),(#72316,#72317),(#72318,#72319),
(#72320,#72321),(#72322,#72323),(#72324,#72325),(#72326,#72327),(#72328,
#72329),(#72330,#72331),(#72332,#72333),(#72334,#72335),(#72336,#72337),
(#72338,#72339),(#72340,#72341),(#72342,#72343),(#72344,#72345),(#72346,
#72347),(#72348,#72349),(#72350,#72351),(#72352,#72353),(#72354,#72355),
(#72356,#72357),(#72358,#72359),(#72360,#72361),(#72362,#72363),(#72364,
#72365),(#72366,#72367),(#72368,#72369),(#72370,#72371),(#72372,#72373),
(#72374,#72375),(#72376,#72377),(#72378,#72379),(#72380,#72381),(#72382,
#72383),(#72384,#72385),(#72386,#72387),(#72388,#72389),(#72390,#72391),
(#72392,#72393),(#72394,#72395),(#72396,#72397),(#72398,#72399),(#72400,
#72401),(#72402,#72403),(#72404,#72405),(#72406,#72407),(#72408,#72409),
(#72410,#72411),(#72412,#72413),(#72414,#72415),(#72416,#72417),(#72418,
#72419),(#72420,#72421),(#72422,#72423),(#72424,#72425),(#72426,#72427),
(#72428,#72429),(#72430,#72431),(#72432,#72433),(#72434,#72435),(#72436,
#72437),(#72438,#72439),(#72440,#72441),(#72442,#72443),(#72444,#72445),
(#72446,#72447),(#72448,#72449),(#72450,#72451),(#72452,#72453),(#72454,
#72455),(#72456,#72457),(#72458,#72459),(#72460,#72461),(#72462,#72463),
(#72464,#72465),(#72466,#72467),(#72468,#72469),(#72470,#72471),(#72472,
#72473),(#72474,#72475),(#72476,#72477),(#72478,#72479),(#72480,#72481),
(#72482,#72483),(#72484,#72485),(#72486,#72487),(#72488,#72489),(#72490,
#72491),(#72492,#72493),(#72494,#72495),(#72496,#72497),(#72498,#72499),
(#72500,#72501),(#72502,#72503),(#72504,#72505),(#72506,#72507),(#72508,
#72509),(#72510,#72511),(#72512,#72513),(#72514,#72515),(#72516,#72517),
(#72518,#72519),(#72520,#72521),(#72522,#72523),(#72524,#72525),(#72526,
#72527),(#72528,#72529),(#72530,#72531),(#72532,#72533),(#72534,#72535),
(#72536,#72537),(#72538,#72539),(#72540,#72541),(#72542,#72543),(#72544,
#72545),(#72546,#72547),(#72548,#72549),(#72550,#72551),(#72552,#72553),
(#72554,#72555),(#72556,#72557),(#72558,#72559),(#72560,#72561),(#72562,
#72563),(#72564,#72565),(#72566,#72567),(#72568,#72569),(#72570,#72571),
(#72572,#72573),(#72574,#72575),(#72576,#72577),(#72578,#72579),(#72580,
#72581),(#72582,#72583),(#72584,#72585),(#72586,#72587),(#72588,#72589),
(#72590,#72591),(#72592,#72593),(#72594,#72595),(#72596,#72597),(#72598,
#72599),(#72600,#72601),(#72602,#72603),(#72604,#72605),(#72606,#72607),
(#72608,#72609),(#72610,#72611),(#72612,#72613),(#72614,#72615),(#72616,
#72617),(#72618,#72619),(#72620,#72621),(#72622,#72623),(#72624,#72625),
(#72626,#72627),(#72628,#72629),(#72630,#72631),(#72632,#72633),(#72634,
#72635),(#72636,#72637),(#72638,#72639),(#72640,#72641),(#72642,#72643),
(#72644,#72645),(#72646,#72647),(#72648,#72649),(#72650,#72651),(#72652,
#72653),(#72654,#72655),(#72656,#72657),(#72658,#72659),(#72660,#72661),
(#72662,#72663),(#72664,#72665),(#72666,#72667),(#72668,#72669),(#72670,
#72671),(#72672,#72673),(#72674,#72675),(#72676,#72677),(#72678,#72679),
(#72680,#72681),(#72682,#72683),(#72684,#72685),(#72686,#72687),(#72688,
#72689),(#72690,#72691),(#72692,#72693),(#72694,#72695),(#72696,#72697),
(#72698,#72699),(#72700,#72701),(#72702,#72703),(#72704,#72705),(#72706,
#72707),(#72708,#72709),(#72710,#72711),(#72712,#72713),(#72714,#72715),
(#72716,#72717),(#72718,#72719),(#72720,#72721),(#72722,#72723),(#72724,
#72725),(#72726,#72727),(#72728,#72729),(#72730,#72731),(#72732,#72733),
(#72734,#72735),(#72736,#72737),(#72738,#72739),(#72740,#72741),(#72742,
#72743),(#72744,#72745),(#72746,#72747),(#72748,#72749),(#72750,#72751),
(#72752,#72753),(#72754,#72755),(#72756,#72757),(#72758,#72759),(#72760,
#72761),(#72762,#72763),(#72764,#72765),(#72766,#72767),(#72768,#72769),
(#72770,#72771),(#72772,#72773),(#72774,#72775),(#72776,#72777),(#72778,
#72779),(#72780,#72781),(#72782,#72783),(#72784,#72785),(#72786,#72787),
(#72788,#72789),(#72790,#72791),(#72792,#72793),(#72794,#72795),(#72796,
#72797),(#72798,#72799),(#72800,#72801),(#72802,#72803),(#72804,#72805),
(#72806,#72807),(#72808,#72809),(#72810,#72811),(#72812,#72813),(#72814,
#72815),(#72816,#72817),(#72818,#72819),(#72820,#72821),(#72822,#72823),
(#72824,#72825),(#72826,#72827),(#72828,#72829),(#72830,#72831),(#72832,
#72833),(#72834,#72835),(#72836,#72837),(#72838,#72839),(#72840,#72841),
(#72842,#72843),(#72844,#72845),(#72846,#72847),(#72848,#72849),(#72850,
#72851),(#72852,#72853),(#72854,#72855),(#72856,#72857),(#72858,#72859),
(#72860,#72861),(#72862,#72863),(#72864,#72865),(#72866,#72867),(#72868,
#72869),(#72870,#72871),(#72872,#72873),(#72874,#72875),(#72876,#72877),
(#72878,#72879),(#72880,#72881),(#72882,#72883),(#72884,#72885),(#72886,
#72887),(#72888,#72889),(#72890,#72891),(#72892,#72893),(#72894,#72895),
(#72896,#72897),(#72898,#72899),(#72900,#72901),(#72902,#72903),(#72904,
#72905),(#72906,#72907),(#72908,#72909),(#72910,#72911),(#72912,#72913),
(#72914,#72915),(#72916,#72917),(#72918,#72919),(#72920,#72921),(#72922,
#72923),(#72924,#72925),(#72926,#72927),(#72928,#72929),(#72930,#72931),
(#72932,#72933),(#72934,#72935),(#72936,#72937),(#72938,#72939),(#72940,
#72941),(#72942,#72943),(#72944,#72945),(#72946,#72947),(#72948,#72949),
(#72950,#72951),(#72952,#72953),(#72954,#72955),(#72956,#72957),(#72958,
#72959),(#72960,#72961),(#72962,#72963),(#72964,#72965),(#72966,#72967),
(#72968,#72969),(#72970,#72971),(#72972,#72973),(#72974,#72975),(#72976,
#72977),(#72978,#72979),(#72980,#72981),(#72982,#72983),(#72984,#72985),
(#72986,#72987),(#72988,#72989),(#72990,#72991),(#72992,#72993),(#72994,
#72995),(#72996,#72997),(#72998,#72999),(#73000,#73001),(#73002,#73003),
(#73004,#73005),(#73006,#73007),(#73008,#73009),(#73010,#73011),(#73012,
#73013),(#73014,#73015),(#73016,#73017),(#73018,#73019),(#73020,#73021),
(#73022,#73023),(#73024,#73025),(#73026,#73027),(#73028,#73029),(#73030,
#73031),(#73032,#73033),(#73034,#73035),(#73036,#73037),(#73038,#73039),
(#73040,#73041),(#73042,#73043),(#73044,#73045),(#73046,#73047),(#73048,
#73049),(#73050,#73051),(#73052,#73053),(#73054,#73055),(#73056,#73057),
(#73058,#73059),(#73060,#73061),(#73062,#73063),(#73064,#73065),(#73066,
#73067),(#73068,#73069),(#73070,#73071),(#73072,#73073),(#73074,#73075),
(#73076,#73077),(#73078,#73079),(#73080,#73081),(#73082,#73083),(#73084,
#73085),(#73086,#73087),(#73088,#73089),(#73090,#73091),(#73092,#73093),
(#73094,#73095),(#73096,#73097),(#73098,#73099),(#73100,#73101),(#73102,
#73103),(#73104,#73105),(#73106,#73107),(#73108,#73109),(#73110,#73111),
(#73112,#73113),(#73114,#73115),(#73116,#73117),(#73118,#73119),(#73120,
#73121),(#73122,#73123),(#73124,#73125),(#73126,#73127),(#73128,#73129),
(#73130,#73131),(#73132,#73133),(#73134,#73135),(#73136,#73137),(#73138,
#73139),(#73140,#73141),(#73142,#73143),(#73144,#73145),(#73146,#73147),
(#73148,#73149),(#73150,#73151),(#73152,#73153),(#73154,#73155),(#73156,
#73157),(#73158,#73159),(#73160,#73161),(#73162,#73163),(#73164,#73165),
(#73166,#73167),(#73168,#73169),(#73170,#73171),(#73172,#73173),(#73174,
#73175),(#73176,#73177),(#73178,#73179),(#73180,#73181),(#73182,#73183),
(#73184,#73185),(#73186,#73187),(#73188,#73189),(#73190,#73191),(#73192,
#73193),(#73194,#73195),(#73196,#73197),(#73198,#73199),(#73200,#73201),
(#73202,#73203),(#73204,#73205),(#73206,#73207),(#73208,#73209),(#73210,
#73211),(#73212,#73213),(#73214,#73215),(#73216,#73217),(#73218,#73219),
(#73220,#73221),(#73222,#73223),(#73224,#73225),(#73226,#73227),(#73228,
#73229),(#73230,#73231),(#73232,#73233),(#73234,#73235),(#73236,#73237),
(#73238,#73239),(#73240,#73241),(#73242,#73243),(#73244,#73245),(#73246,
#73247),(#73248,#73249),(#73250,#73251),(#73252,#73253),(#73254,#73255),
(#73256,#73257),(#73258,#73259),(#73260,#73261),(#73262,#73263),(#73264,
#73265),(#73266,#73267),(#73268,#73269),(#73270,#73271),(#73272,#73273),
(#73274,#73275),(#73276,#73277),(#73278,#73279),(#73280,#73281),(#73282,
#73283),(#73284,#73285),(#73286,#73287),(#73288,#73289),(#73290,#73291),
(#73292,#73293),(#73294,#73295),(#73296,#73297),(#73298,#73299),(#73300,
#73301),(#73302,#73303),(#73304,#73305),(#73306,#73307),(#73308,#73309),
(#73310,#73311),(#73312,#73313),(#73314,#73315),(#73316,#73317),(#73318,
#73319),(#73320,#73321),(#73322,#73323),(#73324,#73325),(#73326,#73327),
(#73328,#73329),(#73330,#73331),(#73332,#73333),(#73334,#73335),(#73336,
#73337),(#73338,#73339),(#73340,#73341),(#73342,#73343),(#73344,#73345),
(#73346,#73347),(#73348,#73349),(#73350,#73351),(#73352,#73353),(#73354,
#73355),(#73356,#73357),(#73358,#73359),(#73360,#73361),(#73362,#73363),
(#73364,#73365),(#73366,#73367),(#73368,#73369),(#73370,#73371),(#73372,
#73373),(#73374,#73375),(#73376,#73377),(#73378,#73379),(#73380,#73381),
(#73382,#73383),(#73384,#73385),(#73386,#73387),(#73388,#73389),(#73390,
#73391),(#73392,#73393),(#73394,#73395),(#73396,#73397),(#73398,#73399),
(#73400,#73401),(#73402,#73403),(#73404,#73405),(#73406,#73407),(#73408,
#73409),(#73410,#73411),(#73412,#73413),(#73414,#73415),(#73416,#73417),
(#73418,#73419),(#73420,#73421),(#73422,#73423),(#73424,#73425),(#73426,
#73427),(#73428,#73429),(#73430,#73431),(#73432,#73433),(#73434,#73435),
(#73436,#73437),(#73438,#73439),(#73440,#73441),(#73442,#73443),(#73444,
#73445),(#73446,#73447),(#73448,#73449),(#73450,#73451),(#73452,#73453),
(#73454,#73455),(#73456,#73457),(#73458,#73459),(#73460,#73461),(#73462,
#73463),(#73464,#73465),(#73466,#73467),(#73468,#73469),(#73470,#73471),
(#73472,#73473),(#73474,#73475),(#73476,#73477),(#73478,#73479),(#73480,
#73481),(#73482,#73483),(#73484,#73485),(#73486,#73487),(#73488,#73489),
(#73490,#73491),(#73492,#73493),(#73494,#73495),(#73496,#73497),(#73498,
#73499),(#73500,#73501),(#73502,#73503),(#73504,#73505),(#73506,#73507),
(#73508,#73509),(#73510,#73511),(#73512,#73513),(#73514,#73515),(#73516,
#73517),(#73518,#73519),(#73520,#73521),(#73522,#73523),(#73524,#73525),
(#73526,#73527),(#73528,#73529),(#73530,#73531),(#73532,#73533),(#73534,
#73535),(#73536,#73537),(#73538,#73539),(#73540,#73541),(#73542,#73543),
(#73544,#73545),(#73546,#73547),(#73548,#73549),(#73550,#73551),(#73552,
#73553),(#73554,#73555),(#73556,#73557),(#73558,#73559),(#73560,#73561),
(#73562,#73563),(#73564,#73565),(#73566,#73567),(#73568,#73569),(#73570,
#73571),(#73572,#73573),(#73574,#73575),(#73576,#73577),(#73578,#73579),
(#73580,#73581),(#73582,#73583),(#73584,#73585),(#73586,#73587),(#73588,
#73589),(#73590,#73591),(#73592,#73593),(#73594,#73595),(#73596,#73597),
(#73598,#73599),(#73600,#73601),(#73602,#73603),(#73604,#73605),(#73606,
#73607),(#73608,#73609),(#73610,#73611),(#73612,#73613),(#73614,#73615),
(#73616,#73617),(#73618,#73619),(#73620,#73621),(#73622,#73623),(#73624,
#73625),(#73626,#73627),(#73628,#73629),(#73630,#73631),(#73632,#73633),
(#73634,#73635),(#73636,#73637),(#73638,#73639),(#73640,#73641),(#73642,
#73643),(#73644,#73645),(#73646,#73647),(#73648,#73649),(#73650,#73651),
(#73652,#73653),(#73654,#73655),(#73656,#73657),(#73658,#73659),(#73660,
#73661),(#73662,#73663),(#73664,#73665),(#73666,#73667),(#73668,#73669),
(#73670,#73671),(#73672,#73673),(#73674,#73675),(#73676,#73677),(#73678,
#73679),(#73680,#73681),(#73682,#73683),(#73684,#73685),(#73686,#73687),
(#73688,#73689),(#73690,#73691),(#73692,#73693),(#73694,#73695),(#73696,
#73697),(#73698,#73699),(#73700,#73701),(#73702,#73703),(#73704,#73705),
(#73706,#73707),(#73708,#73709),(#73710,#73711),(#73712,#73713),(#73714,
#73715),(#73716,#73717),(#73718,#73719),(#73720,#73721),(#73722,#73723),
(#73724,#73725),(#73726,#73727),(#73728,#73729),(#73730,#73731),(#73732,
#73733),(#73734,#73735),(#73736,#73737),(#73738,#73739),(#73740,#73741),
(#73742,#73743),(#73744,#73745),(#73746,#73747),(#73748,#73749),(#73750,
#73751),(#73752,#73753),(#73754,#73755),(#73756,#73757),(#73758,#73759),
(#73760,#73761),(#73762,#73763),(#73764,#73765),(#73766,#73767),(#73768,
#73769),(#73770,#73771),(#73772,#73773),(#73774,#73775),(#73776,#73777),
(#73778,#73779),(#73780,#73781),(#73782,#73783),(#73784,#73785),(#73786,
#73787),(#73788,#73789),(#73790,#73791),(#73792,#73793),(#73794,#73795),
(#73796,#73797),(#73798,#73799),(#73800,#73801),(#73802,#73803),(#73804,
#73805),(#73806,#73807),(#73808,#73809),(#73810,#73811),(#73812,#73813),
(#73814,#73815),(#73816,#73817),(#73818,#73819),(#73820,#73821),(#73822,
#73823),(#73824,#73825),(#73826,#73827),(#73828,#73829),(#73830,#73831),
(#73832,#73833),(#73834,#73835),(#73836,#73837),(#73838,#73839),(#73840,
#73841),(#73842,#73843),(#73844,#73845),(#73846,#73847),(#73848,#73849),
(#73850,#73851),(#73852,#73853),(#73854,#73855),(#73856,#73857),(#73858,
#73859),(#73860,#73861),(#73862,#73863),(#73864,#73865),(#73866,#73867),
(#73868,#73869),(#73870,#73871),(#73872,#73873),(#73874,#73875),(#73876,
#73877),(#73878,#73879),(#73880,#73881),(#73882,#73883),(#73884,#73885),
(#73886,#73887),(#73888,#73889),(#73890,#73891),(#73892,#73893),(#73894,
#73895),(#73896,#73897),(#73898,#73899),(#73900,#73901),(#73902,#73903),
(#73904,#73905),(#73906,#73907),(#73908,#73909),(#73910,#73911),(#73912,
#73913),(#73914,#73915),(#73916,#73917),(#73918,#73919),(#73920,#73921),
(#73922,#73923),(#73924,#73925),(#73926,#73927),(#73928,#73929),(#73930,
#73931),(#73932,#73933),(#73934,#73935),(#73936,#73937),(#73938,#73939),
(#73940,#73941),(#73942,#73943),(#73944,#73945),(#73946,#73947),(#73948,
#73949),(#73950,#73951),(#73952,#73953),(#73954,#73955),(#73956,#73957),
(#73958,#73959),(#73960,#73961),(#73962,#73963),(#73964,#73965),(#73966,
#73967),(#73968,#73969),(#73970,#73971),(#73972,#73973),(#73974,#73975),
(#73976,#73977),(#73978,#73979),(#73980,#73981),(#73982,#73983),(#73984,
#73985),(#73986,#73987),(#73988,#73989),(#73990,#73991),(#73992,#73993),
(#73994,#73995),(#73996,#73997),(#73998,#73999),(#74000,#74001),(#74002,
#74003),(#74004,#74005),(#74006,#74007),(#74008,#74009),(#74010,#74011),
(#74012,#74013),(#74014,#74015),(#74016,#74017),(#74018,#74019),(#74020,
#74021),(#74022,#74023),(#74024,#74025),(#74026,#74027),(#74028,#74029),
(#74030,#74031),(#74032,#74033),(#74034,#74035),(#74036,#74037),(#74038,
#74039),(#74040,#74041),(#74042,#74043),(#74044,#74045),(#74046,#74047),
(#74048,#74049),(#74050,#74051),(#74052,#74053),(#74054,#74055),(#74056,
#74057),(#74058,#74059),(#74060,#74061),(#74062,#74063),(#74064,#74065),
(#74066,#74067),(#74068,#74069),(#74070,#74071),(#74072,#74073),(#74074,
#74075),(#74076,#74077),(#74078,#74079),(#74080,#74081),(#74082,#74083),
(#74084,#74085),(#74086,#74087),(#74088,#74089),(#74090,#74091),(#74092,
#74093),(#74094,#74095),(#74096,#74097),(#74098,#74099),(#74100,#74101),
(#74102,#74103),(#74104,#74105),(#74106,#74107),(#74108,#74109),(#74110,
#74111),(#74112,#74113),(#74114,#74115),(#74116,#74117),(#74118,#74119),
(#74120,#74121),(#74122,#74123),(#74124,#74125),(#74126,#74127),(#74128,
#74129),(#74130,#74131),(#74132,#74133),(#74134,#74135),(#74136,#74137),
(#74138,#74139),(#74140,#74141),(#74142,#74143),(#74144,#74145),(#74146,
#74147),(#74148,#74149),(#74150,#74151),(#74152,#74153),(#74154,#74155),
(#74156,#74157),(#74158,#74159),(#74160,#74161),(#74162,#74163),(#74164,
#74165),(#74166,#74167),(#74168,#74169),(#74170,#74171),(#74172,#74173),
(#74174,#74175),(#74176,#74177),(#74178,#74179),(#74180,#74181),(#74182,
#74183),(#74184,#74185),(#74186,#74187),(#74188,#74189),(#74190,#74191),
(#74192,#74193),(#74194,#74195),(#74196,#74197),(#74198,#74199),(#74200,
#74201),(#74202,#74203),(#74204,#74205),(#74206,#74207),(#74208,#74209),
(#74210,#74211),(#74212,#74213),(#74214,#74215),(#74216,#74217),(#74218,
#74219),(#74220,#74221),(#74222,#74223),(#74224,#74225),(#74226,#74227),
(#74228,#74229),(#74230,#74231),(#74232,#74233),(#74234,#74235),(#74236,
#74237),(#74238,#74239),(#74240,#74241),(#74242,#74243),(#74244,#74245),
(#74246,#74247),(#74248,#74249),(#74250,#74251),(#74252,#74253),(#74254,
#74255),(#74256,#74257),(#74258,#74259),(#74260,#74261),(#74262,#74263),
(#74264,#74265),(#74266,#74267),(#74268,#74269),(#74270,#74271),(#74272,
#74273),(#74274,#74275),(#74276,#74277),(#74278,#74279),(#74280,#74281),
(#74282,#74283),(#74284,#74285),(#74286,#74287),(#74288,#74289),(#74290,
#74291),(#74292,#74293),(#74294,#74295),(#74296,#74297),(#74298,#74299),
(#74300,#74301),(#74302,#74303),(#74304,#74305),(#74306,#74307),(#74308,
#74309),(#74310,#74311),(#74312,#74313),(#74314,#74315),(#74316,#74317),
(#74318,#74319),(#74320,#74321),(#74322,#74323),(#74324,#74325),(#74326,
#74327),(#74328,#74329),(#74330,#74331),(#74332,#74333),(#74334,#74335),
(#74336,#74337),(#74338,#74339),(#74340,#74341),(#74342,#74343),(#74344,
#74345),(#74346,#74347),(#74348,#74349),(#74350,#74351),(#74352,#74353),
(#74354,#74355),(#74356,#74357),(#74358,#74359),(#74360,#74361),(#74362,
#74363),(#74364,#74365),(#74366,#74367),(#74368,#74369),(#74370,#74371),
(#74372,#74373),(#74374,#74375),(#74376,#74377),(#74378,#74379),(#74380,
#74381),(#74382,#74383),(#74384,#74385),(#74386,#74387),(#74388,#74389),
(#74390,#74391),(#74392,#74393),(#74394,#74395),(#74396,#74397),(#74398,
#74399),(#74400,#74401),(#74402,#74403),(#74404,#74405),(#74406,#74407),
(#74408,#74409),(#74410,#74411),(#74412,#74413),(#74414,#74415),(#74416,
#74417),(#74418,#74419),(#74420,#74421),(#74422,#74423),(#74424,#74425),
(#74426,#74427),(#74428,#74429),(#74430,#74431),(#74432,#74433),(#74434,
#74435),(#74436,#74437),(#74438,#74439),(#74440,#74441),(#74442,#74443),
(#74444,#74445),(#74446,#74447),(#74448,#74449),(#74450,#74451),(#74452,
#74453),(#74454,#74455),(#74456,#74457),(#74458,#74459),(#74460,#74461),
(#74462,#74463),(#74464,#74465),(#74466,#74467),(#74468,#74469),(#74470,
#74471),(#74472,#74473),(#74474,#74475),(#74476,#74477),(#74478,#74479),
(#74480,#74481),(#74482,#74483),(#74484,#74485),(#74486,#74487),(#74488,
#74489),(#74490,#74491),(#74492,#74493),(#74494,#74495),(#74496,#74497),
(#74498,#74499),(#74500,#74501),(#74502,#74503),(#74504,#74505),(#74506,
#74507),(#74508,#74509),(#74510,#74511),(#74512,#74513),(#74514,#74515),
(#74516,#74517),(#74518,#74519),(#74520,#74521),(#74522,#74523),(#74524,
#74525),(#74526,#74527),(#74528,#74529),(#74530,#74531),(#74532,#74533),
(#74534,#74535),(#74536,#74537),(#74538,#74539),(#74540,#74541),(#74542,
#74543),(#74544,#74545),(#74546,#74547),(#74548,#74549),(#74550,#74551),
(#74552,#74553),(#74554,#74555),(#74556,#74557),(#74558,#74559),(#74560,
#74561),(#74562,#74563),(#74564,#74565),(#74566,#74567),(#74568,#74569),
(#74570,#74571),(#74572,#74573),(#74574,#74575),(#74576,#74577),(#74578,
#74579),(#74580,#74581),(#74582,#74583),(#74584,#74585),(#74586,#74587),
(#74588,#74589),(#74590,#74591),(#74592,#74593),(#74594,#74595),(#74596,
#74597),(#74598,#74599),(#74600,#74601),(#74602,#74603),(#74604,#74605),
(#74606,#74607),(#74608,#74609),(#74610,#74611),(#74612,#74613),(#74614,
#74615),(#74616,#74617),(#74618,#74619),(#74620,#74621),(#74622,#74623),
(#74624,#74625),(#74626,#74627),(#74628,#74629),(#74630,#74631),(#74632,
#74633),(#74634,#74635),(#74636,#74637),(#74638,#74639),(#74640,#74641),
(#74642,#74643),(#74644,#74645),(#74646,#74647),(#74648,#74649),(#74650,
#74651),(#74652,#74653),(#74654,#74655),(#74656,#74657),(#74658,#74659),
(#74660,#74661),(#74662,#74663),(#74664,#74665),(#74666,#74667),(#74668,
#74669),(#74670,#74671),(#74672,#74673),(#74674,#74675),(#74676,#74677),
(#74678,#74679),(#74680,#74681),(#74682,#74683),(#74684,#74685),(#74686,
#74687),(#74688,#74689),(#74690,#74691),(#74692,#74693),(#74694,#74695),
(#74696,#74697),(#74698,#74699),(#74700,#74701),(#74702,#74703),(#74704,
#74705),(#74706,#74707),(#74708,#74709),(#74710,#74711),(#74712,#74713),
(#74714,#74715),(#74716,#74717),(#74718,#74719),(#74720,#74721),(#74722,
#74723),(#74724,#74725),(#74726,#74727),(#74728,#74729),(#74730,#74731),
(#74732,#74733),(#74734,#74735),(#74736,#74737),(#74738,#74739),(#74740,
#74741),(#74742,#74743),(#74744,#74745),(#74746,#74747),(#74748,#74749),
(#74750,#74751),(#74752,#74753),(#74754,#74755),(#74756,#74757),(#74758,
#74759),(#74760,#74761),(#74762,#74763),(#74764,#74765),(#74766,#74767),
(#74768,#74769),(#74770,#74771),(#74772,#74773),(#74774,#74775),(#74776,
#74777),(#74778,#74779),(#74780,#74781),(#74782,#74783),(#74784,#74785),
(#74786,#74787),(#74788,#74789),(#74790,#74791),(#74792,#74793),(#74794,
#74795),(#74796,#74797),(#74798,#74799),(#74800,#74801),(#74802,#74803),
(#74804,#74805),(#74806,#74807),(#74808,#74809),(#74810,#74811),(#74812,
#74813),(#74814,#74815),(#74816,#74817),(#74818,#74819),(#74820,#74821),
(#74822,#74823),(#74824,#74825),(#74826,#74827),(#74828,#74829),(#74830,
#74831),(#74832,#74833),(#74834,#74835),(#74836,#74837),(#74838,#74839),
(#74840,#74841),(#74842,#74843),(#74844,#74845),(#74846,#74847),(#74848,
#74849),(#74850,#74851),(#74852,#74853),(#74854,#74855),(#74856,#74857),
(#74858,#74859),(#74860,#74861),(#74862,#74863),(#74864,#74865),(#74866,
#74867),(#74868,#74869),(#74870,#74871),(#74872,#74873),(#74874,#74875),
(#74876,#74877),(#74878,#74879),(#74880,#74881),(#74882,#74883),(#74884,
#74885),(#74886,#74887),(#74888,#74889),(#74890,#74891),(#74892,#74893),
(#74894,#74895),(#74896,#74897),(#74898,#74899),(#74900,#74901),(#74902,
#74903),(#74904,#74905),(#74906,#74907),(#74908,#74909),(#74910,#74911),
(#74912,#74913),(#74914,#74915),(#74916,#74917),(#74918,#74919),(#74920,
#74921),(#74922,#74923),(#74924,#74925),(#74926,#74927),(#74928,#74929),
(#74930,#74931),(#74932,#74933),(#74934,#74935),(#74936,#74937),(#74938,
#74939),(#74940,#74941),(#74942,#74943),(#74944,#74945),(#74946,#74947),
(#74948,#74949),(#74950,#74951),(#74952,#74953),(#74954,#74955),(#74956,
#74957),(#74958,#74959),(#74960,#74961),(#74962,#74963),(#74964,#74965),
(#74966,#74967),(#74968,#74969),(#74970,#74971),(#74972,#74973),(#74974,
#74975),(#74976,#74977),(#74978,#74979),(#74980,#74981),(#74982,#74983),
(#74984,#74985),(#74986,#74987),(#74988,#74989),(#74990,#74991),(#74992,
#74993),(#74994,#74995),(#74996,#74997),(#74998,#74999),(#75000,#75001),
(#75002,#75003),(#75004,#75005),(#75006,#75007),(#75008,#75009),(#75010,
#75011),(#75012,#75013),(#75014,#75015),(#75016,#75017),(#75018,#75019),
(#75020,#75021),(#75022,#75023),(#75024,#75025),(#75026,#75027),(#75028,
#75029),(#75030,#75031),(#75032,#75033),(#75034,#75035),(#75036,#75037),
(#75038,#75039),(#75040,#75041),(#75042,#75043),(#75044,#75045),(#75046,
#75047),(#75048,#75049),(#75050,#75051),(#75052,#75053),(#75054,#75055),
(#75056,#75057),(#75058,#75059),(#75060,#75061),(#75062,#75063),(#75064,
#75065),(#75066,#75067),(#75068,#75069),(#75070,#75071),(#75072,#75073),
(#75074,#75075),(#75076,#75077),(#75078,#75079),(#75080,#75081),(#75082,
#75083),(#75084,#75085),(#75086,#75087),(#75088,#75089),(#75090,#75091),
(#75092,#75093),(#75094,#75095),(#75096,#75097),(#75098,#75099),(#75100,
#75101),(#75102,#75103),(#75104,#75105),(#75106,#75107),(#75108,#75109),
(#75110,#75111),(#75112,#75113),(#75114,#75115),(#75116,#75117),(#75118,
#75119),(#75120,#75121),(#75122,#75123),(#75124,#75125),(#75126,#75127),
(#75128,#75129),(#75130,#75131),(#75132,#75133),(#75134,#75135),(#75136,
#75137),(#75138,#75139),(#75140,#75141),(#75142,#75143),(#75144,#75145),
(#75146,#75147),(#75148,#75149),(#75150,#75151),(#75152,#75153),(#75154,
#75155),(#75156,#75157),(#75158,#75159),(#75160,#75161),(#75162,#75163),
(#75164,#75165),(#75166,#75167),(#75168,#75169),(#75170,#75171),(#75172,
#75173),(#75174,#75175),(#75176,#75177),(#75178,#75179),(#75180,#75181),
(#75182,#75183),(#75184,#75185),(#75186,#75187),(#75188,#75189),(#75190,
#75191),(#75192,#75193),(#75194,#75195),(#75196,#75197),(#75198,#75199),
(#75200,#75201),(#75202,#75203),(#75204,#75205),(#75206,#75207),(#75208,
#75209),(#75210,#75211),(#75212,#75213),(#75214,#75215),(#75216,#75217),
(#75218,#75219),(#75220,#75221),(#75222,#75223),(#75224,#75225),(#75226,
#75227),(#75228,#75229),(#75230,#75231),(#75232,#75233),(#75234,#75235),
(#75236,#75237),(#75238,#75239),(#75240,#75241),(#75242,#75243),(#75244,
#75245),(#75246,#75247),(#75248,#75249),(#75250,#75251),(#75252,#75253),
(#75254,#75255),(#75256,#75257),(#75258,#75259),(#75260,#75261),(#75262,
#75263),(#75264,#75265),(#75266,#75267),(#75268,#75269),(#75270,#75271),
(#75272,#75273),(#75274,#75275),(#75276,#75277),(#75278,#75279),(#75280,
#75281),(#75282,#75283),(#75284,#75285),(#75286,#75287),(#75288,#75289),
(#75290,#75291),(#75292,#75293),(#75294,#75295),(#75296,#75297),(#75298,
#75299),(#75300,#75301),(#75302,#75303),(#75304,#75305),(#75306,#75307),
(#75308,#75309),(#75310,#75311),(#75312,#75313),(#75314,#75315),(#75316,
#75317),(#75318,#75319),(#75320,#75321),(#75322,#75323),(#75324,#75325),
(#75326,#75327),(#75328,#75329),(#75330,#75331),(#75332,#75333),(#75334,
#75335),(#75336,#75337),(#75338,#75339),(#75340,#75341),(#75342,#75343),
(#75344,#75345),(#75346,#75347),(#75348,#75349),(#75350,#75351),(#75352,
#75353),(#75354,#75355),(#75356,#75357),(#75358,#75359),(#75360,#75361),
(#75362,#75363),(#75364,#75365),(#75366,#75367),(#75368,#75369),(#75370,
#75371),(#75372,#75373),(#75374,#75375),(#75376,#75377),(#75378,#75379),
(#75380,#75381),(#75382,#75383),(#75384,#75385),(#75386,#75387),(#75388,
#75389),(#75390,#75391),(#75392,#75393),(#75394,#75395),(#75396,#75397),
(#75398,#75399),(#75400,#75401),(#75402,#75403),(#75404,#75405),(#75406,
#75407),(#75408,#75409),(#75410,#75411),(#75412,#75413),(#75414,#75415),
(#75416,#75417),(#75418,#75419),(#75420,#75421),(#75422,#75423),(#75424,
#75425),(#75426,#75427),(#75428,#75429),(#75430,#75431),(#75432,#75433),
(#75434,#75435),(#75436,#75437),(#75438,#75439),(#75440,#75441),(#75442,
#75443),(#75444,#75445),(#75446,#75447),(#75448,#75449),(#75450,#75451),
(#75452,#75453),(#75454,#75455),(#75456,#75457),(#75458,#75459),(#75460,
#75461),(#75462,#75463),(#75464,#75465),(#75466,#75467),(#75468,#75469),
(#75470,#75471),(#75472,#75473),(#75474,#75475),(#75476,#75477),(#75478,
#75479),(#75480,#75481),(#75482,#75483),(#75484,#75485),(#75486,#75487),
(#75488,#75489),(#75490,#75491),(#75492,#75493),(#75494,#75495),(#75496,
#75497),(#75498,#75499),(#75500,#75501),(#75502,#75503),(#75504,#75505),
(#75506,#75507),(#75508,#75509),(#75510,#75511),(#75512,#75513),(#75514,
#75515),(#75516,#75517),(#75518,#75519),(#75520,#75521),(#75522,#75523),
(#75524,#75525),(#75526,#75527),(#75528,#75529),(#75530,#75531),(#75532,
#75533),(#75534,#75535),(#75536,#75537),(#75538,#75539),(#75540,#75541),
(#75542,#75543),(#75544,#75545),(#75546,#75547),(#75548,#75549),(#75550,
#75551),(#75552,#75553),(#75554,#75555),(#75556,#75557),(#75558,#75559),
(#75560,#75561),(#75562,#75563),(#75564,#75565),(#75566,#75567),(#75568,
#75569),(#75570,#75571),(#75572,#75573),(#75574,#75575),(#75576,#75577),
(#75578,#75579),(#75580,#75581),(#75582,#75583),(#75584,#75585),(#75586,
#75587),(#75588,#75589),(#75590,#75591),(#75592,#75593),(#75594,#75595),
(#75596,#75597),(#75598,#75599),(#75600,#75601),(#75602,#75603),(#75604,
#75605),(#75606,#75607),(#75608,#75609),(#75610,#75611),(#75612,#75613),
(#75614,#75615),(#75616,#75617),(#75618,#75619),(#75620,#75621),(#75622,
#75623),(#75624,#75625),(#75626,#75627),(#75628,#75629),(#75630,#75631),
(#75632,#75633),(#75634,#75635),(#75636,#75637),(#75638,#75639),(#75640,
#75641),(#75642,#75643),(#75644,#75645),(#75646,#75647),(#75648,#75649),
(#75650,#75651),(#75652,#75653),(#75654,#75655),(#75656,#75657),(#75658,
#75659),(#75660,#75661),(#75662,#75663),(#75664,#75665),(#75666,#75667),
(#75668,#75669),(#75670,#75671),(#75672,#75673),(#75674,#75675),(#75676,
#75677),(#75678,#75679),(#75680,#75681),(#75682,#75683),(#75684,#75685),
(#75686,#75687),(#75688,#75689),(#75690,#75691),(#75692,#75693),(#75694,
#75695),(#75696,#75697),(#75698,#75699),(#75700,#75701),(#75702,#75703),
(#75704,#75705),(#75706,#75707),(#75708,#75709),(#75710,#75711),(#75712,
#75713),(#75714,#75715),(#75716,#75717),(#75718,#75719),(#75720,#75721),
(#75722,#75723),(#75724,#75725),(#75726,#75727),(#75728,#75729),(#75730,
#75731),(#75732,#75733),(#75734,#75735),(#75736,#75737),(#75738,#75739),
(#75740,#75741),(#75742,#75743),(#75744,#75745),(#75746,#75747),(#75748,
#75749),(#75750,#75751),(#75752,#75753),(#75754,#75755),(#75756,#75757),
(#75758,#75759),(#75760,#75761),(#75762,#75763),(#75764,#75765),(#75766,
#75767),(#75768,#75769),(#75770,#75771),(#75772,#75773),(#75774,#75775),
(#75776,#75777),(#75778,#75779),(#75780,#75781),(#75782,#75783),(#75784,
#75785),(#75786,#75787),(#75788,#75789),(#75790,#75791),(#75792,#75793),
(#75794,#75795),(#75796,#75797),(#75798,#75799),(#75800,#75801),(#75802,
#75803),(#75804,#75805),(#75806,#75807),(#75808,#75809),(#75810,#75811),
(#75812,#75813),(#75814,#75815),(#75816,#75817),(#75818,#75819),(#75820,
#75821),(#75822,#75823),(#75824,#75825),(#75826,#75827),(#75828,#75829),
(#75830,#75831),(#75832,#75833),(#75834,#75835),(#75836,#75837),(#75838,
#75839),(#75840,#75841),(#75842,#75843),(#75844,#75845),(#75846,#75847),
(#75848,#75849),(#75850,#75851),(#75852,#75853),(#75854,#75855),(#75856,
#75857),(#75858,#75859),(#75860,#75861),(#75862,#75863),(#75864,#75865),
(#75866,#75867),(#75868,#75869),(#75870,#75871),(#75872,#75873),(#75874,
#75875),(#75876,#75877),(#75878,#75879),(#75880,#75881),(#75882,#75883),
(#75884,#75885),(#75886,#75887),(#75888,#75889),(#75890,#75891),(#75892,
#75893),(#75894,#75895),(#75896,#75897),(#75898,#75899),(#75900,#75901),
(#75902,#75903),(#75904,#75905),(#75906,#75907),(#75908,#75909),(#75910,
#75911),(#75912,#75913),(#75914,#75915),(#75916,#75917),(#75918,#75919),
(#75920,#75921),(#75922,#75923),(#75924,#75925),(#75926,#75927),(#75928,
#75929),(#75930,#75931),(#75932,#75933),(#75934,#75935),(#75936,#75937),
(#75938,#75939),(#75940,#75941),(#75942,#75943),(#75944,#75945),(#75946,
#75947),(#75948,#75949),(#75950,#75951),(#75952,#75953),(#75954,#75955),
(#75956,#75957),(#75958,#75959),(#75960,#75961),(#75962,#75963),(#75964,
#75965),(#75966,#75967),(#75968,#75969),(#75970,#75971),(#75972,#75973),
(#75974,#75975),(#75976,#75977),(#75978,#75979),(#75980,#75981),(#75982,
#75983),(#75984,#75985),(#75986,#75987),(#75988,#75989),(#75990,#75991),
(#75992,#75993),(#75994,#75995),(#75996,#75997),(#75998,#75999),(#76000,
#76001),(#76002,#76003),(#76004,#76005),(#76006,#76007),(#76008,#76009),
(#76010,#76011),(#76012,#76013),(#76014,#76015),(#76016,#76017),(#76018,
#76019),(#76020,#76021),(#76022,#76023),(#76024,#76025),(#76026,#76027),
(#76028,#76029),(#76030,#76031),(#76032,#76033),(#76034,#76035),(#76036,
#76037),(#76038,#76039),(#76040,#76041),(#76042,#76043),(#76044,#76045),
(#76046,#76047),(#76048,#76049),(#76050,#76051),(#76052,#76053),(#76054,
#76055),(#76056,#76057),(#76058,#76059),(#76060,#76061),(#76062,#76063),
(#76064,#76065),(#76066,#76067),(#76068,#76069),(#76070,#76071),(#76072,
#76073),(#76074,#76075),(#76076,#76077),(#76078,#76079),(#76080,#76081),
(#76082,#76083),(#76084,#76085),(#76086,#76087),(#76088,#76089),(#76090,
#76091),(#76092,#76093),(#76094,#76095),(#76096,#76097),(#76098,#76099),
(#76100,#76101),(#76102,#76103),(#76104,#76105),(#76106,#76107),(#76108,
#76109),(#76110,#76111),(#76112,#76113),(#76114,#76115),(#76116,#76117),
(#76118,#76119),(#76120,#76121),(#76122,#76123),(#76124,#76125),(#76126,
#76127),(#76128,#76129),(#76130,#76131),(#76132,#76133),(#76134,#76135),
(#76136,#76137),(#76138,#76139),(#76140,#76141),(#76142,#76143),(#76144,
#76145),(#76146,#76147),(#76148,#76149),(#76150,#76151),(#76152,#76153),
(#76154,#76155),(#76156,#76157),(#76158,#76159),(#76160,#76161),(#76162,
#76163),(#76164,#76165),(#76166,#76167),(#76168,#76169),(#76170,#76171),
(#76172,#76173),(#76174,#76175),(#76176,#76177),(#76178,#76179),(#76180,
#76181),(#76182,#76183),(#76184,#76185),(#76186,#76187),(#76188,#76189),
(#76190,#76191),(#76192,#76193),(#76194,#76195),(#76196,#76197),(#76198,
#76199),(#76200,#76201),(#76202,#76203),(#76204,#76205),(#76206,#76207),
(#76208,#76209),(#76210,#76211),(#76212,#76213),(#76214,#76215),(#76216,
#76217),(#76218,#76219),(#76220,#76221),(#76222,#76223),(#76224,#76225),
(#76226,#76227),(#76228,#76229),(#76230,#76231),(#76232,#76233),(#76234,
#76235),(#76236,#76237),(#76238,#76239),(#76240,#76241),(#76242,#76243),
(#76244,#76245),(#76246,#76247),(#76248,#76249),(#76250,#76251),(#76252,
#76253),(#76254,#76255),(#76256,#76257),(#76258,#76259),(#76260,#76261),
(#76262,#76263),(#76264,#76265),(#76266,#76267),(#76268,#76269),(#76270,
#76271),(#76272,#76273),(#76274,#76275),(#76276,#76277),(#76278,#76279),
(#76280,#76281),(#76282,#76283),(#76284,#76285),(#76286,#76287),(#76288,
#76289),(#76290,#76291),(#76292,#76293),(#76294,#76295),(#76296,#76297),
(#76298,#76299),(#76300,#76301),(#76302,#76303),(#76304,#76305),(#76306,
#76307),(#76308,#76309),(#76310,#76311),(#76312,#76313),(#76314,#76315),
(#76316,#76317),(#76318,#76319),(#76320,#76321),(#76322,#76323),(#76324,
#76325),(#76326,#76327),(#76328,#76329),(#76330,#76331),(#76332,#76333),
(#76334,#76335),(#76336,#76337),(#76338,#76339),(#76340,#76341),(#76342,
#76343),(#76344,#76345),(#76346,#76347),(#76348,#76349),(#76350,#76351),
(#76352,#76353),(#76354,#76355),(#76356,#76357),(#76358,#76359),(#76360,
#76361),(#76362,#76363),(#76364,#76365),(#76366,#76367),(#76368,#76369),
(#76370,#76371),(#76372,#76373),(#76374,#76375),(#76376,#76377),(#76378,
#76379),(#76380,#76381),(#76382,#76383),(#76384,#76385),(#76386,#76387),
(#76388,#76389),(#76390,#76391),(#76392,#76393),(#76394,#76395),(#76396,
#76397),(#76398,#76399),(#76400,#76401),(#76402,#76403),(#76404,#76405),
(#76406,#76407),(#76408,#76409),(#76410,#76411),(#76412,#76413),(#76414,
#76415),(#76416,#76417),(#76418,#76419),(#76420,#76421),(#76422,#76423),
(#76424,#76425),(#76426,#76427),(#76428,#76429),(#76430,#76431),(#76432,
#76433),(#76434,#76435),(#76436,#76437),(#76438,#76439),(#76440,#76441),
(#76442,#76443),(#76444,#76445),(#76446,#76447),(#76448,#76449),(#76450,
#76451),(#76452,#76453),(#76454,#76455),(#76456,#76457),(#76458,#76459),
(#76460,#76461),(#76462,#76463),(#76464,#76465),(#76466,#76467),(#76468,
#76469),(#76470,#76471),(#76472,#76473),(#76474,#76475),(#76476,#76477),
(#76478,#76479),(#76480,#76481),(#76482,#76483),(#76484,#76485),(#76486,
#76487),(#76488,#76489),(#76490,#76491),(#76492,#76493),(#76494,#76495),
(#76496,#76497),(#76498,#76499),(#76500,#76501),(#76502,#76503),(#76504,
#76505),(#76506,#76507),(#76508,#76509),(#76510,#76511),(#76512,#76513),
(#76514,#76515),(#76516,#76517),(#76518,#76519),(#76520,#76521),(#76522,
#76523),(#76524,#76525),(#76526,#76527),(#76528,#76529),(#76530,#76531),
(#76532,#76533),(#76534,#76535),(#76536,#76537),(#76538,#76539),(#76540,
#76541),(#76542,#76543),(#76544,#76545),(#76546,#76547),(#76548,#76549),
(#76550,#76551),(#76552,#76553),(#76554,#76555),(#76556,#76557),(#76558,
#76559),(#76560,#76561),(#76562,#76563),(#76564,#76565),(#76566,#76567),
(#76568,#76569),(#76570,#76571),(#76572,#76573),(#76574,#76575),(#76576,
#76577),(#76578,#76579),(#76580,#76581),(#76582,#76583),(#76584,#76585),
(#76586,#76587),(#76588,#76589),(#76590,#76591),(#76592,#76593),(#76594,
#76595),(#76596,#76597),(#76598,#76599),(#76600,#76601),(#76602,#76603),
(#76604,#76605),(#76606,#76607),(#76608,#76609),(#76610,#76611),(#76612,
#76613),(#76614,#76615),(#76616,#76617),(#76618,#76619),(#76620,#76621),
(#76622,#76623),(#76624,#76625),(#76626,#76627),(#76628,#76629),(#76630,
#76631),(#76632,#76633),(#76634,#76635),(#76636,#76637),(#76638,#76639),
(#76640,#76641),(#76642,#76643),(#76644,#76645),(#76646,#76647),(#76648,
#76649),(#76650,#76651),(#76652,#76653),(#76654,#76655),(#76656,#76657),
(#76658,#76659),(#76660,#76661),(#76662,#76663),(#76664,#76665),(#76666,
#76667),(#76668,#76669),(#76670,#76671),(#76672,#76673),(#76674,#76675),
(#76676,#76677),(#76678,#76679),(#76680,#76681),(#76682,#76683),(#76684,
#76685),(#76686,#76687),(#76688,#76689),(#76690,#76691),(#76692,#76693),
(#76694,#76695),(#76696,#76697),(#76698,#76699),(#76700,#76701),(#76702,
#76703),(#76704,#76705),(#76706,#76707),(#76708,#76709),(#76710,#76711),
(#76712,#76713),(#76714,#76715),(#76716,#76717),(#76718,#76719),(#76720,
#76721),(#76722,#76723),(#76724,#76725),(#76726,#76727),(#76728,#76729),
(#76730,#76731),(#76732,#76733),(#76734,#76735),(#76736,#76737),(#76738,
#76739),(#76740,#76741),(#76742,#76743),(#76744,#76745),(#76746,#76747),
(#76748,#76749),(#76750,#76751),(#76752,#76753),(#76754,#76755),(#76756,
#76757),(#76758,#76759),(#76760,#76761),(#76762,#76763),(#76764,#76765),
(#76766,#76767),(#76768,#76769),(#76770,#76771),(#76772,#76773),(#76774,
#76775),(#76776,#76777),(#76778,#76779),(#76780,#76781),(#76782,#76783),
(#76784,#76785),(#76786,#76787),(#76788,#76789),(#76790,#76791),(#76792,
#76793),(#76794,#76795),(#76796,#76797),(#76798,#76799),(#76800,#76801),
(#76802,#76803),(#76804,#76805),(#76806,#76807),(#76808,#76809),(#76810,
#76811),(#76812,#76813),(#76814,#76815),(#76816,#76817),(#76818,#76819),
(#76820,#76821),(#76822,#76823),(#76824,#76825),(#76826,#76827),(#76828,
#76829),(#76830,#76831),(#76832,#76833),(#76834,#76835),(#76836,#76837),
(#76838,#76839),(#76840,#76841),(#76842,#76843),(#76844,#76845),(#76846,
#76847),(#76848,#76849),(#76850,#76851),(#76852,#76853),(#76854,#76855),
(#76856,#76857),(#76858,#76859),(#76860,#76861),(#76862,#76863),(#76864,
#76865),(#76866,#76867),(#76868,#76869),(#76870,#76871),(#76872,#76873),
(#76874,#76875),(#76876,#76877),(#76878,#76879),(#76880,#76881),(#76882,
#76883),(#76884,#76885),(#76886,#76887),(#76888,#76889),(#76890,#76891),
(#76892,#76893),(#76894,#76895),(#76896,#76897),(#76898,#76899),(#76900,
#76901),(#76902,#76903),(#76904,#76905),(#76906,#76907),(#76908,#76909),
(#76910,#76911),(#76912,#76913),(#76914,#76915),(#76916,#76917),(#76918,
#76919),(#76920,#76921),(#76922,#76923),(#76924,#76925),(#76926,#76927),
(#76928,#76929),(#76930,#76931),(#76932,#76933),(#76934,#76935),(#76936,
#76937),(#76938,#76939),(#76940,#76941),(#76942,#76943),(#76944,#76945),
(#76946,#76947),(#76948,#76949),(#76950,#76951),(#76952,#76953),(#76954,
#76955),(#76956,#76957),(#76958,#76959),(#76960,#76961),(#76962,#76963),
(#76964,#76965),(#76966,#76967),(#76968,#76969),(#76970,#76971),(#76972,
#76973),(#76974,#76975),(#76976,#76977),(#76978,#76979),(#76980,#76981),
(#76982,#76983),(#76984,#76985),(#76986,#76987),(#76988,#76989),(#76990,
#76991),(#76992,#76993),(#76994,#76995),(#76996,#76997),(#76998,#76999),
(#77000,#77001),(#77002,#77003),(#77004,#77005),(#77006,#77007),(#77008,
#77009),(#77010,#77011),(#77012,#77013),(#77014,#77015),(#77016,#77017),
(#77018,#77019),(#77020,#77021),(#77022,#77023),(#77024,#77025),(#77026,
#77027),(#77028,#77029),(#77030,#77031),(#77032,#77033),(#77034,#77035),
(#77036,#77037),(#77038,#77039),(#77040,#77041),(#77042,#77043),(#77044,
#77045),(#77046,#77047),(#77048,#77049),(#77050,#77051),(#77052,#77053),
(#77054,#77055),(#77056,#77057),(#77058,#77059),(#77060,#77061),(#77062,
#77063),(#77064,#77065),(#77066,#77067),(#77068,#77069),(#77070,#77071),
(#77072,#77073),(#77074,#77075),(#77076,#77077),(#77078,#77079),(#77080,
#77081),(#77082,#77083),(#77084,#77085),(#77086,#77087),(#77088,#77089),
(#77090,#77091),(#77092,#77093),(#77094,#77095),(#77096,#77097),(#77098,
#77099),(#77100,#77101),(#77102,#77103),(#77104,#77105),(#77106,#77107),
(#77108,#77109),(#77110,#77111),(#77112,#77113),(#77114,#77115),(#77116,
#77117),(#77118,#77119),(#77120,#77121),(#77122,#77123),(#77124,#77125),
(#77126,#77127),(#77128,#77129),(#77130,#77131),(#77132,#77133),(#77134,
#77135),(#77136,#77137),(#77138,#77139),(#77140,#77141),(#77142,#77143),
(#77144,#77145),(#77146,#77147),(#77148,#77149),(#77150,#77151),(#77152,
#77153),(#77154,#77155),(#77156,#77157),(#77158,#77159),(#77160,#77161),
(#77162,#77163),(#77164,#77165),(#77166,#77167),(#77168,#77169),(#77170,
#77171),(#77172,#77173),(#77174,#77175),(#77176,#77177),(#77178,#77179),
(#77180,#77181),(#77182,#77183),(#77184,#77185),(#77186,#77187),(#77188,
#77189),(#77190,#77191),(#77192,#77193),(#77194,#77195),(#77196,#77197),
(#77198,#77199),(#77200,#77201),(#77202,#77203),(#77204,#77205),(#77206,
#77207),(#77208,#77209),(#77210,#77211),(#77212,#77213),(#77214,#77215),
(#77216,#77217),(#77218,#77219),(#77220,#77221),(#77222,#77223),(#77224,
#77225),(#77226,#77227),(#77228,#77229),(#77230,#77231),(#77232,#77233),
(#77234,#77235),(#77236,#77237),(#77238,#77239),(#77240,#77241),(#77242,
#77243),(#77244,#77245),(#77246,#77247),(#77248,#77249),(#77250,#77251),
(#77252,#77253),(#77254,#77255),(#77256,#77257),(#77258,#77259),(#77260,
#77261),(#77262,#77263),(#77264,#77265),(#77266,#77267),(#77268,#77269),
(#77270,#77271),(#77272,#77273),(#77274,#77275),(#77276,#77277),(#77278,
#77279),(#77280,#77281),(#77282,#77283),(#77284,#77285),(#77286,#77287),
(#77288,#77289),(#77290,#77291),(#77292,#77293),(#77294,#77295),(#77296,
#77297),(#77298,#77299),(#77300,#77301),(#77302,#77303),(#77304,#77305),
(#77306,#77307),(#77308,#77309),(#77310,#77311),(#77312,#77313),(#77314,
#77315),(#77316,#77317),(#77318,#77319),(#77320,#77321),(#77322,#77323),
(#77324,#77325),(#77326,#77327),(#77328,#77329),(#77330,#77331),(#77332,
#77333),(#77334,#77335),(#77336,#77337),(#77338,#77339),(#77340,#77341),
(#77342,#77343),(#77344,#77345),(#77346,#77347),(#77348,#77349),(#77350,
#77351),(#77352,#77353),(#77354,#77355),(#77356,#77357),(#77358,#77359),
(#77360,#77361),(#77362,#77363),(#77364,#77365),(#77366,#77367),(#77368,
#77369),(#77370,#77371),(#77372,#77373),(#77374,#77375),(#77376,#77377),
(#77378,#77379),(#77380,#77381),(#77382,#77383),(#77384,#77385),(#77386,
#77387),(#77388,#77389),(#77390,#77391),(#77392,#77393),(#77394,#77395),
(#77396,#77397),(#77398,#77399),(#77400,#77401),(#77402,#77403),(#77404,
#77405),(#77406,#77407),(#77408,#77409),(#77410,#77411),(#77412,#77413),
(#77414,#77415),(#77416,#77417),(#77418,#77419),(#77420,#77421),(#77422,
#77423),(#77424,#77425),(#77426,#77427),(#77428,#77429),(#77430,#77431),
(#77432,#77433),(#77434,#77435),(#77436,#77437),(#77438,#77439),(#77440,
#77441),(#77442,#77443),(#77444,#77445),(#77446,#77447),(#77448,#77449),
(#77450,#77451),(#77452,#77453),(#77454,#77455),(#77456,#77457),(#77458,
#77459),(#77460,#77461),(#77462,#77463),(#77464,#77465),(#77466,#77467),
(#77468,#77469),(#77470,#77471),(#77472,#77473),(#77474,#77475),(#77476,
#77477),(#77478,#77479),(#77480,#77481),(#77482,#77483),(#77484,#77485),
(#77486,#77487),(#77488,#77489),(#77490,#77491),(#77492,#77493),(#77494,
#77495),(#77496,#77497),(#77498,#77499),(#77500,#77501),(#77502,#77503),
(#77504,#77505),(#77506,#77507),(#77508,#77509),(#77510,#77511),(#77512,
#77513),(#77514,#77515),(#77516,#77517),(#77518,#77519),(#77520,#77521),
(#77522,#77523),(#77524,#77525),(#77526,#77527),(#77528,#77529),(#77530,
#77531),(#77532,#77533),(#77534,#77535),(#77536,#77537),(#77538,#77539),
(#77540,#77541),(#77542,#77543),(#77544,#77545),(#77546,#77547),(#77548,
#77549),(#77550,#77551),(#77552,#77553),(#77554,#77555),(#77556,#77557),
(#77558,#77559),(#77560,#77561),(#77562,#77563),(#77564,#77565),(#77566,
#77567),(#77568,#77569),(#77570,#77571),(#77572,#77573),(#77574,#77575),
(#77576,#77577),(#77578,#77579),(#77580,#77581),(#77582,#77583),(#77584,
#77585),(#77586,#77587),(#77588,#77589),(#77590,#77591),(#77592,#77593),
(#77594,#77595),(#77596,#77597),(#77598,#77599),(#77600,#77601),(#77602,
#77603),(#77604,#77605),(#77606,#77607),(#77608,#77609),(#77610,#77611),
(#77612,#77613),(#77614,#77615),(#77616,#77617),(#77618,#77619),(#77620,
#77621),(#77622,#77623),(#77624,#77625),(#77626,#77627),(#77628,#77629),
(#77630,#77631),(#77632,#77633),(#77634,#77635),(#77636,#77637),(#77638,
#77639),(#77640,#77641),(#77642,#77643),(#77644,#77645),(#77646,#77647),
(#77648,#77649),(#77650,#77651),(#77652,#77653),(#77654,#77655),(#77656,
#77657),(#77658,#77659),(#77660,#77661),(#77662,#77663),(#77664,#77665),
(#77666,#77667),(#77668,#77669),(#77670,#77671),(#77672,#77673),(#77674,
#77675),(#77676,#77677),(#77678,#77679),(#77680,#77681),(#77682,#77683),
(#77684,#77685),(#77686,#77687),(#77688,#77689),(#77690,#77691),(#77692,
#77693),(#77694,#77695),(#77696,#77697),(#77698,#77699),(#77700,#77701),
(#77702,#77703),(#77704,#77705),(#77706,#77707),(#77708,#77709),(#77710,
#77711),(#77712,#77713),(#77714,#77715),(#77716,#77717),(#77718,#77719),
(#77720,#77721),(#77722,#77723),(#77724,#77725),(#77726,#77727),(#77728,
#77729),(#77730,#77731),(#77732,#77733),(#77734,#77735),(#77736,#77737),
(#77738,#77739),(#77740,#77741),(#77742,#77743),(#77744,#77745),(#77746,
#77747),(#77748,#77749),(#77750,#77751),(#77752,#77753),(#77754,#77755),
(#77756,#77757),(#77758,#77759),(#77760,#77761),(#77762,#77763),(#77764,
#77765),(#77766,#77767),(#77768,#77769),(#77770,#77771),(#77772,#77773),
(#77774,#77775),(#77776,#77777),(#77778,#77779),(#77780,#77781),(#77782,
#77783),(#77784,#77785),(#77786,#77787),(#77788,#77789),(#77790,#77791),
(#77792,#77793),(#77794,#77795),(#77796,#77797),(#77798,#77799),(#77800,
#77801),(#77802,#77803),(#77804,#77805),(#77806,#77807),(#77808,#77809),
(#77810,#77811),(#77812,#77813),(#77814,#77815),(#77816,#77817),(#77818,
#77819),(#77820,#77821),(#77822,#77823),(#77824,#77825),(#77826,#77827),
(#77828,#77829),(#77830,#77831),(#77832,#77833),(#77834,#77835),(#77836,
#77837),(#77838,#77839),(#77840,#77841),(#77842,#77843),(#77844,#77845),
(#77846,#77847),(#77848,#77849),(#77850,#77851),(#77852,#77853),(#77854,
#77855),(#77856,#77857),(#77858,#77859),(#77860,#77861),(#77862,#77863),
(#77864,#77865),(#77866,#77867),(#77868,#77869),(#77870,#77871),(#77872,
#77873),(#77874,#77875),(#77876,#77877),(#77878,#77879),(#77880,#77881),
(#77882,#77883),(#77884,#77885),(#77886,#77887),(#77888,#77889),(#77890,
#77891),(#77892,#77893),(#77894,#77895),(#77896,#77897),(#77898,#77899),
(#77900,#77901),(#77902,#77903),(#77904,#77905),(#77906,#77907),(#77908,
#77909),(#77910,#77911),(#77912,#77913),(#77914,#77915),(#77916,#77917),
(#77918,#77919),(#77920,#77921),(#77922,#77923),(#77924,#77925),(#77926,
#77927),(#77928,#77929),(#77930,#77931),(#77932,#77933),(#77934,#77935),
(#77936,#77937),(#77938,#77939),(#77940,#77941),(#77942,#77943),(#77944,
#77945),(#77946,#77947),(#77948,#77949),(#77950,#77951),(#77952,#77953),
(#77954,#77955),(#77956,#77957),(#77958,#77959),(#77960,#77961),(#77962,
#77963),(#77964,#77965),(#77966,#77967),(#77968,#77969),(#77970,#77971),
(#77972,#77973),(#77974,#77975),(#77976,#77977),(#77978,#77979),(#77980,
#77981),(#77982,#77983),(#77984,#77985),(#77986,#77987),(#77988,#77989),
(#77990,#77991),(#77992,#77993),(#77994,#77995),(#77996,#77997),(#77998,
#77999),(#78000,#78001),(#78002,#78003),(#78004,#78005),(#78006,#78007),
(#78008,#78009),(#78010,#78011),(#78012,#78013),(#78014,#78015),(#78016,
#78017),(#78018,#78019),(#78020,#78021),(#78022,#78023),(#78024,#78025),
(#78026,#78027),(#78028,#78029),(#78030,#78031),(#78032,#78033),(#78034,
#78035),(#78036,#78037),(#78038,#78039),(#78040,#78041),(#78042,#78043),
(#78044,#78045),(#78046,#78047),(#78048,#78049),(#78050,#78051),(#78052,
#78053),(#78054,#78055),(#78056,#78057),(#78058,#78059),(#78060,#78061),
(#78062,#78063),(#78064,#78065),(#78066,#78067),(#78068,#78069),(#78070,
#78071),(#78072,#78073),(#78074,#78075),(#78076,#78077),(#78078,#78079),
(#78080,#78081),(#78082,#78083),(#78084,#78085),(#78086,#78087),(#78088,
#78089),(#78090,#78091),(#78092,#78093),(#78094,#78095),(#78096,#78097),
(#78098,#78099),(#78100,#78101),(#78102,#78103),(#78104,#78105),(#78106,
#78107),(#78108,#78109),(#78110,#78111),(#78112,#78113),(#78114,#78115),
(#78116,#78117),(#78118,#78119),(#78120,#78121),(#78122,#78123),(#78124,
#78125),(#78126,#78127),(#78128,#78129),(#78130,#78131),(#78132,#78133),
(#78134,#78135),(#78136,#78137),(#78138,#78139),(#78140,#78141),(#78142,
#78143),(#78144,#78145),(#78146,#78147),(#78148,#78149),(#78150,#78151),
(#78152,#78153),(#78154,#78155),(#78156,#78157),(#78158,#78159),(#78160,
#78161),(#78162,#78163),(#78164,#78165),(#78166,#78167),(#78168,#78169),
(#78170,#78171),(#78172,#78173),(#78174,#78175),(#78176,#78177),(#78178,
#78179),(#78180,#78181),(#78182,#78183),(#78184,#78185),(#78186,#78187),
(#78188,#78189),(#78190,#78191),(#78192,#78193),(#78194,#78195),(#78196,
#78197),(#78198,#78199),(#78200,#78201),(#78202,#78203),(#78204,#78205),
(#78206,#78207),(#78208,#78209),(#78210,#78211),(#78212,#78213),(#78214,
#78215),(#78216,#78217),(#78218,#78219),(#78220,#78221),(#78222,#78223),
(#78224,#78225),(#78226,#78227),(#78228,#78229),(#78230,#78231),(#78232,
#78233),(#78234,#78235),(#78236,#78237),(#78238,#78239),(#78240,#78241),
(#78242,#78243),(#78244,#78245),(#78246,#78247),(#78248,#78249),(#78250,
#78251),(#78252,#78253),(#78254,#78255),(#78256,#78257),(#78258,#78259),
(#78260,#78261),(#78262,#78263),(#78264,#78265),(#78266,#78267),(#78268,
#78269),(#78270,#78271),(#78272,#78273),(#78274,#78275),(#78276,#78277),
(#78278,#78279),(#78280,#78281),(#78282,#78283),(#78284,#78285),(#78286,
#78287),(#78288,#78289),(#78290,#78291),(#78292,#78293),(#78294,#78295),
(#78296,#78297),(#78298,#78299),(#78300,#78301),(#78302,#78303),(#78304,
#78305),(#78306,#78307),(#78308,#78309),(#78310,#78311),(#78312,#78313),
(#78314,#78315),(#78316,#78317),(#78318,#78319),(#78320,#78321),(#78322,
#78323),(#78324,#78325),(#78326,#78327),(#78328,#78329),(#78330,#78331),
(#78332,#78333),(#78334,#78335),(#78336,#78337),(#78338,#78339),(#78340,
#78341),(#78342,#78343),(#78344,#78345),(#78346,#78347),(#78348,#78349),
(#78350,#78351),(#78352,#78353),(#78354,#78355),(#78356,#78357),(#78358,
#78359),(#78360,#78361),(#78362,#78363),(#78364,#78365),(#78366,#78367),
(#78368,#78369),(#78370,#78371),(#78372,#78373),(#78374,#78375),(#78376,
#78377),(#78378,#78379),(#78380,#78381),(#78382,#78383),(#78384,#78385),
(#78386,#78387),(#78388,#78389),(#78390,#78391),(#78392,#78393),(#78394,
#78395),(#78396,#78397),(#78398,#78399),(#78400,#78401),(#78402,#78403),
(#78404,#78405),(#78406,#78407),(#78408,#78409),(#78410,#78411),(#78412,
#78413),(#78414,#78415),(#78416,#78417),(#78418,#78419),(#78420,#78421),
(#78422,#78423),(#78424,#78425),(#78426,#78427),(#78428,#78429),(#78430,
#78431),(#78432,#78433),(#78434,#78435),(#78436,#78437),(#78438,#78439),
(#78440,#78441),(#78442,#78443),(#78444,#78445),(#78446,#78447),(#78448,
#78449),(#78450,#78451),(#78452,#78453),(#78454,#78455),(#78456,#78457),
(#78458,#78459),(#78460,#78461),(#78462,#78463),(#78464,#78465),(#78466,
#78467),(#78468,#78469),(#78470,#78471),(#78472,#78473),(#78474,#78475),
(#78476,#78477),(#78478,#78479),(#78480,#78481),(#78482,#78483),(#78484,
#78485),(#78486,#78487),(#78488,#78489),(#78490,#78491),(#78492,#78493),
(#78494,#78495),(#78496,#78497),(#78498,#78499),(#78500,#78501),(#78502,
#78503),(#78504,#78505),(#78506,#78507),(#78508,#78509),(#78510,#78511),
(#78512,#78513),(#78514,#78515),(#78516,#78517),(#78518,#78519),(#78520,
#78521),(#78522,#78523),(#78524,#78525),(#78526,#78527),(#78528,#78529),
(#78530,#78531),(#78532,#78533),(#78534,#78535),(#78536,#78537),(#78538,
#78539),(#78540,#78541),(#78542,#78543),(#78544,#78545),(#78546,#78547),
(#78548,#78549),(#78550,#78551),(#78552,#78553),(#78554,#78555),(#78556,
#78557),(#78558,#78559),(#78560,#78561),(#78562,#78563),(#78564,#78565),
(#78566,#78567),(#78568,#78569),(#78570,#78571),(#78572,#78573),(#78574,
#78575),(#78576,#78577),(#78578,#78579),(#78580,#78581),(#78582,#78583),
(#78584,#78585),(#78586,#78587),(#78588,#78589),(#78590,#78591),(#78592,
#78593),(#78594,#78595),(#78596,#78597),(#78598,#78599),(#78600,#78601),
(#78602,#78603),(#78604,#78605),(#78606,#78607),(#78608,#78609),(#78610,
#78611),(#78612,#78613),(#78614,#78615),(#78616,#78617),(#78618,#78619),
(#78620,#78621),(#78622,#78623),(#78624,#78625),(#78626,#78627),(#78628,
#78629),(#78630,#78631),(#78632,#78633),(#78634,#78635),(#78636,#78637),
(#78638,#78639),(#78640,#78641),(#78642,#78643),(#78644,#78645),(#78646,
#78647),(#78648,#78649),(#78650,#78651),(#78652,#78653),(#78654,#78655),
(#78656,#78657),(#78658,#78659),(#78660,#78661),(#78662,#78663),(#78664,
#78665),(#78666,#78667),(#78668,#78669),(#78670,#78671),(#78672,#78673),
(#78674,#78675),(#78676,#78677),(#78678,#78679),(#78680,#78681),(#78682,
#78683),(#78684,#78685),(#78686,#78687),(#78688,#78689),(#78690,#78691),
(#78692,#78693),(#78694,#78695),(#78696,#78697),(#78698,#78699),(#78700,
#78701),(#78702,#78703),(#78704,#78705),(#78706,#78707),(#78708,#78709),
(#78710,#78711),(#78712,#78713),(#78714,#78715),(#78716,#78717),(#78718,
#78719),(#78720,#78721),(#78722,#78723),(#78724,#78725),(#78726,#78727),
(#78728,#78729),(#78730,#78731),(#78732,#78733),(#78734,#78735),(#78736,
#78737),(#78738,#78739),(#78740,#78741),(#78742,#78743),(#78744,#78745),
(#78746,#78747),(#78748,#78749),(#78750,#78751),(#78752,#78753),(#78754,
#78755),(#78756,#78757),(#78758,#78759),(#78760,#78761),(#78762,#78763),
(#78764,#78765),(#78766,#78767),(#78768,#78769),(#78770,#78771),(#78772,
#78773),(#78774,#78775),(#78776,#78777),(#78778,#78779),(#78780,#78781),
(#78782,#78783),(#78784,#78785),(#78786,#78787),(#78788,#78789),(#78790,
#78791),(#78792,#78793),(#78794,#78795),(#78796,#78797),(#78798,#78799),
(#78800,#78801),(#78802,#78803),(#78804,#78805),(#78806,#78807),(#78808,
#78809),(#78810,#78811),(#78812,#78813),(#78814,#78815),(#78816,#78817),
(#78818,#78819),(#78820,#78821),(#78822,#78823),(#78824,#78825),(#78826,
#78827),(#78828,#78829),(#78830,#78831),(#78832,#78833),(#78834,#78835),
(#78836,#78837),(#78838,#78839),(#78840,#78841),(#78842,#78843),(#78844,
#78845),(#78846,#78847),(#78848,#78849),(#78850,#78851),(#78852,#78853),
(#78854,#78855),(#78856,#78857),(#78858,#78859),(#78860,#78861),(#78862,
#78863),(#78864,#78865),(#78866,#78867),(#78868,#78869),(#78870,#78871),
(#78872,#78873),(#78874,#78875),(#78876,#78877),(#78878,#78879),(#78880,
#78881),(#78882,#78883),(#78884,#78885),(#78886,#78887),(#78888,#78889),
(#78890,#78891),(#78892,#78893),(#78894,#78895),(#78896,#78897),(#78898,
#78899),(#78900,#78901),(#78902,#78903),(#78904,#78905),(#78906,#78907),
(#78908,#78909),(#78910,#78911),(#78912,#78913),(#78914,#78915),(#78916,
#78917),(#78918,#78919),(#78920,#78921),(#78922,#78923),(#78924,#78925),
(#78926,#78927),(#78928,#78929),(#78930,#78931),(#78932,#78933),(#78934,
#78935),(#78936,#78937),(#78938,#78939),(#78940,#78941),(#78942,#78943),
(#78944,#78945),(#78946,#78947),(#78948,#78949),(#78950,#78951),(#78952,
#78953),(#78954,#78955),(#78956,#78957),(#78958,#78959),(#78960,#78961),
(#78962,#78963),(#78964,#78965),(#78966,#78967),(#78968,#78969),(#78970,
#78971),(#78972,#78973),(#78974,#78975),(#78976,#78977),(#78978,#78979)),
 .UNSPECIFIED.,.F.,.F.,.F.,(4,1,1,1,1,1,1,1,1,1,1,1,1,1,1,1,1,1,1,1,1,1,
1,1,1,1,1,1,1,1,1,1,1,1,1,1,1,1,1,1,1,1,1,1,1,1,1,1,1,1,1,1,1,1,1,1,1,1,
1,1,1,1,1,1,1,1,1,1,1,1,1,1,1,1,1,1,1,1,1,1,1,1,1,1,1,1,1,1,1,1,1,1,1,1,
1,1,1,1,1,1,1,1,1,1,1,1,1,1,1,1,1,1,1,1,1,1,1,1,1,1,1,1,1,1,1,1,1,1,1,1,
1,1,1,1,1,1,1,1,1,1,1,1,1,1,1,1,1,1,1,1,1,1,1,1,1,1,1,1,1,1,1,1,1,1,1,1,
1,1,1,1,1,1,1,1,1,1,1,1,1,1,1,1,1,1,1,1,1,1,1,1,1,1,1,1,1,1,1,1,1,1,1,1,
1,1,1,1,1,1,1,1,1,1,1,1,1,1,1,1,1,1,1,1,1,1,1,1,1,1,1,1,1,1,1,1,1,1,1,1,
1,1,1,1,1,1,1,1,1,1,1,1,1,1,1,1,1,1,1,1,1,1,1,1,1,1,1,1,1,1,1,1,1,1,1,1,
1,1,1,1,1,1,1,1,1,1,1,1,1,1,1,1,1,1,1,1,1,1,1,1,1,1,1,1,1,1,1,1,1,1,1,1,
1,1,1,1,1,1,1,1,1,1,1,1,1,1,1,1,1,1,1,1,1,1,1,1,1,1,1,1,1,1,1,1,1,1,1,1,
1,1,1,1,1,1,1,1,1,1,1,1,1,1,1,1,1,1,1,1,1,1,1,1,1,1,1,1,1,1,1,1,1,1,1,1,
1,1,1,1,1,1,1,1,1,1,1,1,1,1,1,1,1,1,1,1,1,1,1,1,1,1,1,1,1,1,1,1,1,1,1,1,
1,1,1,1,1,1,1,1,1,1,1,1,1,1,1,1,1,1,1,1,1,1,1,1,1,1,1,1,1,1,1,1,1,1,1,1,
1,1,1,1,1,1,1,1,1,1,1,1,1,1,1,1,1,1,1,1,1,1,1,1,1,1,1,1,1,1,1,1,1,1,1,1,
1,1,1,1,1,1,1,1,1,1,1,1,1,1,1,1,1,1,1,1,1,1,1,1,1,1,1,1,1,1,1,1,1,1,1,1,
1,1,1,1,1,1,1,1,1,1,1,1,1,1,1,1,1,1,1,1,1,1,1,1,1,1,1,1,1,1,1,1,1,1,1,1,
1,1,1,1,1,1,1,1,1,1,1,1,1,1,1,1,1,1,1,1,1,1,1,1,1,1,1,1,1,1,1,1,1,1,1,1,
1,1,1,1,1,1,1,1,1,1,1,1,1,1,1,1,1,1,1,1,1,1,1,1,1,1,1,1,1,1,1,1,1,1,1,1,
1,1,1,1,1,1,1,1,1,1,1,1,1,1,1,1,1,1,1,1,1,1,1,1,1,1,1,1,1,1,1,1,1,1,1,1,
1,1,1,1,1,1,1,1,1,1,1,1,1,1,1,1,1,1,1,1,1,1,1,1,1,1,1,1,1,1,1,1,1,1,1,1,
1,1,1,1,1,1,1,1,1,1,1,1,1,1,1,1,1,1,1,1,1,1,1,1,1,1,1,1,1,1,1,1,1,1,1,1,
1,1,1,1,1,1,1,1,1,1,1,1,1,1,1,1,1,1,1,1,1,1,1,1,1,1,1,1,1,1,1,1,1,1,1,1,
1,1,1,1,1,1,1,1,1,1,1,1,1,1,1,1,1,1,1,1,1,1,1,1,1,1,1,1,1,1,1,1,1,1,1,1,
1,1,1,1,1,1,1,1,1,1,1,1,1,1,1,1,1,1,1,1,1,1,1,1,1,1,1,1,1,1,1,1,1,1,1,1,
1,1,1,1,1,1,1,1,1,1,1,1,1,1,1,1,1,1,1,1,1,1,1,1,1,1,1,1,1,1,1,1,1,1,1,1,
1,1,1,1,1,1,1,1,1,1,1,1,1,1,1,1,1,1,1,1,1,1,1,1,1,1,1,1,1,1,1,1,1,1,1,1,
1,1,1,1,1,1,1,1,1,1,1,1,1,1,1,1,1,1,1,1,1,1,1,1,1,1,1,1,1,1,1,1,1,1,1,1,
1,1,1,1,1,1,1,1,1,1,1,1,1,1,1,1,1,1,1,1,1,1,1,1,1,1,1,1,1,1,1,1,1,1,1,1,
1,1,1,1,1,1,1,1,1,1,1,1,1,1,1,1,1,1,1,1,1,1,1,1,1,1,1,1,1,1,1,1,1,1,1,1,
1,1,1,1,1,1,1,1,1,1,1,1,1,1,1,1,1,1,1,1,1,1,1,1,1,1,1,1,1,1,1,1,1,1,1,1,
1,1,1,1,1,1,1,1,1,1,1,1,1,1,1,1,1,1,1,1,1,1,1,1,1,1,1,1,1,1,1,1,1,1,1,1,
1,1,1,1,1,1,1,1,1,1,1,1,1,1,1,1,1,1,1,1,1,1,1,1,1,1,1,1,1,1,1,1,1,1,1,1,
1,1,1,1,1,1,1,1,1,1,1,1,1,1,1,1,1,1,1,1,1,1,1,1,1,1,1,1,1,1,1,1,1,1,1,1,
1,1,1,1,1,1,1,1,1,1,1,1,1,1,1,1,1,1,1,1,1,1,1,1,1,1,1,1,1,1,1,1,1,1,1,1,
1,1,1,1,1,1,1,1,1,1,1,1,1,1,1,1,1,1,1,1,1,1,1,1,1,1,1,1,1,1,1,1,1,1,1,1,
1,1,1,1,1,1,1,1,1,1,1,1,1,1,1,1,1,1,1,1,1,1,1,1,1,1,1,1,1,1,1,1,1,1,1,1,
1,1,1,1,1,1,1,1,1,1,1,1,1,1,1,1,1,1,1,1,1,1,1,1,1,1,1,1,1,1,1,1,1,1,1,1,
1,1,1,1,1,1,1,1,1,1,1,1,1,1,1,1,1,1,1,1,1,1,1,1,1,1,1,1,1,1,1,1,1,1,1,1,
1,1,1,1,1,1,1,1,1,1,1,1,1,1,1,1,1,1,1,1,1,1,1,1,1,1,1,1,1,1,1,1,1,1,1,1,
1,1,1,1,1,1,1,1,1,1,1,1,1,1,1,1,1,1,1,1,1,1,1,1,1,1,1,1,1,1,1,1,1,1,1,1,
1,1,1,1,1,1,1,1,1,1,1,1,1,1,1,1,1,1,1,1,1,1,1,1,1,1,1,1,1,1,1,1,1,1,1,1,
1,1,1,1,1,1,1,1,1,1,1,1,1,1,1,1,1,1,1,1,1,1,1,1,1,1,1,1,1,1,1,1,1,1,1,1,
1,1,1,1,1,1,1,1,1,1,1,1,1,1,1,1,1,1,1,1,1,1,1,1,1,1,1,1,1,1,1,1,1,1,1,1,
1,1,1,1,1,1,1,1,1,1,1,1,1,1,1,1,1,1,1,1,1,1,1,1,1,1,1,1,1,1,1,1,1,1,1,1,
1,1,1,1,1,1,1,1,1,1,1,1,1,1,1,1,1,1,1,1,1,1,1,1,1,1,1,1,1,1,1,1,1,1,1,1,
1,1,1,1,1,1,1,1,1,1,1,1,1,1,1,1,1,1,1,1,1,1,1,1,1,1,1,1,1,1,1,1,1,1,1,1,
1,1,1,1,1,1,1,1,1,1,1,1,1,1,1,1,1,1,1,1,1,1,1,1,1,1,1,1,1,1,1,1,1,1,1,1,
1,1,1,1,1,1,1,1,1,1,1,1,1,1,1,1,1,1,1,1,1,1,1,1,1,1,1,1,1,1,1,1,1,1,1,1,
1,1,1,1,1,1,1,1,1,1,1,1,1,1,1,1,1,1,1,1,1,1,1,1,1,1,1,1,1,1,1,1,1,1,1,1,
1,1,1,1,1,1,1,1,1,1,1,1,1,1,1,1,1,1,1,1,1,1,1,1,1,1,1,1,1,1,1,1,1,1,1,1,
1,1,1,1,1,1,1,1,1,1,1,1,1,1,1,1,1,1,1,1,1,1,1,1,1,1,1,1,1,1,1,1,1,1,1,1,
1,1,1,1,1,1,1,1,1,1,1,1,1,1,1,1,1,1,1,1,1,1,1,1,1,1,1,1,1,1,1,1,1,1,1,1,
1,1,1,1,1,1,1,1,1,1,1,1,1,1,1,1,1,1,1,1,1,1,1,1,1,1,1,1,1,1,1,1,1,1,1,1,
1,1,1,1,1,1,1,1,1,1,1,1,1,1,1,1,1,1,1,1,1,1,1,1,1,1,1,1,1,1,1,1,1,1,1,1,
1,1,1,1,1,1,1,1,1,1,1,1,1,1,1,1,1,1,1,1,1,1,1,1,1,1,1,1,1,1,1,1,1,1,1,1,
1,1,1,1,1,1,1,1,1,1,1,1,1,1,1,1,1,1,1,1,1,1,1,1,1,1,1,1,1,1,1,1,1,1,1,1,
1,1,1,1,1,1,1,1,1,1,1,1,1,1,1,1,1,1,1,1,1,1,1,1,1,1,1,1,1,1,1,1,1,1,1,1,
1,1,1,1,1,1,1,1,1,1,1,1,1,1,1,1,1,1,1,1,1,1,1,1,1,1,1,1,1,1,1,1,1,1,1,1,
1,1,1,1,1,1,1,1,1,1,1,1,1,1,1,1,1,1,1,1,1,1,1,1,1,1,1,1,1,1,1,1,1,1,1,1,
1,1,1,1,1,1,1,1,1,1,1,1,1,1,1,1,1,1,1,1,1,1,1,1,1,1,1,1,1,1,1,1,1,1,1,1,
1,1,1,1,1,1,1,1,1,1,1,1,1,1,1,1,1,1,1,1,1,1,1,1,1,1,1,1,1,1,1,1,1,1,1,1,
1,1,1,1,1,1,1,1,1,1,1,1,1,1,1,1,1,1,1,1,1,1,1,1,1,1,1,1,1,1,1,1,1,1,1,1,
1,1,1,1,1,1,1,1,1,1,1,1,1,1,1,1,1,1,1,1,1,1,1,1,1,1,1,1,1,1,1,1,1,1,1,1,
1,1,1,1,1,1,1,1,1,1,1,1,1,1,1,1,1,1,1,1,1,1,1,1,1,1,1,1,1,1,1,1,1,1,1,1,
1,1,1,1,1,1,1,1,1,1,1,1,1,1,1,1,1,1,1,1,1,1,1,1,1,1,1,1,1,1,1,1,1,1,1,1,
1,1,1,1,1,1,1,1,1,1,1,1,1,1,1,1,1,1,1,1,1,1,1,1,1,1,1,1,1,1,1,1,1,1,1,1,
1,1,1,1,1,1,1,1,1,1,1,1,1,1,1,1,1,1,1,1,1,1,1,1,1,1,1,1,1,1,1,1,1,1,1,1,
1,1,1,1,1,1,1,1,1,1,1,1,1,1,1,1,1,1,1,1,1,1,1,1,1,1,1,1,1,1,1,1,1,1,1,1,
1,1,1,1,1,1,1,1,1,1,1,1,1,1,1,1,1,1,1,1,1,1,1,1,1,1,1,1,1,1,1,1,1,1,1,1,
1,1,1,1,1,1,1,1,1,1,1,1,1,1,1,1,1,1,1,1,1,1,1,1,1,1,1,1,1,1,1,1,1,1,1,1,
1,1,1,1,1,1,1,1,1,1,1,1,1,1,1,1,1,1,1,1,1,1,1,1,1,1,1,1,1,1,1,1,1,1,1,1,
1,1,1,1,1,1,1,1,1,1,1,1,1,1,1,1,1,1,1,1,1,1,1,1,1,1,1,1,1,1,1,1,1,1,1,1,
1,1,1,1,1,1,1,1,1,1,1,1,1,1,1,1,1,1,1,1,1,1,1,1,1,1,1,1,1,1,1,1,1,1,1,1,
1,1,1,1,1,1,1,1,1,1,1,1,1,1,1,1,1,1,1,1,1,1,1,1,1,1,1,1,1,1,1,1,1,1,1,1,
1,1,1,1,1,1,1,1,1,1,1,1,1,1,1,1,1,1,1,1,1,1,1,1,1,1,1,1,1,1,1,1,1,1,1,1,
1,1,1,1,1,1,1,1,1,1,1,1,1,1,1,1,1,1,1,1,1,1,1,1,1,1,1,1,1,1,1,1,1,1,1,1,
1,1,1,1,1,1,1,1,1,1,1,1,1,1,1,1,1,1,1,1,1,1,1,1,1,1,1,1,1,1,1,1,1,1,1,1,
1,1,1,1,1,1,1,1,1,1,1,1,1,1,1,1,1,1,1,1,1,1,1,1,1,1,1,1,1,1,1,1,1,1,1,1,
1,1,1,1,1,1,1,1,1,1,1,1,1,1,1,1,1,1,1,1,1,1,1,1,1,1,1,1,1,1,1,1,1,1,1,1,
1,1,1,1,1,1,1,1,1,1,1,1,1,1,1,1,1,1,1,1,1,1,1,1,1,1,1,1,1,1,1,1,1,1,1,1,
1,1,1,1,1,1,1,1,1,1,1,1,1,1,1,1,1,1,1,1,1,1,1,1,1,1,1,1,1,1,1,1,1,1,1,1,
1,1,1,1,1,1,1,1,1,1,1,1,1,1,1,1,1,1,1,1,1,1,1,1,1,1,1,1,1,1,1,1,1,1,1,1,
1,1,1,1,1,1,1,1,1,1,1,1,1,1,1,1,1,1,1,1,1,1,1,1,1,1,1,1,1,1,1,1,1,1,1,1,
1,1,1,1,1,1,1,1,1,1,1,1,1,1,1,1,1,1,1,1,1,1,1,1,1,1,1,1,1,1,1,1,1,1,1,1,
1,1,1,1,1,1,1,1,1,1,1,1,1,1,1,1,1,1,1,1,1,1,1,1,1,1,1,1,1,1,1,1,1,1,1,1,
1,1,1,1,1,1,1,1,1,1,1,1,1,1,1,1,1,1,1,1,1,1,1,1,1,1,1,1,1,1,1,1,1,1,1,1,
1,1,1,1,1,1,1,1,1,1,1,1,1,1,1,1,1,1,1,1,1,1,1,1,1,1,1,1,1,1,1,1,1,1,1,1,
1,1,1,1,1,1,1,1,1,1,1,1,1,1,1,1,1,1,1,1,1,1,1,1,1,1,1,1,1,1,1,1,1,1,1,1,
1,1,1,1,1,1,1,1,1,1,1,1,1,1,1,1,1,1,1,1,1,1,1,1,1,1,1,1,1,1,1,1,1,1,1,1,
1,1,1,1,1,1,1,1,1,1,1,1,1,1,1,1,1,1,1,1,1,1,1,1,1,1,1,1,1,1,1,1,1,1,1,1,
1,1,1,1,1,1,1,1,1,1,1,1,1,1,1,1,1,1,1,1,1,1,1,1,1,1,1,1,1,1,1,1,1,1,1,1,
1,1,1,1,1,1,1,1,1,1,1,1,1,1,1,1,1,1,1,1,1,1,1,1,1,1,1,1,1,1,1,1,1,1,1,1,
1,1,1,1,1,1,1,1,1,1,1,1,1,1,1,1,1,1,1,1,1,1,1,1,1,1,1,1,1,1,1,1,1,1,1,1,
1,1,1,1,1,1,1,1,1,1,1,1,1,1,1,1,1,1,1,1,1,1,1,1,1,1,1,1,1,1,1,1,1,1,1,1,
1,1,1,1,1,1,1,1,1,1,1,1,1,1,1,1,1,1,1,1,1,1,1,1,1,1,1,1,1,1,1,1,1,1,1,1,
1,1,1,1,1,1,1,1,1,1,1,1,1,1,1,1,1,1,1,1,1,1,1,1,1,1,1,1,1,1,1,1,1,1,1,1,
1,1,1,1,1,1,1,1,1,1,1,1,1,1,1,1,1,1,1,1,1,1,1,1,1,1,1,1,1,1,1,1,1,1,1,1,
1,1,1,1,4),(2,2),(0.,0.869746702321014,1.7394931589914,2.60923976624962,
3.47983908319159,4.35043840179749,5.22018503077054,6.08993165951504,6.95967828799171,
7.82942491616733,8.69917154401062,9.56891817149224,10.4395174886835,11.3101168056706,
12.179863432132,13.049610058144,13.9193566836854,14.7891033087372,15.6588499332817,
16.5285965573034,17.3991958717975,18.2697951860185,18.7046684974166,19.1395418086746,
19.5744151197912,20.0092884307654,20.4441617415962,20.8790350522825,21.7487816732187,
22.1836549834672,22.6185282935685,23.0534016035221,23.4882749133276,23.9231482229848,
24.3588742245859,24.794600226187,25.2294735355468,26.0992201538203,26.5340934627341,
26.9689667714994,27.4038400801166,27.838713388586,28.2735866969081,28.7084600050832,
29.143333313112,29.5782066209952,30.0130799287334,30.4479532363275,30.8828265437783,
31.3185525442794,31.7542785447804,32.1891518519474,32.6240251589741,33.0588984658616,
33.4937717726112,33.928645079224,34.3635183857014,34.7983916920448,35.2332649982556,
35.6681383043353,36.1030116102854,36.5378849161076,36.9727582218035,37.4076315273749,
37.8425048328235,38.2782308323341,38.7139568318446,39.1488301370532,39.5837034421446,
40.0185767471208,40.4534500519838,40.8883233567357,41.3231966613787,41.7580699659148,
42.1929432703463,42.6278165746754,43.0626898789044,43.4975631830356,43.9324364870714,
44.3673097910142,44.8021830948664,45.2379090935952,45.673635092324,46.1085083960024,
46.5433816995978,46.9782550031127,47.4131283065497,47.8480016099115,48.2828749132006,
48.7177482164198,49.1526215195718,49.5874948226593,50.0223681256851,50.457241428652,
50.8921147315628,51.3269880344203,51.7618613372274,52.197587335454,52.6333133336805,
53.0681866363954,53.5030599390685,53.9379332417027,54.3728065443011,54.8076798468664,
55.2425531494018,55.6774264519101,56.1122997543943,56.5471730568575,56.9820463593026,
57.4169196617326,57.8517929641506,58.2866662665595,58.7215395689624,59.157265567009,
59.5929915650557,60.0278648674556,60.4627381698584,60.8976114722673,61.3324847746853,
61.7673580771153,62.2022313795604,62.6371046820236,63.0719779845079,63.5068512870162,
63.9417245895516,64.376597892117,64.8114711947155,65.2463444973499,65.6812178000231,
66.1169437982275,66.5526697964318,66.9875430991915,67.4224164019987,67.8572897048563,
68.2921630077673,68.7270363107343,69.1619096137603,69.5967829168479,70.0316562200001,
70.4665295232194,70.9014028265087,71.3362761298705,71.7711494333077,72.2060227368227,
72.6408960404182,73.0766220391044,73.5123480377905,73.9472213415547,74.382094645407,
74.8169679493499,75.2518412533859,75.6867145575172,76.1215878617464,76.5564611660756,
76.9913344705072,77.4262077750435,77.8610810796866,78.2959543844386,78.7308276893018,
79.1657009942781,79.6005742993696,80.0363002988208,80.4720262982719,80.9068996035997,
81.3417729090484,81.7766462146199,82.211519520316,82.6463928261383,83.0812661320886,
83.5161394381684,83.9510127443794,84.3858860507229,84.8207593572004,85.2556326638134,
85.6905059705631,86.1253792774507,86.5602525844776,86.995978584908,87.4317045853384,
87.8665778926469,88.3014512000977,88.7363245076919,89.1711978154302,89.6060711233134,
90.0409444313423,90.4758177395175,90.9106910478396,91.345564356309,91.7804376649263,
92.2153109736917,92.6501842826055,93.085057591668,93.5199309008791,93.9556569024059,
94.3913829039327,94.8262562134414,95.2611295230986,95.6960028329042,96.1308761428578,
96.5657494529591,97.0006227632077,97.4354960736028,97.870369384144,98.3052426948304,
98.7401160056612,99.1749893166354,99.6098626277522,100.04473593901,100.915335253024,
101.351061255639,101.785934567313,102.220807879124,102.655681191068,103.090554503145,
103.525427815353,104.395174440154,105.264921065453,105.699794378283,106.134667691232,
106.569541004295,107.004414317471,107.8750136343,108.745612951339,109.615359578629,
110.485106206296,111.354852834309,112.224599462639,113.094346091254,113.964092720119,
114.834692038763,115.705291357499,116.575037986826,117.444784616267,118.314531245777,
119.184277875311,120.054024504821,120.923771134261,121.794370453112,122.66496977189,
123.534716400968,124.404463029834,125.274209658448,126.143956286779,127.013702914792,
127.883449542458,128.754048859798,129.624648176939,130.494394803617,131.364141429857,
132.233888055637,133.103634680937,133.973381305737,134.843127930023,135.71372724472,
136.584326559147,137.019199870684,137.454073182083,137.888946493341,138.323819804458,
139.193566426263,140.063313047491,140.498186357887,140.933059668136,141.367932978237,
141.802806288191,142.237679597997,142.673405599673,143.109131601348,143.544004910857,
143.978878220217,144.413751529429,144.848624838491,145.283498147405,145.718371456171,
146.153244764789,146.588118073258,147.022991381581,147.457864689756,147.892737997785,
148.327611305669,148.762484613407,149.197357921002,149.633083921574,150.068809922147,
150.503683229455,150.938556536623,151.37342984365,151.808303150538,152.243176457288,
152.678049763901,153.112923070379,153.547796376722,153.982669682934,154.417542989014,
154.852416294964,155.287289600787,155.722162906483,156.157036212055,156.592762211626,
157.028488211198,157.463361516526,157.898234821735,158.333108126826,158.767981431803,
159.202854736666,159.637728041419,160.072601346062,160.507474650599,160.94234795503,
161.37722125936,161.812094563589,162.246967867721,162.681841171757,163.1167144757,
163.552440474473,163.988166473247,164.423039777011,164.85791308069,165.292786384286,
165.727659687801,166.162532991238,166.597406294601,167.03227959789,167.46715290111,
167.902026204262,168.33689950735,168.771772810376,169.206646113343,169.641519416254,
170.076392719112,170.512118717363,170.947844715614,171.382718018374,171.817591321089,
172.252464623762,172.687337926397,173.122211228996,173.557084531561,173.991957834097,
174.426831136606,174.86170443909,175.296577741554,175.731451044,176.16632434643,
176.601197648848,177.036070951258,177.471796949306,177.907522947355,178.342396249755,
178.777269552155,179.212142854558,179.647016156968,180.081889459386,180.516762761816,
180.951636064262,181.386509366726,181.82138266921,182.256255971719,182.691129274255,
183.12600257682,183.560875879419,183.995749182054,184.431475180237,184.867201178421,
185.302074481136,185.736947783896,186.171821086704,186.606694389561,187.041567692473,
187.47644099544,187.911314298466,188.346187601554,188.781060904706,189.215934207926,
189.650807511215,190.085680814577,190.520554118015,190.95542742153,191.391153420175,
191.82687941882,192.261752722499,192.696626026263,193.131499330116,193.566372634059,
194.001245938095,194.436119242227,194.870992546456,195.305865850785,195.740739155217,
196.175612459754,196.610485764397,197.045359069149,197.480232374013,197.915105678989,
198.350831678382,198.786557677775,199.221430982984,199.656304288312,200.091177593761,
200.526050899333,200.960924205029,201.395797510852,201.830670816802,202.265544122882,
202.700417429093,203.135290735437,203.570164041915,204.005037348528,204.439910655278,
204.874783962166,205.310509962526,205.746235962887,206.181109270054,206.615982577363,
207.050855884814,207.485729192409,207.920602500147,208.355475808031,208.79034911606,
209.225222424235,209.660095732558,210.094969041027,210.529842349645,210.96471565841,
211.399588967324,211.834462276387,212.27018827784,212.705914279292,213.140787588653,
213.575660898161,214.010534207819,214.880280827579,215.31515413768,215.750027447929,
216.184900758324,216.619774068866,217.054647379553,217.489520690384,218.359267312475,
219.22986662628,219.665592628826,220.100465940363,220.535339252038,220.970212563848,
221.83995918787,222.709705812416,223.579452437468,224.014325750179,224.44919906301,
225.318945689022,226.189545005688,227.060144322571,227.929890949664,228.799637577146,
229.66938420499,230.539130833166,231.408877461643,232.278624090388,233.149223408954,
234.019822727623,234.889569356878,235.759315986267,236.629062615749,237.498809245277,
238.368555874806,239.238302504287,240.108901823183,240.979501142017,241.849247771189,
242.718994400167,243.588741028911,244.458487657389,245.328234285565,246.197980913409,
247.068580230891,247.939179548182,248.80892617507,249.678672801532,250.548419427545,
251.418166053087,252.287912678139,253.157659302684,254.028258617581,254.898857932211,
255.333731243885,255.768604555423,256.203477866821,256.63835117808,257.508097800171,
258.377844421689,258.812717732231,259.247591042627,259.682464352876,260.117337662977,
260.552210972931,260.987936974682,261.858536286089,262.293409595598,262.728282904958,
263.16315621417,263.598029523233,264.032902832147,264.467776140913,264.902649449531,
265.337522758001,265.772396066323,266.207269374499,266.642142682528,267.077015990412,
267.511889298151,267.947615298795,268.383341299439,268.81821460689,269.2530879142,
269.687961221367,270.122834528394,270.557707835282,270.992581142032,271.427454448646,
271.862327755124,272.297201061468,272.732074367679,273.166947673759,273.60182097971,
274.036694285533,274.471567591229,274.907293590862,275.343019590495,275.777892895944,
276.212766201272,276.647639506481,277.082512811573,277.51738611655,277.952259421414,
278.387132726166,278.82200603081,279.256879335346,279.691752639779,280.126625944108,
280.561499248338,280.996372552469,281.431245856506,281.866971855324,282.302697854143,
282.737571157996,283.172444461761,283.60731776544,284.042191069036,284.477064372551,
284.911937675989,285.346810979351,285.781684282641,286.216557585861,286.651430889013,
287.086304192101,287.521177495128,287.956050798095,288.390924101007,288.826650099283,
289.262376097559,289.697249400366,290.132122703127,290.566996005842,291.001869308516,
291.43674261115,291.871615913749,292.306489216315,292.741362518851,293.17623582136,
293.611109123845,294.045982426308,294.480855728754,294.915729031185,295.350602333603,
295.786328331655,296.222054329707,296.65692763211,297.091800934511,297.526674236911,
297.961547539314,298.396420841724,298.831294144142,299.266167446573,299.701040749018,
300.135914051482,300.570787353967,301.005660656476,301.440533959012,301.875407261578,
302.310280564177,302.746006562341,303.181732560506,303.616605863179,304.051479165895,
304.486352468655,304.921225771462,305.35609907432,305.790972377232,306.225845680199,
306.660718983226,307.095592286314,307.530465589466,307.965338892686,308.400212195976,
308.835085499338,309.269958802776,309.705684801381,310.141410799985,310.576284103581,
311.01115740726,311.446030711025,311.880904014878,312.315777318821,312.750650622858,
313.185523926989,313.620397231219,314.055270535549,314.490143839981,314.925017144517,
315.359890449161,315.794763753913,316.229637058777,316.665363058112,317.101089057448,
317.53596236254,317.970835667749,318.405708973077,318.840582278526,319.275455584098,
319.710328889795,320.145202195618,320.580075501568,321.014948807648,321.44982211386,
321.884695420204,322.319568726682,322.754442033295,323.189315340045,323.625041340336,
324.060767340628,324.495640647655,324.930513954822,325.365387262131,325.800260569583,
326.235133877177,326.670007184916,327.1048804928,327.539753800829,327.974627109005,
328.409500417327,328.844373725797,329.279247034415,329.714120343181,330.148993652095,
330.584719653474,331.020445654852,331.455318964064,331.890192273424,332.325065582933,
332.759938892591,333.194812202397,333.629685512351,334.064558822453,334.499432132702,
334.934305443098,335.369178753639,335.804052064326,336.673798686132,337.108671997249,
337.544397999725,337.980124002201,338.4149973136,338.849870625137,339.284743936812,
340.154490560568,341.024237184854,341.459110497191,341.893983809655,342.328857122244,
342.763730434955,343.633477060735,344.504076377234,345.374675693955,346.244422320844,
347.114168948136,347.983915575803,348.853662203817,349.723408832148,350.593155460764,
351.463754779246,352.334354097839,353.204100727012,354.07384735634,354.943593985781,
355.813340615292,356.683087244827,357.552833874338,358.423433193272,359.294032512154,
360.163779141409,361.033525770489,361.903272399355,362.77301902797,363.642765656301,
364.512512284316,365.383111601936,366.253710919371,367.123457546465,367.993204173143,
368.862950799383,369.732697425164,370.602444050463,371.472190675265,372.342789990359,
373.21338930519,373.648262617,374.083135928675,374.952882551611,375.822629173987,
376.257502484962,376.692375795793,377.12724910648,377.562122417021,377.996995727417,
378.431869037666,378.866742347767,379.302468349591,379.738194351416,380.173067661222,
380.607940970879,381.042814280388,381.477687589749,381.91256089896,382.347434208023,
382.782307516937,383.217180825703,383.652054134321,384.086927442791,384.521800751113,
384.956674059289,385.391547367318,385.826420675202,386.262146675918,386.697872676635,
387.13274598423,387.567619291681,388.00249259899,388.437365906157,388.872239213185,
389.307112520073,389.741985826823,390.176859133436,390.611732439914,391.046605746258,
391.48147905247,391.91635235855,392.351225664501,392.786098970323,393.221824970019,
393.657550969714,394.092424275286,394.527297580735,394.962170886063,395.397044191272,
395.831917496364,396.266790801341,396.701664106204,397.136537410957,397.5714107156,
398.006284020137,398.441157324569,398.876030628899,399.310903933128,399.74577723726,
400.181503236126,400.617229234991,401.052102538934,401.486975842787,401.921849146551,
402.356722450231,402.791595753827,403.226469057342,403.66134236078,404.096215664142,
404.531088967432,404.965962270651,405.400835573804,405.835708876892,406.270582179918,
406.705455482886,407.141181481189,407.576907479491,408.01178078235,408.446654085157,
408.881527387917,409.316400690633,409.751273993306,410.186147295941,410.62102059854,
411.055893901106,411.490767203642,411.925640506151,412.360513808636,412.795387111099,
413.230260413545,413.665133715976,414.100859714032,414.536585712088,414.971459014498,
415.406332316901,415.841205619301,416.276078921702,416.710952224105,417.145825526515,
417.580698828933,418.015572131364,418.45044543381,418.885318736273,419.320192038758,
419.755065341267,420.189938643803,420.624811946369,421.060537944515,421.496263942662,
421.931137245297,422.36601054797,422.800883850686,423.235757153446,423.670630456253,
424.105503759112,424.540377062023,424.975250364991,425.410123668017,425.844996971105,
426.279870274258,426.714743577477,427.149616880767,427.584490184129,428.020216182695,
428.455942181261,428.890815484776,429.325688788373,429.760562092052,430.195435395816,
430.630308699669,431.065182003612,431.500055307649,431.93492861178,432.36980191601,
432.80467522034,433.239548524772,433.674421829309,434.109295133952,434.544168438705,
434.979894437984,435.415620437262,435.850493742239,436.285367047331,436.72024035254,
437.155113657869,437.589986963318,438.024860268889,438.459733574586,438.894606880409,
439.32948018636,439.76435349244,440.199226798651,440.634100104995,441.068973411473,
441.503846718087,441.939572718309,442.375298718531,442.810172025419,443.245045332447,
443.679918639614,444.114791946923,444.549665254374,444.984538561969,445.419411869708,
445.854285177591,446.289158485621,446.724031793796,447.158905102119,447.593778410589,
448.028651719207,448.463525027973,448.899251029277,449.334977030581,449.769850339644,
450.639596958216,451.074470267725,451.509343577383,451.944216887189,452.379090197143,
452.813963507244,453.248836817493,453.683710127889,454.118583438431,454.553456749117,
454.988330059949,455.423203370923,455.858929373329,456.294655375734,456.729528686993,
457.164401998391,457.599275309929,458.469021933414,458.90389524536,459.338768557437,
459.773641869646,460.208515181983,460.643388494447,461.078261807036,461.948008432578,
462.818607748906,463.689207065461,464.55895369214,465.428700319234,466.298446946716,
467.16819357456,468.037940202737,468.907686831215,469.778286149605,470.648885468116,
471.518632097196,472.388378726451,473.258125355841,474.127871985322,474.997618614851,
475.86736524438,476.737964563343,477.608563882265,478.478310511593,479.348057140765,
480.217803769743,481.087550398488,481.957297026966,482.827043655142,483.697642972895,
484.568242290469,485.43798891776,486.307735544649,487.177482171112,488.047228797125,
488.916975422667,489.78672204772,490.657321363009,491.09304736596,491.527920678038,
492.397667301793,493.267413925005,494.137160547663,494.57203385878,495.006907169755,
495.441780480586,495.876653791273,496.311527101814,496.74640041221,497.616999724357,
498.052725726255,498.487599036209,498.922472346015,499.357345655673,499.792218965182,
500.227092274542,500.661965583754,501.096838892816,501.531712201731,501.966585510497,
502.401458819114,502.836332127584,503.271205435907,503.706078744082,504.140952052112,
504.576678052901,505.01240405369,505.447277361429,505.882150669023,506.317023976474,
506.751897283783,507.186770590951,507.621643897978,508.056517204866,508.491390511616,
508.92626381823,509.361137124708,509.796010431052,510.230883737263,510.665757043344,
511.100630349294,511.536356349053,511.972082348811,512.406955654506,512.841828960076,
513.276702265523,513.711575570849,514.146448876056,514.581322181146,515.016195486121,
515.451068790983,515.885942095733,516.320815400375,516.75568870491,517.19056200934,
517.625435313668,518.060308617896,518.496034616807,518.931760615718,519.366633919752,
519.801507223694,520.236380527545,520.671253831307,521.106127134985,521.541000438579,
521.975873742092,522.410747045528,522.845620348888,523.280493652176,523.715366955394,
524.150240258545,524.585113561631,525.019986864656,525.455712862985,525.891438861313,
526.326312164223,526.761185467079,527.196058769885,527.630932072643,528.065805375356,
528.500678678029,528.935551980661,529.370425283258,529.805298585822,530.240171888356,
530.675045190863,531.109918493346,531.544791795808,531.979665098252,532.415391096312,
532.851117094373,533.285990396789,533.720863699197,534.155737001598,534.590610303997,
535.025483606395,535.460356908796,535.895230211204,536.330103513621,536.764976816049,
537.199850118493,537.634723420955,538.069596723438,538.504470025945,538.93934332848,
539.375069326608,539.810795324736,540.245668627333,540.680541929966,541.115415232637,
541.550288535351,541.985161838109,542.420035140915,542.854908443771,543.28978174668,
543.724655049646,544.15952835267,544.594401655757,545.029274958907,545.464148262125,
545.899021565413,546.334747563939,546.770473562465,547.205346865901,547.640220169415,
548.075093473009,548.509966776686,548.944840080449,549.3797133843,549.814586688241,
550.249459992276,550.684333296405,551.119206600633,551.554079904961,551.988953209391,
552.423826513926,552.858699818567,553.294425817789,553.73015181701,554.165025121872,
554.599898426846,555.034771731937,555.469645037144,555.90451834247,556.339391647917,
556.774264953487,557.209138259182,557.644011565003,558.078884870951,558.51375817703,
558.948631483239,559.383504789581,559.818378096058,560.254104096209,560.689830096361,
561.12470340311,561.559576709996,561.994450017021,562.429323324187,562.864196631494,
563.299069938943,563.733943246536,564.168816554273,564.603689862154,565.038563170182,
565.473436478355,565.908309786676,566.343183095144,566.77805640376,567.213782404988,
567.649508406216,568.084381715128,568.519255024189,568.954128333399,569.389001642757,
569.823874952264,570.258748261921,570.693621571725,571.128494881677,571.563368191777,
572.433114812417,572.867988122957,573.302861433642,573.737734744471,574.173460746804,
574.609186749136,575.044060060251,575.913806682904,576.783553306113,577.218426617922,
577.653299929865,578.08817324194,578.523046554147,579.392793178944,580.26253980424,
581.13313912039,581.568865123709,582.003738436771,582.87348506323,583.743231690115,
584.612978317402,585.482724945065,586.352471573076,587.222218201403,588.092817519691,
588.963416838109,589.833163467083,590.702910096251,591.572656725575,592.442403355013,
593.31214998452,594.181896614051,595.05249593303,595.92309525198,596.792841881366,
597.662588510618,598.532335139693,599.402081768556,600.271828397167,601.141575025495,
602.012174343369,602.882773661074,603.752520288553,604.622266915642,605.492013542317,
606.361760168553,607.23150679433,608.101253419626,608.971852735101,609.842452050322,
610.71219867434,611.581945297822,612.451691920754,612.886565232011,613.321438543126,
613.756311854099,614.191185164928,615.060931786153,615.931531098516,616.367257100486,
616.802130410586,617.237003720538,617.671877030342,618.106750339998,618.541623649505,
618.976496958863,619.411370268073,619.846243577134,620.281116886046,620.71599019481,
621.150863503426,621.585736811894,622.020610120214,622.455483428388,622.891209429248,
623.326935430108,623.761808737989,624.196682045726,624.631555353319,625.066428660769,
625.501301968075,625.936175275241,626.371048582266,626.805921889153,627.240795195901,
627.675668502512,628.110541808988,628.54541511533,628.98028842154,629.415161727618,
629.850887727438,630.286613727259,630.72148703308,631.156360338774,631.591233644344,
632.026106949791,632.460980255118,632.895853560325,633.330726865415,633.76560017039,
634.200473475251,634.635346780002,635.070220084644,635.505093389179,635.939966693609,
636.374839997937,636.810565996897,637.246291995857,637.681165299986,638.116038604021,
638.550911907962,638.985785211813,639.420658515576,639.855531819253,640.290405122847,
640.725278426361,641.160151729796,641.595025033157,642.029898336444,642.464771639662,
642.899644942813,643.334518245899,643.770244244257,644.205970242616,644.640843545581,
645.075716848491,645.510590151347,645.945463454153,646.380336756911,646.815210059625,
647.250083362296,647.684956664929,648.119829967526,648.55470327009,648.989576572624,
649.424449875131,649.859323177614,650.294196480076,650.729922478144,651.165648476212,
651.600521778641,652.035395081057,652.470268383465,652.905141685866,653.340014988265,
653.774888290663,654.209761593065,654.644634895472,655.079508197889,655.514381500318,
655.949254802762,656.384128105224,656.819001407706,657.253874710213,657.689600708326,
658.12532670644,658.560200009004,658.995073311601,659.429946614234,659.864819916905,
660.299693219619,660.734566522377,661.169439825183,661.604313128039,662.039186430948,
662.474059733914,662.908933036938,663.343806340025,663.778679643175,664.213552946393,
664.649278944883,665.085004943373,665.519878246733,665.954751550169,666.389624853683,
666.824498157277,667.259371460954,667.694244764717,668.129118068568,668.563991372509,
668.998864676544,669.433737980674,669.868611284901,670.303484589229,670.738357893659,
671.173231198194,671.608957197361,672.044683196528,672.479556501278,672.91442980614,
673.349303111115,673.784176416205,674.219049721412,674.653923026738,675.088796332185,
675.523669637755,675.95854294345,676.393416249271,676.82828955522,677.263162861298,
677.698036167508,678.13290947385,678.568635473934,679.004361474018,679.439234780629,
679.874108087377,680.308981394264,680.743854701289,681.178728008455,681.613601315762,
682.048474623211,682.483347930804,682.91822123854,683.353094546422,683.78796785445,
684.222841162623,684.657714470944,685.092587779412,685.528313780566,685.96403978172,
686.398913090483,686.833786399396,687.268659708457,687.703533017666,688.138406327025,
688.573279636532,689.008152946187,689.443026255992,689.877899565944,690.312772876043,
690.74764618629,691.182519496684,691.617392807224,692.052266117909,692.487992120169,
692.92371812243,693.358591433403,694.228338055774,694.663211367171,695.098084678707,
695.532957990379,695.967831302188,696.402704614131,696.837577926207,697.707324550749,
698.577071175797,699.011944488507,699.447670491767,699.883396495028,700.318269807975,
701.188016434211,702.057763060886,702.927509687976,703.797256315454,704.667002943295,
705.536749571467,706.407348889651,707.277948207973,708.147694836835,709.017441465911,
709.887188095163,710.756934724548,711.626681354026,712.496427983551,713.367027302543,
714.237626621516,715.107373250954,715.977119880277,716.846866509446,717.716613138419,
718.586359767161,719.456106395635,720.32670571363,721.197305031464,722.067051659126,
722.936798286414,723.806544913299,724.676291539758,725.546038165767,726.415784791305,
727.286384106969,728.156983422381,729.026730046663,729.896476670415,730.331349982088,
730.766223293624,731.201096605021,731.635969916278,732.505716538366,733.37546315988,
733.81033647042,734.246062472462,734.681788474505,735.116661784752,735.551535094852,
735.986408404804,736.421281714608,736.856155024264,737.291028333771,737.72590164313,
738.160774952339,738.5956482614,739.030521570312,739.465394879076,739.900268187692,
740.33514149616,740.77001480448,741.205740805414,741.641466806347,742.076340114374,
742.511213422256,742.946086729993,743.380960037585,743.815833345035,744.250706652341,
744.685579959507,745.120453266533,745.555326573419,745.990199880167,746.425073186778,
746.859946493254,747.294819799596,747.729693105806,748.165419105691,748.601145105576,
749.036018411525,749.470891717346,749.90576502304,750.34063832861,750.775511634057,
751.210384939384,751.645258244591,752.080131549682,752.515004854656,752.949878159518,
753.384751464269,753.81962476891,754.254498073445,754.689371377875,755.125097376885,
755.560823375895,755.995696680123,756.430569984253,756.865443288287,757.300316592228,
757.735189896079,758.170063199842,758.604936503519,759.039809807113,759.474683110627,
759.909556414062,760.344429717423,760.779303020711,761.214176323929,761.649049627079,
762.084775625469,762.520501623858,762.955374926883,763.390248229848,763.825121532758,
764.259994835614,764.694868138419,765.129741441178,765.564614743891,765.999488046563,
766.434361349196,766.869234651793,767.304107954357,767.738981256891,768.173854559398,
768.608727861881,769.044453859958,769.480179858035,769.915053160479,770.349926462907,
770.784799765324,771.219673067731,771.654546370133,772.089419672531,772.52429297493,
772.959166277331,773.394039579739,773.828912882155,774.263786184584,774.698659487028,
775.13353278949,775.568406091973,776.004132090072,776.439858088172,776.874731390706,
777.30960469327,777.744477995867,778.1793512985,778.614224601171,779.049097903885,
779.483971206643,779.918844509449,780.353717812305,780.788591115215,781.22346441818,
781.658337721205,782.093211024291,782.528084327442,782.963810325897,783.399536324352,
783.834409627639,784.269282931,784.704156234435,785.139029537949,785.573902841543,
786.00877614522,786.443649448983,786.878522752834,787.313396056775,787.74826936081,
788.183142664939,788.618015969167,789.052889273495,789.487762577925,789.923488577038,
790.359214576152,790.794087880793,791.228961185544,791.663834490406,792.098707795381,
792.533581100471,792.968454405678,793.403327711004,793.838201016451,794.273074322021,
794.707947627716,795.142820933537,795.577694239486,796.012567545564,796.447440851774,
796.883166851791,797.318892851808,797.753766158284,798.188639464895,798.623512771643,
799.058386078529,799.493259385555,799.92813269272,800.363006000027,800.797879307477,
801.232752615069,801.667625922806,802.102499230688,802.537372538715,802.972245846889,
803.40711915521,803.84284515629,804.27857115737,804.713444465985,805.148317774749,
805.583191083662,806.018064392723,806.452937701933,806.887811011291,807.322684320798,
808.192430940258,808.62730425021,809.06217756031,809.497050870557,809.931924180951,
810.36679749149,810.802523493679,811.238249495867,811.673122806697,812.542869428785,
812.977742740041,813.412616051438,813.847489362974,814.282362674646,814.717235986455,
815.152109298398,816.021855922681,816.891602547478,817.326475860065,817.762201863265,
818.197927866466,818.632801179295,819.502547805304,820.372294431763,821.242041058648,
822.111787685935,822.981534313598,823.851280941609,824.721880259681,825.5924795779,
826.462226206642,827.331972835616,828.201719464785,829.071466094109,829.941212723546,
830.810959353053,831.681558672047,832.552157991036,833.421904620514,834.2916512499,
835.161397879151,836.031144508226,836.900891137089,837.770637765701,838.641237083811,
839.511836401767,840.381583029608,841.251329657086,842.121076284176,842.990822910851,
843.860569537087,844.730316162863,845.600915478712,846.471514794314,847.341261418855,
848.211008042874,848.645881354683,849.080754666356,849.515627977891,849.950501289288,
850.82024791166,851.689994533462,852.124867844147,852.560593846263,852.996319848379,
853.431193158772,853.866066469019,854.300939779119,855.170686398875,855.605559708531,
856.040433018038,856.475306327397,856.910179636606,857.345052945667,857.77992625458,
858.214799563344,858.64967287196,859.084546180427,859.520272181434,859.95599818244,
860.390871490614,860.825744798641,861.260618106523,861.69549141426,862.130364721852,
862.565238029302,863.000111336609,863.434984643774,863.8698579508,864.304731257686,
864.739604564434,865.174477871045,865.609351177521,866.044224483863,866.479950483814,
866.915676483765,867.350549789843,867.785423095792,868.220296401613,868.655169707307,
869.090043012877,869.524916318325,869.959789623651,870.394662928858,870.829536233948,
871.264409538923,871.699282843785,872.134156148535,872.569029453177,873.003902757712,
873.439628756773,873.875354755834,874.310228060162,874.745101364389,875.179974668519,
875.614847972553,876.049721276495,876.484594580346,876.919467884108,877.354341187786,
877.78921449138,878.224087794893,878.658961098329,879.093834401689,879.528707704977,
879.963581008195,880.399307006616,880.835033005038,881.269906308124,881.704779611148,
882.139652914114,882.574526217024,883.00939951988,883.444272822685,883.879146125444,
884.314019428157,884.748892730829,885.183766033462,885.618639336059,886.053512638623,
886.488385941157,886.923259243664,887.358985241751,887.794711239839,888.2295845423,
888.664457844744,889.099331147173,889.534204449589,889.969077751997,890.403951054398,
890.838824356797,891.273697659195,891.708570961597,892.143444264004,892.578317566421,
893.01319086885,893.448064171293,893.882937473755,894.318663471843,894.75438946993,
895.189262772437,895.624136074971,896.059009377535,896.493882680132,896.928755982765,
897.363629285437,897.798502588151,898.233375890909,898.668249193715,899.103122496571,
899.53799579948,899.972869102446,900.40774240547,900.842615708556,901.278341706978,
901.714067705399,902.148941008617,902.583814311905,903.018687615265,903.453560918701,
903.888434222214,904.323307525808,904.758180829485,905.193054133248,905.627927437099,
906.06280074104,906.497674045075,906.932547349205,907.367420653433,907.80229395776,
908.238019956821,908.673745955883,909.108619260417,909.543492565059,909.978365869809,
910.413239174671,910.848112479646,911.282985784736,911.717859089943,912.152732395269,
912.587605700716,913.022479006287,913.457352311981,913.892225617802,914.327098923751,
914.761972229829,915.19769822978,915.633424229731,916.068297536072,916.503170842548,
916.93804414916,917.372917455908,917.807790762794,918.24266406982,918.677537376985,
919.112410684292,919.547283991742,919.982157299334,920.417030607071,920.851903914953,
921.28677722298,921.721650531154,922.15737653216,922.593102533167,923.027975841635,
923.46284915025,923.897722459014,924.332595767926,924.767469076987,925.202342386197,
925.637215695556,926.072089005063,926.506962314719,926.941835624523,927.376708934475,
927.811582244575,928.246455554822,928.681328865215,929.117054867331,929.987654180132,
930.422527490961,930.857400801934,931.292274113049,931.727147424306,932.162020735703,
932.596894047238,933.46664067072,934.336387294739,934.771260606945,935.20613391928,
935.641007231742,936.076733234882,936.94733255073,937.817079176507,938.686825802743,
939.556572429418,940.426319056508,941.296065683986,942.165812311827,943.036411629783,
943.907010947893,944.776757576505,945.646504205367,946.516250834443,947.385997463694,
948.25574409308,949.125490722558,949.996090041546,950.86668936054,951.736435990048,
952.606182619485,953.475929248809,954.345675877978,955.215422506951,956.085169135693,
956.955768453912,957.826367771985,958.696114399995,959.565861027658,960.435607654946,
961.305354281831,962.175100908289,963.044847534298,963.915446850328,964.786046166116,
965.655792790913,966.525539415195,966.960412727138,967.395286038947,968.265032662155,
969.134779284809,969.569652595924,970.004525906897,970.439399217726,970.875125219914,
971.310851222103,971.745724532643,972.615471153283,973.485217773335,973.920091083139,
974.354964392795,974.789837702302,975.22471101166,975.65958432087,976.094457629931,
976.529330938844,976.964204247608,977.399077556223,977.834803557303,978.270529558383,
978.705402866704,979.140276174877,979.575149482905,980.010022790786,980.444896098523,
980.879769406116,981.314642713565,981.749516020872,982.184389328038,982.619262635063,
983.05413594195,983.489009248698,983.923882555309,984.358755861785,984.794481861802,
985.230207861819,985.665081168029,986.099954474107,986.534827780056,986.969701085877,
987.404574391571,987.839447697141,988.274321002589,988.709194307915,989.144067613122,
989.578940918212,990.013814223187,990.448687528048,990.883560832799,991.31843413744,
991.754160136554,992.189886135667,992.624759440097,993.059632744425,993.494506048653,
993.929379352783,994.364252656817,994.799125960758,995.233999264609,995.668872568372,
996.103745872049,996.538619175643,996.973492479157,997.408365782593,997.843239085953,
998.278112389241,998.713838387696,999.149564386151,999.584437689301,1000.01931099239,
1000.45418429541,1000.88905759838,1001.32393090129,1001.75880420414,1002.19367750695,
1002.62855080971,1003.06342411242,1003.49829741509,1003.93317071773,1004.36804402032,
1004.80291732289,1005.23779062542,1005.67351662352,1006.10924262162,1006.5441159241,
1006.97898922656,1007.41386252901,1007.84873583144,1008.28360913385,1008.71848243626,
1009.15335573866,1009.58822904106,1010.02310234346,1010.45797564586,1010.89284894827,
1011.32772225069,1011.76259555311,1012.19746885556,1012.63319485364,1013.06892085171,
1013.5037941542,1013.9386674567,1014.37354075924,1014.8084140618,1015.2432873644,
1015.67816066703,1016.1130339697,1016.54790727242,1016.98278057517,1017.41765387798,
1017.85252718084,1018.28740048375,1018.72227378671,1019.15714708974,1019.59287308813,
1020.02859908651,1020.46347238967,1020.89834569288,1021.33321899617,1021.76809229953,
1022.20296560297,1022.63783890648,1023.07271221007,1023.50758551375,1023.94245881752,
1024.37733212137,1024.81220542531,1025.24707872935,1025.68195203348,1026.11682533771,
1026.55255133672,1026.98827733573,1027.42315064016,1027.8580239447,1028.29289724934,
1028.72777055409,1029.16264385896,1029.59751716393,1030.03239046902,1030.46726377423,
1030.90213707956,1031.33701038501,1031.77188369058,1032.20675699628,1032.6416303021,
1033.07650360805,1033.51222960793,1033.94795560782,1034.38282891403,1034.81770222038,
1035.25257552685,1035.68744883347,1036.12232214022,1036.5571954471,1036.99206875413,
1037.4269420613,1037.86181536861,1038.29668867606,1038.73156198365,1039.16643529139,
1039.60130859927,1040.0361819073,1040.47190790824,1040.90763390917,1041.34250721749,
1041.77738052596,1042.21225383458,1042.64712714334,1043.08200045226,1043.95174707053,
1044.38662037989,1044.8214936894,1045.25636699906,1045.69124030886,1046.12611361882,
1046.56098692892,1046.99586023917,1047.43158624121,1047.86731224325,1048.3021855538,
1048.73705886448,1049.17193217531,1049.60680548629,1050.0416787974,1050.47655210866,
1050.91142542006,1051.78117204327,1052.21604535508,1052.65091866703,1053.0857919791,
1053.52066529131,1053.95553860365,1054.39126460673,1055.26186392239,1056.13161054793,
1057.00135717395,1057.43623048712,1057.87110380041,1058.7408504273,1059.61059705459,
1060.48034368225,1061.35094300009,1062.22154231809,1063.09128894656,1063.96103557531,
1064.83078220429,1065.70052883346,1066.57027546278,1067.44002209222,1068.3106214112,
1069.18122073019,1070.05096735972,1070.9207139892,1071.79046061859,1072.66020724785,
1073.52995387693,1074.39970050579,1075.27029982411,1076.1408991423,1077.01064577048,
1077.88039239832,1078.7501390258,1079.61988565289,1080.48963227957,1081.35937890581,
1082.22997822202,1083.100577538,1083.97032416305,1084.84007078759,1085.70981741161,
1086.5795640351,1087.44931065803,1087.88418396929,1088.31905728041,1088.75393059138,
1089.18965659365,1089.62538259591,1090.06025590659,1090.93000252753,1091.36487583778,
1091.79974914788,1092.23462245783,1092.66949576764,1093.1043690773,1093.5392423868,
1093.97411569616,1094.40898900538,1094.84386231444,1095.27873562335,1095.71360893212,
1096.14933493327,1096.58506093443,1097.0199342429,1097.45480755122,1097.88968085939,
1098.32455416742,1098.75942747531,1099.19430078305,1099.62917409064,1100.06404739809,
1100.4989207054,1100.93379401257,1101.36866731959,1101.80354062648,1102.23841393323,
1102.67328723984,1103.10901323993,1103.54473924001,1103.97961254636,1104.41448585257,
1104.84935915865,1105.2842324646,1105.71910577042,1106.15397907612,1106.58885238169,
1107.02372568714,1107.45859899246,1107.89347229767,1108.32834560276,1108.76321890774,
1109.1980922126,1109.63296551736,1110.06869151652,1110.50441751569,1110.93929082023,
1111.37416412466,1111.80903742899,1112.24391073322,1112.67878403735,1113.11365734139,
1113.54853064533,1113.98340394918,1114.41827725295,1114.85315055662,1115.28802386022,
1115.72289716374,1116.15777046717,1116.59264377053,1117.02836976903,1117.46409576752,
1117.89896907074,1118.33384237389,1118.76871567698,1119.20358898,1119.63846228297,
1120.07333558588,1120.50820888874,1120.94308219154,1121.3779554943,1121.81282879702,
1122.24770209969,1122.68257540233,1123.11744870492,1123.55232200749,1123.98804800561,
1124.42377400372,1124.85864730623,1125.29352060871,1125.72839391118,1126.16326721362,
1126.59814051605,1127.03301381847,1127.46788712088,1127.90276042328,1128.33763372568,
1128.77250702808,1129.20738033048,1129.64225363289,1130.07712693531,1130.51200023774,
1130.94772623581,1131.38345223388,1131.81832553634,1132.25319883883,1132.68807214134,
1133.12294544387,1133.55781874644,1133.99269204904,1134.42756535167,1134.86243865434,
1135.29731195706,1135.73218525982,1136.16705856263,1136.60193186548,1137.03680516839,
1137.47167847136,1137.90740446972,1138.34313046808,1138.77800377117,1139.21287707432,
1139.64775037754,1140.08262368083,1140.51749698419,1140.95237028763,1141.38724359114,
1141.82211689474,1142.25699019842,1142.69186350218,1143.12673680603,1143.56161010998,
1143.99648341401,1144.43135671814,1144.86708271711,1145.30280871607,1145.7376820204,
1146.17255532483,1146.60742862936,1147.04230193401,1147.47717523876,1147.91204854362,
1148.3469218486,1148.78179515369,1149.2166684589,1149.65154176423,1150.08641506968,
1150.52128837525,1150.95616168094,1151.39103498677,1151.82676098659,1152.26248698641,
1152.69736029249,1153.1322335987,1153.56710690504,1154.00198021152,1154.43685351813,
1154.87172682488,1155.30660013177,1155.7414734388,1156.17634674597,1156.61122005327,
1157.04609336073,1157.48096666832,1157.91583997606,1158.35071328394,1158.7864392848,
1159.22216528566,1159.65703859384,1160.09191190216,1160.52678521063,1160.96165851925,
1161.39653182801,1161.83140513693,1162.26627844599,1162.7011517552,1163.13602506456,
1163.57089837407,1164.00577168373,1164.44064499353,1164.87551830349,1165.74611761556,
1166.18184361753,1166.61671692792,1167.05159023846,1167.48646354915,1167.92133685998,
1168.35621017096,1169.22595679333,1170.09570341627,1170.53057672794,1170.96545003975,
1171.4003233517,1171.83519666377,1172.27006997598,1172.705795979,1173.57639529447,
1174.44614191977,1174.8810152326,1175.31588854555,1176.18563517179,1177.05538179847,
1177.92512842556,1178.79487505304,1179.66547437075,1180.53607368863,1181.40582031696,
1182.27556694557,1183.14531357444,1184.01506020352,1184.88480683277,1185.75455346216,
1186.62515278112,1187.4957521001,1188.36549872963,1189.23524535914,1190.10499198858,
1190.97473861791,1191.84448524708,1192.71423187606,1193.58483119448,1194.45543051277,
1195.3251771411,1196.19492376911,1197.06467039678,1197.93441702407,1198.80416365096,
1199.67391027742,1200.5445095938,1201.41510890996,1202.28485553525,1203.15460216005,
1204.02434878434,1204.89409540809,1205.76384203131,1206.1987153427,1206.63358865396,
1207.06846196508,1207.50418796741,1208.37478728058,1209.2445339018,1209.6794072122,
1210.11428052245,1210.54915383255,1210.9840271425,1211.41890045231,1211.85377376197,
1212.28864707147,1212.72352038083,1213.15839369005,1213.59326699911,1214.02814030802,
1214.46386630925,1214.89959231048,1215.3344656191,1215.76933892757,1216.20421223589,
1216.63908554406,1217.07395885209,1217.50883215998,1217.94370546771,1218.37857877531,
1218.81345208276,1219.24832539007,1219.68319869724,1220.11807200426,1220.55294531115,
1220.9878186179,1221.42354461805,1221.85927061821,1222.29414392468,1222.72901723103,
1223.16389053724,1223.59876384332,1224.03363714927,1224.46851045509,1224.90338376079,
1225.33825706636,1225.77313037181,1226.20800367713,1226.64287698234,1227.07775028743,
1227.51262359241,1227.94749689727,1228.3832228965,1228.81894889572,1229.25382220036,
1229.6886955049,1230.12356880933,1230.55844211366,1230.99331541789,1231.42818872202,
1231.86306202606,1232.29793533,1232.73280863385,1233.16768193762,1233.60255524129,
1234.03742854489,1234.4723018484,1234.90717515184,1235.34290115037,1235.7786271489,
1236.21350045219,1236.64837375541,1237.08324705856,1237.51812036165,1237.95299366467,
1238.38786696764,1238.82274027055,1239.25761357341,1239.69248687621,1240.12736017897,
1240.56223348169,1240.99710678436,1241.431980087,1241.8668533896,1242.30257938773,
1242.73830538585,1243.17317868839,1243.6080519909,1244.04292529338,1244.47779859585,
1244.91267189829,1245.34754520072,1245.78241850314,1246.21729180555,1246.65216510795,
1247.08703841035,1247.52191171275,1247.95678501515,1248.39165831756,1248.82653161998,
1249.26225761804,1249.69798361611,1250.13285691855,1250.56773022101,1251.0026035235,
1251.43747682601,1251.87235012854,1252.30722343111,1252.74209673371,1253.17697003634,
1253.61184333901,1254.04671664173,1254.48158994449,1254.9164632473,1255.35133655015,
1255.78620985306,1256.22193585139,1256.65766184973,1257.09253515275,1257.52740845584,
1257.96228175899,1258.39715506221,1258.8320283655,1259.26690166886,1259.7017749723,
1260.13664827581,1260.57152157941,1261.00639488309,1261.44126818685,1261.8761414907,
1262.31101479465,1262.74588809868,1263.1816140976,1263.61734009651,1264.05221340074,
1264.48708670507,1264.9219600095,1265.35683331403,1265.79170661868,1266.22657992343,
1266.66145322829,1267.09632653327,1267.53119983836,1267.96607314357,1268.4009464489,
1268.83581975434,1269.27069305992,1269.70556636561,1270.14129236537,1270.57701836513,
1271.01189167108,1271.44676497716,1271.88163828337,1272.31651158971,1272.75138489619,
1273.1862582028,1273.62113150955,1274.05600481644,1274.49087812347,1274.92575143063,
1275.36062473794,1275.79549804539,1276.23037135299,1276.66524466073,1277.10097066151,
1277.5366966623,1277.97156997033,1278.40644327851,1278.84131658683,1279.2761898953,
1279.71106320392,1280.14593651268,1280.5808098216,1281.01568313066,1281.45055643987,
1281.88542974923,1282.32030305874,1282.75517636839,1283.1900496782,1283.62492298815,
1284.06064899005,1284.49637499195,1284.9312483022,1285.36612161259,1285.80099492313,
1286.23586823382,1286.67074154465,1287.54048816674,1287.975361478,1288.4102347894,
1288.84510810093,1289.27998141261,1289.71485472442,1290.14972803636,1291.02032735139,
1291.89092666668,1292.32579997914,1292.76067329173,1293.19554660444,1293.63041991727,
1294.50016654328,1295.36991316974,1296.23965979663,1297.10940642392,1297.9800057415,
1298.85060505925,1299.72035168742,1300.5900983159,1301.45984494464,1302.32959157362,
1303.19933820279,1304.06908483212,1304.93968415104,1305.81028347,1306.68003009953,
1307.54977672906,1308.41952335854,1309.28926998793,1310.15901661718,1311.02876324626,
1311.89936256477,1312.76996188316,1313.63970851164,1314.50945513981,1315.37920176765,
1316.24894839514,1317.11869502223,1317.98844164891,1318.85904096546,1319.72964028179,
1320.59938690733,1321.46913353238,1322.33888015692,1323.20862678095,1323.64350009276,
1324.07837340443,1324.51324671597,1324.94812002737,1325.81871934103,1326.68931865441,
1327.12419196524,1327.55906527593,1327.99393858647,1328.42881189686,1328.86368520711,
1329.29855851721,1329.73343182716,1330.16830513697,1330.60317844663,1331.03805175614,
1331.4729250655,1331.90779837471,1332.34267168377,1332.77839768507,1333.21412368638,
1333.64899699514,1334.08387030376,1334.51874361223,1334.95361692055,1335.38849022873,
1335.82336353676,1336.25823684464,1336.69311015238,1337.12798345997,1337.56285676742,
1337.99773007473,1338.4326033819,1338.86747668892,1339.30234999581,1339.73807599603,
1340.17380199625,1340.60867530287,1341.04354860934,1341.47842191569,1341.9132952219,
1342.34816852798,1342.78304183393,1343.21791513975,1343.65278844545,1344.08766175102,
1344.52253505647,1344.95740836179,1345.392281667,1345.82715497209,1346.26202827707,
1346.69775427635,1347.13348027563,1347.56835358038,1348.00322688502,1348.43810018956,
1348.87297349399,1349.30784679832,1349.74272010255,1350.17759340668,1350.61246671072,
1351.04734001466,1351.48221331851,1351.91708662228,1352.35195992595,1352.78683322955,
1353.22170653306,1353.65743253163,1354.09315853019,1354.52803183356,1354.96290513685,
1355.39777844007,1355.83265174322,1356.26752504631,1356.70239834933,1357.1372716523,
1357.57214495521,1358.00701825807,1358.44189156087,1358.87676486363,1359.31163816635,
1359.74651146902,1360.18138477166,1360.6171107698,1361.05283676795,1361.48771007051,
1361.92258337305,1362.35745667556,1362.79232997804,1363.2272032805,1363.66207658295,
1364.09694988538,1364.5318231878,1364.96669649021,1365.40156979261,1365.83644309501,
1366.27131639741,1366.70618969981,1367.14106300222,1367.57678900028,1368.01251499834,
1368.44738830077,1368.88226160321,1369.31713490567,1369.75200820816,1370.18688151067,
1370.6217548132,1371.05662811577,1371.49150141837,1371.926374721,1372.36124802367,
1372.79612132639,1373.23099462915,1373.66586793196,1374.10074123481,1374.53646723311,
1374.97219323142,1375.40706653438,1375.84193983741,1376.2768131405,1376.71168644365,
1377.14655974687,1377.58143305016,1378.01630635352,1378.45117965696,1378.88605296047,
1379.32092626407,1379.75579956775,1380.19067287151,1380.62554617536,1381.06041947931,
1381.49614547817,1381.93187147704,1382.36674478117,1382.8016180854,1383.23649138973,
1383.67136469416,1384.10623799869,1384.54111130334,1384.97598460809,1385.41085791295,
1385.84573121793,1386.28060452302,1386.71547782823,1387.15035113356,1387.585224439,
1388.02009774458,1388.45582374427,1388.89154974397,1389.32642304979,1389.76129635574,
1390.19616966182,1390.63104296803,1391.06591627437,1391.50078958085,1391.93566288746,
1392.37053619421,1392.8054095011,1393.24028280813,1393.6751561153,1394.1100294226,
1394.54490273005,1394.97977603765,1395.41550203836,1395.85122803908,1396.28610134696,
1396.72097465499,1397.15584796317,1397.59072127149,1398.02559457996,1398.46046788858,
1398.89534119734,1399.33021450626,1399.76508781532,1400.19996112453,1400.63483443389,
1401.50458105306,1401.93945436286,1402.37518036469,1402.81090636651,1403.24577967661,
1403.68065298686,1404.11552629725,1404.5503996078,1404.98527291848,1405.85501954029,
1406.2898928514,1406.72476616266,1407.15963947406,1407.5945127856,1408.02938609727,
1408.46425940908,1409.33485872391,1410.205458039,1410.64033135134,1411.07520466381,
1411.51007797639,1411.9449512891,1412.81469791488,1413.68444454112,1414.5541911678,
1415.42393779489,1416.29453711233,1417.16513642995,1418.03488305796,1418.90462968629,
1419.77437631491,1420.64412294377,1421.51386957285,1422.38361620211,1423.25421552099,
1424.12481483992,1424.99456146943,1425.86430809896,1426.73405472847,1427.60380135791,
1428.47354798724,1429.34329461641,1430.21389393501,1431.08449325349,1431.9542398821,
1432.82398651043,1433.69373313844,1434.56347976611,1435.4332263934,1436.30297302029,
1437.17357233701,1438.04417165351,1438.91391827929,1439.78366490459,1440.65341152939,
1441.52315815367,1441.95803146562,1442.39290477743,1442.8277780891,1443.26265140064,
1444.13325071451,1445.00385002811,1445.43872333908,1445.87359664991,1446.3084699606,
1446.74334327114,1447.17821658153,1447.61308989178,1448.48283651184,1448.91770982164,
1449.3525831313,1449.78745644081,1450.22232975017,1450.65720305938,1451.09292906076,
1451.52865506214,1451.96352837105,1452.39840167982,1452.83327498843,1453.2681482969,
1453.70302160522,1454.1378949134,1454.57276822143,1455.00764152931,1455.44251483705,
1455.87738814464,1456.31226145209,1456.7471347594,1457.18200806657,1457.6168813736,
1458.05260737389,1458.48833337418,1458.92320668093,1459.35807998754,1459.79295329402,
1460.22782660036,1460.66269990657,1461.09757321265,1461.5324465186,1461.96731982443,
1462.40219313012,1462.83706643569,1463.27193974114,1463.70681304647,1464.14168635168,
1464.57655965677,1465.0122856561,1465.44801165544,1465.8828849603,1466.31775826505,
1466.7526315697,1467.18750487423,1467.62237817866,1468.05725148299,1468.49212478722,
1468.92699809135,1469.36187139539,1469.79674469933,1470.23161800319,1470.66649130695,
1471.10136461063,1471.53623791422,1471.97196391283,1472.40768991143,1472.84256321487,
1473.27743651823,1473.71230982152,1474.14718312474,1474.58205642789,1475.01692973098,
1475.451803034,1475.88667633697,1476.32154963988,1476.75642294274,1477.19129624555,
1477.62616954831,1478.06104285102,1478.4959161537,1478.93164215186,1479.36736815002,
1479.80224145262,1480.23711475519,1480.67198805772,1481.10686136023,1481.54173466272,
1481.97660796518,1482.41148126762,1482.84635457005,1483.28122787247,1483.71610117488,
1484.15097447728,1484.58584777968,1485.02072108208,1485.45559438449,1485.89132038254,
1486.32704638059,1486.76191968301,1487.19679298544,1487.63166628788,1488.06653959035,
1488.50141289283,1488.93628619534,1489.37115949787,1489.80603280044,1490.24090610304,
1490.67577940567,1491.11065270835,1491.54552601106,1491.98039931382,1492.41527261663,
1492.8509986149,1493.28672461318,1493.72159791609,1494.15647121906,1494.59134452208,
1495.02621782517,1495.46109112832,1495.89596443154,1496.33083773483,1496.76571103819,
1497.20058434163,1497.63545764515,1498.07033094874,1498.50520425242,1498.94007755618,
1499.37495086004,1499.81067685885,1500.24640285767,1500.68127616171,1501.11614946584,
1501.55102277007,1501.9858960744,1502.42076937883,1502.85564268337,1503.29051598801,
1503.72538929276,1504.16026259762,1504.5951359026,1505.03000920769,1505.4648825129,
1505.89975581823,1506.33462912368,1506.77035512331,1507.20608112294,1507.64095442864,
1508.07582773446,1508.51070104041,1508.94557434649,1509.3804476527,1509.81532095904,
1510.25019426552,1510.68506757213,1511.11994087888,1511.55481418577,1511.9896874928,
1512.42456079996,1512.85943410727,1513.29430741472,1513.73003341537,1514.16575941601,
1514.60063272375,1515.03550603163,1515.47037933966,1515.90525264784,1516.34012595616,
1516.77499926463,1517.20987257325,1517.64474588201,1518.07961919093,1518.51449249999,
1518.9493658092,1519.38423911856,1519.81911242807,1520.25398573772,1520.68971173947,
1521.12543774122,1521.56031105118,1521.99518436128,1522.43005767153,1523.29980429246,
1523.73467760315,1524.16955091398,1524.60442422495,1525.03929753607,1525.47417084733,
1525.90904415873,1526.77879078194,1527.64939009657,1528.08511609939,1528.51998941146,
1528.95486272367,1529.38973603601,1530.25948266106,1531.1292292866,1531.99897591261,
1532.86872253907,1533.73846916596,1534.60906848325,1535.47966780073,1536.34941442858,
1537.21916105675,1538.08890768523,1538.95865431398,1539.82840094295,1540.69814757212,
1541.56874689096,1542.43934620985,1543.30909283933,1544.17883946886,1545.04858609839,
1545.91833272787,1546.78807935726,1547.65782598651,1548.52842530518,1549.39902462375,
1550.26877125249,1551.13851788097,1552.00826450914,1552.87801113699,1553.74775776447,
1554.61750439156,1555.48810370844,1556.35870302511,1557.22844965112,1558.09819627666,
1558.96794290171,1559.83768952626,1560.27256283834,1560.70743615028,1561.57718277377,
1562.44778208785,1563.31838140165,1563.75325471277,1564.18812802374,1564.62300133457,
1565.05787464526,1565.9276212662,1566.79736788655,1567.2322411965,1567.66711450631,
1568.10198781596,1568.53686112547,1568.97173443483,1569.40746043628,1569.84318643774,
1570.2780597468,1570.71293305571,1571.14780636448,1571.5826796731,1572.01755298157,
1572.45242628989,1572.88729959806,1573.32217290609,1573.75704621397,1574.19191952171,
1574.62679282931,1575.06166613676,1575.49653944407,1575.93141275123,1576.36713875159,
1576.80286475195,1577.23773805884,1577.67261136559,1578.1074846722,1578.54235797868,
1578.97723128502,1579.41210459124,1579.84697789732,1580.28185120327,1580.71672450909,
1581.15159781478,1581.58647112036,1582.0213444258,1582.45621773113,1582.89109103634,
1583.32681703573,1583.76254303513,1584.1974163401,1584.63228964497,1585.06716294972,
1585.50203625436,1585.9369095589,1586.37178286333,1586.80665616766,1587.24152947189,
1587.67640277602,1588.11127608005,1588.546149384,1588.98102268785,1589.41589599161,
1589.85076929529,1590.28649529394,1590.72222129258,1591.1570945961,1591.59196789953,
1592.0268412029,1592.46171450619,1592.8965878094,1593.33146111256,1593.76633441564,
1594.20120771867,1594.63608102164,1595.07095432455,1595.50582762741,1595.94070093021,
1596.37557423297,1596.81044753569,1597.24617353387,1597.68189953206,1598.11677283469,
1598.55164613729,1598.98651943985,1599.42139274239,1599.8562660449,1600.29113934738,
1600.72601264985,1601.16088595229,1601.59575925472,1602.03063255714,1602.46550585955,
1602.90037916195,1603.33525246435,1603.77012576675,1604.2058517648,1604.64157776285,
1605.07645106526,1605.51132436768,1605.94619767011,1606.38107097255,1606.81594427502,
1607.2508175775,1607.68569088001,1608.12056418254,1608.55543748511,1608.99031078771,
1609.42518409034,1609.86005739302,1610.29493069573,1610.72980399849,1611.16552999674,
1611.60125599499,1612.03612929785,1612.47100260076,1612.90587590373,1613.34074920675,
1613.77562250984,1614.21049581299,1614.64536911621,1615.0802424195,1615.51511572286,
1615.9499890263,1616.38486232981,1616.81973563341,1617.25460893709,1617.68948224085,
1618.12520823963,1618.5609342384,1618.99580754234,1619.43068084638,1619.86555415051,
1620.30042745474,1620.73530075907,1621.1701740635,1621.60504736804,1622.03992067268,
1622.47479397743,1622.90966728229,1623.34454058727,1623.77941389236,1624.21428719757,
1624.6491605029,1625.08488650247,1625.52061250204,1625.95548580761,1626.39035911331,
1626.82523241913,1627.26010572508,1627.69497903116,1628.12985233737,1628.56472564372,
1628.99959895019,1629.43447225681,1629.86934556356,1630.30421887044,1630.73909217747,
1631.17396548464,1631.60883879195,1632.04456479252,1632.48029079309,1632.91516410068,
1633.35003740842,1633.78491071631,1634.21978402433,1634.65465733251,1635.08953064083,
1635.5244039493,1635.95927725792,1636.39415056668,1636.8290238756,1637.26389718466,
1637.69877049387,1638.13364380323,1638.56851711274,1639.00424311442,1639.43996911609,
1639.8748424259,1640.30971573585,1640.74458904595,1641.6143356666,1642.04920897714,
1642.48408228782,1642.91895559865,1643.35382890963,1643.78870222074,1644.223575532,
1645.09332215494,1645.52819546661,1645.96392146936,1646.39964747212,1646.83452078406,
1647.26939409614,1647.70426740834,1648.57401403314,1649.44376065844,1650.31350728422,
1650.74838059729,1651.18325391046,1652.05300053714,1652.92359985428,1653.79419917162,
1654.66394579929,1655.5336924273,1656.40343905563,1657.27318568424,1658.14293231311,
1659.01267894219,1659.88327826096,1660.75387757982,1661.62362420926,1662.49337083877,
1663.3631174683,1664.23286409781,1665.10261072725,1665.97235735658,1666.84295667531,
1667.71355599396,1668.58330262282,1669.45304925143,1670.32279587976,1671.19254250778,
1672.06228913544,1672.93203576273,1673.80263507977,1674.6732343966,1675.54298102284,
1676.41272764862,1677.28247427392,1678.15222089872,1679.021967523,1679.89171414676,
1680.76231346105,1681.19803946366,1681.63291277506,1682.06778608632,1682.50265939743,
1682.93753270841,1683.37240601924,1684.24215264047,1684.67702595086,1685.11189926111,
1685.54677257121,1685.98164588116,1686.41651919097,1686.85139250063,1687.28626581014,
1687.72199181166,1688.15771781319,1688.5925911224,1689.02746443146,1689.46233774038,
1689.89721104914,1690.33208435776,1690.76695766623,1691.20183097455,1691.63670428272,
1692.07157759075,1692.50645089864,1692.94132420637,1693.37619751397,1693.81107082142,
1694.24594412873,1694.68167012916,1695.11739612959,1695.55226943662,1695.9871427435,
1696.42201605025,1696.85688935687,1697.29176266334,1697.72663596969,1698.1615092759,
1698.59638258198,1699.03125588793,1699.46612919375,1699.90100249945,1700.33587580502,
1700.77074911047,1701.20562241579,1701.64134841525,1702.0770744147,1702.51194771979,
1702.94682102476,1703.38169432963,1703.81656763438,1704.25144093902,1704.68631424356,
1705.12118754799,1705.55606085232,1705.99093415655,1706.42580746068,1706.86068076471,
1707.29555406866,1707.73042737251,1708.16530067627,1708.60102667496,1709.03675267365,
1709.47162597724,1709.90649928076,1710.34137258419,1710.77624588756,1711.21111919085,
1711.64599249406,1712.08086579722,1712.5157391003,1712.95061240333,1713.3854857063,
1713.82035900921,1714.25523231207,1714.69010561487,1715.12497891763,1715.56070491584,
1715.99643091404,1716.43130421671,1716.86617751935,1717.30105082195,1717.73592412451,
1718.17079742705,1718.60567072956,1719.04054403204,1719.4754173345,1719.91029063695,
1720.34516393938,1720.7800372418,1721.21491054421,1721.64978384661,1722.08465714901,
1722.52038314706,1722.9561091451,1723.39098244751,1723.82585574992,1724.26072905233,
1724.69560235476,1725.13047565721,1725.56534895967,1726.00022226216,1726.43509556467,
1726.8699688672,1727.30484216977,1727.73971547236,1728.174588775,1728.60946207767,
1729.04433538039,1729.48006137861,1729.91578737684,1730.35066067965,1730.78553398251,
1731.22040728542,1731.65528058838,1732.09015389141,1732.5250271945,1732.95990049765,
1733.39477380087,1733.82964710416,1734.26452040752,1734.69939371096,1735.13426701447,
1735.56914031807,1736.00401362175,1736.43973962048,1736.8754656192,1737.31033892306,
1737.745212227,1738.18008553104,1738.61495883517,1739.0498321394,1739.48470544373,
1739.91957874816,1740.35445205269,1740.78932535734,1741.22419866209,1741.65907196695,
1742.09394527193,1742.52881857702,1742.96369188223,1743.39941788174,1743.83514388125,
1744.2700171867,1744.70489049227,1745.13976379797,1745.57463710379,1746.00951040974,
1746.44438371582,1746.87925702203,1747.31413032837,1747.74900363485,1748.18387694146,
1748.61875024821,1749.0536235551,1749.48849686213,1749.92337016929,1750.3590961698,
1750.7948221703,1751.22969547775,1751.66456878534,1752.09944209308,1752.53431540096,
1752.96918870899,1753.40406201717,1753.83893532549,1754.27380863396,1754.70868194258,
1755.14355525134,1755.57842856026,1756.01330186932,1756.44817517853,1756.88304848789,
1757.31877448949,1757.75450049109,1758.18937380075,1759.05912042051,1759.49399373061,
1759.92886704086,1760.36374035125,1760.79861366179,1761.23348697248,1761.66836028331,
1762.10323359429,1762.5381069054,1763.40785352806,1763.8427268396,1764.27845284228,
1764.71417884496,1765.14905215677,1765.58392546872,1766.0187987808,1766.88854540534,
1767.75829203039,1768.1931653431,1768.62803865593,1769.06291196888,1769.49778528195,
1770.36753190841,1771.2381312254,1772.10873054259,1772.97847717007,1773.84822379791,
1774.71797042609,1775.58771705456,1776.45746368331,1777.32721031228,1778.19780963089,
1779.06840894783,1779.93815555508,1780.80790201176,1781.67764871408),(-1.76619037915008,
-1.18309518948453),.UNSPECIFIED.) ;
#827 = B_SPLINE_SURFACE_WITH_KNOTS('',1,3,((#79059,#79060,#79061,#79062,#79063,
#79064,#79065,#79066,#79067,#79068,#79069,#79070,#79071,#79072,#79073,#79074),
(#79075,#79076,#79077,#79078,#79079,#79080,#79081,#79082,#79083,#79084,
#79085,#79086,#79087,#79088,#79089,#79090)),.UNSPECIFIED.,.F.,.T.,.F.,(2,
2),(4,1,1,1,1,1,1,1,1,1,1,1,1,4),(0.,0.248609854147285),(0.,0.520304865070705,
0.709542561390409,0.804161409708611,0.898780258026813,1.15893269056541,
1.419085123104,1.67923755563226,1.93938998816052,2.03400883639567,2.12862768463082,
2.31786538114359,2.57801781366682,2.83817024619004),.UNSPECIFIED.) ;
#828 = B_SPLINE_SURFACE_WITH_KNOTS('',1,3,((#79115,#79116,#79117,#79118,#79119,
#79120,#79121,#79122,#79123,#79124,#79125,#79126,#79127,#79128,#79129,#79130),
(#79131,#79132,#79133,#79134,#79135,#79136,#79137,#79138,#79139,#79140,
#79141,#79142,#79143,#79144,#79145,#79146)),.UNSPECIFIED.,.F.,.T.,.F.,(2,
2),(4,1,1,1,1,1,1,1,1,1,1,1,1,4),(0.,0.248609854327075),(0.,0.520304865043955,
0.70954256158844,0.804161409794499,0.898780258000557,1.15893269054429,1.41908512308802,
1.67923755561058,1.93938998813313,2.03400883648099,2.12862768482886,2.3178653810957,
2.57801781365659,2.83817024621747),.UNSPECIFIED.) ;
#829 = B_SPLINE_SURFACE_WITH_KNOTS('',1,3,((#79194,#79195,#79196,#79197,#79198,
#79199,#79200,#79201,#79202,#79203,#79204,#79205,#79206,#79207,#79208,#79209),
(#79210,#79211,#79212,#79213,#79214,#79215,#79216,#79217,#79218,#79219,
#79220,#79221,#79222,#79223,#79224,#79225)),.UNSPECIFIED.,.F.,.T.,.F.,(2,
2),(4,1,1,1,1,1,1,1,1,1,1,1,1,4),(0.,0.248609853678558),(0.,0.520304865114576,
0.709542561608101,0.804161409843274,0.898780258078447,1.1589326906067,1.41908512313495,
1.67923755567353,1.9393899882121,2.03400883653032,2.12862768484853,2.31786538116822,
2.57801781373375,2.83817024629929),.UNSPECIFIED.) ;
#830 = B_SPLINE_SURFACE_WITH_KNOTS('',1,3,((#79227,#79228,#79229,#79230,#79231,
#79232,#79233,#79234,#79235,#79236,#79237,#79238,#79239,#79240,#79241,#79242),
(#79243,#79244,#79245,#79246,#79247,#79248,#79249,#79250,#79251,#79252,
#79253,#79254,#79255,#79256,#79257,#79258)),.UNSPECIFIED.,.F.,.T.,.F.,(2,
2),(4,1,1,1,1,1,1,1,1,1,1,1,1,4),(0.,0.248609854201188),(0.,0.520304864990006,
0.709542561256855,0.80416140961432,0.898780257971786,1.15893269048473,1.41908512299766,
1.67923755554141,1.93938998808516,2.03400883629124,2.12862768449733,2.31786538104175,
2.57801781362961,2.83817024621746),.UNSPECIFIED.) ;
#831 = B_SPLINE_SURFACE_WITH_KNOTS('',3,1,((#79282,#79283),(#79284,#79285),
(#79286,#79287),(#79288,#79289),(#79290,#79291),(#79292,#79293),(#79294,
#79295),(#79296,#79297),(#79298,#79299),(#79300,#79301),(#79302,#79303)),
 .UNSPECIFIED.,.T.,.F.,.F.,(4,1,1,1,1,1,1,1,4),(2,2),(0.,0.117806748710524,
0.235613497421048,0.353420242239986,0.471226987058923,0.58903373187812,
0.706840476697317,0.824647225407855,0.942453974118393),(0.,0.239984718977347),
 .UNSPECIFIED.) ;
#832 = B_SPLINE_SURFACE_WITH_KNOTS('',1,3,((#81592,#81593,#81594,#81595,#81596,
#81597,#81598,#81599,#81600,#81601,#81602,#81603,#81604,#81605,#81606,#81607,
#81608,#81609,#81610,#81611,#81612,#81613,#81614,#81615,#81616,#81617,#81618,
#81619,#81620,#81621,#81622,#81623,#81624,#81625,#81626,#81627,#81628,#81629,
#81630,#81631,#81632,#81633,#81634,#81635,#81636,#81637,#81638,#81639,#81640,
#81641,#81642,#81643,#81644,#81645,#81646,#81647,#81648,#81649,#81650,#81651,
#81652,#81653,#81654,#81655,#81656,#81657,#81658,#81659,#81660,#81661,#81662,
#81663,#81664,#81665,#81666,#81667,#81668,#81669,#81670,#81671,#81672,#81673,
#81674,#81675,#81676,#81677,#81678,#81679,#81680,#81681,#81682,#81683,#81684,
#81685,#81686,#81687,#81688,#81689,#81690,#81691,#81692,#81693,#81694,#81695,
#81696,#81697,#81698,#81699,#81700,#81701,#81702,#81703,#81704,#81705,#81706,
#81707,#81708,#81709,#81710,#81711,#81712,#81713,#81714,#81715,#81716,#81717,
#81718,#81719,#81720,#81721,#81722,#81723,#81724,#81725,#81726,#81727,#81728,
#81729,#81730,#81731,#81732,#81733,#81734,#81735,#81736,#81737,#81738,#81739,
#81740,#81741,#81742,#81743,#81744,#81745,#81746,#81747,#81748,#81749,#81750,
#81751,#81752,#81753,#81754,#81755,#81756,#81757,#81758,#81759,#81760,#81761,
#81762,#81763,#81764,#81765,#81766,#81767,#81768,#81769,#81770,#81771,#81772,
#81773,#81774,#81775,#81776,#81777,#81778,#81779,#81780,#81781,#81782,#81783,
#81784,#81785,#81786,#81787,#81788,#81789,#81790,#81791,#81792,#81793,#81794,
#81795,#81796,#81797,#81798,#81799,#81800,#81801,#81802,#81803,#81804,#81805,
#81806,#81807,#81808,#81809,#81810,#81811,#81812,#81813,#81814,#81815,#81816,
#81817,#81818,#81819,#81820,#81821,#81822,#81823,#81824,#81825,#81826,#81827,
#81828,#81829,#81830,#81831,#81832,#81833,#81834,#81835,#81836,#81837,#81838,
#81839,#81840,#81841,#81842,#81843,#81844,#81845,#81846,#81847,#81848,#81849,
#81850,#81851,#81852,#81853,#81854,#81855,#81856,#81857,#81858,#81859,#81860,
#81861,#81862,#81863,#81864,#81865,#81866,#81867,#81868,#81869,#81870,#81871,
#81872,#81873,#81874,#81875,#81876,#81877,#81878,#81879,#81880,#81881,#81882,
#81883,#81884,#81885,#81886,#81887,#81888,#81889,#81890,#81891,#81892,#81893,
#81894,#81895,#81896,#81897,#81898,#81899,#81900,#81901,#81902,#81903,#81904,
#81905,#81906,#81907,#81908,#81909,#81910,#81911,#81912,#81913,#81914,#81915,
#81916,#81917,#81918,#81919,#81920,#81921,#81922,#81923,#81924,#81925,#81926,
#81927,#81928,#81929,#81930,#81931,#81932,#81933,#81934,#81935,#81936,#81937,
#81938,#81939,#81940,#81941,#81942,#81943,#81944,#81945,#81946,#81947,#81948,
#81949,#81950,#81951,#81952,#81953,#81954,#81955,#81956,#81957,#81958,#81959,
#81960,#81961,#81962,#81963,#81964,#81965,#81966,#81967,#81968,#81969,#81970,
#81971,#81972,#81973,#81974,#81975,#81976,#81977,#81978,#81979,#81980,#81981,
#81982,#81983,#81984,#81985,#81986,#81987,#81988,#81989,#81990,#81991,#81992,
#81993,#81994,#81995,#81996,#81997,#81998,#81999,#82000,#82001,#82002,#82003,
#82004,#82005,#82006,#82007,#82008,#82009,#82010,#82011,#82012,#82013,#82014,
#82015,#82016,#82017,#82018,#82019,#82020,#82021,#82022,#82023,#82024,#82025,
#82026,#82027,#82028,#82029,#82030,#82031,#82032,#82033,#82034,#82035,#82036,
#82037,#82038,#82039,#82040,#82041,#82042,#82043,#82044,#82045,#82046,#82047,
#82048,#82049,#82050,#82051,#82052,#82053,#82054,#82055,#82056,#82057,#82058,
#82059,#82060,#82061,#82062,#82063,#82064,#82065,#82066,#82067,#82068,#82069,
#82070,#82071,#82072,#82073,#82074,#82075,#82076,#82077,#82078,#82079,#82080,
#82081,#82082,#82083,#82084,#82085,#82086,#82087,#82088,#82089,#82090,#82091,
#82092,#82093,#82094,#82095,#82096,#82097,#82098,#82099,#82100,#82101,#82102,
#82103,#82104,#82105,#82106,#82107,#82108,#82109,#82110,#82111,#82112,#82113,
#82114,#82115,#82116,#82117,#82118,#82119,#82120,#82121,#82122,#82123,#82124,
#82125,#82126,#82127,#82128,#82129,#82130,#82131,#82132,#82133,#82134,#82135,
#82136,#82137,#82138,#82139,#82140,#82141,#82142,#82143,#82144,#82145,#82146,
#82147,#82148,#82149,#82150,#82151,#82152,#82153,#82154,#82155,#82156,#82157,
#82158,#82159,#82160,#82161,#82162,#82163,#82164,#82165,#82166,#82167,#82168,
#82169,#82170,#82171,#82172,#82173,#82174,#82175,#82176,#82177,#82178,#82179,
#82180,#82181,#82182,#82183,#82184,#82185,#82186,#82187,#82188,#82189,#82190,
#82191,#82192,#82193,#82194,#82195,#82196,#82197,#82198,#82199,#82200,#82201,
#82202,#82203,#82204,#82205,#82206,#82207,#82208,#82209,#82210,#82211,#82212,
#82213,#82214,#82215,#82216,#82217,#82218,#82219,#82220,#82221,#82222,#82223,
#82224,#82225,#82226,#82227,#82228,#82229,#82230,#82231,#82232,#82233,#82234,
#82235,#82236,#82237,#82238,#82239,#82240,#82241,#82242,#82243,#82244,#82245,
#82246,#82247,#82248,#82249,#82250,#82251,#82252,#82253,#82254,#82255,#82256,
#82257,#82258,#82259,#82260,#82261,#82262,#82263,#82264,#82265,#82266,#82267,
#82268,#82269,#82270,#82271,#82272,#82273,#82274,#82275,#82276,#82277,#82278,
#82279,#82280,#82281,#82282,#82283,#82284,#82285,#82286,#82287,#82288,#82289,
#82290,#82291,#82292,#82293,#82294,#82295,#82296,#82297,#82298,#82299,#82300,
#82301,#82302,#82303,#82304,#82305,#82306,#82307,#82308,#82309,#82310,#82311,
#82312,#82313,#82314,#82315,#82316,#82317,#82318,#82319,#82320,#82321,#82322,
#82323,#82324,#82325,#82326,#82327,#82328,#82329,#82330,#82331,#82332,#82333,
#82334,#82335,#82336,#82337,#82338,#82339,#82340,#82341,#82342,#82343,#82344,
#82345,#82346,#82347,#82348,#82349,#82350,#82351,#82352,#82353,#82354,#82355,
#82356,#82357,#82358,#82359,#82360,#82361,#82362,#82363,#82364,#82365,#82366,
#82367,#82368,#82369,#82370,#82371,#82372,#82373,#82374,#82375,#82376,#82377,
#82378,#82379,#82380,#82381,#82382,#82383,#82384,#82385,#82386,#82387,#82388,
#82389,#82390,#82391,#82392,#82393,#82394,#82395,#82396,#82397,#82398,#82399,
#82400,#82401,#82402,#82403,#82404,#82405,#82406,#82407,#82408,#82409,#82410,
#82411,#82412,#82413,#82414,#82415,#82416,#82417,#82418,#82419,#82420,#82421,
#82422,#82423,#82424,#82425,#82426,#82427,#82428,#82429,#82430,#82431,#82432,
#82433,#82434,#82435,#82436,#82437,#82438,#82439,#82440,#82441,#82442,#82443,
#82444,#82445,#82446,#82447,#82448,#82449,#82450,#82451,#82452,#82453,#82454,
#82455,#82456,#82457,#82458,#82459,#82460,#82461,#82462,#82463,#82464,#82465,
#82466,#82467,#82468,#82469,#82470,#82471,#82472,#82473,#82474,#82475,#82476,
#82477,#82478,#82479,#82480,#82481,#82482,#82483,#82484,#82485,#82486,#82487,
#82488,#82489,#82490,#82491,#82492,#82493,#82494,#82495,#82496,#82497,#82498,
#82499,#82500,#82501,#82502,#82503,#82504,#82505,#82506,#82507,#82508,#82509,
#82510,#82511,#82512,#82513,#82514,#82515,#82516,#82517,#82518,#82519,#82520,
#82521,#82522,#82523,#82524,#82525,#82526,#82527,#82528,#82529,#82530,#82531,
#82532,#82533,#82534,#82535,#82536,#82537,#82538,#82539,#82540,#82541,#82542,
#82543,#82544,#82545,#82546,#82547,#82548,#82549,#82550,#82551,#82552,#82553,
#82554,#82555,#82556,#82557,#82558,#82559,#82560,#82561,#82562,#82563,#82564,
#82565,#82566,#82567,#82568,#82569,#82570,#82571,#82572,#82573,#82574,#82575,
#82576,#82577,#82578,#82579,#82580,#82581,#82582,#82583,#82584,#82585,#82586,
#82587,#82588,#82589,#82590,#82591,#82592,#82593,#82594,#82595,#82596,#82597,
#82598,#82599,#82600,#82601,#82602,#82603,#82604,#82605,#82606,#82607,#82608,
#82609,#82610,#82611,#82612,#82613,#82614,#82615,#82616,#82617,#82618,#82619,
#82620,#82621,#82622,#82623,#82624,#82625,#82626,#82627,#82628,#82629,#82630,
#82631,#82632,#82633,#82634,#82635,#82636,#82637,#82638,#82639,#82640,#82641,
#82642,#82643,#82644,#82645,#82646,#82647,#82648,#82649,#82650,#82651,#82652,
#82653,#82654,#82655,#82656,#82657,#82658,#82659,#82660,#82661,#82662,#82663,
#82664,#82665,#82666,#82667,#82668,#82669,#82670,#82671,#82672,#82673,#82674,
#82675,#82676,#82677,#82678,#82679,#82680,#82681,#82682,#82683,#82684,#82685,
#82686,#82687,#82688,#82689,#82690,#82691,#82692,#82693,#82694,#82695,#82696,
#82697,#82698,#82699,#82700,#82701,#82702,#82703,#82704,#82705,#82706,#82707,
#82708,#82709,#82710,#82711,#82712,#82713,#82714,#82715,#82716,#82717,#82718,
#82719,#82720,#82721,#82722,#82723,#82724,#82725,#82726,#82727,#82728,#82729,
#82730,#82731,#82732,#82733,#82734,#82735,#82736,#82737,#82738,#82739,#82740,
#82741,#82742,#82743,#82744,#82745,#82746,#82747,#82748,#82749,#82750,#82751,
#82752,#82753,#82754,#82755,#82756,#82757,#82758,#82759,#82760,#82761,#82762,
#82763,#82764,#82765,#82766,#82767,#82768,#82769,#82770,#82771,#82772,#82773,
#82774,#82775,#82776,#82777,#82778,#82779,#82780,#82781,#82782,#82783,#82784,
#82785,#82786,#82787,#82788,#82789,#82790,#82791,#82792,#82793,#82794,#82795,
#82796,#82797,#82798,#82799,#82800,#82801,#82802,#82803,#82804,#82805,#82806,
#82807,#82808,#82809,#82810,#82811,#82812,#82813,#82814,#82815,#82816,#82817,
#82818,#82819,#82820,#82821,#82822,#82823,#82824,#82825,#82826,#82827,#82828,
#82829,#82830,#82831,#82832,#82833,#82834,#82835,#82836,#82837,#82838,#82839,
#82840,#82841,#82842,#82843,#82844,#82845,#82846,#82847,#82848,#82849,#82850,
#82851,#82852,#82853,#82854,#82855,#82856,#82857,#82858,#82859,#82860,#82861,
#82862,#82863,#82864,#82865,#82866,#82867,#82868,#82869,#82870,#82871,#82872,
#82873,#82874,#82875,#82876,#82877,#82878,#82879,#82880,#82881,#82882,#82883,
#82884,#82885,#82886,#82887,#82888,#82889,#82890,#82891,#82892,#82893,#82894,
#82895,#82896,#82897,#82898,#82899,#82900,#82901,#82902,#82903,#82904,#82905,
#82906,#82907,#82908,#82909,#82910,#82911,#82912,#82913,#82914,#82915,#82916,
#82917,#82918,#82919,#82920,#82921,#82922,#82923,#82924,#82925,#82926,#82927,
#82928,#82929,#82930,#82931,#82932,#82933,#82934,#82935,#82936,#82937,#82938,
#82939,#82940,#82941,#82942,#82943,#82944,#82945,#82946,#82947,#82948,#82949,
#82950,#82951,#82952,#82953,#82954,#82955,#82956,#82957,#82958,#82959,#82960,
#82961,#82962,#82963,#82964,#82965,#82966,#82967,#82968,#82969,#82970,#82971,
#82972,#82973,#82974,#82975,#82976,#82977,#82978,#82979,#82980,#82981,#82982,
#82983,#82984,#82985,#82986,#82987,#82988,#82989,#82990,#82991,#82992,#82993,
#82994,#82995,#82996,#82997,#82998,#82999,#83000,#83001,#83002,#83003,#83004,
#83005,#83006,#83007,#83008,#83009,#83010,#83011,#83012,#83013,#83014,#83015,
#83016,#83017,#83018,#83019,#83020,#83021,#83022,#83023,#83024,#83025,#83026,
#83027,#83028,#83029,#83030,#83031,#83032,#83033,#83034,#83035,#83036,#83037,
#83038,#83039,#83040,#83041,#83042,#83043,#83044,#83045,#83046,#83047,#83048,
#83049,#83050,#83051,#83052,#83053,#83054,#83055,#83056,#83057,#83058,#83059,
#83060,#83061,#83062,#83063,#83064,#83065,#83066,#83067,#83068,#83069,#83070,
#83071,#83072,#83073,#83074,#83075,#83076,#83077,#83078,#83079,#83080,#83081,
#83082,#83083,#83084,#83085,#83086,#83087,#83088,#83089,#83090,#83091,#83092,
#83093,#83094,#83095,#83096,#83097,#83098,#83099,#83100,#83101,#83102,#83103,
#83104,#83105,#83106,#83107,#83108,#83109,#83110,#83111,#83112,#83113,#83114,
#83115,#83116,#83117,#83118,#83119,#83120,#83121,#83122,#83123,#83124,#83125,
#83126,#83127,#83128,#83129,#83130,#83131,#83132,#83133,#83134,#83135,#83136,
#83137,#83138,#83139,#83140,#83141,#83142,#83143,#83144,#83145,#83146,#83147,
#83148,#83149,#83150,#83151,#83152,#83153,#83154,#83155,#83156,#83157,#83158,
#83159,#83160,#83161,#83162,#83163,#83164,#83165,#83166,#83167,#83168,#83169,
#83170,#83171,#83172,#83173,#83174,#83175,#83176,#83177,#83178,#83179,#83180,
#83181,#83182,#83183,#83184,#83185,#83186,#83187,#83188,#83189,#83190,#83191,
#83192,#83193,#83194,#83195,#83196,#83197,#83198,#83199,#83200,#83201,#83202,
#83203,#83204,#83205,#83206,#83207,#83208,#83209,#83210,#83211,#83212,#83213,
#83214,#83215,#83216,#83217,#83218,#83219,#83220,#83221,#83222,#83223,#83224,
#83225,#83226,#83227,#83228,#83229,#83230,#83231,#83232,#83233,#83234,#83235,
#83236,#83237,#83238,#83239,#83240,#83241,#83242,#83243,#83244,#83245,#83246,
#83247,#83248,#83249,#83250,#83251,#83252,#83253,#83254,#83255,#83256,#83257,
#83258,#83259,#83260,#83261,#83262,#83263,#83264,#83265,#83266,#83267,#83268,
#83269,#83270,#83271,#83272,#83273,#83274,#83275,#83276,#83277,#83278,#83279,
#83280,#83281,#83282,#83283,#83284,#83285,#83286,#83287,#83288,#83289,#83290,
#83291,#83292,#83293,#83294,#83295,#83296,#83297,#83298,#83299,#83300,#83301,
#83302,#83303,#83304,#83305,#83306,#83307,#83308,#83309,#83310,#83311,#83312,
#83313,#83314,#83315,#83316,#83317,#83318,#83319,#83320,#83321,#83322,#83323,
#83324,#83325,#83326,#83327,#83328,#83329,#83330,#83331,#83332,#83333,#83334,
#83335,#83336,#83337,#83338,#83339,#83340,#83341,#83342,#83343,#83344,#83345,
#83346,#83347,#83348,#83349,#83350,#83351,#83352,#83353,#83354,#83355,#83356,
#83357,#83358,#83359,#83360,#83361,#83362,#83363,#83364,#83365,#83366,#83367,
#83368,#83369,#83370,#83371,#83372,#83373,#83374,#83375,#83376,#83377,#83378,
#83379,#83380,#83381,#83382,#83383,#83384,#83385,#83386,#83387,#83388,#83389,
#83390,#83391,#83392,#83393,#83394,#83395,#83396,#83397,#83398,#83399,#83400,
#83401,#83402,#83403,#83404,#83405,#83406,#83407,#83408,#83409,#83410,#83411,
#83412,#83413,#83414,#83415,#83416,#83417,#83418,#83419,#83420,#83421,#83422,
#83423,#83424,#83425,#83426,#83427,#83428,#83429,#83430,#83431,#83432,#83433,
#83434,#83435,#83436,#83437,#83438,#83439,#83440,#83441,#83442,#83443,#83444,
#83445,#83446,#83447,#83448,#83449,#83450,#83451,#83452,#83453,#83454,#83455,
#83456,#83457,#83458,#83459,#83460,#83461,#83462,#83463,#83464,#83465,#83466,
#83467,#83468,#83469,#83470,#83471,#83472,#83473,#83474,#83475,#83476,#83477,
#83478,#83479,#83480,#83481,#83482,#83483,#83484,#83485,#83486,#83487,#83488,
#83489,#83490,#83491,#83492,#83493,#83494,#83495,#83496,#83497,#83498,#83499,
#83500,#83501,#83502,#83503,#83504,#83505,#83506,#83507,#83508,#83509,#83510,
#83511,#83512,#83513,#83514,#83515,#83516,#83517,#83518,#83519,#83520,#83521,
#83522,#83523,#83524,#83525,#83526,#83527,#83528,#83529,#83530,#83531,#83532,
#83533,#83534,#83535,#83536,#83537,#83538,#83539,#83540,#83541,#83542,#83543,
#83544,#83545,#83546,#83547,#83548,#83549,#83550,#83551,#83552,#83553,#83554,
#83555,#83556,#83557,#83558,#83559,#83560,#83561,#83562,#83563,#83564,#83565,
#83566,#83567,#83568,#83569,#83570,#83571,#83572,#83573,#83574,#83575,#83576,
#83577,#83578,#83579,#83580,#83581,#83582,#83583,#83584,#83585,#83586,#83587,
#83588,#83589,#83590,#83591,#83592,#83593,#83594,#83595,#83596,#83597,#83598,
#83599,#83600,#83601,#83602,#83603,#83604,#83605,#83606,#83607,#83608,#83609,
#83610,#83611,#83612,#83613,#83614,#83615,#83616,#83617,#83618,#83619,#83620,
#83621,#83622,#83623,#83624,#83625,#83626,#83627,#83628,#83629,#83630,#83631,
#83632,#83633,#83634,#83635,#83636,#83637,#83638,#83639,#83640,#83641,#83642,
#83643,#83644,#83645,#83646,#83647,#83648,#83649,#83650,#83651,#83652,#83653,
#83654,#83655,#83656,#83657,#83658,#83659,#83660,#83661,#83662,#83663,#83664,
#83665,#83666,#83667,#83668,#83669,#83670,#83671,#83672,#83673,#83674,#83675,
#83676,#83677,#83678,#83679,#83680,#83681,#83682,#83683,#83684,#83685,#83686,
#83687,#83688,#83689,#83690,#83691,#83692,#83693,#83694,#83695,#83696,#83697,
#83698,#83699,#83700,#83701,#83702,#83703,#83704,#83705,#83706,#83707,#83708,
#83709,#83710,#83711,#83712,#83713,#83714,#83715,#83716,#83717,#83718,#83719,
#83720,#83721,#83722,#83723,#83724,#83725,#83726,#83727,#83728,#83729,#83730,
#83731,#83732,#83733,#83734,#83735,#83736,#83737,#83738,#83739,#83740,#83741,
#83742,#83743,#83744,#83745,#83746,#83747,#83748,#83749,#83750,#83751,#83752,
#83753,#83754,#83755,#83756,#83757,#83758,#83759,#83760,#83761,#83762,#83763,
#83764,#83765,#83766,#83767,#83768,#83769,#83770,#83771,#83772,#83773,#83774,
#83775,#83776,#83777,#83778,#83779,#83780,#83781,#83782,#83783,#83784,#83785,
#83786,#83787,#83788,#83789,#83790,#83791,#83792,#83793,#83794,#83795,#83796,
#83797,#83798,#83799,#83800,#83801,#83802,#83803,#83804,#83805,#83806,#83807,
#83808,#83809,#83810,#83811,#83812,#83813,#83814,#83815,#83816,#83817,#83818,
#83819,#83820,#83821,#83822,#83823,#83824,#83825,#83826,#83827,#83828,#83829,
#83830,#83831,#83832,#83833,#83834,#83835,#83836,#83837,#83838,#83839,#83840,
#83841,#83842,#83843,#83844,#83845,#83846,#83847,#83848,#83849,#83850,#83851,
#83852,#83853,#83854,#83855,#83856,#83857,#83858,#83859,#83860,#83861,#83862,
#83863,#83864,#83865,#83866,#83867,#83868,#83869,#83870,#83871,#83872,#83873,
#83874,#83875,#83876,#83877,#83878,#83879,#83880,#83881,#83882,#83883,#83884,
#83885,#83886,#83887,#83888,#83889,#83890,#83891,#83892,#83893,#83894,#83895,
#83896,#83897,#83898,#83899,#83900,#83901,#83902,#83903,#83904,#83905,#83906,
#83907,#83908,#83909,#83910,#83911,#83912,#83913,#83914,#83915,#83916,#83917,
#83918,#83919,#83920,#83921,#83922,#83923,#83924,#83925,#83926,#83927,#83928,
#83929,#83930,#83931,#83932,#83933,#83934,#83935,#83936,#83937,#83938,#83939,
#83940,#83941,#83942,#83943,#83944,#83945,#83946,#83947,#83948,#83949,#83950,
#83951,#83952,#83953,#83954,#83955,#83956,#83957,#83958,#83959,#83960,#83961,
#83962,#83963,#83964,#83965,#83966,#83967,#83968,#83969,#83970,#83971,#83972,
#83973,#83974,#83975,#83976,#83977,#83978,#83979,#83980,#83981,#83982,#83983,
#83984,#83985,#83986,#83987,#83988,#83989,#83990,#83991,#83992,#83993,#83994,
#83995,#83996,#83997,#83998,#83999,#84000,#84001,#84002,#84003,#84004,#84005,
#84006,#84007,#84008,#84009,#84010,#84011,#84012,#84013,#84014,#84015,#84016,
#84017,#84018,#84019,#84020,#84021,#84022,#84023,#84024,#84025,#84026,#84027,
#84028,#84029,#84030,#84031,#84032,#84033,#84034,#84035,#84036,#84037,#84038,
#84039,#84040,#84041,#84042,#84043,#84044,#84045,#84046,#84047,#84048,#84049,
#84050,#84051,#84052,#84053,#84054,#84055,#84056,#84057,#84058,#84059,#84060,
#84061,#84062,#84063,#84064,#84065,#84066,#84067,#84068,#84069,#84070,#84071,
#84072,#84073,#84074,#84075,#84076,#84077,#84078,#84079,#84080,#84081,#84082,
#84083,#84084,#84085,#84086,#84087,#84088,#84089,#84090,#84091,#84092,#84093,
#84094,#84095,#84096,#84097,#84098,#84099,#84100,#84101,#84102,#84103,#84104,
#84105,#84106,#84107,#84108,#84109,#84110,#84111,#84112,#84113,#84114,#84115,
#84116,#84117,#84118,#84119,#84120,#84121,#84122,#84123,#84124,#84125,#84126,
#84127,#84128,#84129,#84130,#84131,#84132,#84133,#84134,#84135,#84136,#84137,
#84138,#84139,#84140,#84141,#84142,#84143,#84144,#84145,#84146,#84147,#84148,
#84149,#84150,#84151,#84152,#84153,#84154,#84155,#84156,#84157,#84158,#84159,
#84160,#84161,#84162,#84163,#84164,#84165,#84166,#84167,#84168,#84169,#84170,
#84171,#84172,#84173,#84174,#84175,#84176,#84177,#84178,#84179,#84180,#84181,
#84182,#84183,#84184,#84185,#84186,#84187,#84188,#84189,#84190,#84191,#84192,
#84193,#84194,#84195,#84196,#84197,#84198,#84199,#84200,#84201,#84202,#84203,
#84204,#84205,#84206,#84207,#84208,#84209,#84210,#84211,#84212,#84213,#84214,
#84215,#84216,#84217,#84218,#84219,#84220,#84221,#84222,#84223,#84224,#84225,
#84226,#84227,#84228,#84229,#84230,#84231,#84232,#84233,#84234,#84235,#84236,
#84237,#84238,#84239,#84240,#84241,#84242,#84243,#84244,#84245,#84246,#84247,
#84248,#84249,#84250,#84251,#84252,#84253,#84254,#84255,#84256,#84257,#84258,
#84259,#84260,#84261,#84262,#84263,#84264,#84265,#84266,#84267,#84268,#84269,
#84270,#84271,#84272,#84273,#84274,#84275,#84276,#84277,#84278,#84279,#84280,
#84281,#84282,#84283,#84284,#84285,#84286,#84287,#84288,#84289,#84290,#84291,
#84292,#84293,#84294,#84295,#84296,#84297,#84298,#84299,#84300,#84301,#84302,
#84303,#84304,#84305,#84306,#84307,#84308,#84309,#84310,#84311,#84312,#84313,
#84314,#84315,#84316,#84317,#84318,#84319,#84320,#84321,#84322,#84323,#84324,
#84325,#84326,#84327,#84328,#84329,#84330,#84331,#84332,#84333,#84334,#84335,
#84336,#84337,#84338,#84339,#84340,#84341,#84342,#84343,#84344,#84345,#84346,
#84347,#84348,#84349,#84350,#84351,#84352,#84353,#84354,#84355,#84356,#84357,
#84358,#84359,#84360,#84361,#84362,#84363,#84364,#84365,#84366,#84367,#84368,
#84369,#84370,#84371,#84372,#84373,#84374,#84375,#84376,#84377,#84378,#84379,
#84380,#84381,#84382,#84383,#84384,#84385,#84386,#84387,#84388,#84389,#84390,
#84391,#84392,#84393,#84394,#84395,#84396,#84397,#84398,#84399,#84400,#84401,
#84402,#84403,#84404,#84405,#84406,#84407,#84408,#84409,#84410,#84411,#84412,
#84413,#84414,#84415,#84416,#84417,#84418,#84419,#84420,#84421,#84422,#84423,
#84424,#84425,#84426,#84427,#84428,#84429,#84430,#84431,#84432,#84433,#84434,
#84435,#84436,#84437,#84438,#84439,#84440,#84441,#84442,#84443,#84444,#84445,
#84446,#84447,#84448,#84449,#84450,#84451,#84452,#84453,#84454,#84455,#84456,
#84457,#84458,#84459,#84460,#84461,#84462,#84463,#84464,#84465,#84466,#84467,
#84468,#84469,#84470,#84471,#84472,#84473,#84474,#84475,#84476,#84477,#84478,
#84479,#84480,#84481,#84482,#84483,#84484,#84485,#84486,#84487,#84488,#84489,
#84490,#84491,#84492,#84493,#84494,#84495,#84496,#84497,#84498,#84499,#84500,
#84501,#84502,#84503,#84504,#84505,#84506,#84507,#84508,#84509,#84510,#84511,
#84512,#84513,#84514,#84515,#84516,#84517,#84518,#84519,#84520,#84521,#84522,
#84523,#84524,#84525,#84526,#84527,#84528,#84529,#84530,#84531,#84532,#84533,
#84534,#84535,#84536,#84537,#84538,#84539,#84540,#84541,#84542,#84543,#84544,
#84545,#84546,#84547,#84548,#84549,#84550,#84551,#84552,#84553,#84554,#84555,
#84556,#84557,#84558,#84559,#84560,#84561,#84562,#84563,#84564,#84565,#84566,
#84567,#84568,#84569,#84570,#84571,#84572,#84573,#84574,#84575,#84576,#84577,
#84578,#84579,#84580,#84581,#84582,#84583,#84584,#84585,#84586,#84587,#84588,
#84589,#84590,#84591,#84592,#84593,#84594,#84595,#84596,#84597,#84598,#84599,
#84600,#84601,#84602,#84603,#84604,#84605,#84606,#84607,#84608,#84609,#84610,
#84611,#84612,#84613,#84614,#84615,#84616,#84617,#84618,#84619,#84620,#84621,
#84622,#84623,#84624,#84625,#84626,#84627,#84628,#84629,#84630,#84631,#84632,
#84633,#84634,#84635,#84636,#84637,#84638,#84639,#84640,#84641,#84642,#84643,
#84644,#84645,#84646,#84647,#84648,#84649,#84650,#84651,#84652,#84653,#84654,
#84655,#84656,#84657,#84658,#84659,#84660,#84661,#84662,#84663,#84664,#84665,
#84666,#84667,#84668,#84669,#84670,#84671,#84672,#84673,#84674,#84675,#84676,
#84677,#84678,#84679,#84680,#84681,#84682,#84683,#84684,#84685,#84686,#84687,
#84688,#84689,#84690,#84691,#84692,#84693,#84694,#84695,#84696,#84697,#84698,
#84699,#84700,#84701,#84702,#84703,#84704,#84705,#84706,#84707,#84708,#84709,
#84710,#84711,#84712,#84713,#84714,#84715,#84716,#84717,#84718,#84719,#84720,
#84721,#84722,#84723,#84724,#84725,#84726,#84727,#84728,#84729,#84730,#84731,
#84732,#84733,#84734,#84735,#84736,#84737,#84738,#84739,#84740,#84741,#84742,
#84743,#84744,#84745,#84746,#84747,#84748,#84749,#84750,#84751,#84752,#84753,
#84754,#84755,#84756,#84757,#84758,#84759,#84760,#84761,#84762,#84763,#84764,
#84765,#84766,#84767,#84768,#84769,#84770,#84771,#84772,#84773,#84774,#84775,
#84776,#84777,#84778,#84779,#84780,#84781,#84782,#84783,#84784,#84785,#84786,
#84787,#84788,#84789,#84790,#84791,#84792,#84793,#84794,#84795,#84796,#84797,
#84798,#84799,#84800,#84801,#84802,#84803,#84804,#84805,#84806,#84807,#84808,
#84809,#84810,#84811,#84812,#84813,#84814,#84815,#84816,#84817,#84818,#84819,
#84820,#84821,#84822,#84823,#84824,#84825,#84826,#84827,#84828,#84829,#84830,
#84831,#84832,#84833,#84834,#84835,#84836,#84837,#84838,#84839,#84840,#84841,
#84842,#84843,#84844,#84845,#84846,#84847,#84848,#84849,#84850,#84851,#84852,
#84853,#84854,#84855,#84856,#84857,#84858,#84859,#84860,#84861,#84862,#84863,
#84864,#84865,#84866,#84867,#84868,#84869,#84870,#84871,#84872,#84873,#84874,
#84875,#84876,#84877,#84878,#84879,#84880,#84881,#84882,#84883,#84884,#84885,
#84886,#84887,#84888,#84889,#84890,#84891,#84892,#84893,#84894,#84895,#84896,
#84897,#84898,#84899,#84900,#84901,#84902,#84903,#84904,#84905,#84906,#84907,
#84908,#84909,#84910,#84911,#84912,#84913,#84914,#84915,#84916,#84917,#84918,
#84919,#84920,#84921,#84922,#84923,#84924,#84925,#84926,#84927,#84928,#84929,
#84930,#84931,#84932,#84933,#84934,#84935,#84936,#84937,#84938,#84939,#84940,
#84941,#84942,#84943,#84944,#84945,#84946,#84947,#84948,#84949,#84950,#84951,
#84952,#84953,#84954,#84955,#84956,#84957,#84958,#84959,#84960,#84961,#84962,
#84963,#84964,#84965,#84966,#84967,#84968,#84969,#84970,#84971,#84972,#84973,
#84974,#84975,#84976,#84977,#84978,#84979,#84980,#84981,#84982,#84983,#84984,
#84985,#84986,#84987,#84988,#84989,#84990,#84991,#84992,#84993,#84994,#84995,
#84996,#84997,#84998,#84999,#85000,#85001,#85002,#85003,#85004,#85005,#85006,
#85007,#85008,#85009,#85010,#85011,#85012,#85013,#85014,#85015,#85016,#85017,
#85018,#85019,#85020,#85021,#85022,#85023,#85024,#85025,#85026,#85027,#85028,
#85029,#85030,#85031,#85032,#85033,#85034,#85035,#85036,#85037,#85038,#85039,
#85040,#85041,#85042,#85043,#85044,#85045,#85046,#85047,#85048,#85049,#85050,
#85051,#85052,#85053,#85054,#85055,#85056,#85057,#85058,#85059,#85060,#85061,
#85062,#85063,#85064,#85065,#85066,#85067,#85068,#85069,#85070,#85071,#85072,
#85073,#85074,#85075,#85076),(#85077,#85078,#85079,#85080,#85081,#85082,
#85083,#85084,#85085,#85086,#85087,#85088,#85089,#85090,#85091,#85092,#85093,
#85094,#85095,#85096,#85097,#85098,#85099,#85100,#85101,#85102,#85103,#85104,
#85105,#85106,#85107,#85108,#85109,#85110,#85111,#85112,#85113,#85114,#85115,
#85116,#85117,#85118,#85119,#85120,#85121,#85122,#85123,#85124,#85125,#85126,
#85127,#85128,#85129,#85130,#85131,#85132,#85133,#85134,#85135,#85136,#85137,
#85138,#85139,#85140,#85141,#85142,#85143,#85144,#85145,#85146,#85147,#85148,
#85149,#85150,#85151,#85152,#85153,#85154,#85155,#85156,#85157,#85158,#85159,
#85160,#85161,#85162,#85163,#85164,#85165,#85166,#85167,#85168,#85169,#85170,
#85171,#85172,#85173,#85174,#85175,#85176,#85177,#85178,#85179,#85180,#85181,
#85182,#85183,#85184,#85185,#85186,#85187,#85188,#85189,#85190,#85191,#85192,
#85193,#85194,#85195,#85196,#85197,#85198,#85199,#85200,#85201,#85202,#85203,
#85204,#85205,#85206,#85207,#85208,#85209,#85210,#85211,#85212,#85213,#85214,
#85215,#85216,#85217,#85218,#85219,#85220,#85221,#85222,#85223,#85224,#85225,
#85226,#85227,#85228,#85229,#85230,#85231,#85232,#85233,#85234,#85235,#85236,
#85237,#85238,#85239,#85240,#85241,#85242,#85243,#85244,#85245,#85246,#85247,
#85248,#85249,#85250,#85251,#85252,#85253,#85254,#85255,#85256,#85257,#85258,
#85259,#85260,#85261,#85262,#85263,#85264,#85265,#85266,#85267,#85268,#85269,
#85270,#85271,#85272,#85273,#85274,#85275,#85276,#85277,#85278,#85279,#85280,
#85281,#85282,#85283,#85284,#85285,#85286,#85287,#85288,#85289,#85290,#85291,
#85292,#85293,#85294,#85295,#85296,#85297,#85298,#85299,#85300,#85301,#85302,
#85303,#85304,#85305,#85306,#85307,#85308,#85309,#85310,#85311,#85312,#85313,
#85314,#85315,#85316,#85317,#85318,#85319,#85320,#85321,#85322,#85323,#85324,
#85325,#85326,#85327,#85328,#85329,#85330,#85331,#85332,#85333,#85334,#85335,
#85336,#85337,#85338,#85339,#85340,#85341,#85342,#85343,#85344,#85345,#85346,
#85347,#85348,#85349,#85350,#85351,#85352,#85353,#85354,#85355,#85356,#85357,
#85358,#85359,#85360,#85361,#85362,#85363,#85364,#85365,#85366,#85367,#85368,
#85369,#85370,#85371,#85372,#85373,#85374,#85375,#85376,#85377,#85378,#85379,
#85380,#85381,#85382,#85383,#85384,#85385,#85386,#85387,#85388,#85389,#85390,
#85391,#85392,#85393,#85394,#85395,#85396,#85397,#85398,#85399,#85400,#85401,
#85402,#85403,#85404,#85405,#85406,#85407,#85408,#85409,#85410,#85411,#85412,
#85413,#85414,#85415,#85416,#85417,#85418,#85419,#85420,#85421,#85422,#85423,
#85424,#85425,#85426,#85427,#85428,#85429,#85430,#85431,#85432,#85433,#85434,
#85435,#85436,#85437,#85438,#85439,#85440,#85441,#85442,#85443,#85444,#85445,
#85446,#85447,#85448,#85449,#85450,#85451,#85452,#85453,#85454,#85455,#85456,
#85457,#85458,#85459,#85460,#85461,#85462,#85463,#85464,#85465,#85466,#85467,
#85468,#85469,#85470,#85471,#85472,#85473,#85474,#85475,#85476,#85477,#85478,
#85479,#85480,#85481,#85482,#85483,#85484,#85485,#85486,#85487,#85488,#85489,
#85490,#85491,#85492,#85493,#85494,#85495,#85496,#85497,#85498,#85499,#85500,
#85501,#85502,#85503,#85504,#85505,#85506,#85507,#85508,#85509,#85510,#85511,
#85512,#85513,#85514,#85515,#85516,#85517,#85518,#85519,#85520,#85521,#85522,
#85523,#85524,#85525,#85526,#85527,#85528,#85529,#85530,#85531,#85532,#85533,
#85534,#85535,#85536,#85537,#85538,#85539,#85540,#85541,#85542,#85543,#85544,
#85545,#85546,#85547,#85548,#85549,#85550,#85551,#85552,#85553,#85554,#85555,
#85556,#85557,#85558,#85559,#85560,#85561,#85562,#85563,#85564,#85565,#85566,
#85567,#85568,#85569,#85570,#85571,#85572,#85573,#85574,#85575,#85576,#85577,
#85578,#85579,#85580,#85581,#85582,#85583,#85584,#85585,#85586,#85587,#85588,
#85589,#85590,#85591,#85592,#85593,#85594,#85595,#85596,#85597,#85598,#85599,
#85600,#85601,#85602,#85603,#85604,#85605,#85606,#85607,#85608,#85609,#85610,
#85611,#85612,#85613,#85614,#85615,#85616,#85617,#85618,#85619,#85620,#85621,
#85622,#85623,#85624,#85625,#85626,#85627,#85628,#85629,#85630,#85631,#85632,
#85633,#85634,#85635,#85636,#85637,#85638,#85639,#85640,#85641,#85642,#85643,
#85644,#85645,#85646,#85647,#85648,#85649,#85650,#85651,#85652,#85653,#85654,
#85655,#85656,#85657,#85658,#85659,#85660,#85661,#85662,#85663,#85664,#85665,
#85666,#85667,#85668,#85669,#85670,#85671,#85672,#85673,#85674,#85675,#85676,
#85677,#85678,#85679,#85680,#85681,#85682,#85683,#85684,#85685,#85686,#85687,
#85688,#85689,#85690,#85691,#85692,#85693,#85694,#85695,#85696,#85697,#85698,
#85699,#85700,#85701,#85702,#85703,#85704,#85705,#85706,#85707,#85708,#85709,
#85710,#85711,#85712,#85713,#85714,#85715,#85716,#85717,#85718,#85719,#85720,
#85721,#85722,#85723,#85724,#85725,#85726,#85727,#85728,#85729,#85730,#85731,
#85732,#85733,#85734,#85735,#85736,#85737,#85738,#85739,#85740,#85741,#85742,
#85743,#85744,#85745,#85746,#85747,#85748,#85749,#85750,#85751,#85752,#85753,
#85754,#85755,#85756,#85757,#85758,#85759,#85760,#85761,#85762,#85763,#85764,
#85765,#85766,#85767,#85768,#85769,#85770,#85771,#85772,#85773,#85774,#85775,
#85776,#85777,#85778,#85779,#85780,#85781,#85782,#85783,#85784,#85785,#85786,
#85787,#85788,#85789,#85790,#85791,#85792,#85793,#85794,#85795,#85796,#85797,
#85798,#85799,#85800,#85801,#85802,#85803,#85804,#85805,#85806,#85807,#85808,
#85809,#85810,#85811,#85812,#85813,#85814,#85815,#85816,#85817,#85818,#85819,
#85820,#85821,#85822,#85823,#85824,#85825,#85826,#85827,#85828,#85829,#85830,
#85831,#85832,#85833,#85834,#85835,#85836,#85837,#85838,#85839,#85840,#85841,
#85842,#85843,#85844,#85845,#85846,#85847,#85848,#85849,#85850,#85851,#85852,
#85853,#85854,#85855,#85856,#85857,#85858,#85859,#85860,#85861,#85862,#85863,
#85864,#85865,#85866,#85867,#85868,#85869,#85870,#85871,#85872,#85873,#85874,
#85875,#85876,#85877,#85878,#85879,#85880,#85881,#85882,#85883,#85884,#85885,
#85886,#85887,#85888,#85889,#85890,#85891,#85892,#85893,#85894,#85895,#85896,
#85897,#85898,#85899,#85900,#85901,#85902,#85903,#85904,#85905,#85906,#85907,
#85908,#85909,#85910,#85911,#85912,#85913,#85914,#85915,#85916,#85917,#85918,
#85919,#85920,#85921,#85922,#85923,#85924,#85925,#85926,#85927,#85928,#85929,
#85930,#85931,#85932,#85933,#85934,#85935,#85936,#85937,#85938,#85939,#85940,
#85941,#85942,#85943,#85944,#85945,#85946,#85947,#85948,#85949,#85950,#85951,
#85952,#85953,#85954,#85955,#85956,#85957,#85958,#85959,#85960,#85961,#85962,
#85963,#85964,#85965,#85966,#85967,#85968,#85969,#85970,#85971,#85972,#85973,
#85974,#85975,#85976,#85977,#85978,#85979,#85980,#85981,#85982,#85983,#85984,
#85985,#85986,#85987,#85988,#85989,#85990,#85991,#85992,#85993,#85994,#85995,
#85996,#85997,#85998,#85999,#86000,#86001,#86002,#86003,#86004,#86005,#86006,
#86007,#86008,#86009,#86010,#86011,#86012,#86013,#86014,#86015,#86016,#86017,
#86018,#86019,#86020,#86021,#86022,#86023,#86024,#86025,#86026,#86027,#86028,
#86029,#86030,#86031,#86032,#86033,#86034,#86035,#86036,#86037,#86038,#86039,
#86040,#86041,#86042,#86043,#86044,#86045,#86046,#86047,#86048,#86049,#86050,
#86051,#86052,#86053,#86054,#86055,#86056,#86057,#86058,#86059,#86060,#86061,
#86062,#86063,#86064,#86065,#86066,#86067,#86068,#86069,#86070,#86071,#86072,
#86073,#86074,#86075,#86076,#86077,#86078,#86079,#86080,#86081,#86082,#86083,
#86084,#86085,#86086,#86087,#86088,#86089,#86090,#86091,#86092,#86093,#86094,
#86095,#86096,#86097,#86098,#86099,#86100,#86101,#86102,#86103,#86104,#86105,
#86106,#86107,#86108,#86109,#86110,#86111,#86112,#86113,#86114,#86115,#86116,
#86117,#86118,#86119,#86120,#86121,#86122,#86123,#86124,#86125,#86126,#86127,
#86128,#86129,#86130,#86131,#86132,#86133,#86134,#86135,#86136,#86137,#86138,
#86139,#86140,#86141,#86142,#86143,#86144,#86145,#86146,#86147,#86148,#86149,
#86150,#86151,#86152,#86153,#86154,#86155,#86156,#86157,#86158,#86159,#86160,
#86161,#86162,#86163,#86164,#86165,#86166,#86167,#86168,#86169,#86170,#86171,
#86172,#86173,#86174,#86175,#86176,#86177,#86178,#86179,#86180,#86181,#86182,
#86183,#86184,#86185,#86186,#86187,#86188,#86189,#86190,#86191,#86192,#86193,
#86194,#86195,#86196,#86197,#86198,#86199,#86200,#86201,#86202,#86203,#86204,
#86205,#86206,#86207,#86208,#86209,#86210,#86211,#86212,#86213,#86214,#86215,
#86216,#86217,#86218,#86219,#86220,#86221,#86222,#86223,#86224,#86225,#86226,
#86227,#86228,#86229,#86230,#86231,#86232,#86233,#86234,#86235,#86236,#86237,
#86238,#86239,#86240,#86241,#86242,#86243,#86244,#86245,#86246,#86247,#86248,
#86249,#86250,#86251,#86252,#86253,#86254,#86255,#86256,#86257,#86258,#86259,
#86260,#86261,#86262,#86263,#86264,#86265,#86266,#86267,#86268,#86269,#86270,
#86271,#86272,#86273,#86274,#86275,#86276,#86277,#86278,#86279,#86280,#86281,
#86282,#86283,#86284,#86285,#86286,#86287,#86288,#86289,#86290,#86291,#86292,
#86293,#86294,#86295,#86296,#86297,#86298,#86299,#86300,#86301,#86302,#86303,
#86304,#86305,#86306,#86307,#86308,#86309,#86310,#86311,#86312,#86313,#86314,
#86315,#86316,#86317,#86318,#86319,#86320,#86321,#86322,#86323,#86324,#86325,
#86326,#86327,#86328,#86329,#86330,#86331,#86332,#86333,#86334,#86335,#86336,
#86337,#86338,#86339,#86340,#86341,#86342,#86343,#86344,#86345,#86346,#86347,
#86348,#86349,#86350,#86351,#86352,#86353,#86354,#86355,#86356,#86357,#86358,
#86359,#86360,#86361,#86362,#86363,#86364,#86365,#86366,#86367,#86368,#86369,
#86370,#86371,#86372,#86373,#86374,#86375,#86376,#86377,#86378,#86379,#86380,
#86381,#86382,#86383,#86384,#86385,#86386,#86387,#86388,#86389,#86390,#86391,
#86392,#86393,#86394,#86395,#86396,#86397,#86398,#86399,#86400,#86401,#86402,
#86403,#86404,#86405,#86406,#86407,#86408,#86409,#86410,#86411,#86412,#86413,
#86414,#86415,#86416,#86417,#86418,#86419,#86420,#86421,#86422,#86423,#86424,
#86425,#86426,#86427,#86428,#86429,#86430,#86431,#86432,#86433,#86434,#86435,
#86436,#86437,#86438,#86439,#86440,#86441,#86442,#86443,#86444,#86445,#86446,
#86447,#86448,#86449,#86450,#86451,#86452,#86453,#86454,#86455,#86456,#86457,
#86458,#86459,#86460,#86461,#86462,#86463,#86464,#86465,#86466,#86467,#86468,
#86469,#86470,#86471,#86472,#86473,#86474,#86475,#86476,#86477,#86478,#86479,
#86480,#86481,#86482,#86483,#86484,#86485,#86486,#86487,#86488,#86489,#86490,
#86491,#86492,#86493,#86494,#86495,#86496,#86497,#86498,#86499,#86500,#86501,
#86502,#86503,#86504,#86505,#86506,#86507,#86508,#86509,#86510,#86511,#86512,
#86513,#86514,#86515,#86516,#86517,#86518,#86519,#86520,#86521,#86522,#86523,
#86524,#86525,#86526,#86527,#86528,#86529,#86530,#86531,#86532,#86533,#86534,
#86535,#86536,#86537,#86538,#86539,#86540,#86541,#86542,#86543,#86544,#86545,
#86546,#86547,#86548,#86549,#86550,#86551,#86552,#86553,#86554,#86555,#86556,
#86557,#86558,#86559,#86560,#86561,#86562,#86563,#86564,#86565,#86566,#86567,
#86568,#86569,#86570,#86571,#86572,#86573,#86574,#86575,#86576,#86577,#86578,
#86579,#86580,#86581,#86582,#86583,#86584,#86585,#86586,#86587,#86588,#86589,
#86590,#86591,#86592,#86593,#86594,#86595,#86596,#86597,#86598,#86599,#86600,
#86601,#86602,#86603,#86604,#86605,#86606,#86607,#86608,#86609,#86610,#86611,
#86612,#86613,#86614,#86615,#86616,#86617,#86618,#86619,#86620,#86621,#86622,
#86623,#86624,#86625,#86626,#86627,#86628,#86629,#86630,#86631,#86632,#86633,
#86634,#86635,#86636,#86637,#86638,#86639,#86640,#86641,#86642,#86643,#86644,
#86645,#86646,#86647,#86648,#86649,#86650,#86651,#86652,#86653,#86654,#86655,
#86656,#86657,#86658,#86659,#86660,#86661,#86662,#86663,#86664,#86665,#86666,
#86667,#86668,#86669,#86670,#86671,#86672,#86673,#86674,#86675,#86676,#86677,
#86678,#86679,#86680,#86681,#86682,#86683,#86684,#86685,#86686,#86687,#86688,
#86689,#86690,#86691,#86692,#86693,#86694,#86695,#86696,#86697,#86698,#86699,
#86700,#86701,#86702,#86703,#86704,#86705,#86706,#86707,#86708,#86709,#86710,
#86711,#86712,#86713,#86714,#86715,#86716,#86717,#86718,#86719,#86720,#86721,
#86722,#86723,#86724,#86725,#86726,#86727,#86728,#86729,#86730,#86731,#86732,
#86733,#86734,#86735,#86736,#86737,#86738,#86739,#86740,#86741,#86742,#86743,
#86744,#86745,#86746,#86747,#86748,#86749,#86750,#86751,#86752,#86753,#86754,
#86755,#86756,#86757,#86758,#86759,#86760,#86761,#86762,#86763,#86764,#86765,
#86766,#86767,#86768,#86769,#86770,#86771,#86772,#86773,#86774,#86775,#86776,
#86777,#86778,#86779,#86780,#86781,#86782,#86783,#86784,#86785,#86786,#86787,
#86788,#86789,#86790,#86791,#86792,#86793,#86794,#86795,#86796,#86797,#86798,
#86799,#86800,#86801,#86802,#86803,#86804,#86805,#86806,#86807,#86808,#86809,
#86810,#86811,#86812,#86813,#86814,#86815,#86816,#86817,#86818,#86819,#86820,
#86821,#86822,#86823,#86824,#86825,#86826,#86827,#86828,#86829,#86830,#86831,
#86832,#86833,#86834,#86835,#86836,#86837,#86838,#86839,#86840,#86841,#86842,
#86843,#86844,#86845,#86846,#86847,#86848,#86849,#86850,#86851,#86852,#86853,
#86854,#86855,#86856,#86857,#86858,#86859,#86860,#86861,#86862,#86863,#86864,
#86865,#86866,#86867,#86868,#86869,#86870,#86871,#86872,#86873,#86874,#86875,
#86876,#86877,#86878,#86879,#86880,#86881,#86882,#86883,#86884,#86885,#86886,
#86887,#86888,#86889,#86890,#86891,#86892,#86893,#86894,#86895,#86896,#86897,
#86898,#86899,#86900,#86901,#86902,#86903,#86904,#86905,#86906,#86907,#86908,
#86909,#86910,#86911,#86912,#86913,#86914,#86915,#86916,#86917,#86918,#86919,
#86920,#86921,#86922,#86923,#86924,#86925,#86926,#86927,#86928,#86929,#86930,
#86931,#86932,#86933,#86934,#86935,#86936,#86937,#86938,#86939,#86940,#86941,
#86942,#86943,#86944,#86945,#86946,#86947,#86948,#86949,#86950,#86951,#86952,
#86953,#86954,#86955,#86956,#86957,#86958,#86959,#86960,#86961,#86962,#86963,
#86964,#86965,#86966,#86967,#86968,#86969,#86970,#86971,#86972,#86973,#86974,
#86975,#86976,#86977,#86978,#86979,#86980,#86981,#86982,#86983,#86984,#86985,
#86986,#86987,#86988,#86989,#86990,#86991,#86992,#86993,#86994,#86995,#86996,
#86997,#86998,#86999,#87000,#87001,#87002,#87003,#87004,#87005,#87006,#87007,
#87008,#87009,#87010,#87011,#87012,#87013,#87014,#87015,#87016,#87017,#87018,
#87019,#87020,#87021,#87022,#87023,#87024,#87025,#87026,#87027,#87028,#87029,
#87030,#87031,#87032,#87033,#87034,#87035,#87036,#87037,#87038,#87039,#87040,
#87041,#87042,#87043,#87044,#87045,#87046,#87047,#87048,#87049,#87050,#87051,
#87052,#87053,#87054,#87055,#87056,#87057,#87058,#87059,#87060,#87061,#87062,
#87063,#87064,#87065,#87066,#87067,#87068,#87069,#87070,#87071,#87072,#87073,
#87074,#87075,#87076,#87077,#87078,#87079,#87080,#87081,#87082,#87083,#87084,
#87085,#87086,#87087,#87088,#87089,#87090,#87091,#87092,#87093,#87094,#87095,
#87096,#87097,#87098,#87099,#87100,#87101,#87102,#87103,#87104,#87105,#87106,
#87107,#87108,#87109,#87110,#87111,#87112,#87113,#87114,#87115,#87116,#87117,
#87118,#87119,#87120,#87121,#87122,#87123,#87124,#87125,#87126,#87127,#87128,
#87129,#87130,#87131,#87132,#87133,#87134,#87135,#87136,#87137,#87138,#87139,
#87140,#87141,#87142,#87143,#87144,#87145,#87146,#87147,#87148,#87149,#87150,
#87151,#87152,#87153,#87154,#87155,#87156,#87157,#87158,#87159,#87160,#87161,
#87162,#87163,#87164,#87165,#87166,#87167,#87168,#87169,#87170,#87171,#87172,
#87173,#87174,#87175,#87176,#87177,#87178,#87179,#87180,#87181,#87182,#87183,
#87184,#87185,#87186,#87187,#87188,#87189,#87190,#87191,#87192,#87193,#87194,
#87195,#87196,#87197,#87198,#87199,#87200,#87201,#87202,#87203,#87204,#87205,
#87206,#87207,#87208,#87209,#87210,#87211,#87212,#87213,#87214,#87215,#87216,
#87217,#87218,#87219,#87220,#87221,#87222,#87223,#87224,#87225,#87226,#87227,
#87228,#87229,#87230,#87231,#87232,#87233,#87234,#87235,#87236,#87237,#87238,
#87239,#87240,#87241,#87242,#87243,#87244,#87245,#87246,#87247,#87248,#87249,
#87250,#87251,#87252,#87253,#87254,#87255,#87256,#87257,#87258,#87259,#87260,
#87261,#87262,#87263,#87264,#87265,#87266,#87267,#87268,#87269,#87270,#87271,
#87272,#87273,#87274,#87275,#87276,#87277,#87278,#87279,#87280,#87281,#87282,
#87283,#87284,#87285,#87286,#87287,#87288,#87289,#87290,#87291,#87292,#87293,
#87294,#87295,#87296,#87297,#87298,#87299,#87300,#87301,#87302,#87303,#87304,
#87305,#87306,#87307,#87308,#87309,#87310,#87311,#87312,#87313,#87314,#87315,
#87316,#87317,#87318,#87319,#87320,#87321,#87322,#87323,#87324,#87325,#87326,
#87327,#87328,#87329,#87330,#87331,#87332,#87333,#87334,#87335,#87336,#87337,
#87338,#87339,#87340,#87341,#87342,#87343,#87344,#87345,#87346,#87347,#87348,
#87349,#87350,#87351,#87352,#87353,#87354,#87355,#87356,#87357,#87358,#87359,
#87360,#87361,#87362,#87363,#87364,#87365,#87366,#87367,#87368,#87369,#87370,
#87371,#87372,#87373,#87374,#87375,#87376,#87377,#87378,#87379,#87380,#87381,
#87382,#87383,#87384,#87385,#87386,#87387,#87388,#87389,#87390,#87391,#87392,
#87393,#87394,#87395,#87396,#87397,#87398,#87399,#87400,#87401,#87402,#87403,
#87404,#87405,#87406,#87407,#87408,#87409,#87410,#87411,#87412,#87413,#87414,
#87415,#87416,#87417,#87418,#87419,#87420,#87421,#87422,#87423,#87424,#87425,
#87426,#87427,#87428,#87429,#87430,#87431,#87432,#87433,#87434,#87435,#87436,
#87437,#87438,#87439,#87440,#87441,#87442,#87443,#87444,#87445,#87446,#87447,
#87448,#87449,#87450,#87451,#87452,#87453,#87454,#87455,#87456,#87457,#87458,
#87459,#87460,#87461,#87462,#87463,#87464,#87465,#87466,#87467,#87468,#87469,
#87470,#87471,#87472,#87473,#87474,#87475,#87476,#87477,#87478,#87479,#87480,
#87481,#87482,#87483,#87484,#87485,#87486,#87487,#87488,#87489,#87490,#87491,
#87492,#87493,#87494,#87495,#87496,#87497,#87498,#87499,#87500,#87501,#87502,
#87503,#87504,#87505,#87506,#87507,#87508,#87509,#87510,#87511,#87512,#87513,
#87514,#87515,#87516,#87517,#87518,#87519,#87520,#87521,#87522,#87523,#87524,
#87525,#87526,#87527,#87528,#87529,#87530,#87531,#87532,#87533,#87534,#87535,
#87536,#87537,#87538,#87539,#87540,#87541,#87542,#87543,#87544,#87545,#87546,
#87547,#87548,#87549,#87550,#87551,#87552,#87553,#87554,#87555,#87556,#87557,
#87558,#87559,#87560,#87561,#87562,#87563,#87564,#87565,#87566,#87567,#87568,
#87569,#87570,#87571,#87572,#87573,#87574,#87575,#87576,#87577,#87578,#87579,
#87580,#87581,#87582,#87583,#87584,#87585,#87586,#87587,#87588,#87589,#87590,
#87591,#87592,#87593,#87594,#87595,#87596,#87597,#87598,#87599,#87600,#87601,
#87602,#87603,#87604,#87605,#87606,#87607,#87608,#87609,#87610,#87611,#87612,
#87613,#87614,#87615,#87616,#87617,#87618,#87619,#87620,#87621,#87622,#87623,
#87624,#87625,#87626,#87627,#87628,#87629,#87630,#87631,#87632,#87633,#87634,
#87635,#87636,#87637,#87638,#87639,#87640,#87641,#87642,#87643,#87644,#87645,
#87646,#87647,#87648,#87649,#87650,#87651,#87652,#87653,#87654,#87655,#87656,
#87657,#87658,#87659,#87660,#87661,#87662,#87663,#87664,#87665,#87666,#87667,
#87668,#87669,#87670,#87671,#87672,#87673,#87674,#87675,#87676,#87677,#87678,
#87679,#87680,#87681,#87682,#87683,#87684,#87685,#87686,#87687,#87688,#87689,
#87690,#87691,#87692,#87693,#87694,#87695,#87696,#87697,#87698,#87699,#87700,
#87701,#87702,#87703,#87704,#87705,#87706,#87707,#87708,#87709,#87710,#87711,
#87712,#87713,#87714,#87715,#87716,#87717,#87718,#87719,#87720,#87721,#87722,
#87723,#87724,#87725,#87726,#87727,#87728,#87729,#87730,#87731,#87732,#87733,
#87734,#87735,#87736,#87737,#87738,#87739,#87740,#87741,#87742,#87743,#87744,
#87745,#87746,#87747,#87748,#87749,#87750,#87751,#87752,#87753,#87754,#87755,
#87756,#87757,#87758,#87759,#87760,#87761,#87762,#87763,#87764,#87765,#87766,
#87767,#87768,#87769,#87770,#87771,#87772,#87773,#87774,#87775,#87776,#87777,
#87778,#87779,#87780,#87781,#87782,#87783,#87784,#87785,#87786,#87787,#87788,
#87789,#87790,#87791,#87792,#87793,#87794,#87795,#87796,#87797,#87798,#87799,
#87800,#87801,#87802,#87803,#87804,#87805,#87806,#87807,#87808,#87809,#87810,
#87811,#87812,#87813,#87814,#87815,#87816,#87817,#87818,#87819,#87820,#87821,
#87822,#87823,#87824,#87825,#87826,#87827,#87828,#87829,#87830,#87831,#87832,
#87833,#87834,#87835,#87836,#87837,#87838,#87839,#87840,#87841,#87842,#87843,
#87844,#87845,#87846,#87847,#87848,#87849,#87850,#87851,#87852,#87853,#87854,
#87855,#87856,#87857,#87858,#87859,#87860,#87861,#87862,#87863,#87864,#87865,
#87866,#87867,#87868,#87869,#87870,#87871,#87872,#87873,#87874,#87875,#87876,
#87877,#87878,#87879,#87880,#87881,#87882,#87883,#87884,#87885,#87886,#87887,
#87888,#87889,#87890,#87891,#87892,#87893,#87894,#87895,#87896,#87897,#87898,
#87899,#87900,#87901,#87902,#87903,#87904,#87905,#87906,#87907,#87908,#87909,
#87910,#87911,#87912,#87913,#87914,#87915,#87916,#87917,#87918,#87919,#87920,
#87921,#87922,#87923,#87924,#87925,#87926,#87927,#87928,#87929,#87930,#87931,
#87932,#87933,#87934,#87935,#87936,#87937,#87938,#87939,#87940,#87941,#87942,
#87943,#87944,#87945,#87946,#87947,#87948,#87949,#87950,#87951,#87952,#87953,
#87954,#87955,#87956,#87957,#87958,#87959,#87960,#87961,#87962,#87963,#87964,
#87965,#87966,#87967,#87968,#87969,#87970,#87971,#87972,#87973,#87974,#87975,
#87976,#87977,#87978,#87979,#87980,#87981,#87982,#87983,#87984,#87985,#87986,
#87987,#87988,#87989,#87990,#87991,#87992,#87993,#87994,#87995,#87996,#87997,
#87998,#87999,#88000,#88001,#88002,#88003,#88004,#88005,#88006,#88007,#88008,
#88009,#88010,#88011,#88012,#88013,#88014,#88015,#88016,#88017,#88018,#88019,
#88020,#88021,#88022,#88023,#88024,#88025,#88026,#88027,#88028,#88029,#88030,
#88031,#88032,#88033,#88034,#88035,#88036,#88037,#88038,#88039,#88040,#88041,
#88042,#88043,#88044,#88045,#88046,#88047,#88048,#88049,#88050,#88051,#88052,
#88053,#88054,#88055,#88056,#88057,#88058,#88059,#88060,#88061,#88062,#88063,
#88064,#88065,#88066,#88067,#88068,#88069,#88070,#88071,#88072,#88073,#88074,
#88075,#88076,#88077,#88078,#88079,#88080,#88081,#88082,#88083,#88084,#88085,
#88086,#88087,#88088,#88089,#88090,#88091,#88092,#88093,#88094,#88095,#88096,
#88097,#88098,#88099,#88100,#88101,#88102,#88103,#88104,#88105,#88106,#88107,
#88108,#88109,#88110,#88111,#88112,#88113,#88114,#88115,#88116,#88117,#88118,
#88119,#88120,#88121,#88122,#88123,#88124,#88125,#88126,#88127,#88128,#88129,
#88130,#88131,#88132,#88133,#88134,#88135,#88136,#88137,#88138,#88139,#88140,
#88141,#88142,#88143,#88144,#88145,#88146,#88147,#88148,#88149,#88150,#88151,
#88152,#88153,#88154,#88155,#88156,#88157,#88158,#88159,#88160,#88161,#88162,
#88163,#88164,#88165,#88166,#88167,#88168,#88169,#88170,#88171,#88172,#88173,
#88174,#88175,#88176,#88177,#88178,#88179,#88180,#88181,#88182,#88183,#88184,
#88185,#88186,#88187,#88188,#88189,#88190,#88191,#88192,#88193,#88194,#88195,
#88196,#88197,#88198,#88199,#88200,#88201,#88202,#88203,#88204,#88205,#88206,
#88207,#88208,#88209,#88210,#88211,#88212,#88213,#88214,#88215,#88216,#88217,
#88218,#88219,#88220,#88221,#88222,#88223,#88224,#88225,#88226,#88227,#88228,
#88229,#88230,#88231,#88232,#88233,#88234,#88235,#88236,#88237,#88238,#88239,
#88240,#88241,#88242,#88243,#88244,#88245,#88246,#88247,#88248,#88249,#88250,
#88251,#88252,#88253,#88254,#88255,#88256,#88257,#88258,#88259,#88260,#88261,
#88262,#88263,#88264,#88265,#88266,#88267,#88268,#88269,#88270,#88271,#88272,
#88273,#88274,#88275,#88276,#88277,#88278,#88279,#88280,#88281,#88282,#88283,
#88284,#88285,#88286,#88287,#88288,#88289,#88290,#88291,#88292,#88293,#88294,
#88295,#88296,#88297,#88298,#88299,#88300,#88301,#88302,#88303,#88304,#88305,
#88306,#88307,#88308,#88309,#88310,#88311,#88312,#88313,#88314,#88315,#88316,
#88317,#88318,#88319,#88320,#88321,#88322,#88323,#88324,#88325,#88326,#88327,
#88328,#88329,#88330,#88331,#88332,#88333,#88334,#88335,#88336,#88337,#88338,
#88339,#88340,#88341,#88342,#88343,#88344,#88345,#88346,#88347,#88348,#88349,
#88350,#88351,#88352,#88353,#88354,#88355,#88356,#88357,#88358,#88359,#88360,
#88361,#88362,#88363,#88364,#88365,#88366,#88367,#88368,#88369,#88370,#88371,
#88372,#88373,#88374,#88375,#88376,#88377,#88378,#88379,#88380,#88381,#88382,
#88383,#88384,#88385,#88386,#88387,#88388,#88389,#88390,#88391,#88392,#88393,
#88394,#88395,#88396,#88397,#88398,#88399,#88400,#88401,#88402,#88403,#88404,
#88405,#88406,#88407,#88408,#88409,#88410,#88411,#88412,#88413,#88414,#88415,
#88416,#88417,#88418,#88419,#88420,#88421,#88422,#88423,#88424,#88425,#88426,
#88427,#88428,#88429,#88430,#88431,#88432,#88433,#88434,#88435,#88436,#88437,
#88438,#88439,#88440,#88441,#88442,#88443,#88444,#88445,#88446,#88447,#88448,
#88449,#88450,#88451,#88452,#88453,#88454,#88455,#88456,#88457,#88458,#88459,
#88460,#88461,#88462,#88463,#88464,#88465,#88466,#88467,#88468,#88469,#88470,
#88471,#88472,#88473,#88474,#88475,#88476,#88477,#88478,#88479,#88480,#88481,
#88482,#88483,#88484,#88485,#88486,#88487,#88488,#88489,#88490,#88491,#88492,
#88493,#88494,#88495,#88496,#88497,#88498,#88499,#88500,#88501,#88502,#88503,
#88504,#88505,#88506,#88507,#88508,#88509,#88510,#88511,#88512,#88513,#88514,
#88515,#88516,#88517,#88518,#88519,#88520,#88521,#88522,#88523,#88524,#88525,
#88526,#88527,#88528,#88529,#88530,#88531,#88532,#88533,#88534,#88535,#88536,
#88537,#88538,#88539,#88540,#88541,#88542,#88543,#88544,#88545,#88546,#88547,
#88548,#88549,#88550,#88551,#88552,#88553,#88554,#88555,#88556,#88557,#88558,
#88559,#88560,#88561)),.UNSPECIFIED.,.F.,.F.,.F.,(2,2),(4,1,1,1,1,1,1,1,
1,1,1,1,1,1,1,1,1,1,1,1,1,1,1,1,1,1,1,1,1,1,1,1,1,1,1,1,1,1,1,1,1,1,1,1,
1,1,1,1,1,1,1,1,1,1,1,1,1,1,1,1,1,1,1,1,1,1,1,1,1,1,1,1,1,1,1,1,1,1,1,1,
1,1,1,1,1,1,1,1,1,1,1,1,1,1,1,1,1,1,1,1,1,1,1,1,1,1,1,1,1,1,1,1,1,1,1,1,
1,1,1,1,1,1,1,1,1,1,1,1,1,1,1,1,1,1,1,1,1,1,1,1,1,1,1,1,1,1,1,1,1,1,1,1,
1,1,1,1,1,1,1,1,1,1,1,1,1,1,1,1,1,1,1,1,1,1,1,1,1,1,1,1,1,1,1,1,1,1,1,1,
1,1,1,1,1,1,1,1,1,1,1,1,1,1,1,1,1,1,1,1,1,1,1,1,1,1,1,1,1,1,1,1,1,1,1,1,
1,1,1,1,1,1,1,1,1,1,1,1,1,1,1,1,1,1,1,1,1,1,1,1,1,1,1,1,1,1,1,1,1,1,1,1,
1,1,1,1,1,1,1,1,1,1,1,1,1,1,1,1,1,1,1,1,1,1,1,1,1,1,1,1,1,1,1,1,1,1,1,1,
1,1,1,1,1,1,1,1,1,1,1,1,1,1,1,1,1,1,1,1,1,1,1,1,1,1,1,1,1,1,1,1,1,1,1,1,
1,1,1,1,1,1,1,1,1,1,1,1,1,1,1,1,1,1,1,1,1,1,1,1,1,1,1,1,1,1,1,1,1,1,1,1,
1,1,1,1,1,1,1,1,1,1,1,1,1,1,1,1,1,1,1,1,1,1,1,1,1,1,1,1,1,1,1,1,1,1,1,1,
1,1,1,1,1,1,1,1,1,1,1,1,1,1,1,1,1,1,1,1,1,1,1,1,1,1,1,1,1,1,1,1,1,1,1,1,
1,1,1,1,1,1,1,1,1,1,1,1,1,1,1,1,1,1,1,1,1,1,1,1,1,1,1,1,1,1,1,1,1,1,1,1,
1,1,1,1,1,1,1,1,1,1,1,1,1,1,1,1,1,1,1,1,1,1,1,1,1,1,1,1,1,1,1,1,1,1,1,1,
1,1,1,1,1,1,1,1,1,1,1,1,1,1,1,1,1,1,1,1,1,1,1,1,1,1,1,1,1,1,1,1,1,1,1,1,
1,1,1,1,1,1,1,1,1,1,1,1,1,1,1,1,1,1,1,1,1,1,1,1,1,1,1,1,1,1,1,1,1,1,1,1,
1,1,1,1,1,1,1,1,1,1,1,1,1,1,1,1,1,1,1,1,1,1,1,1,1,1,1,1,1,1,1,1,1,1,1,1,
1,1,1,1,1,1,1,1,1,1,1,1,1,1,1,1,1,1,1,1,1,1,1,1,1,1,1,1,1,1,1,1,1,1,1,1,
1,1,1,1,1,1,1,1,1,1,1,1,1,1,1,1,1,1,1,1,1,1,1,1,1,1,1,1,1,1,1,1,1,1,1,1,
1,1,1,1,1,1,1,1,1,1,1,1,1,1,1,1,1,1,1,1,1,1,1,1,1,1,1,1,1,1,1,1,1,1,1,1,
1,1,1,1,1,1,1,1,1,1,1,1,1,1,1,1,1,1,1,1,1,1,1,1,1,1,1,1,1,1,1,1,1,1,1,1,
1,1,1,1,1,1,1,1,1,1,1,1,1,1,1,1,1,1,1,1,1,1,1,1,1,1,1,1,1,1,1,1,1,1,1,1,
1,1,1,1,1,1,1,1,1,1,1,1,1,1,1,1,1,1,1,1,1,1,1,1,1,1,1,1,1,1,1,1,1,1,1,1,
1,1,1,1,1,1,1,1,1,1,1,1,1,1,1,1,1,1,1,1,1,1,1,1,1,1,1,1,1,1,1,1,1,1,1,1,
1,1,1,1,1,1,1,1,1,1,1,1,1,1,1,1,1,1,1,1,1,1,1,1,1,1,1,1,1,1,1,1,1,1,1,1,
1,1,1,1,1,1,1,1,1,1,1,1,1,1,1,1,1,1,1,1,1,1,1,1,1,1,1,1,1,1,1,1,1,1,1,1,
1,1,1,1,1,1,1,1,1,1,1,1,1,1,1,1,1,1,1,1,1,1,1,1,1,1,1,1,1,1,1,1,1,1,1,1,
1,1,1,1,1,1,1,1,1,1,1,1,1,1,1,1,1,1,1,1,1,1,1,1,1,1,1,1,1,1,1,1,1,1,1,1,
1,1,1,1,1,1,1,1,1,1,1,1,1,1,1,1,1,1,1,1,1,1,1,1,1,1,1,1,1,1,1,1,1,1,1,1,
1,1,1,1,1,1,1,1,1,1,1,1,1,1,1,1,1,1,1,1,1,1,1,1,1,1,1,1,1,1,1,1,1,1,1,1,
1,1,1,1,1,1,1,1,1,1,1,1,1,1,1,1,1,1,1,1,1,1,1,1,1,1,1,1,1,1,1,1,1,1,1,1,
1,1,1,1,1,1,1,1,1,1,1,1,1,1,1,1,1,1,1,1,1,1,1,1,1,1,1,1,1,1,1,1,1,1,1,1,
1,1,1,1,1,1,1,1,1,1,1,1,1,1,1,1,1,1,1,1,1,1,1,1,1,1,1,1,1,1,1,1,1,1,1,1,
1,1,1,1,1,1,1,1,1,1,1,1,1,1,1,1,1,1,1,1,1,1,1,1,1,1,1,1,1,1,1,1,1,1,1,1,
1,1,1,1,1,1,1,1,1,1,1,1,1,1,1,1,1,1,1,1,1,1,1,1,1,1,1,1,1,1,1,1,1,1,1,1,
1,1,1,1,1,1,1,1,1,1,1,1,1,1,1,1,1,1,1,1,1,1,1,1,1,1,1,1,1,1,1,1,1,1,1,1,
1,1,1,1,1,1,1,1,1,1,1,1,1,1,1,1,1,1,1,1,1,1,1,1,1,1,1,1,1,1,1,1,1,1,1,1,
1,1,1,1,1,1,1,1,1,1,1,1,1,1,1,1,1,1,1,1,1,1,1,1,1,1,1,1,1,1,1,1,1,1,1,1,
1,1,1,1,1,1,1,1,1,1,1,1,1,1,1,1,1,1,1,1,1,1,1,1,1,1,1,1,1,1,1,1,1,1,1,1,
1,1,1,1,1,1,1,1,1,1,1,1,1,1,1,1,1,1,1,1,1,1,1,1,1,1,1,1,1,1,1,1,1,1,1,1,
1,1,1,1,1,1,1,1,1,1,1,1,1,1,1,1,1,1,1,1,1,1,1,1,1,1,1,1,1,1,1,1,1,1,1,1,
1,1,1,1,1,1,1,1,1,1,1,1,1,1,1,1,1,1,1,1,1,1,1,1,1,1,1,1,1,1,1,1,1,1,1,1,
1,1,1,1,1,1,1,1,1,1,1,1,1,1,1,1,1,1,1,1,1,1,1,1,1,1,1,1,1,1,1,1,1,1,1,1,
1,1,1,1,1,1,1,1,1,1,1,1,1,1,1,1,1,1,1,1,1,1,1,1,1,1,1,1,1,1,1,1,1,1,1,1,
1,1,1,1,1,1,1,1,1,1,1,1,1,1,1,1,1,1,1,1,1,1,1,1,1,1,1,1,1,1,1,1,1,1,1,1,
1,1,1,1,1,1,1,1,1,1,1,1,1,1,1,1,1,1,1,1,1,1,1,1,1,1,1,1,1,1,1,1,1,1,1,1,
1,1,1,1,1,1,1,1,1,1,1,1,1,1,1,1,1,1,1,1,1,1,1,1,1,1,1,1,1,1,1,1,1,1,1,1,
1,1,1,1,1,1,1,1,1,1,1,1,1,1,1,1,1,1,1,1,1,1,1,1,1,1,1,1,1,1,1,1,1,1,1,1,
1,1,1,1,1,1,1,1,1,1,1,1,1,1,1,1,1,1,1,1,1,1,1,1,1,1,1,1,1,1,1,1,1,1,1,1,
1,1,1,1,1,1,1,1,1,1,1,1,1,1,1,1,1,1,1,1,1,1,1,1,1,1,1,1,1,1,1,1,1,1,1,1,
1,1,1,1,1,1,1,1,1,1,1,1,1,1,1,1,1,1,1,1,1,1,1,1,1,1,1,1,1,1,1,1,1,1,1,1,
1,1,1,1,1,1,1,1,1,1,1,1,1,1,1,1,1,1,1,1,1,1,1,1,1,1,1,1,1,1,1,1,1,1,1,1,
1,1,1,1,1,1,1,1,1,1,1,1,1,1,1,1,1,1,1,1,1,1,1,1,1,1,1,1,1,1,1,1,1,1,1,1,
1,1,1,1,1,1,1,1,1,1,1,1,1,1,1,1,1,1,1,1,1,1,1,1,1,1,1,1,1,1,1,1,1,1,1,1,
1,1,1,1,1,1,1,1,1,1,1,1,1,1,1,1,1,1,1,1,1,1,1,1,1,1,1,1,1,1,1,1,1,1,1,1,
1,1,1,1,1,1,1,1,1,1,1,1,1,1,1,1,1,1,1,1,1,1,1,1,1,1,1,1,1,1,1,1,1,1,1,1,
1,1,1,1,1,1,1,1,1,1,1,1,1,1,1,1,1,1,1,1,1,1,1,1,1,1,1,1,1,1,1,1,1,1,1,1,
1,1,1,1,1,1,1,1,1,1,1,1,1,1,1,1,1,1,1,1,1,1,1,1,1,1,1,1,1,1,1,1,1,1,1,1,
1,1,1,1,1,1,1,1,1,1,1,1,1,1,1,1,1,1,1,1,1,1,1,1,1,1,1,1,1,1,1,1,1,1,1,1,
1,1,1,1,1,1,1,1,1,1,1,1,1,1,1,1,1,1,1,1,1,1,1,1,1,1,1,1,1,1,1,1,1,1,1,1,
1,1,1,1,1,1,1,1,1,1,1,1,1,1,1,1,1,1,1,1,1,1,1,1,1,1,1,1,1,1,1,1,1,1,1,1,
1,1,1,1,1,1,1,1,1,1,1,1,1,1,1,1,1,1,1,1,1,1,1,1,1,1,1,1,1,1,1,1,1,1,1,1,
1,1,1,1,1,1,1,1,1,1,1,1,1,1,1,1,1,1,1,1,1,1,1,1,1,1,1,1,1,1,1,1,1,1,1,1,
1,1,1,1,1,1,1,1,1,1,1,1,1,1,1,1,1,1,1,1,1,1,1,1,1,1,1,1,1,1,1,1,1,1,1,1,
1,1,1,1,1,1,1,1,1,1,1,1,1,1,1,1,1,1,1,1,1,1,1,1,1,1,1,1,1,1,1,1,1,1,1,1,
1,1,1,1,1,1,1,1,1,1,1,1,1,1,1,1,1,1,1,1,1,1,1,1,1,1,1,1,1,1,1,1,1,1,1,1,
1,1,1,1,1,1,1,1,1,1,1,1,1,1,1,1,1,1,1,1,1,1,1,1,1,1,1,1,1,1,1,1,1,1,1,1,
1,1,1,1,1,1,1,1,1,1,1,1,1,1,1,1,1,1,1,1,1,1,1,1,1,1,1,1,1,1,1,1,1,1,1,1,
1,1,1,1,1,1,1,1,1,1,1,1,1,1,1,1,1,1,1,1,1,1,1,1,1,1,1,1,1,1,1,1,1,1,1,1,
1,1,1,1,1,1,1,1,1,1,1,1,1,1,1,1,1,1,1,1,1,1,1,1,1,1,1,1,1,1,1,1,1,1,1,1,
1,1,1,1,1,1,1,1,1,1,1,1,1,1,1,1,1,1,1,1,1,1,1,1,1,1,1,1,1,1,1,1,1,1,1,1,
1,1,1,1,1,1,1,1,1,1,1,1,1,1,1,1,1,1,1,1,1,1,1,1,1,1,1,1,1,1,1,1,1,1,1,1,
1,1,1,1,1,1,1,1,1,1,1,1,1,1,1,1,1,1,1,1,1,1,1,1,1,1,1,1,1,1,1,1,1,1,1,1,
1,1,1,1,1,1,1,1,1,1,1,1,1,1,1,1,1,1,1,1,1,1,1,1,1,1,1,1,1,1,1,1,1,1,1,1,
1,1,1,1,1,1,1,1,1,1,1,1,1,1,1,1,1,1,1,1,1,1,1,1,1,1,1,1,1,1,1,1,1,1,1,1,
1,1,1,1,1,1,1,1,1,1,1,1,1,1,1,1,1,1,1,1,1,1,1,1,1,1,1,1,1,1,1,1,1,1,1,1,
1,1,1,1,1,1,1,1,1,1,1,1,1,1,1,1,1,1,1,1,1,1,1,1,1,1,1,1,1,1,1,1,1,1,1,1,
1,1,1,1,1,1,1,1,1,1,1,1,1,1,1,1,1,1,1,1,1,1,1,1,1,1,1,1,1,1,1,1,1,1,1,1,
1,1,1,1,1,1,1,1,1,1,1,1,1,1,1,1,1,1,1,1,1,1,1,1,1,1,1,1,1,1,1,1,1,1,1,1,
1,1,1,1,1,1,1,1,1,1,1,1,1,1,1,1,1,1,1,1,1,1,1,1,1,1,1,1,1,1,1,1,1,1,1,1,
1,1,1,1,1,1,1,1,1,1,1,1,1,1,1,1,1,1,1,1,1,1,1,1,1,1,1,1,1,1,1,1,1,1,1,1,
1,1,1,1,1,1,1,1,1,1,1,1,1,1,1,1,1,1,1,1,1,1,1,1,1,1,1,1,1,1,1,1,1,1,1,1,
1,1,1,1,1,1,1,1,1,1,1,1,1,1,1,1,1,1,1,1,1,1,1,1,1,1,1,1,1,1,1,1,1,1,1,1,
1,1,1,1,1,1,1,1,1,1,1,1,1,1,1,1,1,1,1,1,1,1,1,1,1,1,1,1,1,1,1,1,1,1,1,1,
1,1,1,1,1,1,1,1,1,1,1,1,1,1,1,1,1,1,1,1,1,1,1,1,1,1,1,1,1,1,1,1,1,1,1,1,
1,1,1,1,1,1,1,1,1,1,1,1,1,1,1,1,1,1,1,1,1,1,1,1,1,1,1,1,1,1,1,1,1,1,1,1,
1,1,1,1,1,1,1,1,1,1,1,1,1,1,1,1,1,1,1,1,1,1,1,1,1,1,1,1,1,1,1,1,1,1,1,1,
1,1,1,1,1,1,1,1,1,1,1,1,1,1,1,1,1,1,1,1,1,1,1,1,1,1,1,1,1,1,1,1,1,1,1,1,
1,1,1,1,1,1,1,1,1,1,1,1,1,1,1,1,1,1,1,1,1,1,1,1,1,1,1,1,1,1,1,1,1,1,1,1,
1,1,1,1,1,1,1,1,1,1,1,1,1,1,1,1,1,1,1,1,1,1,1,1,1,1,1,1,1,1,1,1,1,1,1,1,
1,1,1,1,1,1,1,1,1,1,1,1,1,1,1,1,1,1,1,1,1,1,1,1,1,1,1,1,1,1,1,1,1,1,1,1,
1,1,1,1,1,1,1,1,1,1,1,1,1,1,1,1,1,1,1,1,1,1,1,1,1,1,1,1,1,1,1,1,1,1,1,1,
1,1,1,1,1,1,1,1,1,1,1,1,1,1,1,1,1,1,1,1,1,1,1,1,1,1,1,1,1,1,1,1,1,1,1,1,
1,1,1,1,1,1,1,1,1,1,1,1,1,1,1,1,1,1,1,1,1,1,1,1,1,1,1,1,1,1,1,1,1,1,1,1,
1,1,1,1,1,1,1,1,1,1,1,1,1,1,1,1,1,1,1,1,1,1,1,1,1,1,1,1,1,1,1,1,1,1,1,1,
1,1,1,1,1,1,1,1,1,1,1,1,1,1,1,1,1,1,1,1,1,1,1,1,1,1,1,1,1,1,1,1,1,1,1,1,
1,1,1,1,1,1,1,1,1,1,1,1,1,1,1,1,1,1,4),(-0.58309518948453,0.),(0.,0.869746702321014,
1.7394931589914,2.60923976624962,3.47983908319159,4.35043840179749,5.22018503077054,
6.08993165951504,6.95967828799171,7.82942491616733,8.69917154401062,9.56891817149224,
10.4395174886835,11.3101168056706,12.179863432132,13.049610058144,13.9193566836854,
14.7891033087372,15.6588499332817,16.5285965573034,17.3991958717975,18.2697951860185,
18.7046684974166,19.1395418086746,19.5744151197912,20.0092884307654,20.4441617415962,
20.8790350522825,21.7487816732187,22.1836549834672,22.6185282935685,23.0534016035221,
23.4882749133276,23.9231482229848,24.3588742245859,24.794600226187,25.2294735355468,
26.0992201538203,26.5340934627341,26.9689667714994,27.4038400801166,27.838713388586,
28.2735866969081,28.7084600050832,29.143333313112,29.5782066209952,30.0130799287334,
30.4479532363275,30.8828265437783,31.3185525442794,31.7542785447804,32.1891518519474,
32.6240251589741,33.0588984658616,33.4937717726112,33.928645079224,34.3635183857014,
34.7983916920448,35.2332649982556,35.6681383043353,36.1030116102854,36.5378849161076,
36.9727582218035,37.4076315273749,37.8425048328235,38.2782308323341,38.7139568318446,
39.1488301370532,39.5837034421446,40.0185767471208,40.4534500519838,40.8883233567357,
41.3231966613787,41.7580699659148,42.1929432703463,42.6278165746754,43.0626898789044,
43.4975631830356,43.9324364870714,44.3673097910142,44.8021830948664,45.2379090935952,
45.673635092324,46.1085083960024,46.5433816995978,46.9782550031127,47.4131283065497,
47.8480016099115,48.2828749132006,48.7177482164198,49.1526215195718,49.5874948226593,
50.0223681256851,50.457241428652,50.8921147315628,51.3269880344203,51.7618613372274,
52.197587335454,52.6333133336805,53.0681866363954,53.5030599390685,53.9379332417027,
54.3728065443011,54.8076798468664,55.2425531494018,55.6774264519101,56.1122997543943,
56.5471730568575,56.9820463593026,57.4169196617326,57.8517929641506,58.2866662665595,
58.7215395689624,59.157265567009,59.5929915650557,60.0278648674556,60.4627381698584,
60.8976114722673,61.3324847746853,61.7673580771153,62.2022313795604,62.6371046820236,
63.0719779845079,63.5068512870162,63.9417245895516,64.376597892117,64.8114711947155,
65.2463444973499,65.6812178000231,66.1169437982275,66.5526697964318,66.9875430991915,
67.4224164019987,67.8572897048563,68.2921630077673,68.7270363107343,69.1619096137603,
69.5967829168479,70.0316562200001,70.4665295232194,70.9014028265087,71.3362761298705,
71.7711494333077,72.2060227368227,72.6408960404182,73.0766220391044,73.5123480377905,
73.9472213415547,74.382094645407,74.8169679493499,75.2518412533859,75.6867145575172,
76.1215878617464,76.5564611660756,76.9913344705072,77.4262077750435,77.8610810796866,
78.2959543844386,78.7308276893018,79.1657009942781,79.6005742993696,80.0363002988208,
80.4720262982719,80.9068996035997,81.3417729090484,81.7766462146199,82.211519520316,
82.6463928261383,83.0812661320886,83.5161394381684,83.9510127443794,84.3858860507229,
84.8207593572004,85.2556326638134,85.6905059705631,86.1253792774507,86.5602525844776,
86.995978584908,87.4317045853384,87.8665778926469,88.3014512000977,88.7363245076919,
89.1711978154302,89.6060711233134,90.0409444313423,90.4758177395175,90.9106910478396,
91.345564356309,91.7804376649263,92.2153109736917,92.6501842826055,93.085057591668,
93.5199309008791,93.9556569024059,94.3913829039327,94.8262562134414,95.2611295230986,
95.6960028329042,96.1308761428578,96.5657494529591,97.0006227632077,97.4354960736028,
97.870369384144,98.3052426948304,98.7401160056612,99.1749893166354,99.6098626277522,
100.04473593901,100.915335253024,101.351061255639,101.785934567313,102.220807879124,
102.655681191068,103.090554503145,103.525427815353,104.395174440154,105.264921065453,
105.699794378283,106.134667691232,106.569541004295,107.004414317471,107.8750136343,
108.745612951339,109.615359578629,110.485106206296,111.354852834309,112.224599462639,
113.094346091254,113.964092720119,114.834692038763,115.705291357499,116.575037986826,
117.444784616267,118.314531245777,119.184277875311,120.054024504821,120.923771134261,
121.794370453112,122.66496977189,123.534716400968,124.404463029834,125.274209658448,
126.143956286779,127.013702914792,127.883449542458,128.754048859798,129.624648176939,
130.494394803617,131.364141429857,132.233888055637,133.103634680937,133.973381305737,
134.843127930023,135.71372724472,136.584326559147,137.019199870684,137.454073182083,
137.888946493341,138.323819804458,139.193566426263,140.063313047491,140.498186357887,
140.933059668136,141.367932978237,141.802806288191,142.237679597997,142.673405599673,
143.109131601348,143.544004910857,143.978878220217,144.413751529429,144.848624838491,
145.283498147405,145.718371456171,146.153244764789,146.588118073258,147.022991381581,
147.457864689756,147.892737997785,148.327611305669,148.762484613407,149.197357921002,
149.633083921574,150.068809922147,150.503683229455,150.938556536623,151.37342984365,
151.808303150538,152.243176457288,152.678049763901,153.112923070379,153.547796376722,
153.982669682934,154.417542989014,154.852416294964,155.287289600787,155.722162906483,
156.157036212055,156.592762211626,157.028488211198,157.463361516526,157.898234821735,
158.333108126826,158.767981431803,159.202854736666,159.637728041419,160.072601346062,
160.507474650599,160.94234795503,161.37722125936,161.812094563589,162.246967867721,
162.681841171757,163.1167144757,163.552440474473,163.988166473247,164.423039777011,
164.85791308069,165.292786384286,165.727659687801,166.162532991238,166.597406294601,
167.03227959789,167.46715290111,167.902026204262,168.33689950735,168.771772810376,
169.206646113343,169.641519416254,170.076392719112,170.512118717363,170.947844715614,
171.382718018374,171.817591321089,172.252464623762,172.687337926397,173.122211228996,
173.557084531561,173.991957834097,174.426831136606,174.86170443909,175.296577741554,
175.731451044,176.16632434643,176.601197648848,177.036070951258,177.471796949306,
177.907522947355,178.342396249755,178.777269552155,179.212142854558,179.647016156968,
180.081889459386,180.516762761816,180.951636064262,181.386509366726,181.82138266921,
182.256255971719,182.691129274255,183.12600257682,183.560875879419,183.995749182054,
184.431475180237,184.867201178421,185.302074481136,185.736947783896,186.171821086704,
186.606694389561,187.041567692473,187.47644099544,187.911314298466,188.346187601554,
188.781060904706,189.215934207926,189.650807511215,190.085680814577,190.520554118015,
190.95542742153,191.391153420175,191.82687941882,192.261752722499,192.696626026263,
193.131499330116,193.566372634059,194.001245938095,194.436119242227,194.870992546456,
195.305865850785,195.740739155217,196.175612459754,196.610485764397,197.045359069149,
197.480232374013,197.915105678989,198.350831678382,198.786557677775,199.221430982984,
199.656304288312,200.091177593761,200.526050899333,200.960924205029,201.395797510852,
201.830670816802,202.265544122882,202.700417429093,203.135290735437,203.570164041915,
204.005037348528,204.439910655278,204.874783962166,205.310509962526,205.746235962887,
206.181109270054,206.615982577363,207.050855884814,207.485729192409,207.920602500147,
208.355475808031,208.79034911606,209.225222424235,209.660095732558,210.094969041027,
210.529842349645,210.96471565841,211.399588967324,211.834462276387,212.27018827784,
212.705914279292,213.140787588653,213.575660898161,214.010534207819,214.880280827579,
215.31515413768,215.750027447929,216.184900758324,216.619774068866,217.054647379553,
217.489520690384,218.359267312475,219.22986662628,219.665592628826,220.100465940363,
220.535339252038,220.970212563848,221.83995918787,222.709705812416,223.579452437468,
224.014325750179,224.44919906301,225.318945689022,226.189545005688,227.060144322571,
227.929890949664,228.799637577146,229.66938420499,230.539130833166,231.408877461643,
232.278624090388,233.149223408954,234.019822727623,234.889569356878,235.759315986267,
236.629062615749,237.498809245277,238.368555874806,239.238302504287,240.108901823183,
240.979501142017,241.849247771189,242.718994400167,243.588741028911,244.458487657389,
245.328234285565,246.197980913409,247.068580230891,247.939179548182,248.80892617507,
249.678672801532,250.548419427545,251.418166053087,252.287912678139,253.157659302684,
254.028258617581,254.898857932211,255.333731243885,255.768604555423,256.203477866821,
256.63835117808,257.508097800171,258.377844421689,258.812717732231,259.247591042627,
259.682464352876,260.117337662977,260.552210972931,260.987936974682,261.858536286089,
262.293409595598,262.728282904958,263.16315621417,263.598029523233,264.032902832147,
264.467776140913,264.902649449531,265.337522758001,265.772396066323,266.207269374499,
266.642142682528,267.077015990412,267.511889298151,267.947615298795,268.383341299439,
268.81821460689,269.2530879142,269.687961221367,270.122834528394,270.557707835282,
270.992581142032,271.427454448646,271.862327755124,272.297201061468,272.732074367679,
273.166947673759,273.60182097971,274.036694285533,274.471567591229,274.907293590862,
275.343019590495,275.777892895944,276.212766201272,276.647639506481,277.082512811573,
277.51738611655,277.952259421414,278.387132726166,278.82200603081,279.256879335346,
279.691752639779,280.126625944108,280.561499248338,280.996372552469,281.431245856506,
281.866971855324,282.302697854143,282.737571157996,283.172444461761,283.60731776544,
284.042191069036,284.477064372551,284.911937675989,285.346810979351,285.781684282641,
286.216557585861,286.651430889013,287.086304192101,287.521177495128,287.956050798095,
288.390924101007,288.826650099283,289.262376097559,289.697249400366,290.132122703127,
290.566996005842,291.001869308516,291.43674261115,291.871615913749,292.306489216315,
292.741362518851,293.17623582136,293.611109123845,294.045982426308,294.480855728754,
294.915729031185,295.350602333603,295.786328331655,296.222054329707,296.65692763211,
297.091800934511,297.526674236911,297.961547539314,298.396420841724,298.831294144142,
299.266167446573,299.701040749018,300.135914051482,300.570787353967,301.005660656476,
301.440533959012,301.875407261578,302.310280564177,302.746006562341,303.181732560506,
303.616605863179,304.051479165895,304.486352468655,304.921225771462,305.35609907432,
305.790972377232,306.225845680199,306.660718983226,307.095592286314,307.530465589466,
307.965338892686,308.400212195976,308.835085499338,309.269958802776,309.705684801381,
310.141410799985,310.576284103581,311.01115740726,311.446030711025,311.880904014878,
312.315777318821,312.750650622858,313.185523926989,313.620397231219,314.055270535549,
314.490143839981,314.925017144517,315.359890449161,315.794763753913,316.229637058777,
316.665363058112,317.101089057448,317.53596236254,317.970835667749,318.405708973077,
318.840582278526,319.275455584098,319.710328889795,320.145202195618,320.580075501568,
321.014948807648,321.44982211386,321.884695420204,322.319568726682,322.754442033295,
323.189315340045,323.625041340336,324.060767340628,324.495640647655,324.930513954822,
325.365387262131,325.800260569583,326.235133877177,326.670007184916,327.1048804928,
327.539753800829,327.974627109005,328.409500417327,328.844373725797,329.279247034415,
329.714120343181,330.148993652095,330.584719653474,331.020445654852,331.455318964064,
331.890192273424,332.325065582933,332.759938892591,333.194812202397,333.629685512351,
334.064558822453,334.499432132702,334.934305443098,335.369178753639,335.804052064326,
336.673798686132,337.108671997249,337.544397999725,337.980124002201,338.4149973136,
338.849870625137,339.284743936812,340.154490560568,341.024237184854,341.459110497191,
341.893983809655,342.328857122244,342.763730434955,343.633477060735,344.504076377234,
345.374675693955,346.244422320844,347.114168948136,347.983915575803,348.853662203817,
349.723408832148,350.593155460764,351.463754779246,352.334354097839,353.204100727012,
354.07384735634,354.943593985781,355.813340615292,356.683087244827,357.552833874338,
358.423433193272,359.294032512154,360.163779141409,361.033525770489,361.903272399355,
362.77301902797,363.642765656301,364.512512284316,365.383111601936,366.253710919371,
367.123457546465,367.993204173143,368.862950799383,369.732697425164,370.602444050463,
371.472190675265,372.342789990359,373.21338930519,373.648262617,374.083135928675,
374.952882551611,375.822629173987,376.257502484962,376.692375795793,377.12724910648,
377.562122417021,377.996995727417,378.431869037666,378.866742347767,379.302468349591,
379.738194351416,380.173067661222,380.607940970879,381.042814280388,381.477687589749,
381.91256089896,382.347434208023,382.782307516937,383.217180825703,383.652054134321,
384.086927442791,384.521800751113,384.956674059289,385.391547367318,385.826420675202,
386.262146675918,386.697872676635,387.13274598423,387.567619291681,388.00249259899,
388.437365906157,388.872239213185,389.307112520073,389.741985826823,390.176859133436,
390.611732439914,391.046605746258,391.48147905247,391.91635235855,392.351225664501,
392.786098970323,393.221824970019,393.657550969714,394.092424275286,394.527297580735,
394.962170886063,395.397044191272,395.831917496364,396.266790801341,396.701664106204,
397.136537410957,397.5714107156,398.006284020137,398.441157324569,398.876030628899,
399.310903933128,399.74577723726,400.181503236126,400.617229234991,401.052102538934,
401.486975842787,401.921849146551,402.356722450231,402.791595753827,403.226469057342,
403.66134236078,404.096215664142,404.531088967432,404.965962270651,405.400835573804,
405.835708876892,406.270582179918,406.705455482886,407.141181481189,407.576907479491,
408.01178078235,408.446654085157,408.881527387917,409.316400690633,409.751273993306,
410.186147295941,410.62102059854,411.055893901106,411.490767203642,411.925640506151,
412.360513808636,412.795387111099,413.230260413545,413.665133715976,414.100859714032,
414.536585712088,414.971459014498,415.406332316901,415.841205619301,416.276078921702,
416.710952224105,417.145825526515,417.580698828933,418.015572131364,418.45044543381,
418.885318736273,419.320192038758,419.755065341267,420.189938643803,420.624811946369,
421.060537944515,421.496263942662,421.931137245297,422.36601054797,422.800883850686,
423.235757153446,423.670630456253,424.105503759112,424.540377062023,424.975250364991,
425.410123668017,425.844996971105,426.279870274258,426.714743577477,427.149616880767,
427.584490184129,428.020216182695,428.455942181261,428.890815484776,429.325688788373,
429.760562092052,430.195435395816,430.630308699669,431.065182003612,431.500055307649,
431.93492861178,432.36980191601,432.80467522034,433.239548524772,433.674421829309,
434.109295133952,434.544168438705,434.979894437984,435.415620437262,435.850493742239,
436.285367047331,436.72024035254,437.155113657869,437.589986963318,438.024860268889,
438.459733574586,438.894606880409,439.32948018636,439.76435349244,440.199226798651,
440.634100104995,441.068973411473,441.503846718087,441.939572718309,442.375298718531,
442.810172025419,443.245045332447,443.679918639614,444.114791946923,444.549665254374,
444.984538561969,445.419411869708,445.854285177591,446.289158485621,446.724031793796,
447.158905102119,447.593778410589,448.028651719207,448.463525027973,448.899251029277,
449.334977030581,449.769850339644,450.639596958216,451.074470267725,451.509343577383,
451.944216887189,452.379090197143,452.813963507244,453.248836817493,453.683710127889,
454.118583438431,454.553456749117,454.988330059949,455.423203370923,455.858929373329,
456.294655375734,456.729528686993,457.164401998391,457.599275309929,458.469021933414,
458.90389524536,459.338768557437,459.773641869646,460.208515181983,460.643388494447,
461.078261807036,461.948008432578,462.818607748906,463.689207065461,464.55895369214,
465.428700319234,466.298446946716,467.16819357456,468.037940202737,468.907686831215,
469.778286149605,470.648885468116,471.518632097196,472.388378726451,473.258125355841,
474.127871985322,474.997618614851,475.86736524438,476.737964563343,477.608563882265,
478.478310511593,479.348057140765,480.217803769743,481.087550398488,481.957297026966,
482.827043655142,483.697642972895,484.568242290469,485.43798891776,486.307735544649,
487.177482171112,488.047228797125,488.916975422667,489.78672204772,490.657321363009,
491.09304736596,491.527920678038,492.397667301793,493.267413925005,494.137160547663,
494.57203385878,495.006907169755,495.441780480586,495.876653791273,496.311527101814,
496.74640041221,497.616999724357,498.052725726255,498.487599036209,498.922472346015,
499.357345655673,499.792218965182,500.227092274542,500.661965583754,501.096838892816,
501.531712201731,501.966585510497,502.401458819114,502.836332127584,503.271205435907,
503.706078744082,504.140952052112,504.576678052901,505.01240405369,505.447277361429,
505.882150669023,506.317023976474,506.751897283783,507.186770590951,507.621643897978,
508.056517204866,508.491390511616,508.92626381823,509.361137124708,509.796010431052,
510.230883737263,510.665757043344,511.100630349294,511.536356349053,511.972082348811,
512.406955654506,512.841828960076,513.276702265523,513.711575570849,514.146448876056,
514.581322181146,515.016195486121,515.451068790983,515.885942095733,516.320815400375,
516.75568870491,517.19056200934,517.625435313668,518.060308617896,518.496034616807,
518.931760615718,519.366633919752,519.801507223694,520.236380527545,520.671253831307,
521.106127134985,521.541000438579,521.975873742092,522.410747045528,522.845620348888,
523.280493652176,523.715366955394,524.150240258545,524.585113561631,525.019986864656,
525.455712862985,525.891438861313,526.326312164223,526.761185467079,527.196058769885,
527.630932072643,528.065805375356,528.500678678029,528.935551980661,529.370425283258,
529.805298585822,530.240171888356,530.675045190863,531.109918493346,531.544791795808,
531.979665098252,532.415391096312,532.851117094373,533.285990396789,533.720863699197,
534.155737001598,534.590610303997,535.025483606395,535.460356908796,535.895230211204,
536.330103513621,536.764976816049,537.199850118493,537.634723420955,538.069596723438,
538.504470025945,538.93934332848,539.375069326608,539.810795324736,540.245668627333,
540.680541929966,541.115415232637,541.550288535351,541.985161838109,542.420035140915,
542.854908443771,543.28978174668,543.724655049646,544.15952835267,544.594401655757,
545.029274958907,545.464148262125,545.899021565413,546.334747563939,546.770473562465,
547.205346865901,547.640220169415,548.075093473009,548.509966776686,548.944840080449,
549.3797133843,549.814586688241,550.249459992276,550.684333296405,551.119206600633,
551.554079904961,551.988953209391,552.423826513926,552.858699818567,553.294425817789,
553.73015181701,554.165025121872,554.599898426846,555.034771731937,555.469645037144,
555.90451834247,556.339391647917,556.774264953487,557.209138259182,557.644011565003,
558.078884870951,558.51375817703,558.948631483239,559.383504789581,559.818378096058,
560.254104096209,560.689830096361,561.12470340311,561.559576709996,561.994450017021,
562.429323324187,562.864196631494,563.299069938943,563.733943246536,564.168816554273,
564.603689862154,565.038563170182,565.473436478355,565.908309786676,566.343183095144,
566.77805640376,567.213782404988,567.649508406216,568.084381715128,568.519255024189,
568.954128333399,569.389001642757,569.823874952264,570.258748261921,570.693621571725,
571.128494881677,571.563368191777,572.433114812417,572.867988122957,573.302861433642,
573.737734744471,574.173460746804,574.609186749136,575.044060060251,575.913806682904,
576.783553306113,577.218426617922,577.653299929865,578.08817324194,578.523046554147,
579.392793178944,580.26253980424,581.13313912039,581.568865123709,582.003738436771,
582.87348506323,583.743231690115,584.612978317402,585.482724945065,586.352471573076,
587.222218201403,588.092817519691,588.963416838109,589.833163467083,590.702910096251,
591.572656725575,592.442403355013,593.31214998452,594.181896614051,595.05249593303,
595.92309525198,596.792841881366,597.662588510618,598.532335139693,599.402081768556,
600.271828397167,601.141575025495,602.012174343369,602.882773661074,603.752520288553,
604.622266915642,605.492013542317,606.361760168553,607.23150679433,608.101253419626,
608.971852735101,609.842452050322,610.71219867434,611.581945297822,612.451691920754,
612.886565232011,613.321438543126,613.756311854099,614.191185164928,615.060931786153,
615.931531098516,616.367257100486,616.802130410586,617.237003720538,617.671877030342,
618.106750339998,618.541623649505,618.976496958863,619.411370268073,619.846243577134,
620.281116886046,620.71599019481,621.150863503426,621.585736811894,622.020610120214,
622.455483428388,622.891209429248,623.326935430108,623.761808737989,624.196682045726,
624.631555353319,625.066428660769,625.501301968075,625.936175275241,626.371048582266,
626.805921889153,627.240795195901,627.675668502512,628.110541808988,628.54541511533,
628.98028842154,629.415161727618,629.850887727438,630.286613727259,630.72148703308,
631.156360338774,631.591233644344,632.026106949791,632.460980255118,632.895853560325,
633.330726865415,633.76560017039,634.200473475251,634.635346780002,635.070220084644,
635.505093389179,635.939966693609,636.374839997937,636.810565996897,637.246291995857,
637.681165299986,638.116038604021,638.550911907962,638.985785211813,639.420658515576,
639.855531819253,640.290405122847,640.725278426361,641.160151729796,641.595025033157,
642.029898336444,642.464771639662,642.899644942813,643.334518245899,643.770244244257,
644.205970242616,644.640843545581,645.075716848491,645.510590151347,645.945463454153,
646.380336756911,646.815210059625,647.250083362296,647.684956664929,648.119829967526,
648.55470327009,648.989576572624,649.424449875131,649.859323177614,650.294196480076,
650.729922478144,651.165648476212,651.600521778641,652.035395081057,652.470268383465,
652.905141685866,653.340014988265,653.774888290663,654.209761593065,654.644634895472,
655.079508197889,655.514381500318,655.949254802762,656.384128105224,656.819001407706,
657.253874710213,657.689600708326,658.12532670644,658.560200009004,658.995073311601,
659.429946614234,659.864819916905,660.299693219619,660.734566522377,661.169439825183,
661.604313128039,662.039186430948,662.474059733914,662.908933036938,663.343806340025,
663.778679643175,664.213552946393,664.649278944883,665.085004943373,665.519878246733,
665.954751550169,666.389624853683,666.824498157277,667.259371460954,667.694244764717,
668.129118068568,668.563991372509,668.998864676544,669.433737980674,669.868611284901,
670.303484589229,670.738357893659,671.173231198194,671.608957197361,672.044683196528,
672.479556501278,672.91442980614,673.349303111115,673.784176416205,674.219049721412,
674.653923026738,675.088796332185,675.523669637755,675.95854294345,676.393416249271,
676.82828955522,677.263162861298,677.698036167508,678.13290947385,678.568635473934,
679.004361474018,679.439234780629,679.874108087377,680.308981394264,680.743854701289,
681.178728008455,681.613601315762,682.048474623211,682.483347930804,682.91822123854,
683.353094546422,683.78796785445,684.222841162623,684.657714470944,685.092587779412,
685.528313780566,685.96403978172,686.398913090483,686.833786399396,687.268659708457,
687.703533017666,688.138406327025,688.573279636532,689.008152946187,689.443026255992,
689.877899565944,690.312772876043,690.74764618629,691.182519496684,691.617392807224,
692.052266117909,692.487992120169,692.92371812243,693.358591433403,694.228338055774,
694.663211367171,695.098084678707,695.532957990379,695.967831302188,696.402704614131,
696.837577926207,697.707324550749,698.577071175797,699.011944488507,699.447670491767,
699.883396495028,700.318269807975,701.188016434211,702.057763060886,702.927509687976,
703.797256315454,704.667002943295,705.536749571467,706.407348889651,707.277948207973,
708.147694836835,709.017441465911,709.887188095163,710.756934724548,711.626681354026,
712.496427983551,713.367027302543,714.237626621516,715.107373250954,715.977119880277,
716.846866509446,717.716613138419,718.586359767161,719.456106395635,720.32670571363,
721.197305031464,722.067051659126,722.936798286414,723.806544913299,724.676291539758,
725.546038165767,726.415784791305,727.286384106969,728.156983422381,729.026730046663,
729.896476670415,730.331349982088,730.766223293624,731.201096605021,731.635969916278,
732.505716538366,733.37546315988,733.81033647042,734.246062472462,734.681788474505,
735.116661784752,735.551535094852,735.986408404804,736.421281714608,736.856155024264,
737.291028333771,737.72590164313,738.160774952339,738.5956482614,739.030521570312,
739.465394879076,739.900268187692,740.33514149616,740.77001480448,741.205740805414,
741.641466806347,742.076340114374,742.511213422256,742.946086729993,743.380960037585,
743.815833345035,744.250706652341,744.685579959507,745.120453266533,745.555326573419,
745.990199880167,746.425073186778,746.859946493254,747.294819799596,747.729693105806,
748.165419105691,748.601145105576,749.036018411525,749.470891717346,749.90576502304,
750.34063832861,750.775511634057,751.210384939384,751.645258244591,752.080131549682,
752.515004854656,752.949878159518,753.384751464269,753.81962476891,754.254498073445,
754.689371377875,755.125097376885,755.560823375895,755.995696680123,756.430569984253,
756.865443288287,757.300316592228,757.735189896079,758.170063199842,758.604936503519,
759.039809807113,759.474683110627,759.909556414062,760.344429717423,760.779303020711,
761.214176323929,761.649049627079,762.084775625469,762.520501623858,762.955374926883,
763.390248229848,763.825121532758,764.259994835614,764.694868138419,765.129741441178,
765.564614743891,765.999488046563,766.434361349196,766.869234651793,767.304107954357,
767.738981256891,768.173854559398,768.608727861881,769.044453859958,769.480179858035,
769.915053160479,770.349926462907,770.784799765324,771.219673067731,771.654546370133,
772.089419672531,772.52429297493,772.959166277331,773.394039579739,773.828912882155,
774.263786184584,774.698659487028,775.13353278949,775.568406091973,776.004132090072,
776.439858088172,776.874731390706,777.30960469327,777.744477995867,778.1793512985,
778.614224601171,779.049097903885,779.483971206643,779.918844509449,780.353717812305,
780.788591115215,781.22346441818,781.658337721205,782.093211024291,782.528084327442,
782.963810325897,783.399536324352,783.834409627639,784.269282931,784.704156234435,
785.139029537949,785.573902841543,786.00877614522,786.443649448983,786.878522752834,
787.313396056775,787.74826936081,788.183142664939,788.618015969167,789.052889273495,
789.487762577925,789.923488577038,790.359214576152,790.794087880793,791.228961185544,
791.663834490406,792.098707795381,792.533581100471,792.968454405678,793.403327711004,
793.838201016451,794.273074322021,794.707947627716,795.142820933537,795.577694239486,
796.012567545564,796.447440851774,796.883166851791,797.318892851808,797.753766158284,
798.188639464895,798.623512771643,799.058386078529,799.493259385555,799.92813269272,
800.363006000027,800.797879307477,801.232752615069,801.667625922806,802.102499230688,
802.537372538715,802.972245846889,803.40711915521,803.84284515629,804.27857115737,
804.713444465985,805.148317774749,805.583191083662,806.018064392723,806.452937701933,
806.887811011291,807.322684320798,808.192430940258,808.62730425021,809.06217756031,
809.497050870557,809.931924180951,810.36679749149,810.802523493679,811.238249495867,
811.673122806697,812.542869428785,812.977742740041,813.412616051438,813.847489362974,
814.282362674646,814.717235986455,815.152109298398,816.021855922681,816.891602547478,
817.326475860065,817.762201863265,818.197927866466,818.632801179295,819.502547805304,
820.372294431763,821.242041058648,822.111787685935,822.981534313598,823.851280941609,
824.721880259681,825.5924795779,826.462226206642,827.331972835616,828.201719464785,
829.071466094109,829.941212723546,830.810959353053,831.681558672047,832.552157991036,
833.421904620514,834.2916512499,835.161397879151,836.031144508226,836.900891137089,
837.770637765701,838.641237083811,839.511836401767,840.381583029608,841.251329657086,
842.121076284176,842.990822910851,843.860569537087,844.730316162863,845.600915478712,
846.471514794314,847.341261418855,848.211008042874,848.645881354683,849.080754666356,
849.515627977891,849.950501289288,850.82024791166,851.689994533462,852.124867844147,
852.560593846263,852.996319848379,853.431193158772,853.866066469019,854.300939779119,
855.170686398875,855.605559708531,856.040433018038,856.475306327397,856.910179636606,
857.345052945667,857.77992625458,858.214799563344,858.64967287196,859.084546180427,
859.520272181434,859.95599818244,860.390871490614,860.825744798641,861.260618106523,
861.69549141426,862.130364721852,862.565238029302,863.000111336609,863.434984643774,
863.8698579508,864.304731257686,864.739604564434,865.174477871045,865.609351177521,
866.044224483863,866.479950483814,866.915676483765,867.350549789843,867.785423095792,
868.220296401613,868.655169707307,869.090043012877,869.524916318325,869.959789623651,
870.394662928858,870.829536233948,871.264409538923,871.699282843785,872.134156148535,
872.569029453177,873.003902757712,873.439628756773,873.875354755834,874.310228060162,
874.745101364389,875.179974668519,875.614847972553,876.049721276495,876.484594580346,
876.919467884108,877.354341187786,877.78921449138,878.224087794893,878.658961098329,
879.093834401689,879.528707704977,879.963581008195,880.399307006616,880.835033005038,
881.269906308124,881.704779611148,882.139652914114,882.574526217024,883.00939951988,
883.444272822685,883.879146125444,884.314019428157,884.748892730829,885.183766033462,
885.618639336059,886.053512638623,886.488385941157,886.923259243664,887.358985241751,
887.794711239839,888.2295845423,888.664457844744,889.099331147173,889.534204449589,
889.969077751997,890.403951054398,890.838824356797,891.273697659195,891.708570961597,
892.143444264004,892.578317566421,893.01319086885,893.448064171293,893.882937473755,
894.318663471843,894.75438946993,895.189262772437,895.624136074971,896.059009377535,
896.493882680132,896.928755982765,897.363629285437,897.798502588151,898.233375890909,
898.668249193715,899.103122496571,899.53799579948,899.972869102446,900.40774240547,
900.842615708556,901.278341706978,901.714067705399,902.148941008617,902.583814311905,
903.018687615265,903.453560918701,903.888434222214,904.323307525808,904.758180829485,
905.193054133248,905.627927437099,906.06280074104,906.497674045075,906.932547349205,
907.367420653433,907.80229395776,908.238019956821,908.673745955883,909.108619260417,
909.543492565059,909.978365869809,910.413239174671,910.848112479646,911.282985784736,
911.717859089943,912.152732395269,912.587605700716,913.022479006287,913.457352311981,
913.892225617802,914.327098923751,914.761972229829,915.19769822978,915.633424229731,
916.068297536072,916.503170842548,916.93804414916,917.372917455908,917.807790762794,
918.24266406982,918.677537376985,919.112410684292,919.547283991742,919.982157299334,
920.417030607071,920.851903914953,921.28677722298,921.721650531154,922.15737653216,
922.593102533167,923.027975841635,923.46284915025,923.897722459014,924.332595767926,
924.767469076987,925.202342386197,925.637215695556,926.072089005063,926.506962314719,
926.941835624523,927.376708934475,927.811582244575,928.246455554822,928.681328865215,
929.117054867331,929.987654180132,930.422527490961,930.857400801934,931.292274113049,
931.727147424306,932.162020735703,932.596894047238,933.46664067072,934.336387294739,
934.771260606945,935.20613391928,935.641007231742,936.076733234882,936.94733255073,
937.817079176507,938.686825802743,939.556572429418,940.426319056508,941.296065683986,
942.165812311827,943.036411629783,943.907010947893,944.776757576505,945.646504205367,
946.516250834443,947.385997463694,948.25574409308,949.125490722558,949.996090041546,
950.86668936054,951.736435990048,952.606182619485,953.475929248809,954.345675877978,
955.215422506951,956.085169135693,956.955768453912,957.826367771985,958.696114399995,
959.565861027658,960.435607654946,961.305354281831,962.175100908289,963.044847534298,
963.915446850328,964.786046166116,965.655792790913,966.525539415195,966.960412727138,
967.395286038947,968.265032662155,969.134779284809,969.569652595924,970.004525906897,
970.439399217726,970.875125219914,971.310851222103,971.745724532643,972.615471153283,
973.485217773335,973.920091083139,974.354964392795,974.789837702302,975.22471101166,
975.65958432087,976.094457629931,976.529330938844,976.964204247608,977.399077556223,
977.834803557303,978.270529558383,978.705402866704,979.140276174877,979.575149482905,
980.010022790786,980.444896098523,980.879769406116,981.314642713565,981.749516020872,
982.184389328038,982.619262635063,983.05413594195,983.489009248698,983.923882555309,
984.358755861785,984.794481861802,985.230207861819,985.665081168029,986.099954474107,
986.534827780056,986.969701085877,987.404574391571,987.839447697141,988.274321002589,
988.709194307915,989.144067613122,989.578940918212,990.013814223187,990.448687528048,
990.883560832799,991.31843413744,991.754160136554,992.189886135667,992.624759440097,
993.059632744425,993.494506048653,993.929379352783,994.364252656817,994.799125960758,
995.233999264609,995.668872568372,996.103745872049,996.538619175643,996.973492479157,
997.408365782593,997.843239085953,998.278112389241,998.713838387696,999.149564386151,
999.584437689301,1000.01931099239,1000.45418429541,1000.88905759838,1001.32393090129,
1001.75880420414,1002.19367750695,1002.62855080971,1003.06342411242,1003.49829741509,
1003.93317071773,1004.36804402032,1004.80291732289,1005.23779062542,1005.67351662352,
1006.10924262162,1006.5441159241,1006.97898922656,1007.41386252901,1007.84873583144,
1008.28360913385,1008.71848243626,1009.15335573866,1009.58822904106,1010.02310234346,
1010.45797564586,1010.89284894827,1011.32772225069,1011.76259555311,1012.19746885556,
1012.63319485364,1013.06892085171,1013.5037941542,1013.9386674567,1014.37354075924,
1014.8084140618,1015.2432873644,1015.67816066703,1016.1130339697,1016.54790727242,
1016.98278057517,1017.41765387798,1017.85252718084,1018.28740048375,1018.72227378671,
1019.15714708974,1019.59287308813,1020.02859908651,1020.46347238967,1020.89834569288,
1021.33321899617,1021.76809229953,1022.20296560297,1022.63783890648,1023.07271221007,
1023.50758551375,1023.94245881752,1024.37733212137,1024.81220542531,1025.24707872935,
1025.68195203348,1026.11682533771,1026.55255133672,1026.98827733573,1027.42315064016,
1027.8580239447,1028.29289724934,1028.72777055409,1029.16264385896,1029.59751716393,
1030.03239046902,1030.46726377423,1030.90213707956,1031.33701038501,1031.77188369058,
1032.20675699628,1032.6416303021,1033.07650360805,1033.51222960793,1033.94795560782,
1034.38282891403,1034.81770222038,1035.25257552685,1035.68744883347,1036.12232214022,
1036.5571954471,1036.99206875413,1037.4269420613,1037.86181536861,1038.29668867606,
1038.73156198365,1039.16643529139,1039.60130859927,1040.0361819073,1040.47190790824,
1040.90763390917,1041.34250721749,1041.77738052596,1042.21225383458,1042.64712714334,
1043.08200045226,1043.95174707053,1044.38662037989,1044.8214936894,1045.25636699906,
1045.69124030886,1046.12611361882,1046.56098692892,1046.99586023917,1047.43158624121,
1047.86731224325,1048.3021855538,1048.73705886448,1049.17193217531,1049.60680548629,
1050.0416787974,1050.47655210866,1050.91142542006,1051.78117204327,1052.21604535508,
1052.65091866703,1053.0857919791,1053.52066529131,1053.95553860365,1054.39126460673,
1055.26186392239,1056.13161054793,1057.00135717395,1057.43623048712,1057.87110380041,
1058.7408504273,1059.61059705459,1060.48034368225,1061.35094300009,1062.22154231809,
1063.09128894656,1063.96103557531,1064.83078220429,1065.70052883346,1066.57027546278,
1067.44002209222,1068.3106214112,1069.18122073019,1070.05096735972,1070.9207139892,
1071.79046061859,1072.66020724785,1073.52995387693,1074.39970050579,1075.27029982411,
1076.1408991423,1077.01064577048,1077.88039239832,1078.7501390258,1079.61988565289,
1080.48963227957,1081.35937890581,1082.22997822202,1083.100577538,1083.97032416305,
1084.84007078759,1085.70981741161,1086.5795640351,1087.44931065803,1087.88418396929,
1088.31905728041,1088.75393059138,1089.18965659365,1089.62538259591,1090.06025590659,
1090.93000252753,1091.36487583778,1091.79974914788,1092.23462245783,1092.66949576764,
1093.1043690773,1093.5392423868,1093.97411569616,1094.40898900538,1094.84386231444,
1095.27873562335,1095.71360893212,1096.14933493327,1096.58506093443,1097.0199342429,
1097.45480755122,1097.88968085939,1098.32455416742,1098.75942747531,1099.19430078305,
1099.62917409064,1100.06404739809,1100.4989207054,1100.93379401257,1101.36866731959,
1101.80354062648,1102.23841393323,1102.67328723984,1103.10901323993,1103.54473924001,
1103.97961254636,1104.41448585257,1104.84935915865,1105.2842324646,1105.71910577042,
1106.15397907612,1106.58885238169,1107.02372568714,1107.45859899246,1107.89347229767,
1108.32834560276,1108.76321890774,1109.1980922126,1109.63296551736,1110.06869151652,
1110.50441751569,1110.93929082023,1111.37416412466,1111.80903742899,1112.24391073322,
1112.67878403735,1113.11365734139,1113.54853064533,1113.98340394918,1114.41827725295,
1114.85315055662,1115.28802386022,1115.72289716374,1116.15777046717,1116.59264377053,
1117.02836976903,1117.46409576752,1117.89896907074,1118.33384237389,1118.76871567698,
1119.20358898,1119.63846228297,1120.07333558588,1120.50820888874,1120.94308219154,
1121.3779554943,1121.81282879702,1122.24770209969,1122.68257540233,1123.11744870492,
1123.55232200749,1123.98804800561,1124.42377400372,1124.85864730623,1125.29352060871,
1125.72839391118,1126.16326721362,1126.59814051605,1127.03301381847,1127.46788712088,
1127.90276042328,1128.33763372568,1128.77250702808,1129.20738033048,1129.64225363289,
1130.07712693531,1130.51200023774,1130.94772623581,1131.38345223388,1131.81832553634,
1132.25319883883,1132.68807214134,1133.12294544387,1133.55781874644,1133.99269204904,
1134.42756535167,1134.86243865434,1135.29731195706,1135.73218525982,1136.16705856263,
1136.60193186548,1137.03680516839,1137.47167847136,1137.90740446972,1138.34313046808,
1138.77800377117,1139.21287707432,1139.64775037754,1140.08262368083,1140.51749698419,
1140.95237028763,1141.38724359114,1141.82211689474,1142.25699019842,1142.69186350218,
1143.12673680603,1143.56161010998,1143.99648341401,1144.43135671814,1144.86708271711,
1145.30280871607,1145.7376820204,1146.17255532483,1146.60742862936,1147.04230193401,
1147.47717523876,1147.91204854362,1148.3469218486,1148.78179515369,1149.2166684589,
1149.65154176423,1150.08641506968,1150.52128837525,1150.95616168094,1151.39103498677,
1151.82676098659,1152.26248698641,1152.69736029249,1153.1322335987,1153.56710690504,
1154.00198021152,1154.43685351813,1154.87172682488,1155.30660013177,1155.7414734388,
1156.17634674597,1156.61122005327,1157.04609336073,1157.48096666832,1157.91583997606,
1158.35071328394,1158.7864392848,1159.22216528566,1159.65703859384,1160.09191190216,
1160.52678521063,1160.96165851925,1161.39653182801,1161.83140513693,1162.26627844599,
1162.7011517552,1163.13602506456,1163.57089837407,1164.00577168373,1164.44064499353,
1164.87551830349,1165.74611761556,1166.18184361753,1166.61671692792,1167.05159023846,
1167.48646354915,1167.92133685998,1168.35621017096,1169.22595679333,1170.09570341627,
1170.53057672794,1170.96545003975,1171.4003233517,1171.83519666377,1172.27006997598,
1172.705795979,1173.57639529447,1174.44614191977,1174.8810152326,1175.31588854555,
1176.18563517179,1177.05538179847,1177.92512842556,1178.79487505304,1179.66547437075,
1180.53607368863,1181.40582031696,1182.27556694557,1183.14531357444,1184.01506020352,
1184.88480683277,1185.75455346216,1186.62515278112,1187.4957521001,1188.36549872963,
1189.23524535914,1190.10499198858,1190.97473861791,1191.84448524708,1192.71423187606,
1193.58483119448,1194.45543051277,1195.3251771411,1196.19492376911,1197.06467039678,
1197.93441702407,1198.80416365096,1199.67391027742,1200.5445095938,1201.41510890996,
1202.28485553525,1203.15460216005,1204.02434878434,1204.89409540809,1205.76384203131,
1206.1987153427,1206.63358865396,1207.06846196508,1207.50418796741,1208.37478728058,
1209.2445339018,1209.6794072122,1210.11428052245,1210.54915383255,1210.9840271425,
1211.41890045231,1211.85377376197,1212.28864707147,1212.72352038083,1213.15839369005,
1213.59326699911,1214.02814030802,1214.46386630925,1214.89959231048,1215.3344656191,
1215.76933892757,1216.20421223589,1216.63908554406,1217.07395885209,1217.50883215998,
1217.94370546771,1218.37857877531,1218.81345208276,1219.24832539007,1219.68319869724,
1220.11807200426,1220.55294531115,1220.9878186179,1221.42354461805,1221.85927061821,
1222.29414392468,1222.72901723103,1223.16389053724,1223.59876384332,1224.03363714927,
1224.46851045509,1224.90338376079,1225.33825706636,1225.77313037181,1226.20800367713,
1226.64287698234,1227.07775028743,1227.51262359241,1227.94749689727,1228.3832228965,
1228.81894889572,1229.25382220036,1229.6886955049,1230.12356880933,1230.55844211366,
1230.99331541789,1231.42818872202,1231.86306202606,1232.29793533,1232.73280863385,
1233.16768193762,1233.60255524129,1234.03742854489,1234.4723018484,1234.90717515184,
1235.34290115037,1235.7786271489,1236.21350045219,1236.64837375541,1237.08324705856,
1237.51812036165,1237.95299366467,1238.38786696764,1238.82274027055,1239.25761357341,
1239.69248687621,1240.12736017897,1240.56223348169,1240.99710678436,1241.431980087,
1241.8668533896,1242.30257938773,1242.73830538585,1243.17317868839,1243.6080519909,
1244.04292529338,1244.47779859585,1244.91267189829,1245.34754520072,1245.78241850314,
1246.21729180555,1246.65216510795,1247.08703841035,1247.52191171275,1247.95678501515,
1248.39165831756,1248.82653161998,1249.26225761804,1249.69798361611,1250.13285691855,
1250.56773022101,1251.0026035235,1251.43747682601,1251.87235012854,1252.30722343111,
1252.74209673371,1253.17697003634,1253.61184333901,1254.04671664173,1254.48158994449,
1254.9164632473,1255.35133655015,1255.78620985306,1256.22193585139,1256.65766184973,
1257.09253515275,1257.52740845584,1257.96228175899,1258.39715506221,1258.8320283655,
1259.26690166886,1259.7017749723,1260.13664827581,1260.57152157941,1261.00639488309,
1261.44126818685,1261.8761414907,1262.31101479465,1262.74588809868,1263.1816140976,
1263.61734009651,1264.05221340074,1264.48708670507,1264.9219600095,1265.35683331403,
1265.79170661868,1266.22657992343,1266.66145322829,1267.09632653327,1267.53119983836,
1267.96607314357,1268.4009464489,1268.83581975434,1269.27069305992,1269.70556636561,
1270.14129236537,1270.57701836513,1271.01189167108,1271.44676497716,1271.88163828337,
1272.31651158971,1272.75138489619,1273.1862582028,1273.62113150955,1274.05600481644,
1274.49087812347,1274.92575143063,1275.36062473794,1275.79549804539,1276.23037135299,
1276.66524466073,1277.10097066151,1277.5366966623,1277.97156997033,1278.40644327851,
1278.84131658683,1279.2761898953,1279.71106320392,1280.14593651268,1280.5808098216,
1281.01568313066,1281.45055643987,1281.88542974923,1282.32030305874,1282.75517636839,
1283.1900496782,1283.62492298815,1284.06064899005,1284.49637499195,1284.9312483022,
1285.36612161259,1285.80099492313,1286.23586823382,1286.67074154465,1287.54048816674,
1287.975361478,1288.4102347894,1288.84510810093,1289.27998141261,1289.71485472442,
1290.14972803636,1291.02032735139,1291.89092666668,1292.32579997914,1292.76067329173,
1293.19554660444,1293.63041991727,1294.50016654328,1295.36991316974,1296.23965979663,
1297.10940642392,1297.9800057415,1298.85060505925,1299.72035168742,1300.5900983159,
1301.45984494464,1302.32959157362,1303.19933820279,1304.06908483212,1304.93968415104,
1305.81028347,1306.68003009953,1307.54977672906,1308.41952335854,1309.28926998793,
1310.15901661718,1311.02876324626,1311.89936256477,1312.76996188316,1313.63970851164,
1314.50945513981,1315.37920176765,1316.24894839514,1317.11869502223,1317.98844164891,
1318.85904096546,1319.72964028179,1320.59938690733,1321.46913353238,1322.33888015692,
1323.20862678095,1323.64350009276,1324.07837340443,1324.51324671597,1324.94812002737,
1325.81871934103,1326.68931865441,1327.12419196524,1327.55906527593,1327.99393858647,
1328.42881189686,1328.86368520711,1329.29855851721,1329.73343182716,1330.16830513697,
1330.60317844663,1331.03805175614,1331.4729250655,1331.90779837471,1332.34267168377,
1332.77839768507,1333.21412368638,1333.64899699514,1334.08387030376,1334.51874361223,
1334.95361692055,1335.38849022873,1335.82336353676,1336.25823684464,1336.69311015238,
1337.12798345997,1337.56285676742,1337.99773007473,1338.4326033819,1338.86747668892,
1339.30234999581,1339.73807599603,1340.17380199625,1340.60867530287,1341.04354860934,
1341.47842191569,1341.9132952219,1342.34816852798,1342.78304183393,1343.21791513975,
1343.65278844545,1344.08766175102,1344.52253505647,1344.95740836179,1345.392281667,
1345.82715497209,1346.26202827707,1346.69775427635,1347.13348027563,1347.56835358038,
1348.00322688502,1348.43810018956,1348.87297349399,1349.30784679832,1349.74272010255,
1350.17759340668,1350.61246671072,1351.04734001466,1351.48221331851,1351.91708662228,
1352.35195992595,1352.78683322955,1353.22170653306,1353.65743253163,1354.09315853019,
1354.52803183356,1354.96290513685,1355.39777844007,1355.83265174322,1356.26752504631,
1356.70239834933,1357.1372716523,1357.57214495521,1358.00701825807,1358.44189156087,
1358.87676486363,1359.31163816635,1359.74651146902,1360.18138477166,1360.6171107698,
1361.05283676795,1361.48771007051,1361.92258337305,1362.35745667556,1362.79232997804,
1363.2272032805,1363.66207658295,1364.09694988538,1364.5318231878,1364.96669649021,
1365.40156979261,1365.83644309501,1366.27131639741,1366.70618969981,1367.14106300222,
1367.57678900028,1368.01251499834,1368.44738830077,1368.88226160321,1369.31713490567,
1369.75200820816,1370.18688151067,1370.6217548132,1371.05662811577,1371.49150141837,
1371.926374721,1372.36124802367,1372.79612132639,1373.23099462915,1373.66586793196,
1374.10074123481,1374.53646723311,1374.97219323142,1375.40706653438,1375.84193983741,
1376.2768131405,1376.71168644365,1377.14655974687,1377.58143305016,1378.01630635352,
1378.45117965696,1378.88605296047,1379.32092626407,1379.75579956775,1380.19067287151,
1380.62554617536,1381.06041947931,1381.49614547817,1381.93187147704,1382.36674478117,
1382.8016180854,1383.23649138973,1383.67136469416,1384.10623799869,1384.54111130334,
1384.97598460809,1385.41085791295,1385.84573121793,1386.28060452302,1386.71547782823,
1387.15035113356,1387.585224439,1388.02009774458,1388.45582374427,1388.89154974397,
1389.32642304979,1389.76129635574,1390.19616966182,1390.63104296803,1391.06591627437,
1391.50078958085,1391.93566288746,1392.37053619421,1392.8054095011,1393.24028280813,
1393.6751561153,1394.1100294226,1394.54490273005,1394.97977603765,1395.41550203836,
1395.85122803908,1396.28610134696,1396.72097465499,1397.15584796317,1397.59072127149,
1398.02559457996,1398.46046788858,1398.89534119734,1399.33021450626,1399.76508781532,
1400.19996112453,1400.63483443389,1401.50458105306,1401.93945436286,1402.37518036469,
1402.81090636651,1403.24577967661,1403.68065298686,1404.11552629725,1404.5503996078,
1404.98527291848,1405.85501954029,1406.2898928514,1406.72476616266,1407.15963947406,
1407.5945127856,1408.02938609727,1408.46425940908,1409.33485872391,1410.205458039,
1410.64033135134,1411.07520466381,1411.51007797639,1411.9449512891,1412.81469791488,
1413.68444454112,1414.5541911678,1415.42393779489,1416.29453711233,1417.16513642995,
1418.03488305796,1418.90462968629,1419.77437631491,1420.64412294377,1421.51386957285,
1422.38361620211,1423.25421552099,1424.12481483992,1424.99456146943,1425.86430809896,
1426.73405472847,1427.60380135791,1428.47354798724,1429.34329461641,1430.21389393501,
1431.08449325349,1431.9542398821,1432.82398651043,1433.69373313844,1434.56347976611,
1435.4332263934,1436.30297302029,1437.17357233701,1438.04417165351,1438.91391827929,
1439.78366490459,1440.65341152939,1441.52315815367,1441.95803146562,1442.39290477743,
1442.8277780891,1443.26265140064,1444.13325071451,1445.00385002811,1445.43872333908,
1445.87359664991,1446.3084699606,1446.74334327114,1447.17821658153,1447.61308989178,
1448.48283651184,1448.91770982164,1449.3525831313,1449.78745644081,1450.22232975017,
1450.65720305938,1451.09292906076,1451.52865506214,1451.96352837105,1452.39840167982,
1452.83327498843,1453.2681482969,1453.70302160522,1454.1378949134,1454.57276822143,
1455.00764152931,1455.44251483705,1455.87738814464,1456.31226145209,1456.7471347594,
1457.18200806657,1457.6168813736,1458.05260737389,1458.48833337418,1458.92320668093,
1459.35807998754,1459.79295329402,1460.22782660036,1460.66269990657,1461.09757321265,
1461.5324465186,1461.96731982443,1462.40219313012,1462.83706643569,1463.27193974114,
1463.70681304647,1464.14168635168,1464.57655965677,1465.0122856561,1465.44801165544,
1465.8828849603,1466.31775826505,1466.7526315697,1467.18750487423,1467.62237817866,
1468.05725148299,1468.49212478722,1468.92699809135,1469.36187139539,1469.79674469933,
1470.23161800319,1470.66649130695,1471.10136461063,1471.53623791422,1471.97196391283,
1472.40768991143,1472.84256321487,1473.27743651823,1473.71230982152,1474.14718312474,
1474.58205642789,1475.01692973098,1475.451803034,1475.88667633697,1476.32154963988,
1476.75642294274,1477.19129624555,1477.62616954831,1478.06104285102,1478.4959161537,
1478.93164215186,1479.36736815002,1479.80224145262,1480.23711475519,1480.67198805772,
1481.10686136023,1481.54173466272,1481.97660796518,1482.41148126762,1482.84635457005,
1483.28122787247,1483.71610117488,1484.15097447728,1484.58584777968,1485.02072108208,
1485.45559438449,1485.89132038254,1486.32704638059,1486.76191968301,1487.19679298544,
1487.63166628788,1488.06653959035,1488.50141289283,1488.93628619534,1489.37115949787,
1489.80603280044,1490.24090610304,1490.67577940567,1491.11065270835,1491.54552601106,
1491.98039931382,1492.41527261663,1492.8509986149,1493.28672461318,1493.72159791609,
1494.15647121906,1494.59134452208,1495.02621782517,1495.46109112832,1495.89596443154,
1496.33083773483,1496.76571103819,1497.20058434163,1497.63545764515,1498.07033094874,
1498.50520425242,1498.94007755618,1499.37495086004,1499.81067685885,1500.24640285767,
1500.68127616171,1501.11614946584,1501.55102277007,1501.9858960744,1502.42076937883,
1502.85564268337,1503.29051598801,1503.72538929276,1504.16026259762,1504.5951359026,
1505.03000920769,1505.4648825129,1505.89975581823,1506.33462912368,1506.77035512331,
1507.20608112294,1507.64095442864,1508.07582773446,1508.51070104041,1508.94557434649,
1509.3804476527,1509.81532095904,1510.25019426552,1510.68506757213,1511.11994087888,
1511.55481418577,1511.9896874928,1512.42456079996,1512.85943410727,1513.29430741472,
1513.73003341537,1514.16575941601,1514.60063272375,1515.03550603163,1515.47037933966,
1515.90525264784,1516.34012595616,1516.77499926463,1517.20987257325,1517.64474588201,
1518.07961919093,1518.51449249999,1518.9493658092,1519.38423911856,1519.81911242807,
1520.25398573772,1520.68971173947,1521.12543774122,1521.56031105118,1521.99518436128,
1522.43005767153,1523.29980429246,1523.73467760315,1524.16955091398,1524.60442422495,
1525.03929753607,1525.47417084733,1525.90904415873,1526.77879078194,1527.64939009657,
1528.08511609939,1528.51998941146,1528.95486272367,1529.38973603601,1530.25948266106,
1531.1292292866,1531.99897591261,1532.86872253907,1533.73846916596,1534.60906848325,
1535.47966780073,1536.34941442858,1537.21916105675,1538.08890768523,1538.95865431398,
1539.82840094295,1540.69814757212,1541.56874689096,1542.43934620985,1543.30909283933,
1544.17883946886,1545.04858609839,1545.91833272787,1546.78807935726,1547.65782598651,
1548.52842530518,1549.39902462375,1550.26877125249,1551.13851788097,1552.00826450914,
1552.87801113699,1553.74775776447,1554.61750439156,1555.48810370844,1556.35870302511,
1557.22844965112,1558.09819627666,1558.96794290171,1559.83768952626,1560.27256283834,
1560.70743615028,1561.57718277377,1562.44778208785,1563.31838140165,1563.75325471277,
1564.18812802374,1564.62300133457,1565.05787464526,1565.9276212662,1566.79736788655,
1567.2322411965,1567.66711450631,1568.10198781596,1568.53686112547,1568.97173443483,
1569.40746043628,1569.84318643774,1570.2780597468,1570.71293305571,1571.14780636448,
1571.5826796731,1572.01755298157,1572.45242628989,1572.88729959806,1573.32217290609,
1573.75704621397,1574.19191952171,1574.62679282931,1575.06166613676,1575.49653944407,
1575.93141275123,1576.36713875159,1576.80286475195,1577.23773805884,1577.67261136559,
1578.1074846722,1578.54235797868,1578.97723128502,1579.41210459124,1579.84697789732,
1580.28185120327,1580.71672450909,1581.15159781478,1581.58647112036,1582.0213444258,
1582.45621773113,1582.89109103634,1583.32681703573,1583.76254303513,1584.1974163401,
1584.63228964497,1585.06716294972,1585.50203625436,1585.9369095589,1586.37178286333,
1586.80665616766,1587.24152947189,1587.67640277602,1588.11127608005,1588.546149384,
1588.98102268785,1589.41589599161,1589.85076929529,1590.28649529394,1590.72222129258,
1591.1570945961,1591.59196789953,1592.0268412029,1592.46171450619,1592.8965878094,
1593.33146111256,1593.76633441564,1594.20120771867,1594.63608102164,1595.07095432455,
1595.50582762741,1595.94070093021,1596.37557423297,1596.81044753569,1597.24617353387,
1597.68189953206,1598.11677283469,1598.55164613729,1598.98651943985,1599.42139274239,
1599.8562660449,1600.29113934738,1600.72601264985,1601.16088595229,1601.59575925472,
1602.03063255714,1602.46550585955,1602.90037916195,1603.33525246435,1603.77012576675,
1604.2058517648,1604.64157776285,1605.07645106526,1605.51132436768,1605.94619767011,
1606.38107097255,1606.81594427502,1607.2508175775,1607.68569088001,1608.12056418254,
1608.55543748511,1608.99031078771,1609.42518409034,1609.86005739302,1610.29493069573,
1610.72980399849,1611.16552999674,1611.60125599499,1612.03612929785,1612.47100260076,
1612.90587590373,1613.34074920675,1613.77562250984,1614.21049581299,1614.64536911621,
1615.0802424195,1615.51511572286,1615.9499890263,1616.38486232981,1616.81973563341,
1617.25460893709,1617.68948224085,1618.12520823963,1618.5609342384,1618.99580754234,
1619.43068084638,1619.86555415051,1620.30042745474,1620.73530075907,1621.1701740635,
1621.60504736804,1622.03992067268,1622.47479397743,1622.90966728229,1623.34454058727,
1623.77941389236,1624.21428719757,1624.6491605029,1625.08488650247,1625.52061250204,
1625.95548580761,1626.39035911331,1626.82523241913,1627.26010572508,1627.69497903116,
1628.12985233737,1628.56472564372,1628.99959895019,1629.43447225681,1629.86934556356,
1630.30421887044,1630.73909217747,1631.17396548464,1631.60883879195,1632.04456479252,
1632.48029079309,1632.91516410068,1633.35003740842,1633.78491071631,1634.21978402433,
1634.65465733251,1635.08953064083,1635.5244039493,1635.95927725792,1636.39415056668,
1636.8290238756,1637.26389718466,1637.69877049387,1638.13364380323,1638.56851711274,
1639.00424311442,1639.43996911609,1639.8748424259,1640.30971573585,1640.74458904595,
1641.6143356666,1642.04920897714,1642.48408228782,1642.91895559865,1643.35382890963,
1643.78870222074,1644.223575532,1645.09332215494,1645.52819546661,1645.96392146936,
1646.39964747212,1646.83452078406,1647.26939409614,1647.70426740834,1648.57401403314,
1649.44376065844,1650.31350728422,1650.74838059729,1651.18325391046,1652.05300053714,
1652.92359985428,1653.79419917162,1654.66394579929,1655.5336924273,1656.40343905563,
1657.27318568424,1658.14293231311,1659.01267894219,1659.88327826096,1660.75387757982,
1661.62362420926,1662.49337083877,1663.3631174683,1664.23286409781,1665.10261072725,
1665.97235735658,1666.84295667531,1667.71355599396,1668.58330262282,1669.45304925143,
1670.32279587976,1671.19254250778,1672.06228913544,1672.93203576273,1673.80263507977,
1674.6732343966,1675.54298102284,1676.41272764862,1677.28247427392,1678.15222089872,
1679.021967523,1679.89171414676,1680.76231346105,1681.19803946366,1681.63291277506,
1682.06778608632,1682.50265939743,1682.93753270841,1683.37240601924,1684.24215264047,
1684.67702595086,1685.11189926111,1685.54677257121,1685.98164588116,1686.41651919097,
1686.85139250063,1687.28626581014,1687.72199181166,1688.15771781319,1688.5925911224,
1689.02746443146,1689.46233774038,1689.89721104914,1690.33208435776,1690.76695766623,
1691.20183097455,1691.63670428272,1692.07157759075,1692.50645089864,1692.94132420637,
1693.37619751397,1693.81107082142,1694.24594412873,1694.68167012916,1695.11739612959,
1695.55226943662,1695.9871427435,1696.42201605025,1696.85688935687,1697.29176266334,
1697.72663596969,1698.1615092759,1698.59638258198,1699.03125588793,1699.46612919375,
1699.90100249945,1700.33587580502,1700.77074911047,1701.20562241579,1701.64134841525,
1702.0770744147,1702.51194771979,1702.94682102476,1703.38169432963,1703.81656763438,
1704.25144093902,1704.68631424356,1705.12118754799,1705.55606085232,1705.99093415655,
1706.42580746068,1706.86068076471,1707.29555406866,1707.73042737251,1708.16530067627,
1708.60102667496,1709.03675267365,1709.47162597724,1709.90649928076,1710.34137258419,
1710.77624588756,1711.21111919085,1711.64599249406,1712.08086579722,1712.5157391003,
1712.95061240333,1713.3854857063,1713.82035900921,1714.25523231207,1714.69010561487,
1715.12497891763,1715.56070491584,1715.99643091404,1716.43130421671,1716.86617751935,
1717.30105082195,1717.73592412451,1718.17079742705,1718.60567072956,1719.04054403204,
1719.4754173345,1719.91029063695,1720.34516393938,1720.7800372418,1721.21491054421,
1721.64978384661,1722.08465714901,1722.52038314706,1722.9561091451,1723.39098244751,
1723.82585574992,1724.26072905233,1724.69560235476,1725.13047565721,1725.56534895967,
1726.00022226216,1726.43509556467,1726.8699688672,1727.30484216977,1727.73971547236,
1728.174588775,1728.60946207767,1729.04433538039,1729.48006137861,1729.91578737684,
1730.35066067965,1730.78553398251,1731.22040728542,1731.65528058838,1732.09015389141,
1732.5250271945,1732.95990049765,1733.39477380087,1733.82964710416,1734.26452040752,
1734.69939371096,1735.13426701447,1735.56914031807,1736.00401362175,1736.43973962048,
1736.8754656192,1737.31033892306,1737.745212227,1738.18008553104,1738.61495883517,
1739.0498321394,1739.48470544373,1739.91957874816,1740.35445205269,1740.78932535734,
1741.22419866209,1741.65907196695,1742.09394527193,1742.52881857702,1742.96369188223,
1743.39941788174,1743.83514388125,1744.2700171867,1744.70489049227,1745.13976379797,
1745.57463710379,1746.00951040974,1746.44438371582,1746.87925702203,1747.31413032837,
1747.74900363485,1748.18387694146,1748.61875024821,1749.0536235551,1749.48849686213,
1749.92337016929,1750.3590961698,1750.7948221703,1751.22969547775,1751.66456878534,
1752.09944209308,1752.53431540096,1752.96918870899,1753.40406201717,1753.83893532549,
1754.27380863396,1754.70868194258,1755.14355525134,1755.57842856026,1756.01330186932,
1756.44817517853,1756.88304848789,1757.31877448949,1757.75450049109,1758.18937380075,
1759.05912042051,1759.49399373061,1759.92886704086,1760.36374035125,1760.79861366179,
1761.23348697248,1761.66836028331,1762.10323359429,1762.5381069054,1763.40785352806,
1763.8427268396,1764.27845284228,1764.71417884496,1765.14905215677,1765.58392546872,
1766.0187987808,1766.88854540534,1767.75829203039,1768.1931653431,1768.62803865593,
1769.06291196888,1769.49778528195,1770.36753190841,1771.2381312254,1772.10873054259,
1772.97847717007,1773.84822379791,1774.71797042609,1775.58771705456,1776.45746368331,
1777.32721031228,1778.19780963089,1779.06840894783,1779.93815555508,1780.80790201176,
1781.67764871408),.UNSPECIFIED.) ;
#833 = B_SPLINE_SURFACE_WITH_KNOTS('',1,3,((#88677,#88678,#88679,#88680,#88681,
#88682,#88683,#88684,#88685,#88686,#88687,#88688,#88689,#88690,#88691,#88692,
#88693,#88694,#88695,#88696,#88697,#88698,#88699,#88700,#88701,#88702,#88703,
#88704,#88705,#88706,#88707,#88708,#88709,#88710,#88711,#88712,#88713,#88714,
#88715,#88716,#88717,#88718,#88719,#88720,#88721,#88722,#88723,#88724,#88725,
#88726,#88727,#88728,#88729,#88730,#88731,#88732,#88733,#88734,#88735,#88736,
#88737,#88738,#88739,#88740,#88741,#88742,#88743,#88744,#88745,#88746,#88747,
#88748,#88749,#88750,#88751,#88752,#88753,#88754,#88755,#88756,#88757,#88758,
#88759,#88760,#88761,#88762,#88763,#88764,#88765,#88766,#88767,#88768,#88769,
#88770,#88771,#88772,#88773,#88774,#88775,#88776,#88777,#88778,#88779,#88780,
#88781,#88782,#88783,#88784,#88785,#88786,#88787,#88788,#88789,#88790,#88791,
#88792,#88793,#88794,#88795,#88796,#88797,#88798,#88799,#88800,#88801,#88802,
#88803,#88804,#88805,#88806,#88807,#88808,#88809,#88810,#88811,#88812,#88813,
#88814,#88815,#88816,#88817,#88818,#88819,#88820,#88821,#88822,#88823,#88824,
#88825,#88826,#88827,#88828,#88829,#88830,#88831,#88832,#88833,#88834,#88835,
#88836,#88837,#88838,#88839,#88840,#88841,#88842,#88843,#88844,#88845,#88846,
#88847,#88848,#88849,#88850,#88851,#88852,#88853,#88854,#88855,#88856,#88857,
#88858,#88859,#88860,#88861,#88862,#88863,#88864,#88865,#88866,#88867,#88868,
#88869,#88870,#88871,#88872,#88873,#88874,#88875,#88876,#88877,#88878,#88879,
#88880,#88881,#88882,#88883,#88884,#88885,#88886,#88887,#88888,#88889,#88890,
#88891,#88892,#88893,#88894,#88895,#88896,#88897,#88898,#88899,#88900,#88901,
#88902,#88903,#88904,#88905,#88906,#88907,#88908,#88909,#88910,#88911,#88912,
#88913,#88914,#88915,#88916,#88917,#88918,#88919,#88920,#88921,#88922,#88923,
#88924,#88925,#88926,#88927,#88928,#88929,#88930,#88931,#88932,#88933,#88934,
#88935,#88936,#88937,#88938,#88939,#88940,#88941,#88942,#88943,#88944,#88945,
#88946,#88947,#88948,#88949,#88950,#88951,#88952,#88953,#88954,#88955,#88956,
#88957,#88958,#88959,#88960,#88961,#88962,#88963,#88964,#88965,#88966,#88967,
#88968,#88969,#88970,#88971,#88972,#88973,#88974,#88975,#88976,#88977,#88978,
#88979,#88980,#88981,#88982,#88983,#88984,#88985,#88986,#88987,#88988,#88989,
#88990,#88991,#88992,#88993,#88994,#88995,#88996,#88997,#88998,#88999,#89000,
#89001,#89002,#89003,#89004,#89005,#89006,#89007,#89008,#89009,#89010,#89011,
#89012,#89013,#89014,#89015,#89016,#89017,#89018,#89019,#89020,#89021,#89022,
#89023,#89024,#89025,#89026,#89027,#89028,#89029,#89030,#89031,#89032,#89033,
#89034,#89035,#89036,#89037,#89038,#89039,#89040,#89041,#89042,#89043,#89044,
#89045,#89046,#89047,#89048,#89049,#89050,#89051,#89052,#89053,#89054,#89055,
#89056,#89057,#89058,#89059,#89060,#89061,#89062,#89063,#89064,#89065,#89066,
#89067,#89068,#89069,#89070,#89071,#89072,#89073,#89074,#89075,#89076,#89077,
#89078,#89079,#89080,#89081,#89082,#89083,#89084,#89085,#89086,#89087,#89088,
#89089,#89090,#89091,#89092,#89093,#89094,#89095,#89096,#89097,#89098,#89099,
#89100,#89101,#89102,#89103,#89104,#89105,#89106,#89107,#89108,#89109,#89110,
#89111,#89112,#89113,#89114,#89115,#89116,#89117,#89118,#89119,#89120,#89121,
#89122,#89123,#89124,#89125,#89126,#89127,#89128,#89129,#89130,#89131,#89132,
#89133,#89134,#89135,#89136,#89137,#89138,#89139,#89140,#89141,#89142,#89143,
#89144,#89145,#89146,#89147,#89148,#89149,#89150,#89151,#89152,#89153,#89154,
#89155,#89156,#89157,#89158,#89159,#89160,#89161,#89162,#89163,#89164,#89165,
#89166,#89167,#89168,#89169,#89170,#89171,#89172,#89173,#89174,#89175,#89176,
#89177,#89178,#89179,#89180,#89181,#89182,#89183,#89184,#89185,#89186,#89187,
#89188,#89189,#89190,#89191,#89192,#89193,#89194,#89195,#89196,#89197,#89198,
#89199,#89200,#89201,#89202,#89203,#89204,#89205,#89206,#89207,#89208,#89209,
#89210,#89211,#89212,#89213,#89214,#89215,#89216,#89217,#89218,#89219,#89220,
#89221,#89222,#89223,#89224,#89225,#89226,#89227,#89228,#89229,#89230,#89231,
#89232,#89233,#89234,#89235,#89236,#89237,#89238,#89239,#89240,#89241,#89242,
#89243,#89244,#89245,#89246,#89247,#89248,#89249,#89250,#89251,#89252,#89253,
#89254,#89255,#89256,#89257,#89258,#89259,#89260,#89261,#89262,#89263,#89264,
#89265,#89266,#89267,#89268,#89269,#89270,#89271,#89272,#89273,#89274,#89275,
#89276,#89277,#89278,#89279,#89280,#89281,#89282,#89283,#89284,#89285,#89286,
#89287,#89288,#89289,#89290,#89291,#89292,#89293,#89294,#89295,#89296,#89297,
#89298,#89299,#89300,#89301,#89302,#89303,#89304,#89305,#89306,#89307,#89308,
#89309,#89310,#89311,#89312,#89313,#89314,#89315,#89316,#89317,#89318,#89319,
#89320,#89321,#89322,#89323,#89324,#89325,#89326,#89327,#89328,#89329,#89330,
#89331,#89332,#89333,#89334,#89335,#89336,#89337,#89338,#89339,#89340,#89341,
#89342,#89343,#89344,#89345,#89346,#89347,#89348,#89349,#89350,#89351,#89352,
#89353,#89354,#89355,#89356,#89357,#89358,#89359,#89360,#89361,#89362,#89363,
#89364,#89365,#89366,#89367,#89368,#89369,#89370,#89371,#89372,#89373,#89374,
#89375,#89376,#89377,#89378,#89379,#89380,#89381,#89382,#89383,#89384,#89385,
#89386,#89387,#89388,#89389,#89390,#89391,#89392,#89393,#89394,#89395,#89396,
#89397,#89398,#89399,#89400,#89401,#89402,#89403,#89404,#89405,#89406,#89407,
#89408,#89409,#89410,#89411,#89412,#89413,#89414,#89415,#89416,#89417,#89418,
#89419,#89420,#89421,#89422,#89423,#89424,#89425,#89426,#89427,#89428,#89429,
#89430,#89431,#89432,#89433,#89434,#89435,#89436,#89437,#89438,#89439,#89440,
#89441,#89442,#89443,#89444,#89445,#89446,#89447,#89448,#89449,#89450,#89451,
#89452,#89453,#89454,#89455,#89456,#89457,#89458,#89459,#89460,#89461,#89462,
#89463,#89464,#89465,#89466,#89467,#89468,#89469,#89470,#89471,#89472,#89473,
#89474,#89475,#89476,#89477,#89478,#89479,#89480,#89481,#89482,#89483,#89484,
#89485,#89486,#89487,#89488,#89489,#89490,#89491,#89492,#89493,#89494,#89495,
#89496,#89497,#89498,#89499,#89500,#89501,#89502,#89503,#89504,#89505,#89506,
#89507,#89508,#89509,#89510,#89511,#89512,#89513,#89514,#89515,#89516,#89517,
#89518,#89519,#89520,#89521,#89522,#89523,#89524,#89525,#89526,#89527,#89528,
#89529,#89530,#89531,#89532,#89533,#89534,#89535,#89536,#89537,#89538,#89539,
#89540,#89541,#89542,#89543,#89544,#89545,#89546,#89547,#89548,#89549,#89550,
#89551,#89552,#89553,#89554,#89555,#89556,#89557,#89558,#89559,#89560,#89561,
#89562,#89563,#89564,#89565,#89566,#89567,#89568,#89569,#89570,#89571,#89572,
#89573,#89574,#89575,#89576,#89577,#89578,#89579,#89580,#89581,#89582,#89583,
#89584,#89585,#89586,#89587,#89588,#89589,#89590,#89591,#89592,#89593,#89594,
#89595,#89596,#89597,#89598,#89599,#89600,#89601,#89602,#89603,#89604,#89605,
#89606,#89607,#89608,#89609,#89610,#89611,#89612,#89613,#89614,#89615,#89616,
#89617,#89618,#89619,#89620,#89621,#89622,#89623,#89624,#89625,#89626,#89627,
#89628,#89629,#89630,#89631,#89632,#89633,#89634,#89635,#89636,#89637,#89638,
#89639,#89640,#89641,#89642,#89643,#89644,#89645,#89646,#89647,#89648,#89649,
#89650,#89651,#89652,#89653,#89654,#89655,#89656,#89657,#89658,#89659,#89660,
#89661,#89662,#89663,#89664,#89665,#89666,#89667,#89668,#89669,#89670,#89671,
#89672,#89673,#89674,#89675,#89676,#89677,#89678,#89679,#89680,#89681,#89682,
#89683,#89684,#89685,#89686,#89687,#89688,#89689,#89690,#89691,#89692,#89693,
#89694,#89695,#89696,#89697,#89698,#89699,#89700,#89701,#89702,#89703,#89704,
#89705,#89706,#89707,#89708,#89709,#89710,#89711,#89712,#89713,#89714,#89715,
#89716,#89717,#89718,#89719,#89720,#89721,#89722,#89723,#89724,#89725,#89726,
#89727,#89728,#89729,#89730,#89731,#89732,#89733,#89734,#89735,#89736,#89737,
#89738,#89739,#89740,#89741,#89742,#89743,#89744,#89745,#89746,#89747,#89748,
#89749,#89750,#89751,#89752,#89753,#89754,#89755,#89756,#89757,#89758,#89759,
#89760,#89761,#89762,#89763,#89764,#89765,#89766,#89767,#89768,#89769,#89770,
#89771,#89772,#89773,#89774,#89775,#89776,#89777,#89778,#89779,#89780,#89781,
#89782,#89783,#89784,#89785,#89786,#89787,#89788,#89789,#89790,#89791,#89792,
#89793,#89794,#89795,#89796,#89797,#89798,#89799,#89800,#89801,#89802,#89803,
#89804,#89805,#89806,#89807,#89808,#89809,#89810,#89811,#89812,#89813,#89814,
#89815,#89816,#89817,#89818,#89819,#89820,#89821,#89822,#89823,#89824,#89825,
#89826,#89827,#89828,#89829,#89830,#89831,#89832,#89833,#89834,#89835,#89836,
#89837,#89838,#89839,#89840,#89841,#89842,#89843,#89844,#89845,#89846,#89847,
#89848,#89849,#89850,#89851,#89852,#89853,#89854,#89855,#89856,#89857,#89858,
#89859,#89860,#89861,#89862,#89863,#89864,#89865,#89866,#89867,#89868,#89869,
#89870,#89871,#89872,#89873,#89874,#89875,#89876,#89877,#89878,#89879,#89880,
#89881,#89882,#89883,#89884,#89885,#89886,#89887,#89888,#89889,#89890,#89891,
#89892,#89893,#89894,#89895,#89896,#89897,#89898,#89899,#89900,#89901,#89902,
#89903,#89904,#89905,#89906,#89907,#89908,#89909,#89910,#89911,#89912,#89913,
#89914,#89915,#89916,#89917,#89918,#89919,#89920,#89921,#89922,#89923,#89924,
#89925,#89926,#89927,#89928,#89929,#89930,#89931,#89932,#89933,#89934,#89935,
#89936,#89937,#89938,#89939,#89940,#89941,#89942,#89943,#89944,#89945,#89946,
#89947,#89948,#89949,#89950,#89951,#89952,#89953,#89954,#89955,#89956,#89957,
#89958,#89959,#89960,#89961,#89962,#89963,#89964,#89965,#89966,#89967,#89968,
#89969,#89970,#89971,#89972,#89973,#89974,#89975,#89976,#89977,#89978,#89979,
#89980,#89981,#89982,#89983,#89984,#89985,#89986,#89987,#89988,#89989,#89990,
#89991,#89992,#89993,#89994,#89995,#89996,#89997,#89998,#89999,#90000,#90001,
#90002,#90003,#90004,#90005,#90006,#90007,#90008,#90009,#90010,#90011,#90012,
#90013,#90014,#90015,#90016,#90017,#90018,#90019,#90020,#90021,#90022,#90023,
#90024,#90025,#90026,#90027,#90028,#90029,#90030,#90031,#90032,#90033,#90034,
#90035,#90036,#90037,#90038,#90039,#90040,#90041,#90042,#90043,#90044,#90045,
#90046,#90047,#90048,#90049,#90050,#90051,#90052,#90053,#90054,#90055,#90056,
#90057,#90058,#90059,#90060,#90061,#90062,#90063,#90064,#90065,#90066,#90067,
#90068,#90069,#90070,#90071,#90072,#90073,#90074,#90075,#90076,#90077,#90078,
#90079,#90080,#90081,#90082,#90083,#90084,#90085,#90086,#90087,#90088,#90089,
#90090,#90091,#90092,#90093,#90094,#90095,#90096,#90097,#90098,#90099,#90100,
#90101,#90102,#90103,#90104,#90105,#90106,#90107,#90108,#90109,#90110,#90111,
#90112,#90113,#90114,#90115,#90116,#90117,#90118,#90119,#90120,#90121,#90122,
#90123,#90124,#90125,#90126,#90127,#90128,#90129,#90130,#90131,#90132,#90133,
#90134,#90135,#90136,#90137,#90138,#90139,#90140,#90141,#90142,#90143,#90144,
#90145,#90146,#90147,#90148,#90149,#90150,#90151,#90152,#90153,#90154,#90155,
#90156,#90157,#90158,#90159,#90160,#90161,#90162,#90163,#90164,#90165,#90166,
#90167,#90168,#90169,#90170,#90171,#90172,#90173,#90174,#90175,#90176,#90177,
#90178,#90179,#90180,#90181,#90182,#90183,#90184,#90185,#90186,#90187,#90188,
#90189,#90190,#90191,#90192,#90193,#90194,#90195,#90196,#90197,#90198,#90199,
#90200,#90201,#90202,#90203,#90204,#90205,#90206,#90207,#90208,#90209,#90210,
#90211,#90212,#90213,#90214,#90215,#90216,#90217,#90218,#90219,#90220,#90221,
#90222,#90223,#90224,#90225,#90226,#90227,#90228,#90229,#90230,#90231,#90232,
#90233,#90234,#90235,#90236,#90237,#90238,#90239,#90240,#90241,#90242,#90243,
#90244,#90245,#90246,#90247,#90248,#90249,#90250,#90251,#90252,#90253,#90254,
#90255,#90256,#90257,#90258,#90259,#90260,#90261,#90262,#90263,#90264,#90265,
#90266,#90267,#90268,#90269,#90270,#90271,#90272,#90273,#90274,#90275,#90276,
#90277,#90278,#90279,#90280,#90281,#90282,#90283,#90284,#90285,#90286,#90287,
#90288,#90289,#90290,#90291,#90292,#90293,#90294,#90295,#90296,#90297,#90298,
#90299,#90300,#90301,#90302,#90303,#90304,#90305,#90306,#90307,#90308,#90309,
#90310,#90311,#90312,#90313,#90314,#90315,#90316,#90317,#90318,#90319,#90320,
#90321,#90322,#90323,#90324,#90325,#90326,#90327,#90328,#90329,#90330,#90331,
#90332,#90333,#90334,#90335,#90336,#90337,#90338,#90339,#90340,#90341,#90342,
#90343,#90344,#90345,#90346,#90347,#90348,#90349,#90350,#90351,#90352,#90353,
#90354,#90355,#90356,#90357,#90358,#90359,#90360,#90361,#90362,#90363,#90364,
#90365,#90366,#90367,#90368,#90369,#90370,#90371,#90372,#90373,#90374,#90375,
#90376,#90377,#90378,#90379,#90380,#90381,#90382,#90383,#90384,#90385,#90386,
#90387,#90388,#90389,#90390,#90391,#90392,#90393,#90394,#90395,#90396,#90397,
#90398,#90399,#90400,#90401,#90402,#90403,#90404,#90405,#90406,#90407,#90408,
#90409,#90410,#90411,#90412,#90413,#90414,#90415,#90416,#90417,#90418,#90419,
#90420,#90421,#90422,#90423,#90424,#90425,#90426,#90427,#90428,#90429,#90430,
#90431,#90432,#90433,#90434,#90435,#90436,#90437,#90438,#90439,#90440,#90441,
#90442,#90443,#90444,#90445,#90446,#90447,#90448,#90449,#90450,#90451,#90452,
#90453,#90454,#90455,#90456,#90457,#90458,#90459,#90460,#90461,#90462,#90463,
#90464,#90465,#90466,#90467,#90468,#90469,#90470,#90471,#90472,#90473,#90474,
#90475,#90476,#90477,#90478,#90479,#90480,#90481,#90482,#90483,#90484,#90485,
#90486,#90487,#90488,#90489,#90490,#90491,#90492,#90493,#90494,#90495,#90496,
#90497,#90498,#90499,#90500,#90501,#90502,#90503,#90504,#90505,#90506,#90507,
#90508,#90509,#90510,#90511,#90512,#90513,#90514,#90515,#90516,#90517,#90518,
#90519,#90520,#90521,#90522,#90523,#90524,#90525,#90526,#90527,#90528,#90529,
#90530,#90531,#90532,#90533,#90534,#90535,#90536,#90537,#90538,#90539,#90540,
#90541,#90542,#90543,#90544,#90545,#90546,#90547,#90548,#90549,#90550,#90551,
#90552,#90553,#90554,#90555,#90556,#90557,#90558,#90559,#90560,#90561,#90562,
#90563,#90564,#90565,#90566,#90567,#90568,#90569,#90570,#90571,#90572,#90573,
#90574,#90575,#90576,#90577,#90578,#90579,#90580,#90581,#90582,#90583,#90584,
#90585,#90586,#90587,#90588,#90589,#90590,#90591,#90592,#90593,#90594,#90595,
#90596,#90597,#90598,#90599,#90600,#90601,#90602,#90603,#90604,#90605,#90606,
#90607,#90608,#90609,#90610,#90611,#90612,#90613,#90614,#90615,#90616,#90617,
#90618,#90619,#90620,#90621,#90622,#90623,#90624,#90625,#90626,#90627,#90628,
#90629,#90630,#90631,#90632,#90633,#90634,#90635,#90636,#90637,#90638,#90639,
#90640,#90641,#90642,#90643,#90644,#90645,#90646,#90647,#90648,#90649,#90650,
#90651,#90652,#90653,#90654,#90655,#90656,#90657,#90658,#90659,#90660,#90661,
#90662,#90663,#90664,#90665,#90666,#90667,#90668,#90669,#90670,#90671,#90672,
#90673,#90674,#90675,#90676,#90677,#90678,#90679,#90680,#90681,#90682,#90683,
#90684,#90685,#90686,#90687,#90688,#90689,#90690,#90691,#90692,#90693,#90694,
#90695,#90696,#90697,#90698,#90699,#90700,#90701,#90702,#90703,#90704,#90705,
#90706,#90707,#90708,#90709,#90710,#90711,#90712,#90713,#90714,#90715,#90716,
#90717,#90718,#90719,#90720,#90721,#90722,#90723,#90724,#90725,#90726,#90727,
#90728,#90729,#90730,#90731,#90732,#90733,#90734,#90735,#90736,#90737,#90738,
#90739,#90740,#90741,#90742,#90743,#90744,#90745,#90746,#90747,#90748,#90749,
#90750,#90751,#90752,#90753,#90754,#90755,#90756,#90757,#90758,#90759,#90760,
#90761,#90762,#90763,#90764,#90765,#90766,#90767,#90768,#90769,#90770,#90771,
#90772,#90773,#90774,#90775,#90776,#90777,#90778,#90779,#90780,#90781,#90782,
#90783,#90784,#90785,#90786,#90787,#90788,#90789,#90790,#90791,#90792,#90793,
#90794,#90795,#90796,#90797,#90798,#90799,#90800,#90801,#90802,#90803,#90804,
#90805,#90806,#90807,#90808,#90809,#90810,#90811,#90812,#90813,#90814,#90815,
#90816,#90817,#90818,#90819,#90820,#90821,#90822,#90823,#90824,#90825,#90826,
#90827,#90828,#90829,#90830,#90831,#90832,#90833,#90834,#90835,#90836,#90837,
#90838,#90839,#90840,#90841,#90842,#90843,#90844,#90845,#90846,#90847,#90848,
#90849,#90850,#90851,#90852,#90853,#90854,#90855,#90856,#90857,#90858,#90859,
#90860,#90861,#90862,#90863,#90864,#90865,#90866,#90867,#90868,#90869,#90870,
#90871,#90872,#90873,#90874,#90875,#90876,#90877,#90878,#90879,#90880,#90881,
#90882,#90883,#90884,#90885,#90886,#90887,#90888,#90889,#90890,#90891,#90892,
#90893,#90894,#90895,#90896,#90897,#90898,#90899,#90900,#90901,#90902,#90903,
#90904,#90905,#90906,#90907,#90908,#90909,#90910,#90911,#90912,#90913,#90914,
#90915,#90916,#90917,#90918,#90919,#90920,#90921,#90922,#90923,#90924,#90925,
#90926,#90927,#90928,#90929,#90930,#90931,#90932,#90933,#90934,#90935,#90936,
#90937,#90938,#90939,#90940,#90941,#90942,#90943,#90944,#90945,#90946,#90947,
#90948,#90949,#90950,#90951,#90952,#90953,#90954,#90955,#90956,#90957,#90958,
#90959,#90960,#90961,#90962,#90963,#90964,#90965,#90966,#90967,#90968,#90969,
#90970,#90971,#90972,#90973,#90974,#90975,#90976,#90977,#90978,#90979,#90980,
#90981,#90982,#90983,#90984,#90985,#90986,#90987,#90988,#90989,#90990,#90991,
#90992,#90993,#90994,#90995,#90996,#90997,#90998,#90999,#91000,#91001,#91002,
#91003,#91004,#91005,#91006,#91007,#91008,#91009,#91010,#91011,#91012,#91013,
#91014,#91015,#91016,#91017,#91018,#91019,#91020,#91021,#91022,#91023,#91024,
#91025,#91026,#91027,#91028,#91029,#91030,#91031,#91032,#91033,#91034,#91035,
#91036,#91037,#91038,#91039,#91040,#91041,#91042,#91043,#91044,#91045,#91046,
#91047,#91048,#91049,#91050,#91051,#91052,#91053,#91054,#91055,#91056,#91057,
#91058,#91059,#91060,#91061,#91062,#91063,#91064,#91065,#91066,#91067,#91068,
#91069,#91070,#91071,#91072,#91073,#91074,#91075,#91076,#91077,#91078,#91079,
#91080,#91081,#91082,#91083,#91084,#91085,#91086,#91087,#91088,#91089,#91090,
#91091,#91092,#91093,#91094,#91095,#91096,#91097,#91098,#91099,#91100,#91101,
#91102,#91103,#91104,#91105,#91106,#91107,#91108,#91109,#91110,#91111,#91112,
#91113,#91114,#91115,#91116,#91117,#91118,#91119,#91120,#91121,#91122,#91123,
#91124,#91125,#91126,#91127,#91128,#91129,#91130,#91131,#91132,#91133,#91134,
#91135,#91136,#91137,#91138,#91139,#91140,#91141,#91142,#91143,#91144,#91145,
#91146,#91147,#91148,#91149,#91150,#91151,#91152,#91153,#91154,#91155,#91156,
#91157,#91158,#91159,#91160,#91161,#91162,#91163,#91164,#91165,#91166,#91167,
#91168,#91169,#91170,#91171,#91172,#91173,#91174,#91175,#91176,#91177,#91178,
#91179,#91180,#91181,#91182,#91183,#91184,#91185,#91186,#91187,#91188,#91189,
#91190,#91191,#91192,#91193,#91194,#91195,#91196,#91197,#91198,#91199,#91200,
#91201,#91202,#91203,#91204,#91205,#91206,#91207,#91208,#91209,#91210,#91211,
#91212,#91213,#91214,#91215,#91216,#91217,#91218,#91219,#91220,#91221,#91222,
#91223,#91224,#91225,#91226,#91227,#91228,#91229,#91230,#91231,#91232,#91233,
#91234,#91235,#91236,#91237,#91238,#91239,#91240,#91241,#91242,#91243,#91244,
#91245,#91246,#91247,#91248,#91249,#91250,#91251,#91252,#91253,#91254,#91255,
#91256,#91257,#91258,#91259,#91260,#91261,#91262,#91263,#91264,#91265,#91266,
#91267,#91268,#91269,#91270,#91271,#91272,#91273,#91274,#91275,#91276,#91277,
#91278,#91279,#91280,#91281,#91282,#91283,#91284,#91285,#91286,#91287,#91288,
#91289,#91290,#91291,#91292,#91293,#91294,#91295,#91296,#91297,#91298,#91299,
#91300,#91301,#91302,#91303,#91304,#91305,#91306,#91307,#91308,#91309,#91310,
#91311,#91312,#91313,#91314,#91315,#91316,#91317,#91318,#91319,#91320,#91321,
#91322,#91323,#91324,#91325,#91326,#91327,#91328,#91329,#91330,#91331,#91332,
#91333,#91334,#91335,#91336,#91337,#91338,#91339,#91340,#91341,#91342,#91343,
#91344,#91345,#91346,#91347,#91348,#91349,#91350,#91351,#91352,#91353,#91354,
#91355,#91356,#91357,#91358,#91359,#91360,#91361,#91362,#91363,#91364,#91365,
#91366,#91367,#91368,#91369,#91370,#91371,#91372,#91373,#91374,#91375,#91376,
#91377,#91378,#91379,#91380,#91381,#91382,#91383,#91384,#91385,#91386,#91387,
#91388,#91389,#91390,#91391,#91392,#91393,#91394,#91395,#91396,#91397,#91398,
#91399,#91400,#91401,#91402,#91403,#91404,#91405,#91406,#91407,#91408,#91409,
#91410,#91411,#91412,#91413,#91414,#91415,#91416,#91417,#91418,#91419,#91420,
#91421,#91422,#91423,#91424,#91425,#91426,#91427,#91428,#91429,#91430,#91431,
#91432,#91433,#91434,#91435,#91436,#91437,#91438,#91439,#91440,#91441,#91442,
#91443,#91444,#91445,#91446,#91447,#91448,#91449,#91450,#91451,#91452,#91453,
#91454,#91455,#91456,#91457,#91458,#91459,#91460,#91461,#91462,#91463,#91464,
#91465,#91466,#91467,#91468,#91469,#91470,#91471,#91472,#91473,#91474,#91475,
#91476,#91477,#91478,#91479,#91480,#91481,#91482,#91483,#91484,#91485,#91486,
#91487,#91488,#91489,#91490,#91491,#91492,#91493,#91494,#91495,#91496,#91497,
#91498,#91499,#91500,#91501,#91502,#91503,#91504,#91505,#91506,#91507,#91508,
#91509,#91510,#91511,#91512,#91513,#91514,#91515,#91516,#91517,#91518,#91519,
#91520,#91521,#91522,#91523,#91524,#91525,#91526,#91527,#91528,#91529,#91530,
#91531,#91532,#91533,#91534,#91535,#91536,#91537,#91538,#91539,#91540,#91541,
#91542,#91543,#91544,#91545,#91546,#91547,#91548,#91549,#91550,#91551,#91552,
#91553,#91554,#91555,#91556,#91557,#91558,#91559,#91560,#91561,#91562,#91563,
#91564,#91565,#91566,#91567,#91568,#91569,#91570,#91571,#91572,#91573,#91574,
#91575,#91576,#91577,#91578,#91579,#91580,#91581,#91582,#91583,#91584,#91585,
#91586,#91587,#91588,#91589,#91590,#91591,#91592,#91593,#91594,#91595,#91596,
#91597,#91598,#91599,#91600,#91601,#91602,#91603,#91604,#91605,#91606,#91607,
#91608,#91609,#91610,#91611,#91612,#91613,#91614,#91615,#91616,#91617,#91618,
#91619,#91620,#91621,#91622,#91623,#91624,#91625,#91626,#91627,#91628,#91629,
#91630,#91631,#91632,#91633,#91634,#91635,#91636,#91637,#91638,#91639,#91640,
#91641,#91642,#91643,#91644,#91645,#91646,#91647,#91648,#91649,#91650,#91651,
#91652,#91653,#91654,#91655,#91656,#91657,#91658,#91659,#91660,#91661,#91662,
#91663,#91664,#91665,#91666,#91667,#91668,#91669,#91670,#91671,#91672,#91673,
#91674,#91675,#91676,#91677,#91678,#91679,#91680,#91681,#91682,#91683,#91684,
#91685,#91686,#91687,#91688,#91689,#91690,#91691,#91692,#91693,#91694,#91695,
#91696,#91697,#91698,#91699,#91700,#91701,#91702,#91703,#91704,#91705,#91706,
#91707,#91708,#91709,#91710,#91711,#91712,#91713,#91714,#91715,#91716,#91717,
#91718,#91719,#91720,#91721,#91722,#91723,#91724,#91725,#91726,#91727,#91728,
#91729,#91730,#91731,#91732,#91733,#91734,#91735,#91736,#91737,#91738,#91739,
#91740,#91741,#91742,#91743,#91744,#91745,#91746,#91747,#91748,#91749,#91750,
#91751,#91752,#91753,#91754,#91755,#91756,#91757,#91758,#91759,#91760,#91761,
#91762,#91763,#91764,#91765,#91766,#91767,#91768,#91769,#91770,#91771,#91772,
#91773,#91774,#91775,#91776,#91777,#91778,#91779,#91780,#91781,#91782,#91783,
#91784,#91785,#91786,#91787,#91788,#91789,#91790,#91791,#91792,#91793,#91794,
#91795,#91796,#91797,#91798,#91799,#91800,#91801,#91802,#91803,#91804,#91805,
#91806,#91807,#91808,#91809,#91810,#91811,#91812,#91813,#91814,#91815,#91816,
#91817,#91818,#91819,#91820,#91821,#91822,#91823,#91824,#91825,#91826,#91827,
#91828,#91829,#91830,#91831,#91832,#91833,#91834,#91835,#91836,#91837,#91838,
#91839,#91840,#91841,#91842,#91843,#91844,#91845,#91846,#91847,#91848,#91849,
#91850,#91851,#91852,#91853,#91854,#91855,#91856,#91857,#91858,#91859,#91860,
#91861,#91862,#91863,#91864,#91865,#91866,#91867,#91868,#91869,#91870,#91871,
#91872,#91873,#91874,#91875,#91876,#91877,#91878,#91879,#91880,#91881,#91882,
#91883,#91884,#91885,#91886,#91887,#91888,#91889,#91890,#91891,#91892,#91893,
#91894,#91895,#91896,#91897,#91898,#91899,#91900,#91901,#91902,#91903,#91904,
#91905,#91906,#91907,#91908,#91909,#91910,#91911,#91912,#91913,#91914,#91915,
#91916,#91917,#91918,#91919,#91920,#91921,#91922,#91923,#91924,#91925,#91926,
#91927,#91928,#91929,#91930,#91931,#91932,#91933,#91934,#91935,#91936,#91937,
#91938,#91939,#91940,#91941,#91942,#91943,#91944,#91945,#91946,#91947,#91948,
#91949,#91950,#91951,#91952,#91953,#91954,#91955,#91956,#91957,#91958,#91959,
#91960,#91961,#91962,#91963,#91964,#91965,#91966,#91967,#91968,#91969,#91970,
#91971,#91972,#91973,#91974,#91975,#91976,#91977,#91978,#91979,#91980,#91981,
#91982,#91983,#91984,#91985,#91986,#91987,#91988,#91989,#91990,#91991,#91992,
#91993,#91994,#91995,#91996,#91997,#91998,#91999,#92000,#92001,#92002,#92003,
#92004,#92005,#92006,#92007,#92008,#92009,#92010,#92011,#92012,#92013,#92014,
#92015,#92016,#92017,#92018,#92019,#92020,#92021,#92022,#92023,#92024,#92025,
#92026,#92027,#92028,#92029,#92030,#92031,#92032,#92033,#92034,#92035,#92036,
#92037,#92038,#92039,#92040,#92041,#92042,#92043,#92044,#92045,#92046,#92047,
#92048,#92049,#92050,#92051,#92052,#92053,#92054,#92055,#92056,#92057,#92058,
#92059,#92060,#92061,#92062,#92063,#92064,#92065,#92066,#92067,#92068,#92069,
#92070,#92071,#92072,#92073,#92074,#92075,#92076,#92077,#92078,#92079,#92080,
#92081,#92082,#92083,#92084,#92085,#92086,#92087,#92088,#92089,#92090,#92091,
#92092,#92093,#92094,#92095,#92096,#92097,#92098,#92099,#92100,#92101,#92102,
#92103,#92104,#92105,#92106,#92107,#92108,#92109,#92110,#92111,#92112,#92113,
#92114,#92115,#92116,#92117,#92118,#92119,#92120,#92121,#92122,#92123,#92124,
#92125,#92126,#92127,#92128,#92129,#92130,#92131,#92132,#92133,#92134,#92135,
#92136,#92137,#92138,#92139,#92140,#92141,#92142,#92143,#92144,#92145,#92146,
#92147,#92148,#92149,#92150,#92151,#92152,#92153,#92154,#92155,#92156,#92157,
#92158,#92159,#92160,#92161),(#92162,#92163,#92164,#92165,#92166,#92167,
#92168,#92169,#92170,#92171,#92172,#92173,#92174,#92175,#92176,#92177,#92178,
#92179,#92180,#92181,#92182,#92183,#92184,#92185,#92186,#92187,#92188,#92189,
#92190,#92191,#92192,#92193,#92194,#92195,#92196,#92197,#92198,#92199,#92200,
#92201,#92202,#92203,#92204,#92205,#92206,#92207,#92208,#92209,#92210,#92211,
#92212,#92213,#92214,#92215,#92216,#92217,#92218,#92219,#92220,#92221,#92222,
#92223,#92224,#92225,#92226,#92227,#92228,#92229,#92230,#92231,#92232,#92233,
#92234,#92235,#92236,#92237,#92238,#92239,#92240,#92241,#92242,#92243,#92244,
#92245,#92246,#92247,#92248,#92249,#92250,#92251,#92252,#92253,#92254,#92255,
#92256,#92257,#92258,#92259,#92260,#92261,#92262,#92263,#92264,#92265,#92266,
#92267,#92268,#92269,#92270,#92271,#92272,#92273,#92274,#92275,#92276,#92277,
#92278,#92279,#92280,#92281,#92282,#92283,#92284,#92285,#92286,#92287,#92288,
#92289,#92290,#92291,#92292,#92293,#92294,#92295,#92296,#92297,#92298,#92299,
#92300,#92301,#92302,#92303,#92304,#92305,#92306,#92307,#92308,#92309,#92310,
#92311,#92312,#92313,#92314,#92315,#92316,#92317,#92318,#92319,#92320,#92321,
#92322,#92323,#92324,#92325,#92326,#92327,#92328,#92329,#92330,#92331,#92332,
#92333,#92334,#92335,#92336,#92337,#92338,#92339,#92340,#92341,#92342,#92343,
#92344,#92345,#92346,#92347,#92348,#92349,#92350,#92351,#92352,#92353,#92354,
#92355,#92356,#92357,#92358,#92359,#92360,#92361,#92362,#92363,#92364,#92365,
#92366,#92367,#92368,#92369,#92370,#92371,#92372,#92373,#92374,#92375,#92376,
#92377,#92378,#92379,#92380,#92381,#92382,#92383,#92384,#92385,#92386,#92387,
#92388,#92389,#92390,#92391,#92392,#92393,#92394,#92395,#92396,#92397,#92398,
#92399,#92400,#92401,#92402,#92403,#92404,#92405,#92406,#92407,#92408,#92409,
#92410,#92411,#92412,#92413,#92414,#92415,#92416,#92417,#92418,#92419,#92420,
#92421,#92422,#92423,#92424,#92425,#92426,#92427,#92428,#92429,#92430,#92431,
#92432,#92433,#92434,#92435,#92436,#92437,#92438,#92439,#92440,#92441,#92442,
#92443,#92444,#92445,#92446,#92447,#92448,#92449,#92450,#92451,#92452,#92453,
#92454,#92455,#92456,#92457,#92458,#92459,#92460,#92461,#92462,#92463,#92464,
#92465,#92466,#92467,#92468,#92469,#92470,#92471,#92472,#92473,#92474,#92475,
#92476,#92477,#92478,#92479,#92480,#92481,#92482,#92483,#92484,#92485,#92486,
#92487,#92488,#92489,#92490,#92491,#92492,#92493,#92494,#92495,#92496,#92497,
#92498,#92499,#92500,#92501,#92502,#92503,#92504,#92505,#92506,#92507,#92508,
#92509,#92510,#92511,#92512,#92513,#92514,#92515,#92516,#92517,#92518,#92519,
#92520,#92521,#92522,#92523,#92524,#92525,#92526,#92527,#92528,#92529,#92530,
#92531,#92532,#92533,#92534,#92535,#92536,#92537,#92538,#92539,#92540,#92541,
#92542,#92543,#92544,#92545,#92546,#92547,#92548,#92549,#92550,#92551,#92552,
#92553,#92554,#92555,#92556,#92557,#92558,#92559,#92560,#92561,#92562,#92563,
#92564,#92565,#92566,#92567,#92568,#92569,#92570,#92571,#92572,#92573,#92574,
#92575,#92576,#92577,#92578,#92579,#92580,#92581,#92582,#92583,#92584,#92585,
#92586,#92587,#92588,#92589,#92590,#92591,#92592,#92593,#92594,#92595,#92596,
#92597,#92598,#92599,#92600,#92601,#92602,#92603,#92604,#92605,#92606,#92607,
#92608,#92609,#92610,#92611,#92612,#92613,#92614,#92615,#92616,#92617,#92618,
#92619,#92620,#92621,#92622,#92623,#92624,#92625,#92626,#92627,#92628,#92629,
#92630,#92631,#92632,#92633,#92634,#92635,#92636,#92637,#92638,#92639,#92640,
#92641,#92642,#92643,#92644,#92645,#92646,#92647,#92648,#92649,#92650,#92651,
#92652,#92653,#92654,#92655,#92656,#92657,#92658,#92659,#92660,#92661,#92662,
#92663,#92664,#92665,#92666,#92667,#92668,#92669,#92670,#92671,#92672,#92673,
#92674,#92675,#92676,#92677,#92678,#92679,#92680,#92681,#92682,#92683,#92684,
#92685,#92686,#92687,#92688,#92689,#92690,#92691,#92692,#92693,#92694,#92695,
#92696,#92697,#92698,#92699,#92700,#92701,#92702,#92703,#92704,#92705,#92706,
#92707,#92708,#92709,#92710,#92711,#92712,#92713,#92714,#92715,#92716,#92717,
#92718,#92719,#92720,#92721,#92722,#92723,#92724,#92725,#92726,#92727,#92728,
#92729,#92730,#92731,#92732,#92733,#92734,#92735,#92736,#92737,#92738,#92739,
#92740,#92741,#92742,#92743,#92744,#92745,#92746,#92747,#92748,#92749,#92750,
#92751,#92752,#92753,#92754,#92755,#92756,#92757,#92758,#92759,#92760,#92761,
#92762,#92763,#92764,#92765,#92766,#92767,#92768,#92769,#92770,#92771,#92772,
#92773,#92774,#92775,#92776,#92777,#92778,#92779,#92780,#92781,#92782,#92783,
#92784,#92785,#92786,#92787,#92788,#92789,#92790,#92791,#92792,#92793,#92794,
#92795,#92796,#92797,#92798,#92799,#92800,#92801,#92802,#92803,#92804,#92805,
#92806,#92807,#92808,#92809,#92810,#92811,#92812,#92813,#92814,#92815,#92816,
#92817,#92818,#92819,#92820,#92821,#92822,#92823,#92824,#92825,#92826,#92827,
#92828,#92829,#92830,#92831,#92832,#92833,#92834,#92835,#92836,#92837,#92838,
#92839,#92840,#92841,#92842,#92843,#92844,#92845,#92846,#92847,#92848,#92849,
#92850,#92851,#92852,#92853,#92854,#92855,#92856,#92857,#92858,#92859,#92860,
#92861,#92862,#92863,#92864,#92865,#92866,#92867,#92868,#92869,#92870,#92871,
#92872,#92873,#92874,#92875,#92876,#92877,#92878,#92879,#92880,#92881,#92882,
#92883,#92884,#92885,#92886,#92887,#92888,#92889,#92890,#92891,#92892,#92893,
#92894,#92895,#92896,#92897,#92898,#92899,#92900,#92901,#92902,#92903,#92904,
#92905,#92906,#92907,#92908,#92909,#92910,#92911,#92912,#92913,#92914,#92915,
#92916,#92917,#92918,#92919,#92920,#92921,#92922,#92923,#92924,#92925,#92926,
#92927,#92928,#92929,#92930,#92931,#92932,#92933,#92934,#92935,#92936,#92937,
#92938,#92939,#92940,#92941,#92942,#92943,#92944,#92945,#92946,#92947,#92948,
#92949,#92950,#92951,#92952,#92953,#92954,#92955,#92956,#92957,#92958,#92959,
#92960,#92961,#92962,#92963,#92964,#92965,#92966,#92967,#92968,#92969,#92970,
#92971,#92972,#92973,#92974,#92975,#92976,#92977,#92978,#92979,#92980,#92981,
#92982,#92983,#92984,#92985,#92986,#92987,#92988,#92989,#92990,#92991,#92992,
#92993,#92994,#92995,#92996,#92997,#92998,#92999,#93000,#93001,#93002,#93003,
#93004,#93005,#93006,#93007,#93008,#93009,#93010,#93011,#93012,#93013,#93014,
#93015,#93016,#93017,#93018,#93019,#93020,#93021,#93022,#93023,#93024,#93025,
#93026,#93027,#93028,#93029,#93030,#93031,#93032,#93033,#93034,#93035,#93036,
#93037,#93038,#93039,#93040,#93041,#93042,#93043,#93044,#93045,#93046,#93047,
#93048,#93049,#93050,#93051,#93052,#93053,#93054,#93055,#93056,#93057,#93058,
#93059,#93060,#93061,#93062,#93063,#93064,#93065,#93066,#93067,#93068,#93069,
#93070,#93071,#93072,#93073,#93074,#93075,#93076,#93077,#93078,#93079,#93080,
#93081,#93082,#93083,#93084,#93085,#93086,#93087,#93088,#93089,#93090,#93091,
#93092,#93093,#93094,#93095,#93096,#93097,#93098,#93099,#93100,#93101,#93102,
#93103,#93104,#93105,#93106,#93107,#93108,#93109,#93110,#93111,#93112,#93113,
#93114,#93115,#93116,#93117,#93118,#93119,#93120,#93121,#93122,#93123,#93124,
#93125,#93126,#93127,#93128,#93129,#93130,#93131,#93132,#93133,#93134,#93135,
#93136,#93137,#93138,#93139,#93140,#93141,#93142,#93143,#93144,#93145,#93146,
#93147,#93148,#93149,#93150,#93151,#93152,#93153,#93154,#93155,#93156,#93157,
#93158,#93159,#93160,#93161,#93162,#93163,#93164,#93165,#93166,#93167,#93168,
#93169,#93170,#93171,#93172,#93173,#93174,#93175,#93176,#93177,#93178,#93179,
#93180,#93181,#93182,#93183,#93184,#93185,#93186,#93187,#93188,#93189,#93190,
#93191,#93192,#93193,#93194,#93195,#93196,#93197,#93198,#93199,#93200,#93201,
#93202,#93203,#93204,#93205,#93206,#93207,#93208,#93209,#93210,#93211,#93212,
#93213,#93214,#93215,#93216,#93217,#93218,#93219,#93220,#93221,#93222,#93223,
#93224,#93225,#93226,#93227,#93228,#93229,#93230,#93231,#93232,#93233,#93234,
#93235,#93236,#93237,#93238,#93239,#93240,#93241,#93242,#93243,#93244,#93245,
#93246,#93247,#93248,#93249,#93250,#93251,#93252,#93253,#93254,#93255,#93256,
#93257,#93258,#93259,#93260,#93261,#93262,#93263,#93264,#93265,#93266,#93267,
#93268,#93269,#93270,#93271,#93272,#93273,#93274,#93275,#93276,#93277,#93278,
#93279,#93280,#93281,#93282,#93283,#93284,#93285,#93286,#93287,#93288,#93289,
#93290,#93291,#93292,#93293,#93294,#93295,#93296,#93297,#93298,#93299,#93300,
#93301,#93302,#93303,#93304,#93305,#93306,#93307,#93308,#93309,#93310,#93311,
#93312,#93313,#93314,#93315,#93316,#93317,#93318,#93319,#93320,#93321,#93322,
#93323,#93324,#93325,#93326,#93327,#93328,#93329,#93330,#93331,#93332,#93333,
#93334,#93335,#93336,#93337,#93338,#93339,#93340,#93341,#93342,#93343,#93344,
#93345,#93346,#93347,#93348,#93349,#93350,#93351,#93352,#93353,#93354,#93355,
#93356,#93357,#93358,#93359,#93360,#93361,#93362,#93363,#93364,#93365,#93366,
#93367,#93368,#93369,#93370,#93371,#93372,#93373,#93374,#93375,#93376,#93377,
#93378,#93379,#93380,#93381,#93382,#93383,#93384,#93385,#93386,#93387,#93388,
#93389,#93390,#93391,#93392,#93393,#93394,#93395,#93396,#93397,#93398,#93399,
#93400,#93401,#93402,#93403,#93404,#93405,#93406,#93407,#93408,#93409,#93410,
#93411,#93412,#93413,#93414,#93415,#93416,#93417,#93418,#93419,#93420,#93421,
#93422,#93423,#93424,#93425,#93426,#93427,#93428,#93429,#93430,#93431,#93432,
#93433,#93434,#93435,#93436,#93437,#93438,#93439,#93440,#93441,#93442,#93443,
#93444,#93445,#93446,#93447,#93448,#93449,#93450,#93451,#93452,#93453,#93454,
#93455,#93456,#93457,#93458,#93459,#93460,#93461,#93462,#93463,#93464,#93465,
#93466,#93467,#93468,#93469,#93470,#93471,#93472,#93473,#93474,#93475,#93476,
#93477,#93478,#93479,#93480,#93481,#93482,#93483,#93484,#93485,#93486,#93487,
#93488,#93489,#93490,#93491,#93492,#93493,#93494,#93495,#93496,#93497,#93498,
#93499,#93500,#93501,#93502,#93503,#93504,#93505,#93506,#93507,#93508,#93509,
#93510,#93511,#93512,#93513,#93514,#93515,#93516,#93517,#93518,#93519,#93520,
#93521,#93522,#93523,#93524,#93525,#93526,#93527,#93528,#93529,#93530,#93531,
#93532,#93533,#93534,#93535,#93536,#93537,#93538,#93539,#93540,#93541,#93542,
#93543,#93544,#93545,#93546,#93547,#93548,#93549,#93550,#93551,#93552,#93553,
#93554,#93555,#93556,#93557,#93558,#93559,#93560,#93561,#93562,#93563,#93564,
#93565,#93566,#93567,#93568,#93569,#93570,#93571,#93572,#93573,#93574,#93575,
#93576,#93577,#93578,#93579,#93580,#93581,#93582,#93583,#93584,#93585,#93586,
#93587,#93588,#93589,#93590,#93591,#93592,#93593,#93594,#93595,#93596,#93597,
#93598,#93599,#93600,#93601,#93602,#93603,#93604,#93605,#93606,#93607,#93608,
#93609,#93610,#93611,#93612,#93613,#93614,#93615,#93616,#93617,#93618,#93619,
#93620,#93621,#93622,#93623,#93624,#93625,#93626,#93627,#93628,#93629,#93630,
#93631,#93632,#93633,#93634,#93635,#93636,#93637,#93638,#93639,#93640,#93641,
#93642,#93643,#93644,#93645,#93646,#93647,#93648,#93649,#93650,#93651,#93652,
#93653,#93654,#93655,#93656,#93657,#93658,#93659,#93660,#93661,#93662,#93663,
#93664,#93665,#93666,#93667,#93668,#93669,#93670,#93671,#93672,#93673,#93674,
#93675,#93676,#93677,#93678,#93679,#93680,#93681,#93682,#93683,#93684,#93685,
#93686,#93687,#93688,#93689,#93690,#93691,#93692,#93693,#93694,#93695,#93696,
#93697,#93698,#93699,#93700,#93701,#93702,#93703,#93704,#93705,#93706,#93707,
#93708,#93709,#93710,#93711,#93712,#93713,#93714,#93715,#93716,#93717,#93718,
#93719,#93720,#93721,#93722,#93723,#93724,#93725,#93726,#93727,#93728,#93729,
#93730,#93731,#93732,#93733,#93734,#93735,#93736,#93737,#93738,#93739,#93740,
#93741,#93742,#93743,#93744,#93745,#93746,#93747,#93748,#93749,#93750,#93751,
#93752,#93753,#93754,#93755,#93756,#93757,#93758,#93759,#93760,#93761,#93762,
#93763,#93764,#93765,#93766,#93767,#93768,#93769,#93770,#93771,#93772,#93773,
#93774,#93775,#93776,#93777,#93778,#93779,#93780,#93781,#93782,#93783,#93784,
#93785,#93786,#93787,#93788,#93789,#93790,#93791,#93792,#93793,#93794,#93795,
#93796,#93797,#93798,#93799,#93800,#93801,#93802,#93803,#93804,#93805,#93806,
#93807,#93808,#93809,#93810,#93811,#93812,#93813,#93814,#93815,#93816,#93817,
#93818,#93819,#93820,#93821,#93822,#93823,#93824,#93825,#93826,#93827,#93828,
#93829,#93830,#93831,#93832,#93833,#93834,#93835,#93836,#93837,#93838,#93839,
#93840,#93841,#93842,#93843,#93844,#93845,#93846,#93847,#93848,#93849,#93850,
#93851,#93852,#93853,#93854,#93855,#93856,#93857,#93858,#93859,#93860,#93861,
#93862,#93863,#93864,#93865,#93866,#93867,#93868,#93869,#93870,#93871,#93872,
#93873,#93874,#93875,#93876,#93877,#93878,#93879,#93880,#93881,#93882,#93883,
#93884,#93885,#93886,#93887,#93888,#93889,#93890,#93891,#93892,#93893,#93894,
#93895,#93896,#93897,#93898,#93899,#93900,#93901,#93902,#93903,#93904,#93905,
#93906,#93907,#93908,#93909,#93910,#93911,#93912,#93913,#93914,#93915,#93916,
#93917,#93918,#93919,#93920,#93921,#93922,#93923,#93924,#93925,#93926,#93927,
#93928,#93929,#93930,#93931,#93932,#93933,#93934,#93935,#93936,#93937,#93938,
#93939,#93940,#93941,#93942,#93943,#93944,#93945,#93946,#93947,#93948,#93949,
#93950,#93951,#93952,#93953,#93954,#93955,#93956,#93957,#93958,#93959,#93960,
#93961,#93962,#93963,#93964,#93965,#93966,#93967,#93968,#93969,#93970,#93971,
#93972,#93973,#93974,#93975,#93976,#93977,#93978,#93979,#93980,#93981,#93982,
#93983,#93984,#93985,#93986,#93987,#93988,#93989,#93990,#93991,#93992,#93993,
#93994,#93995,#93996,#93997,#93998,#93999,#94000,#94001,#94002,#94003,#94004,
#94005,#94006,#94007,#94008,#94009,#94010,#94011,#94012,#94013,#94014,#94015,
#94016,#94017,#94018,#94019,#94020,#94021,#94022,#94023,#94024,#94025,#94026,
#94027,#94028,#94029,#94030,#94031,#94032,#94033,#94034,#94035,#94036,#94037,
#94038,#94039,#94040,#94041,#94042,#94043,#94044,#94045,#94046,#94047,#94048,
#94049,#94050,#94051,#94052,#94053,#94054,#94055,#94056,#94057,#94058,#94059,
#94060,#94061,#94062,#94063,#94064,#94065,#94066,#94067,#94068,#94069,#94070,
#94071,#94072,#94073,#94074,#94075,#94076,#94077,#94078,#94079,#94080,#94081,
#94082,#94083,#94084,#94085,#94086,#94087,#94088,#94089,#94090,#94091,#94092,
#94093,#94094,#94095,#94096,#94097,#94098,#94099,#94100,#94101,#94102,#94103,
#94104,#94105,#94106,#94107,#94108,#94109,#94110,#94111,#94112,#94113,#94114,
#94115,#94116,#94117,#94118,#94119,#94120,#94121,#94122,#94123,#94124,#94125,
#94126,#94127,#94128,#94129,#94130,#94131,#94132,#94133,#94134,#94135,#94136,
#94137,#94138,#94139,#94140,#94141,#94142,#94143,#94144,#94145,#94146,#94147,
#94148,#94149,#94150,#94151,#94152,#94153,#94154,#94155,#94156,#94157,#94158,
#94159,#94160,#94161,#94162,#94163,#94164,#94165,#94166,#94167,#94168,#94169,
#94170,#94171,#94172,#94173,#94174,#94175,#94176,#94177,#94178,#94179,#94180,
#94181,#94182,#94183,#94184,#94185,#94186,#94187,#94188,#94189,#94190,#94191,
#94192,#94193,#94194,#94195,#94196,#94197,#94198,#94199,#94200,#94201,#94202,
#94203,#94204,#94205,#94206,#94207,#94208,#94209,#94210,#94211,#94212,#94213,
#94214,#94215,#94216,#94217,#94218,#94219,#94220,#94221,#94222,#94223,#94224,
#94225,#94226,#94227,#94228,#94229,#94230,#94231,#94232,#94233,#94234,#94235,
#94236,#94237,#94238,#94239,#94240,#94241,#94242,#94243,#94244,#94245,#94246,
#94247,#94248,#94249,#94250,#94251,#94252,#94253,#94254,#94255,#94256,#94257,
#94258,#94259,#94260,#94261,#94262,#94263,#94264,#94265,#94266,#94267,#94268,
#94269,#94270,#94271,#94272,#94273,#94274,#94275,#94276,#94277,#94278,#94279,
#94280,#94281,#94282,#94283,#94284,#94285,#94286,#94287,#94288,#94289,#94290,
#94291,#94292,#94293,#94294,#94295,#94296,#94297,#94298,#94299,#94300,#94301,
#94302,#94303,#94304,#94305,#94306,#94307,#94308,#94309,#94310,#94311,#94312,
#94313,#94314,#94315,#94316,#94317,#94318,#94319,#94320,#94321,#94322,#94323,
#94324,#94325,#94326,#94327,#94328,#94329,#94330,#94331,#94332,#94333,#94334,
#94335,#94336,#94337,#94338,#94339,#94340,#94341,#94342,#94343,#94344,#94345,
#94346,#94347,#94348,#94349,#94350,#94351,#94352,#94353,#94354,#94355,#94356,
#94357,#94358,#94359,#94360,#94361,#94362,#94363,#94364,#94365,#94366,#94367,
#94368,#94369,#94370,#94371,#94372,#94373,#94374,#94375,#94376,#94377,#94378,
#94379,#94380,#94381,#94382,#94383,#94384,#94385,#94386,#94387,#94388,#94389,
#94390,#94391,#94392,#94393,#94394,#94395,#94396,#94397,#94398,#94399,#94400,
#94401,#94402,#94403,#94404,#94405,#94406,#94407,#94408,#94409,#94410,#94411,
#94412,#94413,#94414,#94415,#94416,#94417,#94418,#94419,#94420,#94421,#94422,
#94423,#94424,#94425,#94426,#94427,#94428,#94429,#94430,#94431,#94432,#94433,
#94434,#94435,#94436,#94437,#94438,#94439,#94440,#94441,#94442,#94443,#94444,
#94445,#94446,#94447,#94448,#94449,#94450,#94451,#94452,#94453,#94454,#94455,
#94456,#94457,#94458,#94459,#94460,#94461,#94462,#94463,#94464,#94465,#94466,
#94467,#94468,#94469,#94470,#94471,#94472,#94473,#94474,#94475,#94476,#94477,
#94478,#94479,#94480,#94481,#94482,#94483,#94484,#94485,#94486,#94487,#94488,
#94489,#94490,#94491,#94492,#94493,#94494,#94495,#94496,#94497,#94498,#94499,
#94500,#94501,#94502,#94503,#94504,#94505,#94506,#94507,#94508,#94509,#94510,
#94511,#94512,#94513,#94514,#94515,#94516,#94517,#94518,#94519,#94520,#94521,
#94522,#94523,#94524,#94525,#94526,#94527,#94528,#94529,#94530,#94531,#94532,
#94533,#94534,#94535,#94536,#94537,#94538,#94539,#94540,#94541,#94542,#94543,
#94544,#94545,#94546,#94547,#94548,#94549,#94550,#94551,#94552,#94553,#94554,
#94555,#94556,#94557,#94558,#94559,#94560,#94561,#94562,#94563,#94564,#94565,
#94566,#94567,#94568,#94569,#94570,#94571,#94572,#94573,#94574,#94575,#94576,
#94577,#94578,#94579,#94580,#94581,#94582,#94583,#94584,#94585,#94586,#94587,
#94588,#94589,#94590,#94591,#94592,#94593,#94594,#94595,#94596,#94597,#94598,
#94599,#94600,#94601,#94602,#94603,#94604,#94605,#94606,#94607,#94608,#94609,
#94610,#94611,#94612,#94613,#94614,#94615,#94616,#94617,#94618,#94619,#94620,
#94621,#94622,#94623,#94624,#94625,#94626,#94627,#94628,#94629,#94630,#94631,
#94632,#94633,#94634,#94635,#94636,#94637,#94638,#94639,#94640,#94641,#94642,
#94643,#94644,#94645,#94646,#94647,#94648,#94649,#94650,#94651,#94652,#94653,
#94654,#94655,#94656,#94657,#94658,#94659,#94660,#94661,#94662,#94663,#94664,
#94665,#94666,#94667,#94668,#94669,#94670,#94671,#94672,#94673,#94674,#94675,
#94676,#94677,#94678,#94679,#94680,#94681,#94682,#94683,#94684,#94685,#94686,
#94687,#94688,#94689,#94690,#94691,#94692,#94693,#94694,#94695,#94696,#94697,
#94698,#94699,#94700,#94701,#94702,#94703,#94704,#94705,#94706,#94707,#94708,
#94709,#94710,#94711,#94712,#94713,#94714,#94715,#94716,#94717,#94718,#94719,
#94720,#94721,#94722,#94723,#94724,#94725,#94726,#94727,#94728,#94729,#94730,
#94731,#94732,#94733,#94734,#94735,#94736,#94737,#94738,#94739,#94740,#94741,
#94742,#94743,#94744,#94745,#94746,#94747,#94748,#94749,#94750,#94751,#94752,
#94753,#94754,#94755,#94756,#94757,#94758,#94759,#94760,#94761,#94762,#94763,
#94764,#94765,#94766,#94767,#94768,#94769,#94770,#94771,#94772,#94773,#94774,
#94775,#94776,#94777,#94778,#94779,#94780,#94781,#94782,#94783,#94784,#94785,
#94786,#94787,#94788,#94789,#94790,#94791,#94792,#94793,#94794,#94795,#94796,
#94797,#94798,#94799,#94800,#94801,#94802,#94803,#94804,#94805,#94806,#94807,
#94808,#94809,#94810,#94811,#94812,#94813,#94814,#94815,#94816,#94817,#94818,
#94819,#94820,#94821,#94822,#94823,#94824,#94825,#94826,#94827,#94828,#94829,
#94830,#94831,#94832,#94833,#94834,#94835,#94836,#94837,#94838,#94839,#94840,
#94841,#94842,#94843,#94844,#94845,#94846,#94847,#94848,#94849,#94850,#94851,
#94852,#94853,#94854,#94855,#94856,#94857,#94858,#94859,#94860,#94861,#94862,
#94863,#94864,#94865,#94866,#94867,#94868,#94869,#94870,#94871,#94872,#94873,
#94874,#94875,#94876,#94877,#94878,#94879,#94880,#94881,#94882,#94883,#94884,
#94885,#94886,#94887,#94888,#94889,#94890,#94891,#94892,#94893,#94894,#94895,
#94896,#94897,#94898,#94899,#94900,#94901,#94902,#94903,#94904,#94905,#94906,
#94907,#94908,#94909,#94910,#94911,#94912,#94913,#94914,#94915,#94916,#94917,
#94918,#94919,#94920,#94921,#94922,#94923,#94924,#94925,#94926,#94927,#94928,
#94929,#94930,#94931,#94932,#94933,#94934,#94935,#94936,#94937,#94938,#94939,
#94940,#94941,#94942,#94943,#94944,#94945,#94946,#94947,#94948,#94949,#94950,
#94951,#94952,#94953,#94954,#94955,#94956,#94957,#94958,#94959,#94960,#94961,
#94962,#94963,#94964,#94965,#94966,#94967,#94968,#94969,#94970,#94971,#94972,
#94973,#94974,#94975,#94976,#94977,#94978,#94979,#94980,#94981,#94982,#94983,
#94984,#94985,#94986,#94987,#94988,#94989,#94990,#94991,#94992,#94993,#94994,
#94995,#94996,#94997,#94998,#94999,#95000,#95001,#95002,#95003,#95004,#95005,
#95006,#95007,#95008,#95009,#95010,#95011,#95012,#95013,#95014,#95015,#95016,
#95017,#95018,#95019,#95020,#95021,#95022,#95023,#95024,#95025,#95026,#95027,
#95028,#95029,#95030,#95031,#95032,#95033,#95034,#95035,#95036,#95037,#95038,
#95039,#95040,#95041,#95042,#95043,#95044,#95045,#95046,#95047,#95048,#95049,
#95050,#95051,#95052,#95053,#95054,#95055,#95056,#95057,#95058,#95059,#95060,
#95061,#95062,#95063,#95064,#95065,#95066,#95067,#95068,#95069,#95070,#95071,
#95072,#95073,#95074,#95075,#95076,#95077,#95078,#95079,#95080,#95081,#95082,
#95083,#95084,#95085,#95086,#95087,#95088,#95089,#95090,#95091,#95092,#95093,
#95094,#95095,#95096,#95097,#95098,#95099,#95100,#95101,#95102,#95103,#95104,
#95105,#95106,#95107,#95108,#95109,#95110,#95111,#95112,#95113,#95114,#95115,
#95116,#95117,#95118,#95119,#95120,#95121,#95122,#95123,#95124,#95125,#95126,
#95127,#95128,#95129,#95130,#95131,#95132,#95133,#95134,#95135,#95136,#95137,
#95138,#95139,#95140,#95141,#95142,#95143,#95144,#95145,#95146,#95147,#95148,
#95149,#95150,#95151,#95152,#95153,#95154,#95155,#95156,#95157,#95158,#95159,
#95160,#95161,#95162,#95163,#95164,#95165,#95166,#95167,#95168,#95169,#95170,
#95171,#95172,#95173,#95174,#95175,#95176,#95177,#95178,#95179,#95180,#95181,
#95182,#95183,#95184,#95185,#95186,#95187,#95188,#95189,#95190,#95191,#95192,
#95193,#95194,#95195,#95196,#95197,#95198,#95199,#95200,#95201,#95202,#95203,
#95204,#95205,#95206,#95207,#95208,#95209,#95210,#95211,#95212,#95213,#95214,
#95215,#95216,#95217,#95218,#95219,#95220,#95221,#95222,#95223,#95224,#95225,
#95226,#95227,#95228,#95229,#95230,#95231,#95232,#95233,#95234,#95235,#95236,
#95237,#95238,#95239,#95240,#95241,#95242,#95243,#95244,#95245,#95246,#95247,
#95248,#95249,#95250,#95251,#95252,#95253,#95254,#95255,#95256,#95257,#95258,
#95259,#95260,#95261,#95262,#95263,#95264,#95265,#95266,#95267,#95268,#95269,
#95270,#95271,#95272,#95273,#95274,#95275,#95276,#95277,#95278,#95279,#95280,
#95281,#95282,#95283,#95284,#95285,#95286,#95287,#95288,#95289,#95290,#95291,
#95292,#95293,#95294,#95295,#95296,#95297,#95298,#95299,#95300,#95301,#95302,
#95303,#95304,#95305,#95306,#95307,#95308,#95309,#95310,#95311,#95312,#95313,
#95314,#95315,#95316,#95317,#95318,#95319,#95320,#95321,#95322,#95323,#95324,
#95325,#95326,#95327,#95328,#95329,#95330,#95331,#95332,#95333,#95334,#95335,
#95336,#95337,#95338,#95339,#95340,#95341,#95342,#95343,#95344,#95345,#95346,
#95347,#95348,#95349,#95350,#95351,#95352,#95353,#95354,#95355,#95356,#95357,
#95358,#95359,#95360,#95361,#95362,#95363,#95364,#95365,#95366,#95367,#95368,
#95369,#95370,#95371,#95372,#95373,#95374,#95375,#95376,#95377,#95378,#95379,
#95380,#95381,#95382,#95383,#95384,#95385,#95386,#95387,#95388,#95389,#95390,
#95391,#95392,#95393,#95394,#95395,#95396,#95397,#95398,#95399,#95400,#95401,
#95402,#95403,#95404,#95405,#95406,#95407,#95408,#95409,#95410,#95411,#95412,
#95413,#95414,#95415,#95416,#95417,#95418,#95419,#95420,#95421,#95422,#95423,
#95424,#95425,#95426,#95427,#95428,#95429,#95430,#95431,#95432,#95433,#95434,
#95435,#95436,#95437,#95438,#95439,#95440,#95441,#95442,#95443,#95444,#95445,
#95446,#95447,#95448,#95449,#95450,#95451,#95452,#95453,#95454,#95455,#95456,
#95457,#95458,#95459,#95460,#95461,#95462,#95463,#95464,#95465,#95466,#95467,
#95468,#95469,#95470,#95471,#95472,#95473,#95474,#95475,#95476,#95477,#95478,
#95479,#95480,#95481,#95482,#95483,#95484,#95485,#95486,#95487,#95488,#95489,
#95490,#95491,#95492,#95493,#95494,#95495,#95496,#95497,#95498,#95499,#95500,
#95501,#95502,#95503,#95504,#95505,#95506,#95507,#95508,#95509,#95510,#95511,
#95512,#95513,#95514,#95515,#95516,#95517,#95518,#95519,#95520,#95521,#95522,
#95523,#95524,#95525,#95526,#95527,#95528,#95529,#95530,#95531,#95532,#95533,
#95534,#95535,#95536,#95537,#95538,#95539,#95540,#95541,#95542,#95543,#95544,
#95545,#95546,#95547,#95548,#95549,#95550,#95551,#95552,#95553,#95554,#95555,
#95556,#95557,#95558,#95559,#95560,#95561,#95562,#95563,#95564,#95565,#95566,
#95567,#95568,#95569,#95570,#95571,#95572,#95573,#95574,#95575,#95576,#95577,
#95578,#95579,#95580,#95581,#95582,#95583,#95584,#95585,#95586,#95587,#95588,
#95589,#95590,#95591,#95592,#95593,#95594,#95595,#95596,#95597,#95598,#95599,
#95600,#95601,#95602,#95603,#95604,#95605,#95606,#95607,#95608,#95609,#95610,
#95611,#95612,#95613,#95614,#95615,#95616,#95617,#95618,#95619,#95620,#95621,
#95622,#95623,#95624,#95625,#95626,#95627,#95628,#95629,#95630,#95631,#95632,
#95633,#95634,#95635,#95636,#95637,#95638,#95639,#95640,#95641,#95642,#95643,
#95644,#95645,#95646)),.UNSPECIFIED.,.F.,.F.,.F.,(2,2),(4,1,1,1,1,1,1,1,
1,1,1,1,1,1,1,1,1,1,1,1,1,1,1,1,1,1,1,1,1,1,1,1,1,1,1,1,1,1,1,1,1,1,1,1,
1,1,1,1,1,1,1,1,1,1,1,1,1,1,1,1,1,1,1,1,1,1,1,1,1,1,1,1,1,1,1,1,1,1,1,1,
1,1,1,1,1,1,1,1,1,1,1,1,1,1,1,1,1,1,1,1,1,1,1,1,1,1,1,1,1,1,1,1,1,1,1,1,
1,1,1,1,1,1,1,1,1,1,1,1,1,1,1,1,1,1,1,1,1,1,1,1,1,1,1,1,1,1,1,1,1,1,1,1,
1,1,1,1,1,1,1,1,1,1,1,1,1,1,1,1,1,1,1,1,1,1,1,1,1,1,1,1,1,1,1,1,1,1,1,1,
1,1,1,1,1,1,1,1,1,1,1,1,1,1,1,1,1,1,1,1,1,1,1,1,1,1,1,1,1,1,1,1,1,1,1,1,
1,1,1,1,1,1,1,1,1,1,1,1,1,1,1,1,1,1,1,1,1,1,1,1,1,1,1,1,1,1,1,1,1,1,1,1,
1,1,1,1,1,1,1,1,1,1,1,1,1,1,1,1,1,1,1,1,1,1,1,1,1,1,1,1,1,1,1,1,1,1,1,1,
1,1,1,1,1,1,1,1,1,1,1,1,1,1,1,1,1,1,1,1,1,1,1,1,1,1,1,1,1,1,1,1,1,1,1,1,
1,1,1,1,1,1,1,1,1,1,1,1,1,1,1,1,1,1,1,1,1,1,1,1,1,1,1,1,1,1,1,1,1,1,1,1,
1,1,1,1,1,1,1,1,1,1,1,1,1,1,1,1,1,1,1,1,1,1,1,1,1,1,1,1,1,1,1,1,1,1,1,1,
1,1,1,1,1,1,1,1,1,1,1,1,1,1,1,1,1,1,1,1,1,1,1,1,1,1,1,1,1,1,1,1,1,1,1,1,
1,1,1,1,1,1,1,1,1,1,1,1,1,1,1,1,1,1,1,1,1,1,1,1,1,1,1,1,1,1,1,1,1,1,1,1,
1,1,1,1,1,1,1,1,1,1,1,1,1,1,1,1,1,1,1,1,1,1,1,1,1,1,1,1,1,1,1,1,1,1,1,1,
1,1,1,1,1,1,1,1,1,1,1,1,1,1,1,1,1,1,1,1,1,1,1,1,1,1,1,1,1,1,1,1,1,1,1,1,
1,1,1,1,1,1,1,1,1,1,1,1,1,1,1,1,1,1,1,1,1,1,1,1,1,1,1,1,1,1,1,1,1,1,1,1,
1,1,1,1,1,1,1,1,1,1,1,1,1,1,1,1,1,1,1,1,1,1,1,1,1,1,1,1,1,1,1,1,1,1,1,1,
1,1,1,1,1,1,1,1,1,1,1,1,1,1,1,1,1,1,1,1,1,1,1,1,1,1,1,1,1,1,1,1,1,1,1,1,
1,1,1,1,1,1,1,1,1,1,1,1,1,1,1,1,1,1,1,1,1,1,1,1,1,1,1,1,1,1,1,1,1,1,1,1,
1,1,1,1,1,1,1,1,1,1,1,1,1,1,1,1,1,1,1,1,1,1,1,1,1,1,1,1,1,1,1,1,1,1,1,1,
1,1,1,1,1,1,1,1,1,1,1,1,1,1,1,1,1,1,1,1,1,1,1,1,1,1,1,1,1,1,1,1,1,1,1,1,
1,1,1,1,1,1,1,1,1,1,1,1,1,1,1,1,1,1,1,1,1,1,1,1,1,1,1,1,1,1,1,1,1,1,1,1,
1,1,1,1,1,1,1,1,1,1,1,1,1,1,1,1,1,1,1,1,1,1,1,1,1,1,1,1,1,1,1,1,1,1,1,1,
1,1,1,1,1,1,1,1,1,1,1,1,1,1,1,1,1,1,1,1,1,1,1,1,1,1,1,1,1,1,1,1,1,1,1,1,
1,1,1,1,1,1,1,1,1,1,1,1,1,1,1,1,1,1,1,1,1,1,1,1,1,1,1,1,1,1,1,1,1,1,1,1,
1,1,1,1,1,1,1,1,1,1,1,1,1,1,1,1,1,1,1,1,1,1,1,1,1,1,1,1,1,1,1,1,1,1,1,1,
1,1,1,1,1,1,1,1,1,1,1,1,1,1,1,1,1,1,1,1,1,1,1,1,1,1,1,1,1,1,1,1,1,1,1,1,
1,1,1,1,1,1,1,1,1,1,1,1,1,1,1,1,1,1,1,1,1,1,1,1,1,1,1,1,1,1,1,1,1,1,1,1,
1,1,1,1,1,1,1,1,1,1,1,1,1,1,1,1,1,1,1,1,1,1,1,1,1,1,1,1,1,1,1,1,1,1,1,1,
1,1,1,1,1,1,1,1,1,1,1,1,1,1,1,1,1,1,1,1,1,1,1,1,1,1,1,1,1,1,1,1,1,1,1,1,
1,1,1,1,1,1,1,1,1,1,1,1,1,1,1,1,1,1,1,1,1,1,1,1,1,1,1,1,1,1,1,1,1,1,1,1,
1,1,1,1,1,1,1,1,1,1,1,1,1,1,1,1,1,1,1,1,1,1,1,1,1,1,1,1,1,1,1,1,1,1,1,1,
1,1,1,1,1,1,1,1,1,1,1,1,1,1,1,1,1,1,1,1,1,1,1,1,1,1,1,1,1,1,1,1,1,1,1,1,
1,1,1,1,1,1,1,1,1,1,1,1,1,1,1,1,1,1,1,1,1,1,1,1,1,1,1,1,1,1,1,1,1,1,1,1,
1,1,1,1,1,1,1,1,1,1,1,1,1,1,1,1,1,1,1,1,1,1,1,1,1,1,1,1,1,1,1,1,1,1,1,1,
1,1,1,1,1,1,1,1,1,1,1,1,1,1,1,1,1,1,1,1,1,1,1,1,1,1,1,1,1,1,1,1,1,1,1,1,
1,1,1,1,1,1,1,1,1,1,1,1,1,1,1,1,1,1,1,1,1,1,1,1,1,1,1,1,1,1,1,1,1,1,1,1,
1,1,1,1,1,1,1,1,1,1,1,1,1,1,1,1,1,1,1,1,1,1,1,1,1,1,1,1,1,1,1,1,1,1,1,1,
1,1,1,1,1,1,1,1,1,1,1,1,1,1,1,1,1,1,1,1,1,1,1,1,1,1,1,1,1,1,1,1,1,1,1,1,
1,1,1,1,1,1,1,1,1,1,1,1,1,1,1,1,1,1,1,1,1,1,1,1,1,1,1,1,1,1,1,1,1,1,1,1,
1,1,1,1,1,1,1,1,1,1,1,1,1,1,1,1,1,1,1,1,1,1,1,1,1,1,1,1,1,1,1,1,1,1,1,1,
1,1,1,1,1,1,1,1,1,1,1,1,1,1,1,1,1,1,1,1,1,1,1,1,1,1,1,1,1,1,1,1,1,1,1,1,
1,1,1,1,1,1,1,1,1,1,1,1,1,1,1,1,1,1,1,1,1,1,1,1,1,1,1,1,1,1,1,1,1,1,1,1,
1,1,1,1,1,1,1,1,1,1,1,1,1,1,1,1,1,1,1,1,1,1,1,1,1,1,1,1,1,1,1,1,1,1,1,1,
1,1,1,1,1,1,1,1,1,1,1,1,1,1,1,1,1,1,1,1,1,1,1,1,1,1,1,1,1,1,1,1,1,1,1,1,
1,1,1,1,1,1,1,1,1,1,1,1,1,1,1,1,1,1,1,1,1,1,1,1,1,1,1,1,1,1,1,1,1,1,1,1,
1,1,1,1,1,1,1,1,1,1,1,1,1,1,1,1,1,1,1,1,1,1,1,1,1,1,1,1,1,1,1,1,1,1,1,1,
1,1,1,1,1,1,1,1,1,1,1,1,1,1,1,1,1,1,1,1,1,1,1,1,1,1,1,1,1,1,1,1,1,1,1,1,
1,1,1,1,1,1,1,1,1,1,1,1,1,1,1,1,1,1,1,1,1,1,1,1,1,1,1,1,1,1,1,1,1,1,1,1,
1,1,1,1,1,1,1,1,1,1,1,1,1,1,1,1,1,1,1,1,1,1,1,1,1,1,1,1,1,1,1,1,1,1,1,1,
1,1,1,1,1,1,1,1,1,1,1,1,1,1,1,1,1,1,1,1,1,1,1,1,1,1,1,1,1,1,1,1,1,1,1,1,
1,1,1,1,1,1,1,1,1,1,1,1,1,1,1,1,1,1,1,1,1,1,1,1,1,1,1,1,1,1,1,1,1,1,1,1,
1,1,1,1,1,1,1,1,1,1,1,1,1,1,1,1,1,1,1,1,1,1,1,1,1,1,1,1,1,1,1,1,1,1,1,1,
1,1,1,1,1,1,1,1,1,1,1,1,1,1,1,1,1,1,1,1,1,1,1,1,1,1,1,1,1,1,1,1,1,1,1,1,
1,1,1,1,1,1,1,1,1,1,1,1,1,1,1,1,1,1,1,1,1,1,1,1,1,1,1,1,1,1,1,1,1,1,1,1,
1,1,1,1,1,1,1,1,1,1,1,1,1,1,1,1,1,1,1,1,1,1,1,1,1,1,1,1,1,1,1,1,1,1,1,1,
1,1,1,1,1,1,1,1,1,1,1,1,1,1,1,1,1,1,1,1,1,1,1,1,1,1,1,1,1,1,1,1,1,1,1,1,
1,1,1,1,1,1,1,1,1,1,1,1,1,1,1,1,1,1,1,1,1,1,1,1,1,1,1,1,1,1,1,1,1,1,1,1,
1,1,1,1,1,1,1,1,1,1,1,1,1,1,1,1,1,1,1,1,1,1,1,1,1,1,1,1,1,1,1,1,1,1,1,1,
1,1,1,1,1,1,1,1,1,1,1,1,1,1,1,1,1,1,1,1,1,1,1,1,1,1,1,1,1,1,1,1,1,1,1,1,
1,1,1,1,1,1,1,1,1,1,1,1,1,1,1,1,1,1,1,1,1,1,1,1,1,1,1,1,1,1,1,1,1,1,1,1,
1,1,1,1,1,1,1,1,1,1,1,1,1,1,1,1,1,1,1,1,1,1,1,1,1,1,1,1,1,1,1,1,1,1,1,1,
1,1,1,1,1,1,1,1,1,1,1,1,1,1,1,1,1,1,1,1,1,1,1,1,1,1,1,1,1,1,1,1,1,1,1,1,
1,1,1,1,1,1,1,1,1,1,1,1,1,1,1,1,1,1,1,1,1,1,1,1,1,1,1,1,1,1,1,1,1,1,1,1,
1,1,1,1,1,1,1,1,1,1,1,1,1,1,1,1,1,1,1,1,1,1,1,1,1,1,1,1,1,1,1,1,1,1,1,1,
1,1,1,1,1,1,1,1,1,1,1,1,1,1,1,1,1,1,1,1,1,1,1,1,1,1,1,1,1,1,1,1,1,1,1,1,
1,1,1,1,1,1,1,1,1,1,1,1,1,1,1,1,1,1,1,1,1,1,1,1,1,1,1,1,1,1,1,1,1,1,1,1,
1,1,1,1,1,1,1,1,1,1,1,1,1,1,1,1,1,1,1,1,1,1,1,1,1,1,1,1,1,1,1,1,1,1,1,1,
1,1,1,1,1,1,1,1,1,1,1,1,1,1,1,1,1,1,1,1,1,1,1,1,1,1,1,1,1,1,1,1,1,1,1,1,
1,1,1,1,1,1,1,1,1,1,1,1,1,1,1,1,1,1,1,1,1,1,1,1,1,1,1,1,1,1,1,1,1,1,1,1,
1,1,1,1,1,1,1,1,1,1,1,1,1,1,1,1,1,1,1,1,1,1,1,1,1,1,1,1,1,1,1,1,1,1,1,1,
1,1,1,1,1,1,1,1,1,1,1,1,1,1,1,1,1,1,1,1,1,1,1,1,1,1,1,1,1,1,1,1,1,1,1,1,
1,1,1,1,1,1,1,1,1,1,1,1,1,1,1,1,1,1,1,1,1,1,1,1,1,1,1,1,1,1,1,1,1,1,1,1,
1,1,1,1,1,1,1,1,1,1,1,1,1,1,1,1,1,1,1,1,1,1,1,1,1,1,1,1,1,1,1,1,1,1,1,1,
1,1,1,1,1,1,1,1,1,1,1,1,1,1,1,1,1,1,1,1,1,1,1,1,1,1,1,1,1,1,1,1,1,1,1,1,
1,1,1,1,1,1,1,1,1,1,1,1,1,1,1,1,1,1,1,1,1,1,1,1,1,1,1,1,1,1,1,1,1,1,1,1,
1,1,1,1,1,1,1,1,1,1,1,1,1,1,1,1,1,1,1,1,1,1,1,1,1,1,1,1,1,1,1,1,1,1,1,1,
1,1,1,1,1,1,1,1,1,1,1,1,1,1,1,1,1,1,1,1,1,1,1,1,1,1,1,1,1,1,1,1,1,1,1,1,
1,1,1,1,1,1,1,1,1,1,1,1,1,1,1,1,1,1,1,1,1,1,1,1,1,1,1,1,1,1,1,1,1,1,1,1,
1,1,1,1,1,1,1,1,1,1,1,1,1,1,1,1,1,1,1,1,1,1,1,1,1,1,1,1,1,1,1,1,1,1,1,1,
1,1,1,1,1,1,1,1,1,1,1,1,1,1,1,1,1,1,1,1,1,1,1,1,1,1,1,1,1,1,1,1,1,1,1,1,
1,1,1,1,1,1,1,1,1,1,1,1,1,1,1,1,1,1,1,1,1,1,1,1,1,1,1,1,1,1,1,1,1,1,1,1,
1,1,1,1,1,1,1,1,1,1,1,1,1,1,1,1,1,1,1,1,1,1,1,1,1,1,1,1,1,1,1,1,1,1,1,1,
1,1,1,1,1,1,1,1,1,1,1,1,1,1,1,1,1,1,1,1,1,1,1,1,1,1,1,1,1,1,1,1,1,1,1,1,
1,1,1,1,1,1,1,1,1,1,1,1,1,1,1,1,1,1,1,1,1,1,1,1,1,1,1,1,1,1,1,1,1,1,1,1,
1,1,1,1,1,1,1,1,1,1,1,1,1,1,1,1,1,1,1,1,1,1,1,1,1,1,1,1,1,1,1,1,1,1,1,1,
1,1,1,1,1,1,1,1,1,1,1,1,1,1,1,1,1,1,1,1,1,1,1,1,1,1,1,1,1,1,1,1,1,1,1,1,
1,1,1,1,1,1,1,1,1,1,1,1,1,1,1,1,1,1,1,1,1,1,1,1,1,1,1,1,1,1,1,1,1,1,1,1,
1,1,1,1,1,1,1,1,1,1,1,1,1,1,1,1,1,1,1,1,1,1,1,1,1,1,1,1,1,1,1,1,1,1,1,1,
1,1,1,1,1,1,1,1,1,1,1,1,1,1,1,1,1,1,1,1,1,1,1,1,1,1,1,1,1,1,1,1,1,1,1,1,
1,1,1,1,1,1,1,1,1,1,1,1,1,1,1,1,1,1,1,1,1,1,1,1,1,1,1,1,1,1,1,1,1,1,1,1,
1,1,1,1,1,1,1,1,1,1,1,1,1,1,1,1,1,1,1,1,1,1,1,1,1,1,1,1,1,1,1,1,1,1,1,1,
1,1,1,1,1,1,1,1,1,1,1,1,1,1,1,1,1,1,1,1,1,1,1,1,1,1,1,1,1,1,1,1,1,1,1,1,
1,1,1,1,1,1,1,1,1,1,1,1,1,1,1,1,1,1,1,1,1,1,1,1,1,1,1,1,1,1,1,1,1,1,1,1,
1,1,1,1,1,1,1,1,1,1,1,1,1,1,1,1,1,1,1,1,1,1,1,1,1,1,1,1,1,1,1,1,1,1,1,1,
1,1,1,1,1,1,1,1,1,1,1,1,1,1,1,1,1,1,1,1,1,1,1,1,1,1,1,1,1,1,1,1,1,1,1,1,
1,1,1,1,1,1,1,1,1,1,1,1,1,1,1,1,1,1,4),(-1.76619037896906,-1.18309518948453),
(0.,0.869746702321014,1.7394931589914,2.60923976624962,3.47983908319159,
4.35043840179749,5.22018503077054,6.08993165951504,6.95967828799171,7.82942491616733,
8.69917154401062,9.56891817149224,10.4395174886835,11.3101168056706,12.179863432132,
13.049610058144,13.9193566836854,14.7891033087372,15.6588499332817,16.5285965573034,
17.3991958717975,18.2697951860185,18.7046684974166,19.1395418086746,19.5744151197912,
20.0092884307654,20.4441617415962,20.8790350522825,21.7487816732187,22.1836549834672,
22.6185282935685,23.0534016035221,23.4882749133276,23.9231482229848,24.3588742245859,
24.794600226187,25.2294735355468,26.0992201538203,26.5340934627341,26.9689667714994,
27.4038400801166,27.838713388586,28.2735866969081,28.7084600050832,29.143333313112,
29.5782066209952,30.0130799287334,30.4479532363275,30.8828265437783,31.3185525442794,
31.7542785447804,32.1891518519474,32.6240251589741,33.0588984658616,33.4937717726112,
33.928645079224,34.3635183857014,34.7983916920448,35.2332649982556,35.6681383043353,
36.1030116102854,36.5378849161076,36.9727582218035,37.4076315273749,37.8425048328235,
38.2782308323341,38.7139568318446,39.1488301370532,39.5837034421446,40.0185767471208,
40.4534500519838,40.8883233567357,41.3231966613787,41.7580699659148,42.1929432703463,
42.6278165746754,43.0626898789044,43.4975631830356,43.9324364870714,44.3673097910142,
44.8021830948664,45.2379090935952,45.673635092324,46.1085083960024,46.5433816995978,
46.9782550031127,47.4131283065497,47.8480016099115,48.2828749132006,48.7177482164198,
49.1526215195718,49.5874948226593,50.0223681256851,50.457241428652,50.8921147315628,
51.3269880344203,51.7618613372274,52.197587335454,52.6333133336805,53.0681866363954,
53.5030599390685,53.9379332417027,54.3728065443011,54.8076798468664,55.2425531494018,
55.6774264519101,56.1122997543943,56.5471730568575,56.9820463593026,57.4169196617326,
57.8517929641506,58.2866662665595,58.7215395689624,59.157265567009,59.5929915650557,
60.0278648674556,60.4627381698584,60.8976114722673,61.3324847746853,61.7673580771153,
62.2022313795604,62.6371046820236,63.0719779845079,63.5068512870162,63.9417245895516,
64.376597892117,64.8114711947155,65.2463444973499,65.6812178000231,66.1169437982275,
66.5526697964318,66.9875430991915,67.4224164019987,67.8572897048563,68.2921630077673,
68.7270363107343,69.1619096137603,69.5967829168479,70.0316562200001,70.4665295232194,
70.9014028265087,71.3362761298705,71.7711494333077,72.2060227368227,72.6408960404182,
73.0766220391044,73.5123480377905,73.9472213415547,74.382094645407,74.8169679493499,
75.2518412533859,75.6867145575172,76.1215878617464,76.5564611660756,76.9913344705072,
77.4262077750435,77.8610810796866,78.2959543844386,78.7308276893018,79.1657009942781,
79.6005742993696,80.0363002988208,80.4720262982719,80.9068996035997,81.3417729090484,
81.7766462146199,82.211519520316,82.6463928261383,83.0812661320886,83.5161394381684,
83.9510127443794,84.3858860507229,84.8207593572004,85.2556326638134,85.6905059705631,
86.1253792774507,86.5602525844776,86.995978584908,87.4317045853384,87.8665778926469,
88.3014512000977,88.7363245076919,89.1711978154302,89.6060711233134,90.0409444313423,
90.4758177395175,90.9106910478396,91.345564356309,91.7804376649263,92.2153109736917,
92.6501842826055,93.085057591668,93.5199309008791,93.9556569024059,94.3913829039327,
94.8262562134414,95.2611295230986,95.6960028329042,96.1308761428578,96.5657494529591,
97.0006227632077,97.4354960736028,97.870369384144,98.3052426948304,98.7401160056612,
99.1749893166354,99.6098626277522,100.04473593901,100.915335253024,101.351061255639,
101.785934567313,102.220807879124,102.655681191068,103.090554503145,103.525427815353,
104.395174440154,105.264921065453,105.699794378283,106.134667691232,106.569541004295,
107.004414317471,107.8750136343,108.745612951339,109.615359578629,110.485106206296,
111.354852834309,112.224599462639,113.094346091254,113.964092720119,114.834692038763,
115.705291357499,116.575037986826,117.444784616267,118.314531245777,119.184277875311,
120.054024504821,120.923771134261,121.794370453112,122.66496977189,123.534716400968,
124.404463029834,125.274209658448,126.143956286779,127.013702914792,127.883449542458,
128.754048859798,129.624648176939,130.494394803617,131.364141429857,132.233888055637,
133.103634680937,133.973381305737,134.843127930023,135.71372724472,136.584326559147,
137.019199870684,137.454073182083,137.888946493341,138.323819804458,139.193566426263,
140.063313047491,140.498186357887,140.933059668136,141.367932978237,141.802806288191,
142.237679597997,142.673405599673,143.109131601348,143.544004910857,143.978878220217,
144.413751529429,144.848624838491,145.283498147405,145.718371456171,146.153244764789,
146.588118073258,147.022991381581,147.457864689756,147.892737997785,148.327611305669,
148.762484613407,149.197357921002,149.633083921574,150.068809922147,150.503683229455,
150.938556536623,151.37342984365,151.808303150538,152.243176457288,152.678049763901,
153.112923070379,153.547796376722,153.982669682934,154.417542989014,154.852416294964,
155.287289600787,155.722162906483,156.157036212055,156.592762211626,157.028488211198,
157.463361516526,157.898234821735,158.333108126826,158.767981431803,159.202854736666,
159.637728041419,160.072601346062,160.507474650599,160.94234795503,161.37722125936,
161.812094563589,162.246967867721,162.681841171757,163.1167144757,163.552440474473,
163.988166473247,164.423039777011,164.85791308069,165.292786384286,165.727659687801,
166.162532991238,166.597406294601,167.03227959789,167.46715290111,167.902026204262,
168.33689950735,168.771772810376,169.206646113343,169.641519416254,170.076392719112,
170.512118717363,170.947844715614,171.382718018374,171.817591321089,172.252464623762,
172.687337926397,173.122211228996,173.557084531561,173.991957834097,174.426831136606,
174.86170443909,175.296577741554,175.731451044,176.16632434643,176.601197648848,
177.036070951258,177.471796949306,177.907522947355,178.342396249755,178.777269552155,
179.212142854558,179.647016156968,180.081889459386,180.516762761816,180.951636064262,
181.386509366726,181.82138266921,182.256255971719,182.691129274255,183.12600257682,
183.560875879419,183.995749182054,184.431475180237,184.867201178421,185.302074481136,
185.736947783896,186.171821086704,186.606694389561,187.041567692473,187.47644099544,
187.911314298466,188.346187601554,188.781060904706,189.215934207926,189.650807511215,
190.085680814577,190.520554118015,190.95542742153,191.391153420175,191.82687941882,
192.261752722499,192.696626026263,193.131499330116,193.566372634059,194.001245938095,
194.436119242227,194.870992546456,195.305865850785,195.740739155217,196.175612459754,
196.610485764397,197.045359069149,197.480232374013,197.915105678989,198.350831678382,
198.786557677775,199.221430982984,199.656304288312,200.091177593761,200.526050899333,
200.960924205029,201.395797510852,201.830670816802,202.265544122882,202.700417429093,
203.135290735437,203.570164041915,204.005037348528,204.439910655278,204.874783962166,
205.310509962526,205.746235962887,206.181109270054,206.615982577363,207.050855884814,
207.485729192409,207.920602500147,208.355475808031,208.79034911606,209.225222424235,
209.660095732558,210.094969041027,210.529842349645,210.96471565841,211.399588967324,
211.834462276387,212.27018827784,212.705914279292,213.140787588653,213.575660898161,
214.010534207819,214.880280827579,215.31515413768,215.750027447929,216.184900758324,
216.619774068866,217.054647379553,217.489520690384,218.359267312475,219.22986662628,
219.665592628826,220.100465940363,220.535339252038,220.970212563848,221.83995918787,
222.709705812416,223.579452437468,224.014325750179,224.44919906301,225.318945689022,
226.189545005688,227.060144322571,227.929890949664,228.799637577146,229.66938420499,
230.539130833166,231.408877461643,232.278624090388,233.149223408954,234.019822727623,
234.889569356878,235.759315986267,236.629062615749,237.498809245277,238.368555874806,
239.238302504287,240.108901823183,240.979501142017,241.849247771189,242.718994400167,
243.588741028911,244.458487657389,245.328234285565,246.197980913409,247.068580230891,
247.939179548182,248.80892617507,249.678672801532,250.548419427545,251.418166053087,
252.287912678139,253.157659302684,254.028258617581,254.898857932211,255.333731243885,
255.768604555423,256.203477866821,256.63835117808,257.508097800171,258.377844421689,
258.812717732231,259.247591042627,259.682464352876,260.117337662977,260.552210972931,
260.987936974682,261.858536286089,262.293409595598,262.728282904958,263.16315621417,
263.598029523233,264.032902832147,264.467776140913,264.902649449531,265.337522758001,
265.772396066323,266.207269374499,266.642142682528,267.077015990412,267.511889298151,
267.947615298795,268.383341299439,268.81821460689,269.2530879142,269.687961221367,
270.122834528394,270.557707835282,270.992581142032,271.427454448646,271.862327755124,
272.297201061468,272.732074367679,273.166947673759,273.60182097971,274.036694285533,
274.471567591229,274.907293590862,275.343019590495,275.777892895944,276.212766201272,
276.647639506481,277.082512811573,277.51738611655,277.952259421414,278.387132726166,
278.82200603081,279.256879335346,279.691752639779,280.126625944108,280.561499248338,
280.996372552469,281.431245856506,281.866971855324,282.302697854143,282.737571157996,
283.172444461761,283.60731776544,284.042191069036,284.477064372551,284.911937675989,
285.346810979351,285.781684282641,286.216557585861,286.651430889013,287.086304192101,
287.521177495128,287.956050798095,288.390924101007,288.826650099283,289.262376097559,
289.697249400366,290.132122703127,290.566996005842,291.001869308516,291.43674261115,
291.871615913749,292.306489216315,292.741362518851,293.17623582136,293.611109123845,
294.045982426308,294.480855728754,294.915729031185,295.350602333603,295.786328331655,
296.222054329707,296.65692763211,297.091800934511,297.526674236911,297.961547539314,
298.396420841724,298.831294144142,299.266167446573,299.701040749018,300.135914051482,
300.570787353967,301.005660656476,301.440533959012,301.875407261578,302.310280564177,
302.746006562341,303.181732560506,303.616605863179,304.051479165895,304.486352468655,
304.921225771462,305.35609907432,305.790972377232,306.225845680199,306.660718983226,
307.095592286314,307.530465589466,307.965338892686,308.400212195976,308.835085499338,
309.269958802776,309.705684801381,310.141410799985,310.576284103581,311.01115740726,
311.446030711025,311.880904014878,312.315777318821,312.750650622858,313.185523926989,
313.620397231219,314.055270535549,314.490143839981,314.925017144517,315.359890449161,
315.794763753913,316.229637058777,316.665363058112,317.101089057448,317.53596236254,
317.970835667749,318.405708973077,318.840582278526,319.275455584098,319.710328889795,
320.145202195618,320.580075501568,321.014948807648,321.44982211386,321.884695420204,
322.319568726682,322.754442033295,323.189315340045,323.625041340336,324.060767340628,
324.495640647655,324.930513954822,325.365387262131,325.800260569583,326.235133877177,
326.670007184916,327.1048804928,327.539753800829,327.974627109005,328.409500417327,
328.844373725797,329.279247034415,329.714120343181,330.148993652095,330.584719653474,
331.020445654852,331.455318964064,331.890192273424,332.325065582933,332.759938892591,
333.194812202397,333.629685512351,334.064558822453,334.499432132702,334.934305443098,
335.369178753639,335.804052064326,336.673798686132,337.108671997249,337.544397999725,
337.980124002201,338.4149973136,338.849870625137,339.284743936812,340.154490560568,
341.024237184854,341.459110497191,341.893983809655,342.328857122244,342.763730434955,
343.633477060735,344.504076377234,345.374675693955,346.244422320844,347.114168948136,
347.983915575803,348.853662203817,349.723408832148,350.593155460764,351.463754779246,
352.334354097839,353.204100727012,354.07384735634,354.943593985781,355.813340615292,
356.683087244827,357.552833874338,358.423433193272,359.294032512154,360.163779141409,
361.033525770489,361.903272399355,362.77301902797,363.642765656301,364.512512284316,
365.383111601936,366.253710919371,367.123457546465,367.993204173143,368.862950799383,
369.732697425164,370.602444050463,371.472190675265,372.342789990359,373.21338930519,
373.648262617,374.083135928675,374.952882551611,375.822629173987,376.257502484962,
376.692375795793,377.12724910648,377.562122417021,377.996995727417,378.431869037666,
378.866742347767,379.302468349591,379.738194351416,380.173067661222,380.607940970879,
381.042814280388,381.477687589749,381.91256089896,382.347434208023,382.782307516937,
383.217180825703,383.652054134321,384.086927442791,384.521800751113,384.956674059289,
385.391547367318,385.826420675202,386.262146675918,386.697872676635,387.13274598423,
387.567619291681,388.00249259899,388.437365906157,388.872239213185,389.307112520073,
389.741985826823,390.176859133436,390.611732439914,391.046605746258,391.48147905247,
391.91635235855,392.351225664501,392.786098970323,393.221824970019,393.657550969714,
394.092424275286,394.527297580735,394.962170886063,395.397044191272,395.831917496364,
396.266790801341,396.701664106204,397.136537410957,397.5714107156,398.006284020137,
398.441157324569,398.876030628899,399.310903933128,399.74577723726,400.181503236126,
400.617229234991,401.052102538934,401.486975842787,401.921849146551,402.356722450231,
402.791595753827,403.226469057342,403.66134236078,404.096215664142,404.531088967432,
404.965962270651,405.400835573804,405.835708876892,406.270582179918,406.705455482886,
407.141181481189,407.576907479491,408.01178078235,408.446654085157,408.881527387917,
409.316400690633,409.751273993306,410.186147295941,410.62102059854,411.055893901106,
411.490767203642,411.925640506151,412.360513808636,412.795387111099,413.230260413545,
413.665133715976,414.100859714032,414.536585712088,414.971459014498,415.406332316901,
415.841205619301,416.276078921702,416.710952224105,417.145825526515,417.580698828933,
418.015572131364,418.45044543381,418.885318736273,419.320192038758,419.755065341267,
420.189938643803,420.624811946369,421.060537944515,421.496263942662,421.931137245297,
422.36601054797,422.800883850686,423.235757153446,423.670630456253,424.105503759112,
424.540377062023,424.975250364991,425.410123668017,425.844996971105,426.279870274258,
426.714743577477,427.149616880767,427.584490184129,428.020216182695,428.455942181261,
428.890815484776,429.325688788373,429.760562092052,430.195435395816,430.630308699669,
431.065182003612,431.500055307649,431.93492861178,432.36980191601,432.80467522034,
433.239548524772,433.674421829309,434.109295133952,434.544168438705,434.979894437984,
435.415620437262,435.850493742239,436.285367047331,436.72024035254,437.155113657869,
437.589986963318,438.024860268889,438.459733574586,438.894606880409,439.32948018636,
439.76435349244,440.199226798651,440.634100104995,441.068973411473,441.503846718087,
441.939572718309,442.375298718531,442.810172025419,443.245045332447,443.679918639614,
444.114791946923,444.549665254374,444.984538561969,445.419411869708,445.854285177591,
446.289158485621,446.724031793796,447.158905102119,447.593778410589,448.028651719207,
448.463525027973,448.899251029277,449.334977030581,449.769850339644,450.639596958216,
451.074470267725,451.509343577383,451.944216887189,452.379090197143,452.813963507244,
453.248836817493,453.683710127889,454.118583438431,454.553456749117,454.988330059949,
455.423203370923,455.858929373329,456.294655375734,456.729528686993,457.164401998391,
457.599275309929,458.469021933414,458.90389524536,459.338768557437,459.773641869646,
460.208515181983,460.643388494447,461.078261807036,461.948008432578,462.818607748906,
463.689207065461,464.55895369214,465.428700319234,466.298446946716,467.16819357456,
468.037940202737,468.907686831215,469.778286149605,470.648885468116,471.518632097196,
472.388378726451,473.258125355841,474.127871985322,474.997618614851,475.86736524438,
476.737964563343,477.608563882265,478.478310511593,479.348057140765,480.217803769743,
481.087550398488,481.957297026966,482.827043655142,483.697642972895,484.568242290469,
485.43798891776,486.307735544649,487.177482171112,488.047228797125,488.916975422667,
489.78672204772,490.657321363009,491.09304736596,491.527920678038,492.397667301793,
493.267413925005,494.137160547663,494.57203385878,495.006907169755,495.441780480586,
495.876653791273,496.311527101814,496.74640041221,497.616999724357,498.052725726255,
498.487599036209,498.922472346015,499.357345655673,499.792218965182,500.227092274542,
500.661965583754,501.096838892816,501.531712201731,501.966585510497,502.401458819114,
502.836332127584,503.271205435907,503.706078744082,504.140952052112,504.576678052901,
505.01240405369,505.447277361429,505.882150669023,506.317023976474,506.751897283783,
507.186770590951,507.621643897978,508.056517204866,508.491390511616,508.92626381823,
509.361137124708,509.796010431052,510.230883737263,510.665757043344,511.100630349294,
511.536356349053,511.972082348811,512.406955654506,512.841828960076,513.276702265523,
513.711575570849,514.146448876056,514.581322181146,515.016195486121,515.451068790983,
515.885942095733,516.320815400375,516.75568870491,517.19056200934,517.625435313668,
518.060308617896,518.496034616807,518.931760615718,519.366633919752,519.801507223694,
520.236380527545,520.671253831307,521.106127134985,521.541000438579,521.975873742092,
522.410747045528,522.845620348888,523.280493652176,523.715366955394,524.150240258545,
524.585113561631,525.019986864656,525.455712862985,525.891438861313,526.326312164223,
526.761185467079,527.196058769885,527.630932072643,528.065805375356,528.500678678029,
528.935551980661,529.370425283258,529.805298585822,530.240171888356,530.675045190863,
531.109918493346,531.544791795808,531.979665098252,532.415391096312,532.851117094373,
533.285990396789,533.720863699197,534.155737001598,534.590610303997,535.025483606395,
535.460356908796,535.895230211204,536.330103513621,536.764976816049,537.199850118493,
537.634723420955,538.069596723438,538.504470025945,538.93934332848,539.375069326608,
539.810795324736,540.245668627333,540.680541929966,541.115415232637,541.550288535351,
541.985161838109,542.420035140915,542.854908443771,543.28978174668,543.724655049646,
544.15952835267,544.594401655757,545.029274958907,545.464148262125,545.899021565413,
546.334747563939,546.770473562465,547.205346865901,547.640220169415,548.075093473009,
548.509966776686,548.944840080449,549.3797133843,549.814586688241,550.249459992276,
550.684333296405,551.119206600633,551.554079904961,551.988953209391,552.423826513926,
552.858699818567,553.294425817789,553.73015181701,554.165025121872,554.599898426846,
555.034771731937,555.469645037144,555.90451834247,556.339391647917,556.774264953487,
557.209138259182,557.644011565003,558.078884870951,558.51375817703,558.948631483239,
559.383504789581,559.818378096058,560.254104096209,560.689830096361,561.12470340311,
561.559576709996,561.994450017021,562.429323324187,562.864196631494,563.299069938943,
563.733943246536,564.168816554273,564.603689862154,565.038563170182,565.473436478355,
565.908309786676,566.343183095144,566.77805640376,567.213782404988,567.649508406216,
568.084381715128,568.519255024189,568.954128333399,569.389001642757,569.823874952264,
570.258748261921,570.693621571725,571.128494881677,571.563368191777,572.433114812417,
572.867988122957,573.302861433642,573.737734744471,574.173460746804,574.609186749136,
575.044060060251,575.913806682904,576.783553306113,577.218426617922,577.653299929865,
578.08817324194,578.523046554147,579.392793178944,580.26253980424,581.13313912039,
581.568865123709,582.003738436771,582.87348506323,583.743231690115,584.612978317402,
585.482724945065,586.352471573076,587.222218201403,588.092817519691,588.963416838109,
589.833163467083,590.702910096251,591.572656725575,592.442403355013,593.31214998452,
594.181896614051,595.05249593303,595.92309525198,596.792841881366,597.662588510618,
598.532335139693,599.402081768556,600.271828397167,601.141575025495,602.012174343369,
602.882773661074,603.752520288553,604.622266915642,605.492013542317,606.361760168553,
607.23150679433,608.101253419626,608.971852735101,609.842452050322,610.71219867434,
611.581945297822,612.451691920754,612.886565232011,613.321438543126,613.756311854099,
614.191185164928,615.060931786153,615.931531098516,616.367257100486,616.802130410586,
617.237003720538,617.671877030342,618.106750339998,618.541623649505,618.976496958863,
619.411370268073,619.846243577134,620.281116886046,620.71599019481,621.150863503426,
621.585736811894,622.020610120214,622.455483428388,622.891209429248,623.326935430108,
623.761808737989,624.196682045726,624.631555353319,625.066428660769,625.501301968075,
625.936175275241,626.371048582266,626.805921889153,627.240795195901,627.675668502512,
628.110541808988,628.54541511533,628.98028842154,629.415161727618,629.850887727438,
630.286613727259,630.72148703308,631.156360338774,631.591233644344,632.026106949791,
632.460980255118,632.895853560325,633.330726865415,633.76560017039,634.200473475251,
634.635346780002,635.070220084644,635.505093389179,635.939966693609,636.374839997937,
636.810565996897,637.246291995857,637.681165299986,638.116038604021,638.550911907962,
638.985785211813,639.420658515576,639.855531819253,640.290405122847,640.725278426361,
641.160151729796,641.595025033157,642.029898336444,642.464771639662,642.899644942813,
643.334518245899,643.770244244257,644.205970242616,644.640843545581,645.075716848491,
645.510590151347,645.945463454153,646.380336756911,646.815210059625,647.250083362296,
647.684956664929,648.119829967526,648.55470327009,648.989576572624,649.424449875131,
649.859323177614,650.294196480076,650.729922478144,651.165648476212,651.600521778641,
652.035395081057,652.470268383465,652.905141685866,653.340014988265,653.774888290663,
654.209761593065,654.644634895472,655.079508197889,655.514381500318,655.949254802762,
656.384128105224,656.819001407706,657.253874710213,657.689600708326,658.12532670644,
658.560200009004,658.995073311601,659.429946614234,659.864819916905,660.299693219619,
660.734566522377,661.169439825183,661.604313128039,662.039186430948,662.474059733914,
662.908933036938,663.343806340025,663.778679643175,664.213552946393,664.649278944883,
665.085004943373,665.519878246733,665.954751550169,666.389624853683,666.824498157277,
667.259371460954,667.694244764717,668.129118068568,668.563991372509,668.998864676544,
669.433737980674,669.868611284901,670.303484589229,670.738357893659,671.173231198194,
671.608957197361,672.044683196528,672.479556501278,672.91442980614,673.349303111115,
673.784176416205,674.219049721412,674.653923026738,675.088796332185,675.523669637755,
675.95854294345,676.393416249271,676.82828955522,677.263162861298,677.698036167508,
678.13290947385,678.568635473934,679.004361474018,679.439234780629,679.874108087377,
680.308981394264,680.743854701289,681.178728008455,681.613601315762,682.048474623211,
682.483347930804,682.91822123854,683.353094546422,683.78796785445,684.222841162623,
684.657714470944,685.092587779412,685.528313780566,685.96403978172,686.398913090483,
686.833786399396,687.268659708457,687.703533017666,688.138406327025,688.573279636532,
689.008152946187,689.443026255992,689.877899565944,690.312772876043,690.74764618629,
691.182519496684,691.617392807224,692.052266117909,692.487992120169,692.92371812243,
693.358591433403,694.228338055774,694.663211367171,695.098084678707,695.532957990379,
695.967831302188,696.402704614131,696.837577926207,697.707324550749,698.577071175797,
699.011944488507,699.447670491767,699.883396495028,700.318269807975,701.188016434211,
702.057763060886,702.927509687976,703.797256315454,704.667002943295,705.536749571467,
706.407348889651,707.277948207973,708.147694836835,709.017441465911,709.887188095163,
710.756934724548,711.626681354026,712.496427983551,713.367027302543,714.237626621516,
715.107373250954,715.977119880277,716.846866509446,717.716613138419,718.586359767161,
719.456106395635,720.32670571363,721.197305031464,722.067051659126,722.936798286414,
723.806544913299,724.676291539758,725.546038165767,726.415784791305,727.286384106969,
728.156983422381,729.026730046663,729.896476670415,730.331349982088,730.766223293624,
731.201096605021,731.635969916278,732.505716538366,733.37546315988,733.81033647042,
734.246062472462,734.681788474505,735.116661784752,735.551535094852,735.986408404804,
736.421281714608,736.856155024264,737.291028333771,737.72590164313,738.160774952339,
738.5956482614,739.030521570312,739.465394879076,739.900268187692,740.33514149616,
740.77001480448,741.205740805414,741.641466806347,742.076340114374,742.511213422256,
742.946086729993,743.380960037585,743.815833345035,744.250706652341,744.685579959507,
745.120453266533,745.555326573419,745.990199880167,746.425073186778,746.859946493254,
747.294819799596,747.729693105806,748.165419105691,748.601145105576,749.036018411525,
749.470891717346,749.90576502304,750.34063832861,750.775511634057,751.210384939384,
751.645258244591,752.080131549682,752.515004854656,752.949878159518,753.384751464269,
753.81962476891,754.254498073445,754.689371377875,755.125097376885,755.560823375895,
755.995696680123,756.430569984253,756.865443288287,757.300316592228,757.735189896079,
758.170063199842,758.604936503519,759.039809807113,759.474683110627,759.909556414062,
760.344429717423,760.779303020711,761.214176323929,761.649049627079,762.084775625469,
762.520501623858,762.955374926883,763.390248229848,763.825121532758,764.259994835614,
764.694868138419,765.129741441178,765.564614743891,765.999488046563,766.434361349196,
766.869234651793,767.304107954357,767.738981256891,768.173854559398,768.608727861881,
769.044453859958,769.480179858035,769.915053160479,770.349926462907,770.784799765324,
771.219673067731,771.654546370133,772.089419672531,772.52429297493,772.959166277331,
773.394039579739,773.828912882155,774.263786184584,774.698659487028,775.13353278949,
775.568406091973,776.004132090072,776.439858088172,776.874731390706,777.30960469327,
777.744477995867,778.1793512985,778.614224601171,779.049097903885,779.483971206643,
779.918844509449,780.353717812305,780.788591115215,781.22346441818,781.658337721205,
782.093211024291,782.528084327442,782.963810325897,783.399536324352,783.834409627639,
784.269282931,784.704156234435,785.139029537949,785.573902841543,786.00877614522,
786.443649448983,786.878522752834,787.313396056775,787.74826936081,788.183142664939,
788.618015969167,789.052889273495,789.487762577925,789.923488577038,790.359214576152,
790.794087880793,791.228961185544,791.663834490406,792.098707795381,792.533581100471,
792.968454405678,793.403327711004,793.838201016451,794.273074322021,794.707947627716,
795.142820933537,795.577694239486,796.012567545564,796.447440851774,796.883166851791,
797.318892851808,797.753766158284,798.188639464895,798.623512771643,799.058386078529,
799.493259385555,799.92813269272,800.363006000027,800.797879307477,801.232752615069,
801.667625922806,802.102499230688,802.537372538715,802.972245846889,803.40711915521,
803.84284515629,804.27857115737,804.713444465985,805.148317774749,805.583191083662,
806.018064392723,806.452937701933,806.887811011291,807.322684320798,808.192430940258,
808.62730425021,809.06217756031,809.497050870557,809.931924180951,810.36679749149,
810.802523493679,811.238249495867,811.673122806697,812.542869428785,812.977742740041,
813.412616051438,813.847489362974,814.282362674646,814.717235986455,815.152109298398,
816.021855922681,816.891602547478,817.326475860065,817.762201863265,818.197927866466,
818.632801179295,819.502547805304,820.372294431763,821.242041058648,822.111787685935,
822.981534313598,823.851280941609,824.721880259681,825.5924795779,826.462226206642,
827.331972835616,828.201719464785,829.071466094109,829.941212723546,830.810959353053,
831.681558672047,832.552157991036,833.421904620514,834.2916512499,835.161397879151,
836.031144508226,836.900891137089,837.770637765701,838.641237083811,839.511836401767,
840.381583029608,841.251329657086,842.121076284176,842.990822910851,843.860569537087,
844.730316162863,845.600915478712,846.471514794314,847.341261418855,848.211008042874,
848.645881354683,849.080754666356,849.515627977891,849.950501289288,850.82024791166,
851.689994533462,852.124867844147,852.560593846263,852.996319848379,853.431193158772,
853.866066469019,854.300939779119,855.170686398875,855.605559708531,856.040433018038,
856.475306327397,856.910179636606,857.345052945667,857.77992625458,858.214799563344,
858.64967287196,859.084546180427,859.520272181434,859.95599818244,860.390871490614,
860.825744798641,861.260618106523,861.69549141426,862.130364721852,862.565238029302,
863.000111336609,863.434984643774,863.8698579508,864.304731257686,864.739604564434,
865.174477871045,865.609351177521,866.044224483863,866.479950483814,866.915676483765,
867.350549789843,867.785423095792,868.220296401613,868.655169707307,869.090043012877,
869.524916318325,869.959789623651,870.394662928858,870.829536233948,871.264409538923,
871.699282843785,872.134156148535,872.569029453177,873.003902757712,873.439628756773,
873.875354755834,874.310228060162,874.745101364389,875.179974668519,875.614847972553,
876.049721276495,876.484594580346,876.919467884108,877.354341187786,877.78921449138,
878.224087794893,878.658961098329,879.093834401689,879.528707704977,879.963581008195,
880.399307006616,880.835033005038,881.269906308124,881.704779611148,882.139652914114,
882.574526217024,883.00939951988,883.444272822685,883.879146125444,884.314019428157,
884.748892730829,885.183766033462,885.618639336059,886.053512638623,886.488385941157,
886.923259243664,887.358985241751,887.794711239839,888.2295845423,888.664457844744,
889.099331147173,889.534204449589,889.969077751997,890.403951054398,890.838824356797,
891.273697659195,891.708570961597,892.143444264004,892.578317566421,893.01319086885,
893.448064171293,893.882937473755,894.318663471843,894.75438946993,895.189262772437,
895.624136074971,896.059009377535,896.493882680132,896.928755982765,897.363629285437,
897.798502588151,898.233375890909,898.668249193715,899.103122496571,899.53799579948,
899.972869102446,900.40774240547,900.842615708556,901.278341706978,901.714067705399,
902.148941008617,902.583814311905,903.018687615265,903.453560918701,903.888434222214,
904.323307525808,904.758180829485,905.193054133248,905.627927437099,906.06280074104,
906.497674045075,906.932547349205,907.367420653433,907.80229395776,908.238019956821,
908.673745955883,909.108619260417,909.543492565059,909.978365869809,910.413239174671,
910.848112479646,911.282985784736,911.717859089943,912.152732395269,912.587605700716,
913.022479006287,913.457352311981,913.892225617802,914.327098923751,914.761972229829,
915.19769822978,915.633424229731,916.068297536072,916.503170842548,916.93804414916,
917.372917455908,917.807790762794,918.24266406982,918.677537376985,919.112410684292,
919.547283991742,919.982157299334,920.417030607071,920.851903914953,921.28677722298,
921.721650531154,922.15737653216,922.593102533167,923.027975841635,923.46284915025,
923.897722459014,924.332595767926,924.767469076987,925.202342386197,925.637215695556,
926.072089005063,926.506962314719,926.941835624523,927.376708934475,927.811582244575,
928.246455554822,928.681328865215,929.117054867331,929.987654180132,930.422527490961,
930.857400801934,931.292274113049,931.727147424306,932.162020735703,932.596894047238,
933.46664067072,934.336387294739,934.771260606945,935.20613391928,935.641007231742,
936.076733234882,936.94733255073,937.817079176507,938.686825802743,939.556572429418,
940.426319056508,941.296065683986,942.165812311827,943.036411629783,943.907010947893,
944.776757576505,945.646504205367,946.516250834443,947.385997463694,948.25574409308,
949.125490722558,949.996090041546,950.86668936054,951.736435990048,952.606182619485,
953.475929248809,954.345675877978,955.215422506951,956.085169135693,956.955768453912,
957.826367771985,958.696114399995,959.565861027658,960.435607654946,961.305354281831,
962.175100908289,963.044847534298,963.915446850328,964.786046166116,965.655792790913,
966.525539415195,966.960412727138,967.395286038947,968.265032662155,969.134779284809,
969.569652595924,970.004525906897,970.439399217726,970.875125219914,971.310851222103,
971.745724532643,972.615471153283,973.485217773335,973.920091083139,974.354964392795,
974.789837702302,975.22471101166,975.65958432087,976.094457629931,976.529330938844,
976.964204247608,977.399077556223,977.834803557303,978.270529558383,978.705402866704,
979.140276174877,979.575149482905,980.010022790786,980.444896098523,980.879769406116,
981.314642713565,981.749516020872,982.184389328038,982.619262635063,983.05413594195,
983.489009248698,983.923882555309,984.358755861785,984.794481861802,985.230207861819,
985.665081168029,986.099954474107,986.534827780056,986.969701085877,987.404574391571,
987.839447697141,988.274321002589,988.709194307915,989.144067613122,989.578940918212,
990.013814223187,990.448687528048,990.883560832799,991.31843413744,991.754160136554,
992.189886135667,992.624759440097,993.059632744425,993.494506048653,993.929379352783,
994.364252656817,994.799125960758,995.233999264609,995.668872568372,996.103745872049,
996.538619175643,996.973492479157,997.408365782593,997.843239085953,998.278112389241,
998.713838387696,999.149564386151,999.584437689301,1000.01931099239,1000.45418429541,
1000.88905759838,1001.32393090129,1001.75880420414,1002.19367750695,1002.62855080971,
1003.06342411242,1003.49829741509,1003.93317071773,1004.36804402032,1004.80291732289,
1005.23779062542,1005.67351662352,1006.10924262162,1006.5441159241,1006.97898922656,
1007.41386252901,1007.84873583144,1008.28360913385,1008.71848243626,1009.15335573866,
1009.58822904106,1010.02310234346,1010.45797564586,1010.89284894827,1011.32772225069,
1011.76259555311,1012.19746885556,1012.63319485364,1013.06892085171,1013.5037941542,
1013.9386674567,1014.37354075924,1014.8084140618,1015.2432873644,1015.67816066703,
1016.1130339697,1016.54790727242,1016.98278057517,1017.41765387798,1017.85252718084,
1018.28740048375,1018.72227378671,1019.15714708974,1019.59287308813,1020.02859908651,
1020.46347238967,1020.89834569288,1021.33321899617,1021.76809229953,1022.20296560297,
1022.63783890648,1023.07271221007,1023.50758551375,1023.94245881752,1024.37733212137,
1024.81220542531,1025.24707872935,1025.68195203348,1026.11682533771,1026.55255133672,
1026.98827733573,1027.42315064016,1027.8580239447,1028.29289724934,1028.72777055409,
1029.16264385896,1029.59751716393,1030.03239046902,1030.46726377423,1030.90213707956,
1031.33701038501,1031.77188369058,1032.20675699628,1032.6416303021,1033.07650360805,
1033.51222960793,1033.94795560782,1034.38282891403,1034.81770222038,1035.25257552685,
1035.68744883347,1036.12232214022,1036.5571954471,1036.99206875413,1037.4269420613,
1037.86181536861,1038.29668867606,1038.73156198365,1039.16643529139,1039.60130859927,
1040.0361819073,1040.47190790824,1040.90763390917,1041.34250721749,1041.77738052596,
1042.21225383458,1042.64712714334,1043.08200045226,1043.95174707053,1044.38662037989,
1044.8214936894,1045.25636699906,1045.69124030886,1046.12611361882,1046.56098692892,
1046.99586023917,1047.43158624121,1047.86731224325,1048.3021855538,1048.73705886448,
1049.17193217531,1049.60680548629,1050.0416787974,1050.47655210866,1050.91142542006,
1051.78117204327,1052.21604535508,1052.65091866703,1053.0857919791,1053.52066529131,
1053.95553860365,1054.39126460673,1055.26186392239,1056.13161054793,1057.00135717395,
1057.43623048712,1057.87110380041,1058.7408504273,1059.61059705459,1060.48034368225,
1061.35094300009,1062.22154231809,1063.09128894656,1063.96103557531,1064.83078220429,
1065.70052883346,1066.57027546278,1067.44002209222,1068.3106214112,1069.18122073019,
1070.05096735972,1070.9207139892,1071.79046061859,1072.66020724785,1073.52995387693,
1074.39970050579,1075.27029982411,1076.1408991423,1077.01064577048,1077.88039239832,
1078.7501390258,1079.61988565289,1080.48963227957,1081.35937890581,1082.22997822202,
1083.100577538,1083.97032416305,1084.84007078759,1085.70981741161,1086.5795640351,
1087.44931065803,1087.88418396929,1088.31905728041,1088.75393059138,1089.18965659365,
1089.62538259591,1090.06025590659,1090.93000252753,1091.36487583778,1091.79974914788,
1092.23462245783,1092.66949576764,1093.1043690773,1093.5392423868,1093.97411569616,
1094.40898900538,1094.84386231444,1095.27873562335,1095.71360893212,1096.14933493327,
1096.58506093443,1097.0199342429,1097.45480755122,1097.88968085939,1098.32455416742,
1098.75942747531,1099.19430078305,1099.62917409064,1100.06404739809,1100.4989207054,
1100.93379401257,1101.36866731959,1101.80354062648,1102.23841393323,1102.67328723984,
1103.10901323993,1103.54473924001,1103.97961254636,1104.41448585257,1104.84935915865,
1105.2842324646,1105.71910577042,1106.15397907612,1106.58885238169,1107.02372568714,
1107.45859899246,1107.89347229767,1108.32834560276,1108.76321890774,1109.1980922126,
1109.63296551736,1110.06869151652,1110.50441751569,1110.93929082023,1111.37416412466,
1111.80903742899,1112.24391073322,1112.67878403735,1113.11365734139,1113.54853064533,
1113.98340394918,1114.41827725295,1114.85315055662,1115.28802386022,1115.72289716374,
1116.15777046717,1116.59264377053,1117.02836976903,1117.46409576752,1117.89896907074,
1118.33384237389,1118.76871567698,1119.20358898,1119.63846228297,1120.07333558588,
1120.50820888874,1120.94308219154,1121.3779554943,1121.81282879702,1122.24770209969,
1122.68257540233,1123.11744870492,1123.55232200749,1123.98804800561,1124.42377400372,
1124.85864730623,1125.29352060871,1125.72839391118,1126.16326721362,1126.59814051605,
1127.03301381847,1127.46788712088,1127.90276042328,1128.33763372568,1128.77250702808,
1129.20738033048,1129.64225363289,1130.07712693531,1130.51200023774,1130.94772623581,
1131.38345223388,1131.81832553634,1132.25319883883,1132.68807214134,1133.12294544387,
1133.55781874644,1133.99269204904,1134.42756535167,1134.86243865434,1135.29731195706,
1135.73218525982,1136.16705856263,1136.60193186548,1137.03680516839,1137.47167847136,
1137.90740446972,1138.34313046808,1138.77800377117,1139.21287707432,1139.64775037754,
1140.08262368083,1140.51749698419,1140.95237028763,1141.38724359114,1141.82211689474,
1142.25699019842,1142.69186350218,1143.12673680603,1143.56161010998,1143.99648341401,
1144.43135671814,1144.86708271711,1145.30280871607,1145.7376820204,1146.17255532483,
1146.60742862936,1147.04230193401,1147.47717523876,1147.91204854362,1148.3469218486,
1148.78179515369,1149.2166684589,1149.65154176423,1150.08641506968,1150.52128837525,
1150.95616168094,1151.39103498677,1151.82676098659,1152.26248698641,1152.69736029249,
1153.1322335987,1153.56710690504,1154.00198021152,1154.43685351813,1154.87172682488,
1155.30660013177,1155.7414734388,1156.17634674597,1156.61122005327,1157.04609336073,
1157.48096666832,1157.91583997606,1158.35071328394,1158.7864392848,1159.22216528566,
1159.65703859384,1160.09191190216,1160.52678521063,1160.96165851925,1161.39653182801,
1161.83140513693,1162.26627844599,1162.7011517552,1163.13602506456,1163.57089837407,
1164.00577168373,1164.44064499353,1164.87551830349,1165.74611761556,1166.18184361753,
1166.61671692792,1167.05159023846,1167.48646354915,1167.92133685998,1168.35621017096,
1169.22595679333,1170.09570341627,1170.53057672794,1170.96545003975,1171.4003233517,
1171.83519666377,1172.27006997598,1172.705795979,1173.57639529447,1174.44614191977,
1174.8810152326,1175.31588854555,1176.18563517179,1177.05538179847,1177.92512842556,
1178.79487505304,1179.66547437075,1180.53607368863,1181.40582031696,1182.27556694557,
1183.14531357444,1184.01506020352,1184.88480683277,1185.75455346216,1186.62515278112,
1187.4957521001,1188.36549872963,1189.23524535914,1190.10499198858,1190.97473861791,
1191.84448524708,1192.71423187606,1193.58483119448,1194.45543051277,1195.3251771411,
1196.19492376911,1197.06467039678,1197.93441702407,1198.80416365096,1199.67391027742,
1200.5445095938,1201.41510890996,1202.28485553525,1203.15460216005,1204.02434878434,
1204.89409540809,1205.76384203131,1206.1987153427,1206.63358865396,1207.06846196508,
1207.50418796741,1208.37478728058,1209.2445339018,1209.6794072122,1210.11428052245,
1210.54915383255,1210.9840271425,1211.41890045231,1211.85377376197,1212.28864707147,
1212.72352038083,1213.15839369005,1213.59326699911,1214.02814030802,1214.46386630925,
1214.89959231048,1215.3344656191,1215.76933892757,1216.20421223589,1216.63908554406,
1217.07395885209,1217.50883215998,1217.94370546771,1218.37857877531,1218.81345208276,
1219.24832539007,1219.68319869724,1220.11807200426,1220.55294531115,1220.9878186179,
1221.42354461805,1221.85927061821,1222.29414392468,1222.72901723103,1223.16389053724,
1223.59876384332,1224.03363714927,1224.46851045509,1224.90338376079,1225.33825706636,
1225.77313037181,1226.20800367713,1226.64287698234,1227.07775028743,1227.51262359241,
1227.94749689727,1228.3832228965,1228.81894889572,1229.25382220036,1229.6886955049,
1230.12356880933,1230.55844211366,1230.99331541789,1231.42818872202,1231.86306202606,
1232.29793533,1232.73280863385,1233.16768193762,1233.60255524129,1234.03742854489,
1234.4723018484,1234.90717515184,1235.34290115037,1235.7786271489,1236.21350045219,
1236.64837375541,1237.08324705856,1237.51812036165,1237.95299366467,1238.38786696764,
1238.82274027055,1239.25761357341,1239.69248687621,1240.12736017897,1240.56223348169,
1240.99710678436,1241.431980087,1241.8668533896,1242.30257938773,1242.73830538585,
1243.17317868839,1243.6080519909,1244.04292529338,1244.47779859585,1244.91267189829,
1245.34754520072,1245.78241850314,1246.21729180555,1246.65216510795,1247.08703841035,
1247.52191171275,1247.95678501515,1248.39165831756,1248.82653161998,1249.26225761804,
1249.69798361611,1250.13285691855,1250.56773022101,1251.0026035235,1251.43747682601,
1251.87235012854,1252.30722343111,1252.74209673371,1253.17697003634,1253.61184333901,
1254.04671664173,1254.48158994449,1254.9164632473,1255.35133655015,1255.78620985306,
1256.22193585139,1256.65766184973,1257.09253515275,1257.52740845584,1257.96228175899,
1258.39715506221,1258.8320283655,1259.26690166886,1259.7017749723,1260.13664827581,
1260.57152157941,1261.00639488309,1261.44126818685,1261.8761414907,1262.31101479465,
1262.74588809868,1263.1816140976,1263.61734009651,1264.05221340074,1264.48708670507,
1264.9219600095,1265.35683331403,1265.79170661868,1266.22657992343,1266.66145322829,
1267.09632653327,1267.53119983836,1267.96607314357,1268.4009464489,1268.83581975434,
1269.27069305992,1269.70556636561,1270.14129236537,1270.57701836513,1271.01189167108,
1271.44676497716,1271.88163828337,1272.31651158971,1272.75138489619,1273.1862582028,
1273.62113150955,1274.05600481644,1274.49087812347,1274.92575143063,1275.36062473794,
1275.79549804539,1276.23037135299,1276.66524466073,1277.10097066151,1277.5366966623,
1277.97156997033,1278.40644327851,1278.84131658683,1279.2761898953,1279.71106320392,
1280.14593651268,1280.5808098216,1281.01568313066,1281.45055643987,1281.88542974923,
1282.32030305874,1282.75517636839,1283.1900496782,1283.62492298815,1284.06064899005,
1284.49637499195,1284.9312483022,1285.36612161259,1285.80099492313,1286.23586823382,
1286.67074154465,1287.54048816674,1287.975361478,1288.4102347894,1288.84510810093,
1289.27998141261,1289.71485472442,1290.14972803636,1291.02032735139,1291.89092666668,
1292.32579997914,1292.76067329173,1293.19554660444,1293.63041991727,1294.50016654328,
1295.36991316974,1296.23965979663,1297.10940642392,1297.9800057415,1298.85060505925,
1299.72035168742,1300.5900983159,1301.45984494464,1302.32959157362,1303.19933820279,
1304.06908483212,1304.93968415104,1305.81028347,1306.68003009953,1307.54977672906,
1308.41952335854,1309.28926998793,1310.15901661718,1311.02876324626,1311.89936256477,
1312.76996188316,1313.63970851164,1314.50945513981,1315.37920176765,1316.24894839514,
1317.11869502223,1317.98844164891,1318.85904096546,1319.72964028179,1320.59938690733,
1321.46913353238,1322.33888015692,1323.20862678095,1323.64350009276,1324.07837340443,
1324.51324671597,1324.94812002737,1325.81871934103,1326.68931865441,1327.12419196524,
1327.55906527593,1327.99393858647,1328.42881189686,1328.86368520711,1329.29855851721,
1329.73343182716,1330.16830513697,1330.60317844663,1331.03805175614,1331.4729250655,
1331.90779837471,1332.34267168377,1332.77839768507,1333.21412368638,1333.64899699514,
1334.08387030376,1334.51874361223,1334.95361692055,1335.38849022873,1335.82336353676,
1336.25823684464,1336.69311015238,1337.12798345997,1337.56285676742,1337.99773007473,
1338.4326033819,1338.86747668892,1339.30234999581,1339.73807599603,1340.17380199625,
1340.60867530287,1341.04354860934,1341.47842191569,1341.9132952219,1342.34816852798,
1342.78304183393,1343.21791513975,1343.65278844545,1344.08766175102,1344.52253505647,
1344.95740836179,1345.392281667,1345.82715497209,1346.26202827707,1346.69775427635,
1347.13348027563,1347.56835358038,1348.00322688502,1348.43810018956,1348.87297349399,
1349.30784679832,1349.74272010255,1350.17759340668,1350.61246671072,1351.04734001466,
1351.48221331851,1351.91708662228,1352.35195992595,1352.78683322955,1353.22170653306,
1353.65743253163,1354.09315853019,1354.52803183356,1354.96290513685,1355.39777844007,
1355.83265174322,1356.26752504631,1356.70239834933,1357.1372716523,1357.57214495521,
1358.00701825807,1358.44189156087,1358.87676486363,1359.31163816635,1359.74651146902,
1360.18138477166,1360.6171107698,1361.05283676795,1361.48771007051,1361.92258337305,
1362.35745667556,1362.79232997804,1363.2272032805,1363.66207658295,1364.09694988538,
1364.5318231878,1364.96669649021,1365.40156979261,1365.83644309501,1366.27131639741,
1366.70618969981,1367.14106300222,1367.57678900028,1368.01251499834,1368.44738830077,
1368.88226160321,1369.31713490567,1369.75200820816,1370.18688151067,1370.6217548132,
1371.05662811577,1371.49150141837,1371.926374721,1372.36124802367,1372.79612132639,
1373.23099462915,1373.66586793196,1374.10074123481,1374.53646723311,1374.97219323142,
1375.40706653438,1375.84193983741,1376.2768131405,1376.71168644365,1377.14655974687,
1377.58143305016,1378.01630635352,1378.45117965696,1378.88605296047,1379.32092626407,
1379.75579956775,1380.19067287151,1380.62554617536,1381.06041947931,1381.49614547817,
1381.93187147704,1382.36674478117,1382.8016180854,1383.23649138973,1383.67136469416,
1384.10623799869,1384.54111130334,1384.97598460809,1385.41085791295,1385.84573121793,
1386.28060452302,1386.71547782823,1387.15035113356,1387.585224439,1388.02009774458,
1388.45582374427,1388.89154974397,1389.32642304979,1389.76129635574,1390.19616966182,
1390.63104296803,1391.06591627437,1391.50078958085,1391.93566288746,1392.37053619421,
1392.8054095011,1393.24028280813,1393.6751561153,1394.1100294226,1394.54490273005,
1394.97977603765,1395.41550203836,1395.85122803908,1396.28610134696,1396.72097465499,
1397.15584796317,1397.59072127149,1398.02559457996,1398.46046788858,1398.89534119734,
1399.33021450626,1399.76508781532,1400.19996112453,1400.63483443389,1401.50458105306,
1401.93945436286,1402.37518036469,1402.81090636651,1403.24577967661,1403.68065298686,
1404.11552629725,1404.5503996078,1404.98527291848,1405.85501954029,1406.2898928514,
1406.72476616266,1407.15963947406,1407.5945127856,1408.02938609727,1408.46425940908,
1409.33485872391,1410.205458039,1410.64033135134,1411.07520466381,1411.51007797639,
1411.9449512891,1412.81469791488,1413.68444454112,1414.5541911678,1415.42393779489,
1416.29453711233,1417.16513642995,1418.03488305796,1418.90462968629,1419.77437631491,
1420.64412294377,1421.51386957285,1422.38361620211,1423.25421552099,1424.12481483992,
1424.99456146943,1425.86430809896,1426.73405472847,1427.60380135791,1428.47354798724,
1429.34329461641,1430.21389393501,1431.08449325349,1431.9542398821,1432.82398651043,
1433.69373313844,1434.56347976611,1435.4332263934,1436.30297302029,1437.17357233701,
1438.04417165351,1438.91391827929,1439.78366490459,1440.65341152939,1441.52315815367,
1441.95803146562,1442.39290477743,1442.8277780891,1443.26265140064,1444.13325071451,
1445.00385002811,1445.43872333908,1445.87359664991,1446.3084699606,1446.74334327114,
1447.17821658153,1447.61308989178,1448.48283651184,1448.91770982164,1449.3525831313,
1449.78745644081,1450.22232975017,1450.65720305938,1451.09292906076,1451.52865506214,
1451.96352837105,1452.39840167982,1452.83327498843,1453.2681482969,1453.70302160522,
1454.1378949134,1454.57276822143,1455.00764152931,1455.44251483705,1455.87738814464,
1456.31226145209,1456.7471347594,1457.18200806657,1457.6168813736,1458.05260737389,
1458.48833337418,1458.92320668093,1459.35807998754,1459.79295329402,1460.22782660036,
1460.66269990657,1461.09757321265,1461.5324465186,1461.96731982443,1462.40219313012,
1462.83706643569,1463.27193974114,1463.70681304647,1464.14168635168,1464.57655965677,
1465.0122856561,1465.44801165544,1465.8828849603,1466.31775826505,1466.7526315697,
1467.18750487423,1467.62237817866,1468.05725148299,1468.49212478722,1468.92699809135,
1469.36187139539,1469.79674469933,1470.23161800319,1470.66649130695,1471.10136461063,
1471.53623791422,1471.97196391283,1472.40768991143,1472.84256321487,1473.27743651823,
1473.71230982152,1474.14718312474,1474.58205642789,1475.01692973098,1475.451803034,
1475.88667633697,1476.32154963988,1476.75642294274,1477.19129624555,1477.62616954831,
1478.06104285102,1478.4959161537,1478.93164215186,1479.36736815002,1479.80224145262,
1480.23711475519,1480.67198805772,1481.10686136023,1481.54173466272,1481.97660796518,
1482.41148126762,1482.84635457005,1483.28122787247,1483.71610117488,1484.15097447728,
1484.58584777968,1485.02072108208,1485.45559438449,1485.89132038254,1486.32704638059,
1486.76191968301,1487.19679298544,1487.63166628788,1488.06653959035,1488.50141289283,
1488.93628619534,1489.37115949787,1489.80603280044,1490.24090610304,1490.67577940567,
1491.11065270835,1491.54552601106,1491.98039931382,1492.41527261663,1492.8509986149,
1493.28672461318,1493.72159791609,1494.15647121906,1494.59134452208,1495.02621782517,
1495.46109112832,1495.89596443154,1496.33083773483,1496.76571103819,1497.20058434163,
1497.63545764515,1498.07033094874,1498.50520425242,1498.94007755618,1499.37495086004,
1499.81067685885,1500.24640285767,1500.68127616171,1501.11614946584,1501.55102277007,
1501.9858960744,1502.42076937883,1502.85564268337,1503.29051598801,1503.72538929276,
1504.16026259762,1504.5951359026,1505.03000920769,1505.4648825129,1505.89975581823,
1506.33462912368,1506.77035512331,1507.20608112294,1507.64095442864,1508.07582773446,
1508.51070104041,1508.94557434649,1509.3804476527,1509.81532095904,1510.25019426552,
1510.68506757213,1511.11994087888,1511.55481418577,1511.9896874928,1512.42456079996,
1512.85943410727,1513.29430741472,1513.73003341537,1514.16575941601,1514.60063272375,
1515.03550603163,1515.47037933966,1515.90525264784,1516.34012595616,1516.77499926463,
1517.20987257325,1517.64474588201,1518.07961919093,1518.51449249999,1518.9493658092,
1519.38423911856,1519.81911242807,1520.25398573772,1520.68971173947,1521.12543774122,
1521.56031105118,1521.99518436128,1522.43005767153,1523.29980429246,1523.73467760315,
1524.16955091398,1524.60442422495,1525.03929753607,1525.47417084733,1525.90904415873,
1526.77879078194,1527.64939009657,1528.08511609939,1528.51998941146,1528.95486272367,
1529.38973603601,1530.25948266106,1531.1292292866,1531.99897591261,1532.86872253907,
1533.73846916596,1534.60906848325,1535.47966780073,1536.34941442858,1537.21916105675,
1538.08890768523,1538.95865431398,1539.82840094295,1540.69814757212,1541.56874689096,
1542.43934620985,1543.30909283933,1544.17883946886,1545.04858609839,1545.91833272787,
1546.78807935726,1547.65782598651,1548.52842530518,1549.39902462375,1550.26877125249,
1551.13851788097,1552.00826450914,1552.87801113699,1553.74775776447,1554.61750439156,
1555.48810370844,1556.35870302511,1557.22844965112,1558.09819627666,1558.96794290171,
1559.83768952626,1560.27256283834,1560.70743615028,1561.57718277377,1562.44778208785,
1563.31838140165,1563.75325471277,1564.18812802374,1564.62300133457,1565.05787464526,
1565.9276212662,1566.79736788655,1567.2322411965,1567.66711450631,1568.10198781596,
1568.53686112547,1568.97173443483,1569.40746043628,1569.84318643774,1570.2780597468,
1570.71293305571,1571.14780636448,1571.5826796731,1572.01755298157,1572.45242628989,
1572.88729959806,1573.32217290609,1573.75704621397,1574.19191952171,1574.62679282931,
1575.06166613676,1575.49653944407,1575.93141275123,1576.36713875159,1576.80286475195,
1577.23773805884,1577.67261136559,1578.1074846722,1578.54235797868,1578.97723128502,
1579.41210459124,1579.84697789732,1580.28185120327,1580.71672450909,1581.15159781478,
1581.58647112036,1582.0213444258,1582.45621773113,1582.89109103634,1583.32681703573,
1583.76254303513,1584.1974163401,1584.63228964497,1585.06716294972,1585.50203625436,
1585.9369095589,1586.37178286333,1586.80665616766,1587.24152947189,1587.67640277602,
1588.11127608005,1588.546149384,1588.98102268785,1589.41589599161,1589.85076929529,
1590.28649529394,1590.72222129258,1591.1570945961,1591.59196789953,1592.0268412029,
1592.46171450619,1592.8965878094,1593.33146111256,1593.76633441564,1594.20120771867,
1594.63608102164,1595.07095432455,1595.50582762741,1595.94070093021,1596.37557423297,
1596.81044753569,1597.24617353387,1597.68189953206,1598.11677283469,1598.55164613729,
1598.98651943985,1599.42139274239,1599.8562660449,1600.29113934738,1600.72601264985,
1601.16088595229,1601.59575925472,1602.03063255714,1602.46550585955,1602.90037916195,
1603.33525246435,1603.77012576675,1604.2058517648,1604.64157776285,1605.07645106526,
1605.51132436768,1605.94619767011,1606.38107097255,1606.81594427502,1607.2508175775,
1607.68569088001,1608.12056418254,1608.55543748511,1608.99031078771,1609.42518409034,
1609.86005739302,1610.29493069573,1610.72980399849,1611.16552999674,1611.60125599499,
1612.03612929785,1612.47100260076,1612.90587590373,1613.34074920675,1613.77562250984,
1614.21049581299,1614.64536911621,1615.0802424195,1615.51511572286,1615.9499890263,
1616.38486232981,1616.81973563341,1617.25460893709,1617.68948224085,1618.12520823963,
1618.5609342384,1618.99580754234,1619.43068084638,1619.86555415051,1620.30042745474,
1620.73530075907,1621.1701740635,1621.60504736804,1622.03992067268,1622.47479397743,
1622.90966728229,1623.34454058727,1623.77941389236,1624.21428719757,1624.6491605029,
1625.08488650247,1625.52061250204,1625.95548580761,1626.39035911331,1626.82523241913,
1627.26010572508,1627.69497903116,1628.12985233737,1628.56472564372,1628.99959895019,
1629.43447225681,1629.86934556356,1630.30421887044,1630.73909217747,1631.17396548464,
1631.60883879195,1632.04456479252,1632.48029079309,1632.91516410068,1633.35003740842,
1633.78491071631,1634.21978402433,1634.65465733251,1635.08953064083,1635.5244039493,
1635.95927725792,1636.39415056668,1636.8290238756,1637.26389718466,1637.69877049387,
1638.13364380323,1638.56851711274,1639.00424311442,1639.43996911609,1639.8748424259,
1640.30971573585,1640.74458904595,1641.6143356666,1642.04920897714,1642.48408228782,
1642.91895559865,1643.35382890963,1643.78870222074,1644.223575532,1645.09332215494,
1645.52819546661,1645.96392146936,1646.39964747212,1646.83452078406,1647.26939409614,
1647.70426740834,1648.57401403314,1649.44376065844,1650.31350728422,1650.74838059729,
1651.18325391046,1652.05300053714,1652.92359985428,1653.79419917162,1654.66394579929,
1655.5336924273,1656.40343905563,1657.27318568424,1658.14293231311,1659.01267894219,
1659.88327826096,1660.75387757982,1661.62362420926,1662.49337083877,1663.3631174683,
1664.23286409781,1665.10261072725,1665.97235735658,1666.84295667531,1667.71355599396,
1668.58330262282,1669.45304925143,1670.32279587976,1671.19254250778,1672.06228913544,
1672.93203576273,1673.80263507977,1674.6732343966,1675.54298102284,1676.41272764862,
1677.28247427392,1678.15222089872,1679.021967523,1679.89171414676,1680.76231346105,
1681.19803946366,1681.63291277506,1682.06778608632,1682.50265939743,1682.93753270841,
1683.37240601924,1684.24215264047,1684.67702595086,1685.11189926111,1685.54677257121,
1685.98164588116,1686.41651919097,1686.85139250063,1687.28626581014,1687.72199181166,
1688.15771781319,1688.5925911224,1689.02746443146,1689.46233774038,1689.89721104914,
1690.33208435776,1690.76695766623,1691.20183097455,1691.63670428272,1692.07157759075,
1692.50645089864,1692.94132420637,1693.37619751397,1693.81107082142,1694.24594412873,
1694.68167012916,1695.11739612959,1695.55226943662,1695.9871427435,1696.42201605025,
1696.85688935687,1697.29176266334,1697.72663596969,1698.1615092759,1698.59638258198,
1699.03125588793,1699.46612919375,1699.90100249945,1700.33587580502,1700.77074911047,
1701.20562241579,1701.64134841525,1702.0770744147,1702.51194771979,1702.94682102476,
1703.38169432963,1703.81656763438,1704.25144093902,1704.68631424356,1705.12118754799,
1705.55606085232,1705.99093415655,1706.42580746068,1706.86068076471,1707.29555406866,
1707.73042737251,1708.16530067627,1708.60102667496,1709.03675267365,1709.47162597724,
1709.90649928076,1710.34137258419,1710.77624588756,1711.21111919085,1711.64599249406,
1712.08086579722,1712.5157391003,1712.95061240333,1713.3854857063,1713.82035900921,
1714.25523231207,1714.69010561487,1715.12497891763,1715.56070491584,1715.99643091404,
1716.43130421671,1716.86617751935,1717.30105082195,1717.73592412451,1718.17079742705,
1718.60567072956,1719.04054403204,1719.4754173345,1719.91029063695,1720.34516393938,
1720.7800372418,1721.21491054421,1721.64978384661,1722.08465714901,1722.52038314706,
1722.9561091451,1723.39098244751,1723.82585574992,1724.26072905233,1724.69560235476,
1725.13047565721,1725.56534895967,1726.00022226216,1726.43509556467,1726.8699688672,
1727.30484216977,1727.73971547236,1728.174588775,1728.60946207767,1729.04433538039,
1729.48006137861,1729.91578737684,1730.35066067965,1730.78553398251,1731.22040728542,
1731.65528058838,1732.09015389141,1732.5250271945,1732.95990049765,1733.39477380087,
1733.82964710416,1734.26452040752,1734.69939371096,1735.13426701447,1735.56914031807,
1736.00401362175,1736.43973962048,1736.8754656192,1737.31033892306,1737.745212227,
1738.18008553104,1738.61495883517,1739.0498321394,1739.48470544373,1739.91957874816,
1740.35445205269,1740.78932535734,1741.22419866209,1741.65907196695,1742.09394527193,
1742.52881857702,1742.96369188223,1743.39941788174,1743.83514388125,1744.2700171867,
1744.70489049227,1745.13976379797,1745.57463710379,1746.00951040974,1746.44438371582,
1746.87925702203,1747.31413032837,1747.74900363485,1748.18387694146,1748.61875024821,
1749.0536235551,1749.48849686213,1749.92337016929,1750.3590961698,1750.7948221703,
1751.22969547775,1751.66456878534,1752.09944209308,1752.53431540096,1752.96918870899,
1753.40406201717,1753.83893532549,1754.27380863396,1754.70868194258,1755.14355525134,
1755.57842856026,1756.01330186932,1756.44817517853,1756.88304848789,1757.31877448949,
1757.75450049109,1758.18937380075,1759.05912042051,1759.49399373061,1759.92886704086,
1760.36374035125,1760.79861366179,1761.23348697248,1761.66836028331,1762.10323359429,
1762.5381069054,1763.40785352806,1763.8427268396,1764.27845284228,1764.71417884496,
1765.14905215677,1765.58392546872,1766.0187987808,1766.88854540534,1767.75829203039,
1768.1931653431,1768.62803865593,1769.06291196888,1769.49778528195,1770.36753190841,
1771.2381312254,1772.10873054259,1772.97847717007,1773.84822379791,1774.71797042609,
1775.58771705456,1776.45746368331,1777.32721031228,1778.19780963089,1779.06840894783,
1779.93815555508,1780.80790201176,1781.67764871408),.UNSPECIFIED.) ;
#834 = B_SPLINE_SURFACE_WITH_KNOTS('',1,3,((#98733,#98734,#98735,#98736,#98737,
#98738,#98739,#98740,#98741,#98742,#98743,#98744,#98745,#98746,#98747,#98748,
#98749,#98750,#98751,#98752,#98753,#98754,#98755,#98756,#98757,#98758,#98759,
#98760,#98761,#98762,#98763,#98764,#98765,#98766,#98767,#98768,#98769,#98770,
#98771,#98772,#98773,#98774,#98775,#98776,#98777,#98778,#98779,#98780,#98781,
#98782,#98783,#98784,#98785,#98786,#98787,#98788,#98789,#98790,#98791,#98792,
#98793,#98794,#98795,#98796,#98797,#98798,#98799,#98800,#98801,#98802,#98803,
#98804,#98805,#98806,#98807,#98808,#98809,#98810,#98811,#98812,#98813,#98814,
#98815,#98816,#98817,#98818,#98819,#98820,#98821,#98822,#98823,#98824,#98825,
#98826,#98827,#98828,#98829,#98830,#98831,#98832,#98833,#98834,#98835,#98836,
#98837,#98838,#98839,#98840,#98841,#98842,#98843,#98844,#98845,#98846,#98847,
#98848,#98849,#98850,#98851,#98852,#98853,#98854,#98855,#98856,#98857,#98858,
#98859,#98860,#98861,#98862,#98863,#98864,#98865,#98866,#98867,#98868,#98869,
#98870,#98871,#98872,#98873,#98874,#98875,#98876,#98877,#98878,#98879,#98880,
#98881,#98882,#98883,#98884,#98885,#98886,#98887,#98888,#98889,#98890,#98891,
#98892,#98893,#98894,#98895,#98896,#98897,#98898,#98899,#98900,#98901,#98902,
#98903,#98904,#98905,#98906,#98907,#98908,#98909,#98910,#98911,#98912,#98913,
#98914,#98915,#98916,#98917,#98918,#98919,#98920,#98921,#98922,#98923,#98924,
#98925,#98926,#98927,#98928,#98929,#98930,#98931,#98932,#98933,#98934,#98935,
#98936,#98937,#98938,#98939,#98940,#98941,#98942,#98943,#98944,#98945,#98946,
#98947,#98948,#98949,#98950,#98951,#98952,#98953,#98954,#98955,#98956,#98957,
#98958,#98959,#98960,#98961,#98962,#98963,#98964,#98965,#98966,#98967,#98968,
#98969,#98970,#98971,#98972,#98973,#98974,#98975,#98976,#98977,#98978,#98979,
#98980,#98981,#98982,#98983,#98984,#98985,#98986,#98987,#98988,#98989,#98990,
#98991,#98992,#98993,#98994,#98995,#98996,#98997,#98998,#98999,#99000,#99001,
#99002,#99003,#99004,#99005,#99006,#99007,#99008,#99009,#99010,#99011,#99012,
#99013,#99014,#99015,#99016,#99017,#99018,#99019,#99020,#99021,#99022,#99023,
#99024,#99025,#99026,#99027,#99028,#99029,#99030,#99031,#99032,#99033,#99034,
#99035,#99036,#99037,#99038,#99039,#99040,#99041,#99042,#99043,#99044,#99045,
#99046,#99047,#99048,#99049,#99050,#99051,#99052,#99053,#99054,#99055,#99056,
#99057,#99058,#99059,#99060,#99061,#99062,#99063,#99064,#99065,#99066,#99067,
#99068,#99069,#99070,#99071,#99072,#99073,#99074,#99075,#99076,#99077,#99078,
#99079,#99080,#99081,#99082,#99083,#99084,#99085,#99086,#99087,#99088,#99089,
#99090,#99091,#99092,#99093,#99094,#99095,#99096,#99097,#99098,#99099,#99100,
#99101,#99102,#99103,#99104,#99105,#99106,#99107,#99108,#99109,#99110,#99111,
#99112,#99113,#99114,#99115,#99116,#99117,#99118,#99119,#99120,#99121,#99122,
#99123,#99124,#99125,#99126,#99127,#99128,#99129,#99130,#99131,#99132,#99133,
#99134,#99135,#99136,#99137,#99138,#99139,#99140,#99141,#99142,#99143,#99144,
#99145,#99146,#99147,#99148,#99149,#99150,#99151,#99152,#99153,#99154,#99155,
#99156,#99157,#99158,#99159,#99160,#99161,#99162,#99163,#99164,#99165,#99166,
#99167,#99168,#99169,#99170,#99171,#99172,#99173,#99174,#99175,#99176,#99177,
#99178,#99179,#99180,#99181,#99182,#99183,#99184,#99185,#99186,#99187,#99188,
#99189,#99190,#99191,#99192,#99193,#99194,#99195,#99196,#99197,#99198,#99199,
#99200,#99201,#99202,#99203,#99204,#99205,#99206,#99207,#99208,#99209,#99210,
#99211,#99212,#99213,#99214,#99215,#99216,#99217,#99218,#99219,#99220,#99221,
#99222,#99223,#99224,#99225,#99226,#99227,#99228,#99229,#99230,#99231,#99232,
#99233,#99234,#99235,#99236,#99237,#99238,#99239,#99240,#99241,#99242,#99243,
#99244,#99245,#99246,#99247,#99248,#99249,#99250,#99251,#99252,#99253,#99254,
#99255,#99256,#99257,#99258,#99259,#99260,#99261,#99262,#99263,#99264,#99265,
#99266,#99267,#99268,#99269,#99270,#99271,#99272,#99273,#99274,#99275,#99276,
#99277,#99278,#99279,#99280,#99281,#99282,#99283,#99284,#99285,#99286,#99287,
#99288,#99289,#99290,#99291,#99292,#99293,#99294,#99295,#99296,#99297,#99298,
#99299,#99300,#99301,#99302,#99303,#99304,#99305,#99306,#99307,#99308,#99309,
#99310,#99311,#99312,#99313,#99314,#99315,#99316,#99317,#99318,#99319,#99320,
#99321,#99322,#99323,#99324,#99325,#99326,#99327,#99328,#99329,#99330,#99331,
#99332,#99333,#99334,#99335,#99336,#99337,#99338,#99339,#99340,#99341,#99342,
#99343,#99344,#99345,#99346,#99347,#99348,#99349,#99350,#99351,#99352,#99353,
#99354,#99355,#99356,#99357,#99358,#99359,#99360,#99361,#99362,#99363,#99364,
#99365,#99366,#99367,#99368,#99369,#99370,#99371,#99372,#99373,#99374,#99375,
#99376,#99377,#99378,#99379,#99380,#99381,#99382,#99383,#99384,#99385,#99386,
#99387,#99388,#99389,#99390,#99391,#99392,#99393,#99394,#99395,#99396,#99397,
#99398,#99399,#99400,#99401,#99402,#99403,#99404,#99405,#99406,#99407,#99408,
#99409,#99410,#99411,#99412,#99413,#99414,#99415,#99416,#99417,#99418,#99419,
#99420,#99421,#99422,#99423,#99424,#99425,#99426,#99427,#99428,#99429,#99430,
#99431,#99432,#99433,#99434,#99435,#99436,#99437,#99438,#99439,#99440,#99441,
#99442,#99443,#99444,#99445,#99446,#99447,#99448,#99449,#99450,#99451,#99452,
#99453,#99454,#99455,#99456,#99457,#99458,#99459,#99460,#99461,#99462,#99463,
#99464,#99465,#99466,#99467,#99468,#99469,#99470,#99471,#99472,#99473,#99474,
#99475,#99476,#99477,#99478,#99479,#99480,#99481,#99482,#99483,#99484,#99485,
#99486,#99487,#99488,#99489,#99490,#99491,#99492,#99493,#99494,#99495,#99496,
#99497,#99498,#99499,#99500,#99501,#99502,#99503,#99504,#99505,#99506,#99507,
#99508,#99509,#99510,#99511,#99512,#99513,#99514,#99515,#99516,#99517,#99518,
#99519,#99520,#99521,#99522,#99523,#99524,#99525,#99526,#99527,#99528,#99529,
#99530,#99531,#99532,#99533,#99534,#99535,#99536,#99537,#99538,#99539,#99540,
#99541,#99542,#99543,#99544,#99545,#99546,#99547,#99548,#99549,#99550,#99551,
#99552,#99553,#99554,#99555,#99556,#99557,#99558,#99559,#99560,#99561,#99562,
#99563,#99564,#99565,#99566,#99567,#99568,#99569,#99570,#99571,#99572,#99573,
#99574,#99575,#99576,#99577,#99578,#99579,#99580,#99581,#99582,#99583,#99584,
#99585,#99586,#99587,#99588,#99589,#99590,#99591,#99592,#99593,#99594,#99595,
#99596,#99597,#99598,#99599,#99600,#99601,#99602,#99603,#99604,#99605,#99606,
#99607,#99608,#99609,#99610,#99611,#99612,#99613,#99614,#99615,#99616,#99617,
#99618,#99619,#99620,#99621,#99622,#99623,#99624,#99625,#99626,#99627,#99628,
#99629,#99630,#99631,#99632,#99633,#99634,#99635,#99636,#99637,#99638,#99639,
#99640,#99641,#99642,#99643,#99644,#99645,#99646,#99647,#99648,#99649,#99650,
#99651,#99652,#99653,#99654,#99655,#99656,#99657,#99658,#99659,#99660,#99661,
#99662,#99663,#99664,#99665,#99666,#99667,#99668,#99669,#99670,#99671,#99672,
#99673,#99674,#99675,#99676,#99677,#99678,#99679,#99680,#99681,#99682,#99683,
#99684,#99685,#99686,#99687,#99688,#99689,#99690,#99691,#99692,#99693,#99694,
#99695,#99696,#99697,#99698,#99699,#99700,#99701,#99702,#99703,#99704,#99705,
#99706,#99707,#99708,#99709,#99710,#99711,#99712,#99713,#99714,#99715,#99716,
#99717,#99718,#99719,#99720,#99721,#99722,#99723,#99724,#99725,#99726,#99727,
#99728,#99729,#99730,#99731,#99732,#99733,#99734,#99735,#99736,#99737,#99738,
#99739,#99740,#99741,#99742,#99743,#99744,#99745,#99746,#99747,#99748,#99749,
#99750,#99751,#99752,#99753,#99754,#99755,#99756,#99757,#99758,#99759,#99760,
#99761,#99762,#99763,#99764,#99765,#99766,#99767,#99768,#99769,#99770,#99771,
#99772,#99773,#99774,#99775,#99776,#99777,#99778,#99779,#99780,#99781,#99782,
#99783,#99784,#99785,#99786,#99787,#99788,#99789,#99790,#99791,#99792,#99793,
#99794,#99795,#99796,#99797,#99798,#99799,#99800,#99801,#99802,#99803,#99804,
#99805,#99806,#99807,#99808,#99809,#99810,#99811,#99812,#99813,#99814,#99815,
#99816,#99817,#99818,#99819,#99820,#99821,#99822,#99823,#99824,#99825,#99826,
#99827,#99828,#99829,#99830,#99831,#99832,#99833,#99834,#99835,#99836,#99837,
#99838,#99839,#99840,#99841,#99842,#99843,#99844,#99845,#99846,#99847,#99848,
#99849,#99850,#99851,#99852,#99853,#99854,#99855,#99856,#99857,#99858,#99859,
#99860,#99861,#99862,#99863,#99864,#99865,#99866,#99867,#99868,#99869,#99870,
#99871,#99872,#99873,#99874,#99875,#99876,#99877,#99878,#99879,#99880,#99881,
#99882,#99883,#99884,#99885,#99886,#99887,#99888,#99889,#99890,#99891,#99892,
#99893,#99894,#99895,#99896,#99897,#99898,#99899,#99900,#99901,#99902,#99903,
#99904,#99905,#99906,#99907,#99908,#99909,#99910,#99911,#99912,#99913,#99914,
#99915,#99916,#99917,#99918,#99919,#99920,#99921,#99922,#99923,#99924,#99925,
#99926,#99927,#99928,#99929,#99930,#99931,#99932,#99933,#99934,#99935,#99936,
#99937,#99938,#99939,#99940,#99941,#99942,#99943,#99944,#99945,#99946,#99947,
#99948,#99949,#99950,#99951,#99952,#99953,#99954,#99955,#99956,#99957,#99958,
#99959,#99960,#99961,#99962,#99963,#99964,#99965,#99966,#99967,#99968,#99969,
#99970,#99971,#99972,#99973,#99974,#99975,#99976,#99977,#99978,#99979,#99980,
#99981,#99982,#99983,#99984,#99985,#99986,#99987,#99988,#99989,#99990,#99991,
#99992,#99993,#99994,#99995,#99996,#99997,#99998,#99999,#100000,#100001,
#100002,#100003,#100004,#100005,#100006,#100007,#100008,#100009,#100010,
#100011,#100012,#100013,#100014,#100015,#100016,#100017,#100018,#100019,
#100020,#100021,#100022,#100023,#100024,#100025,#100026,#100027,#100028,
#100029,#100030,#100031,#100032,#100033,#100034,#100035,#100036,#100037,
#100038,#100039,#100040,#100041,#100042,#100043,#100044,#100045,#100046,
#100047,#100048,#100049,#100050,#100051,#100052,#100053,#100054,#100055,
#100056,#100057,#100058,#100059,#100060,#100061,#100062,#100063,#100064,
#100065,#100066,#100067,#100068,#100069,#100070,#100071,#100072,#100073,
#100074,#100075,#100076,#100077,#100078,#100079,#100080,#100081,#100082,
#100083,#100084,#100085,#100086,#100087,#100088,#100089,#100090,#100091,
#100092,#100093,#100094,#100095,#100096,#100097,#100098,#100099,#100100,
#100101,#100102,#100103,#100104,#100105,#100106,#100107,#100108,#100109,
#100110,#100111,#100112,#100113,#100114,#100115,#100116,#100117,#100118,
#100119,#100120,#100121,#100122,#100123,#100124,#100125,#100126,#100127,
#100128,#100129,#100130,#100131,#100132,#100133,#100134,#100135,#100136,
#100137,#100138,#100139,#100140,#100141,#100142,#100143,#100144,#100145,
#100146,#100147,#100148,#100149,#100150,#100151,#100152,#100153,#100154,
#100155,#100156,#100157,#100158,#100159,#100160,#100161,#100162,#100163,
#100164,#100165,#100166,#100167,#100168,#100169,#100170,#100171,#100172,
#100173,#100174,#100175,#100176,#100177,#100178,#100179,#100180,#100181,
#100182,#100183,#100184,#100185,#100186,#100187,#100188,#100189,#100190,
#100191,#100192,#100193,#100194,#100195,#100196,#100197,#100198,#100199,
#100200,#100201,#100202,#100203,#100204,#100205,#100206,#100207,#100208,
#100209,#100210,#100211,#100212,#100213,#100214,#100215,#100216,#100217,
#100218,#100219,#100220,#100221,#100222,#100223,#100224,#100225,#100226,
#100227,#100228,#100229,#100230,#100231,#100232,#100233,#100234,#100235,
#100236,#100237,#100238,#100239,#100240,#100241,#100242,#100243,#100244,
#100245,#100246,#100247,#100248,#100249,#100250,#100251,#100252,#100253,
#100254,#100255,#100256,#100257,#100258,#100259,#100260,#100261,#100262,
#100263,#100264,#100265,#100266,#100267,#100268,#100269,#100270,#100271,
#100272,#100273,#100274,#100275,#100276,#100277,#100278,#100279,#100280,
#100281,#100282,#100283,#100284,#100285,#100286,#100287,#100288,#100289,
#100290,#100291,#100292,#100293,#100294,#100295,#100296,#100297,#100298,
#100299,#100300,#100301,#100302,#100303,#100304,#100305,#100306,#100307,
#100308,#100309,#100310,#100311,#100312,#100313,#100314,#100315,#100316,
#100317,#100318,#100319,#100320,#100321,#100322,#100323,#100324,#100325,
#100326,#100327,#100328,#100329,#100330,#100331,#100332,#100333,#100334,
#100335,#100336,#100337,#100338,#100339,#100340,#100341,#100342,#100343,
#100344,#100345,#100346,#100347,#100348,#100349,#100350,#100351,#100352,
#100353,#100354,#100355,#100356,#100357,#100358,#100359,#100360,#100361,
#100362,#100363,#100364,#100365,#100366,#100367,#100368,#100369,#100370,
#100371,#100372,#100373,#100374,#100375,#100376,#100377,#100378,#100379,
#100380,#100381,#100382,#100383,#100384,#100385,#100386,#100387,#100388,
#100389,#100390,#100391,#100392,#100393,#100394,#100395,#100396,#100397,
#100398,#100399,#100400,#100401,#100402,#100403,#100404,#100405,#100406,
#100407,#100408,#100409,#100410,#100411,#100412,#100413,#100414,#100415,
#100416,#100417,#100418,#100419,#100420,#100421,#100422,#100423,#100424,
#100425,#100426,#100427,#100428,#100429,#100430,#100431,#100432,#100433,
#100434,#100435,#100436,#100437,#100438,#100439,#100440,#100441,#100442,
#100443,#100444,#100445,#100446,#100447,#100448,#100449,#100450,#100451,
#100452,#100453,#100454,#100455,#100456,#100457,#100458,#100459,#100460,
#100461,#100462,#100463,#100464,#100465,#100466,#100467,#100468,#100469,
#100470,#100471,#100472,#100473,#100474,#100475,#100476,#100477,#100478,
#100479,#100480,#100481,#100482,#100483,#100484,#100485,#100486,#100487,
#100488,#100489,#100490,#100491,#100492,#100493,#100494,#100495,#100496,
#100497,#100498,#100499,#100500,#100501,#100502,#100503,#100504,#100505,
#100506,#100507,#100508,#100509,#100510,#100511,#100512,#100513,#100514,
#100515,#100516,#100517,#100518,#100519,#100520,#100521,#100522,#100523,
#100524,#100525,#100526,#100527,#100528,#100529,#100530,#100531,#100532,
#100533,#100534,#100535,#100536,#100537,#100538,#100539,#100540,#100541,
#100542,#100543,#100544,#100545,#100546,#100547,#100548,#100549,#100550,
#100551,#100552,#100553,#100554,#100555,#100556,#100557,#100558,#100559,
#100560,#100561,#100562,#100563,#100564,#100565,#100566,#100567,#100568,
#100569,#100570,#100571,#100572,#100573,#100574,#100575,#100576,#100577,
#100578,#100579,#100580,#100581,#100582,#100583,#100584,#100585,#100586,
#100587,#100588,#100589,#100590,#100591,#100592,#100593,#100594,#100595,
#100596,#100597,#100598,#100599,#100600,#100601,#100602,#100603,#100604,
#100605,#100606,#100607,#100608,#100609,#100610,#100611,#100612,#100613,
#100614,#100615,#100616,#100617,#100618,#100619,#100620,#100621,#100622,
#100623,#100624,#100625,#100626,#100627,#100628,#100629,#100630,#100631,
#100632,#100633,#100634,#100635,#100636,#100637,#100638,#100639,#100640,
#100641,#100642,#100643,#100644,#100645,#100646,#100647,#100648,#100649,
#100650,#100651,#100652,#100653,#100654,#100655,#100656,#100657,#100658,
#100659,#100660,#100661,#100662,#100663,#100664,#100665,#100666,#100667,
#100668,#100669,#100670,#100671,#100672,#100673,#100674,#100675,#100676,
#100677,#100678,#100679,#100680,#100681,#100682,#100683,#100684,#100685,
#100686,#100687,#100688,#100689,#100690,#100691,#100692,#100693,#100694,
#100695,#100696,#100697,#100698,#100699,#100700,#100701,#100702,#100703,
#100704,#100705,#100706,#100707,#100708,#100709,#100710,#100711,#100712,
#100713,#100714,#100715,#100716,#100717,#100718,#100719,#100720,#100721,
#100722,#100723,#100724,#100725,#100726,#100727,#100728,#100729,#100730,
#100731,#100732,#100733,#100734,#100735,#100736,#100737,#100738,#100739,
#100740,#100741,#100742,#100743,#100744,#100745,#100746,#100747,#100748,
#100749,#100750,#100751,#100752,#100753,#100754,#100755,#100756,#100757,
#100758,#100759,#100760,#100761,#100762,#100763,#100764,#100765,#100766,
#100767,#100768,#100769,#100770,#100771,#100772,#100773,#100774,#100775,
#100776,#100777,#100778,#100779,#100780,#100781,#100782,#100783,#100784,
#100785,#100786,#100787,#100788,#100789,#100790,#100791,#100792,#100793,
#100794,#100795,#100796,#100797,#100798,#100799,#100800,#100801,#100802,
#100803,#100804,#100805,#100806,#100807,#100808,#100809,#100810,#100811,
#100812,#100813,#100814,#100815,#100816,#100817,#100818,#100819,#100820,
#100821,#100822,#100823,#100824,#100825,#100826,#100827,#100828,#100829,
#100830,#100831,#100832,#100833,#100834,#100835,#100836,#100837,#100838,
#100839,#100840,#100841,#100842,#100843,#100844,#100845,#100846,#100847,
#100848,#100849,#100850,#100851,#100852,#100853,#100854,#100855,#100856,
#100857,#100858,#100859,#100860,#100861,#100862,#100863,#100864,#100865,
#100866,#100867,#100868,#100869,#100870,#100871,#100872,#100873,#100874,
#100875,#100876,#100877,#100878,#100879,#100880,#100881,#100882,#100883,
#100884,#100885,#100886,#100887,#100888,#100889,#100890,#100891,#100892,
#100893,#100894,#100895,#100896,#100897,#100898,#100899,#100900,#100901,
#100902,#100903,#100904,#100905,#100906,#100907,#100908,#100909,#100910,
#100911,#100912,#100913,#100914,#100915,#100916,#100917,#100918,#100919,
#100920,#100921,#100922,#100923,#100924,#100925,#100926,#100927,#100928,
#100929,#100930,#100931,#100932,#100933,#100934,#100935,#100936,#100937,
#100938,#100939,#100940,#100941,#100942,#100943,#100944,#100945,#100946,
#100947,#100948,#100949,#100950,#100951,#100952,#100953,#100954,#100955,
#100956,#100957,#100958,#100959,#100960,#100961,#100962,#100963,#100964,
#100965,#100966,#100967,#100968,#100969,#100970,#100971,#100972,#100973,
#100974,#100975,#100976,#100977,#100978,#100979,#100980,#100981,#100982,
#100983,#100984,#100985,#100986,#100987,#100988,#100989,#100990,#100991,
#100992,#100993,#100994,#100995,#100996,#100997,#100998,#100999,#101000,
#101001,#101002,#101003,#101004,#101005,#101006,#101007,#101008,#101009,
#101010,#101011,#101012,#101013,#101014,#101015,#101016,#101017,#101018,
#101019,#101020,#101021,#101022,#101023,#101024,#101025,#101026,#101027,
#101028,#101029,#101030,#101031,#101032,#101033,#101034,#101035,#101036,
#101037,#101038,#101039,#101040,#101041,#101042,#101043,#101044,#101045,
#101046,#101047,#101048,#101049,#101050,#101051,#101052,#101053,#101054,
#101055,#101056,#101057,#101058,#101059,#101060,#101061,#101062,#101063,
#101064,#101065,#101066,#101067,#101068,#101069,#101070,#101071,#101072,
#101073,#101074,#101075,#101076,#101077,#101078,#101079,#101080,#101081,
#101082,#101083,#101084,#101085,#101086,#101087,#101088,#101089,#101090,
#101091,#101092,#101093,#101094,#101095,#101096,#101097,#101098,#101099,
#101100,#101101,#101102,#101103,#101104,#101105,#101106,#101107,#101108,
#101109,#101110,#101111,#101112,#101113,#101114,#101115,#101116,#101117,
#101118,#101119,#101120,#101121,#101122,#101123,#101124,#101125,#101126,
#101127,#101128,#101129,#101130,#101131,#101132,#101133,#101134,#101135,
#101136,#101137,#101138,#101139,#101140,#101141,#101142,#101143,#101144,
#101145,#101146,#101147,#101148,#101149,#101150,#101151,#101152,#101153,
#101154,#101155,#101156,#101157,#101158,#101159,#101160,#101161,#101162,
#101163,#101164,#101165,#101166,#101167,#101168,#101169,#101170,#101171,
#101172,#101173,#101174,#101175,#101176,#101177,#101178,#101179,#101180,
#101181,#101182,#101183,#101184,#101185,#101186,#101187,#101188,#101189,
#101190,#101191,#101192,#101193,#101194,#101195,#101196,#101197,#101198,
#101199,#101200,#101201,#101202,#101203,#101204,#101205,#101206,#101207,
#101208,#101209,#101210,#101211,#101212,#101213,#101214,#101215,#101216,
#101217,#101218,#101219,#101220,#101221,#101222,#101223,#101224,#101225,
#101226,#101227,#101228,#101229,#101230,#101231,#101232,#101233,#101234,
#101235,#101236,#101237,#101238,#101239,#101240,#101241,#101242,#101243,
#101244,#101245,#101246,#101247,#101248,#101249,#101250,#101251,#101252,
#101253,#101254,#101255,#101256,#101257,#101258,#101259,#101260,#101261,
#101262,#101263,#101264,#101265,#101266,#101267,#101268,#101269,#101270,
#101271,#101272,#101273,#101274,#101275,#101276,#101277,#101278,#101279,
#101280,#101281,#101282,#101283,#101284,#101285,#101286,#101287,#101288,
#101289,#101290,#101291,#101292,#101293,#101294,#101295,#101296,#101297,
#101298,#101299,#101300,#101301,#101302,#101303,#101304,#101305,#101306,
#101307,#101308,#101309,#101310,#101311,#101312,#101313,#101314,#101315,
#101316,#101317,#101318,#101319,#101320,#101321,#101322,#101323,#101324,
#101325,#101326,#101327,#101328,#101329,#101330,#101331,#101332,#101333,
#101334,#101335,#101336,#101337,#101338,#101339,#101340,#101341,#101342,
#101343,#101344,#101345,#101346,#101347,#101348,#101349,#101350,#101351,
#101352,#101353,#101354,#101355,#101356,#101357,#101358,#101359,#101360,
#101361,#101362,#101363,#101364,#101365,#101366,#101367,#101368,#101369,
#101370,#101371,#101372,#101373,#101374,#101375,#101376,#101377,#101378,
#101379,#101380,#101381,#101382,#101383,#101384,#101385,#101386,#101387,
#101388,#101389,#101390,#101391,#101392,#101393,#101394,#101395,#101396,
#101397,#101398,#101399,#101400,#101401,#101402,#101403,#101404,#101405,
#101406,#101407,#101408,#101409,#101410,#101411,#101412,#101413,#101414,
#101415,#101416,#101417,#101418,#101419,#101420,#101421,#101422,#101423,
#101424,#101425,#101426,#101427,#101428,#101429,#101430,#101431,#101432,
#101433,#101434,#101435,#101436,#101437,#101438,#101439,#101440,#101441,
#101442,#101443,#101444,#101445,#101446,#101447,#101448,#101449,#101450,
#101451,#101452,#101453,#101454,#101455,#101456,#101457,#101458,#101459,
#101460,#101461,#101462,#101463,#101464,#101465,#101466,#101467,#101468,
#101469,#101470,#101471,#101472,#101473,#101474,#101475,#101476,#101477,
#101478,#101479,#101480,#101481,#101482,#101483,#101484,#101485,#101486,
#101487,#101488,#101489,#101490,#101491,#101492,#101493,#101494,#101495,
#101496,#101497,#101498,#101499,#101500,#101501,#101502,#101503,#101504,
#101505,#101506,#101507,#101508,#101509,#101510,#101511,#101512,#101513,
#101514,#101515,#101516,#101517,#101518,#101519,#101520,#101521,#101522,
#101523,#101524,#101525,#101526,#101527,#101528,#101529,#101530,#101531,
#101532,#101533,#101534,#101535,#101536,#101537,#101538,#101539,#101540,
#101541,#101542,#101543,#101544,#101545,#101546,#101547,#101548,#101549,
#101550,#101551,#101552,#101553,#101554,#101555,#101556,#101557,#101558,
#101559,#101560,#101561,#101562,#101563,#101564,#101565,#101566,#101567,
#101568,#101569,#101570,#101571,#101572,#101573,#101574,#101575,#101576,
#101577,#101578,#101579,#101580,#101581,#101582,#101583,#101584,#101585,
#101586,#101587,#101588,#101589,#101590,#101591,#101592,#101593,#101594,
#101595,#101596,#101597,#101598,#101599,#101600,#101601,#101602,#101603,
#101604,#101605,#101606,#101607,#101608,#101609,#101610,#101611,#101612,
#101613,#101614,#101615,#101616,#101617,#101618,#101619,#101620,#101621,
#101622,#101623,#101624,#101625,#101626,#101627,#101628,#101629,#101630,
#101631,#101632,#101633,#101634,#101635,#101636,#101637,#101638,#101639,
#101640,#101641,#101642,#101643,#101644,#101645,#101646,#101647,#101648,
#101649,#101650,#101651,#101652,#101653,#101654,#101655,#101656,#101657,
#101658,#101659,#101660,#101661,#101662,#101663,#101664,#101665,#101666,
#101667,#101668,#101669,#101670,#101671,#101672,#101673,#101674,#101675,
#101676,#101677,#101678,#101679,#101680,#101681,#101682,#101683,#101684,
#101685,#101686,#101687,#101688,#101689,#101690,#101691,#101692,#101693,
#101694,#101695,#101696,#101697,#101698,#101699,#101700,#101701,#101702,
#101703,#101704,#101705,#101706,#101707,#101708,#101709,#101710,#101711,
#101712,#101713,#101714,#101715,#101716,#101717,#101718,#101719,#101720,
#101721,#101722,#101723,#101724,#101725,#101726,#101727,#101728,#101729,
#101730,#101731,#101732,#101733,#101734,#101735,#101736,#101737,#101738,
#101739,#101740,#101741,#101742,#101743,#101744,#101745,#101746,#101747,
#101748,#101749,#101750,#101751,#101752,#101753,#101754,#101755,#101756,
#101757,#101758,#101759,#101760,#101761,#101762,#101763,#101764,#101765,
#101766,#101767,#101768,#101769,#101770,#101771,#101772,#101773,#101774,
#101775,#101776,#101777,#101778,#101779,#101780,#101781,#101782,#101783,
#101784,#101785,#101786,#101787,#101788,#101789,#101790,#101791,#101792,
#101793,#101794,#101795,#101796,#101797,#101798,#101799,#101800,#101801,
#101802,#101803,#101804,#101805,#101806,#101807,#101808,#101809,#101810,
#101811,#101812,#101813,#101814,#101815,#101816,#101817,#101818,#101819,
#101820,#101821,#101822,#101823,#101824,#101825,#101826,#101827,#101828,
#101829,#101830,#101831,#101832,#101833,#101834,#101835,#101836,#101837,
#101838,#101839,#101840,#101841,#101842,#101843,#101844,#101845,#101846,
#101847,#101848,#101849,#101850,#101851,#101852,#101853,#101854,#101855,
#101856,#101857,#101858,#101859,#101860,#101861,#101862,#101863,#101864,
#101865,#101866,#101867,#101868,#101869,#101870,#101871,#101872,#101873,
#101874,#101875,#101876,#101877,#101878,#101879,#101880,#101881,#101882,
#101883,#101884,#101885,#101886,#101887,#101888,#101889,#101890,#101891,
#101892,#101893,#101894,#101895,#101896,#101897,#101898,#101899,#101900,
#101901,#101902,#101903,#101904,#101905,#101906,#101907,#101908,#101909,
#101910,#101911,#101912,#101913,#101914,#101915,#101916,#101917,#101918,
#101919,#101920,#101921,#101922,#101923,#101924,#101925,#101926,#101927,
#101928,#101929,#101930,#101931,#101932,#101933,#101934,#101935,#101936,
#101937,#101938,#101939,#101940,#101941,#101942,#101943,#101944,#101945,
#101946,#101947,#101948,#101949,#101950,#101951,#101952,#101953,#101954,
#101955,#101956,#101957,#101958,#101959,#101960,#101961,#101962,#101963,
#101964,#101965,#101966,#101967,#101968,#101969,#101970,#101971,#101972,
#101973,#101974,#101975,#101976,#101977,#101978,#101979,#101980,#101981,
#101982,#101983,#101984,#101985,#101986,#101987,#101988,#101989,#101990,
#101991,#101992,#101993,#101994,#101995,#101996,#101997,#101998,#101999,
#102000,#102001,#102002,#102003,#102004,#102005,#102006,#102007,#102008,
#102009,#102010,#102011,#102012,#102013,#102014,#102015,#102016,#102017,
#102018,#102019,#102020,#102021,#102022,#102023,#102024,#102025,#102026,
#102027,#102028,#102029,#102030,#102031,#102032,#102033,#102034,#102035,
#102036,#102037,#102038,#102039,#102040,#102041,#102042,#102043,#102044,
#102045,#102046,#102047,#102048,#102049,#102050,#102051,#102052,#102053,
#102054,#102055,#102056,#102057,#102058,#102059,#102060,#102061,#102062,
#102063,#102064,#102065,#102066,#102067,#102068,#102069,#102070,#102071,
#102072,#102073,#102074,#102075,#102076,#102077,#102078,#102079,#102080,
#102081,#102082,#102083,#102084,#102085,#102086,#102087,#102088,#102089,
#102090,#102091,#102092,#102093,#102094,#102095,#102096,#102097,#102098,
#102099,#102100,#102101,#102102,#102103,#102104,#102105,#102106,#102107,
#102108,#102109,#102110,#102111,#102112,#102113,#102114,#102115,#102116,
#102117,#102118,#102119,#102120,#102121,#102122,#102123,#102124,#102125,
#102126,#102127,#102128,#102129,#102130,#102131,#102132,#102133,#102134,
#102135,#102136,#102137,#102138,#102139,#102140,#102141,#102142,#102143,
#102144,#102145,#102146,#102147,#102148,#102149,#102150,#102151,#102152,
#102153,#102154,#102155,#102156,#102157,#102158,#102159,#102160,#102161,
#102162,#102163,#102164,#102165,#102166,#102167,#102168,#102169,#102170,
#102171,#102172,#102173,#102174,#102175,#102176,#102177,#102178,#102179,
#102180,#102181,#102182,#102183,#102184,#102185,#102186,#102187,#102188,
#102189,#102190,#102191,#102192,#102193,#102194,#102195,#102196,#102197,
#102198,#102199,#102200,#102201,#102202,#102203,#102204,#102205,#102206,
#102207,#102208,#102209,#102210,#102211,#102212,#102213,#102214,#102215,
#102216,#102217),(#102218,#102219,#102220,#102221,#102222,#102223,#102224,
#102225,#102226,#102227,#102228,#102229,#102230,#102231,#102232,#102233,
#102234,#102235,#102236,#102237,#102238,#102239,#102240,#102241,#102242,
#102243,#102244,#102245,#102246,#102247,#102248,#102249,#102250,#102251,
#102252,#102253,#102254,#102255,#102256,#102257,#102258,#102259,#102260,
#102261,#102262,#102263,#102264,#102265,#102266,#102267,#102268,#102269,
#102270,#102271,#102272,#102273,#102274,#102275,#102276,#102277,#102278,
#102279,#102280,#102281,#102282,#102283,#102284,#102285,#102286,#102287,
#102288,#102289,#102290,#102291,#102292,#102293,#102294,#102295,#102296,
#102297,#102298,#102299,#102300,#102301,#102302,#102303,#102304,#102305,
#102306,#102307,#102308,#102309,#102310,#102311,#102312,#102313,#102314,
#102315,#102316,#102317,#102318,#102319,#102320,#102321,#102322,#102323,
#102324,#102325,#102326,#102327,#102328,#102329,#102330,#102331,#102332,
#102333,#102334,#102335,#102336,#102337,#102338,#102339,#102340,#102341,
#102342,#102343,#102344,#102345,#102346,#102347,#102348,#102349,#102350,
#102351,#102352,#102353,#102354,#102355,#102356,#102357,#102358,#102359,
#102360,#102361,#102362,#102363,#102364,#102365,#102366,#102367,#102368,
#102369,#102370,#102371,#102372,#102373,#102374,#102375,#102376,#102377,
#102378,#102379,#102380,#102381,#102382,#102383,#102384,#102385,#102386,
#102387,#102388,#102389,#102390,#102391,#102392,#102393,#102394,#102395,
#102396,#102397,#102398,#102399,#102400,#102401,#102402,#102403,#102404,
#102405,#102406,#102407,#102408,#102409,#102410,#102411,#102412,#102413,
#102414,#102415,#102416,#102417,#102418,#102419,#102420,#102421,#102422,
#102423,#102424,#102425,#102426,#102427,#102428,#102429,#102430,#102431,
#102432,#102433,#102434,#102435,#102436,#102437,#102438,#102439,#102440,
#102441,#102442,#102443,#102444,#102445,#102446,#102447,#102448,#102449,
#102450,#102451,#102452,#102453,#102454,#102455,#102456,#102457,#102458,
#102459,#102460,#102461,#102462,#102463,#102464,#102465,#102466,#102467,
#102468,#102469,#102470,#102471,#102472,#102473,#102474,#102475,#102476,
#102477,#102478,#102479,#102480,#102481,#102482,#102483,#102484,#102485,
#102486,#102487,#102488,#102489,#102490,#102491,#102492,#102493,#102494,
#102495,#102496,#102497,#102498,#102499,#102500,#102501,#102502,#102503,
#102504,#102505,#102506,#102507,#102508,#102509,#102510,#102511,#102512,
#102513,#102514,#102515,#102516,#102517,#102518,#102519,#102520,#102521,
#102522,#102523,#102524,#102525,#102526,#102527,#102528,#102529,#102530,
#102531,#102532,#102533,#102534,#102535,#102536,#102537,#102538,#102539,
#102540,#102541,#102542,#102543,#102544,#102545,#102546,#102547,#102548,
#102549,#102550,#102551,#102552,#102553,#102554,#102555,#102556,#102557,
#102558,#102559,#102560,#102561,#102562,#102563,#102564,#102565,#102566,
#102567,#102568,#102569,#102570,#102571,#102572,#102573,#102574,#102575,
#102576,#102577,#102578,#102579,#102580,#102581,#102582,#102583,#102584,
#102585,#102586,#102587,#102588,#102589,#102590,#102591,#102592,#102593,
#102594,#102595,#102596,#102597,#102598,#102599,#102600,#102601,#102602,
#102603,#102604,#102605,#102606,#102607,#102608,#102609,#102610,#102611,
#102612,#102613,#102614,#102615,#102616,#102617,#102618,#102619,#102620,
#102621,#102622,#102623,#102624,#102625,#102626,#102627,#102628,#102629,
#102630,#102631,#102632,#102633,#102634,#102635,#102636,#102637,#102638,
#102639,#102640,#102641,#102642,#102643,#102644,#102645,#102646,#102647,
#102648,#102649,#102650,#102651,#102652,#102653,#102654,#102655,#102656,
#102657,#102658,#102659,#102660,#102661,#102662,#102663,#102664,#102665,
#102666,#102667,#102668,#102669,#102670,#102671,#102672,#102673,#102674,
#102675,#102676,#102677,#102678,#102679,#102680,#102681,#102682,#102683,
#102684,#102685,#102686,#102687,#102688,#102689,#102690,#102691,#102692,
#102693,#102694,#102695,#102696,#102697,#102698,#102699,#102700,#102701,
#102702,#102703,#102704,#102705,#102706,#102707,#102708,#102709,#102710,
#102711,#102712,#102713,#102714,#102715,#102716,#102717,#102718,#102719,
#102720,#102721,#102722,#102723,#102724,#102725,#102726,#102727,#102728,
#102729,#102730,#102731,#102732,#102733,#102734,#102735,#102736,#102737,
#102738,#102739,#102740,#102741,#102742,#102743,#102744,#102745,#102746,
#102747,#102748,#102749,#102750,#102751,#102752,#102753,#102754,#102755,
#102756,#102757,#102758,#102759,#102760,#102761,#102762,#102763,#102764,
#102765,#102766,#102767,#102768,#102769,#102770,#102771,#102772,#102773,
#102774,#102775,#102776,#102777,#102778,#102779,#102780,#102781,#102782,
#102783,#102784,#102785,#102786,#102787,#102788,#102789,#102790,#102791,
#102792,#102793,#102794,#102795,#102796,#102797,#102798,#102799,#102800,
#102801,#102802,#102803,#102804,#102805,#102806,#102807,#102808,#102809,
#102810,#102811,#102812,#102813,#102814,#102815,#102816,#102817,#102818,
#102819,#102820,#102821,#102822,#102823,#102824,#102825,#102826,#102827,
#102828,#102829,#102830,#102831,#102832,#102833,#102834,#102835,#102836,
#102837,#102838,#102839,#102840,#102841,#102842,#102843,#102844,#102845,
#102846,#102847,#102848,#102849,#102850,#102851,#102852,#102853,#102854,
#102855,#102856,#102857,#102858,#102859,#102860,#102861,#102862,#102863,
#102864,#102865,#102866,#102867,#102868,#102869,#102870,#102871,#102872,
#102873,#102874,#102875,#102876,#102877,#102878,#102879,#102880,#102881,
#102882,#102883,#102884,#102885,#102886,#102887,#102888,#102889,#102890,
#102891,#102892,#102893,#102894,#102895,#102896,#102897,#102898,#102899,
#102900,#102901,#102902,#102903,#102904,#102905,#102906,#102907,#102908,
#102909,#102910,#102911,#102912,#102913,#102914,#102915,#102916,#102917,
#102918,#102919,#102920,#102921,#102922,#102923,#102924,#102925,#102926,
#102927,#102928,#102929,#102930,#102931,#102932,#102933,#102934,#102935,
#102936,#102937,#102938,#102939,#102940,#102941,#102942,#102943,#102944,
#102945,#102946,#102947,#102948,#102949,#102950,#102951,#102952,#102953,
#102954,#102955,#102956,#102957,#102958,#102959,#102960,#102961,#102962,
#102963,#102964,#102965,#102966,#102967,#102968,#102969,#102970,#102971,
#102972,#102973,#102974,#102975,#102976,#102977,#102978,#102979,#102980,
#102981,#102982,#102983,#102984,#102985,#102986,#102987,#102988,#102989,
#102990,#102991,#102992,#102993,#102994,#102995,#102996,#102997,#102998,
#102999,#103000,#103001,#103002,#103003,#103004,#103005,#103006,#103007,
#103008,#103009,#103010,#103011,#103012,#103013,#103014,#103015,#103016,
#103017,#103018,#103019,#103020,#103021,#103022,#103023,#103024,#103025,
#103026,#103027,#103028,#103029,#103030,#103031,#103032,#103033,#103034,
#103035,#103036,#103037,#103038,#103039,#103040,#103041,#103042,#103043,
#103044,#103045,#103046,#103047,#103048,#103049,#103050,#103051,#103052,
#103053,#103054,#103055,#103056,#103057,#103058,#103059,#103060,#103061,
#103062,#103063,#103064,#103065,#103066,#103067,#103068,#103069,#103070,
#103071,#103072,#103073,#103074,#103075,#103076,#103077,#103078,#103079,
#103080,#103081,#103082,#103083,#103084,#103085,#103086,#103087,#103088,
#103089,#103090,#103091,#103092,#103093,#103094,#103095,#103096,#103097,
#103098,#103099,#103100,#103101,#103102,#103103,#103104,#103105,#103106,
#103107,#103108,#103109,#103110,#103111,#103112,#103113,#103114,#103115,
#103116,#103117,#103118,#103119,#103120,#103121,#103122,#103123,#103124,
#103125,#103126,#103127,#103128,#103129,#103130,#103131,#103132,#103133,
#103134,#103135,#103136,#103137,#103138,#103139,#103140,#103141,#103142,
#103143,#103144,#103145,#103146,#103147,#103148,#103149,#103150,#103151,
#103152,#103153,#103154,#103155,#103156,#103157,#103158,#103159,#103160,
#103161,#103162,#103163,#103164,#103165,#103166,#103167,#103168,#103169,
#103170,#103171,#103172,#103173,#103174,#103175,#103176,#103177,#103178,
#103179,#103180,#103181,#103182,#103183,#103184,#103185,#103186,#103187,
#103188,#103189,#103190,#103191,#103192,#103193,#103194,#103195,#103196,
#103197,#103198,#103199,#103200,#103201,#103202,#103203,#103204,#103205,
#103206,#103207,#103208,#103209,#103210,#103211,#103212,#103213,#103214,
#103215,#103216,#103217,#103218,#103219,#103220,#103221,#103222,#103223,
#103224,#103225,#103226,#103227,#103228,#103229,#103230,#103231,#103232,
#103233,#103234,#103235,#103236,#103237,#103238,#103239,#103240,#103241,
#103242,#103243,#103244,#103245,#103246,#103247,#103248,#103249,#103250,
#103251,#103252,#103253,#103254,#103255,#103256,#103257,#103258,#103259,
#103260,#103261,#103262,#103263,#103264,#103265,#103266,#103267,#103268,
#103269,#103270,#103271,#103272,#103273,#103274,#103275,#103276,#103277,
#103278,#103279,#103280,#103281,#103282,#103283,#103284,#103285,#103286,
#103287,#103288,#103289,#103290,#103291,#103292,#103293,#103294,#103295,
#103296,#103297,#103298,#103299,#103300,#103301,#103302,#103303,#103304,
#103305,#103306,#103307,#103308,#103309,#103310,#103311,#103312,#103313,
#103314,#103315,#103316,#103317,#103318,#103319,#103320,#103321,#103322,
#103323,#103324,#103325,#103326,#103327,#103328,#103329,#103330,#103331,
#103332,#103333,#103334,#103335,#103336,#103337,#103338,#103339,#103340,
#103341,#103342,#103343,#103344,#103345,#103346,#103347,#103348,#103349,
#103350,#103351,#103352,#103353,#103354,#103355,#103356,#103357,#103358,
#103359,#103360,#103361,#103362,#103363,#103364,#103365,#103366,#103367,
#103368,#103369,#103370,#103371,#103372,#103373,#103374,#103375,#103376,
#103377,#103378,#103379,#103380,#103381,#103382,#103383,#103384,#103385,
#103386,#103387,#103388,#103389,#103390,#103391,#103392,#103393,#103394,
#103395,#103396,#103397,#103398,#103399,#103400,#103401,#103402,#103403,
#103404,#103405,#103406,#103407,#103408,#103409,#103410,#103411,#103412,
#103413,#103414,#103415,#103416,#103417,#103418,#103419,#103420,#103421,
#103422,#103423,#103424,#103425,#103426,#103427,#103428,#103429,#103430,
#103431,#103432,#103433,#103434,#103435,#103436,#103437,#103438,#103439,
#103440,#103441,#103442,#103443,#103444,#103445,#103446,#103447,#103448,
#103449,#103450,#103451,#103452,#103453,#103454,#103455,#103456,#103457,
#103458,#103459,#103460,#103461,#103462,#103463,#103464,#103465,#103466,
#103467,#103468,#103469,#103470,#103471,#103472,#103473,#103474,#103475,
#103476,#103477,#103478,#103479,#103480,#103481,#103482,#103483,#103484,
#103485,#103486,#103487,#103488,#103489,#103490,#103491,#103492,#103493,
#103494,#103495,#103496,#103497,#103498,#103499,#103500,#103501,#103502,
#103503,#103504,#103505,#103506,#103507,#103508,#103509,#103510,#103511,
#103512,#103513,#103514,#103515,#103516,#103517,#103518,#103519,#103520,
#103521,#103522,#103523,#103524,#103525,#103526,#103527,#103528,#103529,
#103530,#103531,#103532,#103533,#103534,#103535,#103536,#103537,#103538,
#103539,#103540,#103541,#103542,#103543,#103544,#103545,#103546,#103547,
#103548,#103549,#103550,#103551,#103552,#103553,#103554,#103555,#103556,
#103557,#103558,#103559,#103560,#103561,#103562,#103563,#103564,#103565,
#103566,#103567,#103568,#103569,#103570,#103571,#103572,#103573,#103574,
#103575,#103576,#103577,#103578,#103579,#103580,#103581,#103582,#103583,
#103584,#103585,#103586,#103587,#103588,#103589,#103590,#103591,#103592,
#103593,#103594,#103595,#103596,#103597,#103598,#103599,#103600,#103601,
#103602,#103603,#103604,#103605,#103606,#103607,#103608,#103609,#103610,
#103611,#103612,#103613,#103614,#103615,#103616,#103617,#103618,#103619,
#103620,#103621,#103622,#103623,#103624,#103625,#103626,#103627,#103628,
#103629,#103630,#103631,#103632,#103633,#103634,#103635,#103636,#103637,
#103638,#103639,#103640,#103641,#103642,#103643,#103644,#103645,#103646,
#103647,#103648,#103649,#103650,#103651,#103652,#103653,#103654,#103655,
#103656,#103657,#103658,#103659,#103660,#103661,#103662,#103663,#103664,
#103665,#103666,#103667,#103668,#103669,#103670,#103671,#103672,#103673,
#103674,#103675,#103676,#103677,#103678,#103679,#103680,#103681,#103682,
#103683,#103684,#103685,#103686,#103687,#103688,#103689,#103690,#103691,
#103692,#103693,#103694,#103695,#103696,#103697,#103698,#103699,#103700,
#103701,#103702,#103703,#103704,#103705,#103706,#103707,#103708,#103709,
#103710,#103711,#103712,#103713,#103714,#103715,#103716,#103717,#103718,
#103719,#103720,#103721,#103722,#103723,#103724,#103725,#103726,#103727,
#103728,#103729,#103730,#103731,#103732,#103733,#103734,#103735,#103736,
#103737,#103738,#103739,#103740,#103741,#103742,#103743,#103744,#103745,
#103746,#103747,#103748,#103749,#103750,#103751,#103752,#103753,#103754,
#103755,#103756,#103757,#103758,#103759,#103760,#103761,#103762,#103763,
#103764,#103765,#103766,#103767,#103768,#103769,#103770,#103771,#103772,
#103773,#103774,#103775,#103776,#103777,#103778,#103779,#103780,#103781,
#103782,#103783,#103784,#103785,#103786,#103787,#103788,#103789,#103790,
#103791,#103792,#103793,#103794,#103795,#103796,#103797,#103798,#103799,
#103800,#103801,#103802,#103803,#103804,#103805,#103806,#103807,#103808,
#103809,#103810,#103811,#103812,#103813,#103814,#103815,#103816,#103817,
#103818,#103819,#103820,#103821,#103822,#103823,#103824,#103825,#103826,
#103827,#103828,#103829,#103830,#103831,#103832,#103833,#103834,#103835,
#103836,#103837,#103838,#103839,#103840,#103841,#103842,#103843,#103844,
#103845,#103846,#103847,#103848,#103849,#103850,#103851,#103852,#103853,
#103854,#103855,#103856,#103857,#103858,#103859,#103860,#103861,#103862,
#103863,#103864,#103865,#103866,#103867,#103868,#103869,#103870,#103871,
#103872,#103873,#103874,#103875,#103876,#103877,#103878,#103879,#103880,
#103881,#103882,#103883,#103884,#103885,#103886,#103887,#103888,#103889,
#103890,#103891,#103892,#103893,#103894,#103895,#103896,#103897,#103898,
#103899,#103900,#103901,#103902,#103903,#103904,#103905,#103906,#103907,
#103908,#103909,#103910,#103911,#103912,#103913,#103914,#103915,#103916,
#103917,#103918,#103919,#103920,#103921,#103922,#103923,#103924,#103925,
#103926,#103927,#103928,#103929,#103930,#103931,#103932,#103933,#103934,
#103935,#103936,#103937,#103938,#103939,#103940,#103941,#103942,#103943,
#103944,#103945,#103946,#103947,#103948,#103949,#103950,#103951,#103952,
#103953,#103954,#103955,#103956,#103957,#103958,#103959,#103960,#103961,
#103962,#103963,#103964,#103965,#103966,#103967,#103968,#103969,#103970,
#103971,#103972,#103973,#103974,#103975,#103976,#103977,#103978,#103979,
#103980,#103981,#103982,#103983,#103984,#103985,#103986,#103987,#103988,
#103989,#103990,#103991,#103992,#103993,#103994,#103995,#103996,#103997,
#103998,#103999,#104000,#104001,#104002,#104003,#104004,#104005,#104006,
#104007,#104008,#104009,#104010,#104011,#104012,#104013,#104014,#104015,
#104016,#104017,#104018,#104019,#104020,#104021,#104022,#104023,#104024,
#104025,#104026,#104027,#104028,#104029,#104030,#104031,#104032,#104033,
#104034,#104035,#104036,#104037,#104038,#104039,#104040,#104041,#104042,
#104043,#104044,#104045,#104046,#104047,#104048,#104049,#104050,#104051,
#104052,#104053,#104054,#104055,#104056,#104057,#104058,#104059,#104060,
#104061,#104062,#104063,#104064,#104065,#104066,#104067,#104068,#104069,
#104070,#104071,#104072,#104073,#104074,#104075,#104076,#104077,#104078,
#104079,#104080,#104081,#104082,#104083,#104084,#104085,#104086,#104087,
#104088,#104089,#104090,#104091,#104092,#104093,#104094,#104095,#104096,
#104097,#104098,#104099,#104100,#104101,#104102,#104103,#104104,#104105,
#104106,#104107,#104108,#104109,#104110,#104111,#104112,#104113,#104114,
#104115,#104116,#104117,#104118,#104119,#104120,#104121,#104122,#104123,
#104124,#104125,#104126,#104127,#104128,#104129,#104130,#104131,#104132,
#104133,#104134,#104135,#104136,#104137,#104138,#104139,#104140,#104141,
#104142,#104143,#104144,#104145,#104146,#104147,#104148,#104149,#104150,
#104151,#104152,#104153,#104154,#104155,#104156,#104157,#104158,#104159,
#104160,#104161,#104162,#104163,#104164,#104165,#104166,#104167,#104168,
#104169,#104170,#104171,#104172,#104173,#104174,#104175,#104176,#104177,
#104178,#104179,#104180,#104181,#104182,#104183,#104184,#104185,#104186,
#104187,#104188,#104189,#104190,#104191,#104192,#104193,#104194,#104195,
#104196,#104197,#104198,#104199,#104200,#104201,#104202,#104203,#104204,
#104205,#104206,#104207,#104208,#104209,#104210,#104211,#104212,#104213,
#104214,#104215,#104216,#104217,#104218,#104219,#104220,#104221,#104222,
#104223,#104224,#104225,#104226,#104227,#104228,#104229,#104230,#104231,
#104232,#104233,#104234,#104235,#104236,#104237,#104238,#104239,#104240,
#104241,#104242,#104243,#104244,#104245,#104246,#104247,#104248,#104249,
#104250,#104251,#104252,#104253,#104254,#104255,#104256,#104257,#104258,
#104259,#104260,#104261,#104262,#104263,#104264,#104265,#104266,#104267,
#104268,#104269,#104270,#104271,#104272,#104273,#104274,#104275,#104276,
#104277,#104278,#104279,#104280,#104281,#104282,#104283,#104284,#104285,
#104286,#104287,#104288,#104289,#104290,#104291,#104292,#104293,#104294,
#104295,#104296,#104297,#104298,#104299,#104300,#104301,#104302,#104303,
#104304,#104305,#104306,#104307,#104308,#104309,#104310,#104311,#104312,
#104313,#104314,#104315,#104316,#104317,#104318,#104319,#104320,#104321,
#104322,#104323,#104324,#104325,#104326,#104327,#104328,#104329,#104330,
#104331,#104332,#104333,#104334,#104335,#104336,#104337,#104338,#104339,
#104340,#104341,#104342,#104343,#104344,#104345,#104346,#104347,#104348,
#104349,#104350,#104351,#104352,#104353,#104354,#104355,#104356,#104357,
#104358,#104359,#104360,#104361,#104362,#104363,#104364,#104365,#104366,
#104367,#104368,#104369,#104370,#104371,#104372,#104373,#104374,#104375,
#104376,#104377,#104378,#104379,#104380,#104381,#104382,#104383,#104384,
#104385,#104386,#104387,#104388,#104389,#104390,#104391,#104392,#104393,
#104394,#104395,#104396,#104397,#104398,#104399,#104400,#104401,#104402,
#104403,#104404,#104405,#104406,#104407,#104408,#104409,#104410,#104411,
#104412,#104413,#104414,#104415,#104416,#104417,#104418,#104419,#104420,
#104421,#104422,#104423,#104424,#104425,#104426,#104427,#104428,#104429,
#104430,#104431,#104432,#104433,#104434,#104435,#104436,#104437,#104438,
#104439,#104440,#104441,#104442,#104443,#104444,#104445,#104446,#104447,
#104448,#104449,#104450,#104451,#104452,#104453,#104454,#104455,#104456,
#104457,#104458,#104459,#104460,#104461,#104462,#104463,#104464,#104465,
#104466,#104467,#104468,#104469,#104470,#104471,#104472,#104473,#104474,
#104475,#104476,#104477,#104478,#104479,#104480,#104481,#104482,#104483,
#104484,#104485,#104486,#104487,#104488,#104489,#104490,#104491,#104492,
#104493,#104494,#104495,#104496,#104497,#104498,#104499,#104500,#104501,
#104502,#104503,#104504,#104505,#104506,#104507,#104508,#104509,#104510,
#104511,#104512,#104513,#104514,#104515,#104516,#104517,#104518,#104519,
#104520,#104521,#104522,#104523,#104524,#104525,#104526,#104527,#104528,
#104529,#104530,#104531,#104532,#104533,#104534,#104535,#104536,#104537,
#104538,#104539,#104540,#104541,#104542,#104543,#104544,#104545,#104546,
#104547,#104548,#104549,#104550,#104551,#104552,#104553,#104554,#104555,
#104556,#104557,#104558,#104559,#104560,#104561,#104562,#104563,#104564,
#104565,#104566,#104567,#104568,#104569,#104570,#104571,#104572,#104573,
#104574,#104575,#104576,#104577,#104578,#104579,#104580,#104581,#104582,
#104583,#104584,#104585,#104586,#104587,#104588,#104589,#104590,#104591,
#104592,#104593,#104594,#104595,#104596,#104597,#104598,#104599,#104600,
#104601,#104602,#104603,#104604,#104605,#104606,#104607,#104608,#104609,
#104610,#104611,#104612,#104613,#104614,#104615,#104616,#104617,#104618,
#104619,#104620,#104621,#104622,#104623,#104624,#104625,#104626,#104627,
#104628,#104629,#104630,#104631,#104632,#104633,#104634,#104635,#104636,
#104637,#104638,#104639,#104640,#104641,#104642,#104643,#104644,#104645,
#104646,#104647,#104648,#104649,#104650,#104651,#104652,#104653,#104654,
#104655,#104656,#104657,#104658,#104659,#104660,#104661,#104662,#104663,
#104664,#104665,#104666,#104667,#104668,#104669,#104670,#104671,#104672,
#104673,#104674,#104675,#104676,#104677,#104678,#104679,#104680,#104681,
#104682,#104683,#104684,#104685,#104686,#104687,#104688,#104689,#104690,
#104691,#104692,#104693,#104694,#104695,#104696,#104697,#104698,#104699,
#104700,#104701,#104702,#104703,#104704,#104705,#104706,#104707,#104708,
#104709,#104710,#104711,#104712,#104713,#104714,#104715,#104716,#104717,
#104718,#104719,#104720,#104721,#104722,#104723,#104724,#104725,#104726,
#104727,#104728,#104729,#104730,#104731,#104732,#104733,#104734,#104735,
#104736,#104737,#104738,#104739,#104740,#104741,#104742,#104743,#104744,
#104745,#104746,#104747,#104748,#104749,#104750,#104751,#104752,#104753,
#104754,#104755,#104756,#104757,#104758,#104759,#104760,#104761,#104762,
#104763,#104764,#104765,#104766,#104767,#104768,#104769,#104770,#104771,
#104772,#104773,#104774,#104775,#104776,#104777,#104778,#104779,#104780,
#104781,#104782,#104783,#104784,#104785,#104786,#104787,#104788,#104789,
#104790,#104791,#104792,#104793,#104794,#104795,#104796,#104797,#104798,
#104799,#104800,#104801,#104802,#104803,#104804,#104805,#104806,#104807,
#104808,#104809,#104810,#104811,#104812,#104813,#104814,#104815,#104816,
#104817,#104818,#104819,#104820,#104821,#104822,#104823,#104824,#104825,
#104826,#104827,#104828,#104829,#104830,#104831,#104832,#104833,#104834,
#104835,#104836,#104837,#104838,#104839,#104840,#104841,#104842,#104843,
#104844,#104845,#104846,#104847,#104848,#104849,#104850,#104851,#104852,
#104853,#104854,#104855,#104856,#104857,#104858,#104859,#104860,#104861,
#104862,#104863,#104864,#104865,#104866,#104867,#104868,#104869,#104870,
#104871,#104872,#104873,#104874,#104875,#104876,#104877,#104878,#104879,
#104880,#104881,#104882,#104883,#104884,#104885,#104886,#104887,#104888,
#104889,#104890,#104891,#104892,#104893,#104894,#104895,#104896,#104897,
#104898,#104899,#104900,#104901,#104902,#104903,#104904,#104905,#104906,
#104907,#104908,#104909,#104910,#104911,#104912,#104913,#104914,#104915,
#104916,#104917,#104918,#104919,#104920,#104921,#104922,#104923,#104924,
#104925,#104926,#104927,#104928,#104929,#104930,#104931,#104932,#104933,
#104934,#104935,#104936,#104937,#104938,#104939,#104940,#104941,#104942,
#104943,#104944,#104945,#104946,#104947,#104948,#104949,#104950,#104951,
#104952,#104953,#104954,#104955,#104956,#104957,#104958,#104959,#104960,
#104961,#104962,#104963,#104964,#104965,#104966,#104967,#104968,#104969,
#104970,#104971,#104972,#104973,#104974,#104975,#104976,#104977,#104978,
#104979,#104980,#104981,#104982,#104983,#104984,#104985,#104986,#104987,
#104988,#104989,#104990,#104991,#104992,#104993,#104994,#104995,#104996,
#104997,#104998,#104999,#105000,#105001,#105002,#105003,#105004,#105005,
#105006,#105007,#105008,#105009,#105010,#105011,#105012,#105013,#105014,
#105015,#105016,#105017,#105018,#105019,#105020,#105021,#105022,#105023,
#105024,#105025,#105026,#105027,#105028,#105029,#105030,#105031,#105032,
#105033,#105034,#105035,#105036,#105037,#105038,#105039,#105040,#105041,
#105042,#105043,#105044,#105045,#105046,#105047,#105048,#105049,#105050,
#105051,#105052,#105053,#105054,#105055,#105056,#105057,#105058,#105059,
#105060,#105061,#105062,#105063,#105064,#105065,#105066,#105067,#105068,
#105069,#105070,#105071,#105072,#105073,#105074,#105075,#105076,#105077,
#105078,#105079,#105080,#105081,#105082,#105083,#105084,#105085,#105086,
#105087,#105088,#105089,#105090,#105091,#105092,#105093,#105094,#105095,
#105096,#105097,#105098,#105099,#105100,#105101,#105102,#105103,#105104,
#105105,#105106,#105107,#105108,#105109,#105110,#105111,#105112,#105113,
#105114,#105115,#105116,#105117,#105118,#105119,#105120,#105121,#105122,
#105123,#105124,#105125,#105126,#105127,#105128,#105129,#105130,#105131,
#105132,#105133,#105134,#105135,#105136,#105137,#105138,#105139,#105140,
#105141,#105142,#105143,#105144,#105145,#105146,#105147,#105148,#105149,
#105150,#105151,#105152,#105153,#105154,#105155,#105156,#105157,#105158,
#105159,#105160,#105161,#105162,#105163,#105164,#105165,#105166,#105167,
#105168,#105169,#105170,#105171,#105172,#105173,#105174,#105175,#105176,
#105177,#105178,#105179,#105180,#105181,#105182,#105183,#105184,#105185,
#105186,#105187,#105188,#105189,#105190,#105191,#105192,#105193,#105194,
#105195,#105196,#105197,#105198,#105199,#105200,#105201,#105202,#105203,
#105204,#105205,#105206,#105207,#105208,#105209,#105210,#105211,#105212,
#105213,#105214,#105215,#105216,#105217,#105218,#105219,#105220,#105221,
#105222,#105223,#105224,#105225,#105226,#105227,#105228,#105229,#105230,
#105231,#105232,#105233,#105234,#105235,#105236,#105237,#105238,#105239,
#105240,#105241,#105242,#105243,#105244,#105245,#105246,#105247,#105248,
#105249,#105250,#105251,#105252,#105253,#105254,#105255,#105256,#105257,
#105258,#105259,#105260,#105261,#105262,#105263,#105264,#105265,#105266,
#105267,#105268,#105269,#105270,#105271,#105272,#105273,#105274,#105275,
#105276,#105277,#105278,#105279,#105280,#105281,#105282,#105283,#105284,
#105285,#105286,#105287,#105288,#105289,#105290,#105291,#105292,#105293,
#105294,#105295,#105296,#105297,#105298,#105299,#105300,#105301,#105302,
#105303,#105304,#105305,#105306,#105307,#105308,#105309,#105310,#105311,
#105312,#105313,#105314,#105315,#105316,#105317,#105318,#105319,#105320,
#105321,#105322,#105323,#105324,#105325,#105326,#105327,#105328,#105329,
#105330,#105331,#105332,#105333,#105334,#105335,#105336,#105337,#105338,
#105339,#105340,#105341,#105342,#105343,#105344,#105345,#105346,#105347,
#105348,#105349,#105350,#105351,#105352,#105353,#105354,#105355,#105356,
#105357,#105358,#105359,#105360,#105361,#105362,#105363,#105364,#105365,
#105366,#105367,#105368,#105369,#105370,#105371,#105372,#105373,#105374,
#105375,#105376,#105377,#105378,#105379,#105380,#105381,#105382,#105383,
#105384,#105385,#105386,#105387,#105388,#105389,#105390,#105391,#105392,
#105393,#105394,#105395,#105396,#105397,#105398,#105399,#105400,#105401,
#105402,#105403,#105404,#105405,#105406,#105407,#105408,#105409,#105410,
#105411,#105412,#105413,#105414,#105415,#105416,#105417,#105418,#105419,
#105420,#105421,#105422,#105423,#105424,#105425,#105426,#105427,#105428,
#105429,#105430,#105431,#105432,#105433,#105434,#105435,#105436,#105437,
#105438,#105439,#105440,#105441,#105442,#105443,#105444,#105445,#105446,
#105447,#105448,#105449,#105450,#105451,#105452,#105453,#105454,#105455,
#105456,#105457,#105458,#105459,#105460,#105461,#105462,#105463,#105464,
#105465,#105466,#105467,#105468,#105469,#105470,#105471,#105472,#105473,
#105474,#105475,#105476,#105477,#105478,#105479,#105480,#105481,#105482,
#105483,#105484,#105485,#105486,#105487,#105488,#105489,#105490,#105491,
#105492,#105493,#105494,#105495,#105496,#105497,#105498,#105499,#105500,
#105501,#105502,#105503,#105504,#105505,#105506,#105507,#105508,#105509,
#105510,#105511,#105512,#105513,#105514,#105515,#105516,#105517,#105518,
#105519,#105520,#105521,#105522,#105523,#105524,#105525,#105526,#105527,
#105528,#105529,#105530,#105531,#105532,#105533,#105534,#105535,#105536,
#105537,#105538,#105539,#105540,#105541,#105542,#105543,#105544,#105545,
#105546,#105547,#105548,#105549,#105550,#105551,#105552,#105553,#105554,
#105555,#105556,#105557,#105558,#105559,#105560,#105561,#105562,#105563,
#105564,#105565,#105566,#105567,#105568,#105569,#105570,#105571,#105572,
#105573,#105574,#105575,#105576,#105577,#105578,#105579,#105580,#105581,
#105582,#105583,#105584,#105585,#105586,#105587,#105588,#105589,#105590,
#105591,#105592,#105593,#105594,#105595,#105596,#105597,#105598,#105599,
#105600,#105601,#105602,#105603,#105604,#105605,#105606,#105607,#105608,
#105609,#105610,#105611,#105612,#105613,#105614,#105615,#105616,#105617,
#105618,#105619,#105620,#105621,#105622,#105623,#105624,#105625,#105626,
#105627,#105628,#105629,#105630,#105631,#105632,#105633,#105634,#105635,
#105636,#105637,#105638,#105639,#105640,#105641,#105642,#105643,#105644,
#105645,#105646,#105647,#105648,#105649,#105650,#105651,#105652,#105653,
#105654,#105655,#105656,#105657,#105658,#105659,#105660,#105661,#105662,
#105663,#105664,#105665,#105666,#105667,#105668,#105669,#105670,#105671,
#105672,#105673,#105674,#105675,#105676,#105677,#105678,#105679,#105680,
#105681,#105682,#105683,#105684,#105685,#105686,#105687,#105688,#105689,
#105690,#105691,#105692,#105693,#105694,#105695,#105696,#105697,#105698,
#105699,#105700,#105701,#105702)),.UNSPECIFIED.,.F.,.F.,.F.,(2,2),(4,1,
1,1,1,1,1,1,1,1,1,1,1,1,1,1,1,1,1,1,1,1,1,1,1,1,1,1,1,1,1,1,1,1,1,1,1,1,
1,1,1,1,1,1,1,1,1,1,1,1,1,1,1,1,1,1,1,1,1,1,1,1,1,1,1,1,1,1,1,1,1,1,1,1,
1,1,1,1,1,1,1,1,1,1,1,1,1,1,1,1,1,1,1,1,1,1,1,1,1,1,1,1,1,1,1,1,1,1,1,1,
1,1,1,1,1,1,1,1,1,1,1,1,1,1,1,1,1,1,1,1,1,1,1,1,1,1,1,1,1,1,1,1,1,1,1,1,
1,1,1,1,1,1,1,1,1,1,1,1,1,1,1,1,1,1,1,1,1,1,1,1,1,1,1,1,1,1,1,1,1,1,1,1,
1,1,1,1,1,1,1,1,1,1,1,1,1,1,1,1,1,1,1,1,1,1,1,1,1,1,1,1,1,1,1,1,1,1,1,1,
1,1,1,1,1,1,1,1,1,1,1,1,1,1,1,1,1,1,1,1,1,1,1,1,1,1,1,1,1,1,1,1,1,1,1,1,
1,1,1,1,1,1,1,1,1,1,1,1,1,1,1,1,1,1,1,1,1,1,1,1,1,1,1,1,1,1,1,1,1,1,1,1,
1,1,1,1,1,1,1,1,1,1,1,1,1,1,1,1,1,1,1,1,1,1,1,1,1,1,1,1,1,1,1,1,1,1,1,1,
1,1,1,1,1,1,1,1,1,1,1,1,1,1,1,1,1,1,1,1,1,1,1,1,1,1,1,1,1,1,1,1,1,1,1,1,
1,1,1,1,1,1,1,1,1,1,1,1,1,1,1,1,1,1,1,1,1,1,1,1,1,1,1,1,1,1,1,1,1,1,1,1,
1,1,1,1,1,1,1,1,1,1,1,1,1,1,1,1,1,1,1,1,1,1,1,1,1,1,1,1,1,1,1,1,1,1,1,1,
1,1,1,1,1,1,1,1,1,1,1,1,1,1,1,1,1,1,1,1,1,1,1,1,1,1,1,1,1,1,1,1,1,1,1,1,
1,1,1,1,1,1,1,1,1,1,1,1,1,1,1,1,1,1,1,1,1,1,1,1,1,1,1,1,1,1,1,1,1,1,1,1,
1,1,1,1,1,1,1,1,1,1,1,1,1,1,1,1,1,1,1,1,1,1,1,1,1,1,1,1,1,1,1,1,1,1,1,1,
1,1,1,1,1,1,1,1,1,1,1,1,1,1,1,1,1,1,1,1,1,1,1,1,1,1,1,1,1,1,1,1,1,1,1,1,
1,1,1,1,1,1,1,1,1,1,1,1,1,1,1,1,1,1,1,1,1,1,1,1,1,1,1,1,1,1,1,1,1,1,1,1,
1,1,1,1,1,1,1,1,1,1,1,1,1,1,1,1,1,1,1,1,1,1,1,1,1,1,1,1,1,1,1,1,1,1,1,1,
1,1,1,1,1,1,1,1,1,1,1,1,1,1,1,1,1,1,1,1,1,1,1,1,1,1,1,1,1,1,1,1,1,1,1,1,
1,1,1,1,1,1,1,1,1,1,1,1,1,1,1,1,1,1,1,1,1,1,1,1,1,1,1,1,1,1,1,1,1,1,1,1,
1,1,1,1,1,1,1,1,1,1,1,1,1,1,1,1,1,1,1,1,1,1,1,1,1,1,1,1,1,1,1,1,1,1,1,1,
1,1,1,1,1,1,1,1,1,1,1,1,1,1,1,1,1,1,1,1,1,1,1,1,1,1,1,1,1,1,1,1,1,1,1,1,
1,1,1,1,1,1,1,1,1,1,1,1,1,1,1,1,1,1,1,1,1,1,1,1,1,1,1,1,1,1,1,1,1,1,1,1,
1,1,1,1,1,1,1,1,1,1,1,1,1,1,1,1,1,1,1,1,1,1,1,1,1,1,1,1,1,1,1,1,1,1,1,1,
1,1,1,1,1,1,1,1,1,1,1,1,1,1,1,1,1,1,1,1,1,1,1,1,1,1,1,1,1,1,1,1,1,1,1,1,
1,1,1,1,1,1,1,1,1,1,1,1,1,1,1,1,1,1,1,1,1,1,1,1,1,1,1,1,1,1,1,1,1,1,1,1,
1,1,1,1,1,1,1,1,1,1,1,1,1,1,1,1,1,1,1,1,1,1,1,1,1,1,1,1,1,1,1,1,1,1,1,1,
1,1,1,1,1,1,1,1,1,1,1,1,1,1,1,1,1,1,1,1,1,1,1,1,1,1,1,1,1,1,1,1,1,1,1,1,
1,1,1,1,1,1,1,1,1,1,1,1,1,1,1,1,1,1,1,1,1,1,1,1,1,1,1,1,1,1,1,1,1,1,1,1,
1,1,1,1,1,1,1,1,1,1,1,1,1,1,1,1,1,1,1,1,1,1,1,1,1,1,1,1,1,1,1,1,1,1,1,1,
1,1,1,1,1,1,1,1,1,1,1,1,1,1,1,1,1,1,1,1,1,1,1,1,1,1,1,1,1,1,1,1,1,1,1,1,
1,1,1,1,1,1,1,1,1,1,1,1,1,1,1,1,1,1,1,1,1,1,1,1,1,1,1,1,1,1,1,1,1,1,1,1,
1,1,1,1,1,1,1,1,1,1,1,1,1,1,1,1,1,1,1,1,1,1,1,1,1,1,1,1,1,1,1,1,1,1,1,1,
1,1,1,1,1,1,1,1,1,1,1,1,1,1,1,1,1,1,1,1,1,1,1,1,1,1,1,1,1,1,1,1,1,1,1,1,
1,1,1,1,1,1,1,1,1,1,1,1,1,1,1,1,1,1,1,1,1,1,1,1,1,1,1,1,1,1,1,1,1,1,1,1,
1,1,1,1,1,1,1,1,1,1,1,1,1,1,1,1,1,1,1,1,1,1,1,1,1,1,1,1,1,1,1,1,1,1,1,1,
1,1,1,1,1,1,1,1,1,1,1,1,1,1,1,1,1,1,1,1,1,1,1,1,1,1,1,1,1,1,1,1,1,1,1,1,
1,1,1,1,1,1,1,1,1,1,1,1,1,1,1,1,1,1,1,1,1,1,1,1,1,1,1,1,1,1,1,1,1,1,1,1,
1,1,1,1,1,1,1,1,1,1,1,1,1,1,1,1,1,1,1,1,1,1,1,1,1,1,1,1,1,1,1,1,1,1,1,1,
1,1,1,1,1,1,1,1,1,1,1,1,1,1,1,1,1,1,1,1,1,1,1,1,1,1,1,1,1,1,1,1,1,1,1,1,
1,1,1,1,1,1,1,1,1,1,1,1,1,1,1,1,1,1,1,1,1,1,1,1,1,1,1,1,1,1,1,1,1,1,1,1,
1,1,1,1,1,1,1,1,1,1,1,1,1,1,1,1,1,1,1,1,1,1,1,1,1,1,1,1,1,1,1,1,1,1,1,1,
1,1,1,1,1,1,1,1,1,1,1,1,1,1,1,1,1,1,1,1,1,1,1,1,1,1,1,1,1,1,1,1,1,1,1,1,
1,1,1,1,1,1,1,1,1,1,1,1,1,1,1,1,1,1,1,1,1,1,1,1,1,1,1,1,1,1,1,1,1,1,1,1,
1,1,1,1,1,1,1,1,1,1,1,1,1,1,1,1,1,1,1,1,1,1,1,1,1,1,1,1,1,1,1,1,1,1,1,1,
1,1,1,1,1,1,1,1,1,1,1,1,1,1,1,1,1,1,1,1,1,1,1,1,1,1,1,1,1,1,1,1,1,1,1,1,
1,1,1,1,1,1,1,1,1,1,1,1,1,1,1,1,1,1,1,1,1,1,1,1,1,1,1,1,1,1,1,1,1,1,1,1,
1,1,1,1,1,1,1,1,1,1,1,1,1,1,1,1,1,1,1,1,1,1,1,1,1,1,1,1,1,1,1,1,1,1,1,1,
1,1,1,1,1,1,1,1,1,1,1,1,1,1,1,1,1,1,1,1,1,1,1,1,1,1,1,1,1,1,1,1,1,1,1,1,
1,1,1,1,1,1,1,1,1,1,1,1,1,1,1,1,1,1,1,1,1,1,1,1,1,1,1,1,1,1,1,1,1,1,1,1,
1,1,1,1,1,1,1,1,1,1,1,1,1,1,1,1,1,1,1,1,1,1,1,1,1,1,1,1,1,1,1,1,1,1,1,1,
1,1,1,1,1,1,1,1,1,1,1,1,1,1,1,1,1,1,1,1,1,1,1,1,1,1,1,1,1,1,1,1,1,1,1,1,
1,1,1,1,1,1,1,1,1,1,1,1,1,1,1,1,1,1,1,1,1,1,1,1,1,1,1,1,1,1,1,1,1,1,1,1,
1,1,1,1,1,1,1,1,1,1,1,1,1,1,1,1,1,1,1,1,1,1,1,1,1,1,1,1,1,1,1,1,1,1,1,1,
1,1,1,1,1,1,1,1,1,1,1,1,1,1,1,1,1,1,1,1,1,1,1,1,1,1,1,1,1,1,1,1,1,1,1,1,
1,1,1,1,1,1,1,1,1,1,1,1,1,1,1,1,1,1,1,1,1,1,1,1,1,1,1,1,1,1,1,1,1,1,1,1,
1,1,1,1,1,1,1,1,1,1,1,1,1,1,1,1,1,1,1,1,1,1,1,1,1,1,1,1,1,1,1,1,1,1,1,1,
1,1,1,1,1,1,1,1,1,1,1,1,1,1,1,1,1,1,1,1,1,1,1,1,1,1,1,1,1,1,1,1,1,1,1,1,
1,1,1,1,1,1,1,1,1,1,1,1,1,1,1,1,1,1,1,1,1,1,1,1,1,1,1,1,1,1,1,1,1,1,1,1,
1,1,1,1,1,1,1,1,1,1,1,1,1,1,1,1,1,1,1,1,1,1,1,1,1,1,1,1,1,1,1,1,1,1,1,1,
1,1,1,1,1,1,1,1,1,1,1,1,1,1,1,1,1,1,1,1,1,1,1,1,1,1,1,1,1,1,1,1,1,1,1,1,
1,1,1,1,1,1,1,1,1,1,1,1,1,1,1,1,1,1,1,1,1,1,1,1,1,1,1,1,1,1,1,1,1,1,1,1,
1,1,1,1,1,1,1,1,1,1,1,1,1,1,1,1,1,1,1,1,1,1,1,1,1,1,1,1,1,1,1,1,1,1,1,1,
1,1,1,1,1,1,1,1,1,1,1,1,1,1,1,1,1,1,1,1,1,1,1,1,1,1,1,1,1,1,1,1,1,1,1,1,
1,1,1,1,1,1,1,1,1,1,1,1,1,1,1,1,1,1,1,1,1,1,1,1,1,1,1,1,1,1,1,1,1,1,1,1,
1,1,1,1,1,1,1,1,1,1,1,1,1,1,1,1,1,1,1,1,1,1,1,1,1,1,1,1,1,1,1,1,1,1,1,1,
1,1,1,1,1,1,1,1,1,1,1,1,1,1,1,1,1,1,1,1,1,1,1,1,1,1,1,1,1,1,1,1,1,1,1,1,
1,1,1,1,1,1,1,1,1,1,1,1,1,1,1,1,1,1,1,1,1,1,1,1,1,1,1,1,1,1,1,1,1,1,1,1,
1,1,1,1,1,1,1,1,1,1,1,1,1,1,1,1,1,1,1,1,1,1,1,1,1,1,1,1,1,1,1,1,1,1,1,1,
1,1,1,1,1,1,1,1,1,1,1,1,1,1,1,1,1,1,1,1,1,1,1,1,1,1,1,1,1,1,1,1,1,1,1,1,
1,1,1,1,1,1,1,1,1,1,1,1,1,1,1,1,1,1,1,1,1,1,1,1,1,1,1,1,1,1,1,1,1,1,1,1,
1,1,1,1,1,1,1,1,1,1,1,1,1,1,1,1,1,1,1,1,1,1,1,1,1,1,1,1,1,1,1,1,1,1,1,1,
1,1,1,1,1,1,1,1,1,1,1,1,1,1,1,1,1,1,1,1,1,1,1,1,1,1,1,1,1,1,1,1,1,1,1,1,
1,1,1,1,1,1,1,1,1,1,1,1,1,1,1,1,1,1,1,1,1,1,1,1,1,1,1,1,1,1,1,1,1,1,1,1,
1,1,1,1,1,1,1,1,1,1,1,1,1,1,1,1,1,1,1,1,1,1,1,1,1,1,1,1,1,1,1,1,1,1,1,1,
1,1,1,1,1,1,1,1,1,1,1,1,1,1,1,1,1,1,1,1,1,1,1,1,1,1,1,1,1,1,1,1,1,1,1,1,
1,1,1,1,1,1,1,1,1,1,1,1,1,1,1,1,1,1,1,1,1,1,1,1,1,1,1,1,1,1,1,1,1,1,1,1,
1,1,1,1,1,1,1,1,1,1,1,1,1,1,1,1,1,1,1,1,1,1,1,1,1,1,1,1,1,1,1,1,1,1,1,1,
1,1,1,1,1,1,1,1,1,1,1,1,1,1,1,1,1,1,1,1,1,1,1,1,1,1,1,1,1,1,1,1,1,1,1,1,
1,1,1,1,1,1,1,1,1,1,1,1,1,1,1,1,1,1,1,1,1,1,1,1,1,1,1,1,1,1,1,1,1,1,1,1,
1,1,1,1,1,1,1,1,1,1,1,1,1,1,1,1,1,1,1,1,1,1,1,1,1,1,1,1,1,1,1,1,1,1,1,1,
1,1,1,1,1,1,1,1,1,1,1,1,1,1,1,1,1,1,1,1,1,1,1,1,1,1,1,1,1,1,1,1,1,1,1,1,
1,1,1,1,1,1,1,1,1,1,1,1,1,1,1,1,1,1,1,1,1,1,1,1,1,1,1,1,1,1,1,1,1,1,1,1,
1,1,1,1,1,1,1,1,1,1,1,1,1,1,1,1,1,1,1,1,1,1,1,1,1,1,1,1,1,1,1,1,1,1,1,1,
1,1,1,1,1,1,1,1,1,1,1,1,1,1,1,1,1,1,1,1,1,1,1,1,1,1,1,1,1,1,1,1,1,1,1,1,
1,1,1,1,1,1,1,1,1,1,1,1,1,1,1,1,1,1,1,1,1,1,1,1,1,1,1,1,1,1,1,1,1,1,1,1,
1,1,1,1,1,1,1,1,1,1,1,1,1,1,1,1,1,1,1,1,1,1,1,1,1,1,1,1,1,1,1,1,1,1,1,1,
1,1,1,1,1,1,1,1,1,1,1,1,1,1,1,1,1,1,1,1,1,1,1,1,1,1,1,1,1,1,1,1,1,1,1,1,
1,1,1,1,1,1,1,1,1,1,1,1,1,1,1,1,1,1,1,1,1,1,1,1,1,1,1,1,1,1,1,1,1,1,1,1,
1,1,1,1,1,1,1,1,1,1,1,1,1,1,1,1,1,1,1,1,1,1,1,1,1,1,1,1,1,1,1,1,1,1,1,1,
1,1,1,1,1,1,1,1,1,1,1,1,1,1,1,1,1,1,1,1,1,1,1,1,1,1,1,1,1,1,1,1,1,1,1,1,
1,1,1,1,1,1,1,1,1,1,1,1,1,1,1,1,1,1,1,1,1,1,1,1,1,1,1,1,1,1,1,1,1,1,1,1,
1,1,1,1,1,1,1,1,1,1,1,1,1,1,1,1,1,1,1,1,1,1,1,1,1,1,1,1,1,1,1,1,1,1,1,1,
1,1,1,1,1,1,1,1,1,1,1,1,1,1,1,1,1,1,1,1,1,1,1,1,1,1,1,1,1,1,1,1,1,1,1,1,
1,1,1,1,1,1,1,1,1,1,1,1,1,1,1,1,1,1,1,1,1,1,1,1,1,1,1,1,1,1,1,1,1,1,1,1,
1,1,1,1,1,1,1,1,1,1,1,1,1,1,1,1,1,1,1,1,1,1,1,1,1,1,1,1,1,1,1,1,1,1,1,1,
1,1,1,1,1,1,1,1,1,1,1,1,1,1,1,1,1,1,1,1,1,1,1,1,4),(-0.58309518948453,0.),
(0.,0.869746702321014,1.7394931589914,2.60923976624962,3.47983908319159,
4.35043840179749,5.22018503077054,6.08993165951504,6.95967828799171,7.82942491616733,
8.69917154401062,9.56891817149224,10.4395174886835,11.3101168056706,12.179863432132,
13.049610058144,13.9193566836854,14.7891033087372,15.6588499332817,16.5285965573034,
17.3991958717975,18.2697951860185,18.7046684974166,19.1395418086746,19.5744151197912,
20.0092884307654,20.4441617415962,20.8790350522825,21.7487816732187,22.1836549834672,
22.6185282935685,23.0534016035221,23.4882749133276,23.9231482229848,24.3588742245859,
24.794600226187,25.2294735355468,26.0992201538203,26.5340934627341,26.9689667714994,
27.4038400801166,27.838713388586,28.2735866969081,28.7084600050832,29.143333313112,
29.5782066209952,30.0130799287334,30.4479532363275,30.8828265437783,31.3185525442794,
31.7542785447804,32.1891518519474,32.6240251589741,33.0588984658616,33.4937717726112,
33.928645079224,34.3635183857014,34.7983916920448,35.2332649982556,35.6681383043353,
36.1030116102854,36.5378849161076,36.9727582218035,37.4076315273749,37.8425048328235,
38.2782308323341,38.7139568318446,39.1488301370532,39.5837034421446,40.0185767471208,
40.4534500519838,40.8883233567357,41.3231966613787,41.7580699659148,42.1929432703463,
42.6278165746754,43.0626898789044,43.4975631830356,43.9324364870714,44.3673097910142,
44.8021830948664,45.2379090935952,45.673635092324,46.1085083960024,46.5433816995978,
46.9782550031127,47.4131283065497,47.8480016099115,48.2828749132006,48.7177482164198,
49.1526215195718,49.5874948226593,50.0223681256851,50.457241428652,50.8921147315628,
51.3269880344203,51.7618613372274,52.197587335454,52.6333133336805,53.0681866363954,
53.5030599390685,53.9379332417027,54.3728065443011,54.8076798468664,55.2425531494018,
55.6774264519101,56.1122997543943,56.5471730568575,56.9820463593026,57.4169196617326,
57.8517929641506,58.2866662665595,58.7215395689624,59.157265567009,59.5929915650557,
60.0278648674556,60.4627381698584,60.8976114722673,61.3324847746853,61.7673580771153,
62.2022313795604,62.6371046820236,63.0719779845079,63.5068512870162,63.9417245895516,
64.376597892117,64.8114711947155,65.2463444973499,65.6812178000231,66.1169437982275,
66.5526697964318,66.9875430991915,67.4224164019987,67.8572897048563,68.2921630077673,
68.7270363107343,69.1619096137603,69.5967829168479,70.0316562200001,70.4665295232194,
70.9014028265087,71.3362761298705,71.7711494333077,72.2060227368227,72.6408960404182,
73.0766220391044,73.5123480377905,73.9472213415547,74.382094645407,74.8169679493499,
75.2518412533859,75.6867145575172,76.1215878617464,76.5564611660756,76.9913344705072,
77.4262077750435,77.8610810796866,78.2959543844386,78.7308276893018,79.1657009942781,
79.6005742993696,80.0363002988208,80.4720262982719,80.9068996035997,81.3417729090484,
81.7766462146199,82.211519520316,82.6463928261383,83.0812661320886,83.5161394381684,
83.9510127443794,84.3858860507229,84.8207593572004,85.2556326638134,85.6905059705631,
86.1253792774507,86.5602525844776,86.995978584908,87.4317045853384,87.8665778926469,
88.3014512000977,88.7363245076919,89.1711978154302,89.6060711233134,90.0409444313423,
90.4758177395175,90.9106910478396,91.345564356309,91.7804376649263,92.2153109736917,
92.6501842826055,93.085057591668,93.5199309008791,93.9556569024059,94.3913829039327,
94.8262562134414,95.2611295230986,95.6960028329042,96.1308761428578,96.5657494529591,
97.0006227632077,97.4354960736028,97.870369384144,98.3052426948304,98.7401160056612,
99.1749893166354,99.6098626277522,100.04473593901,100.915335253024,101.351061255639,
101.785934567313,102.220807879124,102.655681191068,103.090554503145,103.525427815353,
104.395174440154,105.264921065453,105.699794378283,106.134667691232,106.569541004295,
107.004414317471,107.8750136343,108.745612951339,109.615359578629,110.485106206296,
111.354852834309,112.224599462639,113.094346091254,113.964092720119,114.834692038763,
115.705291357499,116.575037986826,117.444784616267,118.314531245777,119.184277875311,
120.054024504821,120.923771134261,121.794370453112,122.66496977189,123.534716400968,
124.404463029834,125.274209658448,126.143956286779,127.013702914792,127.883449542458,
128.754048859798,129.624648176939,130.494394803617,131.364141429857,132.233888055637,
133.103634680937,133.973381305737,134.843127930023,135.71372724472,136.584326559147,
137.019199870684,137.454073182083,137.888946493341,138.323819804458,139.193566426263,
140.063313047491,140.498186357887,140.933059668136,141.367932978237,141.802806288191,
142.237679597997,142.673405599673,143.109131601348,143.544004910857,143.978878220217,
144.413751529429,144.848624838491,145.283498147405,145.718371456171,146.153244764789,
146.588118073258,147.022991381581,147.457864689756,147.892737997785,148.327611305669,
148.762484613407,149.197357921002,149.633083921574,150.068809922147,150.503683229455,
150.938556536623,151.37342984365,151.808303150538,152.243176457288,152.678049763901,
153.112923070379,153.547796376722,153.982669682934,154.417542989014,154.852416294964,
155.287289600787,155.722162906483,156.157036212055,156.592762211626,157.028488211198,
157.463361516526,157.898234821735,158.333108126826,158.767981431803,159.202854736666,
159.637728041419,160.072601346062,160.507474650599,160.94234795503,161.37722125936,
161.812094563589,162.246967867721,162.681841171757,163.1167144757,163.552440474473,
163.988166473247,164.423039777011,164.85791308069,165.292786384286,165.727659687801,
166.162532991238,166.597406294601,167.03227959789,167.46715290111,167.902026204262,
168.33689950735,168.771772810376,169.206646113343,169.641519416254,170.076392719112,
170.512118717363,170.947844715614,171.382718018374,171.817591321089,172.252464623762,
172.687337926397,173.122211228996,173.557084531561,173.991957834097,174.426831136606,
174.86170443909,175.296577741554,175.731451044,176.16632434643,176.601197648848,
177.036070951258,177.471796949306,177.907522947355,178.342396249755,178.777269552155,
179.212142854558,179.647016156968,180.081889459386,180.516762761816,180.951636064262,
181.386509366726,181.82138266921,182.256255971719,182.691129274255,183.12600257682,
183.560875879419,183.995749182054,184.431475180237,184.867201178421,185.302074481136,
185.736947783896,186.171821086704,186.606694389561,187.041567692473,187.47644099544,
187.911314298466,188.346187601554,188.781060904706,189.215934207926,189.650807511215,
190.085680814577,190.520554118015,190.95542742153,191.391153420175,191.82687941882,
192.261752722499,192.696626026263,193.131499330116,193.566372634059,194.001245938095,
194.436119242227,194.870992546456,195.305865850785,195.740739155217,196.175612459754,
196.610485764397,197.045359069149,197.480232374013,197.915105678989,198.350831678382,
198.786557677775,199.221430982984,199.656304288312,200.091177593761,200.526050899333,
200.960924205029,201.395797510852,201.830670816802,202.265544122882,202.700417429093,
203.135290735437,203.570164041915,204.005037348528,204.439910655278,204.874783962166,
205.310509962526,205.746235962887,206.181109270054,206.615982577363,207.050855884814,
207.485729192409,207.920602500147,208.355475808031,208.79034911606,209.225222424235,
209.660095732558,210.094969041027,210.529842349645,210.96471565841,211.399588967324,
211.834462276387,212.27018827784,212.705914279292,213.140787588653,213.575660898161,
214.010534207819,214.880280827579,215.31515413768,215.750027447929,216.184900758324,
216.619774068866,217.054647379553,217.489520690384,218.359267312475,219.22986662628,
219.665592628826,220.100465940363,220.535339252038,220.970212563848,221.83995918787,
222.709705812416,223.579452437468,224.014325750179,224.44919906301,225.318945689022,
226.189545005688,227.060144322571,227.929890949664,228.799637577146,229.66938420499,
230.539130833166,231.408877461643,232.278624090388,233.149223408954,234.019822727623,
234.889569356878,235.759315986267,236.629062615749,237.498809245277,238.368555874806,
239.238302504287,240.108901823183,240.979501142017,241.849247771189,242.718994400167,
243.588741028911,244.458487657389,245.328234285565,246.197980913409,247.068580230891,
247.939179548182,248.80892617507,249.678672801532,250.548419427545,251.418166053087,
252.287912678139,253.157659302684,254.028258617581,254.898857932211,255.333731243885,
255.768604555423,256.203477866821,256.63835117808,257.508097800171,258.377844421689,
258.812717732231,259.247591042627,259.682464352876,260.117337662977,260.552210972931,
260.987936974682,261.858536286089,262.293409595598,262.728282904958,263.16315621417,
263.598029523233,264.032902832147,264.467776140913,264.902649449531,265.337522758001,
265.772396066323,266.207269374499,266.642142682528,267.077015990412,267.511889298151,
267.947615298795,268.383341299439,268.81821460689,269.2530879142,269.687961221367,
270.122834528394,270.557707835282,270.992581142032,271.427454448646,271.862327755124,
272.297201061468,272.732074367679,273.166947673759,273.60182097971,274.036694285533,
274.471567591229,274.907293590862,275.343019590495,275.777892895944,276.212766201272,
276.647639506481,277.082512811573,277.51738611655,277.952259421414,278.387132726166,
278.82200603081,279.256879335346,279.691752639779,280.126625944108,280.561499248338,
280.996372552469,281.431245856506,281.866971855324,282.302697854143,282.737571157996,
283.172444461761,283.60731776544,284.042191069036,284.477064372551,284.911937675989,
285.346810979351,285.781684282641,286.216557585861,286.651430889013,287.086304192101,
287.521177495128,287.956050798095,288.390924101007,288.826650099283,289.262376097559,
289.697249400366,290.132122703127,290.566996005842,291.001869308516,291.43674261115,
291.871615913749,292.306489216315,292.741362518851,293.17623582136,293.611109123845,
294.045982426308,294.480855728754,294.915729031185,295.350602333603,295.786328331655,
296.222054329707,296.65692763211,297.091800934511,297.526674236911,297.961547539314,
298.396420841724,298.831294144142,299.266167446573,299.701040749018,300.135914051482,
300.570787353967,301.005660656476,301.440533959012,301.875407261578,302.310280564177,
302.746006562341,303.181732560506,303.616605863179,304.051479165895,304.486352468655,
304.921225771462,305.35609907432,305.790972377232,306.225845680199,306.660718983226,
307.095592286314,307.530465589466,307.965338892686,308.400212195976,308.835085499338,
309.269958802776,309.705684801381,310.141410799985,310.576284103581,311.01115740726,
311.446030711025,311.880904014878,312.315777318821,312.750650622858,313.185523926989,
313.620397231219,314.055270535549,314.490143839981,314.925017144517,315.359890449161,
315.794763753913,316.229637058777,316.665363058112,317.101089057448,317.53596236254,
317.970835667749,318.405708973077,318.840582278526,319.275455584098,319.710328889795,
320.145202195618,320.580075501568,321.014948807648,321.44982211386,321.884695420204,
322.319568726682,322.754442033295,323.189315340045,323.625041340336,324.060767340628,
324.495640647655,324.930513954822,325.365387262131,325.800260569583,326.235133877177,
326.670007184916,327.1048804928,327.539753800829,327.974627109005,328.409500417327,
328.844373725797,329.279247034415,329.714120343181,330.148993652095,330.584719653474,
331.020445654852,331.455318964064,331.890192273424,332.325065582933,332.759938892591,
333.194812202397,333.629685512351,334.064558822453,334.499432132702,334.934305443098,
335.369178753639,335.804052064326,336.673798686132,337.108671997249,337.544397999725,
337.980124002201,338.4149973136,338.849870625137,339.284743936812,340.154490560568,
341.024237184854,341.459110497191,341.893983809655,342.328857122244,342.763730434955,
343.633477060735,344.504076377234,345.374675693955,346.244422320844,347.114168948136,
347.983915575803,348.853662203817,349.723408832148,350.593155460764,351.463754779246,
352.334354097839,353.204100727012,354.07384735634,354.943593985781,355.813340615292,
356.683087244827,357.552833874338,358.423433193272,359.294032512154,360.163779141409,
361.033525770489,361.903272399355,362.77301902797,363.642765656301,364.512512284316,
365.383111601936,366.253710919371,367.123457546465,367.993204173143,368.862950799383,
369.732697425164,370.602444050463,371.472190675265,372.342789990359,373.21338930519,
373.648262617,374.083135928675,374.952882551611,375.822629173987,376.257502484962,
376.692375795793,377.12724910648,377.562122417021,377.996995727417,378.431869037666,
378.866742347767,379.302468349591,379.738194351416,380.173067661222,380.607940970879,
381.042814280388,381.477687589749,381.91256089896,382.347434208023,382.782307516937,
383.217180825703,383.652054134321,384.086927442791,384.521800751113,384.956674059289,
385.391547367318,385.826420675202,386.262146675918,386.697872676635,387.13274598423,
387.567619291681,388.00249259899,388.437365906157,388.872239213185,389.307112520073,
389.741985826823,390.176859133436,390.611732439914,391.046605746258,391.48147905247,
391.91635235855,392.351225664501,392.786098970323,393.221824970019,393.657550969714,
394.092424275286,394.527297580735,394.962170886063,395.397044191272,395.831917496364,
396.266790801341,396.701664106204,397.136537410957,397.5714107156,398.006284020137,
398.441157324569,398.876030628899,399.310903933128,399.74577723726,400.181503236126,
400.617229234991,401.052102538934,401.486975842787,401.921849146551,402.356722450231,
402.791595753827,403.226469057342,403.66134236078,404.096215664142,404.531088967432,
404.965962270651,405.400835573804,405.835708876892,406.270582179918,406.705455482886,
407.141181481189,407.576907479491,408.01178078235,408.446654085157,408.881527387917,
409.316400690633,409.751273993306,410.186147295941,410.62102059854,411.055893901106,
411.490767203642,411.925640506151,412.360513808636,412.795387111099,413.230260413545,
413.665133715976,414.100859714032,414.536585712088,414.971459014498,415.406332316901,
415.841205619301,416.276078921702,416.710952224105,417.145825526515,417.580698828933,
418.015572131364,418.45044543381,418.885318736273,419.320192038758,419.755065341267,
420.189938643803,420.624811946369,421.060537944515,421.496263942662,421.931137245297,
422.36601054797,422.800883850686,423.235757153446,423.670630456253,424.105503759112,
424.540377062023,424.975250364991,425.410123668017,425.844996971105,426.279870274258,
426.714743577477,427.149616880767,427.584490184129,428.020216182695,428.455942181261,
428.890815484776,429.325688788373,429.760562092052,430.195435395816,430.630308699669,
431.065182003612,431.500055307649,431.93492861178,432.36980191601,432.80467522034,
433.239548524772,433.674421829309,434.109295133952,434.544168438705,434.979894437984,
435.415620437262,435.850493742239,436.285367047331,436.72024035254,437.155113657869,
437.589986963318,438.024860268889,438.459733574586,438.894606880409,439.32948018636,
439.76435349244,440.199226798651,440.634100104995,441.068973411473,441.503846718087,
441.939572718309,442.375298718531,442.810172025419,443.245045332447,443.679918639614,
444.114791946923,444.549665254374,444.984538561969,445.419411869708,445.854285177591,
446.289158485621,446.724031793796,447.158905102119,447.593778410589,448.028651719207,
448.463525027973,448.899251029277,449.334977030581,449.769850339644,450.639596958216,
451.074470267725,451.509343577383,451.944216887189,452.379090197143,452.813963507244,
453.248836817493,453.683710127889,454.118583438431,454.553456749117,454.988330059949,
455.423203370923,455.858929373329,456.294655375734,456.729528686993,457.164401998391,
457.599275309929,458.469021933414,458.90389524536,459.338768557437,459.773641869646,
460.208515181983,460.643388494447,461.078261807036,461.948008432578,462.818607748906,
463.689207065461,464.55895369214,465.428700319234,466.298446946716,467.16819357456,
468.037940202737,468.907686831215,469.778286149605,470.648885468116,471.518632097196,
472.388378726451,473.258125355841,474.127871985322,474.997618614851,475.86736524438,
476.737964563343,477.608563882265,478.478310511593,479.348057140765,480.217803769743,
481.087550398488,481.957297026966,482.827043655142,483.697642972895,484.568242290469,
485.43798891776,486.307735544649,487.177482171112,488.047228797125,488.916975422667,
489.78672204772,490.657321363009,491.09304736596,491.527920678038,492.397667301793,
493.267413925005,494.137160547663,494.57203385878,495.006907169755,495.441780480586,
495.876653791273,496.311527101814,496.74640041221,497.616999724357,498.052725726255,
498.487599036209,498.922472346015,499.357345655673,499.792218965182,500.227092274542,
500.661965583754,501.096838892816,501.531712201731,501.966585510497,502.401458819114,
502.836332127584,503.271205435907,503.706078744082,504.140952052112,504.576678052901,
505.01240405369,505.447277361429,505.882150669023,506.317023976474,506.751897283783,
507.186770590951,507.621643897978,508.056517204866,508.491390511616,508.92626381823,
509.361137124708,509.796010431052,510.230883737263,510.665757043344,511.100630349294,
511.536356349053,511.972082348811,512.406955654506,512.841828960076,513.276702265523,
513.711575570849,514.146448876056,514.581322181146,515.016195486121,515.451068790983,
515.885942095733,516.320815400375,516.75568870491,517.19056200934,517.625435313668,
518.060308617896,518.496034616807,518.931760615718,519.366633919752,519.801507223694,
520.236380527545,520.671253831307,521.106127134985,521.541000438579,521.975873742092,
522.410747045528,522.845620348888,523.280493652176,523.715366955394,524.150240258545,
524.585113561631,525.019986864656,525.455712862985,525.891438861313,526.326312164223,
526.761185467079,527.196058769885,527.630932072643,528.065805375356,528.500678678029,
528.935551980661,529.370425283258,529.805298585822,530.240171888356,530.675045190863,
531.109918493346,531.544791795808,531.979665098252,532.415391096312,532.851117094373,
533.285990396789,533.720863699197,534.155737001598,534.590610303997,535.025483606395,
535.460356908796,535.895230211204,536.330103513621,536.764976816049,537.199850118493,
537.634723420955,538.069596723438,538.504470025945,538.93934332848,539.375069326608,
539.810795324736,540.245668627333,540.680541929966,541.115415232637,541.550288535351,
541.985161838109,542.420035140915,542.854908443771,543.28978174668,543.724655049646,
544.15952835267,544.594401655757,545.029274958907,545.464148262125,545.899021565413,
546.334747563939,546.770473562465,547.205346865901,547.640220169415,548.075093473009,
548.509966776686,548.944840080449,549.3797133843,549.814586688241,550.249459992276,
550.684333296405,551.119206600633,551.554079904961,551.988953209391,552.423826513926,
552.858699818567,553.294425817789,553.73015181701,554.165025121872,554.599898426846,
555.034771731937,555.469645037144,555.90451834247,556.339391647917,556.774264953487,
557.209138259182,557.644011565003,558.078884870951,558.51375817703,558.948631483239,
559.383504789581,559.818378096058,560.254104096209,560.689830096361,561.12470340311,
561.559576709996,561.994450017021,562.429323324187,562.864196631494,563.299069938943,
563.733943246536,564.168816554273,564.603689862154,565.038563170182,565.473436478355,
565.908309786676,566.343183095144,566.77805640376,567.213782404988,567.649508406216,
568.084381715128,568.519255024189,568.954128333399,569.389001642757,569.823874952264,
570.258748261921,570.693621571725,571.128494881677,571.563368191777,572.433114812417,
572.867988122957,573.302861433642,573.737734744471,574.173460746804,574.609186749136,
575.044060060251,575.913806682904,576.783553306113,577.218426617922,577.653299929865,
578.08817324194,578.523046554147,579.392793178944,580.26253980424,581.13313912039,
581.568865123709,582.003738436771,582.87348506323,583.743231690115,584.612978317402,
585.482724945065,586.352471573076,587.222218201403,588.092817519691,588.963416838109,
589.833163467083,590.702910096251,591.572656725575,592.442403355013,593.31214998452,
594.181896614051,595.05249593303,595.92309525198,596.792841881366,597.662588510618,
598.532335139693,599.402081768556,600.271828397167,601.141575025495,602.012174343369,
602.882773661074,603.752520288553,604.622266915642,605.492013542317,606.361760168553,
607.23150679433,608.101253419626,608.971852735101,609.842452050322,610.71219867434,
611.581945297822,612.451691920754,612.886565232011,613.321438543126,613.756311854099,
614.191185164928,615.060931786153,615.931531098516,616.367257100486,616.802130410586,
617.237003720538,617.671877030342,618.106750339998,618.541623649505,618.976496958863,
619.411370268073,619.846243577134,620.281116886046,620.71599019481,621.150863503426,
621.585736811894,622.020610120214,622.455483428388,622.891209429248,623.326935430108,
623.761808737989,624.196682045726,624.631555353319,625.066428660769,625.501301968075,
625.936175275241,626.371048582266,626.805921889153,627.240795195901,627.675668502512,
628.110541808988,628.54541511533,628.98028842154,629.415161727618,629.850887727438,
630.286613727259,630.72148703308,631.156360338774,631.591233644344,632.026106949791,
632.460980255118,632.895853560325,633.330726865415,633.76560017039,634.200473475251,
634.635346780002,635.070220084644,635.505093389179,635.939966693609,636.374839997937,
636.810565996897,637.246291995857,637.681165299986,638.116038604021,638.550911907962,
638.985785211813,639.420658515576,639.855531819253,640.290405122847,640.725278426361,
641.160151729796,641.595025033157,642.029898336444,642.464771639662,642.899644942813,
643.334518245899,643.770244244257,644.205970242616,644.640843545581,645.075716848491,
645.510590151347,645.945463454153,646.380336756911,646.815210059625,647.250083362296,
647.684956664929,648.119829967526,648.55470327009,648.989576572624,649.424449875131,
649.859323177614,650.294196480076,650.729922478144,651.165648476212,651.600521778641,
652.035395081057,652.470268383465,652.905141685866,653.340014988265,653.774888290663,
654.209761593065,654.644634895472,655.079508197889,655.514381500318,655.949254802762,
656.384128105224,656.819001407706,657.253874710213,657.689600708326,658.12532670644,
658.560200009004,658.995073311601,659.429946614234,659.864819916905,660.299693219619,
660.734566522377,661.169439825183,661.604313128039,662.039186430948,662.474059733914,
662.908933036938,663.343806340025,663.778679643175,664.213552946393,664.649278944883,
665.085004943373,665.519878246733,665.954751550169,666.389624853683,666.824498157277,
667.259371460954,667.694244764717,668.129118068568,668.563991372509,668.998864676544,
669.433737980674,669.868611284901,670.303484589229,670.738357893659,671.173231198194,
671.608957197361,672.044683196528,672.479556501278,672.91442980614,673.349303111115,
673.784176416205,674.219049721412,674.653923026738,675.088796332185,675.523669637755,
675.95854294345,676.393416249271,676.82828955522,677.263162861298,677.698036167508,
678.13290947385,678.568635473934,679.004361474018,679.439234780629,679.874108087377,
680.308981394264,680.743854701289,681.178728008455,681.613601315762,682.048474623211,
682.483347930804,682.91822123854,683.353094546422,683.78796785445,684.222841162623,
684.657714470944,685.092587779412,685.528313780566,685.96403978172,686.398913090483,
686.833786399396,687.268659708457,687.703533017666,688.138406327025,688.573279636532,
689.008152946187,689.443026255992,689.877899565944,690.312772876043,690.74764618629,
691.182519496684,691.617392807224,692.052266117909,692.487992120169,692.92371812243,
693.358591433403,694.228338055774,694.663211367171,695.098084678707,695.532957990379,
695.967831302188,696.402704614131,696.837577926207,697.707324550749,698.577071175797,
699.011944488507,699.447670491767,699.883396495028,700.318269807975,701.188016434211,
702.057763060886,702.927509687976,703.797256315454,704.667002943295,705.536749571467,
706.407348889651,707.277948207973,708.147694836835,709.017441465911,709.887188095163,
710.756934724548,711.626681354026,712.496427983551,713.367027302543,714.237626621516,
715.107373250954,715.977119880277,716.846866509446,717.716613138419,718.586359767161,
719.456106395635,720.32670571363,721.197305031464,722.067051659126,722.936798286414,
723.806544913299,724.676291539758,725.546038165767,726.415784791305,727.286384106969,
728.156983422381,729.026730046663,729.896476670415,730.331349982088,730.766223293624,
731.201096605021,731.635969916278,732.505716538366,733.37546315988,733.81033647042,
734.246062472462,734.681788474505,735.116661784752,735.551535094852,735.986408404804,
736.421281714608,736.856155024264,737.291028333771,737.72590164313,738.160774952339,
738.5956482614,739.030521570312,739.465394879076,739.900268187692,740.33514149616,
740.77001480448,741.205740805414,741.641466806347,742.076340114374,742.511213422256,
742.946086729993,743.380960037585,743.815833345035,744.250706652341,744.685579959507,
745.120453266533,745.555326573419,745.990199880167,746.425073186778,746.859946493254,
747.294819799596,747.729693105806,748.165419105691,748.601145105576,749.036018411525,
749.470891717346,749.90576502304,750.34063832861,750.775511634057,751.210384939384,
751.645258244591,752.080131549682,752.515004854656,752.949878159518,753.384751464269,
753.81962476891,754.254498073445,754.689371377875,755.125097376885,755.560823375895,
755.995696680123,756.430569984253,756.865443288287,757.300316592228,757.735189896079,
758.170063199842,758.604936503519,759.039809807113,759.474683110627,759.909556414062,
760.344429717423,760.779303020711,761.214176323929,761.649049627079,762.084775625469,
762.520501623858,762.955374926883,763.390248229848,763.825121532758,764.259994835614,
764.694868138419,765.129741441178,765.564614743891,765.999488046563,766.434361349196,
766.869234651793,767.304107954357,767.738981256891,768.173854559398,768.608727861881,
769.044453859958,769.480179858035,769.915053160479,770.349926462907,770.784799765324,
771.219673067731,771.654546370133,772.089419672531,772.52429297493,772.959166277331,
773.394039579739,773.828912882155,774.263786184584,774.698659487028,775.13353278949,
775.568406091973,776.004132090072,776.439858088172,776.874731390706,777.30960469327,
777.744477995867,778.1793512985,778.614224601171,779.049097903885,779.483971206643,
779.918844509449,780.353717812305,780.788591115215,781.22346441818,781.658337721205,
782.093211024291,782.528084327442,782.963810325897,783.399536324352,783.834409627639,
784.269282931,784.704156234435,785.139029537949,785.573902841543,786.00877614522,
786.443649448983,786.878522752834,787.313396056775,787.74826936081,788.183142664939,
788.618015969167,789.052889273495,789.487762577925,789.923488577038,790.359214576152,
790.794087880793,791.228961185544,791.663834490406,792.098707795381,792.533581100471,
792.968454405678,793.403327711004,793.838201016451,794.273074322021,794.707947627716,
795.142820933537,795.577694239486,796.012567545564,796.447440851774,796.883166851791,
797.318892851808,797.753766158284,798.188639464895,798.623512771643,799.058386078529,
799.493259385555,799.92813269272,800.363006000027,800.797879307477,801.232752615069,
801.667625922806,802.102499230688,802.537372538715,802.972245846889,803.40711915521,
803.84284515629,804.27857115737,804.713444465985,805.148317774749,805.583191083662,
806.018064392723,806.452937701933,806.887811011291,807.322684320798,808.192430940258,
808.62730425021,809.06217756031,809.497050870557,809.931924180951,810.36679749149,
810.802523493679,811.238249495867,811.673122806697,812.542869428785,812.977742740041,
813.412616051438,813.847489362974,814.282362674646,814.717235986455,815.152109298398,
816.021855922681,816.891602547478,817.326475860065,817.762201863265,818.197927866466,
818.632801179295,819.502547805304,820.372294431763,821.242041058648,822.111787685935,
822.981534313598,823.851280941609,824.721880259681,825.5924795779,826.462226206642,
827.331972835616,828.201719464785,829.071466094109,829.941212723546,830.810959353053,
831.681558672047,832.552157991036,833.421904620514,834.2916512499,835.161397879151,
836.031144508226,836.900891137089,837.770637765701,838.641237083811,839.511836401767,
840.381583029608,841.251329657086,842.121076284176,842.990822910851,843.860569537087,
844.730316162863,845.600915478712,846.471514794314,847.341261418855,848.211008042874,
848.645881354683,849.080754666356,849.515627977891,849.950501289288,850.82024791166,
851.689994533462,852.124867844147,852.560593846263,852.996319848379,853.431193158772,
853.866066469019,854.300939779119,855.170686398875,855.605559708531,856.040433018038,
856.475306327397,856.910179636606,857.345052945667,857.77992625458,858.214799563344,
858.64967287196,859.084546180427,859.520272181434,859.95599818244,860.390871490614,
860.825744798641,861.260618106523,861.69549141426,862.130364721852,862.565238029302,
863.000111336609,863.434984643774,863.8698579508,864.304731257686,864.739604564434,
865.174477871045,865.609351177521,866.044224483863,866.479950483814,866.915676483765,
867.350549789843,867.785423095792,868.220296401613,868.655169707307,869.090043012877,
869.524916318325,869.959789623651,870.394662928858,870.829536233948,871.264409538923,
871.699282843785,872.134156148535,872.569029453177,873.003902757712,873.439628756773,
873.875354755834,874.310228060162,874.745101364389,875.179974668519,875.614847972553,
876.049721276495,876.484594580346,876.919467884108,877.354341187786,877.78921449138,
878.224087794893,878.658961098329,879.093834401689,879.528707704977,879.963581008195,
880.399307006616,880.835033005038,881.269906308124,881.704779611148,882.139652914114,
882.574526217024,883.00939951988,883.444272822685,883.879146125444,884.314019428157,
884.748892730829,885.183766033462,885.618639336059,886.053512638623,886.488385941157,
886.923259243664,887.358985241751,887.794711239839,888.2295845423,888.664457844744,
889.099331147173,889.534204449589,889.969077751997,890.403951054398,890.838824356797,
891.273697659195,891.708570961597,892.143444264004,892.578317566421,893.01319086885,
893.448064171293,893.882937473755,894.318663471843,894.75438946993,895.189262772437,
895.624136074971,896.059009377535,896.493882680132,896.928755982765,897.363629285437,
897.798502588151,898.233375890909,898.668249193715,899.103122496571,899.53799579948,
899.972869102446,900.40774240547,900.842615708556,901.278341706978,901.714067705399,
902.148941008617,902.583814311905,903.018687615265,903.453560918701,903.888434222214,
904.323307525808,904.758180829485,905.193054133248,905.627927437099,906.06280074104,
906.497674045075,906.932547349205,907.367420653433,907.80229395776,908.238019956821,
908.673745955883,909.108619260417,909.543492565059,909.978365869809,910.413239174671,
910.848112479646,911.282985784736,911.717859089943,912.152732395269,912.587605700716,
913.022479006287,913.457352311981,913.892225617802,914.327098923751,914.761972229829,
915.19769822978,915.633424229731,916.068297536072,916.503170842548,916.93804414916,
917.372917455908,917.807790762794,918.24266406982,918.677537376985,919.112410684292,
919.547283991742,919.982157299334,920.417030607071,920.851903914953,921.28677722298,
921.721650531154,922.15737653216,922.593102533167,923.027975841635,923.46284915025,
923.897722459014,924.332595767926,924.767469076987,925.202342386197,925.637215695556,
926.072089005063,926.506962314719,926.941835624523,927.376708934475,927.811582244575,
928.246455554822,928.681328865215,929.117054867331,929.987654180132,930.422527490961,
930.857400801934,931.292274113049,931.727147424306,932.162020735703,932.596894047238,
933.46664067072,934.336387294739,934.771260606945,935.20613391928,935.641007231742,
936.076733234882,936.94733255073,937.817079176507,938.686825802743,939.556572429418,
940.426319056508,941.296065683986,942.165812311827,943.036411629783,943.907010947893,
944.776757576505,945.646504205367,946.516250834443,947.385997463694,948.25574409308,
949.125490722558,949.996090041546,950.86668936054,951.736435990048,952.606182619485,
953.475929248809,954.345675877978,955.215422506951,956.085169135693,956.955768453912,
957.826367771985,958.696114399995,959.565861027658,960.435607654946,961.305354281831,
962.175100908289,963.044847534298,963.915446850328,964.786046166116,965.655792790913,
966.525539415195,966.960412727138,967.395286038947,968.265032662155,969.134779284809,
969.569652595924,970.004525906897,970.439399217726,970.875125219914,971.310851222103,
971.745724532643,972.615471153283,973.485217773335,973.920091083139,974.354964392795,
974.789837702302,975.22471101166,975.65958432087,976.094457629931,976.529330938844,
976.964204247608,977.399077556223,977.834803557303,978.270529558383,978.705402866704,
979.140276174877,979.575149482905,980.010022790786,980.444896098523,980.879769406116,
981.314642713565,981.749516020872,982.184389328038,982.619262635063,983.05413594195,
983.489009248698,983.923882555309,984.358755861785,984.794481861802,985.230207861819,
985.665081168029,986.099954474107,986.534827780056,986.969701085877,987.404574391571,
987.839447697141,988.274321002589,988.709194307915,989.144067613122,989.578940918212,
990.013814223187,990.448687528048,990.883560832799,991.31843413744,991.754160136554,
992.189886135667,992.624759440097,993.059632744425,993.494506048653,993.929379352783,
994.364252656817,994.799125960758,995.233999264609,995.668872568372,996.103745872049,
996.538619175643,996.973492479157,997.408365782593,997.843239085953,998.278112389241,
998.713838387696,999.149564386151,999.584437689301,1000.01931099239,1000.45418429541,
1000.88905759838,1001.32393090129,1001.75880420414,1002.19367750695,1002.62855080971,
1003.06342411242,1003.49829741509,1003.93317071773,1004.36804402032,1004.80291732289,
1005.23779062542,1005.67351662352,1006.10924262162,1006.5441159241,1006.97898922656,
1007.41386252901,1007.84873583144,1008.28360913385,1008.71848243626,1009.15335573866,
1009.58822904106,1010.02310234346,1010.45797564586,1010.89284894827,1011.32772225069,
1011.76259555311,1012.19746885556,1012.63319485364,1013.06892085171,1013.5037941542,
1013.9386674567,1014.37354075924,1014.8084140618,1015.2432873644,1015.67816066703,
1016.1130339697,1016.54790727242,1016.98278057517,1017.41765387798,1017.85252718084,
1018.28740048375,1018.72227378671,1019.15714708974,1019.59287308813,1020.02859908651,
1020.46347238967,1020.89834569288,1021.33321899617,1021.76809229953,1022.20296560297,
1022.63783890648,1023.07271221007,1023.50758551375,1023.94245881752,1024.37733212137,
1024.81220542531,1025.24707872935,1025.68195203348,1026.11682533771,1026.55255133672,
1026.98827733573,1027.42315064016,1027.8580239447,1028.29289724934,1028.72777055409,
1029.16264385896,1029.59751716393,1030.03239046902,1030.46726377423,1030.90213707956,
1031.33701038501,1031.77188369058,1032.20675699628,1032.6416303021,1033.07650360805,
1033.51222960793,1033.94795560782,1034.38282891403,1034.81770222038,1035.25257552685,
1035.68744883347,1036.12232214022,1036.5571954471,1036.99206875413,1037.4269420613,
1037.86181536861,1038.29668867606,1038.73156198365,1039.16643529139,1039.60130859927,
1040.0361819073,1040.47190790824,1040.90763390917,1041.34250721749,1041.77738052596,
1042.21225383458,1042.64712714334,1043.08200045226,1043.95174707053,1044.38662037989,
1044.8214936894,1045.25636699906,1045.69124030886,1046.12611361882,1046.56098692892,
1046.99586023917,1047.43158624121,1047.86731224325,1048.3021855538,1048.73705886448,
1049.17193217531,1049.60680548629,1050.0416787974,1050.47655210866,1050.91142542006,
1051.78117204327,1052.21604535508,1052.65091866703,1053.0857919791,1053.52066529131,
1053.95553860365,1054.39126460673,1055.26186392239,1056.13161054793,1057.00135717395,
1057.43623048712,1057.87110380041,1058.7408504273,1059.61059705459,1060.48034368225,
1061.35094300009,1062.22154231809,1063.09128894656,1063.96103557531,1064.83078220429,
1065.70052883346,1066.57027546278,1067.44002209222,1068.3106214112,1069.18122073019,
1070.05096735972,1070.9207139892,1071.79046061859,1072.66020724785,1073.52995387693,
1074.39970050579,1075.27029982411,1076.1408991423,1077.01064577048,1077.88039239832,
1078.7501390258,1079.61988565289,1080.48963227957,1081.35937890581,1082.22997822202,
1083.100577538,1083.97032416305,1084.84007078759,1085.70981741161,1086.5795640351,
1087.44931065803,1087.88418396929,1088.31905728041,1088.75393059138,1089.18965659365,
1089.62538259591,1090.06025590659,1090.93000252753,1091.36487583778,1091.79974914788,
1092.23462245783,1092.66949576764,1093.1043690773,1093.5392423868,1093.97411569616,
1094.40898900538,1094.84386231444,1095.27873562335,1095.71360893212,1096.14933493327,
1096.58506093443,1097.0199342429,1097.45480755122,1097.88968085939,1098.32455416742,
1098.75942747531,1099.19430078305,1099.62917409064,1100.06404739809,1100.4989207054,
1100.93379401257,1101.36866731959,1101.80354062648,1102.23841393323,1102.67328723984,
1103.10901323993,1103.54473924001,1103.97961254636,1104.41448585257,1104.84935915865,
1105.2842324646,1105.71910577042,1106.15397907612,1106.58885238169,1107.02372568714,
1107.45859899246,1107.89347229767,1108.32834560276,1108.76321890774,1109.1980922126,
1109.63296551736,1110.06869151652,1110.50441751569,1110.93929082023,1111.37416412466,
1111.80903742899,1112.24391073322,1112.67878403735,1113.11365734139,1113.54853064533,
1113.98340394918,1114.41827725295,1114.85315055662,1115.28802386022,1115.72289716374,
1116.15777046717,1116.59264377053,1117.02836976903,1117.46409576752,1117.89896907074,
1118.33384237389,1118.76871567698,1119.20358898,1119.63846228297,1120.07333558588,
1120.50820888874,1120.94308219154,1121.3779554943,1121.81282879702,1122.24770209969,
1122.68257540233,1123.11744870492,1123.55232200749,1123.98804800561,1124.42377400372,
1124.85864730623,1125.29352060871,1125.72839391118,1126.16326721362,1126.59814051605,
1127.03301381847,1127.46788712088,1127.90276042328,1128.33763372568,1128.77250702808,
1129.20738033048,1129.64225363289,1130.07712693531,1130.51200023774,1130.94772623581,
1131.38345223388,1131.81832553634,1132.25319883883,1132.68807214134,1133.12294544387,
1133.55781874644,1133.99269204904,1134.42756535167,1134.86243865434,1135.29731195706,
1135.73218525982,1136.16705856263,1136.60193186548,1137.03680516839,1137.47167847136,
1137.90740446972,1138.34313046808,1138.77800377117,1139.21287707432,1139.64775037754,
1140.08262368083,1140.51749698419,1140.95237028763,1141.38724359114,1141.82211689474,
1142.25699019842,1142.69186350218,1143.12673680603,1143.56161010998,1143.99648341401,
1144.43135671814,1144.86708271711,1145.30280871607,1145.7376820204,1146.17255532483,
1146.60742862936,1147.04230193401,1147.47717523876,1147.91204854362,1148.3469218486,
1148.78179515369,1149.2166684589,1149.65154176423,1150.08641506968,1150.52128837525,
1150.95616168094,1151.39103498677,1151.82676098659,1152.26248698641,1152.69736029249,
1153.1322335987,1153.56710690504,1154.00198021152,1154.43685351813,1154.87172682488,
1155.30660013177,1155.7414734388,1156.17634674597,1156.61122005327,1157.04609336073,
1157.48096666832,1157.91583997606,1158.35071328394,1158.7864392848,1159.22216528566,
1159.65703859384,1160.09191190216,1160.52678521063,1160.96165851925,1161.39653182801,
1161.83140513693,1162.26627844599,1162.7011517552,1163.13602506456,1163.57089837407,
1164.00577168373,1164.44064499353,1164.87551830349,1165.74611761556,1166.18184361753,
1166.61671692792,1167.05159023846,1167.48646354915,1167.92133685998,1168.35621017096,
1169.22595679333,1170.09570341627,1170.53057672794,1170.96545003975,1171.4003233517,
1171.83519666377,1172.27006997598,1172.705795979,1173.57639529447,1174.44614191977,
1174.8810152326,1175.31588854555,1176.18563517179,1177.05538179847,1177.92512842556,
1178.79487505304,1179.66547437075,1180.53607368863,1181.40582031696,1182.27556694557,
1183.14531357444,1184.01506020352,1184.88480683277,1185.75455346216,1186.62515278112,
1187.4957521001,1188.36549872963,1189.23524535914,1190.10499198858,1190.97473861791,
1191.84448524708,1192.71423187606,1193.58483119448,1194.45543051277,1195.3251771411,
1196.19492376911,1197.06467039678,1197.93441702407,1198.80416365096,1199.67391027742,
1200.5445095938,1201.41510890996,1202.28485553525,1203.15460216005,1204.02434878434,
1204.89409540809,1205.76384203131,1206.1987153427,1206.63358865396,1207.06846196508,
1207.50418796741,1208.37478728058,1209.2445339018,1209.6794072122,1210.11428052245,
1210.54915383255,1210.9840271425,1211.41890045231,1211.85377376197,1212.28864707147,
1212.72352038083,1213.15839369005,1213.59326699911,1214.02814030802,1214.46386630925,
1214.89959231048,1215.3344656191,1215.76933892757,1216.20421223589,1216.63908554406,
1217.07395885209,1217.50883215998,1217.94370546771,1218.37857877531,1218.81345208276,
1219.24832539007,1219.68319869724,1220.11807200426,1220.55294531115,1220.9878186179,
1221.42354461805,1221.85927061821,1222.29414392468,1222.72901723103,1223.16389053724,
1223.59876384332,1224.03363714927,1224.46851045509,1224.90338376079,1225.33825706636,
1225.77313037181,1226.20800367713,1226.64287698234,1227.07775028743,1227.51262359241,
1227.94749689727,1228.3832228965,1228.81894889572,1229.25382220036,1229.6886955049,
1230.12356880933,1230.55844211366,1230.99331541789,1231.42818872202,1231.86306202606,
1232.29793533,1232.73280863385,1233.16768193762,1233.60255524129,1234.03742854489,
1234.4723018484,1234.90717515184,1235.34290115037,1235.7786271489,1236.21350045219,
1236.64837375541,1237.08324705856,1237.51812036165,1237.95299366467,1238.38786696764,
1238.82274027055,1239.25761357341,1239.69248687621,1240.12736017897,1240.56223348169,
1240.99710678436,1241.431980087,1241.8668533896,1242.30257938773,1242.73830538585,
1243.17317868839,1243.6080519909,1244.04292529338,1244.47779859585,1244.91267189829,
1245.34754520072,1245.78241850314,1246.21729180555,1246.65216510795,1247.08703841035,
1247.52191171275,1247.95678501515,1248.39165831756,1248.82653161998,1249.26225761804,
1249.69798361611,1250.13285691855,1250.56773022101,1251.0026035235,1251.43747682601,
1251.87235012854,1252.30722343111,1252.74209673371,1253.17697003634,1253.61184333901,
1254.04671664173,1254.48158994449,1254.9164632473,1255.35133655015,1255.78620985306,
1256.22193585139,1256.65766184973,1257.09253515275,1257.52740845584,1257.96228175899,
1258.39715506221,1258.8320283655,1259.26690166886,1259.7017749723,1260.13664827581,
1260.57152157941,1261.00639488309,1261.44126818685,1261.8761414907,1262.31101479465,
1262.74588809868,1263.1816140976,1263.61734009651,1264.05221340074,1264.48708670507,
1264.9219600095,1265.35683331403,1265.79170661868,1266.22657992343,1266.66145322829,
1267.09632653327,1267.53119983836,1267.96607314357,1268.4009464489,1268.83581975434,
1269.27069305992,1269.70556636561,1270.14129236537,1270.57701836513,1271.01189167108,
1271.44676497716,1271.88163828337,1272.31651158971,1272.75138489619,1273.1862582028,
1273.62113150955,1274.05600481644,1274.49087812347,1274.92575143063,1275.36062473794,
1275.79549804539,1276.23037135299,1276.66524466073,1277.10097066151,1277.5366966623,
1277.97156997033,1278.40644327851,1278.84131658683,1279.2761898953,1279.71106320392,
1280.14593651268,1280.5808098216,1281.01568313066,1281.45055643987,1281.88542974923,
1282.32030305874,1282.75517636839,1283.1900496782,1283.62492298815,1284.06064899005,
1284.49637499195,1284.9312483022,1285.36612161259,1285.80099492313,1286.23586823382,
1286.67074154465,1287.54048816674,1287.975361478,1288.4102347894,1288.84510810093,
1289.27998141261,1289.71485472442,1290.14972803636,1291.02032735139,1291.89092666668,
1292.32579997914,1292.76067329173,1293.19554660444,1293.63041991727,1294.50016654328,
1295.36991316974,1296.23965979663,1297.10940642392,1297.9800057415,1298.85060505925,
1299.72035168742,1300.5900983159,1301.45984494464,1302.32959157362,1303.19933820279,
1304.06908483212,1304.93968415104,1305.81028347,1306.68003009953,1307.54977672906,
1308.41952335854,1309.28926998793,1310.15901661718,1311.02876324626,1311.89936256477,
1312.76996188316,1313.63970851164,1314.50945513981,1315.37920176765,1316.24894839514,
1317.11869502223,1317.98844164891,1318.85904096546,1319.72964028179,1320.59938690733,
1321.46913353238,1322.33888015692,1323.20862678095,1323.64350009276,1324.07837340443,
1324.51324671597,1324.94812002737,1325.81871934103,1326.68931865441,1327.12419196524,
1327.55906527593,1327.99393858647,1328.42881189686,1328.86368520711,1329.29855851721,
1329.73343182716,1330.16830513697,1330.60317844663,1331.03805175614,1331.4729250655,
1331.90779837471,1332.34267168377,1332.77839768507,1333.21412368638,1333.64899699514,
1334.08387030376,1334.51874361223,1334.95361692055,1335.38849022873,1335.82336353676,
1336.25823684464,1336.69311015238,1337.12798345997,1337.56285676742,1337.99773007473,
1338.4326033819,1338.86747668892,1339.30234999581,1339.73807599603,1340.17380199625,
1340.60867530287,1341.04354860934,1341.47842191569,1341.9132952219,1342.34816852798,
1342.78304183393,1343.21791513975,1343.65278844545,1344.08766175102,1344.52253505647,
1344.95740836179,1345.392281667,1345.82715497209,1346.26202827707,1346.69775427635,
1347.13348027563,1347.56835358038,1348.00322688502,1348.43810018956,1348.87297349399,
1349.30784679832,1349.74272010255,1350.17759340668,1350.61246671072,1351.04734001466,
1351.48221331851,1351.91708662228,1352.35195992595,1352.78683322955,1353.22170653306,
1353.65743253163,1354.09315853019,1354.52803183356,1354.96290513685,1355.39777844007,
1355.83265174322,1356.26752504631,1356.70239834933,1357.1372716523,1357.57214495521,
1358.00701825807,1358.44189156087,1358.87676486363,1359.31163816635,1359.74651146902,
1360.18138477166,1360.6171107698,1361.05283676795,1361.48771007051,1361.92258337305,
1362.35745667556,1362.79232997804,1363.2272032805,1363.66207658295,1364.09694988538,
1364.5318231878,1364.96669649021,1365.40156979261,1365.83644309501,1366.27131639741,
1366.70618969981,1367.14106300222,1367.57678900028,1368.01251499834,1368.44738830077,
1368.88226160321,1369.31713490567,1369.75200820816,1370.18688151067,1370.6217548132,
1371.05662811577,1371.49150141837,1371.926374721,1372.36124802367,1372.79612132639,
1373.23099462915,1373.66586793196,1374.10074123481,1374.53646723311,1374.97219323142,
1375.40706653438,1375.84193983741,1376.2768131405,1376.71168644365,1377.14655974687,
1377.58143305016,1378.01630635352,1378.45117965696,1378.88605296047,1379.32092626407,
1379.75579956775,1380.19067287151,1380.62554617536,1381.06041947931,1381.49614547817,
1381.93187147704,1382.36674478117,1382.8016180854,1383.23649138973,1383.67136469416,
1384.10623799869,1384.54111130334,1384.97598460809,1385.41085791295,1385.84573121793,
1386.28060452302,1386.71547782823,1387.15035113356,1387.585224439,1388.02009774458,
1388.45582374427,1388.89154974397,1389.32642304979,1389.76129635574,1390.19616966182,
1390.63104296803,1391.06591627437,1391.50078958085,1391.93566288746,1392.37053619421,
1392.8054095011,1393.24028280813,1393.6751561153,1394.1100294226,1394.54490273005,
1394.97977603765,1395.41550203836,1395.85122803908,1396.28610134696,1396.72097465499,
1397.15584796317,1397.59072127149,1398.02559457996,1398.46046788858,1398.89534119734,
1399.33021450626,1399.76508781532,1400.19996112453,1400.63483443389,1401.50458105306,
1401.93945436286,1402.37518036469,1402.81090636651,1403.24577967661,1403.68065298686,
1404.11552629725,1404.5503996078,1404.98527291848,1405.85501954029,1406.2898928514,
1406.72476616266,1407.15963947406,1407.5945127856,1408.02938609727,1408.46425940908,
1409.33485872391,1410.205458039,1410.64033135134,1411.07520466381,1411.51007797639,
1411.9449512891,1412.81469791488,1413.68444454112,1414.5541911678,1415.42393779489,
1416.29453711233,1417.16513642995,1418.03488305796,1418.90462968629,1419.77437631491,
1420.64412294377,1421.51386957285,1422.38361620211,1423.25421552099,1424.12481483992,
1424.99456146943,1425.86430809896,1426.73405472847,1427.60380135791,1428.47354798724,
1429.34329461641,1430.21389393501,1431.08449325349,1431.9542398821,1432.82398651043,
1433.69373313844,1434.56347976611,1435.4332263934,1436.30297302029,1437.17357233701,
1438.04417165351,1438.91391827929,1439.78366490459,1440.65341152939,1441.52315815367,
1441.95803146562,1442.39290477743,1442.8277780891,1443.26265140064,1444.13325071451,
1445.00385002811,1445.43872333908,1445.87359664991,1446.3084699606,1446.74334327114,
1447.17821658153,1447.61308989178,1448.48283651184,1448.91770982164,1449.3525831313,
1449.78745644081,1450.22232975017,1450.65720305938,1451.09292906076,1451.52865506214,
1451.96352837105,1452.39840167982,1452.83327498843,1453.2681482969,1453.70302160522,
1454.1378949134,1454.57276822143,1455.00764152931,1455.44251483705,1455.87738814464,
1456.31226145209,1456.7471347594,1457.18200806657,1457.6168813736,1458.05260737389,
1458.48833337418,1458.92320668093,1459.35807998754,1459.79295329402,1460.22782660036,
1460.66269990657,1461.09757321265,1461.5324465186,1461.96731982443,1462.40219313012,
1462.83706643569,1463.27193974114,1463.70681304647,1464.14168635168,1464.57655965677,
1465.0122856561,1465.44801165544,1465.8828849603,1466.31775826505,1466.7526315697,
1467.18750487423,1467.62237817866,1468.05725148299,1468.49212478722,1468.92699809135,
1469.36187139539,1469.79674469933,1470.23161800319,1470.66649130695,1471.10136461063,
1471.53623791422,1471.97196391283,1472.40768991143,1472.84256321487,1473.27743651823,
1473.71230982152,1474.14718312474,1474.58205642789,1475.01692973098,1475.451803034,
1475.88667633697,1476.32154963988,1476.75642294274,1477.19129624555,1477.62616954831,
1478.06104285102,1478.4959161537,1478.93164215186,1479.36736815002,1479.80224145262,
1480.23711475519,1480.67198805772,1481.10686136023,1481.54173466272,1481.97660796518,
1482.41148126762,1482.84635457005,1483.28122787247,1483.71610117488,1484.15097447728,
1484.58584777968,1485.02072108208,1485.45559438449,1485.89132038254,1486.32704638059,
1486.76191968301,1487.19679298544,1487.63166628788,1488.06653959035,1488.50141289283,
1488.93628619534,1489.37115949787,1489.80603280044,1490.24090610304,1490.67577940567,
1491.11065270835,1491.54552601106,1491.98039931382,1492.41527261663,1492.8509986149,
1493.28672461318,1493.72159791609,1494.15647121906,1494.59134452208,1495.02621782517,
1495.46109112832,1495.89596443154,1496.33083773483,1496.76571103819,1497.20058434163,
1497.63545764515,1498.07033094874,1498.50520425242,1498.94007755618,1499.37495086004,
1499.81067685885,1500.24640285767,1500.68127616171,1501.11614946584,1501.55102277007,
1501.9858960744,1502.42076937883,1502.85564268337,1503.29051598801,1503.72538929276,
1504.16026259762,1504.5951359026,1505.03000920769,1505.4648825129,1505.89975581823,
1506.33462912368,1506.77035512331,1507.20608112294,1507.64095442864,1508.07582773446,
1508.51070104041,1508.94557434649,1509.3804476527,1509.81532095904,1510.25019426552,
1510.68506757213,1511.11994087888,1511.55481418577,1511.9896874928,1512.42456079996,
1512.85943410727,1513.29430741472,1513.73003341537,1514.16575941601,1514.60063272375,
1515.03550603163,1515.47037933966,1515.90525264784,1516.34012595616,1516.77499926463,
1517.20987257325,1517.64474588201,1518.07961919093,1518.51449249999,1518.9493658092,
1519.38423911856,1519.81911242807,1520.25398573772,1520.68971173947,1521.12543774122,
1521.56031105118,1521.99518436128,1522.43005767153,1523.29980429246,1523.73467760315,
1524.16955091398,1524.60442422495,1525.03929753607,1525.47417084733,1525.90904415873,
1526.77879078194,1527.64939009657,1528.08511609939,1528.51998941146,1528.95486272367,
1529.38973603601,1530.25948266106,1531.1292292866,1531.99897591261,1532.86872253907,
1533.73846916596,1534.60906848325,1535.47966780073,1536.34941442858,1537.21916105675,
1538.08890768523,1538.95865431398,1539.82840094295,1540.69814757212,1541.56874689096,
1542.43934620985,1543.30909283933,1544.17883946886,1545.04858609839,1545.91833272787,
1546.78807935726,1547.65782598651,1548.52842530518,1549.39902462375,1550.26877125249,
1551.13851788097,1552.00826450914,1552.87801113699,1553.74775776447,1554.61750439156,
1555.48810370844,1556.35870302511,1557.22844965112,1558.09819627666,1558.96794290171,
1559.83768952626,1560.27256283834,1560.70743615028,1561.57718277377,1562.44778208785,
1563.31838140165,1563.75325471277,1564.18812802374,1564.62300133457,1565.05787464526,
1565.9276212662,1566.79736788655,1567.2322411965,1567.66711450631,1568.10198781596,
1568.53686112547,1568.97173443483,1569.40746043628,1569.84318643774,1570.2780597468,
1570.71293305571,1571.14780636448,1571.5826796731,1572.01755298157,1572.45242628989,
1572.88729959806,1573.32217290609,1573.75704621397,1574.19191952171,1574.62679282931,
1575.06166613676,1575.49653944407,1575.93141275123,1576.36713875159,1576.80286475195,
1577.23773805884,1577.67261136559,1578.1074846722,1578.54235797868,1578.97723128502,
1579.41210459124,1579.84697789732,1580.28185120327,1580.71672450909,1581.15159781478,
1581.58647112036,1582.0213444258,1582.45621773113,1582.89109103634,1583.32681703573,
1583.76254303513,1584.1974163401,1584.63228964497,1585.06716294972,1585.50203625436,
1585.9369095589,1586.37178286333,1586.80665616766,1587.24152947189,1587.67640277602,
1588.11127608005,1588.546149384,1588.98102268785,1589.41589599161,1589.85076929529,
1590.28649529394,1590.72222129258,1591.1570945961,1591.59196789953,1592.0268412029,
1592.46171450619,1592.8965878094,1593.33146111256,1593.76633441564,1594.20120771867,
1594.63608102164,1595.07095432455,1595.50582762741,1595.94070093021,1596.37557423297,
1596.81044753569,1597.24617353387,1597.68189953206,1598.11677283469,1598.55164613729,
1598.98651943985,1599.42139274239,1599.8562660449,1600.29113934738,1600.72601264985,
1601.16088595229,1601.59575925472,1602.03063255714,1602.46550585955,1602.90037916195,
1603.33525246435,1603.77012576675,1604.2058517648,1604.64157776285,1605.07645106526,
1605.51132436768,1605.94619767011,1606.38107097255,1606.81594427502,1607.2508175775,
1607.68569088001,1608.12056418254,1608.55543748511,1608.99031078771,1609.42518409034,
1609.86005739302,1610.29493069573,1610.72980399849,1611.16552999674,1611.60125599499,
1612.03612929785,1612.47100260076,1612.90587590373,1613.34074920675,1613.77562250984,
1614.21049581299,1614.64536911621,1615.0802424195,1615.51511572286,1615.9499890263,
1616.38486232981,1616.81973563341,1617.25460893709,1617.68948224085,1618.12520823963,
1618.5609342384,1618.99580754234,1619.43068084638,1619.86555415051,1620.30042745474,
1620.73530075907,1621.1701740635,1621.60504736804,1622.03992067268,1622.47479397743,
1622.90966728229,1623.34454058727,1623.77941389236,1624.21428719757,1624.6491605029,
1625.08488650247,1625.52061250204,1625.95548580761,1626.39035911331,1626.82523241913,
1627.26010572508,1627.69497903116,1628.12985233737,1628.56472564372,1628.99959895019,
1629.43447225681,1629.86934556356,1630.30421887044,1630.73909217747,1631.17396548464,
1631.60883879195,1632.04456479252,1632.48029079309,1632.91516410068,1633.35003740842,
1633.78491071631,1634.21978402433,1634.65465733251,1635.08953064083,1635.5244039493,
1635.95927725792,1636.39415056668,1636.8290238756,1637.26389718466,1637.69877049387,
1638.13364380323,1638.56851711274,1639.00424311442,1639.43996911609,1639.8748424259,
1640.30971573585,1640.74458904595,1641.6143356666,1642.04920897714,1642.48408228782,
1642.91895559865,1643.35382890963,1643.78870222074,1644.223575532,1645.09332215494,
1645.52819546661,1645.96392146936,1646.39964747212,1646.83452078406,1647.26939409614,
1647.70426740834,1648.57401403314,1649.44376065844,1650.31350728422,1650.74838059729,
1651.18325391046,1652.05300053714,1652.92359985428,1653.79419917162,1654.66394579929,
1655.5336924273,1656.40343905563,1657.27318568424,1658.14293231311,1659.01267894219,
1659.88327826096,1660.75387757982,1661.62362420926,1662.49337083877,1663.3631174683,
1664.23286409781,1665.10261072725,1665.97235735658,1666.84295667531,1667.71355599396,
1668.58330262282,1669.45304925143,1670.32279587976,1671.19254250778,1672.06228913544,
1672.93203576273,1673.80263507977,1674.6732343966,1675.54298102284,1676.41272764862,
1677.28247427392,1678.15222089872,1679.021967523,1679.89171414676,1680.76231346105,
1681.19803946366,1681.63291277506,1682.06778608632,1682.50265939743,1682.93753270841,
1683.37240601924,1684.24215264047,1684.67702595086,1685.11189926111,1685.54677257121,
1685.98164588116,1686.41651919097,1686.85139250063,1687.28626581014,1687.72199181166,
1688.15771781319,1688.5925911224,1689.02746443146,1689.46233774038,1689.89721104914,
1690.33208435776,1690.76695766623,1691.20183097455,1691.63670428272,1692.07157759075,
1692.50645089864,1692.94132420637,1693.37619751397,1693.81107082142,1694.24594412873,
1694.68167012916,1695.11739612959,1695.55226943662,1695.9871427435,1696.42201605025,
1696.85688935687,1697.29176266334,1697.72663596969,1698.1615092759,1698.59638258198,
1699.03125588793,1699.46612919375,1699.90100249945,1700.33587580502,1700.77074911047,
1701.20562241579,1701.64134841525,1702.0770744147,1702.51194771979,1702.94682102476,
1703.38169432963,1703.81656763438,1704.25144093902,1704.68631424356,1705.12118754799,
1705.55606085232,1705.99093415655,1706.42580746068,1706.86068076471,1707.29555406866,
1707.73042737251,1708.16530067627,1708.60102667496,1709.03675267365,1709.47162597724,
1709.90649928076,1710.34137258419,1710.77624588756,1711.21111919085,1711.64599249406,
1712.08086579722,1712.5157391003,1712.95061240333,1713.3854857063,1713.82035900921,
1714.25523231207,1714.69010561487,1715.12497891763,1715.56070491584,1715.99643091404,
1716.43130421671,1716.86617751935,1717.30105082195,1717.73592412451,1718.17079742705,
1718.60567072956,1719.04054403204,1719.4754173345,1719.91029063695,1720.34516393938,
1720.7800372418,1721.21491054421,1721.64978384661,1722.08465714901,1722.52038314706,
1722.9561091451,1723.39098244751,1723.82585574992,1724.26072905233,1724.69560235476,
1725.13047565721,1725.56534895967,1726.00022226216,1726.43509556467,1726.8699688672,
1727.30484216977,1727.73971547236,1728.174588775,1728.60946207767,1729.04433538039,
1729.48006137861,1729.91578737684,1730.35066067965,1730.78553398251,1731.22040728542,
1731.65528058838,1732.09015389141,1732.5250271945,1732.95990049765,1733.39477380087,
1733.82964710416,1734.26452040752,1734.69939371096,1735.13426701447,1735.56914031807,
1736.00401362175,1736.43973962048,1736.8754656192,1737.31033892306,1737.745212227,
1738.18008553104,1738.61495883517,1739.0498321394,1739.48470544373,1739.91957874816,
1740.35445205269,1740.78932535734,1741.22419866209,1741.65907196695,1742.09394527193,
1742.52881857702,1742.96369188223,1743.39941788174,1743.83514388125,1744.2700171867,
1744.70489049227,1745.13976379797,1745.57463710379,1746.00951040974,1746.44438371582,
1746.87925702203,1747.31413032837,1747.74900363485,1748.18387694146,1748.61875024821,
1749.0536235551,1749.48849686213,1749.92337016929,1750.3590961698,1750.7948221703,
1751.22969547775,1751.66456878534,1752.09944209308,1752.53431540096,1752.96918870899,
1753.40406201717,1753.83893532549,1754.27380863396,1754.70868194258,1755.14355525134,
1755.57842856026,1756.01330186932,1756.44817517853,1756.88304848789,1757.31877448949,
1757.75450049109,1758.18937380075,1759.05912042051,1759.49399373061,1759.92886704086,
1760.36374035125,1760.79861366179,1761.23348697248,1761.66836028331,1762.10323359429,
1762.5381069054,1763.40785352806,1763.8427268396,1764.27845284228,1764.71417884496,
1765.14905215677,1765.58392546872,1766.0187987808,1766.88854540534,1767.75829203039,
1768.1931653431,1768.62803865593,1769.06291196888,1769.49778528195,1770.36753190841,
1771.2381312254,1772.10873054259,1772.97847717007,1773.84822379791,1774.71797042609,
1775.58771705456,1776.45746368331,1777.32721031228,1778.19780963089,1779.06840894783,
1779.93815555508,1780.80790201176,1781.67764871408),.UNSPECIFIED.) ;
#835 = B_SPLINE_SURFACE_WITH_KNOTS('',1,3,((#105818,#105819,#105820,#105821,
#105822,#105823,#105824,#105825,#105826,#105827,#105828,#105829,#105830,
#105831,#105832,#105833,#105834,#105835,#105836,#105837,#105838,#105839,
#105840,#105841,#105842,#105843,#105844,#105845,#105846,#105847,#105848,
#105849,#105850,#105851,#105852,#105853,#105854,#105855,#105856,#105857,
#105858,#105859,#105860,#105861,#105862,#105863,#105864,#105865,#105866,
#105867,#105868,#105869,#105870,#105871,#105872,#105873,#105874,#105875,
#105876,#105877,#105878,#105879,#105880,#105881,#105882,#105883,#105884,
#105885,#105886,#105887,#105888,#105889,#105890,#105891,#105892,#105893,
#105894,#105895,#105896,#105897,#105898,#105899,#105900,#105901,#105902,
#105903,#105904,#105905,#105906,#105907,#105908,#105909,#105910,#105911,
#105912,#105913,#105914,#105915,#105916,#105917,#105918,#105919,#105920,
#105921,#105922,#105923,#105924,#105925,#105926,#105927,#105928,#105929,
#105930,#105931,#105932,#105933,#105934,#105935,#105936,#105937,#105938,
#105939,#105940,#105941,#105942,#105943,#105944,#105945,#105946,#105947,
#105948,#105949,#105950,#105951,#105952,#105953,#105954,#105955,#105956,
#105957,#105958,#105959,#105960,#105961,#105962,#105963,#105964,#105965,
#105966,#105967,#105968,#105969,#105970,#105971,#105972,#105973,#105974,
#105975,#105976,#105977,#105978,#105979,#105980,#105981,#105982,#105983,
#105984,#105985,#105986,#105987,#105988,#105989,#105990,#105991,#105992,
#105993,#105994,#105995,#105996,#105997,#105998,#105999,#106000,#106001,
#106002,#106003,#106004,#106005,#106006,#106007,#106008,#106009,#106010,
#106011,#106012,#106013,#106014,#106015,#106016,#106017,#106018,#106019,
#106020,#106021,#106022,#106023,#106024,#106025,#106026,#106027,#106028,
#106029,#106030,#106031,#106032,#106033,#106034,#106035,#106036,#106037,
#106038,#106039,#106040,#106041,#106042,#106043,#106044,#106045,#106046,
#106047,#106048,#106049,#106050,#106051,#106052,#106053,#106054,#106055,
#106056,#106057,#106058,#106059,#106060,#106061,#106062,#106063,#106064,
#106065,#106066,#106067,#106068,#106069,#106070,#106071,#106072,#106073,
#106074,#106075,#106076,#106077,#106078,#106079,#106080,#106081,#106082,
#106083,#106084,#106085,#106086,#106087,#106088,#106089,#106090,#106091,
#106092,#106093,#106094,#106095,#106096,#106097,#106098,#106099,#106100,
#106101,#106102,#106103,#106104,#106105,#106106,#106107,#106108,#106109,
#106110,#106111,#106112,#106113,#106114,#106115,#106116,#106117,#106118,
#106119,#106120,#106121,#106122,#106123,#106124,#106125,#106126,#106127,
#106128,#106129,#106130,#106131,#106132,#106133,#106134,#106135,#106136,
#106137,#106138,#106139,#106140,#106141,#106142,#106143,#106144,#106145,
#106146,#106147,#106148,#106149,#106150,#106151,#106152,#106153,#106154,
#106155,#106156,#106157,#106158,#106159,#106160,#106161,#106162,#106163,
#106164,#106165,#106166,#106167,#106168,#106169,#106170,#106171,#106172,
#106173,#106174,#106175,#106176,#106177,#106178,#106179,#106180,#106181,
#106182,#106183,#106184,#106185,#106186,#106187,#106188,#106189,#106190,
#106191,#106192,#106193,#106194,#106195,#106196,#106197,#106198,#106199,
#106200,#106201,#106202,#106203,#106204,#106205,#106206,#106207,#106208,
#106209,#106210,#106211,#106212,#106213,#106214,#106215,#106216,#106217,
#106218,#106219,#106220,#106221,#106222,#106223,#106224,#106225,#106226,
#106227,#106228,#106229,#106230,#106231,#106232,#106233,#106234,#106235,
#106236,#106237,#106238,#106239,#106240,#106241,#106242,#106243,#106244,
#106245,#106246,#106247,#106248,#106249,#106250,#106251,#106252,#106253,
#106254,#106255,#106256,#106257,#106258,#106259,#106260,#106261,#106262,
#106263,#106264,#106265,#106266,#106267,#106268,#106269,#106270,#106271,
#106272,#106273,#106274,#106275,#106276,#106277,#106278,#106279,#106280,
#106281,#106282,#106283,#106284,#106285,#106286,#106287,#106288,#106289,
#106290,#106291,#106292,#106293,#106294,#106295,#106296,#106297,#106298,
#106299,#106300,#106301,#106302,#106303,#106304,#106305,#106306,#106307,
#106308,#106309,#106310,#106311,#106312,#106313,#106314,#106315,#106316,
#106317,#106318,#106319,#106320,#106321,#106322,#106323,#106324,#106325,
#106326,#106327,#106328,#106329,#106330,#106331,#106332,#106333,#106334,
#106335,#106336,#106337,#106338,#106339,#106340,#106341,#106342,#106343,
#106344,#106345,#106346,#106347,#106348,#106349,#106350,#106351,#106352,
#106353,#106354,#106355,#106356,#106357,#106358,#106359,#106360,#106361,
#106362,#106363,#106364,#106365,#106366,#106367,#106368,#106369,#106370,
#106371,#106372,#106373,#106374,#106375,#106376,#106377,#106378,#106379,
#106380,#106381,#106382,#106383,#106384,#106385,#106386,#106387,#106388,
#106389,#106390,#106391,#106392,#106393,#106394,#106395,#106396,#106397,
#106398,#106399,#106400,#106401,#106402,#106403,#106404,#106405,#106406,
#106407,#106408,#106409,#106410,#106411,#106412,#106413,#106414,#106415,
#106416,#106417,#106418,#106419,#106420,#106421,#106422,#106423,#106424,
#106425,#106426,#106427,#106428,#106429,#106430,#106431,#106432,#106433,
#106434,#106435,#106436,#106437,#106438,#106439,#106440,#106441,#106442,
#106443,#106444,#106445,#106446,#106447,#106448,#106449,#106450,#106451,
#106452,#106453,#106454,#106455,#106456,#106457,#106458,#106459,#106460,
#106461,#106462,#106463,#106464,#106465,#106466,#106467,#106468,#106469,
#106470,#106471,#106472,#106473,#106474,#106475,#106476,#106477,#106478,
#106479,#106480,#106481,#106482,#106483,#106484,#106485,#106486,#106487,
#106488,#106489,#106490,#106491,#106492,#106493,#106494,#106495,#106496,
#106497,#106498,#106499,#106500,#106501,#106502,#106503,#106504,#106505,
#106506,#106507,#106508,#106509,#106510,#106511,#106512,#106513,#106514,
#106515,#106516,#106517,#106518,#106519,#106520,#106521,#106522,#106523,
#106524,#106525,#106526,#106527,#106528,#106529,#106530,#106531,#106532,
#106533,#106534,#106535,#106536,#106537,#106538,#106539,#106540,#106541,
#106542,#106543,#106544,#106545,#106546,#106547,#106548,#106549,#106550,
#106551,#106552,#106553,#106554,#106555,#106556,#106557,#106558,#106559,
#106560,#106561,#106562,#106563,#106564,#106565,#106566,#106567,#106568,
#106569,#106570,#106571,#106572,#106573,#106574,#106575,#106576,#106577,
#106578,#106579,#106580,#106581,#106582,#106583,#106584,#106585,#106586,
#106587,#106588,#106589,#106590,#106591,#106592,#106593,#106594,#106595,
#106596,#106597,#106598,#106599,#106600,#106601,#106602,#106603,#106604,
#106605,#106606,#106607,#106608,#106609,#106610,#106611,#106612,#106613,
#106614,#106615,#106616,#106617,#106618,#106619,#106620,#106621,#106622,
#106623,#106624,#106625,#106626,#106627,#106628,#106629,#106630,#106631,
#106632,#106633,#106634,#106635,#106636,#106637,#106638,#106639,#106640,
#106641,#106642,#106643,#106644,#106645,#106646,#106647,#106648,#106649,
#106650,#106651,#106652,#106653,#106654,#106655,#106656,#106657,#106658,
#106659,#106660,#106661,#106662,#106663,#106664,#106665,#106666,#106667,
#106668,#106669,#106670,#106671,#106672,#106673,#106674,#106675,#106676,
#106677,#106678,#106679,#106680,#106681,#106682,#106683,#106684,#106685,
#106686,#106687,#106688,#106689,#106690,#106691,#106692,#106693,#106694,
#106695,#106696,#106697,#106698,#106699,#106700,#106701,#106702,#106703,
#106704,#106705,#106706,#106707,#106708,#106709,#106710,#106711,#106712,
#106713,#106714,#106715,#106716,#106717,#106718,#106719,#106720,#106721,
#106722,#106723,#106724,#106725,#106726,#106727,#106728,#106729,#106730,
#106731,#106732,#106733,#106734,#106735,#106736,#106737,#106738,#106739,
#106740,#106741,#106742,#106743,#106744,#106745,#106746,#106747,#106748,
#106749,#106750,#106751,#106752,#106753,#106754,#106755,#106756,#106757,
#106758,#106759,#106760,#106761,#106762,#106763,#106764,#106765,#106766,
#106767,#106768,#106769,#106770,#106771,#106772,#106773,#106774,#106775,
#106776,#106777,#106778,#106779,#106780,#106781,#106782,#106783,#106784,
#106785,#106786,#106787,#106788,#106789,#106790,#106791,#106792,#106793,
#106794,#106795,#106796,#106797,#106798,#106799,#106800,#106801,#106802,
#106803,#106804,#106805,#106806,#106807,#106808,#106809,#106810,#106811,
#106812,#106813,#106814,#106815,#106816,#106817,#106818,#106819,#106820,
#106821,#106822,#106823,#106824,#106825,#106826,#106827,#106828,#106829,
#106830,#106831,#106832,#106833,#106834,#106835,#106836,#106837,#106838,
#106839,#106840,#106841,#106842,#106843,#106844,#106845,#106846,#106847,
#106848,#106849,#106850,#106851,#106852,#106853,#106854,#106855,#106856,
#106857,#106858,#106859,#106860,#106861,#106862,#106863,#106864,#106865,
#106866,#106867,#106868,#106869,#106870,#106871,#106872,#106873,#106874,
#106875,#106876,#106877,#106878,#106879,#106880,#106881,#106882,#106883,
#106884,#106885,#106886,#106887,#106888,#106889,#106890,#106891,#106892,
#106893,#106894,#106895,#106896,#106897,#106898,#106899,#106900,#106901,
#106902,#106903,#106904,#106905,#106906,#106907,#106908,#106909,#106910,
#106911,#106912,#106913,#106914,#106915,#106916,#106917,#106918,#106919,
#106920,#106921,#106922,#106923,#106924,#106925,#106926,#106927,#106928,
#106929,#106930,#106931,#106932,#106933,#106934,#106935,#106936,#106937,
#106938,#106939,#106940,#106941,#106942,#106943,#106944,#106945,#106946,
#106947,#106948,#106949,#106950,#106951,#106952,#106953,#106954,#106955,
#106956,#106957,#106958,#106959,#106960,#106961,#106962,#106963,#106964,
#106965,#106966,#106967,#106968,#106969,#106970,#106971,#106972,#106973,
#106974,#106975,#106976,#106977,#106978,#106979,#106980,#106981,#106982,
#106983,#106984,#106985,#106986,#106987,#106988,#106989,#106990,#106991,
#106992,#106993,#106994,#106995,#106996,#106997,#106998,#106999,#107000,
#107001,#107002,#107003,#107004,#107005,#107006,#107007,#107008,#107009,
#107010,#107011,#107012,#107013,#107014,#107015,#107016,#107017,#107018,
#107019,#107020,#107021,#107022,#107023,#107024,#107025,#107026,#107027,
#107028,#107029,#107030,#107031,#107032,#107033,#107034,#107035,#107036,
#107037,#107038,#107039,#107040,#107041,#107042,#107043,#107044,#107045,
#107046,#107047,#107048,#107049,#107050,#107051,#107052,#107053,#107054,
#107055,#107056,#107057,#107058,#107059,#107060,#107061,#107062,#107063,
#107064,#107065,#107066,#107067,#107068,#107069,#107070,#107071,#107072,
#107073,#107074,#107075,#107076,#107077,#107078,#107079,#107080,#107081,
#107082,#107083,#107084,#107085,#107086,#107087,#107088,#107089,#107090,
#107091,#107092,#107093,#107094,#107095,#107096,#107097,#107098,#107099,
#107100,#107101,#107102,#107103,#107104,#107105,#107106,#107107,#107108,
#107109,#107110,#107111,#107112,#107113,#107114,#107115,#107116,#107117,
#107118,#107119,#107120,#107121,#107122,#107123,#107124,#107125,#107126,
#107127,#107128,#107129,#107130,#107131,#107132,#107133,#107134,#107135,
#107136,#107137,#107138,#107139,#107140,#107141,#107142,#107143,#107144,
#107145,#107146,#107147,#107148,#107149,#107150,#107151,#107152,#107153,
#107154,#107155,#107156,#107157,#107158,#107159,#107160,#107161,#107162,
#107163,#107164,#107165,#107166,#107167,#107168,#107169,#107170,#107171,
#107172,#107173,#107174,#107175,#107176,#107177,#107178,#107179,#107180,
#107181,#107182,#107183,#107184,#107185,#107186,#107187,#107188,#107189,
#107190,#107191,#107192,#107193,#107194,#107195,#107196,#107197,#107198,
#107199,#107200,#107201,#107202,#107203,#107204,#107205,#107206,#107207,
#107208,#107209,#107210,#107211,#107212,#107213,#107214,#107215,#107216,
#107217,#107218,#107219,#107220,#107221,#107222,#107223,#107224,#107225,
#107226,#107227,#107228,#107229,#107230,#107231,#107232,#107233,#107234,
#107235,#107236,#107237,#107238,#107239,#107240,#107241,#107242,#107243,
#107244,#107245,#107246,#107247,#107248,#107249,#107250,#107251,#107252,
#107253,#107254,#107255,#107256,#107257,#107258,#107259,#107260,#107261,
#107262,#107263,#107264,#107265,#107266,#107267,#107268,#107269,#107270,
#107271,#107272,#107273,#107274,#107275,#107276,#107277,#107278,#107279,
#107280,#107281,#107282,#107283,#107284,#107285,#107286,#107287,#107288,
#107289,#107290,#107291,#107292,#107293,#107294,#107295,#107296,#107297,
#107298,#107299,#107300,#107301,#107302,#107303,#107304,#107305,#107306,
#107307,#107308,#107309,#107310,#107311,#107312,#107313,#107314,#107315,
#107316,#107317,#107318,#107319,#107320,#107321,#107322,#107323,#107324,
#107325,#107326,#107327,#107328,#107329,#107330,#107331,#107332,#107333,
#107334,#107335,#107336,#107337,#107338,#107339,#107340,#107341,#107342,
#107343,#107344,#107345,#107346,#107347,#107348,#107349,#107350,#107351,
#107352,#107353,#107354,#107355,#107356,#107357,#107358,#107359,#107360,
#107361,#107362,#107363,#107364,#107365,#107366,#107367,#107368,#107369,
#107370,#107371,#107372,#107373,#107374,#107375,#107376,#107377,#107378,
#107379,#107380,#107381,#107382,#107383,#107384,#107385,#107386,#107387,
#107388,#107389,#107390,#107391,#107392,#107393,#107394,#107395,#107396,
#107397,#107398,#107399,#107400,#107401,#107402,#107403,#107404,#107405,
#107406,#107407,#107408,#107409,#107410,#107411,#107412,#107413,#107414,
#107415,#107416,#107417,#107418,#107419,#107420,#107421,#107422,#107423,
#107424,#107425,#107426,#107427,#107428,#107429,#107430,#107431,#107432,
#107433,#107434,#107435,#107436,#107437,#107438,#107439,#107440,#107441,
#107442,#107443,#107444,#107445,#107446,#107447,#107448,#107449,#107450,
#107451,#107452,#107453,#107454,#107455,#107456,#107457,#107458,#107459,
#107460,#107461,#107462,#107463,#107464,#107465,#107466,#107467,#107468,
#107469,#107470,#107471,#107472,#107473,#107474,#107475,#107476,#107477,
#107478,#107479,#107480,#107481,#107482,#107483,#107484,#107485,#107486,
#107487,#107488,#107489,#107490,#107491,#107492,#107493,#107494,#107495,
#107496,#107497,#107498,#107499,#107500,#107501,#107502,#107503,#107504,
#107505,#107506,#107507,#107508,#107509,#107510,#107511,#107512,#107513,
#107514,#107515,#107516,#107517,#107518,#107519,#107520,#107521,#107522,
#107523,#107524,#107525,#107526,#107527,#107528,#107529,#107530,#107531,
#107532,#107533,#107534,#107535,#107536,#107537,#107538,#107539,#107540,
#107541,#107542,#107543,#107544,#107545,#107546,#107547,#107548,#107549,
#107550,#107551,#107552,#107553,#107554,#107555,#107556,#107557,#107558,
#107559,#107560,#107561,#107562,#107563,#107564,#107565,#107566,#107567,
#107568,#107569,#107570,#107571,#107572,#107573,#107574,#107575,#107576,
#107577,#107578,#107579,#107580,#107581,#107582,#107583,#107584,#107585,
#107586,#107587,#107588,#107589,#107590,#107591,#107592,#107593,#107594,
#107595,#107596,#107597,#107598,#107599,#107600,#107601,#107602,#107603,
#107604,#107605,#107606,#107607,#107608,#107609,#107610,#107611,#107612,
#107613,#107614,#107615,#107616,#107617,#107618,#107619,#107620,#107621,
#107622,#107623,#107624,#107625,#107626,#107627,#107628,#107629,#107630,
#107631,#107632,#107633,#107634,#107635,#107636,#107637,#107638,#107639,
#107640,#107641,#107642,#107643,#107644,#107645,#107646,#107647,#107648,
#107649,#107650,#107651,#107652,#107653,#107654,#107655,#107656,#107657,
#107658,#107659,#107660,#107661,#107662,#107663,#107664,#107665,#107666,
#107667,#107668,#107669,#107670,#107671,#107672,#107673,#107674,#107675,
#107676,#107677,#107678,#107679,#107680,#107681,#107682,#107683,#107684,
#107685,#107686,#107687,#107688,#107689,#107690,#107691,#107692,#107693,
#107694,#107695,#107696,#107697,#107698,#107699,#107700,#107701,#107702,
#107703,#107704,#107705,#107706,#107707,#107708,#107709,#107710,#107711,
#107712,#107713,#107714,#107715,#107716,#107717,#107718,#107719,#107720,
#107721,#107722,#107723,#107724,#107725,#107726,#107727,#107728,#107729,
#107730,#107731,#107732,#107733,#107734,#107735,#107736,#107737,#107738,
#107739,#107740,#107741,#107742,#107743,#107744,#107745,#107746,#107747,
#107748,#107749,#107750,#107751,#107752,#107753,#107754,#107755,#107756,
#107757,#107758,#107759,#107760,#107761,#107762,#107763,#107764,#107765,
#107766,#107767,#107768,#107769,#107770,#107771,#107772,#107773,#107774,
#107775,#107776,#107777,#107778,#107779,#107780,#107781,#107782,#107783,
#107784,#107785,#107786,#107787,#107788,#107789,#107790,#107791,#107792,
#107793,#107794,#107795,#107796,#107797,#107798,#107799,#107800,#107801,
#107802,#107803,#107804,#107805,#107806,#107807,#107808,#107809,#107810,
#107811,#107812,#107813,#107814,#107815,#107816,#107817,#107818,#107819,
#107820,#107821,#107822,#107823,#107824,#107825,#107826,#107827,#107828,
#107829,#107830,#107831,#107832,#107833,#107834,#107835,#107836,#107837,
#107838,#107839,#107840,#107841,#107842,#107843,#107844,#107845,#107846,
#107847,#107848,#107849,#107850,#107851,#107852,#107853,#107854,#107855,
#107856,#107857,#107858,#107859,#107860,#107861,#107862,#107863,#107864,
#107865,#107866,#107867,#107868,#107869,#107870,#107871,#107872,#107873,
#107874,#107875,#107876,#107877,#107878,#107879,#107880,#107881,#107882,
#107883,#107884,#107885,#107886,#107887,#107888,#107889,#107890,#107891,
#107892,#107893,#107894,#107895,#107896,#107897,#107898,#107899,#107900,
#107901,#107902,#107903,#107904,#107905,#107906,#107907,#107908,#107909,
#107910,#107911,#107912,#107913,#107914,#107915,#107916,#107917,#107918,
#107919,#107920,#107921,#107922,#107923,#107924,#107925,#107926,#107927,
#107928,#107929,#107930,#107931,#107932,#107933,#107934,#107935,#107936,
#107937,#107938,#107939,#107940,#107941,#107942,#107943,#107944,#107945,
#107946,#107947,#107948,#107949,#107950,#107951,#107952,#107953,#107954,
#107955,#107956,#107957,#107958,#107959,#107960,#107961,#107962,#107963,
#107964,#107965,#107966,#107967,#107968,#107969,#107970,#107971,#107972,
#107973,#107974,#107975,#107976,#107977,#107978,#107979,#107980,#107981,
#107982,#107983,#107984,#107985,#107986,#107987,#107988,#107989,#107990,
#107991,#107992,#107993,#107994,#107995,#107996,#107997,#107998,#107999,
#108000,#108001,#108002,#108003,#108004,#108005,#108006,#108007,#108008,
#108009,#108010,#108011,#108012,#108013,#108014,#108015,#108016,#108017,
#108018,#108019,#108020,#108021,#108022,#108023,#108024,#108025,#108026,
#108027,#108028,#108029,#108030,#108031,#108032,#108033,#108034,#108035,
#108036,#108037,#108038,#108039,#108040,#108041,#108042,#108043,#108044,
#108045,#108046,#108047,#108048,#108049,#108050,#108051,#108052,#108053,
#108054,#108055,#108056,#108057,#108058,#108059,#108060,#108061,#108062,
#108063,#108064,#108065,#108066,#108067,#108068,#108069,#108070,#108071,
#108072,#108073,#108074,#108075,#108076,#108077,#108078,#108079,#108080,
#108081,#108082,#108083,#108084,#108085,#108086,#108087,#108088,#108089,
#108090,#108091,#108092,#108093,#108094,#108095,#108096,#108097,#108098,
#108099,#108100,#108101,#108102,#108103,#108104,#108105,#108106,#108107,
#108108,#108109,#108110,#108111,#108112,#108113,#108114,#108115,#108116,
#108117,#108118,#108119,#108120,#108121,#108122,#108123,#108124,#108125,
#108126,#108127,#108128,#108129,#108130,#108131,#108132,#108133,#108134,
#108135,#108136,#108137,#108138,#108139,#108140,#108141,#108142,#108143,
#108144,#108145,#108146,#108147,#108148,#108149,#108150,#108151,#108152,
#108153,#108154,#108155,#108156,#108157,#108158,#108159,#108160,#108161,
#108162,#108163,#108164,#108165,#108166,#108167,#108168,#108169,#108170,
#108171,#108172,#108173,#108174,#108175,#108176,#108177,#108178,#108179,
#108180,#108181,#108182,#108183,#108184,#108185,#108186,#108187,#108188,
#108189,#108190,#108191,#108192,#108193,#108194,#108195,#108196,#108197,
#108198,#108199,#108200,#108201,#108202,#108203,#108204,#108205,#108206,
#108207,#108208,#108209,#108210,#108211,#108212,#108213,#108214,#108215,
#108216,#108217,#108218,#108219,#108220,#108221,#108222,#108223,#108224,
#108225,#108226,#108227,#108228,#108229,#108230,#108231,#108232,#108233,
#108234,#108235,#108236,#108237,#108238,#108239,#108240,#108241,#108242,
#108243,#108244,#108245,#108246,#108247,#108248,#108249,#108250,#108251,
#108252,#108253,#108254,#108255,#108256,#108257,#108258,#108259,#108260,
#108261,#108262,#108263,#108264,#108265,#108266,#108267,#108268,#108269,
#108270,#108271,#108272,#108273,#108274,#108275,#108276,#108277,#108278,
#108279,#108280,#108281,#108282,#108283,#108284,#108285,#108286,#108287,
#108288,#108289,#108290,#108291,#108292,#108293,#108294,#108295,#108296,
#108297,#108298,#108299,#108300,#108301,#108302,#108303,#108304,#108305,
#108306,#108307,#108308,#108309,#108310,#108311,#108312,#108313,#108314,
#108315,#108316,#108317,#108318,#108319,#108320,#108321,#108322,#108323,
#108324,#108325,#108326,#108327,#108328,#108329,#108330,#108331,#108332,
#108333,#108334,#108335,#108336,#108337,#108338,#108339,#108340,#108341,
#108342,#108343,#108344,#108345,#108346,#108347,#108348,#108349,#108350,
#108351,#108352,#108353,#108354,#108355,#108356,#108357,#108358,#108359,
#108360,#108361,#108362,#108363,#108364,#108365,#108366,#108367,#108368,
#108369,#108370,#108371,#108372,#108373,#108374,#108375,#108376,#108377,
#108378,#108379,#108380,#108381,#108382,#108383,#108384,#108385,#108386,
#108387,#108388,#108389,#108390,#108391,#108392,#108393,#108394,#108395,
#108396,#108397,#108398,#108399,#108400,#108401,#108402,#108403,#108404,
#108405,#108406,#108407,#108408,#108409,#108410,#108411,#108412,#108413,
#108414,#108415,#108416,#108417,#108418,#108419,#108420,#108421,#108422,
#108423,#108424,#108425,#108426,#108427,#108428,#108429,#108430,#108431,
#108432,#108433,#108434,#108435,#108436,#108437,#108438,#108439,#108440,
#108441,#108442,#108443,#108444,#108445,#108446,#108447,#108448,#108449,
#108450,#108451,#108452,#108453,#108454,#108455,#108456,#108457,#108458,
#108459,#108460,#108461,#108462,#108463,#108464,#108465,#108466,#108467,
#108468,#108469,#108470,#108471,#108472,#108473,#108474,#108475,#108476,
#108477,#108478,#108479,#108480,#108481,#108482,#108483,#108484,#108485,
#108486,#108487,#108488,#108489,#108490,#108491,#108492,#108493,#108494,
#108495,#108496,#108497,#108498,#108499,#108500,#108501,#108502,#108503,
#108504,#108505,#108506,#108507,#108508,#108509,#108510,#108511,#108512,
#108513,#108514,#108515,#108516,#108517,#108518,#108519,#108520,#108521,
#108522,#108523,#108524,#108525,#108526,#108527,#108528,#108529,#108530,
#108531,#108532,#108533,#108534,#108535,#108536,#108537,#108538,#108539,
#108540,#108541,#108542,#108543,#108544,#108545,#108546,#108547,#108548,
#108549,#108550,#108551,#108552,#108553,#108554,#108555,#108556,#108557,
#108558,#108559,#108560,#108561,#108562,#108563,#108564,#108565,#108566,
#108567,#108568,#108569,#108570,#108571,#108572,#108573,#108574,#108575,
#108576,#108577,#108578,#108579,#108580,#108581,#108582,#108583,#108584,
#108585,#108586,#108587,#108588,#108589,#108590,#108591,#108592,#108593,
#108594,#108595,#108596,#108597,#108598,#108599,#108600,#108601,#108602,
#108603,#108604,#108605,#108606,#108607,#108608,#108609,#108610,#108611,
#108612,#108613,#108614,#108615,#108616,#108617,#108618,#108619,#108620,
#108621,#108622,#108623,#108624,#108625,#108626,#108627,#108628,#108629,
#108630,#108631,#108632,#108633,#108634,#108635,#108636,#108637,#108638,
#108639,#108640,#108641,#108642,#108643,#108644,#108645,#108646,#108647,
#108648,#108649,#108650,#108651,#108652,#108653,#108654,#108655,#108656,
#108657,#108658,#108659,#108660,#108661,#108662,#108663,#108664,#108665,
#108666,#108667,#108668,#108669,#108670,#108671,#108672,#108673,#108674,
#108675,#108676,#108677,#108678,#108679,#108680,#108681,#108682,#108683,
#108684,#108685,#108686,#108687,#108688,#108689,#108690,#108691,#108692,
#108693,#108694,#108695,#108696,#108697,#108698,#108699,#108700,#108701,
#108702,#108703,#108704,#108705,#108706,#108707,#108708,#108709,#108710,
#108711,#108712,#108713,#108714,#108715,#108716,#108717,#108718,#108719,
#108720,#108721,#108722,#108723,#108724,#108725,#108726,#108727,#108728,
#108729,#108730,#108731,#108732,#108733,#108734,#108735,#108736,#108737,
#108738,#108739,#108740,#108741,#108742,#108743,#108744,#108745,#108746,
#108747,#108748,#108749,#108750,#108751,#108752,#108753,#108754,#108755,
#108756,#108757,#108758,#108759,#108760,#108761,#108762,#108763,#108764,
#108765,#108766,#108767,#108768,#108769,#108770,#108771,#108772,#108773,
#108774,#108775,#108776,#108777,#108778,#108779,#108780,#108781,#108782,
#108783,#108784,#108785,#108786,#108787,#108788,#108789,#108790,#108791,
#108792,#108793,#108794,#108795,#108796,#108797,#108798,#108799,#108800,
#108801,#108802,#108803,#108804,#108805,#108806,#108807,#108808,#108809,
#108810,#108811,#108812,#108813,#108814,#108815,#108816,#108817,#108818,
#108819,#108820,#108821,#108822,#108823,#108824,#108825,#108826,#108827,
#108828,#108829,#108830,#108831,#108832,#108833,#108834,#108835,#108836,
#108837,#108838,#108839,#108840,#108841,#108842,#108843,#108844,#108845,
#108846,#108847,#108848,#108849,#108850,#108851,#108852,#108853,#108854,
#108855,#108856,#108857,#108858,#108859,#108860,#108861,#108862,#108863,
#108864,#108865,#108866,#108867,#108868,#108869,#108870,#108871,#108872,
#108873,#108874,#108875,#108876,#108877,#108878,#108879,#108880,#108881,
#108882,#108883,#108884,#108885,#108886,#108887,#108888,#108889,#108890,
#108891,#108892,#108893,#108894,#108895,#108896,#108897,#108898,#108899,
#108900,#108901,#108902,#108903,#108904,#108905,#108906,#108907,#108908,
#108909,#108910,#108911,#108912,#108913,#108914,#108915,#108916,#108917,
#108918,#108919,#108920,#108921,#108922,#108923,#108924,#108925,#108926,
#108927,#108928,#108929,#108930,#108931,#108932,#108933,#108934,#108935,
#108936,#108937,#108938,#108939,#108940,#108941,#108942,#108943,#108944,
#108945,#108946,#108947,#108948,#108949,#108950,#108951,#108952,#108953,
#108954,#108955,#108956,#108957,#108958,#108959,#108960,#108961,#108962,
#108963,#108964,#108965,#108966,#108967,#108968,#108969,#108970,#108971,
#108972,#108973,#108974,#108975,#108976,#108977,#108978,#108979,#108980,
#108981,#108982,#108983,#108984,#108985,#108986,#108987,#108988,#108989,
#108990,#108991,#108992,#108993,#108994,#108995,#108996,#108997,#108998,
#108999,#109000,#109001,#109002,#109003,#109004,#109005,#109006,#109007,
#109008,#109009,#109010,#109011,#109012,#109013,#109014,#109015,#109016,
#109017,#109018,#109019,#109020,#109021,#109022,#109023,#109024,#109025,
#109026,#109027,#109028,#109029,#109030,#109031,#109032,#109033,#109034,
#109035,#109036,#109037,#109038,#109039,#109040,#109041,#109042,#109043,
#109044,#109045,#109046,#109047,#109048,#109049,#109050,#109051,#109052,
#109053,#109054,#109055,#109056,#109057,#109058,#109059,#109060,#109061,
#109062,#109063,#109064,#109065,#109066,#109067,#109068,#109069,#109070,
#109071,#109072,#109073,#109074,#109075,#109076,#109077,#109078,#109079,
#109080,#109081,#109082,#109083,#109084,#109085,#109086,#109087,#109088,
#109089,#109090,#109091,#109092,#109093,#109094,#109095,#109096,#109097,
#109098,#109099,#109100,#109101,#109102,#109103,#109104,#109105,#109106,
#109107,#109108,#109109,#109110,#109111,#109112,#109113,#109114,#109115,
#109116,#109117,#109118,#109119,#109120,#109121,#109122,#109123,#109124,
#109125,#109126,#109127,#109128,#109129,#109130,#109131,#109132,#109133,
#109134,#109135,#109136,#109137,#109138,#109139,#109140,#109141,#109142,
#109143,#109144,#109145,#109146,#109147,#109148,#109149,#109150,#109151,
#109152,#109153,#109154,#109155,#109156,#109157,#109158,#109159,#109160,
#109161,#109162,#109163,#109164,#109165,#109166,#109167,#109168,#109169,
#109170,#109171,#109172,#109173,#109174,#109175,#109176,#109177,#109178,
#109179,#109180,#109181,#109182,#109183,#109184,#109185,#109186,#109187,
#109188,#109189,#109190,#109191,#109192,#109193,#109194,#109195,#109196,
#109197,#109198,#109199,#109200,#109201,#109202,#109203,#109204,#109205,
#109206,#109207,#109208,#109209,#109210,#109211,#109212,#109213,#109214,
#109215,#109216,#109217,#109218,#109219,#109220,#109221,#109222,#109223,
#109224,#109225,#109226,#109227,#109228,#109229,#109230,#109231,#109232,
#109233,#109234,#109235,#109236,#109237,#109238,#109239,#109240,#109241,
#109242,#109243,#109244,#109245,#109246,#109247,#109248,#109249,#109250,
#109251,#109252,#109253,#109254,#109255,#109256,#109257,#109258,#109259,
#109260,#109261,#109262,#109263,#109264,#109265,#109266,#109267,#109268,
#109269,#109270,#109271,#109272,#109273,#109274,#109275,#109276,#109277,
#109278,#109279,#109280,#109281,#109282,#109283,#109284,#109285,#109286,
#109287,#109288,#109289,#109290,#109291,#109292,#109293,#109294,#109295,
#109296,#109297,#109298,#109299,#109300,#109301,#109302),(#109303,#109304,
#109305,#109306,#109307,#109308,#109309,#109310,#109311,#109312,#109313,
#109314,#109315,#109316,#109317,#109318,#109319,#109320,#109321,#109322,
#109323,#109324,#109325,#109326,#109327,#109328,#109329,#109330,#109331,
#109332,#109333,#109334,#109335,#109336,#109337,#109338,#109339,#109340,
#109341,#109342,#109343,#109344,#109345,#109346,#109347,#109348,#109349,
#109350,#109351,#109352,#109353,#109354,#109355,#109356,#109357,#109358,
#109359,#109360,#109361,#109362,#109363,#109364,#109365,#109366,#109367,
#109368,#109369,#109370,#109371,#109372,#109373,#109374,#109375,#109376,
#109377,#109378,#109379,#109380,#109381,#109382,#109383,#109384,#109385,
#109386,#109387,#109388,#109389,#109390,#109391,#109392,#109393,#109394,
#109395,#109396,#109397,#109398,#109399,#109400,#109401,#109402,#109403,
#109404,#109405,#109406,#109407,#109408,#109409,#109410,#109411,#109412,
#109413,#109414,#109415,#109416,#109417,#109418,#109419,#109420,#109421,
#109422,#109423,#109424,#109425,#109426,#109427,#109428,#109429,#109430,
#109431,#109432,#109433,#109434,#109435,#109436,#109437,#109438,#109439,
#109440,#109441,#109442,#109443,#109444,#109445,#109446,#109447,#109448,
#109449,#109450,#109451,#109452,#109453,#109454,#109455,#109456,#109457,
#109458,#109459,#109460,#109461,#109462,#109463,#109464,#109465,#109466,
#109467,#109468,#109469,#109470,#109471,#109472,#109473,#109474,#109475,
#109476,#109477,#109478,#109479,#109480,#109481,#109482,#109483,#109484,
#109485,#109486,#109487,#109488,#109489,#109490,#109491,#109492,#109493,
#109494,#109495,#109496,#109497,#109498,#109499,#109500,#109501,#109502,
#109503,#109504,#109505,#109506,#109507,#109508,#109509,#109510,#109511,
#109512,#109513,#109514,#109515,#109516,#109517,#109518,#109519,#109520,
#109521,#109522,#109523,#109524,#109525,#109526,#109527,#109528,#109529,
#109530,#109531,#109532,#109533,#109534,#109535,#109536,#109537,#109538,
#109539,#109540,#109541,#109542,#109543,#109544,#109545,#109546,#109547,
#109548,#109549,#109550,#109551,#109552,#109553,#109554,#109555,#109556,
#109557,#109558,#109559,#109560,#109561,#109562,#109563,#109564,#109565,
#109566,#109567,#109568,#109569,#109570,#109571,#109572,#109573,#109574,
#109575,#109576,#109577,#109578,#109579,#109580,#109581,#109582,#109583,
#109584,#109585,#109586,#109587,#109588,#109589,#109590,#109591,#109592,
#109593,#109594,#109595,#109596,#109597,#109598,#109599,#109600,#109601,
#109602,#109603,#109604,#109605,#109606,#109607,#109608,#109609,#109610,
#109611,#109612,#109613,#109614,#109615,#109616,#109617,#109618,#109619,
#109620,#109621,#109622,#109623,#109624,#109625,#109626,#109627,#109628,
#109629,#109630,#109631,#109632,#109633,#109634,#109635,#109636,#109637,
#109638,#109639,#109640,#109641,#109642,#109643,#109644,#109645,#109646,
#109647,#109648,#109649,#109650,#109651,#109652,#109653,#109654,#109655,
#109656,#109657,#109658,#109659,#109660,#109661,#109662,#109663,#109664,
#109665,#109666,#109667,#109668,#109669,#109670,#109671,#109672,#109673,
#109674,#109675,#109676,#109677,#109678,#109679,#109680,#109681,#109682,
#109683,#109684,#109685,#109686,#109687,#109688,#109689,#109690,#109691,
#109692,#109693,#109694,#109695,#109696,#109697,#109698,#109699,#109700,
#109701,#109702,#109703,#109704,#109705,#109706,#109707,#109708,#109709,
#109710,#109711,#109712,#109713,#109714,#109715,#109716,#109717,#109718,
#109719,#109720,#109721,#109722,#109723,#109724,#109725,#109726,#109727,
#109728,#109729,#109730,#109731,#109732,#109733,#109734,#109735,#109736,
#109737,#109738,#109739,#109740,#109741,#109742,#109743,#109744,#109745,
#109746,#109747,#109748,#109749,#109750,#109751,#109752,#109753,#109754,
#109755,#109756,#109757,#109758,#109759,#109760,#109761,#109762,#109763,
#109764,#109765,#109766,#109767,#109768,#109769,#109770,#109771,#109772,
#109773,#109774,#109775,#109776,#109777,#109778,#109779,#109780,#109781,
#109782,#109783,#109784,#109785,#109786,#109787,#109788,#109789,#109790,
#109791,#109792,#109793,#109794,#109795,#109796,#109797,#109798,#109799,
#109800,#109801,#109802,#109803,#109804,#109805,#109806,#109807,#109808,
#109809,#109810,#109811,#109812,#109813,#109814,#109815,#109816,#109817,
#109818,#109819,#109820,#109821,#109822,#109823,#109824,#109825,#109826,
#109827,#109828,#109829,#109830,#109831,#109832,#109833,#109834,#109835,
#109836,#109837,#109838,#109839,#109840,#109841,#109842,#109843,#109844,
#109845,#109846,#109847,#109848,#109849,#109850,#109851,#109852,#109853,
#109854,#109855,#109856,#109857,#109858,#109859,#109860,#109861,#109862,
#109863,#109864,#109865,#109866,#109867,#109868,#109869,#109870,#109871,
#109872,#109873,#109874,#109875,#109876,#109877,#109878,#109879,#109880,
#109881,#109882,#109883,#109884,#109885,#109886,#109887,#109888,#109889,
#109890,#109891,#109892,#109893,#109894,#109895,#109896,#109897,#109898,
#109899,#109900,#109901,#109902,#109903,#109904,#109905,#109906,#109907,
#109908,#109909,#109910,#109911,#109912,#109913,#109914,#109915,#109916,
#109917,#109918,#109919,#109920,#109921,#109922,#109923,#109924,#109925,
#109926,#109927,#109928,#109929,#109930,#109931,#109932,#109933,#109934,
#109935,#109936,#109937,#109938,#109939,#109940,#109941,#109942,#109943,
#109944,#109945,#109946,#109947,#109948,#109949,#109950,#109951,#109952,
#109953,#109954,#109955,#109956,#109957,#109958,#109959,#109960,#109961,
#109962,#109963,#109964,#109965,#109966,#109967,#109968,#109969,#109970,
#109971,#109972,#109973,#109974,#109975,#109976,#109977,#109978,#109979,
#109980,#109981,#109982,#109983,#109984,#109985,#109986,#109987,#109988,
#109989,#109990,#109991,#109992,#109993,#109994,#109995,#109996,#109997,
#109998,#109999,#110000,#110001,#110002,#110003,#110004,#110005,#110006,
#110007,#110008,#110009,#110010,#110011,#110012,#110013,#110014,#110015,
#110016,#110017,#110018,#110019,#110020,#110021,#110022,#110023,#110024,
#110025,#110026,#110027,#110028,#110029,#110030,#110031,#110032,#110033,
#110034,#110035,#110036,#110037,#110038,#110039,#110040,#110041,#110042,
#110043,#110044,#110045,#110046,#110047,#110048,#110049,#110050,#110051,
#110052,#110053,#110054,#110055,#110056,#110057,#110058,#110059,#110060,
#110061,#110062,#110063,#110064,#110065,#110066,#110067,#110068,#110069,
#110070,#110071,#110072,#110073,#110074,#110075,#110076,#110077,#110078,
#110079,#110080,#110081,#110082,#110083,#110084,#110085,#110086,#110087,
#110088,#110089,#110090,#110091,#110092,#110093,#110094,#110095,#110096,
#110097,#110098,#110099,#110100,#110101,#110102,#110103,#110104,#110105,
#110106,#110107,#110108,#110109,#110110,#110111,#110112,#110113,#110114,
#110115,#110116,#110117,#110118,#110119,#110120,#110121,#110122,#110123,
#110124,#110125,#110126,#110127,#110128,#110129,#110130,#110131,#110132,
#110133,#110134,#110135,#110136,#110137,#110138,#110139,#110140,#110141,
#110142,#110143,#110144,#110145,#110146,#110147,#110148,#110149,#110150,
#110151,#110152,#110153,#110154,#110155,#110156,#110157,#110158,#110159,
#110160,#110161,#110162,#110163,#110164,#110165,#110166,#110167,#110168,
#110169,#110170,#110171,#110172,#110173,#110174,#110175,#110176,#110177,
#110178,#110179,#110180,#110181,#110182,#110183,#110184,#110185,#110186,
#110187,#110188,#110189,#110190,#110191,#110192,#110193,#110194,#110195,
#110196,#110197,#110198,#110199,#110200,#110201,#110202,#110203,#110204,
#110205,#110206,#110207,#110208,#110209,#110210,#110211,#110212,#110213,
#110214,#110215,#110216,#110217,#110218,#110219,#110220,#110221,#110222,
#110223,#110224,#110225,#110226,#110227,#110228,#110229,#110230,#110231,
#110232,#110233,#110234,#110235,#110236,#110237,#110238,#110239,#110240,
#110241,#110242,#110243,#110244,#110245,#110246,#110247,#110248,#110249,
#110250,#110251,#110252,#110253,#110254,#110255,#110256,#110257,#110258,
#110259,#110260,#110261,#110262,#110263,#110264,#110265,#110266,#110267,
#110268,#110269,#110270,#110271,#110272,#110273,#110274,#110275,#110276,
#110277,#110278,#110279,#110280,#110281,#110282,#110283,#110284,#110285,
#110286,#110287,#110288,#110289,#110290,#110291,#110292,#110293,#110294,
#110295,#110296,#110297,#110298,#110299,#110300,#110301,#110302,#110303,
#110304,#110305,#110306,#110307,#110308,#110309,#110310,#110311,#110312,
#110313,#110314,#110315,#110316,#110317,#110318,#110319,#110320,#110321,
#110322,#110323,#110324,#110325,#110326,#110327,#110328,#110329,#110330,
#110331,#110332,#110333,#110334,#110335,#110336,#110337,#110338,#110339,
#110340,#110341,#110342,#110343,#110344,#110345,#110346,#110347,#110348,
#110349,#110350,#110351,#110352,#110353,#110354,#110355,#110356,#110357,
#110358,#110359,#110360,#110361,#110362,#110363,#110364,#110365,#110366,
#110367,#110368,#110369,#110370,#110371,#110372,#110373,#110374,#110375,
#110376,#110377,#110378,#110379,#110380,#110381,#110382,#110383,#110384,
#110385,#110386,#110387,#110388,#110389,#110390,#110391,#110392,#110393,
#110394,#110395,#110396,#110397,#110398,#110399,#110400,#110401,#110402,
#110403,#110404,#110405,#110406,#110407,#110408,#110409,#110410,#110411,
#110412,#110413,#110414,#110415,#110416,#110417,#110418,#110419,#110420,
#110421,#110422,#110423,#110424,#110425,#110426,#110427,#110428,#110429,
#110430,#110431,#110432,#110433,#110434,#110435,#110436,#110437,#110438,
#110439,#110440,#110441,#110442,#110443,#110444,#110445,#110446,#110447,
#110448,#110449,#110450,#110451,#110452,#110453,#110454,#110455,#110456,
#110457,#110458,#110459,#110460,#110461,#110462,#110463,#110464,#110465,
#110466,#110467,#110468,#110469,#110470,#110471,#110472,#110473,#110474,
#110475,#110476,#110477,#110478,#110479,#110480,#110481,#110482,#110483,
#110484,#110485,#110486,#110487,#110488,#110489,#110490,#110491,#110492,
#110493,#110494,#110495,#110496,#110497,#110498,#110499,#110500,#110501,
#110502,#110503,#110504,#110505,#110506,#110507,#110508,#110509,#110510,
#110511,#110512,#110513,#110514,#110515,#110516,#110517,#110518,#110519,
#110520,#110521,#110522,#110523,#110524,#110525,#110526,#110527,#110528,
#110529,#110530,#110531,#110532,#110533,#110534,#110535,#110536,#110537,
#110538,#110539,#110540,#110541,#110542,#110543,#110544,#110545,#110546,
#110547,#110548,#110549,#110550,#110551,#110552,#110553,#110554,#110555,
#110556,#110557,#110558,#110559,#110560,#110561,#110562,#110563,#110564,
#110565,#110566,#110567,#110568,#110569,#110570,#110571,#110572,#110573,
#110574,#110575,#110576,#110577,#110578,#110579,#110580,#110581,#110582,
#110583,#110584,#110585,#110586,#110587,#110588,#110589,#110590,#110591,
#110592,#110593,#110594,#110595,#110596,#110597,#110598,#110599,#110600,
#110601,#110602,#110603,#110604,#110605,#110606,#110607,#110608,#110609,
#110610,#110611,#110612,#110613,#110614,#110615,#110616,#110617,#110618,
#110619,#110620,#110621,#110622,#110623,#110624,#110625,#110626,#110627,
#110628,#110629,#110630,#110631,#110632,#110633,#110634,#110635,#110636,
#110637,#110638,#110639,#110640,#110641,#110642,#110643,#110644,#110645,
#110646,#110647,#110648,#110649,#110650,#110651,#110652,#110653,#110654,
#110655,#110656,#110657,#110658,#110659,#110660,#110661,#110662,#110663,
#110664,#110665,#110666,#110667,#110668,#110669,#110670,#110671,#110672,
#110673,#110674,#110675,#110676,#110677,#110678,#110679,#110680,#110681,
#110682,#110683,#110684,#110685,#110686,#110687,#110688,#110689,#110690,
#110691,#110692,#110693,#110694,#110695,#110696,#110697,#110698,#110699,
#110700,#110701,#110702,#110703,#110704,#110705,#110706,#110707,#110708,
#110709,#110710,#110711,#110712,#110713,#110714,#110715,#110716,#110717,
#110718,#110719,#110720,#110721,#110722,#110723,#110724,#110725,#110726,
#110727,#110728,#110729,#110730,#110731,#110732,#110733,#110734,#110735,
#110736,#110737,#110738,#110739,#110740,#110741,#110742,#110743,#110744,
#110745,#110746,#110747,#110748,#110749,#110750,#110751,#110752,#110753,
#110754,#110755,#110756,#110757,#110758,#110759,#110760,#110761,#110762,
#110763,#110764,#110765,#110766,#110767,#110768,#110769,#110770,#110771,
#110772,#110773,#110774,#110775,#110776,#110777,#110778,#110779,#110780,
#110781,#110782,#110783,#110784,#110785,#110786,#110787,#110788,#110789,
#110790,#110791,#110792,#110793,#110794,#110795,#110796,#110797,#110798,
#110799,#110800,#110801,#110802,#110803,#110804,#110805,#110806,#110807,
#110808,#110809,#110810,#110811,#110812,#110813,#110814,#110815,#110816,
#110817,#110818,#110819,#110820,#110821,#110822,#110823,#110824,#110825,
#110826,#110827,#110828,#110829,#110830,#110831,#110832,#110833,#110834,
#110835,#110836,#110837,#110838,#110839,#110840,#110841,#110842,#110843,
#110844,#110845,#110846,#110847,#110848,#110849,#110850,#110851,#110852,
#110853,#110854,#110855,#110856,#110857,#110858,#110859,#110860,#110861,
#110862,#110863,#110864,#110865,#110866,#110867,#110868,#110869,#110870,
#110871,#110872,#110873,#110874,#110875,#110876,#110877,#110878,#110879,
#110880,#110881,#110882,#110883,#110884,#110885,#110886,#110887,#110888,
#110889,#110890,#110891,#110892,#110893,#110894,#110895,#110896,#110897,
#110898,#110899,#110900,#110901,#110902,#110903,#110904,#110905,#110906,
#110907,#110908,#110909,#110910,#110911,#110912,#110913,#110914,#110915,
#110916,#110917,#110918,#110919,#110920,#110921,#110922,#110923,#110924,
#110925,#110926,#110927,#110928,#110929,#110930,#110931,#110932,#110933,
#110934,#110935,#110936,#110937,#110938,#110939,#110940,#110941,#110942,
#110943,#110944,#110945,#110946,#110947,#110948,#110949,#110950,#110951,
#110952,#110953,#110954,#110955,#110956,#110957,#110958,#110959,#110960,
#110961,#110962,#110963,#110964,#110965,#110966,#110967,#110968,#110969,
#110970,#110971,#110972,#110973,#110974,#110975,#110976,#110977,#110978,
#110979,#110980,#110981,#110982,#110983,#110984,#110985,#110986,#110987,
#110988,#110989,#110990,#110991,#110992,#110993,#110994,#110995,#110996,
#110997,#110998,#110999,#111000,#111001,#111002,#111003,#111004,#111005,
#111006,#111007,#111008,#111009,#111010,#111011,#111012,#111013,#111014,
#111015,#111016,#111017,#111018,#111019,#111020,#111021,#111022,#111023,
#111024,#111025,#111026,#111027,#111028,#111029,#111030,#111031,#111032,
#111033,#111034,#111035,#111036,#111037,#111038,#111039,#111040,#111041,
#111042,#111043,#111044,#111045,#111046,#111047,#111048,#111049,#111050,
#111051,#111052,#111053,#111054,#111055,#111056,#111057,#111058,#111059,
#111060,#111061,#111062,#111063,#111064,#111065,#111066,#111067,#111068,
#111069,#111070,#111071,#111072,#111073,#111074,#111075,#111076,#111077,
#111078,#111079,#111080,#111081,#111082,#111083,#111084,#111085,#111086,
#111087,#111088,#111089,#111090,#111091,#111092,#111093,#111094,#111095,
#111096,#111097,#111098,#111099,#111100,#111101,#111102,#111103,#111104,
#111105,#111106,#111107,#111108,#111109,#111110,#111111,#111112,#111113,
#111114,#111115,#111116,#111117,#111118,#111119,#111120,#111121,#111122,
#111123,#111124,#111125,#111126,#111127,#111128,#111129,#111130,#111131,
#111132,#111133,#111134,#111135,#111136,#111137,#111138,#111139,#111140,
#111141,#111142,#111143,#111144,#111145,#111146,#111147,#111148,#111149,
#111150,#111151,#111152,#111153,#111154,#111155,#111156,#111157,#111158,
#111159,#111160,#111161,#111162,#111163,#111164,#111165,#111166,#111167,
#111168,#111169,#111170,#111171,#111172,#111173,#111174,#111175,#111176,
#111177,#111178,#111179,#111180,#111181,#111182,#111183,#111184,#111185,
#111186,#111187,#111188,#111189,#111190,#111191,#111192,#111193,#111194,
#111195,#111196,#111197,#111198,#111199,#111200,#111201,#111202,#111203,
#111204,#111205,#111206,#111207,#111208,#111209,#111210,#111211,#111212,
#111213,#111214,#111215,#111216,#111217,#111218,#111219,#111220,#111221,
#111222,#111223,#111224,#111225,#111226,#111227,#111228,#111229,#111230,
#111231,#111232,#111233,#111234,#111235,#111236,#111237,#111238,#111239,
#111240,#111241,#111242,#111243,#111244,#111245,#111246,#111247,#111248,
#111249,#111250,#111251,#111252,#111253,#111254,#111255,#111256,#111257,
#111258,#111259,#111260,#111261,#111262,#111263,#111264,#111265,#111266,
#111267,#111268,#111269,#111270,#111271,#111272,#111273,#111274,#111275,
#111276,#111277,#111278,#111279,#111280,#111281,#111282,#111283,#111284,
#111285,#111286,#111287,#111288,#111289,#111290,#111291,#111292,#111293,
#111294,#111295,#111296,#111297,#111298,#111299,#111300,#111301,#111302,
#111303,#111304,#111305,#111306,#111307,#111308,#111309,#111310,#111311,
#111312,#111313,#111314,#111315,#111316,#111317,#111318,#111319,#111320,
#111321,#111322,#111323,#111324,#111325,#111326,#111327,#111328,#111329,
#111330,#111331,#111332,#111333,#111334,#111335,#111336,#111337,#111338,
#111339,#111340,#111341,#111342,#111343,#111344,#111345,#111346,#111347,
#111348,#111349,#111350,#111351,#111352,#111353,#111354,#111355,#111356,
#111357,#111358,#111359,#111360,#111361,#111362,#111363,#111364,#111365,
#111366,#111367,#111368,#111369,#111370,#111371,#111372,#111373,#111374,
#111375,#111376,#111377,#111378,#111379,#111380,#111381,#111382,#111383,
#111384,#111385,#111386,#111387,#111388,#111389,#111390,#111391,#111392,
#111393,#111394,#111395,#111396,#111397,#111398,#111399,#111400,#111401,
#111402,#111403,#111404,#111405,#111406,#111407,#111408,#111409,#111410,
#111411,#111412,#111413,#111414,#111415,#111416,#111417,#111418,#111419,
#111420,#111421,#111422,#111423,#111424,#111425,#111426,#111427,#111428,
#111429,#111430,#111431,#111432,#111433,#111434,#111435,#111436,#111437,
#111438,#111439,#111440,#111441,#111442,#111443,#111444,#111445,#111446,
#111447,#111448,#111449,#111450,#111451,#111452,#111453,#111454,#111455,
#111456,#111457,#111458,#111459,#111460,#111461,#111462,#111463,#111464,
#111465,#111466,#111467,#111468,#111469,#111470,#111471,#111472,#111473,
#111474,#111475,#111476,#111477,#111478,#111479,#111480,#111481,#111482,
#111483,#111484,#111485,#111486,#111487,#111488,#111489,#111490,#111491,
#111492,#111493,#111494,#111495,#111496,#111497,#111498,#111499,#111500,
#111501,#111502,#111503,#111504,#111505,#111506,#111507,#111508,#111509,
#111510,#111511,#111512,#111513,#111514,#111515,#111516,#111517,#111518,
#111519,#111520,#111521,#111522,#111523,#111524,#111525,#111526,#111527,
#111528,#111529,#111530,#111531,#111532,#111533,#111534,#111535,#111536,
#111537,#111538,#111539,#111540,#111541,#111542,#111543,#111544,#111545,
#111546,#111547,#111548,#111549,#111550,#111551,#111552,#111553,#111554,
#111555,#111556,#111557,#111558,#111559,#111560,#111561,#111562,#111563,
#111564,#111565,#111566,#111567,#111568,#111569,#111570,#111571,#111572,
#111573,#111574,#111575,#111576,#111577,#111578,#111579,#111580,#111581,
#111582,#111583,#111584,#111585,#111586,#111587,#111588,#111589,#111590,
#111591,#111592,#111593,#111594,#111595,#111596,#111597,#111598,#111599,
#111600,#111601,#111602,#111603,#111604,#111605,#111606,#111607,#111608,
#111609,#111610,#111611,#111612,#111613,#111614,#111615,#111616,#111617,
#111618,#111619,#111620,#111621,#111622,#111623,#111624,#111625,#111626,
#111627,#111628,#111629,#111630,#111631,#111632,#111633,#111634,#111635,
#111636,#111637,#111638,#111639,#111640,#111641,#111642,#111643,#111644,
#111645,#111646,#111647,#111648,#111649,#111650,#111651,#111652,#111653,
#111654,#111655,#111656,#111657,#111658,#111659,#111660,#111661,#111662,
#111663,#111664,#111665,#111666,#111667,#111668,#111669,#111670,#111671,
#111672,#111673,#111674,#111675,#111676,#111677,#111678,#111679,#111680,
#111681,#111682,#111683,#111684,#111685,#111686,#111687,#111688,#111689,
#111690,#111691,#111692,#111693,#111694,#111695,#111696,#111697,#111698,
#111699,#111700,#111701,#111702,#111703,#111704,#111705,#111706,#111707,
#111708,#111709,#111710,#111711,#111712,#111713,#111714,#111715,#111716,
#111717,#111718,#111719,#111720,#111721,#111722,#111723,#111724,#111725,
#111726,#111727,#111728,#111729,#111730,#111731,#111732,#111733,#111734,
#111735,#111736,#111737,#111738,#111739,#111740,#111741,#111742,#111743,
#111744,#111745,#111746,#111747,#111748,#111749,#111750,#111751,#111752,
#111753,#111754,#111755,#111756,#111757,#111758,#111759,#111760,#111761,
#111762,#111763,#111764,#111765,#111766,#111767,#111768,#111769,#111770,
#111771,#111772,#111773,#111774,#111775,#111776,#111777,#111778,#111779,
#111780,#111781,#111782,#111783,#111784,#111785,#111786,#111787,#111788,
#111789,#111790,#111791,#111792,#111793,#111794,#111795,#111796,#111797,
#111798,#111799,#111800,#111801,#111802,#111803,#111804,#111805,#111806,
#111807,#111808,#111809,#111810,#111811,#111812,#111813,#111814,#111815,
#111816,#111817,#111818,#111819,#111820,#111821,#111822,#111823,#111824,
#111825,#111826,#111827,#111828,#111829,#111830,#111831,#111832,#111833,
#111834,#111835,#111836,#111837,#111838,#111839,#111840,#111841,#111842,
#111843,#111844,#111845,#111846,#111847,#111848,#111849,#111850,#111851,
#111852,#111853,#111854,#111855,#111856,#111857,#111858,#111859,#111860,
#111861,#111862,#111863,#111864,#111865,#111866,#111867,#111868,#111869,
#111870,#111871,#111872,#111873,#111874,#111875,#111876,#111877,#111878,
#111879,#111880,#111881,#111882,#111883,#111884,#111885,#111886,#111887,
#111888,#111889,#111890,#111891,#111892,#111893,#111894,#111895,#111896,
#111897,#111898,#111899,#111900,#111901,#111902,#111903,#111904,#111905,
#111906,#111907,#111908,#111909,#111910,#111911,#111912,#111913,#111914,
#111915,#111916,#111917,#111918,#111919,#111920,#111921,#111922,#111923,
#111924,#111925,#111926,#111927,#111928,#111929,#111930,#111931,#111932,
#111933,#111934,#111935,#111936,#111937,#111938,#111939,#111940,#111941,
#111942,#111943,#111944,#111945,#111946,#111947,#111948,#111949,#111950,
#111951,#111952,#111953,#111954,#111955,#111956,#111957,#111958,#111959,
#111960,#111961,#111962,#111963,#111964,#111965,#111966,#111967,#111968,
#111969,#111970,#111971,#111972,#111973,#111974,#111975,#111976,#111977,
#111978,#111979,#111980,#111981,#111982,#111983,#111984,#111985,#111986,
#111987,#111988,#111989,#111990,#111991,#111992,#111993,#111994,#111995,
#111996,#111997,#111998,#111999,#112000,#112001,#112002,#112003,#112004,
#112005,#112006,#112007,#112008,#112009,#112010,#112011,#112012,#112013,
#112014,#112015,#112016,#112017,#112018,#112019,#112020,#112021,#112022,
#112023,#112024,#112025,#112026,#112027,#112028,#112029,#112030,#112031,
#112032,#112033,#112034,#112035,#112036,#112037,#112038,#112039,#112040,
#112041,#112042,#112043,#112044,#112045,#112046,#112047,#112048,#112049,
#112050,#112051,#112052,#112053,#112054,#112055,#112056,#112057,#112058,
#112059,#112060,#112061,#112062,#112063,#112064,#112065,#112066,#112067,
#112068,#112069,#112070,#112071,#112072,#112073,#112074,#112075,#112076,
#112077,#112078,#112079,#112080,#112081,#112082,#112083,#112084,#112085,
#112086,#112087,#112088,#112089,#112090,#112091,#112092,#112093,#112094,
#112095,#112096,#112097,#112098,#112099,#112100,#112101,#112102,#112103,
#112104,#112105,#112106,#112107,#112108,#112109,#112110,#112111,#112112,
#112113,#112114,#112115,#112116,#112117,#112118,#112119,#112120,#112121,
#112122,#112123,#112124,#112125,#112126,#112127,#112128,#112129,#112130,
#112131,#112132,#112133,#112134,#112135,#112136,#112137,#112138,#112139,
#112140,#112141,#112142,#112143,#112144,#112145,#112146,#112147,#112148,
#112149,#112150,#112151,#112152,#112153,#112154,#112155,#112156,#112157,
#112158,#112159,#112160,#112161,#112162,#112163,#112164,#112165,#112166,
#112167,#112168,#112169,#112170,#112171,#112172,#112173,#112174,#112175,
#112176,#112177,#112178,#112179,#112180,#112181,#112182,#112183,#112184,
#112185,#112186,#112187,#112188,#112189,#112190,#112191,#112192,#112193,
#112194,#112195,#112196,#112197,#112198,#112199,#112200,#112201,#112202,
#112203,#112204,#112205,#112206,#112207,#112208,#112209,#112210,#112211,
#112212,#112213,#112214,#112215,#112216,#112217,#112218,#112219,#112220,
#112221,#112222,#112223,#112224,#112225,#112226,#112227,#112228,#112229,
#112230,#112231,#112232,#112233,#112234,#112235,#112236,#112237,#112238,
#112239,#112240,#112241,#112242,#112243,#112244,#112245,#112246,#112247,
#112248,#112249,#112250,#112251,#112252,#112253,#112254,#112255,#112256,
#112257,#112258,#112259,#112260,#112261,#112262,#112263,#112264,#112265,
#112266,#112267,#112268,#112269,#112270,#112271,#112272,#112273,#112274,
#112275,#112276,#112277,#112278,#112279,#112280,#112281,#112282,#112283,
#112284,#112285,#112286,#112287,#112288,#112289,#112290,#112291,#112292,
#112293,#112294,#112295,#112296,#112297,#112298,#112299,#112300,#112301,
#112302,#112303,#112304,#112305,#112306,#112307,#112308,#112309,#112310,
#112311,#112312,#112313,#112314,#112315,#112316,#112317,#112318,#112319,
#112320,#112321,#112322,#112323,#112324,#112325,#112326,#112327,#112328,
#112329,#112330,#112331,#112332,#112333,#112334,#112335,#112336,#112337,
#112338,#112339,#112340,#112341,#112342,#112343,#112344,#112345,#112346,
#112347,#112348,#112349,#112350,#112351,#112352,#112353,#112354,#112355,
#112356,#112357,#112358,#112359,#112360,#112361,#112362,#112363,#112364,
#112365,#112366,#112367,#112368,#112369,#112370,#112371,#112372,#112373,
#112374,#112375,#112376,#112377,#112378,#112379,#112380,#112381,#112382,
#112383,#112384,#112385,#112386,#112387,#112388,#112389,#112390,#112391,
#112392,#112393,#112394,#112395,#112396,#112397,#112398,#112399,#112400,
#112401,#112402,#112403,#112404,#112405,#112406,#112407,#112408,#112409,
#112410,#112411,#112412,#112413,#112414,#112415,#112416,#112417,#112418,
#112419,#112420,#112421,#112422,#112423,#112424,#112425,#112426,#112427,
#112428,#112429,#112430,#112431,#112432,#112433,#112434,#112435,#112436,
#112437,#112438,#112439,#112440,#112441,#112442,#112443,#112444,#112445,
#112446,#112447,#112448,#112449,#112450,#112451,#112452,#112453,#112454,
#112455,#112456,#112457,#112458,#112459,#112460,#112461,#112462,#112463,
#112464,#112465,#112466,#112467,#112468,#112469,#112470,#112471,#112472,
#112473,#112474,#112475,#112476,#112477,#112478,#112479,#112480,#112481,
#112482,#112483,#112484,#112485,#112486,#112487,#112488,#112489,#112490,
#112491,#112492,#112493,#112494,#112495,#112496,#112497,#112498,#112499,
#112500,#112501,#112502,#112503,#112504,#112505,#112506,#112507,#112508,
#112509,#112510,#112511,#112512,#112513,#112514,#112515,#112516,#112517,
#112518,#112519,#112520,#112521,#112522,#112523,#112524,#112525,#112526,
#112527,#112528,#112529,#112530,#112531,#112532,#112533,#112534,#112535,
#112536,#112537,#112538,#112539,#112540,#112541,#112542,#112543,#112544,
#112545,#112546,#112547,#112548,#112549,#112550,#112551,#112552,#112553,
#112554,#112555,#112556,#112557,#112558,#112559,#112560,#112561,#112562,
#112563,#112564,#112565,#112566,#112567,#112568,#112569,#112570,#112571,
#112572,#112573,#112574,#112575,#112576,#112577,#112578,#112579,#112580,
#112581,#112582,#112583,#112584,#112585,#112586,#112587,#112588,#112589,
#112590,#112591,#112592,#112593,#112594,#112595,#112596,#112597,#112598,
#112599,#112600,#112601,#112602,#112603,#112604,#112605,#112606,#112607,
#112608,#112609,#112610,#112611,#112612,#112613,#112614,#112615,#112616,
#112617,#112618,#112619,#112620,#112621,#112622,#112623,#112624,#112625,
#112626,#112627,#112628,#112629,#112630,#112631,#112632,#112633,#112634,
#112635,#112636,#112637,#112638,#112639,#112640,#112641,#112642,#112643,
#112644,#112645,#112646,#112647,#112648,#112649,#112650,#112651,#112652,
#112653,#112654,#112655,#112656,#112657,#112658,#112659,#112660,#112661,
#112662,#112663,#112664,#112665,#112666,#112667,#112668,#112669,#112670,
#112671,#112672,#112673,#112674,#112675,#112676,#112677,#112678,#112679,
#112680,#112681,#112682,#112683,#112684,#112685,#112686,#112687,#112688,
#112689,#112690,#112691,#112692,#112693,#112694,#112695,#112696,#112697,
#112698,#112699,#112700,#112701,#112702,#112703,#112704,#112705,#112706,
#112707,#112708,#112709,#112710,#112711,#112712,#112713,#112714,#112715,
#112716,#112717,#112718,#112719,#112720,#112721,#112722,#112723,#112724,
#112725,#112726,#112727,#112728,#112729,#112730,#112731,#112732,#112733,
#112734,#112735,#112736,#112737,#112738,#112739,#112740,#112741,#112742,
#112743,#112744,#112745,#112746,#112747,#112748,#112749,#112750,#112751,
#112752,#112753,#112754,#112755,#112756,#112757,#112758,#112759,#112760,
#112761,#112762,#112763,#112764,#112765,#112766,#112767,#112768,#112769,
#112770,#112771,#112772,#112773,#112774,#112775,#112776,#112777,#112778,
#112779,#112780,#112781,#112782,#112783,#112784,#112785,#112786,#112787)),
 .UNSPECIFIED.,.F.,.F.,.F.,(2,2),(4,1,1,1,1,1,1,1,1,1,1,1,1,1,1,1,1,1,1,
1,1,1,1,1,1,1,1,1,1,1,1,1,1,1,1,1,1,1,1,1,1,1,1,1,1,1,1,1,1,1,1,1,1,1,1,
1,1,1,1,1,1,1,1,1,1,1,1,1,1,1,1,1,1,1,1,1,1,1,1,1,1,1,1,1,1,1,1,1,1,1,1,
1,1,1,1,1,1,1,1,1,1,1,1,1,1,1,1,1,1,1,1,1,1,1,1,1,1,1,1,1,1,1,1,1,1,1,1,
1,1,1,1,1,1,1,1,1,1,1,1,1,1,1,1,1,1,1,1,1,1,1,1,1,1,1,1,1,1,1,1,1,1,1,1,
1,1,1,1,1,1,1,1,1,1,1,1,1,1,1,1,1,1,1,1,1,1,1,1,1,1,1,1,1,1,1,1,1,1,1,1,
1,1,1,1,1,1,1,1,1,1,1,1,1,1,1,1,1,1,1,1,1,1,1,1,1,1,1,1,1,1,1,1,1,1,1,1,
1,1,1,1,1,1,1,1,1,1,1,1,1,1,1,1,1,1,1,1,1,1,1,1,1,1,1,1,1,1,1,1,1,1,1,1,
1,1,1,1,1,1,1,1,1,1,1,1,1,1,1,1,1,1,1,1,1,1,1,1,1,1,1,1,1,1,1,1,1,1,1,1,
1,1,1,1,1,1,1,1,1,1,1,1,1,1,1,1,1,1,1,1,1,1,1,1,1,1,1,1,1,1,1,1,1,1,1,1,
1,1,1,1,1,1,1,1,1,1,1,1,1,1,1,1,1,1,1,1,1,1,1,1,1,1,1,1,1,1,1,1,1,1,1,1,
1,1,1,1,1,1,1,1,1,1,1,1,1,1,1,1,1,1,1,1,1,1,1,1,1,1,1,1,1,1,1,1,1,1,1,1,
1,1,1,1,1,1,1,1,1,1,1,1,1,1,1,1,1,1,1,1,1,1,1,1,1,1,1,1,1,1,1,1,1,1,1,1,
1,1,1,1,1,1,1,1,1,1,1,1,1,1,1,1,1,1,1,1,1,1,1,1,1,1,1,1,1,1,1,1,1,1,1,1,
1,1,1,1,1,1,1,1,1,1,1,1,1,1,1,1,1,1,1,1,1,1,1,1,1,1,1,1,1,1,1,1,1,1,1,1,
1,1,1,1,1,1,1,1,1,1,1,1,1,1,1,1,1,1,1,1,1,1,1,1,1,1,1,1,1,1,1,1,1,1,1,1,
1,1,1,1,1,1,1,1,1,1,1,1,1,1,1,1,1,1,1,1,1,1,1,1,1,1,1,1,1,1,1,1,1,1,1,1,
1,1,1,1,1,1,1,1,1,1,1,1,1,1,1,1,1,1,1,1,1,1,1,1,1,1,1,1,1,1,1,1,1,1,1,1,
1,1,1,1,1,1,1,1,1,1,1,1,1,1,1,1,1,1,1,1,1,1,1,1,1,1,1,1,1,1,1,1,1,1,1,1,
1,1,1,1,1,1,1,1,1,1,1,1,1,1,1,1,1,1,1,1,1,1,1,1,1,1,1,1,1,1,1,1,1,1,1,1,
1,1,1,1,1,1,1,1,1,1,1,1,1,1,1,1,1,1,1,1,1,1,1,1,1,1,1,1,1,1,1,1,1,1,1,1,
1,1,1,1,1,1,1,1,1,1,1,1,1,1,1,1,1,1,1,1,1,1,1,1,1,1,1,1,1,1,1,1,1,1,1,1,
1,1,1,1,1,1,1,1,1,1,1,1,1,1,1,1,1,1,1,1,1,1,1,1,1,1,1,1,1,1,1,1,1,1,1,1,
1,1,1,1,1,1,1,1,1,1,1,1,1,1,1,1,1,1,1,1,1,1,1,1,1,1,1,1,1,1,1,1,1,1,1,1,
1,1,1,1,1,1,1,1,1,1,1,1,1,1,1,1,1,1,1,1,1,1,1,1,1,1,1,1,1,1,1,1,1,1,1,1,
1,1,1,1,1,1,1,1,1,1,1,1,1,1,1,1,1,1,1,1,1,1,1,1,1,1,1,1,1,1,1,1,1,1,1,1,
1,1,1,1,1,1,1,1,1,1,1,1,1,1,1,1,1,1,1,1,1,1,1,1,1,1,1,1,1,1,1,1,1,1,1,1,
1,1,1,1,1,1,1,1,1,1,1,1,1,1,1,1,1,1,1,1,1,1,1,1,1,1,1,1,1,1,1,1,1,1,1,1,
1,1,1,1,1,1,1,1,1,1,1,1,1,1,1,1,1,1,1,1,1,1,1,1,1,1,1,1,1,1,1,1,1,1,1,1,
1,1,1,1,1,1,1,1,1,1,1,1,1,1,1,1,1,1,1,1,1,1,1,1,1,1,1,1,1,1,1,1,1,1,1,1,
1,1,1,1,1,1,1,1,1,1,1,1,1,1,1,1,1,1,1,1,1,1,1,1,1,1,1,1,1,1,1,1,1,1,1,1,
1,1,1,1,1,1,1,1,1,1,1,1,1,1,1,1,1,1,1,1,1,1,1,1,1,1,1,1,1,1,1,1,1,1,1,1,
1,1,1,1,1,1,1,1,1,1,1,1,1,1,1,1,1,1,1,1,1,1,1,1,1,1,1,1,1,1,1,1,1,1,1,1,
1,1,1,1,1,1,1,1,1,1,1,1,1,1,1,1,1,1,1,1,1,1,1,1,1,1,1,1,1,1,1,1,1,1,1,1,
1,1,1,1,1,1,1,1,1,1,1,1,1,1,1,1,1,1,1,1,1,1,1,1,1,1,1,1,1,1,1,1,1,1,1,1,
1,1,1,1,1,1,1,1,1,1,1,1,1,1,1,1,1,1,1,1,1,1,1,1,1,1,1,1,1,1,1,1,1,1,1,1,
1,1,1,1,1,1,1,1,1,1,1,1,1,1,1,1,1,1,1,1,1,1,1,1,1,1,1,1,1,1,1,1,1,1,1,1,
1,1,1,1,1,1,1,1,1,1,1,1,1,1,1,1,1,1,1,1,1,1,1,1,1,1,1,1,1,1,1,1,1,1,1,1,
1,1,1,1,1,1,1,1,1,1,1,1,1,1,1,1,1,1,1,1,1,1,1,1,1,1,1,1,1,1,1,1,1,1,1,1,
1,1,1,1,1,1,1,1,1,1,1,1,1,1,1,1,1,1,1,1,1,1,1,1,1,1,1,1,1,1,1,1,1,1,1,1,
1,1,1,1,1,1,1,1,1,1,1,1,1,1,1,1,1,1,1,1,1,1,1,1,1,1,1,1,1,1,1,1,1,1,1,1,
1,1,1,1,1,1,1,1,1,1,1,1,1,1,1,1,1,1,1,1,1,1,1,1,1,1,1,1,1,1,1,1,1,1,1,1,
1,1,1,1,1,1,1,1,1,1,1,1,1,1,1,1,1,1,1,1,1,1,1,1,1,1,1,1,1,1,1,1,1,1,1,1,
1,1,1,1,1,1,1,1,1,1,1,1,1,1,1,1,1,1,1,1,1,1,1,1,1,1,1,1,1,1,1,1,1,1,1,1,
1,1,1,1,1,1,1,1,1,1,1,1,1,1,1,1,1,1,1,1,1,1,1,1,1,1,1,1,1,1,1,1,1,1,1,1,
1,1,1,1,1,1,1,1,1,1,1,1,1,1,1,1,1,1,1,1,1,1,1,1,1,1,1,1,1,1,1,1,1,1,1,1,
1,1,1,1,1,1,1,1,1,1,1,1,1,1,1,1,1,1,1,1,1,1,1,1,1,1,1,1,1,1,1,1,1,1,1,1,
1,1,1,1,1,1,1,1,1,1,1,1,1,1,1,1,1,1,1,1,1,1,1,1,1,1,1,1,1,1,1,1,1,1,1,1,
1,1,1,1,1,1,1,1,1,1,1,1,1,1,1,1,1,1,1,1,1,1,1,1,1,1,1,1,1,1,1,1,1,1,1,1,
1,1,1,1,1,1,1,1,1,1,1,1,1,1,1,1,1,1,1,1,1,1,1,1,1,1,1,1,1,1,1,1,1,1,1,1,
1,1,1,1,1,1,1,1,1,1,1,1,1,1,1,1,1,1,1,1,1,1,1,1,1,1,1,1,1,1,1,1,1,1,1,1,
1,1,1,1,1,1,1,1,1,1,1,1,1,1,1,1,1,1,1,1,1,1,1,1,1,1,1,1,1,1,1,1,1,1,1,1,
1,1,1,1,1,1,1,1,1,1,1,1,1,1,1,1,1,1,1,1,1,1,1,1,1,1,1,1,1,1,1,1,1,1,1,1,
1,1,1,1,1,1,1,1,1,1,1,1,1,1,1,1,1,1,1,1,1,1,1,1,1,1,1,1,1,1,1,1,1,1,1,1,
1,1,1,1,1,1,1,1,1,1,1,1,1,1,1,1,1,1,1,1,1,1,1,1,1,1,1,1,1,1,1,1,1,1,1,1,
1,1,1,1,1,1,1,1,1,1,1,1,1,1,1,1,1,1,1,1,1,1,1,1,1,1,1,1,1,1,1,1,1,1,1,1,
1,1,1,1,1,1,1,1,1,1,1,1,1,1,1,1,1,1,1,1,1,1,1,1,1,1,1,1,1,1,1,1,1,1,1,1,
1,1,1,1,1,1,1,1,1,1,1,1,1,1,1,1,1,1,1,1,1,1,1,1,1,1,1,1,1,1,1,1,1,1,1,1,
1,1,1,1,1,1,1,1,1,1,1,1,1,1,1,1,1,1,1,1,1,1,1,1,1,1,1,1,1,1,1,1,1,1,1,1,
1,1,1,1,1,1,1,1,1,1,1,1,1,1,1,1,1,1,1,1,1,1,1,1,1,1,1,1,1,1,1,1,1,1,1,1,
1,1,1,1,1,1,1,1,1,1,1,1,1,1,1,1,1,1,1,1,1,1,1,1,1,1,1,1,1,1,1,1,1,1,1,1,
1,1,1,1,1,1,1,1,1,1,1,1,1,1,1,1,1,1,1,1,1,1,1,1,1,1,1,1,1,1,1,1,1,1,1,1,
1,1,1,1,1,1,1,1,1,1,1,1,1,1,1,1,1,1,1,1,1,1,1,1,1,1,1,1,1,1,1,1,1,1,1,1,
1,1,1,1,1,1,1,1,1,1,1,1,1,1,1,1,1,1,1,1,1,1,1,1,1,1,1,1,1,1,1,1,1,1,1,1,
1,1,1,1,1,1,1,1,1,1,1,1,1,1,1,1,1,1,1,1,1,1,1,1,1,1,1,1,1,1,1,1,1,1,1,1,
1,1,1,1,1,1,1,1,1,1,1,1,1,1,1,1,1,1,1,1,1,1,1,1,1,1,1,1,1,1,1,1,1,1,1,1,
1,1,1,1,1,1,1,1,1,1,1,1,1,1,1,1,1,1,1,1,1,1,1,1,1,1,1,1,1,1,1,1,1,1,1,1,
1,1,1,1,1,1,1,1,1,1,1,1,1,1,1,1,1,1,1,1,1,1,1,1,1,1,1,1,1,1,1,1,1,1,1,1,
1,1,1,1,1,1,1,1,1,1,1,1,1,1,1,1,1,1,1,1,1,1,1,1,1,1,1,1,1,1,1,1,1,1,1,1,
1,1,1,1,1,1,1,1,1,1,1,1,1,1,1,1,1,1,1,1,1,1,1,1,1,1,1,1,1,1,1,1,1,1,1,1,
1,1,1,1,1,1,1,1,1,1,1,1,1,1,1,1,1,1,1,1,1,1,1,1,1,1,1,1,1,1,1,1,1,1,1,1,
1,1,1,1,1,1,1,1,1,1,1,1,1,1,1,1,1,1,1,1,1,1,1,1,1,1,1,1,1,1,1,1,1,1,1,1,
1,1,1,1,1,1,1,1,1,1,1,1,1,1,1,1,1,1,1,1,1,1,1,1,1,1,1,1,1,1,1,1,1,1,1,1,
1,1,1,1,1,1,1,1,1,1,1,1,1,1,1,1,1,1,1,1,1,1,1,1,1,1,1,1,1,1,1,1,1,1,1,1,
1,1,1,1,1,1,1,1,1,1,1,1,1,1,1,1,1,1,1,1,1,1,1,1,1,1,1,1,1,1,1,1,1,1,1,1,
1,1,1,1,1,1,1,1,1,1,1,1,1,1,1,1,1,1,1,1,1,1,1,1,1,1,1,1,1,1,1,1,1,1,1,1,
1,1,1,1,1,1,1,1,1,1,1,1,1,1,1,1,1,1,1,1,1,1,1,1,1,1,1,1,1,1,1,1,1,1,1,1,
1,1,1,1,1,1,1,1,1,1,1,1,1,1,1,1,1,1,1,1,1,1,1,1,1,1,1,1,1,1,1,1,1,1,1,1,
1,1,1,1,1,1,1,1,1,1,1,1,1,1,1,1,1,1,1,1,1,1,1,1,1,1,1,1,1,1,1,1,1,1,1,1,
1,1,1,1,1,1,1,1,1,1,1,1,1,1,1,1,1,1,1,1,1,1,1,1,1,1,1,1,1,1,1,1,1,1,1,1,
1,1,1,1,1,1,1,1,1,1,1,1,1,1,1,1,1,1,1,1,1,1,1,1,1,1,1,1,1,1,1,1,1,1,1,1,
1,1,1,1,1,1,1,1,1,1,1,1,1,1,1,1,1,1,1,1,1,1,1,1,1,1,1,1,1,1,1,1,1,1,1,1,
1,1,1,1,1,1,1,1,1,1,1,1,1,1,1,1,1,1,1,1,1,1,1,1,1,1,1,1,1,1,1,1,1,1,1,1,
1,1,1,1,1,1,1,1,1,1,1,1,1,1,1,1,1,1,1,1,1,1,1,1,1,1,1,1,1,1,1,1,1,1,1,1,
1,1,1,1,1,1,1,1,1,1,1,1,1,1,1,1,1,1,1,1,1,1,1,1,1,1,1,1,1,1,1,1,1,1,1,1,
1,1,1,1,1,1,1,1,1,1,1,1,1,1,1,1,1,1,1,1,1,1,1,1,1,1,1,1,1,1,1,1,1,1,1,1,
1,1,1,1,1,1,1,1,1,1,1,1,1,1,1,1,1,1,1,1,1,1,1,1,1,1,1,1,1,1,1,1,1,1,1,1,
1,1,1,1,1,1,1,1,1,1,1,1,1,1,1,1,1,1,1,1,1,1,1,1,1,1,1,1,1,1,1,1,1,1,1,1,
1,1,1,1,1,1,1,1,1,1,1,1,1,1,1,1,1,1,1,1,1,1,1,1,1,1,1,1,1,1,1,1,1,1,1,1,
1,1,1,1,1,1,1,1,1,1,1,1,1,1,1,1,1,1,1,1,1,1,1,1,1,1,1,1,1,1,1,1,1,1,1,1,
1,1,1,1,1,1,1,1,1,1,1,1,1,1,1,1,1,1,1,1,1,1,1,1,1,1,1,1,1,1,1,1,1,1,1,1,
1,1,1,1,1,1,1,1,1,1,1,1,1,1,1,1,1,1,1,1,1,1,1,1,1,1,1,1,1,1,1,1,1,1,1,1,
1,1,1,1,1,1,1,1,1,1,1,1,1,1,1,1,1,1,1,1,1,1,1,1,1,1,1,1,1,1,1,1,1,1,1,1,
1,1,1,1,1,1,1,1,1,1,1,1,1,1,1,1,1,1,1,1,1,1,1,1,1,1,1,1,1,1,1,1,1,1,1,1,
1,1,1,1,1,1,1,1,1,1,1,1,1,1,1,1,1,1,1,1,1,1,1,1,1,1,1,1,1,1,1,1,1,1,1,1,
1,1,1,1,1,1,1,1,1,1,1,1,1,1,1,1,1,1,1,1,1,1,1,1,1,1,1,1,1,1,1,1,1,1,1,1,
1,1,1,1,1,1,1,1,1,1,1,1,1,1,1,1,1,1,1,1,1,1,1,1,1,1,1,1,1,1,1,1,1,1,1,1,
1,1,1,1,1,1,1,4),(-1.76619037896906,-1.18309518948453),(0.,0.869746702321014,
1.7394931589914,2.60923976624962,3.47983908319159,4.35043840179749,5.22018503077054,
6.08993165951504,6.95967828799171,7.82942491616733,8.69917154401062,9.56891817149224,
10.4395174886835,11.3101168056706,12.179863432132,13.049610058144,13.9193566836854,
14.7891033087372,15.6588499332817,16.5285965573034,17.3991958717975,18.2697951860185,
18.7046684974166,19.1395418086746,19.5744151197912,20.0092884307654,20.4441617415962,
20.8790350522825,21.7487816732187,22.1836549834672,22.6185282935685,23.0534016035221,
23.4882749133276,23.9231482229848,24.3588742245859,24.794600226187,25.2294735355468,
26.0992201538203,26.5340934627341,26.9689667714994,27.4038400801166,27.838713388586,
28.2735866969081,28.7084600050832,29.143333313112,29.5782066209952,30.0130799287334,
30.4479532363275,30.8828265437783,31.3185525442794,31.7542785447804,32.1891518519474,
32.6240251589741,33.0588984658616,33.4937717726112,33.928645079224,34.3635183857014,
34.7983916920448,35.2332649982556,35.6681383043353,36.1030116102854,36.5378849161076,
36.9727582218035,37.4076315273749,37.8425048328235,38.2782308323341,38.7139568318446,
39.1488301370532,39.5837034421446,40.0185767471208,40.4534500519838,40.8883233567357,
41.3231966613787,41.7580699659148,42.1929432703463,42.6278165746754,43.0626898789044,
43.4975631830356,43.9324364870714,44.3673097910142,44.8021830948664,45.2379090935952,
45.673635092324,46.1085083960024,46.5433816995978,46.9782550031127,47.4131283065497,
47.8480016099115,48.2828749132006,48.7177482164198,49.1526215195718,49.5874948226593,
50.0223681256851,50.457241428652,50.8921147315628,51.3269880344203,51.7618613372274,
52.197587335454,52.6333133336805,53.0681866363954,53.5030599390685,53.9379332417027,
54.3728065443011,54.8076798468664,55.2425531494018,55.6774264519101,56.1122997543943,
56.5471730568575,56.9820463593026,57.4169196617326,57.8517929641506,58.2866662665595,
58.7215395689624,59.157265567009,59.5929915650557,60.0278648674556,60.4627381698584,
60.8976114722673,61.3324847746853,61.7673580771153,62.2022313795604,62.6371046820236,
63.0719779845079,63.5068512870162,63.9417245895516,64.376597892117,64.8114711947155,
65.2463444973499,65.6812178000231,66.1169437982275,66.5526697964318,66.9875430991915,
67.4224164019987,67.8572897048563,68.2921630077673,68.7270363107343,69.1619096137603,
69.5967829168479,70.0316562200001,70.4665295232194,70.9014028265087,71.3362761298705,
71.7711494333077,72.2060227368227,72.6408960404182,73.0766220391044,73.5123480377905,
73.9472213415547,74.382094645407,74.8169679493499,75.2518412533859,75.6867145575172,
76.1215878617464,76.5564611660756,76.9913344705072,77.4262077750435,77.8610810796866,
78.2959543844386,78.7308276893018,79.1657009942781,79.6005742993696,80.0363002988208,
80.4720262982719,80.9068996035997,81.3417729090484,81.7766462146199,82.211519520316,
82.6463928261383,83.0812661320886,83.5161394381684,83.9510127443794,84.3858860507229,
84.8207593572004,85.2556326638134,85.6905059705631,86.1253792774507,86.5602525844776,
86.995978584908,87.4317045853384,87.8665778926469,88.3014512000977,88.7363245076919,
89.1711978154302,89.6060711233134,90.0409444313423,90.4758177395175,90.9106910478396,
91.345564356309,91.7804376649263,92.2153109736917,92.6501842826055,93.085057591668,
93.5199309008791,93.9556569024059,94.3913829039327,94.8262562134414,95.2611295230986,
95.6960028329042,96.1308761428578,96.5657494529591,97.0006227632077,97.4354960736028,
97.870369384144,98.3052426948304,98.7401160056612,99.1749893166354,99.6098626277522,
100.04473593901,100.915335253024,101.351061255639,101.785934567313,102.220807879124,
102.655681191068,103.090554503145,103.525427815353,104.395174440154,105.264921065453,
105.699794378283,106.134667691232,106.569541004295,107.004414317471,107.8750136343,
108.745612951339,109.615359578629,110.485106206296,111.354852834309,112.224599462639,
113.094346091254,113.964092720119,114.834692038763,115.705291357499,116.575037986826,
117.444784616267,118.314531245777,119.184277875311,120.054024504821,120.923771134261,
121.794370453112,122.66496977189,123.534716400968,124.404463029834,125.274209658448,
126.143956286779,127.013702914792,127.883449542458,128.754048859798,129.624648176939,
130.494394803617,131.364141429857,132.233888055637,133.103634680937,133.973381305737,
134.843127930023,135.71372724472,136.584326559147,137.019199870684,137.454073182083,
137.888946493341,138.323819804458,139.193566426263,140.063313047491,140.498186357887,
140.933059668136,141.367932978237,141.802806288191,142.237679597997,142.673405599673,
143.109131601348,143.544004910857,143.978878220217,144.413751529429,144.848624838491,
145.283498147405,145.718371456171,146.153244764789,146.588118073258,147.022991381581,
147.457864689756,147.892737997785,148.327611305669,148.762484613407,149.197357921002,
149.633083921574,150.068809922147,150.503683229455,150.938556536623,151.37342984365,
151.808303150538,152.243176457288,152.678049763901,153.112923070379,153.547796376722,
153.982669682934,154.417542989014,154.852416294964,155.287289600787,155.722162906483,
156.157036212055,156.592762211626,157.028488211198,157.463361516526,157.898234821735,
158.333108126826,158.767981431803,159.202854736666,159.637728041419,160.072601346062,
160.507474650599,160.94234795503,161.37722125936,161.812094563589,162.246967867721,
162.681841171757,163.1167144757,163.552440474473,163.988166473247,164.423039777011,
164.85791308069,165.292786384286,165.727659687801,166.162532991238,166.597406294601,
167.03227959789,167.46715290111,167.902026204262,168.33689950735,168.771772810376,
169.206646113343,169.641519416254,170.076392719112,170.512118717363,170.947844715614,
171.382718018374,171.817591321089,172.252464623762,172.687337926397,173.122211228996,
173.557084531561,173.991957834097,174.426831136606,174.86170443909,175.296577741554,
175.731451044,176.16632434643,176.601197648848,177.036070951258,177.471796949306,
177.907522947355,178.342396249755,178.777269552155,179.212142854558,179.647016156968,
180.081889459386,180.516762761816,180.951636064262,181.386509366726,181.82138266921,
182.256255971719,182.691129274255,183.12600257682,183.560875879419,183.995749182054,
184.431475180237,184.867201178421,185.302074481136,185.736947783896,186.171821086704,
186.606694389561,187.041567692473,187.47644099544,187.911314298466,188.346187601554,
188.781060904706,189.215934207926,189.650807511215,190.085680814577,190.520554118015,
190.95542742153,191.391153420175,191.82687941882,192.261752722499,192.696626026263,
193.131499330116,193.566372634059,194.001245938095,194.436119242227,194.870992546456,
195.305865850785,195.740739155217,196.175612459754,196.610485764397,197.045359069149,
197.480232374013,197.915105678989,198.350831678382,198.786557677775,199.221430982984,
199.656304288312,200.091177593761,200.526050899333,200.960924205029,201.395797510852,
201.830670816802,202.265544122882,202.700417429093,203.135290735437,203.570164041915,
204.005037348528,204.439910655278,204.874783962166,205.310509962526,205.746235962887,
206.181109270054,206.615982577363,207.050855884814,207.485729192409,207.920602500147,
208.355475808031,208.79034911606,209.225222424235,209.660095732558,210.094969041027,
210.529842349645,210.96471565841,211.399588967324,211.834462276387,212.27018827784,
212.705914279292,213.140787588653,213.575660898161,214.010534207819,214.880280827579,
215.31515413768,215.750027447929,216.184900758324,216.619774068866,217.054647379553,
217.489520690384,218.359267312475,219.22986662628,219.665592628826,220.100465940363,
220.535339252038,220.970212563848,221.83995918787,222.709705812416,223.579452437468,
224.014325750179,224.44919906301,225.318945689022,226.189545005688,227.060144322571,
227.929890949664,228.799637577146,229.66938420499,230.539130833166,231.408877461643,
232.278624090388,233.149223408954,234.019822727623,234.889569356878,235.759315986267,
236.629062615749,237.498809245277,238.368555874806,239.238302504287,240.108901823183,
240.979501142017,241.849247771189,242.718994400167,243.588741028911,244.458487657389,
245.328234285565,246.197980913409,247.068580230891,247.939179548182,248.80892617507,
249.678672801532,250.548419427545,251.418166053087,252.287912678139,253.157659302684,
254.028258617581,254.898857932211,255.333731243885,255.768604555423,256.203477866821,
256.63835117808,257.508097800171,258.377844421689,258.812717732231,259.247591042627,
259.682464352876,260.117337662977,260.552210972931,260.987936974682,261.858536286089,
262.293409595598,262.728282904958,263.16315621417,263.598029523233,264.032902832147,
264.467776140913,264.902649449531,265.337522758001,265.772396066323,266.207269374499,
266.642142682528,267.077015990412,267.511889298151,267.947615298795,268.383341299439,
268.81821460689,269.2530879142,269.687961221367,270.122834528394,270.557707835282,
270.992581142032,271.427454448646,271.862327755124,272.297201061468,272.732074367679,
273.166947673759,273.60182097971,274.036694285533,274.471567591229,274.907293590862,
275.343019590495,275.777892895944,276.212766201272,276.647639506481,277.082512811573,
277.51738611655,277.952259421414,278.387132726166,278.82200603081,279.256879335346,
279.691752639779,280.126625944108,280.561499248338,280.996372552469,281.431245856506,
281.866971855324,282.302697854143,282.737571157996,283.172444461761,283.60731776544,
284.042191069036,284.477064372551,284.911937675989,285.346810979351,285.781684282641,
286.216557585861,286.651430889013,287.086304192101,287.521177495128,287.956050798095,
288.390924101007,288.826650099283,289.262376097559,289.697249400366,290.132122703127,
290.566996005842,291.001869308516,291.43674261115,291.871615913749,292.306489216315,
292.741362518851,293.17623582136,293.611109123845,294.045982426308,294.480855728754,
294.915729031185,295.350602333603,295.786328331655,296.222054329707,296.65692763211,
297.091800934511,297.526674236911,297.961547539314,298.396420841724,298.831294144142,
299.266167446573,299.701040749018,300.135914051482,300.570787353967,301.005660656476,
301.440533959012,301.875407261578,302.310280564177,302.746006562341,303.181732560506,
303.616605863179,304.051479165895,304.486352468655,304.921225771462,305.35609907432,
305.790972377232,306.225845680199,306.660718983226,307.095592286314,307.530465589466,
307.965338892686,308.400212195976,308.835085499338,309.269958802776,309.705684801381,
310.141410799985,310.576284103581,311.01115740726,311.446030711025,311.880904014878,
312.315777318821,312.750650622858,313.185523926989,313.620397231219,314.055270535549,
314.490143839981,314.925017144517,315.359890449161,315.794763753913,316.229637058777,
316.665363058112,317.101089057448,317.53596236254,317.970835667749,318.405708973077,
318.840582278526,319.275455584098,319.710328889795,320.145202195618,320.580075501568,
321.014948807648,321.44982211386,321.884695420204,322.319568726682,322.754442033295,
323.189315340045,323.625041340336,324.060767340628,324.495640647655,324.930513954822,
325.365387262131,325.800260569583,326.235133877177,326.670007184916,327.1048804928,
327.539753800829,327.974627109005,328.409500417327,328.844373725797,329.279247034415,
329.714120343181,330.148993652095,330.584719653474,331.020445654852,331.455318964064,
331.890192273424,332.325065582933,332.759938892591,333.194812202397,333.629685512351,
334.064558822453,334.499432132702,334.934305443098,335.369178753639,335.804052064326,
336.673798686132,337.108671997249,337.544397999725,337.980124002201,338.4149973136,
338.849870625137,339.284743936812,340.154490560568,341.024237184854,341.459110497191,
341.893983809655,342.328857122244,342.763730434955,343.633477060735,344.504076377234,
345.374675693955,346.244422320844,347.114168948136,347.983915575803,348.853662203817,
349.723408832148,350.593155460764,351.463754779246,352.334354097839,353.204100727012,
354.07384735634,354.943593985781,355.813340615292,356.683087244827,357.552833874338,
358.423433193272,359.294032512154,360.163779141409,361.033525770489,361.903272399355,
362.77301902797,363.642765656301,364.512512284316,365.383111601936,366.253710919371,
367.123457546465,367.993204173143,368.862950799383,369.732697425164,370.602444050463,
371.472190675265,372.342789990359,373.21338930519,373.648262617,374.083135928675,
374.952882551611,375.822629173987,376.257502484962,376.692375795793,377.12724910648,
377.562122417021,377.996995727417,378.431869037666,378.866742347767,379.302468349591,
379.738194351416,380.173067661222,380.607940970879,381.042814280388,381.477687589749,
381.91256089896,382.347434208023,382.782307516937,383.217180825703,383.652054134321,
384.086927442791,384.521800751113,384.956674059289,385.391547367318,385.826420675202,
386.262146675918,386.697872676635,387.13274598423,387.567619291681,388.00249259899,
388.437365906157,388.872239213185,389.307112520073,389.741985826823,390.176859133436,
390.611732439914,391.046605746258,391.48147905247,391.91635235855,392.351225664501,
392.786098970323,393.221824970019,393.657550969714,394.092424275286,394.527297580735,
394.962170886063,395.397044191272,395.831917496364,396.266790801341,396.701664106204,
397.136537410957,397.5714107156,398.006284020137,398.441157324569,398.876030628899,
399.310903933128,399.74577723726,400.181503236126,400.617229234991,401.052102538934,
401.486975842787,401.921849146551,402.356722450231,402.791595753827,403.226469057342,
403.66134236078,404.096215664142,404.531088967432,404.965962270651,405.400835573804,
405.835708876892,406.270582179918,406.705455482886,407.141181481189,407.576907479491,
408.01178078235,408.446654085157,408.881527387917,409.316400690633,409.751273993306,
410.186147295941,410.62102059854,411.055893901106,411.490767203642,411.925640506151,
412.360513808636,412.795387111099,413.230260413545,413.665133715976,414.100859714032,
414.536585712088,414.971459014498,415.406332316901,415.841205619301,416.276078921702,
416.710952224105,417.145825526515,417.580698828933,418.015572131364,418.45044543381,
418.885318736273,419.320192038758,419.755065341267,420.189938643803,420.624811946369,
421.060537944515,421.496263942662,421.931137245297,422.36601054797,422.800883850686,
423.235757153446,423.670630456253,424.105503759112,424.540377062023,424.975250364991,
425.410123668017,425.844996971105,426.279870274258,426.714743577477,427.149616880767,
427.584490184129,428.020216182695,428.455942181261,428.890815484776,429.325688788373,
429.760562092052,430.195435395816,430.630308699669,431.065182003612,431.500055307649,
431.93492861178,432.36980191601,432.80467522034,433.239548524772,433.674421829309,
434.109295133952,434.544168438705,434.979894437984,435.415620437262,435.850493742239,
436.285367047331,436.72024035254,437.155113657869,437.589986963318,438.024860268889,
438.459733574586,438.894606880409,439.32948018636,439.76435349244,440.199226798651,
440.634100104995,441.068973411473,441.503846718087,441.939572718309,442.375298718531,
442.810172025419,443.245045332447,443.679918639614,444.114791946923,444.549665254374,
444.984538561969,445.419411869708,445.854285177591,446.289158485621,446.724031793796,
447.158905102119,447.593778410589,448.028651719207,448.463525027973,448.899251029277,
449.334977030581,449.769850339644,450.639596958216,451.074470267725,451.509343577383,
451.944216887189,452.379090197143,452.813963507244,453.248836817493,453.683710127889,
454.118583438431,454.553456749117,454.988330059949,455.423203370923,455.858929373329,
456.294655375734,456.729528686993,457.164401998391,457.599275309929,458.469021933414,
458.90389524536,459.338768557437,459.773641869646,460.208515181983,460.643388494447,
461.078261807036,461.948008432578,462.818607748906,463.689207065461,464.55895369214,
465.428700319234,466.298446946716,467.16819357456,468.037940202737,468.907686831215,
469.778286149605,470.648885468116,471.518632097196,472.388378726451,473.258125355841,
474.127871985322,474.997618614851,475.86736524438,476.737964563343,477.608563882265,
478.478310511593,479.348057140765,480.217803769743,481.087550398488,481.957297026966,
482.827043655142,483.697642972895,484.568242290469,485.43798891776,486.307735544649,
487.177482171112,488.047228797125,488.916975422667,489.78672204772,490.657321363009,
491.09304736596,491.527920678038,492.397667301793,493.267413925005,494.137160547663,
494.57203385878,495.006907169755,495.441780480586,495.876653791273,496.311527101814,
496.74640041221,497.616999724357,498.052725726255,498.487599036209,498.922472346015,
499.357345655673,499.792218965182,500.227092274542,500.661965583754,501.096838892816,
501.531712201731,501.966585510497,502.401458819114,502.836332127584,503.271205435907,
503.706078744082,504.140952052112,504.576678052901,505.01240405369,505.447277361429,
505.882150669023,506.317023976474,506.751897283783,507.186770590951,507.621643897978,
508.056517204866,508.491390511616,508.92626381823,509.361137124708,509.796010431052,
510.230883737263,510.665757043344,511.100630349294,511.536356349053,511.972082348811,
512.406955654506,512.841828960076,513.276702265523,513.711575570849,514.146448876056,
514.581322181146,515.016195486121,515.451068790983,515.885942095733,516.320815400375,
516.75568870491,517.19056200934,517.625435313668,518.060308617896,518.496034616807,
518.931760615718,519.366633919752,519.801507223694,520.236380527545,520.671253831307,
521.106127134985,521.541000438579,521.975873742092,522.410747045528,522.845620348888,
523.280493652176,523.715366955394,524.150240258545,524.585113561631,525.019986864656,
525.455712862985,525.891438861313,526.326312164223,526.761185467079,527.196058769885,
527.630932072643,528.065805375356,528.500678678029,528.935551980661,529.370425283258,
529.805298585822,530.240171888356,530.675045190863,531.109918493346,531.544791795808,
531.979665098252,532.415391096312,532.851117094373,533.285990396789,533.720863699197,
534.155737001598,534.590610303997,535.025483606395,535.460356908796,535.895230211204,
536.330103513621,536.764976816049,537.199850118493,537.634723420955,538.069596723438,
538.504470025945,538.93934332848,539.375069326608,539.810795324736,540.245668627333,
540.680541929966,541.115415232637,541.550288535351,541.985161838109,542.420035140915,
542.854908443771,543.28978174668,543.724655049646,544.15952835267,544.594401655757,
545.029274958907,545.464148262125,545.899021565413,546.334747563939,546.770473562465,
547.205346865901,547.640220169415,548.075093473009,548.509966776686,548.944840080449,
549.3797133843,549.814586688241,550.249459992276,550.684333296405,551.119206600633,
551.554079904961,551.988953209391,552.423826513926,552.858699818567,553.294425817789,
553.73015181701,554.165025121872,554.599898426846,555.034771731937,555.469645037144,
555.90451834247,556.339391647917,556.774264953487,557.209138259182,557.644011565003,
558.078884870951,558.51375817703,558.948631483239,559.383504789581,559.818378096058,
560.254104096209,560.689830096361,561.12470340311,561.559576709996,561.994450017021,
562.429323324187,562.864196631494,563.299069938943,563.733943246536,564.168816554273,
564.603689862154,565.038563170182,565.473436478355,565.908309786676,566.343183095144,
566.77805640376,567.213782404988,567.649508406216,568.084381715128,568.519255024189,
568.954128333399,569.389001642757,569.823874952264,570.258748261921,570.693621571725,
571.128494881677,571.563368191777,572.433114812417,572.867988122957,573.302861433642,
573.737734744471,574.173460746804,574.609186749136,575.044060060251,575.913806682904,
576.783553306113,577.218426617922,577.653299929865,578.08817324194,578.523046554147,
579.392793178944,580.26253980424,581.13313912039,581.568865123709,582.003738436771,
582.87348506323,583.743231690115,584.612978317402,585.482724945065,586.352471573076,
587.222218201403,588.092817519691,588.963416838109,589.833163467083,590.702910096251,
591.572656725575,592.442403355013,593.31214998452,594.181896614051,595.05249593303,
595.92309525198,596.792841881366,597.662588510618,598.532335139693,599.402081768556,
600.271828397167,601.141575025495,602.012174343369,602.882773661074,603.752520288553,
604.622266915642,605.492013542317,606.361760168553,607.23150679433,608.101253419626,
608.971852735101,609.842452050322,610.71219867434,611.581945297822,612.451691920754,
612.886565232011,613.321438543126,613.756311854099,614.191185164928,615.060931786153,
615.931531098516,616.367257100486,616.802130410586,617.237003720538,617.671877030342,
618.106750339998,618.541623649505,618.976496958863,619.411370268073,619.846243577134,
620.281116886046,620.71599019481,621.150863503426,621.585736811894,622.020610120214,
622.455483428388,622.891209429248,623.326935430108,623.761808737989,624.196682045726,
624.631555353319,625.066428660769,625.501301968075,625.936175275241,626.371048582266,
626.805921889153,627.240795195901,627.675668502512,628.110541808988,628.54541511533,
628.98028842154,629.415161727618,629.850887727438,630.286613727259,630.72148703308,
631.156360338774,631.591233644344,632.026106949791,632.460980255118,632.895853560325,
633.330726865415,633.76560017039,634.200473475251,634.635346780002,635.070220084644,
635.505093389179,635.939966693609,636.374839997937,636.810565996897,637.246291995857,
637.681165299986,638.116038604021,638.550911907962,638.985785211813,639.420658515576,
639.855531819253,640.290405122847,640.725278426361,641.160151729796,641.595025033157,
642.029898336444,642.464771639662,642.899644942813,643.334518245899,643.770244244257,
644.205970242616,644.640843545581,645.075716848491,645.510590151347,645.945463454153,
646.380336756911,646.815210059625,647.250083362296,647.684956664929,648.119829967526,
648.55470327009,648.989576572624,649.424449875131,649.859323177614,650.294196480076,
650.729922478144,651.165648476212,651.600521778641,652.035395081057,652.470268383465,
652.905141685866,653.340014988265,653.774888290663,654.209761593065,654.644634895472,
655.079508197889,655.514381500318,655.949254802762,656.384128105224,656.819001407706,
657.253874710213,657.689600708326,658.12532670644,658.560200009004,658.995073311601,
659.429946614234,659.864819916905,660.299693219619,660.734566522377,661.169439825183,
661.604313128039,662.039186430948,662.474059733914,662.908933036938,663.343806340025,
663.778679643175,664.213552946393,664.649278944883,665.085004943373,665.519878246733,
665.954751550169,666.389624853683,666.824498157277,667.259371460954,667.694244764717,
668.129118068568,668.563991372509,668.998864676544,669.433737980674,669.868611284901,
670.303484589229,670.738357893659,671.173231198194,671.608957197361,672.044683196528,
672.479556501278,672.91442980614,673.349303111115,673.784176416205,674.219049721412,
674.653923026738,675.088796332185,675.523669637755,675.95854294345,676.393416249271,
676.82828955522,677.263162861298,677.698036167508,678.13290947385,678.568635473934,
679.004361474018,679.439234780629,679.874108087377,680.308981394264,680.743854701289,
681.178728008455,681.613601315762,682.048474623211,682.483347930804,682.91822123854,
683.353094546422,683.78796785445,684.222841162623,684.657714470944,685.092587779412,
685.528313780566,685.96403978172,686.398913090483,686.833786399396,687.268659708457,
687.703533017666,688.138406327025,688.573279636532,689.008152946187,689.443026255992,
689.877899565944,690.312772876043,690.74764618629,691.182519496684,691.617392807224,
692.052266117909,692.487992120169,692.92371812243,693.358591433403,694.228338055774,
694.663211367171,695.098084678707,695.532957990379,695.967831302188,696.402704614131,
696.837577926207,697.707324550749,698.577071175797,699.011944488507,699.447670491767,
699.883396495028,700.318269807975,701.188016434211,702.057763060886,702.927509687976,
703.797256315454,704.667002943295,705.536749571467,706.407348889651,707.277948207973,
708.147694836835,709.017441465911,709.887188095163,710.756934724548,711.626681354026,
712.496427983551,713.367027302543,714.237626621516,715.107373250954,715.977119880277,
716.846866509446,717.716613138419,718.586359767161,719.456106395635,720.32670571363,
721.197305031464,722.067051659126,722.936798286414,723.806544913299,724.676291539758,
725.546038165767,726.415784791305,727.286384106969,728.156983422381,729.026730046663,
729.896476670415,730.331349982088,730.766223293624,731.201096605021,731.635969916278,
732.505716538366,733.37546315988,733.81033647042,734.246062472462,734.681788474505,
735.116661784752,735.551535094852,735.986408404804,736.421281714608,736.856155024264,
737.291028333771,737.72590164313,738.160774952339,738.5956482614,739.030521570312,
739.465394879076,739.900268187692,740.33514149616,740.77001480448,741.205740805414,
741.641466806347,742.076340114374,742.511213422256,742.946086729993,743.380960037585,
743.815833345035,744.250706652341,744.685579959507,745.120453266533,745.555326573419,
745.990199880167,746.425073186778,746.859946493254,747.294819799596,747.729693105806,
748.165419105691,748.601145105576,749.036018411525,749.470891717346,749.90576502304,
750.34063832861,750.775511634057,751.210384939384,751.645258244591,752.080131549682,
752.515004854656,752.949878159518,753.384751464269,753.81962476891,754.254498073445,
754.689371377875,755.125097376885,755.560823375895,755.995696680123,756.430569984253,
756.865443288287,757.300316592228,757.735189896079,758.170063199842,758.604936503519,
759.039809807113,759.474683110627,759.909556414062,760.344429717423,760.779303020711,
761.214176323929,761.649049627079,762.084775625469,762.520501623858,762.955374926883,
763.390248229848,763.825121532758,764.259994835614,764.694868138419,765.129741441178,
765.564614743891,765.999488046563,766.434361349196,766.869234651793,767.304107954357,
767.738981256891,768.173854559398,768.608727861881,769.044453859958,769.480179858035,
769.915053160479,770.349926462907,770.784799765324,771.219673067731,771.654546370133,
772.089419672531,772.52429297493,772.959166277331,773.394039579739,773.828912882155,
774.263786184584,774.698659487028,775.13353278949,775.568406091973,776.004132090072,
776.439858088172,776.874731390706,777.30960469327,777.744477995867,778.1793512985,
778.614224601171,779.049097903885,779.483971206643,779.918844509449,780.353717812305,
780.788591115215,781.22346441818,781.658337721205,782.093211024291,782.528084327442,
782.963810325897,783.399536324352,783.834409627639,784.269282931,784.704156234435,
785.139029537949,785.573902841543,786.00877614522,786.443649448983,786.878522752834,
787.313396056775,787.74826936081,788.183142664939,788.618015969167,789.052889273495,
789.487762577925,789.923488577038,790.359214576152,790.794087880793,791.228961185544,
791.663834490406,792.098707795381,792.533581100471,792.968454405678,793.403327711004,
793.838201016451,794.273074322021,794.707947627716,795.142820933537,795.577694239486,
796.012567545564,796.447440851774,796.883166851791,797.318892851808,797.753766158284,
798.188639464895,798.623512771643,799.058386078529,799.493259385555,799.92813269272,
800.363006000027,800.797879307477,801.232752615069,801.667625922806,802.102499230688,
802.537372538715,802.972245846889,803.40711915521,803.84284515629,804.27857115737,
804.713444465985,805.148317774749,805.583191083662,806.018064392723,806.452937701933,
806.887811011291,807.322684320798,808.192430940258,808.62730425021,809.06217756031,
809.497050870557,809.931924180951,810.36679749149,810.802523493679,811.238249495867,
811.673122806697,812.542869428785,812.977742740041,813.412616051438,813.847489362974,
814.282362674646,814.717235986455,815.152109298398,816.021855922681,816.891602547478,
817.326475860065,817.762201863265,818.197927866466,818.632801179295,819.502547805304,
820.372294431763,821.242041058648,822.111787685935,822.981534313598,823.851280941609,
824.721880259681,825.5924795779,826.462226206642,827.331972835616,828.201719464785,
829.071466094109,829.941212723546,830.810959353053,831.681558672047,832.552157991036,
833.421904620514,834.2916512499,835.161397879151,836.031144508226,836.900891137089,
837.770637765701,838.641237083811,839.511836401767,840.381583029608,841.251329657086,
842.121076284176,842.990822910851,843.860569537087,844.730316162863,845.600915478712,
846.471514794314,847.341261418855,848.211008042874,848.645881354683,849.080754666356,
849.515627977891,849.950501289288,850.82024791166,851.689994533462,852.124867844147,
852.560593846263,852.996319848379,853.431193158772,853.866066469019,854.300939779119,
855.170686398875,855.605559708531,856.040433018038,856.475306327397,856.910179636606,
857.345052945667,857.77992625458,858.214799563344,858.64967287196,859.084546180427,
859.520272181434,859.95599818244,860.390871490614,860.825744798641,861.260618106523,
861.69549141426,862.130364721852,862.565238029302,863.000111336609,863.434984643774,
863.8698579508,864.304731257686,864.739604564434,865.174477871045,865.609351177521,
866.044224483863,866.479950483814,866.915676483765,867.350549789843,867.785423095792,
868.220296401613,868.655169707307,869.090043012877,869.524916318325,869.959789623651,
870.394662928858,870.829536233948,871.264409538923,871.699282843785,872.134156148535,
872.569029453177,873.003902757712,873.439628756773,873.875354755834,874.310228060162,
874.745101364389,875.179974668519,875.614847972553,876.049721276495,876.484594580346,
876.919467884108,877.354341187786,877.78921449138,878.224087794893,878.658961098329,
879.093834401689,879.528707704977,879.963581008195,880.399307006616,880.835033005038,
881.269906308124,881.704779611148,882.139652914114,882.574526217024,883.00939951988,
883.444272822685,883.879146125444,884.314019428157,884.748892730829,885.183766033462,
885.618639336059,886.053512638623,886.488385941157,886.923259243664,887.358985241751,
887.794711239839,888.2295845423,888.664457844744,889.099331147173,889.534204449589,
889.969077751997,890.403951054398,890.838824356797,891.273697659195,891.708570961597,
892.143444264004,892.578317566421,893.01319086885,893.448064171293,893.882937473755,
894.318663471843,894.75438946993,895.189262772437,895.624136074971,896.059009377535,
896.493882680132,896.928755982765,897.363629285437,897.798502588151,898.233375890909,
898.668249193715,899.103122496571,899.53799579948,899.972869102446,900.40774240547,
900.842615708556,901.278341706978,901.714067705399,902.148941008617,902.583814311905,
903.018687615265,903.453560918701,903.888434222214,904.323307525808,904.758180829485,
905.193054133248,905.627927437099,906.06280074104,906.497674045075,906.932547349205,
907.367420653433,907.80229395776,908.238019956821,908.673745955883,909.108619260417,
909.543492565059,909.978365869809,910.413239174671,910.848112479646,911.282985784736,
911.717859089943,912.152732395269,912.587605700716,913.022479006287,913.457352311981,
913.892225617802,914.327098923751,914.761972229829,915.19769822978,915.633424229731,
916.068297536072,916.503170842548,916.93804414916,917.372917455908,917.807790762794,
918.24266406982,918.677537376985,919.112410684292,919.547283991742,919.982157299334,
920.417030607071,920.851903914953,921.28677722298,921.721650531154,922.15737653216,
922.593102533167,923.027975841635,923.46284915025,923.897722459014,924.332595767926,
924.767469076987,925.202342386197,925.637215695556,926.072089005063,926.506962314719,
926.941835624523,927.376708934475,927.811582244575,928.246455554822,928.681328865215,
929.117054867331,929.987654180132,930.422527490961,930.857400801934,931.292274113049,
931.727147424306,932.162020735703,932.596894047238,933.46664067072,934.336387294739,
934.771260606945,935.20613391928,935.641007231742,936.076733234882,936.94733255073,
937.817079176507,938.686825802743,939.556572429418,940.426319056508,941.296065683986,
942.165812311827,943.036411629783,943.907010947893,944.776757576505,945.646504205367,
946.516250834443,947.385997463694,948.25574409308,949.125490722558,949.996090041546,
950.86668936054,951.736435990048,952.606182619485,953.475929248809,954.345675877978,
955.215422506951,956.085169135693,956.955768453912,957.826367771985,958.696114399995,
959.565861027658,960.435607654946,961.305354281831,962.175100908289,963.044847534298,
963.915446850328,964.786046166116,965.655792790913,966.525539415195,966.960412727138,
967.395286038947,968.265032662155,969.134779284809,969.569652595924,970.004525906897,
970.439399217726,970.875125219914,971.310851222103,971.745724532643,972.615471153283,
973.485217773335,973.920091083139,974.354964392795,974.789837702302,975.22471101166,
975.65958432087,976.094457629931,976.529330938844,976.964204247608,977.399077556223,
977.834803557303,978.270529558383,978.705402866704,979.140276174877,979.575149482905,
980.010022790786,980.444896098523,980.879769406116,981.314642713565,981.749516020872,
982.184389328038,982.619262635063,983.05413594195,983.489009248698,983.923882555309,
984.358755861785,984.794481861802,985.230207861819,985.665081168029,986.099954474107,
986.534827780056,986.969701085877,987.404574391571,987.839447697141,988.274321002589,
988.709194307915,989.144067613122,989.578940918212,990.013814223187,990.448687528048,
990.883560832799,991.31843413744,991.754160136554,992.189886135667,992.624759440097,
993.059632744425,993.494506048653,993.929379352783,994.364252656817,994.799125960758,
995.233999264609,995.668872568372,996.103745872049,996.538619175643,996.973492479157,
997.408365782593,997.843239085953,998.278112389241,998.713838387696,999.149564386151,
999.584437689301,1000.01931099239,1000.45418429541,1000.88905759838,1001.32393090129,
1001.75880420414,1002.19367750695,1002.62855080971,1003.06342411242,1003.49829741509,
1003.93317071773,1004.36804402032,1004.80291732289,1005.23779062542,1005.67351662352,
1006.10924262162,1006.5441159241,1006.97898922656,1007.41386252901,1007.84873583144,
1008.28360913385,1008.71848243626,1009.15335573866,1009.58822904106,1010.02310234346,
1010.45797564586,1010.89284894827,1011.32772225069,1011.76259555311,1012.19746885556,
1012.63319485364,1013.06892085171,1013.5037941542,1013.9386674567,1014.37354075924,
1014.8084140618,1015.2432873644,1015.67816066703,1016.1130339697,1016.54790727242,
1016.98278057517,1017.41765387798,1017.85252718084,1018.28740048375,1018.72227378671,
1019.15714708974,1019.59287308813,1020.02859908651,1020.46347238967,1020.89834569288,
1021.33321899617,1021.76809229953,1022.20296560297,1022.63783890648,1023.07271221007,
1023.50758551375,1023.94245881752,1024.37733212137,1024.81220542531,1025.24707872935,
1025.68195203348,1026.11682533771,1026.55255133672,1026.98827733573,1027.42315064016,
1027.8580239447,1028.29289724934,1028.72777055409,1029.16264385896,1029.59751716393,
1030.03239046902,1030.46726377423,1030.90213707956,1031.33701038501,1031.77188369058,
1032.20675699628,1032.6416303021,1033.07650360805,1033.51222960793,1033.94795560782,
1034.38282891403,1034.81770222038,1035.25257552685,1035.68744883347,1036.12232214022,
1036.5571954471,1036.99206875413,1037.4269420613,1037.86181536861,1038.29668867606,
1038.73156198365,1039.16643529139,1039.60130859927,1040.0361819073,1040.47190790824,
1040.90763390917,1041.34250721749,1041.77738052596,1042.21225383458,1042.64712714334,
1043.08200045226,1043.95174707053,1044.38662037989,1044.8214936894,1045.25636699906,
1045.69124030886,1046.12611361882,1046.56098692892,1046.99586023917,1047.43158624121,
1047.86731224325,1048.3021855538,1048.73705886448,1049.17193217531,1049.60680548629,
1050.0416787974,1050.47655210866,1050.91142542006,1051.78117204327,1052.21604535508,
1052.65091866703,1053.0857919791,1053.52066529131,1053.95553860365,1054.39126460673,
1055.26186392239,1056.13161054793,1057.00135717395,1057.43623048712,1057.87110380041,
1058.7408504273,1059.61059705459,1060.48034368225,1061.35094300009,1062.22154231809,
1063.09128894656,1063.96103557531,1064.83078220429,1065.70052883346,1066.57027546278,
1067.44002209222,1068.3106214112,1069.18122073019,1070.05096735972,1070.9207139892,
1071.79046061859,1072.66020724785,1073.52995387693,1074.39970050579,1075.27029982411,
1076.1408991423,1077.01064577048,1077.88039239832,1078.7501390258,1079.61988565289,
1080.48963227957,1081.35937890581,1082.22997822202,1083.100577538,1083.97032416305,
1084.84007078759,1085.70981741161,1086.5795640351,1087.44931065803,1087.88418396929,
1088.31905728041,1088.75393059138,1089.18965659365,1089.62538259591,1090.06025590659,
1090.93000252753,1091.36487583778,1091.79974914788,1092.23462245783,1092.66949576764,
1093.1043690773,1093.5392423868,1093.97411569616,1094.40898900538,1094.84386231444,
1095.27873562335,1095.71360893212,1096.14933493327,1096.58506093443,1097.0199342429,
1097.45480755122,1097.88968085939,1098.32455416742,1098.75942747531,1099.19430078305,
1099.62917409064,1100.06404739809,1100.4989207054,1100.93379401257,1101.36866731959,
1101.80354062648,1102.23841393323,1102.67328723984,1103.10901323993,1103.54473924001,
1103.97961254636,1104.41448585257,1104.84935915865,1105.2842324646,1105.71910577042,
1106.15397907612,1106.58885238169,1107.02372568714,1107.45859899246,1107.89347229767,
1108.32834560276,1108.76321890774,1109.1980922126,1109.63296551736,1110.06869151652,
1110.50441751569,1110.93929082023,1111.37416412466,1111.80903742899,1112.24391073322,
1112.67878403735,1113.11365734139,1113.54853064533,1113.98340394918,1114.41827725295,
1114.85315055662,1115.28802386022,1115.72289716374,1116.15777046717,1116.59264377053,
1117.02836976903,1117.46409576752,1117.89896907074,1118.33384237389,1118.76871567698,
1119.20358898,1119.63846228297,1120.07333558588,1120.50820888874,1120.94308219154,
1121.3779554943,1121.81282879702,1122.24770209969,1122.68257540233,1123.11744870492,
1123.55232200749,1123.98804800561,1124.42377400372,1124.85864730623,1125.29352060871,
1125.72839391118,1126.16326721362,1126.59814051605,1127.03301381847,1127.46788712088,
1127.90276042328,1128.33763372568,1128.77250702808,1129.20738033048,1129.64225363289,
1130.07712693531,1130.51200023774,1130.94772623581,1131.38345223388,1131.81832553634,
1132.25319883883,1132.68807214134,1133.12294544387,1133.55781874644,1133.99269204904,
1134.42756535167,1134.86243865434,1135.29731195706,1135.73218525982,1136.16705856263,
1136.60193186548,1137.03680516839,1137.47167847136,1137.90740446972,1138.34313046808,
1138.77800377117,1139.21287707432,1139.64775037754,1140.08262368083,1140.51749698419,
1140.95237028763,1141.38724359114,1141.82211689474,1142.25699019842,1142.69186350218,
1143.12673680603,1143.56161010998,1143.99648341401,1144.43135671814,1144.86708271711,
1145.30280871607,1145.7376820204,1146.17255532483,1146.60742862936,1147.04230193401,
1147.47717523876,1147.91204854362,1148.3469218486,1148.78179515369,1149.2166684589,
1149.65154176423,1150.08641506968,1150.52128837525,1150.95616168094,1151.39103498677,
1151.82676098659,1152.26248698641,1152.69736029249,1153.1322335987,1153.56710690504,
1154.00198021152,1154.43685351813,1154.87172682488,1155.30660013177,1155.7414734388,
1156.17634674597,1156.61122005327,1157.04609336073,1157.48096666832,1157.91583997606,
1158.35071328394,1158.7864392848,1159.22216528566,1159.65703859384,1160.09191190216,
1160.52678521063,1160.96165851925,1161.39653182801,1161.83140513693,1162.26627844599,
1162.7011517552,1163.13602506456,1163.57089837407,1164.00577168373,1164.44064499353,
1164.87551830349,1165.74611761556,1166.18184361753,1166.61671692792,1167.05159023846,
1167.48646354915,1167.92133685998,1168.35621017096,1169.22595679333,1170.09570341627,
1170.53057672794,1170.96545003975,1171.4003233517,1171.83519666377,1172.27006997598,
1172.705795979,1173.57639529447,1174.44614191977,1174.8810152326,1175.31588854555,
1176.18563517179,1177.05538179847,1177.92512842556,1178.79487505304,1179.66547437075,
1180.53607368863,1181.40582031696,1182.27556694557,1183.14531357444,1184.01506020352,
1184.88480683277,1185.75455346216,1186.62515278112,1187.4957521001,1188.36549872963,
1189.23524535914,1190.10499198858,1190.97473861791,1191.84448524708,1192.71423187606,
1193.58483119448,1194.45543051277,1195.3251771411,1196.19492376911,1197.06467039678,
1197.93441702407,1198.80416365096,1199.67391027742,1200.5445095938,1201.41510890996,
1202.28485553525,1203.15460216005,1204.02434878434,1204.89409540809,1205.76384203131,
1206.1987153427,1206.63358865396,1207.06846196508,1207.50418796741,1208.37478728058,
1209.2445339018,1209.6794072122,1210.11428052245,1210.54915383255,1210.9840271425,
1211.41890045231,1211.85377376197,1212.28864707147,1212.72352038083,1213.15839369005,
1213.59326699911,1214.02814030802,1214.46386630925,1214.89959231048,1215.3344656191,
1215.76933892757,1216.20421223589,1216.63908554406,1217.07395885209,1217.50883215998,
1217.94370546771,1218.37857877531,1218.81345208276,1219.24832539007,1219.68319869724,
1220.11807200426,1220.55294531115,1220.9878186179,1221.42354461805,1221.85927061821,
1222.29414392468,1222.72901723103,1223.16389053724,1223.59876384332,1224.03363714927,
1224.46851045509,1224.90338376079,1225.33825706636,1225.77313037181,1226.20800367713,
1226.64287698234,1227.07775028743,1227.51262359241,1227.94749689727,1228.3832228965,
1228.81894889572,1229.25382220036,1229.6886955049,1230.12356880933,1230.55844211366,
1230.99331541789,1231.42818872202,1231.86306202606,1232.29793533,1232.73280863385,
1233.16768193762,1233.60255524129,1234.03742854489,1234.4723018484,1234.90717515184,
1235.34290115037,1235.7786271489,1236.21350045219,1236.64837375541,1237.08324705856,
1237.51812036165,1237.95299366467,1238.38786696764,1238.82274027055,1239.25761357341,
1239.69248687621,1240.12736017897,1240.56223348169,1240.99710678436,1241.431980087,
1241.8668533896,1242.30257938773,1242.73830538585,1243.17317868839,1243.6080519909,
1244.04292529338,1244.47779859585,1244.91267189829,1245.34754520072,1245.78241850314,
1246.21729180555,1246.65216510795,1247.08703841035,1247.52191171275,1247.95678501515,
1248.39165831756,1248.82653161998,1249.26225761804,1249.69798361611,1250.13285691855,
1250.56773022101,1251.0026035235,1251.43747682601,1251.87235012854,1252.30722343111,
1252.74209673371,1253.17697003634,1253.61184333901,1254.04671664173,1254.48158994449,
1254.9164632473,1255.35133655015,1255.78620985306,1256.22193585139,1256.65766184973,
1257.09253515275,1257.52740845584,1257.96228175899,1258.39715506221,1258.8320283655,
1259.26690166886,1259.7017749723,1260.13664827581,1260.57152157941,1261.00639488309,
1261.44126818685,1261.8761414907,1262.31101479465,1262.74588809868,1263.1816140976,
1263.61734009651,1264.05221340074,1264.48708670507,1264.9219600095,1265.35683331403,
1265.79170661868,1266.22657992343,1266.66145322829,1267.09632653327,1267.53119983836,
1267.96607314357,1268.4009464489,1268.83581975434,1269.27069305992,1269.70556636561,
1270.14129236537,1270.57701836513,1271.01189167108,1271.44676497716,1271.88163828337,
1272.31651158971,1272.75138489619,1273.1862582028,1273.62113150955,1274.05600481644,
1274.49087812347,1274.92575143063,1275.36062473794,1275.79549804539,1276.23037135299,
1276.66524466073,1277.10097066151,1277.5366966623,1277.97156997033,1278.40644327851,
1278.84131658683,1279.2761898953,1279.71106320392,1280.14593651268,1280.5808098216,
1281.01568313066,1281.45055643987,1281.88542974923,1282.32030305874,1282.75517636839,
1283.1900496782,1283.62492298815,1284.06064899005,1284.49637499195,1284.9312483022,
1285.36612161259,1285.80099492313,1286.23586823382,1286.67074154465,1287.54048816674,
1287.975361478,1288.4102347894,1288.84510810093,1289.27998141261,1289.71485472442,
1290.14972803636,1291.02032735139,1291.89092666668,1292.32579997914,1292.76067329173,
1293.19554660444,1293.63041991727,1294.50016654328,1295.36991316974,1296.23965979663,
1297.10940642392,1297.9800057415,1298.85060505925,1299.72035168742,1300.5900983159,
1301.45984494464,1302.32959157362,1303.19933820279,1304.06908483212,1304.93968415104,
1305.81028347,1306.68003009953,1307.54977672906,1308.41952335854,1309.28926998793,
1310.15901661718,1311.02876324626,1311.89936256477,1312.76996188316,1313.63970851164,
1314.50945513981,1315.37920176765,1316.24894839514,1317.11869502223,1317.98844164891,
1318.85904096546,1319.72964028179,1320.59938690733,1321.46913353238,1322.33888015692,
1323.20862678095,1323.64350009276,1324.07837340443,1324.51324671597,1324.94812002737,
1325.81871934103,1326.68931865441,1327.12419196524,1327.55906527593,1327.99393858647,
1328.42881189686,1328.86368520711,1329.29855851721,1329.73343182716,1330.16830513697,
1330.60317844663,1331.03805175614,1331.4729250655,1331.90779837471,1332.34267168377,
1332.77839768507,1333.21412368638,1333.64899699514,1334.08387030376,1334.51874361223,
1334.95361692055,1335.38849022873,1335.82336353676,1336.25823684464,1336.69311015238,
1337.12798345997,1337.56285676742,1337.99773007473,1338.4326033819,1338.86747668892,
1339.30234999581,1339.73807599603,1340.17380199625,1340.60867530287,1341.04354860934,
1341.47842191569,1341.9132952219,1342.34816852798,1342.78304183393,1343.21791513975,
1343.65278844545,1344.08766175102,1344.52253505647,1344.95740836179,1345.392281667,
1345.82715497209,1346.26202827707,1346.69775427635,1347.13348027563,1347.56835358038,
1348.00322688502,1348.43810018956,1348.87297349399,1349.30784679832,1349.74272010255,
1350.17759340668,1350.61246671072,1351.04734001466,1351.48221331851,1351.91708662228,
1352.35195992595,1352.78683322955,1353.22170653306,1353.65743253163,1354.09315853019,
1354.52803183356,1354.96290513685,1355.39777844007,1355.83265174322,1356.26752504631,
1356.70239834933,1357.1372716523,1357.57214495521,1358.00701825807,1358.44189156087,
1358.87676486363,1359.31163816635,1359.74651146902,1360.18138477166,1360.6171107698,
1361.05283676795,1361.48771007051,1361.92258337305,1362.35745667556,1362.79232997804,
1363.2272032805,1363.66207658295,1364.09694988538,1364.5318231878,1364.96669649021,
1365.40156979261,1365.83644309501,1366.27131639741,1366.70618969981,1367.14106300222,
1367.57678900028,1368.01251499834,1368.44738830077,1368.88226160321,1369.31713490567,
1369.75200820816,1370.18688151067,1370.6217548132,1371.05662811577,1371.49150141837,
1371.926374721,1372.36124802367,1372.79612132639,1373.23099462915,1373.66586793196,
1374.10074123481,1374.53646723311,1374.97219323142,1375.40706653438,1375.84193983741,
1376.2768131405,1376.71168644365,1377.14655974687,1377.58143305016,1378.01630635352,
1378.45117965696,1378.88605296047,1379.32092626407,1379.75579956775,1380.19067287151,
1380.62554617536,1381.06041947931,1381.49614547817,1381.93187147704,1382.36674478117,
1382.8016180854,1383.23649138973,1383.67136469416,1384.10623799869,1384.54111130334,
1384.97598460809,1385.41085791295,1385.84573121793,1386.28060452302,1386.71547782823,
1387.15035113356,1387.585224439,1388.02009774458,1388.45582374427,1388.89154974397,
1389.32642304979,1389.76129635574,1390.19616966182,1390.63104296803,1391.06591627437,
1391.50078958085,1391.93566288746,1392.37053619421,1392.8054095011,1393.24028280813,
1393.6751561153,1394.1100294226,1394.54490273005,1394.97977603765,1395.41550203836,
1395.85122803908,1396.28610134696,1396.72097465499,1397.15584796317,1397.59072127149,
1398.02559457996,1398.46046788858,1398.89534119734,1399.33021450626,1399.76508781532,
1400.19996112453,1400.63483443389,1401.50458105306,1401.93945436286,1402.37518036469,
1402.81090636651,1403.24577967661,1403.68065298686,1404.11552629725,1404.5503996078,
1404.98527291848,1405.85501954029,1406.2898928514,1406.72476616266,1407.15963947406,
1407.5945127856,1408.02938609727,1408.46425940908,1409.33485872391,1410.205458039,
1410.64033135134,1411.07520466381,1411.51007797639,1411.9449512891,1412.81469791488,
1413.68444454112,1414.5541911678,1415.42393779489,1416.29453711233,1417.16513642995,
1418.03488305796,1418.90462968629,1419.77437631491,1420.64412294377,1421.51386957285,
1422.38361620211,1423.25421552099,1424.12481483992,1424.99456146943,1425.86430809896,
1426.73405472847,1427.60380135791,1428.47354798724,1429.34329461641,1430.21389393501,
1431.08449325349,1431.9542398821,1432.82398651043,1433.69373313844,1434.56347976611,
1435.4332263934,1436.30297302029,1437.17357233701,1438.04417165351,1438.91391827929,
1439.78366490459,1440.65341152939,1441.52315815367,1441.95803146562,1442.39290477743,
1442.8277780891,1443.26265140064,1444.13325071451,1445.00385002811,1445.43872333908,
1445.87359664991,1446.3084699606,1446.74334327114,1447.17821658153,1447.61308989178,
1448.48283651184,1448.91770982164,1449.3525831313,1449.78745644081,1450.22232975017,
1450.65720305938,1451.09292906076,1451.52865506214,1451.96352837105,1452.39840167982,
1452.83327498843,1453.2681482969,1453.70302160522,1454.1378949134,1454.57276822143,
1455.00764152931,1455.44251483705,1455.87738814464,1456.31226145209,1456.7471347594,
1457.18200806657,1457.6168813736,1458.05260737389,1458.48833337418,1458.92320668093,
1459.35807998754,1459.79295329402,1460.22782660036,1460.66269990657,1461.09757321265,
1461.5324465186,1461.96731982443,1462.40219313012,1462.83706643569,1463.27193974114,
1463.70681304647,1464.14168635168,1464.57655965677,1465.0122856561,1465.44801165544,
1465.8828849603,1466.31775826505,1466.7526315697,1467.18750487423,1467.62237817866,
1468.05725148299,1468.49212478722,1468.92699809135,1469.36187139539,1469.79674469933,
1470.23161800319,1470.66649130695,1471.10136461063,1471.53623791422,1471.97196391283,
1472.40768991143,1472.84256321487,1473.27743651823,1473.71230982152,1474.14718312474,
1474.58205642789,1475.01692973098,1475.451803034,1475.88667633697,1476.32154963988,
1476.75642294274,1477.19129624555,1477.62616954831,1478.06104285102,1478.4959161537,
1478.93164215186,1479.36736815002,1479.80224145262,1480.23711475519,1480.67198805772,
1481.10686136023,1481.54173466272,1481.97660796518,1482.41148126762,1482.84635457005,
1483.28122787247,1483.71610117488,1484.15097447728,1484.58584777968,1485.02072108208,
1485.45559438449,1485.89132038254,1486.32704638059,1486.76191968301,1487.19679298544,
1487.63166628788,1488.06653959035,1488.50141289283,1488.93628619534,1489.37115949787,
1489.80603280044,1490.24090610304,1490.67577940567,1491.11065270835,1491.54552601106,
1491.98039931382,1492.41527261663,1492.8509986149,1493.28672461318,1493.72159791609,
1494.15647121906,1494.59134452208,1495.02621782517,1495.46109112832,1495.89596443154,
1496.33083773483,1496.76571103819,1497.20058434163,1497.63545764515,1498.07033094874,
1498.50520425242,1498.94007755618,1499.37495086004,1499.81067685885,1500.24640285767,
1500.68127616171,1501.11614946584,1501.55102277007,1501.9858960744,1502.42076937883,
1502.85564268337,1503.29051598801,1503.72538929276,1504.16026259762,1504.5951359026,
1505.03000920769,1505.4648825129,1505.89975581823,1506.33462912368,1506.77035512331,
1507.20608112294,1507.64095442864,1508.07582773446,1508.51070104041,1508.94557434649,
1509.3804476527,1509.81532095904,1510.25019426552,1510.68506757213,1511.11994087888,
1511.55481418577,1511.9896874928,1512.42456079996,1512.85943410727,1513.29430741472,
1513.73003341537,1514.16575941601,1514.60063272375,1515.03550603163,1515.47037933966,
1515.90525264784,1516.34012595616,1516.77499926463,1517.20987257325,1517.64474588201,
1518.07961919093,1518.51449249999,1518.9493658092,1519.38423911856,1519.81911242807,
1520.25398573772,1520.68971173947,1521.12543774122,1521.56031105118,1521.99518436128,
1522.43005767153,1523.29980429246,1523.73467760315,1524.16955091398,1524.60442422495,
1525.03929753607,1525.47417084733,1525.90904415873,1526.77879078194,1527.64939009657,
1528.08511609939,1528.51998941146,1528.95486272367,1529.38973603601,1530.25948266106,
1531.1292292866,1531.99897591261,1532.86872253907,1533.73846916596,1534.60906848325,
1535.47966780073,1536.34941442858,1537.21916105675,1538.08890768523,1538.95865431398,
1539.82840094295,1540.69814757212,1541.56874689096,1542.43934620985,1543.30909283933,
1544.17883946886,1545.04858609839,1545.91833272787,1546.78807935726,1547.65782598651,
1548.52842530518,1549.39902462375,1550.26877125249,1551.13851788097,1552.00826450914,
1552.87801113699,1553.74775776447,1554.61750439156,1555.48810370844,1556.35870302511,
1557.22844965112,1558.09819627666,1558.96794290171,1559.83768952626,1560.27256283834,
1560.70743615028,1561.57718277377,1562.44778208785,1563.31838140165,1563.75325471277,
1564.18812802374,1564.62300133457,1565.05787464526,1565.9276212662,1566.79736788655,
1567.2322411965,1567.66711450631,1568.10198781596,1568.53686112547,1568.97173443483,
1569.40746043628,1569.84318643774,1570.2780597468,1570.71293305571,1571.14780636448,
1571.5826796731,1572.01755298157,1572.45242628989,1572.88729959806,1573.32217290609,
1573.75704621397,1574.19191952171,1574.62679282931,1575.06166613676,1575.49653944407,
1575.93141275123,1576.36713875159,1576.80286475195,1577.23773805884,1577.67261136559,
1578.1074846722,1578.54235797868,1578.97723128502,1579.41210459124,1579.84697789732,
1580.28185120327,1580.71672450909,1581.15159781478,1581.58647112036,1582.0213444258,
1582.45621773113,1582.89109103634,1583.32681703573,1583.76254303513,1584.1974163401,
1584.63228964497,1585.06716294972,1585.50203625436,1585.9369095589,1586.37178286333,
1586.80665616766,1587.24152947189,1587.67640277602,1588.11127608005,1588.546149384,
1588.98102268785,1589.41589599161,1589.85076929529,1590.28649529394,1590.72222129258,
1591.1570945961,1591.59196789953,1592.0268412029,1592.46171450619,1592.8965878094,
1593.33146111256,1593.76633441564,1594.20120771867,1594.63608102164,1595.07095432455,
1595.50582762741,1595.94070093021,1596.37557423297,1596.81044753569,1597.24617353387,
1597.68189953206,1598.11677283469,1598.55164613729,1598.98651943985,1599.42139274239,
1599.8562660449,1600.29113934738,1600.72601264985,1601.16088595229,1601.59575925472,
1602.03063255714,1602.46550585955,1602.90037916195,1603.33525246435,1603.77012576675,
1604.2058517648,1604.64157776285,1605.07645106526,1605.51132436768,1605.94619767011,
1606.38107097255,1606.81594427502,1607.2508175775,1607.68569088001,1608.12056418254,
1608.55543748511,1608.99031078771,1609.42518409034,1609.86005739302,1610.29493069573,
1610.72980399849,1611.16552999674,1611.60125599499,1612.03612929785,1612.47100260076,
1612.90587590373,1613.34074920675,1613.77562250984,1614.21049581299,1614.64536911621,
1615.0802424195,1615.51511572286,1615.9499890263,1616.38486232981,1616.81973563341,
1617.25460893709,1617.68948224085,1618.12520823963,1618.5609342384,1618.99580754234,
1619.43068084638,1619.86555415051,1620.30042745474,1620.73530075907,1621.1701740635,
1621.60504736804,1622.03992067268,1622.47479397743,1622.90966728229,1623.34454058727,
1623.77941389236,1624.21428719757,1624.6491605029,1625.08488650247,1625.52061250204,
1625.95548580761,1626.39035911331,1626.82523241913,1627.26010572508,1627.69497903116,
1628.12985233737,1628.56472564372,1628.99959895019,1629.43447225681,1629.86934556356,
1630.30421887044,1630.73909217747,1631.17396548464,1631.60883879195,1632.04456479252,
1632.48029079309,1632.91516410068,1633.35003740842,1633.78491071631,1634.21978402433,
1634.65465733251,1635.08953064083,1635.5244039493,1635.95927725792,1636.39415056668,
1636.8290238756,1637.26389718466,1637.69877049387,1638.13364380323,1638.56851711274,
1639.00424311442,1639.43996911609,1639.8748424259,1640.30971573585,1640.74458904595,
1641.6143356666,1642.04920897714,1642.48408228782,1642.91895559865,1643.35382890963,
1643.78870222074,1644.223575532,1645.09332215494,1645.52819546661,1645.96392146936,
1646.39964747212,1646.83452078406,1647.26939409614,1647.70426740834,1648.57401403314,
1649.44376065844,1650.31350728422,1650.74838059729,1651.18325391046,1652.05300053714,
1652.92359985428,1653.79419917162,1654.66394579929,1655.5336924273,1656.40343905563,
1657.27318568424,1658.14293231311,1659.01267894219,1659.88327826096,1660.75387757982,
1661.62362420926,1662.49337083877,1663.3631174683,1664.23286409781,1665.10261072725,
1665.97235735658,1666.84295667531,1667.71355599396,1668.58330262282,1669.45304925143,
1670.32279587976,1671.19254250778,1672.06228913544,1672.93203576273,1673.80263507977,
1674.6732343966,1675.54298102284,1676.41272764862,1677.28247427392,1678.15222089872,
1679.021967523,1679.89171414676,1680.76231346105,1681.19803946366,1681.63291277506,
1682.06778608632,1682.50265939743,1682.93753270841,1683.37240601924,1684.24215264047,
1684.67702595086,1685.11189926111,1685.54677257121,1685.98164588116,1686.41651919097,
1686.85139250063,1687.28626581014,1687.72199181166,1688.15771781319,1688.5925911224,
1689.02746443146,1689.46233774038,1689.89721104914,1690.33208435776,1690.76695766623,
1691.20183097455,1691.63670428272,1692.07157759075,1692.50645089864,1692.94132420637,
1693.37619751397,1693.81107082142,1694.24594412873,1694.68167012916,1695.11739612959,
1695.55226943662,1695.9871427435,1696.42201605025,1696.85688935687,1697.29176266334,
1697.72663596969,1698.1615092759,1698.59638258198,1699.03125588793,1699.46612919375,
1699.90100249945,1700.33587580502,1700.77074911047,1701.20562241579,1701.64134841525,
1702.0770744147,1702.51194771979,1702.94682102476,1703.38169432963,1703.81656763438,
1704.25144093902,1704.68631424356,1705.12118754799,1705.55606085232,1705.99093415655,
1706.42580746068,1706.86068076471,1707.29555406866,1707.73042737251,1708.16530067627,
1708.60102667496,1709.03675267365,1709.47162597724,1709.90649928076,1710.34137258419,
1710.77624588756,1711.21111919085,1711.64599249406,1712.08086579722,1712.5157391003,
1712.95061240333,1713.3854857063,1713.82035900921,1714.25523231207,1714.69010561487,
1715.12497891763,1715.56070491584,1715.99643091404,1716.43130421671,1716.86617751935,
1717.30105082195,1717.73592412451,1718.17079742705,1718.60567072956,1719.04054403204,
1719.4754173345,1719.91029063695,1720.34516393938,1720.7800372418,1721.21491054421,
1721.64978384661,1722.08465714901,1722.52038314706,1722.9561091451,1723.39098244751,
1723.82585574992,1724.26072905233,1724.69560235476,1725.13047565721,1725.56534895967,
1726.00022226216,1726.43509556467,1726.8699688672,1727.30484216977,1727.73971547236,
1728.174588775,1728.60946207767,1729.04433538039,1729.48006137861,1729.91578737684,
1730.35066067965,1730.78553398251,1731.22040728542,1731.65528058838,1732.09015389141,
1732.5250271945,1732.95990049765,1733.39477380087,1733.82964710416,1734.26452040752,
1734.69939371096,1735.13426701447,1735.56914031807,1736.00401362175,1736.43973962048,
1736.8754656192,1737.31033892306,1737.745212227,1738.18008553104,1738.61495883517,
1739.0498321394,1739.48470544373,1739.91957874816,1740.35445205269,1740.78932535734,
1741.22419866209,1741.65907196695,1742.09394527193,1742.52881857702,1742.96369188223,
1743.39941788174,1743.83514388125,1744.2700171867,1744.70489049227,1745.13976379797,
1745.57463710379,1746.00951040974,1746.44438371582,1746.87925702203,1747.31413032837,
1747.74900363485,1748.18387694146,1748.61875024821,1749.0536235551,1749.48849686213,
1749.92337016929,1750.3590961698,1750.7948221703,1751.22969547775,1751.66456878534,
1752.09944209308,1752.53431540096,1752.96918870899,1753.40406201717,1753.83893532549,
1754.27380863396,1754.70868194258,1755.14355525134,1755.57842856026,1756.01330186932,
1756.44817517853,1756.88304848789,1757.31877448949,1757.75450049109,1758.18937380075,
1759.05912042051,1759.49399373061,1759.92886704086,1760.36374035125,1760.79861366179,
1761.23348697248,1761.66836028331,1762.10323359429,1762.5381069054,1763.40785352806,
1763.8427268396,1764.27845284228,1764.71417884496,1765.14905215677,1765.58392546872,
1766.0187987808,1766.88854540534,1767.75829203039,1768.1931653431,1768.62803865593,
1769.06291196888,1769.49778528195,1770.36753190841,1771.2381312254,1772.10873054259,
1772.97847717007,1773.84822379791,1774.71797042609,1775.58771705456,1776.45746368331,
1777.32721031228,1778.19780963089,1779.06840894783,1779.93815555508,1780.80790201176,
1781.67764871408),.UNSPECIFIED.) ;
#836 = B_SPLINE_SURFACE_WITH_KNOTS('',3,1,((#113116,#113117),(#113118,#113119),
(#113120,#113121),(#113122,#113123),(#113124,#113125),(#113126,#113127),
(#113128,#113129),(#113130,#113131),(#113132,#113133),(#113134,#113135),
(#113136,#113137),(#113138,#113139),(#113140,#113141),(#113142,#113143),
(#113144,#113145),(#113146,#113147),(#113148,#113149),(#113150,#113151),
(#113152,#113153)),.UNSPECIFIED.,.T.,.F.,.F.,(4,1,1,1,1,1,1,1,1,1,1,1,1,
1,1,1,4),(2,2),(0.,0.84428169467316,1.68856338934632,2.53284508400807,3.37712677866981,
4.22140847333581,5.06569016800181,5.90997186266355,6.75425355732529,7.5985352519836,
8.44281694664192,9.28709864130792,10.1313803359739,10.9756620306322,11.8199437252905,
12.664225419956,13.5085071146214),(-0.0112712723153948,0.214916064351503),
 .UNSPECIFIED.) ;
#837 = B_SPLINE_SURFACE_WITH_KNOTS('',3,1,((#113155,#113156),(#113157,#113158),
(#113159,#113160),(#113161,#113162),(#113163,#113164),(#113165,#113166),
(#113167,#113168),(#113169,#113170),(#113171,#113172),(#113173,#113174),
(#113175,#113176)),.UNSPECIFIED.,.F.,.F.,.F.,(4,1,1,1,1,1,1,1,4),(2,2),
(0.,1.04064620349252,2.08129240698504,3.12193860703556,4.16258480708607,
5.2032310071414,6.24387720719673,7.28452341068926,8.32516961418179),(0.,
0.214915892336475),.UNSPECIFIED.) ;
#838 = B_SPLINE_SURFACE_WITH_KNOTS('',3,1,((#113179,#113180),(#113181,#113182),
(#113183,#113184),(#113185,#113186)),.UNSPECIFIED.,.F.,.F.,.F.,(4,4),(2,
2),(-1.11022302462516E-16,3.4846841528001),(0.,0.212356567860224),
 .UNSPECIFIED.) ;
#839 = B_SPLINE_SURFACE_WITH_KNOTS('',3,1,((#113188,#113189),(#113190,#113191),
(#113192,#113193),(#113194,#113195),(#113196,#113197),(#113198,#113199),
(#113200,#113201),(#113202,#113203),(#113204,#113205),(#113206,#113207),
(#113208,#113209)),.UNSPECIFIED.,.F.,.F.,.F.,(4,1,1,1,1,1,1,1,4),(2,2),
(0.,1.04062614942685,2.0812522988537,3.12187844827608,4.16250459769846,
5.20313074711661,6.24375689653477,7.28438304596783,8.32500919540089),(0.,
0.214916063344347),.UNSPECIFIED.) ;
#840 = B_SPLINE_SURFACE_WITH_KNOTS('',3,1,((#113211,#113212),(#113213,#113214),
(#113215,#113216),(#113217,#113218)),.UNSPECIFIED.,.F.,.F.,.F.,(4,4),(2,
2),(1.11022302462516E-16,4.51848390029441),(-6.99189760998493E-5,0.212356567829038),
 .UNSPECIFIED.) ;
#841 = B_SPLINE_SURFACE_WITH_KNOTS('',3,1,((#113219,#113220),(#113221,#113222),
(#113223,#113224),(#113225,#113226),(#113227,#113228),(#113229,#113230),
(#113231,#113232),(#113233,#113234),(#113235,#113236),(#113237,#113238),
(#113239,#113240),(#113241,#113242),(#113243,#113244),(#113245,#113246),
(#113247,#113248),(#113249,#113250),(#113251,#113252),(#113253,#113254),
(#113255,#113256)),.UNSPECIFIED.,.T.,.F.,.F.,(4,1,1,1,1,1,1,1,1,1,1,1,1,
1,1,1,4),(2,2),(0.,2.69519445779221,5.61545499238393,8.53571552697323,11.2309099847624,
13.9261044425515,16.8463649771433,19.7666255117326,22.4618199695218,25.1570144273109,
28.0772749619002,30.9975354964919,33.6927299542811,36.3879244120703,39.3081849466596,
42.2284454812513,44.9236399390405),(-0.021515064961137,0.21515064961137),
 .UNSPECIFIED.) ;
#842 = B_SPLINE_SURFACE_WITH_KNOTS('',3,1,((#113258,#113259),(#113260,#113261),
(#113262,#113263),(#113264,#113265)),.UNSPECIFIED.,.F.,.F.,.F.,(4,4),(2,
2),(0.,3.40704145701401),(-0.000292126274588819,0.212844506430303),
 .UNSPECIFIED.) ;
#843 = B_SPLINE_SURFACE_WITH_KNOTS('',3,1,((#113268,#113269),(#113270,#113271),
(#113272,#113273),(#113274,#113275),(#113276,#113277),(#113278,#113279),
(#113280,#113281),(#113282,#113283),(#113284,#113285)),.UNSPECIFIED.,.F.,
 .F.,.F.,(4,1,1,1,1,1,4),(2,2),(-0.00583358110187113,1.29587390932424,1.94381087119108,
2.59174783305793,3.23968479492214,3.88762175678635,5.18932922796654),(-0.00583356183498457,
0.218727515757821),.UNSPECIFIED.) ;
#844 = B_SPLINE_SURFACE_WITH_KNOTS('',3,1,((#113287,#113288),(#113289,#113290),
(#113291,#113292),(#113293,#113294)),.UNSPECIFIED.,.F.,.F.,.F.,(4,4),(2,
2),(0.,2.26229870547718),(0.,0.212844507129699),.UNSPECIFIED.) ;
#845 = B_SPLINE_SURFACE_WITH_KNOTS('',3,1,((#113296,#113297),(#113298,#113299),
(#113300,#113301),(#113302,#113303),(#113304,#113305),(#113306,#113307),
(#113308,#113309),(#113310,#113311),(#113312,#113313)),.UNSPECIFIED.,.F.,
 .F.,.F.,(4,1,1,1,1,1,4),(2,2),(0.,1.29587422179682,1.94381133989722,2.59174845799762,
3.23968557610065,3.88762269420369,5.18349660704779),(0.,0.218727518540508),
 .UNSPECIFIED.) ;
#846 = B_SPLINE_SURFACE_WITH_KNOTS('',3,1,((#113566,#113567),(#113568,#113569),
(#113570,#113571),(#113572,#113573),(#113574,#113575),(#113576,#113577),
(#113578,#113579),(#113580,#113581),(#113582,#113583),(#113584,#113585),
(#113586,#113587),(#113588,#113589),(#113590,#113591),(#113592,#113593),
(#113594,#113595),(#113596,#113597),(#113598,#113599),(#113600,#113601),
(#113602,#113603)),.UNSPECIFIED.,.T.,.F.,.F.,(4,1,1,1,1,1,1,1,1,1,1,1,1,
1,1,1,4),(2,2),(0.,0.844281694673181,1.68856338934636,2.5328450840081,3.37712677866985,
4.22140847333585,5.06569016800186,5.90997186266359,6.75425355732532,7.59853525198361,
8.44281694664191,9.28709864130793,10.131380335974,10.9756620306357,11.8199437252974,
12.6642254199629,13.5085071146283),(-0.0112712723182462,0.214916064351496),
 .UNSPECIFIED.) ;
#847 = B_SPLINE_SURFACE_WITH_KNOTS('',3,1,((#113605,#113606),(#113607,#113608),
(#113609,#113610),(#113611,#113612),(#113613,#113614),(#113615,#113616),
(#113617,#113618),(#113619,#113620),(#113621,#113622),(#113623,#113624),
(#113625,#113626)),.UNSPECIFIED.,.F.,.F.,.F.,(4,1,1,1,1,1,1,1,4),(2,2),
(0.,1.04064620349252,2.08129240698504,3.12193860704037,4.16258480709569,
5.20323100714621,6.24387720719672,7.28452341068925,8.32516961418178),(0.,
0.214915892305322),.UNSPECIFIED.) ;
#848 = B_SPLINE_SURFACE_WITH_KNOTS('',3,1,((#113629,#113630),(#113631,#113632),
(#113633,#113634),(#113635,#113636)),.UNSPECIFIED.,.F.,.F.,.F.,(4,4),(2,
2),(-1.11022302462516E-16,3.4846841528001),(0.,0.212356567860235),
 .UNSPECIFIED.) ;
#849 = B_SPLINE_SURFACE_WITH_KNOTS('',3,1,((#113638,#113639),(#113640,#113641),
(#113642,#113643),(#113644,#113645),(#113646,#113647),(#113648,#113649),
(#113650,#113651),(#113652,#113653),(#113654,#113655),(#113656,#113657),
(#113658,#113659)),.UNSPECIFIED.,.F.,.F.,.F.,(4,1,1,1,1,1,1,1,4),(2,2),
(0.,1.04062614942688,2.08125229885376,3.12187844827613,4.1625045976985,
5.20313074711665,6.24375689653479,7.28438304596787,8.32500919540094),(0.,
0.214916063344399),.UNSPECIFIED.) ;
#850 = B_SPLINE_SURFACE_WITH_KNOTS('',3,1,((#113661,#113662),(#113663,#113664),
(#113665,#113666),(#113667,#113668)),.UNSPECIFIED.,.F.,.F.,.F.,(4,4),(2,
2),(-1.11022302462516E-16,4.5184839002944),(-6.99189761287855E-5,0.212356567829033),
 .UNSPECIFIED.) ;
#851 = B_SPLINE_SURFACE_WITH_KNOTS('',3,1,((#113669,#113670),(#113671,#113672),
(#113673,#113674),(#113675,#113676),(#113677,#113678),(#113679,#113680),
(#113681,#113682),(#113683,#113684),(#113685,#113686),(#113687,#113688),
(#113689,#113690),(#113691,#113692),(#113693,#113694),(#113695,#113696),
(#113697,#113698),(#113699,#113700),(#113701,#113702),(#113703,#113704),
(#113705,#113706)),.UNSPECIFIED.,.T.,.F.,.F.,(4,1,1,1,1,1,1,1,1,1,1,1,1,
1,1,1,4),(2,2),(0.,2.69519445779222,5.61545499238395,8.53571552697321,11.2309099847624,
13.9261044425516,16.8463649771433,19.7666255117326,22.4618199695217,25.1570144273109,
28.0772749619002,30.9975354964919,33.692729954281,36.3879244120702,39.3081849466595,
42.2284454812513,44.9236399390404),(-0.0215150649611441,0.215150649611441),
 .UNSPECIFIED.) ;
#852 = B_SPLINE_SURFACE_WITH_KNOTS('',3,1,((#113708,#113709),(#113710,#113711),
(#113712,#113713),(#113714,#113715)),.UNSPECIFIED.,.F.,.F.,.F.,(4,4),(2,
2),(-1.20032081259135E-14,3.40704145701401),(-0.000292137134752522,0.212844506430324),
 .UNSPECIFIED.) ;
#853 = B_SPLINE_SURFACE_WITH_KNOTS('',3,1,((#113718,#113719),(#113720,#113721),
(#113722,#113723),(#113724,#113725),(#113726,#113727),(#113728,#113729),
(#113730,#113731),(#113732,#113733),(#113734,#113735)),.UNSPECIFIED.,.F.,
 .F.,.F.,(4,1,1,1,1,1,4),(2,2),(0.,1.2958739093245,1.94381087119137,2.59174783305825,
3.23968479492247,3.88762175678669,5.18349566611894),(0.,0.218727515290808),
 .UNSPECIFIED.) ;
#854 = B_SPLINE_SURFACE_WITH_KNOTS('',3,1,((#113737,#113738),(#113739,#113740),
(#113741,#113742),(#113743,#113744)),.UNSPECIFIED.,.F.,.F.,.F.,(4,4),(2,
2),(0.,2.26229870547723),(0.,0.212844507129729),.UNSPECIFIED.) ;
#855 = B_SPLINE_SURFACE_WITH_KNOTS('',3,1,((#113746,#113747),(#113748,#113749),
(#113750,#113751),(#113752,#113753),(#113754,#113755),(#113756,#113757),
(#113758,#113759),(#113760,#113761),(#113762,#113763)),.UNSPECIFIED.,.F.,
 .F.,.F.,(4,1,1,1,1,1,4),(2,2),(0.,1.29587422179652,1.94381133989956,2.5917484580026,
3.23968557610299,3.88762269420339,5.18349691602093),(0.,0.21872751905286),
 .UNSPECIFIED.) ;
#856 = B_SPLINE_SURFACE_WITH_KNOTS('',3,1,((#113764,#113765),(#113766,#113767),
(#113768,#113769),(#113770,#113771),(#113772,#113773),(#113774,#113775),
(#113776,#113777),(#113778,#113779),(#113780,#113781),(#113782,#113783),
(#113784,#113785)),.UNSPECIFIED.,.T.,.F.,.F.,(4,1,1,1,1,1,1,1,4),(2,2),
(0.,0.903185063809554,1.80637013757091,2.70955520128371,3.61274027504511,
4.51592534880276,5.4191104125156,6.32229548627704,7.22548054998985),(0.,
0.223990409920864),.UNSPECIFIED.) ;
#857 = B_SPLINE_SURFACE_WITH_KNOTS('',1,3,((#113835,#113836,#113837,#113838,
#113839,#113840,#113841,#113842,#113843,#113844,#113845,#113846,#113847,
#113848,#113849,#113850,#113851,#113852,#113853),(#113854,#113855,#113856,
#113857,#113858,#113859,#113860,#113861,#113862,#113863,#113864,#113865,
#113866,#113867,#113868,#113869,#113870,#113871,#113872)),.UNSPECIFIED.,
 .F.,.T.,.F.,(2,2),(4,1,1,1,1,1,1,1,1,1,1,1,1,1,1,1,4),(0.,0.431146952730274),
(0.,0.667571568814079,1.33514313762816,2.00271471386765,2.67028629010715,
3.33785785892125,4.00542942773535,4.67300100397484,5.34057258021434,6.00814415645112,
6.67571573268789,7.34328730150198,8.01085887031606,8.67843044655556,9.34600202279505,
10.0135735916092,10.6811451604233),.UNSPECIFIED.) ;
#858 = B_SPLINE_SURFACE_WITH_KNOTS('',3,1,((#113874,#113875),(#113876,#113877),
(#113878,#113879),(#113880,#113881),(#113882,#113883),(#113884,#113885),
(#113886,#113887),(#113888,#113889),(#113890,#113891),(#113892,#113893),
(#113894,#113895),(#113896,#113897),(#113898,#113899),(#113900,#113901),
(#113902,#113903),(#113904,#113905),(#113906,#113907),(#113908,#113909),
(#113910,#113911)),.UNSPECIFIED.,.T.,.F.,.F.,(4,1,1,1,1,1,1,1,1,1,1,1,1,
1,1,1,4),(2,2),(0.,0.667571568814083,1.33514313762817,2.00271471386766,
2.67028629010715,3.33785785892125,4.00542942773535,4.67300100397484,5.34057258021433,
6.00814415645111,6.67571573268789,7.34328730150198,8.01085887031607,8.67843044655557,
9.34600202279507,10.0135735916092,10.6811451604233),(0.,0.431146952730387),
 .UNSPECIFIED.) ;
#859 = FACE_OUTER_BOUND('',#1332,.T.) ;
#860 = FACE_OUTER_BOUND('',#1333,.T.) ;
#861 = FACE_OUTER_BOUND('',#1334,.T.) ;
#862 = FACE_OUTER_BOUND('',#1335,.T.) ;
#863 = FACE_OUTER_BOUND('',#1336,.T.) ;
#864 = FACE_OUTER_BOUND('',#1337,.T.) ;
#865 = FACE_OUTER_BOUND('',#1338,.T.) ;
#866 = FACE_OUTER_BOUND('',#1343,.T.) ;
#867 = FACE_OUTER_BOUND('',#1344,.T.) ;
#868 = FACE_OUTER_BOUND('',#1345,.T.) ;
#869 = FACE_OUTER_BOUND('',#1346,.T.) ;
#870 = FACE_OUTER_BOUND('',#1347,.T.) ;
#871 = FACE_OUTER_BOUND('',#1348,.T.) ;
#872 = FACE_OUTER_BOUND('',#1349,.T.) ;
#873 = FACE_OUTER_BOUND('',#1350,.T.) ;
#874 = FACE_OUTER_BOUND('',#1351,.T.) ;
#875 = FACE_OUTER_BOUND('',#1352,.T.) ;
#876 = FACE_OUTER_BOUND('',#1353,.T.) ;
#877 = FACE_OUTER_BOUND('',#1354,.T.) ;
#878 = FACE_OUTER_BOUND('',#1355,.T.) ;
#879 = FACE_OUTER_BOUND('',#1356,.T.) ;
#880 = FACE_OUTER_BOUND('',#1357,.T.) ;
#881 = FACE_OUTER_BOUND('',#1362,.T.) ;
#882 = FACE_OUTER_BOUND('',#1364,.T.) ;
#883 = FACE_OUTER_BOUND('',#1366,.T.) ;
#884 = FACE_OUTER_BOUND('',#1367,.T.) ;
#885 = FACE_OUTER_BOUND('',#1368,.T.) ;
#886 = FACE_OUTER_BOUND('',#1369,.T.) ;
#887 = FACE_OUTER_BOUND('',#1370,.T.) ;
#888 = FACE_OUTER_BOUND('',#1371,.T.) ;
#889 = FACE_OUTER_BOUND('',#1372,.T.) ;
#890 = FACE_OUTER_BOUND('',#1373,.T.) ;
#891 = FACE_OUTER_BOUND('',#1374,.T.) ;
#892 = FACE_OUTER_BOUND('',#1375,.T.) ;
#893 = FACE_OUTER_BOUND('',#1376,.T.) ;
#894 = FACE_OUTER_BOUND('',#1377,.T.) ;
#895 = FACE_OUTER_BOUND('',#1378,.T.) ;
#896 = FACE_OUTER_BOUND('',#1379,.T.) ;
#897 = FACE_OUTER_BOUND('',#1380,.T.) ;
#898 = FACE_OUTER_BOUND('',#1381,.T.) ;
#899 = FACE_OUTER_BOUND('',#1382,.T.) ;
#900 = FACE_OUTER_BOUND('',#1383,.T.) ;
#901 = FACE_OUTER_BOUND('',#1384,.T.) ;
#902 = FACE_OUTER_BOUND('',#1385,.T.) ;
#903 = FACE_OUTER_BOUND('',#1386,.T.) ;
#904 = FACE_OUTER_BOUND('',#1387,.T.) ;
#905 = FACE_OUTER_BOUND('',#1388,.T.) ;
#906 = FACE_OUTER_BOUND('',#1389,.T.) ;
#907 = FACE_OUTER_BOUND('',#1390,.T.) ;
#908 = FACE_OUTER_BOUND('',#1391,.T.) ;
#909 = FACE_OUTER_BOUND('',#1392,.T.) ;
#910 = FACE_OUTER_BOUND('',#1393,.T.) ;
#911 = FACE_OUTER_BOUND('',#1394,.T.) ;
#912 = FACE_OUTER_BOUND('',#1395,.T.) ;
#913 = FACE_OUTER_BOUND('',#1396,.T.) ;
#914 = FACE_OUTER_BOUND('',#1397,.T.) ;
#915 = FACE_OUTER_BOUND('',#1398,.T.) ;
#916 = FACE_OUTER_BOUND('',#1399,.T.) ;
#917 = FACE_OUTER_BOUND('',#1400,.T.) ;
#918 = FACE_OUTER_BOUND('',#1401,.T.) ;
#919 = FACE_OUTER_BOUND('',#1402,.T.) ;
#920 = FACE_OUTER_BOUND('',#1403,.T.) ;
#921 = FACE_OUTER_BOUND('',#1404,.T.) ;
#922 = FACE_OUTER_BOUND('',#1405,.T.) ;
#923 = FACE_OUTER_BOUND('',#1406,.T.) ;
#924 = FACE_OUTER_BOUND('',#1407,.T.) ;
#925 = FACE_OUTER_BOUND('',#1408,.T.) ;
#926 = FACE_OUTER_BOUND('',#1409,.T.) ;
#927 = FACE_OUTER_BOUND('',#1410,.T.) ;
#928 = FACE_OUTER_BOUND('',#1411,.T.) ;
#929 = FACE_OUTER_BOUND('',#1413,.T.) ;
#930 = FACE_OUTER_BOUND('',#1414,.T.) ;
#931 = FACE_OUTER_BOUND('',#1415,.T.) ;
#932 = FACE_OUTER_BOUND('',#1416,.T.) ;
#933 = FACE_OUTER_BOUND('',#1417,.T.) ;
#934 = FACE_OUTER_BOUND('',#1418,.T.) ;
#935 = FACE_OUTER_BOUND('',#1419,.T.) ;
#936 = FACE_OUTER_BOUND('',#1420,.T.) ;
#937 = FACE_OUTER_BOUND('',#1421,.T.) ;
#938 = FACE_OUTER_BOUND('',#1422,.T.) ;
#939 = FACE_OUTER_BOUND('',#1423,.T.) ;
#940 = FACE_OUTER_BOUND('',#1424,.T.) ;
#941 = FACE_OUTER_BOUND('',#1425,.T.) ;
#942 = FACE_OUTER_BOUND('',#1426,.T.) ;
#943 = FACE_OUTER_BOUND('',#1427,.T.) ;
#944 = FACE_OUTER_BOUND('',#1428,.T.) ;
#945 = FACE_OUTER_BOUND('',#1429,.T.) ;
#946 = FACE_OUTER_BOUND('',#1430,.T.) ;
#947 = FACE_OUTER_BOUND('',#1432,.T.) ;
#948 = FACE_OUTER_BOUND('',#1433,.T.) ;
#949 = FACE_OUTER_BOUND('',#1434,.T.) ;
#950 = FACE_OUTER_BOUND('',#1435,.T.) ;
#951 = FACE_OUTER_BOUND('',#1436,.T.) ;
#952 = FACE_OUTER_BOUND('',#1437,.T.) ;
#953 = FACE_OUTER_BOUND('',#1438,.T.) ;
#954 = FACE_OUTER_BOUND('',#1439,.T.) ;
#955 = FACE_OUTER_BOUND('',#1440,.T.) ;
#956 = FACE_OUTER_BOUND('',#1441,.T.) ;
#957 = FACE_OUTER_BOUND('',#1442,.T.) ;
#958 = FACE_OUTER_BOUND('',#1443,.T.) ;
#959 = FACE_OUTER_BOUND('',#1444,.T.) ;
#960 = FACE_OUTER_BOUND('',#1450,.T.) ;
#961 = FACE_OUTER_BOUND('',#1456,.T.) ;
#962 = FACE_OUTER_BOUND('',#1457,.T.) ;
#963 = FACE_OUTER_BOUND('',#1458,.T.) ;
#964 = FACE_OUTER_BOUND('',#1459,.T.) ;
#965 = FACE_OUTER_BOUND('',#1460,.T.) ;
#966 = FACE_OUTER_BOUND('',#1461,.T.) ;
#967 = FACE_OUTER_BOUND('',#1462,.T.) ;
#968 = FACE_OUTER_BOUND('',#1463,.T.) ;
#969 = FACE_OUTER_BOUND('',#1464,.T.) ;
#970 = FACE_OUTER_BOUND('',#1465,.T.) ;
#971 = FACE_OUTER_BOUND('',#1466,.T.) ;
#972 = FACE_OUTER_BOUND('',#1467,.T.) ;
#973 = FACE_OUTER_BOUND('',#1468,.T.) ;
#974 = FACE_OUTER_BOUND('',#1469,.T.) ;
#975 = FACE_OUTER_BOUND('',#1470,.T.) ;
#976 = FACE_OUTER_BOUND('',#1471,.T.) ;
#977 = FACE_OUTER_BOUND('',#1472,.T.) ;
#978 = FACE_OUTER_BOUND('',#1473,.T.) ;
#979 = FACE_OUTER_BOUND('',#1474,.T.) ;
#980 = FACE_OUTER_BOUND('',#1475,.T.) ;
#981 = FACE_OUTER_BOUND('',#1476,.T.) ;
#982 = FACE_OUTER_BOUND('',#1477,.T.) ;
#983 = FACE_OUTER_BOUND('',#1478,.T.) ;
#984 = FACE_OUTER_BOUND('',#1479,.T.) ;
#985 = FACE_OUTER_BOUND('',#1480,.T.) ;
#986 = FACE_OUTER_BOUND('',#1486,.T.) ;
#987 = FACE_OUTER_BOUND('',#1492,.T.) ;
#988 = FACE_OUTER_BOUND('',#1493,.T.) ;
#989 = FACE_OUTER_BOUND('',#1494,.T.) ;
#990 = FACE_OUTER_BOUND('',#1495,.T.) ;
#991 = FACE_OUTER_BOUND('',#1496,.T.) ;
#992 = FACE_OUTER_BOUND('',#1497,.T.) ;
#993 = FACE_OUTER_BOUND('',#1498,.T.) ;
#994 = FACE_OUTER_BOUND('',#1499,.T.) ;
#995 = FACE_OUTER_BOUND('',#1500,.T.) ;
#996 = FACE_OUTER_BOUND('',#1501,.T.) ;
#997 = FACE_OUTER_BOUND('',#1502,.T.) ;
#998 = FACE_OUTER_BOUND('',#1503,.T.) ;
#999 = FACE_OUTER_BOUND('',#1504,.T.) ;
#1000 = FACE_OUTER_BOUND('',#1505,.T.) ;
#1001 = FACE_OUTER_BOUND('',#1506,.T.) ;
#1002 = FACE_OUTER_BOUND('',#1507,.T.) ;
#1003 = FACE_OUTER_BOUND('',#1508,.T.) ;
#1004 = FACE_OUTER_BOUND('',#1509,.T.) ;
#1005 = FACE_OUTER_BOUND('',#1510,.T.) ;
#1006 = FACE_OUTER_BOUND('',#1511,.T.) ;
#1007 = FACE_OUTER_BOUND('',#1512,.T.) ;
#1008 = FACE_OUTER_BOUND('',#1513,.T.) ;
#1009 = FACE_OUTER_BOUND('',#1514,.T.) ;
#1010 = FACE_OUTER_BOUND('',#1515,.T.) ;
#1011 = FACE_OUTER_BOUND('',#1516,.T.) ;
#1012 = FACE_OUTER_BOUND('',#1517,.T.) ;
#1013 = FACE_OUTER_BOUND('',#1518,.T.) ;
#1014 = FACE_OUTER_BOUND('',#1519,.T.) ;
#1015 = FACE_OUTER_BOUND('',#1520,.T.) ;
#1016 = FACE_OUTER_BOUND('',#1521,.T.) ;
#1017 = FACE_OUTER_BOUND('',#1522,.T.) ;
#1018 = FACE_OUTER_BOUND('',#1523,.T.) ;
#1019 = FACE_OUTER_BOUND('',#1524,.T.) ;
#1020 = FACE_OUTER_BOUND('',#1525,.T.) ;
#1021 = FACE_OUTER_BOUND('',#1526,.T.) ;
#1022 = FACE_OUTER_BOUND('',#1527,.T.) ;
#1023 = FACE_OUTER_BOUND('',#1528,.T.) ;
#1024 = FACE_OUTER_BOUND('',#1529,.T.) ;
#1025 = FACE_OUTER_BOUND('',#1530,.T.) ;
#1026 = FACE_OUTER_BOUND('',#1531,.T.) ;
#1027 = FACE_OUTER_BOUND('',#1534,.T.) ;
#1028 = FACE_OUTER_BOUND('',#1537,.T.) ;
#1029 = FACE_OUTER_BOUND('',#1538,.T.) ;
#1030 = FACE_OUTER_BOUND('',#1539,.T.) ;
#1031 = FACE_OUTER_BOUND('',#1540,.T.) ;
#1032 = FACE_OUTER_BOUND('',#1541,.T.) ;
#1033 = FACE_OUTER_BOUND('',#1542,.T.) ;
#1034 = FACE_OUTER_BOUND('',#1543,.T.) ;
#1035 = FACE_OUTER_BOUND('',#1544,.T.) ;
#1036 = FACE_OUTER_BOUND('',#1545,.T.) ;
#1037 = FACE_OUTER_BOUND('',#1546,.T.) ;
#1038 = FACE_OUTER_BOUND('',#1547,.T.) ;
#1039 = FACE_OUTER_BOUND('',#1548,.T.) ;
#1040 = FACE_OUTER_BOUND('',#1549,.T.) ;
#1041 = FACE_OUTER_BOUND('',#1550,.T.) ;
#1042 = FACE_OUTER_BOUND('',#1551,.T.) ;
#1043 = FACE_OUTER_BOUND('',#1552,.T.) ;
#1044 = FACE_OUTER_BOUND('',#1553,.T.) ;
#1045 = FACE_OUTER_BOUND('',#1554,.T.) ;
#1046 = FACE_OUTER_BOUND('',#1555,.T.) ;
#1047 = FACE_OUTER_BOUND('',#1556,.T.) ;
#1048 = FACE_OUTER_BOUND('',#1557,.T.) ;
#1049 = FACE_OUTER_BOUND('',#1558,.T.) ;
#1050 = FACE_OUTER_BOUND('',#1559,.T.) ;
#1051 = FACE_OUTER_BOUND('',#1560,.T.) ;
#1052 = FACE_OUTER_BOUND('',#1561,.T.) ;
#1053 = FACE_OUTER_BOUND('',#1562,.T.) ;
#1054 = FACE_OUTER_BOUND('',#1563,.T.) ;
#1055 = FACE_OUTER_BOUND('',#1564,.T.) ;
#1056 = FACE_OUTER_BOUND('',#1565,.T.) ;
#1057 = FACE_OUTER_BOUND('',#1566,.T.) ;
#1058 = FACE_OUTER_BOUND('',#1567,.T.) ;
#1059 = FACE_OUTER_BOUND('',#1568,.T.) ;
#1060 = FACE_OUTER_BOUND('',#1569,.T.) ;
#1061 = FACE_OUTER_BOUND('',#1570,.T.) ;
#1062 = FACE_OUTER_BOUND('',#1571,.T.) ;
#1063 = FACE_OUTER_BOUND('',#1572,.T.) ;
#1064 = FACE_OUTER_BOUND('',#1573,.T.) ;
#1065 = FACE_OUTER_BOUND('',#1574,.T.) ;
#1066 = FACE_OUTER_BOUND('',#1575,.T.) ;
#1067 = FACE_OUTER_BOUND('',#1576,.T.) ;
#1068 = FACE_OUTER_BOUND('',#1577,.T.) ;
#1069 = FACE_OUTER_BOUND('',#1578,.T.) ;
#1070 = FACE_OUTER_BOUND('',#1579,.T.) ;
#1071 = FACE_OUTER_BOUND('',#1580,.T.) ;
#1072 = FACE_OUTER_BOUND('',#1581,.T.) ;
#1073 = FACE_OUTER_BOUND('',#1582,.T.) ;
#1074 = FACE_OUTER_BOUND('',#1583,.T.) ;
#1075 = FACE_OUTER_BOUND('',#1584,.T.) ;
#1076 = FACE_OUTER_BOUND('',#1585,.T.) ;
#1077 = FACE_OUTER_BOUND('',#1586,.T.) ;
#1078 = FACE_OUTER_BOUND('',#1587,.T.) ;
#1079 = FACE_OUTER_BOUND('',#1588,.T.) ;
#1080 = FACE_OUTER_BOUND('',#1589,.T.) ;
#1081 = FACE_OUTER_BOUND('',#1590,.T.) ;
#1082 = FACE_OUTER_BOUND('',#1591,.T.) ;
#1083 = FACE_OUTER_BOUND('',#1592,.T.) ;
#1084 = FACE_OUTER_BOUND('',#1593,.T.) ;
#1085 = FACE_OUTER_BOUND('',#1594,.T.) ;
#1086 = FACE_OUTER_BOUND('',#1595,.T.) ;
#1087 = FACE_OUTER_BOUND('',#1596,.T.) ;
#1088 = FACE_OUTER_BOUND('',#1597,.T.) ;
#1089 = FACE_OUTER_BOUND('',#1598,.T.) ;
#1090 = FACE_OUTER_BOUND('',#1599,.T.) ;
#1091 = FACE_OUTER_BOUND('',#1600,.T.) ;
#1092 = FACE_OUTER_BOUND('',#1601,.T.) ;
#1093 = FACE_OUTER_BOUND('',#1602,.T.) ;
#1094 = FACE_OUTER_BOUND('',#1603,.T.) ;
#1095 = FACE_OUTER_BOUND('',#1604,.T.) ;
#1096 = FACE_OUTER_BOUND('',#1607,.T.) ;
#1097 = FACE_OUTER_BOUND('',#1610,.T.) ;
#1098 = FACE_OUTER_BOUND('',#1611,.T.) ;
#1099 = FACE_OUTER_BOUND('',#1613,.T.) ;
#1100 = FACE_OUTER_BOUND('',#1615,.T.) ;
#1101 = FACE_OUTER_BOUND('',#1616,.T.) ;
#1102 = FACE_OUTER_BOUND('',#1618,.T.) ;
#1103 = FACE_OUTER_BOUND('',#1620,.T.) ;
#1104 = FACE_OUTER_BOUND('',#1621,.T.) ;
#1105 = FACE_OUTER_BOUND('',#1622,.T.) ;
#1106 = FACE_OUTER_BOUND('',#1623,.T.) ;
#1107 = FACE_OUTER_BOUND('',#1624,.T.) ;
#1108 = FACE_OUTER_BOUND('',#1625,.T.) ;
#1109 = FACE_OUTER_BOUND('',#1626,.T.) ;
#1110 = FACE_OUTER_BOUND('',#1627,.T.) ;
#1111 = FACE_OUTER_BOUND('',#1628,.T.) ;
#1112 = FACE_OUTER_BOUND('',#1629,.T.) ;
#1113 = FACE_OUTER_BOUND('',#1630,.T.) ;
#1114 = FACE_OUTER_BOUND('',#1631,.T.) ;
#1115 = FACE_OUTER_BOUND('',#1632,.T.) ;
#1116 = FACE_OUTER_BOUND('',#1633,.T.) ;
#1117 = FACE_OUTER_BOUND('',#1634,.T.) ;
#1118 = FACE_OUTER_BOUND('',#1635,.T.) ;
#1119 = FACE_OUTER_BOUND('',#1636,.T.) ;
#1120 = FACE_OUTER_BOUND('',#1637,.T.) ;
#1121 = FACE_OUTER_BOUND('',#1638,.T.) ;
#1122 = FACE_OUTER_BOUND('',#1639,.T.) ;
#1123 = FACE_OUTER_BOUND('',#1640,.T.) ;
#1124 = FACE_OUTER_BOUND('',#1641,.T.) ;
#1125 = FACE_OUTER_BOUND('',#1642,.T.) ;
#1126 = FACE_OUTER_BOUND('',#1643,.T.) ;
#1127 = FACE_OUTER_BOUND('',#1644,.T.) ;
#1128 = FACE_OUTER_BOUND('',#1645,.T.) ;
#1129 = FACE_OUTER_BOUND('',#1646,.T.) ;
#1130 = FACE_OUTER_BOUND('',#1647,.T.) ;
#1131 = FACE_OUTER_BOUND('',#1648,.T.) ;
#1132 = FACE_OUTER_BOUND('',#1649,.T.) ;
#1133 = FACE_OUTER_BOUND('',#1650,.T.) ;
#1134 = FACE_OUTER_BOUND('',#1651,.T.) ;
#1135 = FACE_OUTER_BOUND('',#1652,.T.) ;
#1136 = FACE_OUTER_BOUND('',#1653,.T.) ;
#1137 = FACE_OUTER_BOUND('',#1654,.T.) ;
#1138 = FACE_OUTER_BOUND('',#1655,.T.) ;
#1139 = FACE_OUTER_BOUND('',#1656,.T.) ;
#1140 = FACE_OUTER_BOUND('',#1657,.T.) ;
#1141 = FACE_OUTER_BOUND('',#1658,.T.) ;
#1142 = FACE_OUTER_BOUND('',#1659,.T.) ;
#1143 = FACE_OUTER_BOUND('',#1660,.T.) ;
#1144 = FACE_OUTER_BOUND('',#1661,.T.) ;
#1145 = FACE_OUTER_BOUND('',#1662,.T.) ;
#1146 = FACE_OUTER_BOUND('',#1663,.T.) ;
#1147 = FACE_OUTER_BOUND('',#1664,.T.) ;
#1148 = FACE_OUTER_BOUND('',#1665,.T.) ;
#1149 = FACE_OUTER_BOUND('',#1666,.T.) ;
#1150 = FACE_OUTER_BOUND('',#1667,.T.) ;
#1151 = FACE_OUTER_BOUND('',#1668,.T.) ;
#1152 = FACE_OUTER_BOUND('',#1669,.T.) ;
#1153 = FACE_OUTER_BOUND('',#1670,.T.) ;
#1154 = FACE_OUTER_BOUND('',#1671,.T.) ;
#1155 = FACE_OUTER_BOUND('',#1672,.T.) ;
#1156 = FACE_OUTER_BOUND('',#1673,.T.) ;
#1157 = FACE_OUTER_BOUND('',#1674,.T.) ;
#1158 = FACE_OUTER_BOUND('',#1675,.T.) ;
#1159 = FACE_OUTER_BOUND('',#1676,.T.) ;
#1160 = FACE_OUTER_BOUND('',#1677,.T.) ;
#1161 = FACE_OUTER_BOUND('',#1678,.T.) ;
#1162 = FACE_OUTER_BOUND('',#1679,.T.) ;
#1163 = FACE_OUTER_BOUND('',#1680,.T.) ;
#1164 = FACE_OUTER_BOUND('',#1681,.T.) ;
#1165 = FACE_OUTER_BOUND('',#1682,.T.) ;
#1166 = FACE_OUTER_BOUND('',#1683,.T.) ;
#1167 = FACE_OUTER_BOUND('',#1684,.T.) ;
#1168 = FACE_OUTER_BOUND('',#1685,.T.) ;
#1169 = FACE_OUTER_BOUND('',#1686,.T.) ;
#1170 = FACE_OUTER_BOUND('',#1687,.T.) ;
#1171 = FACE_OUTER_BOUND('',#1688,.T.) ;
#1172 = FACE_OUTER_BOUND('',#1689,.T.) ;
#1173 = FACE_OUTER_BOUND('',#1690,.T.) ;
#1174 = FACE_OUTER_BOUND('',#1691,.T.) ;
#1175 = FACE_OUTER_BOUND('',#1692,.T.) ;
#1176 = FACE_OUTER_BOUND('',#1693,.T.) ;
#1177 = FACE_OUTER_BOUND('',#1694,.T.) ;
#1178 = FACE_OUTER_BOUND('',#1695,.T.) ;
#1179 = FACE_OUTER_BOUND('',#1696,.T.) ;
#1180 = FACE_OUTER_BOUND('',#1697,.T.) ;
#1181 = FACE_OUTER_BOUND('',#1698,.T.) ;
#1182 = FACE_OUTER_BOUND('',#1699,.T.) ;
#1183 = FACE_OUTER_BOUND('',#1700,.T.) ;
#1184 = FACE_OUTER_BOUND('',#1701,.T.) ;
#1185 = FACE_OUTER_BOUND('',#1702,.T.) ;
#1186 = FACE_OUTER_BOUND('',#1703,.T.) ;
#1187 = FACE_OUTER_BOUND('',#1704,.T.) ;
#1188 = FACE_OUTER_BOUND('',#1705,.T.) ;
#1189 = FACE_OUTER_BOUND('',#1706,.T.) ;
#1190 = FACE_OUTER_BOUND('',#1707,.T.) ;
#1191 = FACE_OUTER_BOUND('',#1708,.T.) ;
#1192 = FACE_OUTER_BOUND('',#1709,.T.) ;
#1193 = FACE_OUTER_BOUND('',#1710,.T.) ;
#1194 = FACE_OUTER_BOUND('',#1711,.T.) ;
#1195 = FACE_OUTER_BOUND('',#1712,.T.) ;
#1196 = FACE_OUTER_BOUND('',#1713,.T.) ;
#1197 = FACE_OUTER_BOUND('',#1714,.T.) ;
#1198 = FACE_OUTER_BOUND('',#1715,.T.) ;
#1199 = FACE_OUTER_BOUND('',#1716,.T.) ;
#1200 = FACE_OUTER_BOUND('',#1717,.T.) ;
#1201 = FACE_OUTER_BOUND('',#1718,.T.) ;
#1202 = FACE_OUTER_BOUND('',#1719,.T.) ;
#1203 = FACE_OUTER_BOUND('',#1720,.T.) ;
#1204 = FACE_OUTER_BOUND('',#1721,.T.) ;
#1205 = FACE_OUTER_BOUND('',#1722,.T.) ;
#1206 = FACE_OUTER_BOUND('',#1723,.T.) ;
#1207 = FACE_OUTER_BOUND('',#1724,.T.) ;
#1208 = FACE_OUTER_BOUND('',#1725,.T.) ;
#1209 = FACE_OUTER_BOUND('',#1726,.T.) ;
#1210 = FACE_OUTER_BOUND('',#1727,.T.) ;
#1211 = FACE_OUTER_BOUND('',#1728,.T.) ;
#1212 = FACE_OUTER_BOUND('',#1729,.T.) ;
#1213 = FACE_OUTER_BOUND('',#1730,.T.) ;
#1214 = FACE_OUTER_BOUND('',#1731,.T.) ;
#1215 = FACE_OUTER_BOUND('',#1732,.T.) ;
#1216 = FACE_OUTER_BOUND('',#1733,.T.) ;
#1217 = FACE_OUTER_BOUND('',#1734,.T.) ;
#1218 = FACE_OUTER_BOUND('',#1735,.T.) ;
#1219 = FACE_OUTER_BOUND('',#1736,.T.) ;
#1220 = FACE_OUTER_BOUND('',#1737,.T.) ;
#1221 = FACE_OUTER_BOUND('',#1738,.T.) ;
#1222 = FACE_OUTER_BOUND('',#1739,.T.) ;
#1223 = FACE_OUTER_BOUND('',#1740,.T.) ;
#1224 = FACE_OUTER_BOUND('',#1741,.T.) ;
#1225 = FACE_OUTER_BOUND('',#1742,.T.) ;
#1226 = FACE_OUTER_BOUND('',#1743,.T.) ;
#1227 = FACE_OUTER_BOUND('',#1744,.T.) ;
#1228 = FACE_OUTER_BOUND('',#1745,.T.) ;
#1229 = FACE_OUTER_BOUND('',#1746,.T.) ;
#1230 = FACE_OUTER_BOUND('',#1747,.T.) ;
#1231 = FACE_OUTER_BOUND('',#1748,.T.) ;
#1232 = FACE_OUTER_BOUND('',#1749,.T.) ;
#1233 = FACE_OUTER_BOUND('',#1750,.T.) ;
#1234 = FACE_OUTER_BOUND('',#1751,.T.) ;
#1235 = FACE_OUTER_BOUND('',#1752,.T.) ;
#1236 = FACE_OUTER_BOUND('',#1753,.T.) ;
#1237 = FACE_OUTER_BOUND('',#1754,.T.) ;
#1238 = FACE_OUTER_BOUND('',#1755,.T.) ;
#1239 = FACE_OUTER_BOUND('',#1756,.T.) ;
#1240 = FACE_OUTER_BOUND('',#1757,.T.) ;
#1241 = FACE_OUTER_BOUND('',#1758,.T.) ;
#1242 = FACE_OUTER_BOUND('',#1759,.T.) ;
#1243 = FACE_OUTER_BOUND('',#1760,.T.) ;
#1244 = FACE_OUTER_BOUND('',#1761,.T.) ;
#1245 = FACE_OUTER_BOUND('',#1762,.T.) ;
#1246 = FACE_OUTER_BOUND('',#1763,.T.) ;
#1247 = FACE_OUTER_BOUND('',#1764,.T.) ;
#1248 = FACE_OUTER_BOUND('',#1765,.T.) ;
#1249 = FACE_OUTER_BOUND('',#1766,.T.) ;
#1250 = FACE_OUTER_BOUND('',#1767,.T.) ;
#1251 = FACE_OUTER_BOUND('',#1768,.T.) ;
#1252 = FACE_OUTER_BOUND('',#1769,.T.) ;
#1253 = FACE_OUTER_BOUND('',#1770,.T.) ;
#1254 = FACE_OUTER_BOUND('',#1771,.T.) ;
#1255 = FACE_OUTER_BOUND('',#1772,.T.) ;
#1256 = FACE_OUTER_BOUND('',#1773,.T.) ;
#1257 = FACE_OUTER_BOUND('',#1774,.T.) ;
#1258 = FACE_OUTER_BOUND('',#1775,.T.) ;
#1259 = FACE_OUTER_BOUND('',#1776,.T.) ;
#1260 = FACE_OUTER_BOUND('',#1777,.T.) ;
#1261 = FACE_OUTER_BOUND('',#1778,.T.) ;
#1262 = FACE_OUTER_BOUND('',#1779,.T.) ;
#1263 = FACE_OUTER_BOUND('',#1780,.T.) ;
#1264 = FACE_OUTER_BOUND('',#1781,.T.) ;
#1265 = FACE_OUTER_BOUND('',#1782,.T.) ;
#1266 = FACE_OUTER_BOUND('',#1783,.T.) ;
#1267 = FACE_OUTER_BOUND('',#1784,.T.) ;
#1268 = FACE_OUTER_BOUND('',#1785,.T.) ;
#1269 = FACE_OUTER_BOUND('',#1786,.T.) ;
#1270 = FACE_OUTER_BOUND('',#1787,.T.) ;
#1271 = FACE_OUTER_BOUND('',#1788,.T.) ;
#1272 = FACE_OUTER_BOUND('',#1789,.T.) ;
#1273 = FACE_OUTER_BOUND('',#1790,.T.) ;
#1274 = FACE_OUTER_BOUND('',#1791,.T.) ;
#1275 = FACE_OUTER_BOUND('',#1792,.T.) ;
#1276 = FACE_OUTER_BOUND('',#1793,.T.) ;
#1277 = FACE_OUTER_BOUND('',#1794,.T.) ;
#1278 = FACE_OUTER_BOUND('',#1795,.T.) ;
#1279 = FACE_OUTER_BOUND('',#1796,.T.) ;
#1280 = FACE_OUTER_BOUND('',#1797,.T.) ;
#1281 = FACE_OUTER_BOUND('',#1798,.T.) ;
#1282 = FACE_OUTER_BOUND('',#1799,.T.) ;
#1283 = FACE_OUTER_BOUND('',#1800,.T.) ;
#1284 = FACE_OUTER_BOUND('',#1801,.T.) ;
#1285 = FACE_OUTER_BOUND('',#1802,.T.) ;
#1286 = FACE_OUTER_BOUND('',#1809,.T.) ;
#1287 = FACE_OUTER_BOUND('',#1811,.T.) ;
#1288 = FACE_OUTER_BOUND('',#1812,.T.) ;
#1289 = FACE_OUTER_BOUND('',#1813,.T.) ;
#1290 = FACE_OUTER_BOUND('',#1814,.T.) ;
#1291 = FACE_OUTER_BOUND('',#1815,.T.) ;
#1292 = FACE_OUTER_BOUND('',#1816,.T.) ;
#1293 = FACE_OUTER_BOUND('',#1817,.T.) ;
#1294 = FACE_OUTER_BOUND('',#1818,.T.) ;
#1295 = FACE_OUTER_BOUND('',#1819,.T.) ;
#1296 = FACE_OUTER_BOUND('',#1820,.T.) ;
#1297 = FACE_OUTER_BOUND('',#1821,.T.) ;
#1298 = FACE_OUTER_BOUND('',#1822,.T.) ;
#1299 = FACE_OUTER_BOUND('',#1823,.T.) ;
#1300 = FACE_OUTER_BOUND('',#1824,.T.) ;
#1301 = FACE_OUTER_BOUND('',#1825,.T.) ;
#1302 = FACE_OUTER_BOUND('',#1826,.T.) ;
#1303 = FACE_OUTER_BOUND('',#1827,.T.) ;
#1304 = FACE_OUTER_BOUND('',#1828,.T.) ;
#1305 = FACE_OUTER_BOUND('',#1829,.T.) ;
#1306 = FACE_OUTER_BOUND('',#1830,.T.) ;
#1307 = FACE_OUTER_BOUND('',#1831,.T.) ;
#1308 = FACE_OUTER_BOUND('',#1832,.T.) ;
#1309 = FACE_OUTER_BOUND('',#1833,.T.) ;
#1310 = FACE_OUTER_BOUND('',#1834,.T.) ;
#1311 = FACE_OUTER_BOUND('',#1835,.T.) ;
#1312 = FACE_OUTER_BOUND('',#1836,.T.) ;
#1313 = FACE_OUTER_BOUND('',#1837,.T.) ;
#1314 = FACE_OUTER_BOUND('',#1838,.T.) ;
#1315 = FACE_OUTER_BOUND('',#1839,.T.) ;
#1316 = FACE_OUTER_BOUND('',#1840,.T.) ;
#1317 = FACE_OUTER_BOUND('',#1841,.T.) ;
#1318 = FACE_OUTER_BOUND('',#1842,.T.) ;
#1319 = FACE_OUTER_BOUND('',#1843,.T.) ;
#1320 = FACE_OUTER_BOUND('',#1844,.T.) ;
#1321 = FACE_OUTER_BOUND('',#1845,.T.) ;
#1322 = FACE_OUTER_BOUND('',#1846,.T.) ;
#1323 = FACE_OUTER_BOUND('',#1847,.T.) ;
#1324 = FACE_OUTER_BOUND('',#1848,.T.) ;
#1325 = FACE_OUTER_BOUND('',#1849,.T.) ;
#1326 = FACE_OUTER_BOUND('',#1850,.T.) ;
#1327 = FACE_OUTER_BOUND('',#1851,.T.) ;
#1328 = FACE_OUTER_BOUND('',#1852,.T.) ;
#1329 = FACE_OUTER_BOUND('',#1853,.T.) ;
#1330 = FACE_OUTER_BOUND('',#1854,.T.) ;
#1331 = FACE_OUTER_BOUND('',#1856,.T.) ;
#1332 = EDGE_LOOP('',(#5568,#5569,#5570,#5571,#5572,#5573)) ;
#1333 = EDGE_LOOP('',(#5574,#5575,#5576,#5577,#5578,#5579)) ;
#1334 = EDGE_LOOP('',(#5580,#5581,#5582,#5583,#5584)) ;
#1335 = EDGE_LOOP('',(#5585,#5586,#5587,#5588,#5589)) ;
#1336 = EDGE_LOOP('',(#5590,#5591,#5592,#5593,#5594)) ;
#1337 = EDGE_LOOP('',(#5595,#5596,#5597,#5598,#5599)) ;
#1338 = EDGE_LOOP('',(#5600,#5601,#5602,#5603)) ;
#1339 = EDGE_LOOP('',(#5604)) ;
#1340 = EDGE_LOOP('',(#5605)) ;
#1341 = EDGE_LOOP('',(#5606)) ;
#1342 = EDGE_LOOP('',(#5607)) ;
#1343 = EDGE_LOOP('',(#5608)) ;
#1344 = EDGE_LOOP('',(#5609)) ;
#1345 = EDGE_LOOP('',(#5610,#5611,#5612,#5613)) ;
#1346 = EDGE_LOOP('',(#5614,#5615,#5616,#5617)) ;
#1347 = EDGE_LOOP('',(#5618,#5619,#5620,#5621,#5622,#5623)) ;
#1348 = EDGE_LOOP('',(#5624,#5625,#5626,#5627,#5628,#5629)) ;
#1349 = EDGE_LOOP('',(#5630,#5631,#5632,#5633,#5634,#5635)) ;
#1350 = EDGE_LOOP('',(#5636,#5637,#5638,#5639,#5640,#5641)) ;
#1351 = EDGE_LOOP('',(#5642,#5643,#5644,#5645)) ;
#1352 = EDGE_LOOP('',(#5646,#5647,#5648,#5649)) ;
#1353 = EDGE_LOOP('',(#5650,#5651,#5652,#5653)) ;
#1354 = EDGE_LOOP('',(#5654,#5655,#5656,#5657)) ;
#1355 = EDGE_LOOP('',(#5658,#5659,#5660,#5661)) ;
#1356 = EDGE_LOOP('',(#5662,#5663,#5664,#5665)) ;
#1357 = EDGE_LOOP('',(#5666,#5667,#5668,#5669)) ;
#1358 = EDGE_LOOP('',(#5670)) ;
#1359 = EDGE_LOOP('',(#5671)) ;
#1360 = EDGE_LOOP('',(#5672)) ;
#1361 = EDGE_LOOP('',(#5673)) ;
#1362 = EDGE_LOOP('',(#5674)) ;
#1363 = EDGE_LOOP('',(#5675,#5676,#5677)) ;
#1364 = EDGE_LOOP('',(#5678)) ;
#1365 = EDGE_LOOP('',(#5679,#5680,#5681)) ;
#1366 = EDGE_LOOP('',(#5682,#5683,#5684,#5685)) ;
#1367 = EDGE_LOOP('',(#5686,#5687,#5688,#5689)) ;
#1368 = EDGE_LOOP('',(#5690,#5691,#5692,#5693)) ;
#1369 = EDGE_LOOP('',(#5694,#5695,#5696,#5697)) ;
#1370 = EDGE_LOOP('',(#5698,#5699,#5700)) ;
#1371 = EDGE_LOOP('',(#5701,#5702,#5703)) ;
#1372 = EDGE_LOOP('',(#5704,#5705,#5706,#5707,#5708)) ;
#1373 = EDGE_LOOP('',(#5709,#5710,#5711,#5712)) ;
#1374 = EDGE_LOOP('',(#5713,#5714,#5715,#5716,#5717,#5718,#5719,#5720,#5721,
#5722,#5723,#5724)) ;
#1375 = EDGE_LOOP('',(#5725,#5726,#5727)) ;
#1376 = EDGE_LOOP('',(#5728,#5729,#5730,#5731,#5732,#5733)) ;
#1377 = EDGE_LOOP('',(#5734,#5735,#5736,#5737,#5738,#5739,#5740,#5741,#5742,
#5743,#5744,#5745,#5746)) ;
#1378 = EDGE_LOOP('',(#5747,#5748,#5749)) ;
#1379 = EDGE_LOOP('',(#5750,#5751,#5752,#5753,#5754,#5755,#5756,#5757,#5758,
#5759,#5760,#5761,#5762,#5763,#5764,#5765,#5766)) ;
#1380 = EDGE_LOOP('',(#5767,#5768,#5769)) ;
#1381 = EDGE_LOOP('',(#5770,#5771,#5772)) ;
#1382 = EDGE_LOOP('',(#5773,#5774,#5775,#5776,#5777)) ;
#1383 = EDGE_LOOP('',(#5778,#5779,#5780,#5781,#5782,#5783,#5784,#5785,#5786,
#5787,#5788)) ;
#1384 = EDGE_LOOP('',(#5789,#5790,#5791,#5792,#5793,#5794,#5795,#5796,#5797,
#5798,#5799,#5800,#5801)) ;
#1385 = EDGE_LOOP('',(#5802,#5803,#5804,#5805,#5806,#5807,#5808,#5809,#5810,
#5811,#5812,#5813,#5814,#5815,#5816,#5817)) ;
#1386 = EDGE_LOOP('',(#5818,#5819,#5820,#5821,#5822,#5823,#5824,#5825,#5826,
#5827)) ;
#1387 = EDGE_LOOP('',(#5828,#5829,#5830,#5831,#5832)) ;
#1388 = EDGE_LOOP('',(#5833,#5834,#5835,#5836,#5837,#5838,#5839,#5840,#5841,
#5842,#5843,#5844,#5845)) ;
#1389 = EDGE_LOOP('',(#5846,#5847,#5848,#5849,#5850)) ;
#1390 = EDGE_LOOP('',(#5851,#5852,#5853,#5854,#5855,#5856,#5857,#5858,#5859,
#5860)) ;
#1391 = EDGE_LOOP('',(#5861,#5862,#5863,#5864,#5865,#5866,#5867,#5868,#5869,
#5870,#5871,#5872,#5873)) ;
#1392 = EDGE_LOOP('',(#5874,#5875,#5876,#5877,#5878)) ;
#1393 = EDGE_LOOP('',(#5879,#5880,#5881,#5882,#5883)) ;
#1394 = EDGE_LOOP('',(#5884,#5885,#5886,#5887,#5888)) ;
#1395 = EDGE_LOOP('',(#5889)) ;
#1396 = EDGE_LOOP('',(#5890)) ;
#1397 = EDGE_LOOP('',(#5891,#5892,#5893,#5894,#5895)) ;
#1398 = EDGE_LOOP('',(#5896,#5897,#5898,#5899)) ;
#1399 = EDGE_LOOP('',(#5900)) ;
#1400 = EDGE_LOOP('',(#5901)) ;
#1401 = EDGE_LOOP('',(#5902,#5903,#5904,#5905)) ;
#1402 = EDGE_LOOP('',(#5906,#5907,#5908,#5909)) ;
#1403 = EDGE_LOOP('',(#5910,#5911,#5912,#5913)) ;
#1404 = EDGE_LOOP('',(#5914,#5915,#5916,#5917)) ;
#1405 = EDGE_LOOP('',(#5918,#5919,#5920,#5921)) ;
#1406 = EDGE_LOOP('',(#5922,#5923,#5924)) ;
#1407 = EDGE_LOOP('',(#5925,#5926,#5927,#5928,#5929,#5930,#5931)) ;
#1408 = EDGE_LOOP('',(#5932,#5933,#5934,#5935,#5936,#5937,#5938,#5939,#5940)) ;
#1409 = EDGE_LOOP('',(#5941,#5942,#5943,#5944,#5945,#5946,#5947,#5948,#5949)) ;
#1410 = EDGE_LOOP('',(#5950,#5951,#5952,#5953,#5954,#5955,#5956)) ;
#1411 = EDGE_LOOP('',(#5957)) ;
#1412 = EDGE_LOOP('',(#5958,#5959,#5960,#5961,#5962,#5963)) ;
#1413 = EDGE_LOOP('',(#5964,#5965,#5966,#5967)) ;
#1414 = EDGE_LOOP('',(#5968,#5969,#5970,#5971)) ;
#1415 = EDGE_LOOP('',(#5972,#5973,#5974,#5975)) ;
#1416 = EDGE_LOOP('',(#5976,#5977,#5978,#5979)) ;
#1417 = EDGE_LOOP('',(#5980,#5981,#5982,#5983)) ;
#1418 = EDGE_LOOP('',(#5984,#5985,#5986,#5987)) ;
#1419 = EDGE_LOOP('',(#5988,#5989,#5990,#5991,#5992,#5993)) ;
#1420 = EDGE_LOOP('',(#5994,#5995,#5996,#5997)) ;
#1421 = EDGE_LOOP('',(#5998,#5999,#6000,#6001)) ;
#1422 = EDGE_LOOP('',(#6002,#6003,#6004,#6005)) ;
#1423 = EDGE_LOOP('',(#6006,#6007,#6008,#6009)) ;
#1424 = EDGE_LOOP('',(#6010,#6011,#6012,#6013)) ;
#1425 = EDGE_LOOP('',(#6014,#6015,#6016)) ;
#1426 = EDGE_LOOP('',(#6017,#6018,#6019,#6020,#6021,#6022,#6023)) ;
#1427 = EDGE_LOOP('',(#6024,#6025,#6026,#6027,#6028,#6029,#6030,#6031,#6032)) ;
#1428 = EDGE_LOOP('',(#6033,#6034,#6035,#6036,#6037,#6038,#6039,#6040,#6041)) ;
#1429 = EDGE_LOOP('',(#6042,#6043,#6044,#6045,#6046,#6047,#6048)) ;
#1430 = EDGE_LOOP('',(#6049)) ;
#1431 = EDGE_LOOP('',(#6050,#6051,#6052,#6053,#6054,#6055)) ;
#1432 = EDGE_LOOP('',(#6056,#6057,#6058,#6059)) ;
#1433 = EDGE_LOOP('',(#6060,#6061,#6062,#6063)) ;
#1434 = EDGE_LOOP('',(#6064,#6065,#6066,#6067)) ;
#1435 = EDGE_LOOP('',(#6068,#6069,#6070,#6071)) ;
#1436 = EDGE_LOOP('',(#6072,#6073,#6074,#6075)) ;
#1437 = EDGE_LOOP('',(#6076,#6077,#6078,#6079)) ;
#1438 = EDGE_LOOP('',(#6080,#6081,#6082,#6083,#6084,#6085)) ;
#1439 = EDGE_LOOP('',(#6086,#6087,#6088,#6089)) ;
#1440 = EDGE_LOOP('',(#6090,#6091,#6092,#6093)) ;
#1441 = EDGE_LOOP('',(#6094,#6095,#6096,#6097)) ;
#1442 = EDGE_LOOP('',(#6098,#6099,#6100,#6101)) ;
#1443 = EDGE_LOOP('',(#6102,#6103,#6104,#6105)) ;
#1444 = EDGE_LOOP('',(#6106,#6107,#6108,#6109)) ;
#1445 = EDGE_LOOP('',(#6110)) ;
#1446 = EDGE_LOOP('',(#6111,#6112,#6113,#6114)) ;
#1447 = EDGE_LOOP('',(#6115)) ;
#1448 = EDGE_LOOP('',(#6116,#6117,#6118,#6119)) ;
#1449 = EDGE_LOOP('',(#6120)) ;
#1450 = EDGE_LOOP('',(#6121,#6122,#6123,#6124)) ;
#1451 = EDGE_LOOP('',(#6125)) ;
#1452 = EDGE_LOOP('',(#6126)) ;
#1453 = EDGE_LOOP('',(#6127,#6128,#6129,#6130)) ;
#1454 = EDGE_LOOP('',(#6131,#6132,#6133,#6134)) ;
#1455 = EDGE_LOOP('',(#6135)) ;
#1456 = EDGE_LOOP('',(#6136,#6137,#6138,#6139)) ;
#1457 = EDGE_LOOP('',(#6140,#6141,#6142,#6143)) ;
#1458 = EDGE_LOOP('',(#6144,#6145,#6146,#6147)) ;
#1459 = EDGE_LOOP('',(#6148,#6149,#6150,#6151)) ;
#1460 = EDGE_LOOP('',(#6152,#6153,#6154,#6155)) ;
#1461 = EDGE_LOOP('',(#6156,#6157,#6158,#6159)) ;
#1462 = EDGE_LOOP('',(#6160,#6161,#6162,#6163)) ;
#1463 = EDGE_LOOP('',(#6164,#6165,#6166,#6167)) ;
#1464 = EDGE_LOOP('',(#6168,#6169,#6170,#6171)) ;
#1465 = EDGE_LOOP('',(#6172,#6173,#6174,#6175)) ;
#1466 = EDGE_LOOP('',(#6176,#6177,#6178,#6179)) ;
#1467 = EDGE_LOOP('',(#6180,#6181,#6182,#6183)) ;
#1468 = EDGE_LOOP('',(#6184,#6185,#6186,#6187)) ;
#1469 = EDGE_LOOP('',(#6188,#6189,#6190,#6191)) ;
#1470 = EDGE_LOOP('',(#6192,#6193,#6194,#6195)) ;
#1471 = EDGE_LOOP('',(#6196,#6197,#6198,#6199)) ;
#1472 = EDGE_LOOP('',(#6200,#6201,#6202,#6203)) ;
#1473 = EDGE_LOOP('',(#6204,#6205,#6206,#6207)) ;
#1474 = EDGE_LOOP('',(#6208,#6209,#6210,#6211)) ;
#1475 = EDGE_LOOP('',(#6212,#6213,#6214,#6215)) ;
#1476 = EDGE_LOOP('',(#6216,#6217,#6218,#6219)) ;
#1477 = EDGE_LOOP('',(#6220,#6221,#6222,#6223)) ;
#1478 = EDGE_LOOP('',(#6224,#6225,#6226,#6227)) ;
#1479 = EDGE_LOOP('',(#6228,#6229,#6230,#6231)) ;
#1480 = EDGE_LOOP('',(#6232,#6233,#6234,#6235)) ;
#1481 = EDGE_LOOP('',(#6236)) ;
#1482 = EDGE_LOOP('',(#6237,#6238,#6239,#6240)) ;
#1483 = EDGE_LOOP('',(#6241)) ;
#1484 = EDGE_LOOP('',(#6242,#6243,#6244,#6245)) ;
#1485 = EDGE_LOOP('',(#6246)) ;
#1486 = EDGE_LOOP('',(#6247,#6248,#6249,#6250)) ;
#1487 = EDGE_LOOP('',(#6251)) ;
#1488 = EDGE_LOOP('',(#6252,#6253,#6254,#6255)) ;
#1489 = EDGE_LOOP('',(#6256)) ;
#1490 = EDGE_LOOP('',(#6257,#6258,#6259,#6260)) ;
#1491 = EDGE_LOOP('',(#6261)) ;
#1492 = EDGE_LOOP('',(#6262,#6263,#6264,#6265)) ;
#1493 = EDGE_LOOP('',(#6266,#6267,#6268,#6269)) ;
#1494 = EDGE_LOOP('',(#6270,#6271,#6272,#6273)) ;
#1495 = EDGE_LOOP('',(#6274,#6275,#6276,#6277)) ;
#1496 = EDGE_LOOP('',(#6278,#6279,#6280,#6281)) ;
#1497 = EDGE_LOOP('',(#6282,#6283,#6284,#6285)) ;
#1498 = EDGE_LOOP('',(#6286,#6287,#6288,#6289)) ;
#1499 = EDGE_LOOP('',(#6290,#6291,#6292,#6293)) ;
#1500 = EDGE_LOOP('',(#6294,#6295,#6296,#6297)) ;
#1501 = EDGE_LOOP('',(#6298,#6299,#6300,#6301)) ;
#1502 = EDGE_LOOP('',(#6302,#6303,#6304,#6305)) ;
#1503 = EDGE_LOOP('',(#6306,#6307,#6308,#6309)) ;
#1504 = EDGE_LOOP('',(#6310,#6311,#6312,#6313)) ;
#1505 = EDGE_LOOP('',(#6314,#6315,#6316,#6317)) ;
#1506 = EDGE_LOOP('',(#6318,#6319,#6320,#6321)) ;
#1507 = EDGE_LOOP('',(#6322,#6323,#6324,#6325)) ;
#1508 = EDGE_LOOP('',(#6326,#6327,#6328,#6329)) ;
#1509 = EDGE_LOOP('',(#6330,#6331,#6332,#6333)) ;
#1510 = EDGE_LOOP('',(#6334,#6335,#6336,#6337)) ;
#1511 = EDGE_LOOP('',(#6338,#6339,#6340,#6341)) ;
#1512 = EDGE_LOOP('',(#6342,#6343,#6344,#6345)) ;
#1513 = EDGE_LOOP('',(#6346,#6347,#6348,#6349)) ;
#1514 = EDGE_LOOP('',(#6350,#6351,#6352,#6353)) ;
#1515 = EDGE_LOOP('',(#6354)) ;
#1516 = EDGE_LOOP('',(#6355)) ;
#1517 = EDGE_LOOP('',(#6356,#6357,#6358,#6359)) ;
#1518 = EDGE_LOOP('',(#6360,#6361,#6362,#6363)) ;
#1519 = EDGE_LOOP('',(#6364,#6365,#6366,#6367)) ;
#1520 = EDGE_LOOP('',(#6368,#6369,#6370,#6371)) ;
#1521 = EDGE_LOOP('',(#6372,#6373,#6374,#6375)) ;
#1522 = EDGE_LOOP('',(#6376,#6377,#6378,#6379)) ;
#1523 = EDGE_LOOP('',(#6380,#6381,#6382,#6383)) ;
#1524 = EDGE_LOOP('',(#6384,#6385,#6386,#6387)) ;
#1525 = EDGE_LOOP('',(#6388,#6389,#6390,#6391)) ;
#1526 = EDGE_LOOP('',(#6392,#6393,#6394,#6395)) ;
#1527 = EDGE_LOOP('',(#6396,#6397,#6398,#6399)) ;
#1528 = EDGE_LOOP('',(#6400,#6401,#6402,#6403)) ;
#1529 = EDGE_LOOP('',(#6404,#6405,#6406,#6407)) ;
#1530 = EDGE_LOOP('',(#6408,#6409,#6410,#6411)) ;
#1531 = EDGE_LOOP('',(#6412,#6413,#6414,#6415,#6416,#6417,#6418,#6419,#6420,
#6421,#6422,#6423)) ;
#1532 = EDGE_LOOP('',(#6424)) ;
#1533 = EDGE_LOOP('',(#6425)) ;
#1534 = EDGE_LOOP('',(#6426,#6427,#6428,#6429,#6430,#6431,#6432,#6433,#6434,
#6435,#6436,#6437)) ;
#1535 = EDGE_LOOP('',(#6438)) ;
#1536 = EDGE_LOOP('',(#6439)) ;
#1537 = EDGE_LOOP('',(#6440,#6441,#6442,#6443)) ;
#1538 = EDGE_LOOP('',(#6444,#6445,#6446,#6447)) ;
#1539 = EDGE_LOOP('',(#6448,#6449,#6450)) ;
#1540 = EDGE_LOOP('',(#6451,#6452,#6453)) ;
#1541 = EDGE_LOOP('',(#6454,#6455,#6456,#6457)) ;
#1542 = EDGE_LOOP('',(#6458,#6459,#6460,#6461)) ;
#1543 = EDGE_LOOP('',(#6462,#6463,#6464,#6465)) ;
#1544 = EDGE_LOOP('',(#6466,#6467,#6468,#6469)) ;
#1545 = EDGE_LOOP('',(#6470,#6471,#6472)) ;
#1546 = EDGE_LOOP('',(#6473,#6474,#6475)) ;
#1547 = EDGE_LOOP('',(#6476,#6477,#6478,#6479)) ;
#1548 = EDGE_LOOP('',(#6480,#6481,#6482,#6483)) ;
#1549 = EDGE_LOOP('',(#6484,#6485,#6486,#6487)) ;
#1550 = EDGE_LOOP('',(#6488,#6489,#6490,#6491)) ;
#1551 = EDGE_LOOP('',(#6492)) ;
#1552 = EDGE_LOOP('',(#6493,#6494,#6495,#6496,#6497,#6498,#6499,#6500)) ;
#1553 = EDGE_LOOP('',(#6501,#6502,#6503,#6504,#6505,#6506)) ;
#1554 = EDGE_LOOP('',(#6507,#6508,#6509,#6510,#6511,#6512)) ;
#1555 = EDGE_LOOP('',(#6513,#6514,#6515,#6516,#6517,#6518)) ;
#1556 = EDGE_LOOP('',(#6519)) ;
#1557 = EDGE_LOOP('',(#6520,#6521,#6522,#6523,#6524,#6525,#6526,#6527)) ;
#1558 = EDGE_LOOP('',(#6528,#6529,#6530,#6531,#6532,#6533)) ;
#1559 = EDGE_LOOP('',(#6534,#6535,#6536,#6537,#6538,#6539)) ;
#1560 = EDGE_LOOP('',(#6540,#6541,#6542,#6543,#6544,#6545)) ;
#1561 = EDGE_LOOP('',(#6546,#6547,#6548)) ;
#1562 = EDGE_LOOP('',(#6549,#6550,#6551)) ;
#1563 = EDGE_LOOP('',(#6552,#6553,#6554)) ;
#1564 = EDGE_LOOP('',(#6555,#6556,#6557)) ;
#1565 = EDGE_LOOP('',(#6558,#6559,#6560,#6561)) ;
#1566 = EDGE_LOOP('',(#6562,#6563,#6564,#6565)) ;
#1567 = EDGE_LOOP('',(#6566,#6567,#6568,#6569)) ;
#1568 = EDGE_LOOP('',(#6570,#6571,#6572,#6573)) ;
#1569 = EDGE_LOOP('',(#6574,#6575,#6576)) ;
#1570 = EDGE_LOOP('',(#6577,#6578,#6579)) ;
#1571 = EDGE_LOOP('',(#6580,#6581,#6582,#6583)) ;
#1572 = EDGE_LOOP('',(#6584,#6585,#6586,#6587)) ;
#1573 = EDGE_LOOP('',(#6588,#6589,#6590,#6591)) ;
#1574 = EDGE_LOOP('',(#6592,#6593,#6594,#6595)) ;
#1575 = EDGE_LOOP('',(#6596)) ;
#1576 = EDGE_LOOP('',(#6597,#6598,#6599,#6600,#6601,#6602,#6603,#6604)) ;
#1577 = EDGE_LOOP('',(#6605,#6606,#6607,#6608,#6609,#6610)) ;
#1578 = EDGE_LOOP('',(#6611,#6612,#6613,#6614,#6615,#6616)) ;
#1579 = EDGE_LOOP('',(#6617,#6618,#6619,#6620,#6621,#6622)) ;
#1580 = EDGE_LOOP('',(#6623)) ;
#1581 = EDGE_LOOP('',(#6624,#6625,#6626,#6627,#6628,#6629,#6630,#6631)) ;
#1582 = EDGE_LOOP('',(#6632,#6633,#6634,#6635,#6636,#6637)) ;
#1583 = EDGE_LOOP('',(#6638,#6639,#6640,#6641,#6642,#6643)) ;
#1584 = EDGE_LOOP('',(#6644,#6645,#6646,#6647,#6648,#6649)) ;
#1585 = EDGE_LOOP('',(#6650,#6651,#6652)) ;
#1586 = EDGE_LOOP('',(#6653,#6654,#6655)) ;
#1587 = EDGE_LOOP('',(#6656,#6657,#6658,#6659)) ;
#1588 = EDGE_LOOP('',(#6660,#6661,#6662,#6663)) ;
#1589 = EDGE_LOOP('',(#6664,#6665,#6666,#6667)) ;
#1590 = EDGE_LOOP('',(#6668,#6669,#6670,#6671)) ;
#1591 = EDGE_LOOP('',(#6672,#6673,#6674,#6675)) ;
#1592 = EDGE_LOOP('',(#6676,#6677,#6678,#6679)) ;
#1593 = EDGE_LOOP('',(#6680,#6681,#6682,#6683)) ;
#1594 = EDGE_LOOP('',(#6684,#6685,#6686,#6687)) ;
#1595 = EDGE_LOOP('',(#6688,#6689,#6690,#6691)) ;
#1596 = EDGE_LOOP('',(#6692,#6693,#6694,#6695)) ;
#1597 = EDGE_LOOP('',(#6696,#6697,#6698,#6699)) ;
#1598 = EDGE_LOOP('',(#6700,#6701,#6702,#6703)) ;
#1599 = EDGE_LOOP('',(#6704,#6705,#6706,#6707)) ;
#1600 = EDGE_LOOP('',(#6708,#6709,#6710,#6711)) ;
#1601 = EDGE_LOOP('',(#6712,#6713,#6714,#6715)) ;
#1602 = EDGE_LOOP('',(#6716,#6717,#6718,#6719)) ;
#1603 = EDGE_LOOP('',(#6720,#6721,#6722,#6723)) ;
#1604 = EDGE_LOOP('',(#6724,#6725,#6726,#6727,#6728,#6729,#6730,#6731,#6732,
#6733,#6734,#6735,#6736,#6737,#6738)) ;
#1605 = EDGE_LOOP('',(#6739)) ;
#1606 = EDGE_LOOP('',(#6740)) ;
#1607 = EDGE_LOOP('',(#6741,#6742,#6743,#6744,#6745,#6746,#6747,#6748,#6749,
#6750,#6751,#6752,#6753,#6754,#6755)) ;
#1608 = EDGE_LOOP('',(#6756)) ;
#1609 = EDGE_LOOP('',(#6757)) ;
#1610 = EDGE_LOOP('',(#6758,#6759,#6760,#6761)) ;
#1611 = EDGE_LOOP('',(#6762)) ;
#1612 = EDGE_LOOP('',(#6763)) ;
#1613 = EDGE_LOOP('',(#6764)) ;
#1614 = EDGE_LOOP('',(#6765)) ;
#1615 = EDGE_LOOP('',(#6766,#6767,#6768,#6769)) ;
#1616 = EDGE_LOOP('',(#6770)) ;
#1617 = EDGE_LOOP('',(#6771)) ;
#1618 = EDGE_LOOP('',(#6772)) ;
#1619 = EDGE_LOOP('',(#6773)) ;
#1620 = EDGE_LOOP('',(#6774,#6775,#6776,#6777)) ;
#1621 = EDGE_LOOP('',(#6778,#6779,#6780,#6781)) ;
#1622 = EDGE_LOOP('',(#6782,#6783,#6784,#6785)) ;
#1623 = EDGE_LOOP('',(#6786,#6787,#6788,#6789)) ;
#1624 = EDGE_LOOP('',(#6790,#6791,#6792,#6793)) ;
#1625 = EDGE_LOOP('',(#6794,#6795,#6796,#6797)) ;
#1626 = EDGE_LOOP('',(#6798,#6799,#6800,#6801)) ;
#1627 = EDGE_LOOP('',(#6802,#6803,#6804,#6805)) ;
#1628 = EDGE_LOOP('',(#6806,#6807,#6808,#6809)) ;
#1629 = EDGE_LOOP('',(#6810,#6811,#6812,#6813)) ;
#1630 = EDGE_LOOP('',(#6814,#6815,#6816,#6817)) ;
#1631 = EDGE_LOOP('',(#6818,#6819,#6820,#6821)) ;
#1632 = EDGE_LOOP('',(#6822,#6823,#6824,#6825)) ;
#1633 = EDGE_LOOP('',(#6826,#6827,#6828,#6829)) ;
#1634 = EDGE_LOOP('',(#6830,#6831,#6832,#6833)) ;
#1635 = EDGE_LOOP('',(#6834,#6835,#6836,#6837)) ;
#1636 = EDGE_LOOP('',(#6838,#6839,#6840,#6841)) ;
#1637 = EDGE_LOOP('',(#6842,#6843,#6844,#6845)) ;
#1638 = EDGE_LOOP('',(#6846,#6847,#6848,#6849)) ;
#1639 = EDGE_LOOP('',(#6850,#6851,#6852,#6853)) ;
#1640 = EDGE_LOOP('',(#6854,#6855,#6856,#6857)) ;
#1641 = EDGE_LOOP('',(#6858,#6859,#6860,#6861)) ;
#1642 = EDGE_LOOP('',(#6862,#6863,#6864,#6865)) ;
#1643 = EDGE_LOOP('',(#6866,#6867,#6868,#6869)) ;
#1644 = EDGE_LOOP('',(#6870,#6871,#6872,#6873)) ;
#1645 = EDGE_LOOP('',(#6874,#6875,#6876,#6877)) ;
#1646 = EDGE_LOOP('',(#6878,#6879,#6880,#6881)) ;
#1647 = EDGE_LOOP('',(#6882,#6883,#6884,#6885)) ;
#1648 = EDGE_LOOP('',(#6886,#6887,#6888,#6889)) ;
#1649 = EDGE_LOOP('',(#6890,#6891,#6892,#6893)) ;
#1650 = EDGE_LOOP('',(#6894,#6895,#6896,#6897)) ;
#1651 = EDGE_LOOP('',(#6898,#6899,#6900,#6901)) ;
#1652 = EDGE_LOOP('',(#6902,#6903,#6904,#6905)) ;
#1653 = EDGE_LOOP('',(#6906,#6907,#6908,#6909)) ;
#1654 = EDGE_LOOP('',(#6910,#6911,#6912,#6913)) ;
#1655 = EDGE_LOOP('',(#6914,#6915,#6916,#6917)) ;
#1656 = EDGE_LOOP('',(#6918,#6919,#6920,#6921)) ;
#1657 = EDGE_LOOP('',(#6922,#6923,#6924,#6925)) ;
#1658 = EDGE_LOOP('',(#6926,#6927,#6928,#6929)) ;
#1659 = EDGE_LOOP('',(#6930,#6931,#6932,#6933)) ;
#1660 = EDGE_LOOP('',(#6934,#6935,#6936,#6937)) ;
#1661 = EDGE_LOOP('',(#6938,#6939,#6940,#6941)) ;
#1662 = EDGE_LOOP('',(#6942,#6943,#6944,#6945)) ;
#1663 = EDGE_LOOP('',(#6946,#6947,#6948,#6949)) ;
#1664 = EDGE_LOOP('',(#6950,#6951,#6952,#6953)) ;
#1665 = EDGE_LOOP('',(#6954,#6955,#6956,#6957)) ;
#1666 = EDGE_LOOP('',(#6958,#6959,#6960,#6961)) ;
#1667 = EDGE_LOOP('',(#6962,#6963,#6964,#6965)) ;
#1668 = EDGE_LOOP('',(#6966,#6967,#6968,#6969)) ;
#1669 = EDGE_LOOP('',(#6970,#6971,#6972,#6973)) ;
#1670 = EDGE_LOOP('',(#6974,#6975,#6976,#6977)) ;
#1671 = EDGE_LOOP('',(#6978,#6979,#6980,#6981)) ;
#1672 = EDGE_LOOP('',(#6982,#6983,#6984,#6985)) ;
#1673 = EDGE_LOOP('',(#6986,#6987,#6988,#6989)) ;
#1674 = EDGE_LOOP('',(#6990,#6991,#6992,#6993)) ;
#1675 = EDGE_LOOP('',(#6994,#6995,#6996,#6997)) ;
#1676 = EDGE_LOOP('',(#6998,#6999,#7000,#7001)) ;
#1677 = EDGE_LOOP('',(#7002,#7003,#7004,#7005)) ;
#1678 = EDGE_LOOP('',(#7006,#7007,#7008,#7009)) ;
#1679 = EDGE_LOOP('',(#7010,#7011,#7012,#7013)) ;
#1680 = EDGE_LOOP('',(#7014,#7015,#7016,#7017)) ;
#1681 = EDGE_LOOP('',(#7018,#7019,#7020,#7021)) ;
#1682 = EDGE_LOOP('',(#7022,#7023,#7024,#7025)) ;
#1683 = EDGE_LOOP('',(#7026,#7027,#7028,#7029)) ;
#1684 = EDGE_LOOP('',(#7030,#7031,#7032,#7033)) ;
#1685 = EDGE_LOOP('',(#7034,#7035,#7036,#7037)) ;
#1686 = EDGE_LOOP('',(#7038,#7039,#7040,#7041)) ;
#1687 = EDGE_LOOP('',(#7042,#7043,#7044,#7045)) ;
#1688 = EDGE_LOOP('',(#7046,#7047,#7048,#7049)) ;
#1689 = EDGE_LOOP('',(#7050,#7051,#7052,#7053)) ;
#1690 = EDGE_LOOP('',(#7054,#7055,#7056,#7057)) ;
#1691 = EDGE_LOOP('',(#7058,#7059,#7060,#7061)) ;
#1692 = EDGE_LOOP('',(#7062,#7063,#7064,#7065)) ;
#1693 = EDGE_LOOP('',(#7066,#7067,#7068,#7069)) ;
#1694 = EDGE_LOOP('',(#7070,#7071,#7072,#7073)) ;
#1695 = EDGE_LOOP('',(#7074,#7075,#7076,#7077)) ;
#1696 = EDGE_LOOP('',(#7078,#7079,#7080,#7081)) ;
#1697 = EDGE_LOOP('',(#7082,#7083,#7084,#7085)) ;
#1698 = EDGE_LOOP('',(#7086,#7087,#7088,#7089)) ;
#1699 = EDGE_LOOP('',(#7090,#7091,#7092,#7093)) ;
#1700 = EDGE_LOOP('',(#7094,#7095,#7096,#7097)) ;
#1701 = EDGE_LOOP('',(#7098,#7099,#7100,#7101)) ;
#1702 = EDGE_LOOP('',(#7102,#7103,#7104,#7105)) ;
#1703 = EDGE_LOOP('',(#7106,#7107,#7108,#7109)) ;
#1704 = EDGE_LOOP('',(#7110,#7111,#7112,#7113)) ;
#1705 = EDGE_LOOP('',(#7114,#7115,#7116,#7117)) ;
#1706 = EDGE_LOOP('',(#7118,#7119,#7120,#7121)) ;
#1707 = EDGE_LOOP('',(#7122,#7123,#7124,#7125)) ;
#1708 = EDGE_LOOP('',(#7126,#7127,#7128,#7129)) ;
#1709 = EDGE_LOOP('',(#7130,#7131,#7132,#7133)) ;
#1710 = EDGE_LOOP('',(#7134,#7135,#7136,#7137)) ;
#1711 = EDGE_LOOP('',(#7138,#7139,#7140,#7141)) ;
#1712 = EDGE_LOOP('',(#7142,#7143,#7144,#7145)) ;
#1713 = EDGE_LOOP('',(#7146,#7147,#7148,#7149)) ;
#1714 = EDGE_LOOP('',(#7150,#7151,#7152,#7153)) ;
#1715 = EDGE_LOOP('',(#7154,#7155,#7156,#7157)) ;
#1716 = EDGE_LOOP('',(#7158,#7159,#7160,#7161)) ;
#1717 = EDGE_LOOP('',(#7162,#7163,#7164,#7165)) ;
#1718 = EDGE_LOOP('',(#7166,#7167,#7168,#7169)) ;
#1719 = EDGE_LOOP('',(#7170,#7171,#7172,#7173)) ;
#1720 = EDGE_LOOP('',(#7174,#7175,#7176,#7177)) ;
#1721 = EDGE_LOOP('',(#7178,#7179,#7180,#7181)) ;
#1722 = EDGE_LOOP('',(#7182,#7183,#7184,#7185)) ;
#1723 = EDGE_LOOP('',(#7186,#7187,#7188,#7189)) ;
#1724 = EDGE_LOOP('',(#7190,#7191,#7192,#7193)) ;
#1725 = EDGE_LOOP('',(#7194,#7195,#7196,#7197)) ;
#1726 = EDGE_LOOP('',(#7198,#7199,#7200,#7201)) ;
#1727 = EDGE_LOOP('',(#7202,#7203,#7204,#7205)) ;
#1728 = EDGE_LOOP('',(#7206,#7207,#7208,#7209)) ;
#1729 = EDGE_LOOP('',(#7210,#7211,#7212,#7213)) ;
#1730 = EDGE_LOOP('',(#7214,#7215,#7216,#7217)) ;
#1731 = EDGE_LOOP('',(#7218,#7219,#7220,#7221)) ;
#1732 = EDGE_LOOP('',(#7222,#7223,#7224,#7225)) ;
#1733 = EDGE_LOOP('',(#7226,#7227,#7228,#7229)) ;
#1734 = EDGE_LOOP('',(#7230,#7231,#7232,#7233)) ;
#1735 = EDGE_LOOP('',(#7234,#7235,#7236,#7237)) ;
#1736 = EDGE_LOOP('',(#7238,#7239,#7240,#7241)) ;
#1737 = EDGE_LOOP('',(#7242,#7243,#7244,#7245)) ;
#1738 = EDGE_LOOP('',(#7246,#7247,#7248,#7249)) ;
#1739 = EDGE_LOOP('',(#7250,#7251,#7252,#7253)) ;
#1740 = EDGE_LOOP('',(#7254,#7255,#7256,#7257)) ;
#1741 = EDGE_LOOP('',(#7258,#7259,#7260,#7261)) ;
#1742 = EDGE_LOOP('',(#7262,#7263,#7264,#7265)) ;
#1743 = EDGE_LOOP('',(#7266,#7267,#7268,#7269)) ;
#1744 = EDGE_LOOP('',(#7270,#7271,#7272,#7273)) ;
#1745 = EDGE_LOOP('',(#7274,#7275,#7276,#7277)) ;
#1746 = EDGE_LOOP('',(#7278,#7279,#7280,#7281)) ;
#1747 = EDGE_LOOP('',(#7282,#7283,#7284,#7285)) ;
#1748 = EDGE_LOOP('',(#7286,#7287,#7288,#7289)) ;
#1749 = EDGE_LOOP('',(#7290,#7291,#7292,#7293)) ;
#1750 = EDGE_LOOP('',(#7294,#7295,#7296,#7297)) ;
#1751 = EDGE_LOOP('',(#7298,#7299,#7300,#7301)) ;
#1752 = EDGE_LOOP('',(#7302,#7303,#7304,#7305)) ;
#1753 = EDGE_LOOP('',(#7306,#7307,#7308,#7309)) ;
#1754 = EDGE_LOOP('',(#7310,#7311,#7312,#7313)) ;
#1755 = EDGE_LOOP('',(#7314,#7315,#7316,#7317)) ;
#1756 = EDGE_LOOP('',(#7318,#7319,#7320,#7321)) ;
#1757 = EDGE_LOOP('',(#7322,#7323,#7324,#7325)) ;
#1758 = EDGE_LOOP('',(#7326,#7327,#7328,#7329)) ;
#1759 = EDGE_LOOP('',(#7330,#7331,#7332,#7333)) ;
#1760 = EDGE_LOOP('',(#7334,#7335,#7336,#7337)) ;
#1761 = EDGE_LOOP('',(#7338,#7339,#7340,#7341)) ;
#1762 = EDGE_LOOP('',(#7342,#7343,#7344,#7345)) ;
#1763 = EDGE_LOOP('',(#7346,#7347,#7348,#7349)) ;
#1764 = EDGE_LOOP('',(#7350,#7351,#7352,#7353)) ;
#1765 = EDGE_LOOP('',(#7354,#7355,#7356,#7357)) ;
#1766 = EDGE_LOOP('',(#7358,#7359,#7360,#7361)) ;
#1767 = EDGE_LOOP('',(#7362,#7363,#7364,#7365)) ;
#1768 = EDGE_LOOP('',(#7366,#7367,#7368,#7369)) ;
#1769 = EDGE_LOOP('',(#7370,#7371,#7372,#7373)) ;
#1770 = EDGE_LOOP('',(#7374,#7375,#7376,#7377)) ;
#1771 = EDGE_LOOP('',(#7378,#7379,#7380,#7381)) ;
#1772 = EDGE_LOOP('',(#7382,#7383,#7384,#7385)) ;
#1773 = EDGE_LOOP('',(#7386,#7387,#7388,#7389)) ;
#1774 = EDGE_LOOP('',(#7390,#7391,#7392,#7393)) ;
#1775 = EDGE_LOOP('',(#7394,#7395,#7396,#7397)) ;
#1776 = EDGE_LOOP('',(#7398,#7399,#7400,#7401)) ;
#1777 = EDGE_LOOP('',(#7402,#7403,#7404,#7405)) ;
#1778 = EDGE_LOOP('',(#7406,#7407,#7408,#7409)) ;
#1779 = EDGE_LOOP('',(#7410,#7411,#7412,#7413)) ;
#1780 = EDGE_LOOP('',(#7414,#7415,#7416,#7417)) ;
#1781 = EDGE_LOOP('',(#7418,#7419,#7420,#7421)) ;
#1782 = EDGE_LOOP('',(#7422,#7423,#7424,#7425)) ;
#1783 = EDGE_LOOP('',(#7426,#7427,#7428,#7429)) ;
#1784 = EDGE_LOOP('',(#7430,#7431,#7432,#7433)) ;
#1785 = EDGE_LOOP('',(#7434,#7435,#7436,#7437)) ;
#1786 = EDGE_LOOP('',(#7438,#7439,#7440,#7441)) ;
#1787 = EDGE_LOOP('',(#7442,#7443,#7444,#7445)) ;
#1788 = EDGE_LOOP('',(#7446,#7447,#7448,#7449)) ;
#1789 = EDGE_LOOP('',(#7450,#7451,#7452,#7453)) ;
#1790 = EDGE_LOOP('',(#7454,#7455,#7456,#7457)) ;
#1791 = EDGE_LOOP('',(#7458,#7459,#7460,#7461)) ;
#1792 = EDGE_LOOP('',(#7462,#7463,#7464,#7465)) ;
#1793 = EDGE_LOOP('',(#7466,#7467,#7468,#7469)) ;
#1794 = EDGE_LOOP('',(#7470,#7471,#7472,#7473)) ;
#1795 = EDGE_LOOP('',(#7474,#7475,#7476,#7477)) ;
#1796 = EDGE_LOOP('',(#7478,#7479,#7480,#7481)) ;
#1797 = EDGE_LOOP('',(#7482,#7483,#7484,#7485)) ;
#1798 = EDGE_LOOP('',(#7486,#7487,#7488,#7489)) ;
#1799 = EDGE_LOOP('',(#7490,#7491,#7492,#7493)) ;
#1800 = EDGE_LOOP('',(#7494,#7495,#7496,#7497)) ;
#1801 = EDGE_LOOP('',(#7498,#7499,#7500,#7501)) ;
#1802 = EDGE_LOOP('',(#7502,#7503,#7504,#7505,#7506,#7507,#7508,#7509,#7510,
#7511,#7512,#7513,#7514,#7515,#7516,#7517,#7518,#7519,#7520,#7521,#7522,
#7523,#7524,#7525,#7526,#7527,#7528,#7529,#7530,#7531,#7532,#7533,#7534,
#7535,#7536,#7537,#7538,#7539,#7540,#7541,#7542,#7543,#7544,#7545,#7546,
#7547,#7548,#7549,#7550,#7551,#7552,#7553,#7554,#7555,#7556,#7557,#7558,
#7559,#7560,#7561,#7562,#7563,#7564,#7565,#7566,#7567,#7568,#7569,#7570,
#7571,#7572,#7573,#7574,#7575,#7576,#7577,#7578,#7579,#7580,#7581,#7582,
#7583,#7584,#7585,#7586,#7587,#7588,#7589,#7590,#7591,#7592,#7593,#7594,
#7595,#7596,#7597,#7598,#7599,#7600,#7601,#7602,#7603,#7604,#7605,#7606,
#7607,#7608,#7609,#7610,#7611,#7612,#7613,#7614,#7615,#7616,#7617,#7618,
#7619,#7620,#7621,#7622,#7623,#7624,#7625,#7626,#7627,#7628,#7629,#7630,
#7631,#7632,#7633,#7634,#7635,#7636,#7637,#7638,#7639,#7640,#7641,#7642,
#7643,#7644,#7645,#7646,#7647,#7648,#7649,#7650,#7651,#7652,#7653,#7654,
#7655,#7656,#7657,#7658,#7659,#7660,#7661,#7662,#7663,#7664,#7665,#7666,
#7667,#7668,#7669,#7670,#7671,#7672,#7673,#7674,#7675,#7676,#7677,#7678,
#7679,#7680,#7681)) ;
#1803 = EDGE_LOOP('',(#7682,#7683,#7684,#7685,#7686,#7687,#7688,#7689)) ;
#1804 = EDGE_LOOP('',(#7690)) ;
#1805 = EDGE_LOOP('',(#7691,#7692,#7693,#7694,#7695,#7696,#7697,#7698)) ;
#1806 = EDGE_LOOP('',(#7699,#7700,#7701,#7702,#7703,#7704,#7705,#7706)) ;
#1807 = EDGE_LOOP('',(#7707,#7708,#7709,#7710,#7711,#7712,#7713,#7714)) ;
#1808 = EDGE_LOOP('',(#7715,#7716,#7717,#7718,#7719,#7720,#7721,#7722)) ;
#1809 = EDGE_LOOP('',(#7723,#7724,#7725,#7726,#7727,#7728,#7729,#7730,#7731,
#7732,#7733,#7734,#7735,#7736,#7737,#7738,#7739,#7740,#7741,#7742,#7743,
#7744,#7745,#7746,#7747,#7748,#7749,#7750,#7751,#7752,#7753,#7754,#7755,
#7756,#7757,#7758,#7759,#7760,#7761,#7762,#7763,#7764,#7765,#7766,#7767,
#7768,#7769,#7770,#7771,#7772,#7773,#7774,#7775,#7776,#7777,#7778,#7779,
#7780,#7781,#7782,#7783,#7784,#7785,#7786,#7787,#7788,#7789,#7790,#7791,
#7792,#7793,#7794,#7795,#7796,#7797,#7798,#7799,#7800,#7801,#7802,#7803,
#7804,#7805,#7806,#7807,#7808,#7809,#7810,#7811,#7812,#7813,#7814,#7815,
#7816,#7817,#7818,#7819,#7820,#7821,#7822,#7823,#7824,#7825,#7826,#7827,
#7828,#7829,#7830,#7831,#7832,#7833,#7834,#7835,#7836,#7837,#7838,#7839,
#7840,#7841,#7842,#7843,#7844,#7845,#7846,#7847,#7848,#7849,#7850,#7851,
#7852,#7853,#7854,#7855,#7856,#7857,#7858,#7859,#7860,#7861,#7862,#7863,
#7864,#7865,#7866,#7867,#7868,#7869,#7870,#7871,#7872,#7873,#7874,#7875,
#7876,#7877,#7878,#7879,#7880,#7881,#7882,#7883,#7884,#7885,#7886,#7887,
#7888,#7889,#7890,#7891,#7892,#7893,#7894,#7895,#7896,#7897,#7898,#7899,
#7900,#7901,#7902)) ;
#1810 = EDGE_LOOP('',(#7903)) ;
#1811 = EDGE_LOOP('',(#7904,#7905,#7906,#7907)) ;
#1812 = EDGE_LOOP('',(#7908,#7909,#7910,#7911)) ;
#1813 = EDGE_LOOP('',(#7912,#7913,#7914,#7915)) ;
#1814 = EDGE_LOOP('',(#7916,#7917,#7918,#7919)) ;
#1815 = EDGE_LOOP('',(#7920,#7921,#7922,#7923)) ;
#1816 = EDGE_LOOP('',(#7924,#7925,#7926,#7927)) ;
#1817 = EDGE_LOOP('',(#7928,#7929,#7930,#7931)) ;
#1818 = EDGE_LOOP('',(#7932,#7933,#7934,#7935)) ;
#1819 = EDGE_LOOP('',(#7936,#7937,#7938,#7939)) ;
#1820 = EDGE_LOOP('',(#7940,#7941,#7942,#7943)) ;
#1821 = EDGE_LOOP('',(#7944,#7945,#7946,#7947)) ;
#1822 = EDGE_LOOP('',(#7948,#7949,#7950,#7951)) ;
#1823 = EDGE_LOOP('',(#7952,#7953,#7954,#7955)) ;
#1824 = EDGE_LOOP('',(#7956,#7957,#7958,#7959)) ;
#1825 = EDGE_LOOP('',(#7960,#7961,#7962,#7963)) ;
#1826 = EDGE_LOOP('',(#7964,#7965,#7966,#7967)) ;
#1827 = EDGE_LOOP('',(#7968,#7969,#7970,#7971)) ;
#1828 = EDGE_LOOP('',(#7972,#7973,#7974,#7975)) ;
#1829 = EDGE_LOOP('',(#7976,#7977,#7978,#7979)) ;
#1830 = EDGE_LOOP('',(#7980,#7981,#7982,#7983)) ;
#1831 = EDGE_LOOP('',(#7984,#7985,#7986,#7987)) ;
#1832 = EDGE_LOOP('',(#7988,#7989,#7990,#7991)) ;
#1833 = EDGE_LOOP('',(#7992,#7993,#7994,#7995)) ;
#1834 = EDGE_LOOP('',(#7996,#7997,#7998,#7999)) ;
#1835 = EDGE_LOOP('',(#8000,#8001,#8002,#8003)) ;
#1836 = EDGE_LOOP('',(#8004,#8005,#8006,#8007)) ;
#1837 = EDGE_LOOP('',(#8008,#8009,#8010,#8011)) ;
#1838 = EDGE_LOOP('',(#8012,#8013,#8014,#8015)) ;
#1839 = EDGE_LOOP('',(#8016,#8017,#8018,#8019)) ;
#1840 = EDGE_LOOP('',(#8020,#8021,#8022,#8023)) ;
#1841 = EDGE_LOOP('',(#8024,#8025,#8026,#8027)) ;
#1842 = EDGE_LOOP('',(#8028,#8029,#8030,#8031)) ;
#1843 = EDGE_LOOP('',(#8032,#8033,#8034,#8035)) ;
#1844 = EDGE_LOOP('',(#8036,#8037,#8038,#8039)) ;
#1845 = EDGE_LOOP('',(#8040,#8041,#8042,#8043)) ;
#1846 = EDGE_LOOP('',(#8044,#8045,#8046,#8047)) ;
#1847 = EDGE_LOOP('',(#8048,#8049,#8050,#8051)) ;
#1848 = EDGE_LOOP('',(#8052,#8053,#8054,#8055)) ;
#1849 = EDGE_LOOP('',(#8056,#8057,#8058,#8059)) ;
#1850 = EDGE_LOOP('',(#8060,#8061,#8062,#8063)) ;
#1851 = EDGE_LOOP('',(#8064,#8065,#8066,#8067)) ;
#1852 = EDGE_LOOP('',(#8068,#8069,#8070,#8071)) ;
#1853 = EDGE_LOOP('',(#8072,#8073,#8074,#8075)) ;
#1854 = EDGE_LOOP('',(#8076)) ;
#1855 = EDGE_LOOP('',(#8077)) ;
#1856 = EDGE_LOOP('',(#8078)) ;
#1857 = EDGE_LOOP('',(#8079,#8080,#8081,#8082,#8083,#8084,#8085,#8086)) ;
#1858 = EDGE_LOOP('',(#8087)) ;
#1859 = EDGE_LOOP('',(#8088,#8089,#8090,#8091,#8092,#8093,#8094,#8095)) ;
#1860 = EDGE_LOOP('',(#8096,#8097,#8098,#8099,#8100,#8101,#8102,#8103)) ;
#1861 = EDGE_LOOP('',(#8104,#8105,#8106,#8107,#8108,#8109,#8110,#8111)) ;
#1862 = EDGE_LOOP('',(#8112,#8113,#8114,#8115,#8116,#8117,#8118,#8119)) ;
#1863 = LINE('',#11652,#2566) ;
#1864 = LINE('',#11926,#2567) ;
#1865 = LINE('',#12157,#2568) ;
#1866 = LINE('',#12204,#2569) ;
#1867 = LINE('',#12251,#2570) ;
#1868 = LINE('',#12298,#2571) ;
#1869 = LINE('',#12318,#2572) ;
#1870 = LINE('',#12400,#2573) ;
#1871 = LINE('',#12439,#2574) ;
#1872 = LINE('',#12443,#2575) ;
#1873 = LINE('',#12710,#2576) ;
#1874 = LINE('',#12984,#2577) ;
#1875 = LINE('',#13955,#2578) ;
#1876 = LINE('',#15019,#2579) ;
#1877 = LINE('',#15157,#2580) ;
#1878 = LINE('',#15764,#2581) ;
#1879 = LINE('',#16034,#2582) ;
#1880 = LINE('',#16289,#2583) ;
#1881 = LINE('',#17911,#2584) ;
#1882 = LINE('',#18440,#2585) ;
#1883 = LINE('',#18926,#2586) ;
#1884 = LINE('',#18965,#2587) ;
#1885 = LINE('',#18969,#2588) ;
#1886 = LINE('',#18978,#2589) ;
#1887 = LINE('',#33347,#2590) ;
#1888 = LINE('',#33351,#2591) ;
#1889 = LINE('',#41430,#2592) ;
#1890 = LINE('',#43252,#2593) ;
#1891 = LINE('',#64560,#2594) ;
#1892 = LINE('',#64562,#2595) ;
#1893 = LINE('',#64563,#2596) ;
#1894 = LINE('',#71962,#2597) ;
#1895 = LINE('',#79048,#2598) ;
#1896 = LINE('',#79091,#2599) ;
#1897 = LINE('',#79094,#2600) ;
#1898 = LINE('',#79147,#2601) ;
#1899 = LINE('',#79150,#2602) ;
#1900 = LINE('',#79183,#2603) ;
#1901 = LINE('',#79226,#2604) ;
#1902 = LINE('',#79259,#2605) ;
#1903 = LINE('',#79264,#2606) ;
#1904 = LINE('',#79304,#2607) ;
#1905 = LINE('',#79309,#2608) ;
#1906 = LINE('',#79316,#2609) ;
#1907 = LINE('',#79633,#2610) ;
#1908 = LINE('',#80089,#2611) ;
#1909 = LINE('',#80536,#2612) ;
#1910 = LINE('',#81518,#2613) ;
#1911 = LINE('',#81591,#2614) ;
#1912 = LINE('',#95701,#2615) ;
#1913 = LINE('',#95705,#2616) ;
#1914 = LINE('',#95707,#2617) ;
#1915 = LINE('',#95709,#2618) ;
#1916 = LINE('',#95711,#2619) ;
#1917 = LINE('',#95713,#2620) ;
#1918 = LINE('',#95714,#2621) ;
#1919 = LINE('',#95717,#2622) ;
#1920 = LINE('',#95719,#2623) ;
#1921 = LINE('',#95720,#2624) ;
#1922 = LINE('',#95723,#2625) ;
#1923 = LINE('',#95724,#2626) ;
#1924 = LINE('',#95727,#2627) ;
#1925 = LINE('',#95728,#2628) ;
#1926 = LINE('',#95731,#2629) ;
#1927 = LINE('',#95732,#2630) ;
#1928 = LINE('',#95735,#2631) ;
#1929 = LINE('',#95736,#2632) ;
#1930 = LINE('',#95738,#2633) ;
#1931 = LINE('',#95743,#2634) ;
#1932 = LINE('',#96060,#2635) ;
#1933 = LINE('',#97232,#2636) ;
#1934 = LINE('',#97679,#2637) ;
#1935 = LINE('',#98660,#2638) ;
#1936 = LINE('',#98663,#2639) ;
#1937 = LINE('',#112841,#2640) ;
#1938 = LINE('',#112846,#2641) ;
#1939 = LINE('',#112848,#2642) ;
#1940 = LINE('',#112850,#2643) ;
#1941 = LINE('',#112852,#2644) ;
#1942 = LINE('',#112854,#2645) ;
#1943 = LINE('',#112855,#2646) ;
#1944 = LINE('',#112858,#2647) ;
#1945 = LINE('',#112860,#2648) ;
#1946 = LINE('',#112861,#2649) ;
#1947 = LINE('',#112864,#2650) ;
#1948 = LINE('',#112865,#2651) ;
#1949 = LINE('',#112868,#2652) ;
#1950 = LINE('',#112869,#2653) ;
#1951 = LINE('',#112872,#2654) ;
#1952 = LINE('',#112873,#2655) ;
#1953 = LINE('',#112876,#2656) ;
#1954 = LINE('',#112877,#2657) ;
#1955 = LINE('',#112879,#2658) ;
#1956 = LINE('',#112886,#2659) ;
#1957 = LINE('',#112889,#2660) ;
#1958 = LINE('',#112894,#2661) ;
#1959 = LINE('',#112900,#2662) ;
#1960 = LINE('',#112909,#2663) ;
#1961 = LINE('',#113041,#2664) ;
#1962 = LINE('',#113044,#2665) ;
#1963 = LINE('',#113046,#2666) ;
#1964 = LINE('',#113060,#2667) ;
#1965 = LINE('',#113064,#2668) ;
#1966 = LINE('',#113086,#2669) ;
#1967 = LINE('',#113089,#2670) ;
#1968 = LINE('',#113091,#2671) ;
#1969 = LINE('',#113100,#2672) ;
#1970 = LINE('',#113104,#2673) ;
#1971 = LINE('',#113154,#2674) ;
#1972 = LINE('',#113177,#2675) ;
#1973 = LINE('',#113178,#2676) ;
#1974 = LINE('',#113187,#2677) ;
#1975 = LINE('',#113210,#2678) ;
#1976 = LINE('',#113257,#2679) ;
#1977 = LINE('',#113266,#2680) ;
#1978 = LINE('',#113267,#2681) ;
#1979 = LINE('',#113286,#2682) ;
#1980 = LINE('',#113295,#2683) ;
#1981 = LINE('',#113319,#2684) ;
#1982 = LINE('',#113322,#2685) ;
#1983 = LINE('',#113327,#2686) ;
#1984 = LINE('',#113333,#2687) ;
#1985 = LINE('',#113469,#2688) ;
#1986 = LINE('',#113472,#2689) ;
#1987 = LINE('',#113474,#2690) ;
#1988 = LINE('',#113488,#2691) ;
#1989 = LINE('',#113492,#2692) ;
#1990 = LINE('',#113514,#2693) ;
#1991 = LINE('',#113517,#2694) ;
#1992 = LINE('',#113519,#2695) ;
#1993 = LINE('',#113528,#2696) ;
#1994 = LINE('',#113540,#2697) ;
#1995 = LINE('',#113565,#2698) ;
#1996 = LINE('',#113604,#2699) ;
#1997 = LINE('',#113627,#2700) ;
#1998 = LINE('',#113628,#2701) ;
#1999 = LINE('',#113637,#2702) ;
#2000 = LINE('',#113660,#2703) ;
#2001 = LINE('',#113707,#2704) ;
#2002 = LINE('',#113716,#2705) ;
#2003 = LINE('',#113717,#2706) ;
#2004 = LINE('',#113736,#2707) ;
#2005 = LINE('',#113745,#2708) ;
#2006 = LINE('',#113786,#2709) ;
#2007 = LINE('',#113791,#2710) ;
#2008 = LINE('',#113873,#2711) ;
#2009 = LINE('',#113912,#2712) ;
#2010 = LINE('',#113918,#2713) ;
#2011 = LINE('',#113921,#2714) ;
#2012 = LINE('',#113924,#2715) ;
#2013 = LINE('',#113926,#2716) ;
#2014 = LINE('',#113927,#2717) ;
#2015 = LINE('',#113932,#2718) ;
#2016 = LINE('',#113938,#2719) ;
#2017 = LINE('',#113942,#2720) ;
#2018 = LINE('',#113944,#2721) ;
#2019 = LINE('',#113945,#2722) ;
#2020 = LINE('',#113948,#2723) ;
#2021 = LINE('',#113950,#2724) ;
#2022 = LINE('',#113951,#2725) ;
#2023 = LINE('',#113956,#2726) ;
#2024 = LINE('',#113960,#2727) ;
#2025 = LINE('',#113962,#2728) ;
#2026 = LINE('',#113963,#2729) ;
#2027 = LINE('',#113968,#2730) ;
#2028 = LINE('',#113974,#2731) ;
#2029 = LINE('',#113978,#2732) ;
#2030 = LINE('',#113980,#2733) ;
#2031 = LINE('',#113981,#2734) ;
#2032 = LINE('',#113996,#2735) ;
#2033 = LINE('',#113998,#2736) ;
#2034 = LINE('',#114002,#2737) ;
#2035 = LINE('',#114055,#2738) ;
#2036 = LINE('',#114168,#2739) ;
#2037 = LINE('',#114187,#2740) ;
#2038 = LINE('',#114192,#2741) ;
#2039 = LINE('',#114243,#2742) ;
#2040 = LINE('',#114356,#2743) ;
#2041 = LINE('',#114376,#2744) ;
#2042 = LINE('',#134170,#2745) ;
#2043 = LINE('',#154157,#2746) ;
#2044 = LINE('',#154359,#2747) ;
#2045 = LINE('',#154410,#2748) ;
#2046 = LINE('',#154523,#2749) ;
#2047 = LINE('',#154543,#2750) ;
#2048 = LINE('',#154547,#2751) ;
#2049 = LINE('',#154600,#2752) ;
#2050 = LINE('',#154713,#2753) ;
#2051 = LINE('',#154732,#2754) ;
#2052 = LINE('',#174526,#2755) ;
#2053 = LINE('',#194513,#2756) ;
#2054 = LINE('',#194714,#2757) ;
#2055 = LINE('',#194716,#2758) ;
#2056 = LINE('',#194718,#2759) ;
#2057 = LINE('',#194719,#2760) ;
#2058 = LINE('',#194729,#2761) ;
#2059 = LINE('',#194735,#2762) ;
#2060 = LINE('',#194741,#2763) ;
#2061 = LINE('',#194747,#2764) ;
#2062 = LINE('',#194753,#2765) ;
#2063 = LINE('',#194759,#2766) ;
#2064 = LINE('',#194763,#2767) ;
#2065 = LINE('',#194765,#2768) ;
#2066 = LINE('',#194766,#2769) ;
#2067 = LINE('',#194771,#2770) ;
#2068 = LINE('',#194775,#2771) ;
#2069 = LINE('',#194777,#2772) ;
#2070 = LINE('',#194778,#2773) ;
#2071 = LINE('',#194783,#2774) ;
#2072 = LINE('',#194789,#2775) ;
#2073 = LINE('',#194795,#2776) ;
#2074 = LINE('',#194806,#2777) ;
#2075 = LINE('',#194809,#2778) ;
#2076 = LINE('',#194810,#2779) ;
#2077 = LINE('',#194815,#2780) ;
#2078 = LINE('',#194821,#2781) ;
#2079 = LINE('',#194829,#2782) ;
#2080 = LINE('',#194843,#2783) ;
#2081 = LINE('',#194850,#2784) ;
#2082 = LINE('',#194852,#2785) ;
#2083 = LINE('',#194856,#2786) ;
#2084 = LINE('',#194858,#2787) ;
#2085 = LINE('',#194860,#2788) ;
#2086 = LINE('',#194861,#2789) ;
#2087 = LINE('',#194875,#2790) ;
#2088 = LINE('',#194879,#2791) ;
#2089 = LINE('',#194881,#2792) ;
#2090 = LINE('',#194882,#2793) ;
#2091 = LINE('',#194885,#2794) ;
#2092 = LINE('',#194887,#2795) ;
#2093 = LINE('',#194888,#2796) ;
#2094 = LINE('',#194902,#2797) ;
#2095 = LINE('',#194906,#2798) ;
#2096 = LINE('',#194908,#2799) ;
#2097 = LINE('',#194909,#2800) ;
#2098 = LINE('',#194912,#2801) ;
#2099 = LINE('',#194914,#2802) ;
#2100 = LINE('',#194915,#2803) ;
#2101 = LINE('',#194929,#2804) ;
#2102 = LINE('',#194933,#2805) ;
#2103 = LINE('',#194935,#2806) ;
#2104 = LINE('',#194936,#2807) ;
#2105 = LINE('',#194939,#2808) ;
#2106 = LINE('',#194941,#2809) ;
#2107 = LINE('',#194942,#2810) ;
#2108 = LINE('',#194956,#2811) ;
#2109 = LINE('',#194960,#2812) ;
#2110 = LINE('',#194962,#2813) ;
#2111 = LINE('',#194963,#2814) ;
#2112 = LINE('',#194966,#2815) ;
#2113 = LINE('',#194968,#2816) ;
#2114 = LINE('',#194969,#2817) ;
#2115 = LINE('',#194983,#2818) ;
#2116 = LINE('',#194987,#2819) ;
#2117 = LINE('',#194989,#2820) ;
#2118 = LINE('',#194990,#2821) ;
#2119 = LINE('',#194993,#2822) ;
#2120 = LINE('',#194995,#2823) ;
#2121 = LINE('',#194996,#2824) ;
#2122 = LINE('',#195010,#2825) ;
#2123 = LINE('',#195014,#2826) ;
#2124 = LINE('',#195016,#2827) ;
#2125 = LINE('',#195017,#2828) ;
#2126 = LINE('',#195020,#2829) ;
#2127 = LINE('',#195022,#2830) ;
#2128 = LINE('',#195023,#2831) ;
#2129 = LINE('',#195037,#2832) ;
#2130 = LINE('',#195041,#2833) ;
#2131 = LINE('',#195043,#2834) ;
#2132 = LINE('',#195044,#2835) ;
#2133 = LINE('',#195047,#2836) ;
#2134 = LINE('',#195049,#2837) ;
#2135 = LINE('',#195050,#2838) ;
#2136 = LINE('',#195064,#2839) ;
#2137 = LINE('',#195068,#2840) ;
#2138 = LINE('',#195070,#2841) ;
#2139 = LINE('',#195071,#2842) ;
#2140 = LINE('',#195074,#2843) ;
#2141 = LINE('',#195076,#2844) ;
#2142 = LINE('',#195077,#2845) ;
#2143 = LINE('',#195091,#2846) ;
#2144 = LINE('',#195095,#2847) ;
#2145 = LINE('',#195097,#2848) ;
#2146 = LINE('',#195098,#2849) ;
#2147 = LINE('',#195101,#2850) ;
#2148 = LINE('',#195103,#2851) ;
#2149 = LINE('',#195104,#2852) ;
#2150 = LINE('',#195118,#2853) ;
#2151 = LINE('',#195122,#2854) ;
#2152 = LINE('',#195124,#2855) ;
#2153 = LINE('',#195125,#2856) ;
#2154 = LINE('',#195128,#2857) ;
#2155 = LINE('',#195130,#2858) ;
#2156 = LINE('',#195131,#2859) ;
#2157 = LINE('',#195145,#2860) ;
#2158 = LINE('',#195149,#2861) ;
#2159 = LINE('',#195151,#2862) ;
#2160 = LINE('',#195152,#2863) ;
#2161 = LINE('',#195155,#2864) ;
#2162 = LINE('',#195157,#2865) ;
#2163 = LINE('',#195158,#2866) ;
#2164 = LINE('',#195172,#2867) ;
#2165 = LINE('',#195176,#2868) ;
#2166 = LINE('',#195178,#2869) ;
#2167 = LINE('',#195179,#2870) ;
#2168 = LINE('',#195182,#2871) ;
#2169 = LINE('',#195184,#2872) ;
#2170 = LINE('',#195185,#2873) ;
#2171 = LINE('',#195199,#2874) ;
#2172 = LINE('',#195203,#2875) ;
#2173 = LINE('',#195205,#2876) ;
#2174 = LINE('',#195206,#2877) ;
#2175 = LINE('',#195209,#2878) ;
#2176 = LINE('',#195211,#2879) ;
#2177 = LINE('',#195212,#2880) ;
#2178 = LINE('',#195226,#2881) ;
#2179 = LINE('',#195230,#2882) ;
#2180 = LINE('',#195232,#2883) ;
#2181 = LINE('',#195233,#2884) ;
#2182 = LINE('',#195236,#2885) ;
#2183 = LINE('',#195238,#2886) ;
#2184 = LINE('',#195239,#2887) ;
#2185 = LINE('',#195253,#2888) ;
#2186 = LINE('',#195257,#2889) ;
#2187 = LINE('',#195259,#2890) ;
#2188 = LINE('',#195260,#2891) ;
#2189 = LINE('',#195263,#2892) ;
#2190 = LINE('',#195265,#2893) ;
#2191 = LINE('',#195266,#2894) ;
#2192 = LINE('',#195280,#2895) ;
#2193 = LINE('',#195284,#2896) ;
#2194 = LINE('',#195286,#2897) ;
#2195 = LINE('',#195287,#2898) ;
#2196 = LINE('',#195290,#2899) ;
#2197 = LINE('',#195292,#2900) ;
#2198 = LINE('',#195293,#2901) ;
#2199 = LINE('',#195307,#2902) ;
#2200 = LINE('',#195311,#2903) ;
#2201 = LINE('',#195313,#2904) ;
#2202 = LINE('',#195314,#2905) ;
#2203 = LINE('',#195317,#2906) ;
#2204 = LINE('',#195319,#2907) ;
#2205 = LINE('',#195320,#2908) ;
#2206 = LINE('',#195334,#2909) ;
#2207 = LINE('',#195338,#2910) ;
#2208 = LINE('',#195340,#2911) ;
#2209 = LINE('',#195341,#2912) ;
#2210 = LINE('',#195344,#2913) ;
#2211 = LINE('',#195346,#2914) ;
#2212 = LINE('',#195347,#2915) ;
#2213 = LINE('',#195361,#2916) ;
#2214 = LINE('',#195365,#2917) ;
#2215 = LINE('',#195367,#2918) ;
#2216 = LINE('',#195368,#2919) ;
#2217 = LINE('',#195371,#2920) ;
#2218 = LINE('',#195373,#2921) ;
#2219 = LINE('',#195374,#2922) ;
#2220 = LINE('',#195388,#2923) ;
#2221 = LINE('',#195392,#2924) ;
#2222 = LINE('',#195394,#2925) ;
#2223 = LINE('',#195395,#2926) ;
#2224 = LINE('',#195398,#2927) ;
#2225 = LINE('',#195400,#2928) ;
#2226 = LINE('',#195401,#2929) ;
#2227 = LINE('',#195415,#2930) ;
#2228 = LINE('',#195419,#2931) ;
#2229 = LINE('',#195421,#2932) ;
#2230 = LINE('',#195422,#2933) ;
#2231 = LINE('',#195425,#2934) ;
#2232 = LINE('',#195427,#2935) ;
#2233 = LINE('',#195428,#2936) ;
#2234 = LINE('',#195442,#2937) ;
#2235 = LINE('',#195446,#2938) ;
#2236 = LINE('',#195448,#2939) ;
#2237 = LINE('',#195449,#2940) ;
#2238 = LINE('',#195452,#2941) ;
#2239 = LINE('',#195454,#2942) ;
#2240 = LINE('',#195455,#2943) ;
#2241 = LINE('',#195469,#2944) ;
#2242 = LINE('',#195473,#2945) ;
#2243 = LINE('',#195475,#2946) ;
#2244 = LINE('',#195476,#2947) ;
#2245 = LINE('',#195479,#2948) ;
#2246 = LINE('',#195481,#2949) ;
#2247 = LINE('',#195482,#2950) ;
#2248 = LINE('',#195496,#2951) ;
#2249 = LINE('',#195500,#2952) ;
#2250 = LINE('',#195502,#2953) ;
#2251 = LINE('',#195503,#2954) ;
#2252 = LINE('',#195506,#2955) ;
#2253 = LINE('',#195508,#2956) ;
#2254 = LINE('',#195509,#2957) ;
#2255 = LINE('',#195523,#2958) ;
#2256 = LINE('',#195527,#2959) ;
#2257 = LINE('',#195529,#2960) ;
#2258 = LINE('',#195530,#2961) ;
#2259 = LINE('',#195533,#2962) ;
#2260 = LINE('',#195535,#2963) ;
#2261 = LINE('',#195536,#2964) ;
#2262 = LINE('',#195550,#2965) ;
#2263 = LINE('',#195554,#2966) ;
#2264 = LINE('',#195556,#2967) ;
#2265 = LINE('',#195557,#2968) ;
#2266 = LINE('',#195560,#2969) ;
#2267 = LINE('',#195562,#2970) ;
#2268 = LINE('',#195563,#2971) ;
#2269 = LINE('',#195577,#2972) ;
#2270 = LINE('',#195581,#2973) ;
#2271 = LINE('',#195583,#2974) ;
#2272 = LINE('',#195584,#2975) ;
#2273 = LINE('',#195587,#2976) ;
#2274 = LINE('',#195589,#2977) ;
#2275 = LINE('',#195590,#2978) ;
#2276 = LINE('',#195604,#2979) ;
#2277 = LINE('',#195608,#2980) ;
#2278 = LINE('',#195610,#2981) ;
#2279 = LINE('',#195611,#2982) ;
#2280 = LINE('',#195614,#2983) ;
#2281 = LINE('',#195616,#2984) ;
#2282 = LINE('',#195617,#2985) ;
#2283 = LINE('',#195631,#2986) ;
#2284 = LINE('',#195635,#2987) ;
#2285 = LINE('',#195637,#2988) ;
#2286 = LINE('',#195638,#2989) ;
#2287 = LINE('',#195641,#2990) ;
#2288 = LINE('',#195643,#2991) ;
#2289 = LINE('',#195644,#2992) ;
#2290 = LINE('',#195658,#2993) ;
#2291 = LINE('',#195662,#2994) ;
#2292 = LINE('',#195664,#2995) ;
#2293 = LINE('',#195665,#2996) ;
#2294 = LINE('',#195668,#2997) ;
#2295 = LINE('',#195670,#2998) ;
#2296 = LINE('',#195671,#2999) ;
#2297 = LINE('',#195685,#3000) ;
#2298 = LINE('',#195689,#3001) ;
#2299 = LINE('',#195691,#3002) ;
#2300 = LINE('',#195692,#3003) ;
#2301 = LINE('',#195695,#3004) ;
#2302 = LINE('',#195697,#3005) ;
#2303 = LINE('',#195698,#3006) ;
#2304 = LINE('',#195712,#3007) ;
#2305 = LINE('',#195716,#3008) ;
#2306 = LINE('',#195718,#3009) ;
#2307 = LINE('',#195719,#3010) ;
#2308 = LINE('',#195722,#3011) ;
#2309 = LINE('',#195724,#3012) ;
#2310 = LINE('',#195725,#3013) ;
#2311 = LINE('',#195739,#3014) ;
#2312 = LINE('',#195743,#3015) ;
#2313 = LINE('',#195745,#3016) ;
#2314 = LINE('',#195746,#3017) ;
#2315 = LINE('',#195749,#3018) ;
#2316 = LINE('',#195751,#3019) ;
#2317 = LINE('',#195752,#3020) ;
#2318 = LINE('',#195766,#3021) ;
#2319 = LINE('',#195770,#3022) ;
#2320 = LINE('',#195772,#3023) ;
#2321 = LINE('',#195773,#3024) ;
#2322 = LINE('',#195776,#3025) ;
#2323 = LINE('',#195778,#3026) ;
#2324 = LINE('',#195779,#3027) ;
#2325 = LINE('',#195793,#3028) ;
#2326 = LINE('',#195797,#3029) ;
#2327 = LINE('',#195799,#3030) ;
#2328 = LINE('',#195800,#3031) ;
#2329 = LINE('',#195803,#3032) ;
#2330 = LINE('',#195805,#3033) ;
#2331 = LINE('',#195806,#3034) ;
#2332 = LINE('',#195820,#3035) ;
#2333 = LINE('',#195824,#3036) ;
#2334 = LINE('',#195826,#3037) ;
#2335 = LINE('',#195827,#3038) ;
#2336 = LINE('',#195830,#3039) ;
#2337 = LINE('',#195832,#3040) ;
#2338 = LINE('',#195833,#3041) ;
#2339 = LINE('',#195847,#3042) ;
#2340 = LINE('',#195851,#3043) ;
#2341 = LINE('',#195853,#3044) ;
#2342 = LINE('',#195854,#3045) ;
#2343 = LINE('',#195857,#3046) ;
#2344 = LINE('',#195859,#3047) ;
#2345 = LINE('',#195860,#3048) ;
#2346 = LINE('',#195874,#3049) ;
#2347 = LINE('',#195878,#3050) ;
#2348 = LINE('',#195880,#3051) ;
#2349 = LINE('',#195881,#3052) ;
#2350 = LINE('',#195884,#3053) ;
#2351 = LINE('',#195886,#3054) ;
#2352 = LINE('',#195887,#3055) ;
#2353 = LINE('',#195901,#3056) ;
#2354 = LINE('',#195905,#3057) ;
#2355 = LINE('',#195907,#3058) ;
#2356 = LINE('',#195908,#3059) ;
#2357 = LINE('',#195911,#3060) ;
#2358 = LINE('',#195913,#3061) ;
#2359 = LINE('',#195914,#3062) ;
#2360 = LINE('',#195928,#3063) ;
#2361 = LINE('',#195932,#3064) ;
#2362 = LINE('',#195934,#3065) ;
#2363 = LINE('',#195935,#3066) ;
#2364 = LINE('',#195938,#3067) ;
#2365 = LINE('',#195940,#3068) ;
#2366 = LINE('',#195941,#3069) ;
#2367 = LINE('',#195955,#3070) ;
#2368 = LINE('',#195959,#3071) ;
#2369 = LINE('',#195961,#3072) ;
#2370 = LINE('',#195962,#3073) ;
#2371 = LINE('',#195965,#3074) ;
#2372 = LINE('',#195967,#3075) ;
#2373 = LINE('',#195968,#3076) ;
#2374 = LINE('',#195982,#3077) ;
#2375 = LINE('',#195986,#3078) ;
#2376 = LINE('',#195988,#3079) ;
#2377 = LINE('',#195989,#3080) ;
#2378 = LINE('',#195992,#3081) ;
#2379 = LINE('',#195994,#3082) ;
#2380 = LINE('',#195995,#3083) ;
#2381 = LINE('',#196009,#3084) ;
#2382 = LINE('',#196013,#3085) ;
#2383 = LINE('',#196015,#3086) ;
#2384 = LINE('',#196016,#3087) ;
#2385 = LINE('',#196019,#3088) ;
#2386 = LINE('',#196021,#3089) ;
#2387 = LINE('',#196022,#3090) ;
#2388 = LINE('',#196036,#3091) ;
#2389 = LINE('',#196040,#3092) ;
#2390 = LINE('',#196042,#3093) ;
#2391 = LINE('',#196043,#3094) ;
#2392 = LINE('',#196046,#3095) ;
#2393 = LINE('',#196048,#3096) ;
#2394 = LINE('',#196049,#3097) ;
#2395 = LINE('',#196063,#3098) ;
#2396 = LINE('',#196067,#3099) ;
#2397 = LINE('',#196069,#3100) ;
#2398 = LINE('',#196070,#3101) ;
#2399 = LINE('',#196073,#3102) ;
#2400 = LINE('',#196075,#3103) ;
#2401 = LINE('',#196076,#3104) ;
#2402 = LINE('',#196090,#3105) ;
#2403 = LINE('',#196094,#3106) ;
#2404 = LINE('',#196096,#3107) ;
#2405 = LINE('',#196097,#3108) ;
#2406 = LINE('',#196100,#3109) ;
#2407 = LINE('',#196102,#3110) ;
#2408 = LINE('',#196103,#3111) ;
#2409 = LINE('',#196117,#3112) ;
#2410 = LINE('',#196121,#3113) ;
#2411 = LINE('',#196123,#3114) ;
#2412 = LINE('',#196124,#3115) ;
#2413 = LINE('',#196127,#3116) ;
#2414 = LINE('',#196129,#3117) ;
#2415 = LINE('',#196130,#3118) ;
#2416 = LINE('',#196144,#3119) ;
#2417 = LINE('',#196148,#3120) ;
#2418 = LINE('',#196150,#3121) ;
#2419 = LINE('',#196151,#3122) ;
#2420 = LINE('',#196154,#3123) ;
#2421 = LINE('',#196156,#3124) ;
#2422 = LINE('',#196157,#3125) ;
#2423 = LINE('',#196171,#3126) ;
#2424 = LINE('',#196175,#3127) ;
#2425 = LINE('',#196177,#3128) ;
#2426 = LINE('',#196178,#3129) ;
#2427 = LINE('',#196181,#3130) ;
#2428 = LINE('',#196183,#3131) ;
#2429 = LINE('',#196184,#3132) ;
#2430 = LINE('',#196198,#3133) ;
#2431 = LINE('',#196202,#3134) ;
#2432 = LINE('',#196204,#3135) ;
#2433 = LINE('',#196205,#3136) ;
#2434 = LINE('',#196208,#3137) ;
#2435 = LINE('',#196210,#3138) ;
#2436 = LINE('',#196211,#3139) ;
#2437 = LINE('',#196225,#3140) ;
#2438 = LINE('',#196229,#3141) ;
#2439 = LINE('',#196231,#3142) ;
#2440 = LINE('',#196232,#3143) ;
#2441 = LINE('',#196235,#3144) ;
#2442 = LINE('',#196237,#3145) ;
#2443 = LINE('',#196238,#3146) ;
#2444 = LINE('',#196252,#3147) ;
#2445 = LINE('',#196256,#3148) ;
#2446 = LINE('',#196258,#3149) ;
#2447 = LINE('',#196259,#3150) ;
#2448 = LINE('',#196262,#3151) ;
#2449 = LINE('',#196264,#3152) ;
#2450 = LINE('',#196265,#3153) ;
#2451 = LINE('',#196279,#3154) ;
#2452 = LINE('',#196283,#3155) ;
#2453 = LINE('',#196285,#3156) ;
#2454 = LINE('',#196286,#3157) ;
#2455 = LINE('',#196289,#3158) ;
#2456 = LINE('',#196291,#3159) ;
#2457 = LINE('',#196292,#3160) ;
#2458 = LINE('',#196306,#3161) ;
#2459 = LINE('',#196310,#3162) ;
#2460 = LINE('',#196312,#3163) ;
#2461 = LINE('',#196313,#3164) ;
#2462 = LINE('',#196316,#3165) ;
#2463 = LINE('',#196318,#3166) ;
#2464 = LINE('',#196319,#3167) ;
#2465 = LINE('',#196333,#3168) ;
#2466 = LINE('',#196337,#3169) ;
#2467 = LINE('',#196339,#3170) ;
#2468 = LINE('',#196340,#3171) ;
#2469 = LINE('',#196343,#3172) ;
#2470 = LINE('',#196345,#3173) ;
#2471 = LINE('',#196346,#3174) ;
#2472 = LINE('',#196360,#3175) ;
#2473 = LINE('',#196364,#3176) ;
#2474 = LINE('',#196366,#3177) ;
#2475 = LINE('',#196367,#3178) ;
#2476 = LINE('',#196370,#3179) ;
#2477 = LINE('',#196372,#3180) ;
#2478 = LINE('',#196373,#3181) ;
#2479 = LINE('',#196387,#3182) ;
#2480 = LINE('',#196391,#3183) ;
#2481 = LINE('',#196393,#3184) ;
#2482 = LINE('',#196394,#3185) ;
#2483 = LINE('',#196397,#3186) ;
#2484 = LINE('',#196399,#3187) ;
#2485 = LINE('',#196400,#3188) ;
#2486 = LINE('',#196414,#3189) ;
#2487 = LINE('',#196418,#3190) ;
#2488 = LINE('',#196420,#3191) ;
#2489 = LINE('',#196421,#3192) ;
#2490 = LINE('',#196424,#3193) ;
#2491 = LINE('',#196426,#3194) ;
#2492 = LINE('',#196427,#3195) ;
#2493 = LINE('',#196441,#3196) ;
#2494 = LINE('',#196445,#3197) ;
#2495 = LINE('',#196447,#3198) ;
#2496 = LINE('',#196448,#3199) ;
#2497 = LINE('',#196451,#3200) ;
#2498 = LINE('',#196453,#3201) ;
#2499 = LINE('',#196454,#3202) ;
#2500 = LINE('',#196468,#3203) ;
#2501 = LINE('',#196471,#3204) ;
#2502 = LINE('',#196472,#3205) ;
#2503 = LINE('',#196476,#3206) ;
#2504 = LINE('',#196484,#3207) ;
#2505 = LINE('',#196494,#3208) ;
#2506 = LINE('',#196502,#3209) ;
#2507 = LINE('',#196510,#3210) ;
#2508 = LINE('',#196518,#3211) ;
#2509 = LINE('',#196526,#3212) ;
#2510 = LINE('',#196534,#3213) ;
#2511 = LINE('',#196542,#3214) ;
#2512 = LINE('',#196550,#3215) ;
#2513 = LINE('',#196561,#3216) ;
#2514 = LINE('',#196564,#3217) ;
#2515 = LINE('',#196568,#3218) ;
#2516 = LINE('',#196571,#3219) ;
#2517 = LINE('',#196572,#3220) ;
#2518 = LINE('',#196576,#3221) ;
#2519 = LINE('',#196580,#3222) ;
#2520 = LINE('',#196584,#3223) ;
#2521 = LINE('',#196587,#3224) ;
#2522 = LINE('',#196588,#3225) ;
#2523 = LINE('',#196594,#3226) ;
#2524 = LINE('',#196597,#3227) ;
#2525 = LINE('',#196600,#3228) ;
#2526 = LINE('',#196604,#3229) ;
#2527 = LINE('',#196607,#3230) ;
#2528 = LINE('',#196608,#3231) ;
#2529 = LINE('',#196612,#3232) ;
#2530 = LINE('',#196616,#3233) ;
#2531 = LINE('',#196620,#3234) ;
#2532 = LINE('',#196623,#3235) ;
#2533 = LINE('',#196624,#3236) ;
#2534 = LINE('',#196629,#3237) ;
#2535 = LINE('',#196632,#3238) ;
#2536 = LINE('',#196636,#3239) ;
#2537 = LINE('',#196639,#3240) ;
#2538 = LINE('',#196640,#3241) ;
#2539 = LINE('',#196644,#3242) ;
#2540 = LINE('',#196648,#3243) ;
#2541 = LINE('',#196652,#3244) ;
#2542 = LINE('',#196655,#3245) ;
#2543 = LINE('',#196656,#3246) ;
#2544 = LINE('',#196661,#3247) ;
#2545 = LINE('',#196664,#3248) ;
#2546 = LINE('',#196668,#3249) ;
#2547 = LINE('',#196671,#3250) ;
#2548 = LINE('',#196672,#3251) ;
#2549 = LINE('',#196676,#3252) ;
#2550 = LINE('',#196680,#3253) ;
#2551 = LINE('',#196684,#3254) ;
#2552 = LINE('',#196687,#3255) ;
#2553 = LINE('',#196688,#3256) ;
#2554 = LINE('',#196693,#3257) ;
#2555 = LINE('',#196696,#3258) ;
#2556 = LINE('',#196700,#3259) ;
#2557 = LINE('',#196703,#3260) ;
#2558 = LINE('',#196704,#3261) ;
#2559 = LINE('',#196708,#3262) ;
#2560 = LINE('',#196712,#3263) ;
#2561 = LINE('',#196716,#3264) ;
#2562 = LINE('',#196719,#3265) ;
#2563 = LINE('',#196720,#3266) ;
#2564 = LINE('',#196725,#3267) ;
#2565 = LINE('',#196731,#3268) ;
#2566 = VECTOR('',#9461,0.300000000000011) ;
#2567 = VECTOR('',#9464,0.299999999999991) ;
#2568 = VECTOR('',#9465,10.) ;
#2569 = VECTOR('',#9466,10.) ;
#2570 = VECTOR('',#9467,10.) ;
#2571 = VECTOR('',#9468,10.) ;
#2572 = VECTOR('',#9473,3.00000000000003) ;
#2573 = VECTOR('',#9480,10.) ;
#2574 = VECTOR('',#9481,10.) ;
#2575 = VECTOR('',#9484,1.2500000000303) ;
#2576 = VECTOR('',#9489,1.2500000000303) ;
#2577 = VECTOR('',#9492,1.2500000000303) ;
#2578 = VECTOR('',#9495,1.2500000000303) ;
#2579 = VECTOR('',#9498,1.2500000000303) ;
#2580 = VECTOR('',#9501,1.25000000003033) ;
#2581 = VECTOR('',#9506,1.25000000003033) ;
#2582 = VECTOR('',#9509,1.25000000003033) ;
#2583 = VECTOR('',#9512,1.25000000003033) ;
#2584 = VECTOR('',#9515,1.25000000003033) ;
#2585 = VECTOR('',#9520,2.00000000000006) ;
#2586 = VECTOR('',#9527,10.) ;
#2587 = VECTOR('',#9528,10.) ;
#2588 = VECTOR('',#9531,1.12500000002727) ;
#2589 = VECTOR('',#9540,1.12500000002727) ;
#2590 = VECTOR('',#9545,10.) ;
#2591 = VECTOR('',#9548,10.) ;
#2592 = VECTOR('',#9553,10.) ;
#2593 = VECTOR('',#9564,1.2500000000303) ;
#2594 = VECTOR('',#9567,10.) ;
#2595 = VECTOR('',#9570,10.) ;
#2596 = VECTOR('',#9571,10.) ;
#2597 = VECTOR('',#9574,1.25000000003033) ;
#2598 = VECTOR('',#9577,0.300000000000011) ;
#2599 = VECTOR('',#9578,10.) ;
#2600 = VECTOR('',#9581,0.300000000000011) ;
#2601 = VECTOR('',#9582,10.) ;
#2602 = VECTOR('',#9585,0.299999999999991) ;
#2603 = VECTOR('',#9588,0.299999999999991) ;
#2604 = VECTOR('',#9589,10.) ;
#2605 = VECTOR('',#9590,10.) ;
#2606 = VECTOR('',#9595,0.299999999999991) ;
#2607 = VECTOR('',#9604,10.) ;
#2608 = VECTOR('',#9609,0.300000000000007) ;
#2609 = VECTOR('',#9618,1.21492629244945) ;
#2610 = VECTOR('',#9623,1.21492629244945) ;
#2611 = VECTOR('',#9626,1.21492629244945) ;
#2612 = VECTOR('',#9629,1.21492629244945) ;
#2613 = VECTOR('',#9636,0.119992720241923) ;
#2614 = VECTOR('',#9641,0.239985440483837) ;
#2615 = VECTOR('',#9646,0.199999999999989) ;
#2616 = VECTOR('',#9649,10.) ;
#2617 = VECTOR('',#9650,10.) ;
#2618 = VECTOR('',#9651,10.) ;
#2619 = VECTOR('',#9652,10.) ;
#2620 = VECTOR('',#9653,10.) ;
#2621 = VECTOR('',#9654,10.) ;
#2622 = VECTOR('',#9657,10.) ;
#2623 = VECTOR('',#9658,10.) ;
#2624 = VECTOR('',#9659,10.) ;
#2625 = VECTOR('',#9662,10.) ;
#2626 = VECTOR('',#9663,10.) ;
#2627 = VECTOR('',#9666,10.) ;
#2628 = VECTOR('',#9667,10.) ;
#2629 = VECTOR('',#9670,10.) ;
#2630 = VECTOR('',#9671,10.) ;
#2631 = VECTOR('',#9674,10.) ;
#2632 = VECTOR('',#9675,10.) ;
#2633 = VECTOR('',#9678,10.) ;
#2634 = VECTOR('',#9683,1.21492629244947) ;
#2635 = VECTOR('',#9688,1.21492629244947) ;
#2636 = VECTOR('',#9691,1.21492629244947) ;
#2637 = VECTOR('',#9694,1.21492629244947) ;
#2638 = VECTOR('',#9703,0.119992720241926) ;
#2639 = VECTOR('',#9706,0.23998544048385) ;
#2640 = VECTOR('',#9709,0.199999999999993) ;
#2641 = VECTOR('',#9714,10.) ;
#2642 = VECTOR('',#9715,10.) ;
#2643 = VECTOR('',#9716,10.) ;
#2644 = VECTOR('',#9717,10.) ;
#2645 = VECTOR('',#9718,10.) ;
#2646 = VECTOR('',#9719,10.) ;
#2647 = VECTOR('',#9722,10.) ;
#2648 = VECTOR('',#9723,10.) ;
#2649 = VECTOR('',#9724,10.) ;
#2650 = VECTOR('',#9727,10.) ;
#2651 = VECTOR('',#9728,10.) ;
#2652 = VECTOR('',#9731,10.) ;
#2653 = VECTOR('',#9732,10.) ;
#2654 = VECTOR('',#9735,10.) ;
#2655 = VECTOR('',#9736,10.) ;
#2656 = VECTOR('',#9739,10.) ;
#2657 = VECTOR('',#9740,10.) ;
#2658 = VECTOR('',#9743,10.) ;
#2659 = VECTOR('',#9750,10.) ;
#2660 = VECTOR('',#9753,10.) ;
#2661 = VECTOR('',#9758,10.) ;
#2662 = VECTOR('',#9765,10.) ;
#2663 = VECTOR('',#9778,1.00000000000001) ;
#2664 = VECTOR('',#9817,2.00000000000002) ;
#2665 = VECTOR('',#9820,10.) ;
#2666 = VECTOR('',#9821,10.) ;
#2667 = VECTOR('',#9824,10.) ;
#2668 = VECTOR('',#9829,10.) ;
#2669 = VECTOR('',#9836,6.99999999999997) ;
#2670 = VECTOR('',#9839,10.) ;
#2671 = VECTOR('',#9840,10.) ;
#2672 = VECTOR('',#9843,10.) ;
#2673 = VECTOR('',#9848,10.) ;
#2674 = VECTOR('',#9853,10.) ;
#2675 = VECTOR('',#9854,10.) ;
#2676 = VECTOR('',#9855,10.) ;
#2677 = VECTOR('',#9856,10.) ;
#2678 = VECTOR('',#9857,10.) ;
#2679 = VECTOR('',#9858,10.) ;
#2680 = VECTOR('',#9859,10.) ;
#2681 = VECTOR('',#9860,10.) ;
#2682 = VECTOR('',#9861,10.) ;
#2683 = VECTOR('',#9862,10.) ;
#2684 = VECTOR('',#9867,10.) ;
#2685 = VECTOR('',#9870,10.) ;
#2686 = VECTOR('',#9875,10.) ;
#2687 = VECTOR('',#9882,10.) ;
#2688 = VECTOR('',#9929,2.) ;
#2689 = VECTOR('',#9932,10.) ;
#2690 = VECTOR('',#9933,10.) ;
#2691 = VECTOR('',#9936,10.) ;
#2692 = VECTOR('',#9941,10.) ;
#2693 = VECTOR('',#9948,6.99999999999998) ;
#2694 = VECTOR('',#9951,10.) ;
#2695 = VECTOR('',#9952,10.) ;
#2696 = VECTOR('',#9955,10.) ;
#2697 = VECTOR('',#9958,10.) ;
#2698 = VECTOR('',#9965,0.999999999999981) ;
#2699 = VECTOR('',#9966,10.) ;
#2700 = VECTOR('',#9967,10.) ;
#2701 = VECTOR('',#9968,10.) ;
#2702 = VECTOR('',#9969,10.) ;
#2703 = VECTOR('',#9970,10.) ;
#2704 = VECTOR('',#9971,10.) ;
#2705 = VECTOR('',#9972,10.) ;
#2706 = VECTOR('',#9973,10.) ;
#2707 = VECTOR('',#9974,10.) ;
#2708 = VECTOR('',#9975,10.) ;
#2709 = VECTOR('',#9976,10.) ;
#2710 = VECTOR('',#9981,2.00000000000003) ;
#2711 = VECTOR('',#9988,10.) ;
#2712 = VECTOR('',#9989,10.) ;
#2713 = VECTOR('',#9994,10.) ;
#2714 = VECTOR('',#9997,10.) ;
#2715 = VECTOR('',#10000,10.) ;
#2716 = VECTOR('',#10001,10.) ;
#2717 = VECTOR('',#10002,10.) ;
#2718 = VECTOR('',#10007,10.) ;
#2719 = VECTOR('',#10014,10.) ;
#2720 = VECTOR('',#10019,10.) ;
#2721 = VECTOR('',#10020,10.) ;
#2722 = VECTOR('',#10021,10.) ;
#2723 = VECTOR('',#10024,10.) ;
#2724 = VECTOR('',#10025,10.) ;
#2725 = VECTOR('',#10026,10.) ;
#2726 = VECTOR('',#10031,10.) ;
#2727 = VECTOR('',#10036,10.) ;
#2728 = VECTOR('',#10037,10.) ;
#2729 = VECTOR('',#10038,10.) ;
#2730 = VECTOR('',#10043,10.) ;
#2731 = VECTOR('',#10050,10.) ;
#2732 = VECTOR('',#10055,10.) ;
#2733 = VECTOR('',#10056,10.) ;
#2734 = VECTOR('',#10057,10.) ;
#2735 = VECTOR('',#10078,1.00000000000007) ;
#2736 = VECTOR('',#10081,2.00000000000001) ;
#2737 = VECTOR('',#10084,10.) ;
#2738 = VECTOR('',#10093,10.) ;
#2739 = VECTOR('',#10098,10.) ;
#2740 = VECTOR('',#10099,10.) ;
#2741 = VECTOR('',#10104,10.) ;
#2742 = VECTOR('',#10109,10.) ;
#2743 = VECTOR('',#10114,10.) ;
#2744 = VECTOR('',#10117,10.) ;
#2745 = VECTOR('',#10130,10.) ;
#2746 = VECTOR('',#10149,10.) ;
#2747 = VECTOR('',#10164,10.) ;
#2748 = VECTOR('',#10169,10.) ;
#2749 = VECTOR('',#10174,10.) ;
#2750 = VECTOR('',#10177,10.) ;
#2751 = VECTOR('',#10180,10.) ;
#2752 = VECTOR('',#10189,10.) ;
#2753 = VECTOR('',#10194,10.) ;
#2754 = VECTOR('',#10195,10.) ;
#2755 = VECTOR('',#10208,10.) ;
#2756 = VECTOR('',#10227,10.) ;
#2757 = VECTOR('',#10240,10.) ;
#2758 = VECTOR('',#10241,10.) ;
#2759 = VECTOR('',#10242,10.) ;
#2760 = VECTOR('',#10243,10.) ;
#2761 = VECTOR('',#10246,10.) ;
#2762 = VECTOR('',#10253,10.) ;
#2763 = VECTOR('',#10260,10.) ;
#2764 = VECTOR('',#10267,10.) ;
#2765 = VECTOR('',#10274,10.) ;
#2766 = VECTOR('',#10281,10.) ;
#2767 = VECTOR('',#10286,10.) ;
#2768 = VECTOR('',#10287,10.) ;
#2769 = VECTOR('',#10288,10.) ;
#2770 = VECTOR('',#10293,10.) ;
#2771 = VECTOR('',#10298,10.) ;
#2772 = VECTOR('',#10299,10.) ;
#2773 = VECTOR('',#10300,10.) ;
#2774 = VECTOR('',#10305,10.) ;
#2775 = VECTOR('',#10312,10.) ;
#2776 = VECTOR('',#10319,10.) ;
#2777 = VECTOR('',#10324,10.) ;
#2778 = VECTOR('',#10329,10.) ;
#2779 = VECTOR('',#10330,10.) ;
#2780 = VECTOR('',#10335,2.00000000000001) ;
#2781 = VECTOR('',#10342,0.999999999999978) ;
#2782 = VECTOR('',#10353,7.00000000000021) ;
#2783 = VECTOR('',#10370,13.7469842874597) ;
#2784 = VECTOR('',#10381,7.00000000000021) ;
#2785 = VECTOR('',#10384,3.00000000000005) ;
#2786 = VECTOR('',#10387,10.) ;
#2787 = VECTOR('',#10388,10.) ;
#2788 = VECTOR('',#10389,10.) ;
#2789 = VECTOR('',#10390,10.) ;
#2790 = VECTOR('',#10393,10.) ;
#2791 = VECTOR('',#10398,10.) ;
#2792 = VECTOR('',#10399,10.) ;
#2793 = VECTOR('',#10400,10.) ;
#2794 = VECTOR('',#10403,10.) ;
#2795 = VECTOR('',#10404,10.) ;
#2796 = VECTOR('',#10405,10.) ;
#2797 = VECTOR('',#10408,10.) ;
#2798 = VECTOR('',#10413,10.) ;
#2799 = VECTOR('',#10414,10.) ;
#2800 = VECTOR('',#10415,10.) ;
#2801 = VECTOR('',#10418,10.) ;
#2802 = VECTOR('',#10419,10.) ;
#2803 = VECTOR('',#10420,10.) ;
#2804 = VECTOR('',#10423,10.) ;
#2805 = VECTOR('',#10428,10.) ;
#2806 = VECTOR('',#10429,10.) ;
#2807 = VECTOR('',#10430,10.) ;
#2808 = VECTOR('',#10433,10.) ;
#2809 = VECTOR('',#10434,10.) ;
#2810 = VECTOR('',#10435,10.) ;
#2811 = VECTOR('',#10438,10.) ;
#2812 = VECTOR('',#10443,10.) ;
#2813 = VECTOR('',#10444,10.) ;
#2814 = VECTOR('',#10445,10.) ;
#2815 = VECTOR('',#10448,10.) ;
#2816 = VECTOR('',#10449,10.) ;
#2817 = VECTOR('',#10450,10.) ;
#2818 = VECTOR('',#10453,10.) ;
#2819 = VECTOR('',#10458,10.) ;
#2820 = VECTOR('',#10459,10.) ;
#2821 = VECTOR('',#10460,10.) ;
#2822 = VECTOR('',#10463,10.) ;
#2823 = VECTOR('',#10464,10.) ;
#2824 = VECTOR('',#10465,10.) ;
#2825 = VECTOR('',#10468,10.) ;
#2826 = VECTOR('',#10473,10.) ;
#2827 = VECTOR('',#10474,10.) ;
#2828 = VECTOR('',#10475,10.) ;
#2829 = VECTOR('',#10478,10.) ;
#2830 = VECTOR('',#10479,10.) ;
#2831 = VECTOR('',#10480,10.) ;
#2832 = VECTOR('',#10483,10.) ;
#2833 = VECTOR('',#10488,10.) ;
#2834 = VECTOR('',#10489,10.) ;
#2835 = VECTOR('',#10490,10.) ;
#2836 = VECTOR('',#10493,10.) ;
#2837 = VECTOR('',#10494,10.) ;
#2838 = VECTOR('',#10495,10.) ;
#2839 = VECTOR('',#10498,10.) ;
#2840 = VECTOR('',#10503,10.) ;
#2841 = VECTOR('',#10504,10.) ;
#2842 = VECTOR('',#10505,10.) ;
#2843 = VECTOR('',#10508,10.) ;
#2844 = VECTOR('',#10509,10.) ;
#2845 = VECTOR('',#10510,10.) ;
#2846 = VECTOR('',#10513,10.) ;
#2847 = VECTOR('',#10518,10.) ;
#2848 = VECTOR('',#10519,10.) ;
#2849 = VECTOR('',#10520,10.) ;
#2850 = VECTOR('',#10523,10.) ;
#2851 = VECTOR('',#10524,10.) ;
#2852 = VECTOR('',#10525,10.) ;
#2853 = VECTOR('',#10528,10.) ;
#2854 = VECTOR('',#10533,10.) ;
#2855 = VECTOR('',#10534,10.) ;
#2856 = VECTOR('',#10535,10.) ;
#2857 = VECTOR('',#10538,10.) ;
#2858 = VECTOR('',#10539,10.) ;
#2859 = VECTOR('',#10540,10.) ;
#2860 = VECTOR('',#10543,10.) ;
#2861 = VECTOR('',#10548,10.) ;
#2862 = VECTOR('',#10549,10.) ;
#2863 = VECTOR('',#10550,10.) ;
#2864 = VECTOR('',#10553,10.) ;
#2865 = VECTOR('',#10554,10.) ;
#2866 = VECTOR('',#10555,10.) ;
#2867 = VECTOR('',#10558,10.) ;
#2868 = VECTOR('',#10563,10.) ;
#2869 = VECTOR('',#10564,10.) ;
#2870 = VECTOR('',#10565,10.) ;
#2871 = VECTOR('',#10568,10.) ;
#2872 = VECTOR('',#10569,10.) ;
#2873 = VECTOR('',#10570,10.) ;
#2874 = VECTOR('',#10573,10.) ;
#2875 = VECTOR('',#10578,10.) ;
#2876 = VECTOR('',#10579,10.) ;
#2877 = VECTOR('',#10580,10.) ;
#2878 = VECTOR('',#10583,10.) ;
#2879 = VECTOR('',#10584,10.) ;
#2880 = VECTOR('',#10585,10.) ;
#2881 = VECTOR('',#10588,10.) ;
#2882 = VECTOR('',#10593,10.) ;
#2883 = VECTOR('',#10594,10.) ;
#2884 = VECTOR('',#10595,10.) ;
#2885 = VECTOR('',#10598,10.) ;
#2886 = VECTOR('',#10599,10.) ;
#2887 = VECTOR('',#10600,10.) ;
#2888 = VECTOR('',#10603,10.) ;
#2889 = VECTOR('',#10608,10.) ;
#2890 = VECTOR('',#10609,10.) ;
#2891 = VECTOR('',#10610,10.) ;
#2892 = VECTOR('',#10613,10.) ;
#2893 = VECTOR('',#10614,10.) ;
#2894 = VECTOR('',#10615,10.) ;
#2895 = VECTOR('',#10618,10.) ;
#2896 = VECTOR('',#10623,10.) ;
#2897 = VECTOR('',#10624,10.) ;
#2898 = VECTOR('',#10625,10.) ;
#2899 = VECTOR('',#10628,10.) ;
#2900 = VECTOR('',#10629,10.) ;
#2901 = VECTOR('',#10630,10.) ;
#2902 = VECTOR('',#10633,10.) ;
#2903 = VECTOR('',#10638,10.) ;
#2904 = VECTOR('',#10639,10.) ;
#2905 = VECTOR('',#10640,10.) ;
#2906 = VECTOR('',#10643,10.) ;
#2907 = VECTOR('',#10644,10.) ;
#2908 = VECTOR('',#10645,10.) ;
#2909 = VECTOR('',#10648,10.) ;
#2910 = VECTOR('',#10653,10.) ;
#2911 = VECTOR('',#10654,10.) ;
#2912 = VECTOR('',#10655,10.) ;
#2913 = VECTOR('',#10658,10.) ;
#2914 = VECTOR('',#10659,10.) ;
#2915 = VECTOR('',#10660,10.) ;
#2916 = VECTOR('',#10663,10.) ;
#2917 = VECTOR('',#10668,10.) ;
#2918 = VECTOR('',#10669,10.) ;
#2919 = VECTOR('',#10670,10.) ;
#2920 = VECTOR('',#10673,10.) ;
#2921 = VECTOR('',#10674,10.) ;
#2922 = VECTOR('',#10675,10.) ;
#2923 = VECTOR('',#10678,10.) ;
#2924 = VECTOR('',#10683,10.) ;
#2925 = VECTOR('',#10684,10.) ;
#2926 = VECTOR('',#10685,10.) ;
#2927 = VECTOR('',#10688,10.) ;
#2928 = VECTOR('',#10689,10.) ;
#2929 = VECTOR('',#10690,10.) ;
#2930 = VECTOR('',#10693,10.) ;
#2931 = VECTOR('',#10698,10.) ;
#2932 = VECTOR('',#10699,10.) ;
#2933 = VECTOR('',#10700,10.) ;
#2934 = VECTOR('',#10703,10.) ;
#2935 = VECTOR('',#10704,10.) ;
#2936 = VECTOR('',#10705,10.) ;
#2937 = VECTOR('',#10708,10.) ;
#2938 = VECTOR('',#10713,10.) ;
#2939 = VECTOR('',#10714,10.) ;
#2940 = VECTOR('',#10715,10.) ;
#2941 = VECTOR('',#10718,10.) ;
#2942 = VECTOR('',#10719,10.) ;
#2943 = VECTOR('',#10720,10.) ;
#2944 = VECTOR('',#10723,10.) ;
#2945 = VECTOR('',#10728,10.) ;
#2946 = VECTOR('',#10729,10.) ;
#2947 = VECTOR('',#10730,10.) ;
#2948 = VECTOR('',#10733,10.) ;
#2949 = VECTOR('',#10734,10.) ;
#2950 = VECTOR('',#10735,10.) ;
#2951 = VECTOR('',#10738,10.) ;
#2952 = VECTOR('',#10743,10.) ;
#2953 = VECTOR('',#10744,10.) ;
#2954 = VECTOR('',#10745,10.) ;
#2955 = VECTOR('',#10748,10.) ;
#2956 = VECTOR('',#10749,10.) ;
#2957 = VECTOR('',#10750,10.) ;
#2958 = VECTOR('',#10753,10.) ;
#2959 = VECTOR('',#10758,10.) ;
#2960 = VECTOR('',#10759,10.) ;
#2961 = VECTOR('',#10760,10.) ;
#2962 = VECTOR('',#10763,10.) ;
#2963 = VECTOR('',#10764,10.) ;
#2964 = VECTOR('',#10765,10.) ;
#2965 = VECTOR('',#10768,10.) ;
#2966 = VECTOR('',#10773,10.) ;
#2967 = VECTOR('',#10774,10.) ;
#2968 = VECTOR('',#10775,10.) ;
#2969 = VECTOR('',#10778,10.) ;
#2970 = VECTOR('',#10779,10.) ;
#2971 = VECTOR('',#10780,10.) ;
#2972 = VECTOR('',#10783,10.) ;
#2973 = VECTOR('',#10788,10.) ;
#2974 = VECTOR('',#10789,10.) ;
#2975 = VECTOR('',#10790,10.) ;
#2976 = VECTOR('',#10793,10.) ;
#2977 = VECTOR('',#10794,10.) ;
#2978 = VECTOR('',#10795,10.) ;
#2979 = VECTOR('',#10798,10.) ;
#2980 = VECTOR('',#10803,10.) ;
#2981 = VECTOR('',#10804,10.) ;
#2982 = VECTOR('',#10805,10.) ;
#2983 = VECTOR('',#10808,10.) ;
#2984 = VECTOR('',#10809,10.) ;
#2985 = VECTOR('',#10810,10.) ;
#2986 = VECTOR('',#10813,10.) ;
#2987 = VECTOR('',#10818,10.) ;
#2988 = VECTOR('',#10819,10.) ;
#2989 = VECTOR('',#10820,10.) ;
#2990 = VECTOR('',#10823,10.) ;
#2991 = VECTOR('',#10824,10.) ;
#2992 = VECTOR('',#10825,10.) ;
#2993 = VECTOR('',#10828,10.) ;
#2994 = VECTOR('',#10833,10.) ;
#2995 = VECTOR('',#10834,10.) ;
#2996 = VECTOR('',#10835,10.) ;
#2997 = VECTOR('',#10838,10.) ;
#2998 = VECTOR('',#10839,10.) ;
#2999 = VECTOR('',#10840,10.) ;
#3000 = VECTOR('',#10843,10.) ;
#3001 = VECTOR('',#10848,10.) ;
#3002 = VECTOR('',#10849,10.) ;
#3003 = VECTOR('',#10850,10.) ;
#3004 = VECTOR('',#10853,10.) ;
#3005 = VECTOR('',#10854,10.) ;
#3006 = VECTOR('',#10855,10.) ;
#3007 = VECTOR('',#10858,10.) ;
#3008 = VECTOR('',#10863,10.) ;
#3009 = VECTOR('',#10864,10.) ;
#3010 = VECTOR('',#10865,10.) ;
#3011 = VECTOR('',#10868,10.) ;
#3012 = VECTOR('',#10869,10.) ;
#3013 = VECTOR('',#10870,10.) ;
#3014 = VECTOR('',#10873,10.) ;
#3015 = VECTOR('',#10878,10.) ;
#3016 = VECTOR('',#10879,10.) ;
#3017 = VECTOR('',#10880,10.) ;
#3018 = VECTOR('',#10883,10.) ;
#3019 = VECTOR('',#10884,10.) ;
#3020 = VECTOR('',#10885,10.) ;
#3021 = VECTOR('',#10888,10.) ;
#3022 = VECTOR('',#10893,10.) ;
#3023 = VECTOR('',#10894,10.) ;
#3024 = VECTOR('',#10895,10.) ;
#3025 = VECTOR('',#10898,10.) ;
#3026 = VECTOR('',#10899,10.) ;
#3027 = VECTOR('',#10900,10.) ;
#3028 = VECTOR('',#10903,10.) ;
#3029 = VECTOR('',#10908,10.) ;
#3030 = VECTOR('',#10909,10.) ;
#3031 = VECTOR('',#10910,10.) ;
#3032 = VECTOR('',#10913,10.) ;
#3033 = VECTOR('',#10914,10.) ;
#3034 = VECTOR('',#10915,10.) ;
#3035 = VECTOR('',#10918,10.) ;
#3036 = VECTOR('',#10923,10.) ;
#3037 = VECTOR('',#10924,10.) ;
#3038 = VECTOR('',#10925,10.) ;
#3039 = VECTOR('',#10928,10.) ;
#3040 = VECTOR('',#10929,10.) ;
#3041 = VECTOR('',#10930,10.) ;
#3042 = VECTOR('',#10933,10.) ;
#3043 = VECTOR('',#10938,10.) ;
#3044 = VECTOR('',#10939,10.) ;
#3045 = VECTOR('',#10940,10.) ;
#3046 = VECTOR('',#10943,10.) ;
#3047 = VECTOR('',#10944,10.) ;
#3048 = VECTOR('',#10945,10.) ;
#3049 = VECTOR('',#10948,10.) ;
#3050 = VECTOR('',#10953,10.) ;
#3051 = VECTOR('',#10954,10.) ;
#3052 = VECTOR('',#10955,10.) ;
#3053 = VECTOR('',#10958,10.) ;
#3054 = VECTOR('',#10959,10.) ;
#3055 = VECTOR('',#10960,10.) ;
#3056 = VECTOR('',#10963,10.) ;
#3057 = VECTOR('',#10968,10.) ;
#3058 = VECTOR('',#10969,10.) ;
#3059 = VECTOR('',#10970,10.) ;
#3060 = VECTOR('',#10973,10.) ;
#3061 = VECTOR('',#10974,10.) ;
#3062 = VECTOR('',#10975,10.) ;
#3063 = VECTOR('',#10978,10.) ;
#3064 = VECTOR('',#10983,10.) ;
#3065 = VECTOR('',#10984,10.) ;
#3066 = VECTOR('',#10985,10.) ;
#3067 = VECTOR('',#10988,10.) ;
#3068 = VECTOR('',#10989,10.) ;
#3069 = VECTOR('',#10990,10.) ;
#3070 = VECTOR('',#10993,10.) ;
#3071 = VECTOR('',#10998,10.) ;
#3072 = VECTOR('',#10999,10.) ;
#3073 = VECTOR('',#11000,10.) ;
#3074 = VECTOR('',#11003,10.) ;
#3075 = VECTOR('',#11004,10.) ;
#3076 = VECTOR('',#11005,10.) ;
#3077 = VECTOR('',#11008,10.) ;
#3078 = VECTOR('',#11013,10.) ;
#3079 = VECTOR('',#11014,10.) ;
#3080 = VECTOR('',#11015,10.) ;
#3081 = VECTOR('',#11018,10.) ;
#3082 = VECTOR('',#11019,10.) ;
#3083 = VECTOR('',#11020,10.) ;
#3084 = VECTOR('',#11023,10.) ;
#3085 = VECTOR('',#11028,10.) ;
#3086 = VECTOR('',#11029,10.) ;
#3087 = VECTOR('',#11030,10.) ;
#3088 = VECTOR('',#11033,10.) ;
#3089 = VECTOR('',#11034,10.) ;
#3090 = VECTOR('',#11035,10.) ;
#3091 = VECTOR('',#11038,10.) ;
#3092 = VECTOR('',#11043,10.) ;
#3093 = VECTOR('',#11044,10.) ;
#3094 = VECTOR('',#11045,10.) ;
#3095 = VECTOR('',#11048,10.) ;
#3096 = VECTOR('',#11049,10.) ;
#3097 = VECTOR('',#11050,10.) ;
#3098 = VECTOR('',#11053,10.) ;
#3099 = VECTOR('',#11058,10.) ;
#3100 = VECTOR('',#11059,10.) ;
#3101 = VECTOR('',#11060,10.) ;
#3102 = VECTOR('',#11063,10.) ;
#3103 = VECTOR('',#11064,10.) ;
#3104 = VECTOR('',#11065,10.) ;
#3105 = VECTOR('',#11068,10.) ;
#3106 = VECTOR('',#11073,10.) ;
#3107 = VECTOR('',#11074,10.) ;
#3108 = VECTOR('',#11075,10.) ;
#3109 = VECTOR('',#11078,10.) ;
#3110 = VECTOR('',#11079,10.) ;
#3111 = VECTOR('',#11080,10.) ;
#3112 = VECTOR('',#11083,10.) ;
#3113 = VECTOR('',#11088,10.) ;
#3114 = VECTOR('',#11089,10.) ;
#3115 = VECTOR('',#11090,10.) ;
#3116 = VECTOR('',#11093,10.) ;
#3117 = VECTOR('',#11094,10.) ;
#3118 = VECTOR('',#11095,10.) ;
#3119 = VECTOR('',#11098,10.) ;
#3120 = VECTOR('',#11103,10.) ;
#3121 = VECTOR('',#11104,10.) ;
#3122 = VECTOR('',#11105,10.) ;
#3123 = VECTOR('',#11108,10.) ;
#3124 = VECTOR('',#11109,10.) ;
#3125 = VECTOR('',#11110,10.) ;
#3126 = VECTOR('',#11113,10.) ;
#3127 = VECTOR('',#11118,10.) ;
#3128 = VECTOR('',#11119,10.) ;
#3129 = VECTOR('',#11120,10.) ;
#3130 = VECTOR('',#11123,10.) ;
#3131 = VECTOR('',#11124,10.) ;
#3132 = VECTOR('',#11125,10.) ;
#3133 = VECTOR('',#11128,10.) ;
#3134 = VECTOR('',#11133,10.) ;
#3135 = VECTOR('',#11134,10.) ;
#3136 = VECTOR('',#11135,10.) ;
#3137 = VECTOR('',#11138,10.) ;
#3138 = VECTOR('',#11139,10.) ;
#3139 = VECTOR('',#11140,10.) ;
#3140 = VECTOR('',#11143,10.) ;
#3141 = VECTOR('',#11148,10.) ;
#3142 = VECTOR('',#11149,10.) ;
#3143 = VECTOR('',#11150,10.) ;
#3144 = VECTOR('',#11153,10.) ;
#3145 = VECTOR('',#11154,10.) ;
#3146 = VECTOR('',#11155,10.) ;
#3147 = VECTOR('',#11158,10.) ;
#3148 = VECTOR('',#11163,10.) ;
#3149 = VECTOR('',#11164,10.) ;
#3150 = VECTOR('',#11165,10.) ;
#3151 = VECTOR('',#11168,10.) ;
#3152 = VECTOR('',#11169,10.) ;
#3153 = VECTOR('',#11170,10.) ;
#3154 = VECTOR('',#11173,10.) ;
#3155 = VECTOR('',#11178,10.) ;
#3156 = VECTOR('',#11179,10.) ;
#3157 = VECTOR('',#11180,10.) ;
#3158 = VECTOR('',#11183,10.) ;
#3159 = VECTOR('',#11184,10.) ;
#3160 = VECTOR('',#11185,10.) ;
#3161 = VECTOR('',#11188,10.) ;
#3162 = VECTOR('',#11193,10.) ;
#3163 = VECTOR('',#11194,10.) ;
#3164 = VECTOR('',#11195,10.) ;
#3165 = VECTOR('',#11198,10.) ;
#3166 = VECTOR('',#11199,10.) ;
#3167 = VECTOR('',#11200,10.) ;
#3168 = VECTOR('',#11203,10.) ;
#3169 = VECTOR('',#11208,10.) ;
#3170 = VECTOR('',#11209,10.) ;
#3171 = VECTOR('',#11210,10.) ;
#3172 = VECTOR('',#11213,10.) ;
#3173 = VECTOR('',#11214,10.) ;
#3174 = VECTOR('',#11215,10.) ;
#3175 = VECTOR('',#11218,10.) ;
#3176 = VECTOR('',#11223,10.) ;
#3177 = VECTOR('',#11224,10.) ;
#3178 = VECTOR('',#11225,10.) ;
#3179 = VECTOR('',#11228,10.) ;
#3180 = VECTOR('',#11229,10.) ;
#3181 = VECTOR('',#11230,10.) ;
#3182 = VECTOR('',#11233,10.) ;
#3183 = VECTOR('',#11238,10.) ;
#3184 = VECTOR('',#11239,10.) ;
#3185 = VECTOR('',#11240,10.) ;
#3186 = VECTOR('',#11243,10.) ;
#3187 = VECTOR('',#11244,10.) ;
#3188 = VECTOR('',#11245,10.) ;
#3189 = VECTOR('',#11248,10.) ;
#3190 = VECTOR('',#11253,10.) ;
#3191 = VECTOR('',#11254,10.) ;
#3192 = VECTOR('',#11255,10.) ;
#3193 = VECTOR('',#11258,10.) ;
#3194 = VECTOR('',#11259,10.) ;
#3195 = VECTOR('',#11260,10.) ;
#3196 = VECTOR('',#11263,10.) ;
#3197 = VECTOR('',#11268,10.) ;
#3198 = VECTOR('',#11269,10.) ;
#3199 = VECTOR('',#11270,10.) ;
#3200 = VECTOR('',#11273,10.) ;
#3201 = VECTOR('',#11274,10.) ;
#3202 = VECTOR('',#11275,10.) ;
#3203 = VECTOR('',#11278,10.) ;
#3204 = VECTOR('',#11283,10.) ;
#3205 = VECTOR('',#11284,10.) ;
#3206 = VECTOR('',#11287,10.) ;
#3207 = VECTOR('',#11294,10.) ;
#3208 = VECTOR('',#11303,10.) ;
#3209 = VECTOR('',#11310,10.) ;
#3210 = VECTOR('',#11317,10.) ;
#3211 = VECTOR('',#11324,10.) ;
#3212 = VECTOR('',#11331,10.) ;
#3213 = VECTOR('',#11338,10.) ;
#3214 = VECTOR('',#11345,10.) ;
#3215 = VECTOR('',#11352,10.) ;
#3216 = VECTOR('',#11365,10.) ;
#3217 = VECTOR('',#11368,10.) ;
#3218 = VECTOR('',#11373,10.) ;
#3219 = VECTOR('',#11376,10.) ;
#3220 = VECTOR('',#11377,10.) ;
#3221 = VECTOR('',#11382,10.) ;
#3222 = VECTOR('',#11387,10.) ;
#3223 = VECTOR('',#11392,10.) ;
#3224 = VECTOR('',#11395,10.) ;
#3225 = VECTOR('',#11396,10.) ;
#3226 = VECTOR('',#11405,8.00000000000007) ;
#3227 = VECTOR('',#11408,10.) ;
#3228 = VECTOR('',#11411,10.) ;
#3229 = VECTOR('',#11416,10.) ;
#3230 = VECTOR('',#11419,10.) ;
#3231 = VECTOR('',#11420,10.) ;
#3232 = VECTOR('',#11425,10.) ;
#3233 = VECTOR('',#11430,10.) ;
#3234 = VECTOR('',#11435,10.) ;
#3235 = VECTOR('',#11438,10.) ;
#3236 = VECTOR('',#11439,10.) ;
#3237 = VECTOR('',#11446,10.) ;
#3238 = VECTOR('',#11449,10.) ;
#3239 = VECTOR('',#11454,10.) ;
#3240 = VECTOR('',#11457,10.) ;
#3241 = VECTOR('',#11458,10.) ;
#3242 = VECTOR('',#11463,10.) ;
#3243 = VECTOR('',#11468,10.) ;
#3244 = VECTOR('',#11473,10.) ;
#3245 = VECTOR('',#11476,10.) ;
#3246 = VECTOR('',#11477,10.) ;
#3247 = VECTOR('',#11484,10.) ;
#3248 = VECTOR('',#11487,10.) ;
#3249 = VECTOR('',#11492,10.) ;
#3250 = VECTOR('',#11495,10.) ;
#3251 = VECTOR('',#11496,10.) ;
#3252 = VECTOR('',#11501,10.) ;
#3253 = VECTOR('',#11506,10.) ;
#3254 = VECTOR('',#11511,10.) ;
#3255 = VECTOR('',#11514,10.) ;
#3256 = VECTOR('',#11515,10.) ;
#3257 = VECTOR('',#11522,10.) ;
#3258 = VECTOR('',#11525,10.) ;
#3259 = VECTOR('',#11530,10.) ;
#3260 = VECTOR('',#11533,10.) ;
#3261 = VECTOR('',#11534,10.) ;
#3262 = VECTOR('',#11539,10.) ;
#3263 = VECTOR('',#11544,10.) ;
#3264 = VECTOR('',#11549,10.) ;
#3265 = VECTOR('',#11552,10.) ;
#3266 = VECTOR('',#11553,10.) ;
#3267 = VECTOR('',#11560,83.314636823702) ;
#3268 = VECTOR('',#11567,81.1146368237021) ;
#3269 = B_SPLINE_CURVE_WITH_KNOTS('',3,(#11581,#11582,#11583,#11584,#11585,
#11586,#11587,#11588,#11589,#11590,#11591,#11592,#11593,#11594,#11595,#11596,
#11597,#11598,#11599,#11600,#11601,#11602,#11603,#11604,#11605,#11606,#11607,
#11608,#11609,#11610,#11611,#11612,#11613,#11614,#11615,#11616,#11617,#11618,
#11619,#11620,#11621,#11622,#11623,#11624,#11625,#11626,#11627,#11628,#11629,
#11630,#11631,#11632,#11633,#11634,#11635,#11636,#11637,#11638,#11639,#11640,
#11641,#11642,#11643,#11644,#11645,#11646,#11647,#11648,#11649,#11650),
 .UNSPECIFIED.,.F.,.F.,(4,3,3,3,3,3,3,3,3,3,3,3,3,3,3,3,3,3,3,3,3,3,3,4),
(0.,0.0793197138435201,0.158771385884217,0.238558484111915,0.306313523372651,
0.403832448656896,0.433069184072941,0.511729267835096,0.590263878581832,
0.613631069879533,0.690390876330624,0.707969844415473,0.800502285413489,
0.876862882016797,0.95333936184816,0.982878828682618,1.06189090503122,1.14078623960736,
1.21960243454601,1.29840986633391,1.32860366242735,1.39861936931628,1.41593872955056,
1.41596897684906),.UNSPECIFIED.) ;
#3270 = B_SPLINE_CURVE_WITH_KNOTS('',3,(#11654,#11655,#11656,#11657,#11658,
#11659,#11660,#11661,#11662,#11663,#11664,#11665,#11666,#11667,#11668,#11669,
#11670,#11671,#11672,#11673,#11674,#11675,#11676,#11677,#11678,#11679,#11680,
#11681,#11682,#11683,#11684,#11685,#11686,#11687,#11688,#11689,#11690,#11691,
#11692,#11693,#11694,#11695,#11696,#11697,#11698,#11699,#11700,#11701,#11702,
#11703,#11704,#11705,#11706,#11707,#11708,#11709,#11710,#11711,#11712,#11713,
#11714,#11715,#11716,#11717),.UNSPECIFIED.,.F.,.F.,(4,3,3,3,3,3,3,3,3,3,
3,3,3,3,3,3,3,3,3,3,3,4),(1.41596880340121,1.49262148871634,1.5668573581781,
1.64471845141992,1.72257954466174,1.80445466514378,1.84900113443533,1.92515260613569,
2.0012049728828,2.03137767770577,2.12391011870702,2.19942692290802,2.21824889324341,
2.29711576720828,2.37613469075668,2.39881077905672,2.48964910629467,2.58046623905025,
2.67010886019969,2.72490396964329,2.79646171749926,2.83187996310763),
 .UNSPECIFIED.) ;
#3271 = B_SPLINE_CURVE_WITH_KNOTS('',3,(#11718,#11719,#11720,#11721,#11722,
#11723,#11724,#11725,#11726,#11727,#11728,#11729,#11730,#11731,#11732,#11733,
#11734,#11735,#11736,#11737,#11738,#11739,#11740,#11741,#11742,#11743,#11744,
#11745,#11746,#11747,#11748,#11749,#11750,#11751,#11752,#11753,#11754,#11755,
#11756,#11757,#11758,#11759,#11760,#11761,#11762,#11763,#11764,#11765,#11766,
#11767,#11768,#11769,#11770,#11771,#11772,#11773,#11774,#11775,#11776,#11777,
#11778,#11779,#11780,#11781,#11782,#11783,#11784,#11785,#11786,#11787),
 .UNSPECIFIED.,.F.,.F.,(4,3,3,3,3,3,3,3,3,3,3,3,3,3,3,3,3,3,3,3,3,3,3,4),
(0.,0.0793133374912053,0.158758235390486,0.238538175205765,0.306301524869595,
0.403803180865383,0.433059753999551,0.511690783685005,0.590197964800243,
0.615437173415573,0.692151852374993,0.707970137120889,0.802309447772199,
0.878720775265787,0.955248849211538,0.982872196325326,1.06188787249591,
1.14078682148802,1.21960661441308,1.2984175189742,1.32858362623266,1.39860014615873,
1.41594123358707,1.41596880340121),.UNSPECIFIED.) ;
#3272 = B_SPLINE_CURVE_WITH_KNOTS('',3,(#11788,#11789,#11790,#11791,#11792,
#11793,#11794,#11795,#11796,#11797,#11798,#11799,#11800,#11801,#11802,#11803,
#11804,#11805,#11806,#11807,#11808,#11809,#11810,#11811,#11812,#11813,#11814,
#11815,#11816,#11817,#11818,#11819,#11820,#11821,#11822,#11823,#11824,#11825,
#11826,#11827,#11828,#11829,#11830,#11831,#11832,#11833,#11834,#11835,#11836,
#11837,#11838,#11839,#11840,#11841,#11842,#11843,#11844,#11845,#11846,#11847,
#11848,#11849,#11850,#11851),.UNSPECIFIED.,.F.,.F.,(4,3,3,3,3,3,3,3,3,3,
3,3,3,3,3,3,3,3,3,3,3,4),(1.41596897684906,1.49265653903016,1.56689293584109,
1.64480608070727,1.72271922557345,1.80458348138907,1.84899944094778,1.92515534328894,
2.0012121330888,2.03137686036412,2.12390982409441,2.19935680708818,2.21644278782049,
2.2952634447841,2.37423511805567,2.39882020722706,2.48964792234117,2.58045374598227,
2.6700867011423,2.72489655815223,2.79645311316558,2.83187996119986),
 .UNSPECIFIED.) ;
#3273 = B_SPLINE_CURVE_WITH_KNOTS('',3,(#11855,#11856,#11857,#11858,#11859,
#11860,#11861,#11862,#11863,#11864,#11865,#11866,#11867,#11868,#11869,#11870,
#11871,#11872,#11873,#11874,#11875,#11876,#11877,#11878,#11879,#11880,#11881,
#11882,#11883,#11884,#11885,#11886,#11887,#11888,#11889,#11890,#11891,#11892,
#11893,#11894,#11895,#11896,#11897,#11898,#11899,#11900,#11901,#11902,#11903,
#11904,#11905,#11906,#11907,#11908,#11909,#11910,#11911,#11912,#11913,#11914,
#11915,#11916,#11917,#11918,#11919,#11920,#11921,#11922,#11923,#11924),
 .UNSPECIFIED.,.F.,.F.,(4,3,3,3,3,3,3,3,3,3,3,3,3,3,3,3,3,3,3,3,3,3,3,4),
(0.,0.0793133370868211,0.158758234556949,0.238538173913318,0.306301520321067,
0.403803175477182,0.433059753978827,0.511690783698259,0.590197964845532,
0.615437173388124,0.692151852363811,0.707970137104854,0.802309447755686,
0.87872077528125,0.955248849259362,0.982872196316439,1.06188787193309,1.14078682038421,
1.21960661277611,1.29841751684233,1.32858364651257,1.39860016603356,1.41594123355621,
1.41596880335427),.UNSPECIFIED.) ;
#3274 = B_SPLINE_CURVE_WITH_KNOTS('',3,(#11928,#11929,#11930,#11931,#11932,
#11933,#11934,#11935,#11936,#11937,#11938,#11939,#11940,#11941,#11942,#11943,
#11944,#11945,#11946,#11947,#11948,#11949,#11950,#11951,#11952,#11953,#11954,
#11955,#11956,#11957,#11958,#11959,#11960,#11961,#11962,#11963,#11964,#11965,
#11966,#11967,#11968,#11969,#11970,#11971,#11972,#11973,#11974,#11975,#11976,
#11977,#11978,#11979,#11980,#11981,#11982,#11983,#11984,#11985,#11986,#11987,
#11988,#11989,#11990,#11991),.UNSPECIFIED.,.F.,.F.,(4,3,3,3,3,3,3,3,3,3,
3,3,3,3,3,3,3,3,3,3,3,4),(1.41596956338659,1.49266311646134,1.56690058990888,
1.64482218279723,1.72274377568557,1.80460850560754,1.849007766784,1.92524484137593,
2.00137969415775,2.02957051533547,2.12390982598676,2.19939955812894,2.21644278969928,
2.29526521978404,2.37423861455297,2.39882020911001,2.48964647817264,2.58045077014705,
2.67008242771561,2.72489376468843,2.79645019556297,2.83187996310763),
 .UNSPECIFIED.) ;
#3275 = B_SPLINE_CURVE_WITH_KNOTS('',3,(#11992,#11993,#11994,#11995,#11996,
#11997,#11998,#11999,#12000,#12001,#12002,#12003,#12004,#12005,#12006,#12007,
#12008,#12009,#12010,#12011,#12012,#12013,#12014,#12015,#12016,#12017,#12018,
#12019,#12020,#12021,#12022,#12023,#12024,#12025,#12026,#12027,#12028,#12029,
#12030,#12031,#12032,#12033,#12034,#12035,#12036,#12037,#12038,#12039,#12040,
#12041,#12042,#12043,#12044,#12045,#12046,#12047,#12048,#12049,#12050,#12051,
#12052,#12053,#12054,#12055,#12056,#12057,#12058,#12059,#12060,#12061),
 .UNSPECIFIED.,.F.,.F.,(4,3,3,3,3,3,3,3,3,3,3,3,3,3,3,3,3,3,3,3,3,3,3,4),
(0.,0.0793198911693566,0.158771759312593,0.238559074159999,0.306312735619829,
0.403832566518769,0.433069184052406,0.511730463050406,0.590266238023745,
0.61363106986425,0.690383033927815,0.707969844400602,0.800502285411225,
0.876854197724648,0.953321820846053,0.982878828678875,1.06189673932164,
1.14079797822371,1.21962007756801,1.29843326555185,1.32859538269108,1.3986125617673,
1.41593872952055,1.41596956338659),.UNSPECIFIED.) ;
#3276 = B_SPLINE_CURVE_WITH_KNOTS('',3,(#12062,#12063,#12064,#12065,#12066,
#12067,#12068,#12069,#12070,#12071,#12072,#12073,#12074,#12075,#12076,#12077,
#12078,#12079,#12080,#12081,#12082,#12083,#12084,#12085,#12086,#12087,#12088,
#12089,#12090,#12091,#12092,#12093,#12094,#12095,#12096,#12097,#12098,#12099,
#12100,#12101,#12102,#12103,#12104,#12105,#12106,#12107,#12108,#12109,#12110,
#12111,#12112,#12113,#12114,#12115,#12116,#12117,#12118,#12119,#12120,#12121,
#12122,#12123,#12124,#12125),.UNSPECIFIED.,.F.,.F.,(4,3,3,3,3,3,3,3,3,3,
3,3,3,3,3,3,3,3,3,3,3,4),(1.41596880335427,1.49262163677989,1.56685751827755,
1.64471882766714,1.72258013705673,1.80445525976957,1.84900113442618,1.92515260611125,
2.00120497284308,2.03137767770062,2.12391011869139,2.19942692303724,2.21824889322736,
2.29711576705383,2.37613469046074,2.39881077903564,2.48964909647063,2.58046621914314,
2.67010883124273,2.72490414691485,2.79646188868388,2.83187996310738),
 .UNSPECIFIED.) ;
#3277 = B_SPLINE_CURVE_WITH_KNOTS('',3,(#12158,#12159,#12160,#12161,#12162,
#12163,#12164,#12165,#12166,#12167,#12168,#12169,#12170,#12171,#12172),
 .UNSPECIFIED.,.T.,.F.,(4,1,1,1,1,1,1,1,1,1,1,1,4),(0.,0.433069184072941,
0.613631069879533,0.707969844415473,0.800502285413489,0.982878828682618,
1.41593872955056,1.84899944094778,2.03137686036412,2.12390982409441,2.21644278782049,
2.39882020722706,2.83187996119986),.UNSPECIFIED.) ;
#3278 = B_SPLINE_CURVE_WITH_KNOTS('',3,(#12205,#12206,#12207,#12208,#12209,
#12210,#12211,#12212,#12213,#12214,#12215,#12216,#12217,#12218,#12219),
 .UNSPECIFIED.,.T.,.F.,(4,1,1,1,1,1,1,1,1,1,1,1,4),(0.,0.433059753999551,
0.615437173415573,0.707970137120889,0.802309447772199,0.982872196325326,
1.41594123358707,1.84900113443533,2.03137767770577,2.12391011870702,2.21824889324341,
2.39881077905672,2.83187996310763),.UNSPECIFIED.) ;
#3279 = B_SPLINE_CURVE_WITH_KNOTS('',3,(#12252,#12253,#12254,#12255,#12256,
#12257,#12258,#12259,#12260,#12261,#12262,#12263,#12264,#12265,#12266),
 .UNSPECIFIED.,.T.,.F.,(4,1,1,1,1,1,1,1,1,1,1,1,4),(0.,0.433059753978827,
0.615437173388124,0.707970137104854,0.802309447755686,0.982872196316439,
1.41594123355621,1.84900113442618,2.03137767770062,2.12391011869139,2.21824889322736,
2.39881077903564,2.83187996310738),.UNSPECIFIED.) ;
#3280 = B_SPLINE_CURVE_WITH_KNOTS('',3,(#12299,#12300,#12301,#12302,#12303,
#12304,#12305,#12306,#12307,#12308,#12309,#12310,#12311,#12312,#12313),
 .UNSPECIFIED.,.T.,.F.,(4,1,1,1,1,1,1,1,1,1,1,1,4),(0.,0.433069184052406,
0.61363106986425,0.707969844400602,0.800502285411225,0.982878828678875,
1.41593872952055,1.849007766784,2.02957051533547,2.12390982598676,2.21644278969928,
2.39882020911001,2.83187996310763),.UNSPECIFIED.) ;
#3281 = B_SPLINE_CURVE_WITH_KNOTS('',3,(#12322,#12323,#12324,#12325,#12326,
#12327,#12328,#12329,#12330,#12331,#12332,#12333,#12334,#12335,#12336,#12337,
#12338,#12339,#12340),.UNSPECIFIED.,.T.,.F.,(4,1,1,1,1,1,1,1,1,1,1,1,1,
1,1,1,4),(0.,1.11916410687735,2.23832821375471,3.35749232063191,4.47665642750911,
5.59582053438647,6.71498464126383,7.83414874814102,8.95331285501821,10.0724769618908,
11.1916410687635,12.3108051756408,13.4299692825182,14.5491333893954,15.6682974962725,
16.7874616031499,17.9066257100273),.UNSPECIFIED.) ;
#3282 = B_SPLINE_CURVE_WITH_KNOTS('',3,(#12343,#12344,#12345,#12346,#12347,
#12348,#12349,#12350,#12351,#12352,#12353,#12354,#12355,#12356,#12357,#12358,
#12359,#12360,#12361),.UNSPECIFIED.,.T.,.F.,(4,1,1,1,1,1,1,1,1,1,1,1,1,
1,1,1,4),(0.,1.11916410687736,2.23832821375472,3.35749232063194,4.47665642750915,
5.5958205343865,6.71498464126385,7.83414874813648,8.95331285500911,10.0724769618863,
11.1916410687635,12.3108051756408,13.4299692825181,14.5491333893953,15.6682974962725,
16.7874616031499,17.9066257100273),.UNSPECIFIED.) ;
#3283 = B_SPLINE_CURVE_WITH_KNOTS('',3,(#12445,#12446,#12447,#12448,#12449,
#12450,#12451,#12452,#12453,#12454,#12455,#12456,#12457,#12458,#12459,#12460,
#12461,#12462,#12463,#12464,#12465,#12466,#12467,#12468,#12469,#12470,#12471,
#12472,#12473,#12474,#12475,#12476,#12477,#12478,#12479,#12480,#12481,#12482,
#12483,#12484,#12485,#12486,#12487,#12488,#12489,#12490,#12491,#12492,#12493,
#12494,#12495,#12496,#12497,#12498,#12499,#12500,#12501,#12502,#12503,#12504,
#12505,#12506,#12507,#12508,#12509,#12510,#12511),.UNSPECIFIED.,.F.,.F.,
(4,3,3,3,3,3,3,3,3,3,3,3,3,3,3,3,3,3,3,3,3,3,4),(3.9356112509829,4.03938538435145,
4.25784115129902,4.47513630847502,4.69377120659221,4.91046481666321,4.91951265349917,
5.12906709974552,5.34636177928887,5.56439507544428,5.78215798493518,5.90340082783371,
5.99918563324319,6.21796471286197,6.43674372019706,6.6534047490877,6.87204193031312,
6.88730285777762,7.08914731456076,7.30660608033134,7.52524368403693,7.7424025902883,
7.87117652775501),.UNSPECIFIED.) ;
#3284 = B_SPLINE_CURVE_WITH_KNOTS('',3,(#12513,#12514,#12515,#12516,#12517,
#12518,#12519,#12520,#12521,#12522),.UNSPECIFIED.,.F.,.F.,(4,2,2,2,4),(-0.0222585247231994,
-0.013985790625096,-0.011129717560957,-0.00783049479114727,-1.0000000337726E-6),
 .UNSPECIFIED.) ;
#3285 = B_SPLINE_CURVE_WITH_KNOTS('',3,(#12526,#12527,#12528,#12529,#12530,
#12531,#12532,#12533,#12534,#12535,#12536,#12537,#12538,#12539,#12540,#12541,
#12542,#12543,#12544,#12545,#12546,#12547,#12548,#12549,#12550,#12551,#12552,
#12553,#12554,#12555,#12556,#12557,#12558,#12559,#12560,#12561,#12562,#12563,
#12564,#12565,#12566,#12567,#12568,#12569,#12570,#12571,#12572,#12573,#12574,
#12575,#12576,#12577,#12578,#12579,#12580,#12581,#12582,#12583,#12584,#12585,
#12586,#12587,#12588,#12589,#12590,#12591,#12592,#12593,#12594,#12595,#12596,
#12597,#12598,#12599,#12600,#12601,#12602,#12603,#12604,#12605,#12606,#12607,
#12608,#12609,#12610,#12611,#12612,#12613,#12614,#12615,#12616,#12617,#12618,
#12619,#12620,#12621,#12622,#12623,#12624,#12625,#12626,#12627,#12628,#12629,
#12630,#12631,#12632,#12633,#12634,#12635,#12636,#12637,#12638,#12639),
 .UNSPECIFIED.,.F.,.F.,(4,2,2,2,2,2,2,2,2,2,2,2,2,2,2,2,2,2,2,2,2,2,2,2,
2,2,2,2,2,2,2,2,2,2,2,2,2,2,2,2,2,2,2,2,2,2,2,2,2,2,2,2,2,2,2,2,4),(-0.153462776225972,
-0.152324705127337,-0.151118454999884,-0.149333742371031,-0.145003214516893,
-0.13835659712187,-0.133835373411754,-0.132745313227134,-0.131847384401116,
-0.13097205154426,-0.129823508837882,-0.127628091775407,-0.119960423600932,
-0.115469114271048,-0.113272377032872,-0.111856947000151,-0.110720541727474,
-0.109751593502618,-0.108578093950052,-0.106442248036253,-0.0998082973084651,
-0.0941484535210442,-0.0917783941701622,-0.0915983015956296,-0.091502767009933,
-0.0913135982719603,-0.0911645589693218,-0.0910481152418994,-0.090957691313955,
-0.0908877816714908,-0.0894531021162402,-0.0883725557521577,-0.0873006436271552,
-0.0858223201796501,-0.0808094581085911,-0.0767363546008492,-0.0716521834197286,
-0.0692343146257553,-0.0676572673759575,-0.0657419763951433,-0.0633985116058406,
-0.0593409392751851,-0.0518183669518645,-0.0482968499863042,-0.0448444812234441,
-0.0386199857778131,-0.035642628427599,-0.0334832603615144,-0.0314977259350848,
-0.0263932638373145,-0.0225987907781864,-0.0202713898632133,-0.0181006589461003,
-0.0127737986074514,-0.00352391886801092,-0.00160881093620446,-1.00000000588518E-6),
 .UNSPECIFIED.) ;
#3286 = B_SPLINE_CURVE_WITH_KNOTS('',3,(#12640,#12641,#12642,#12643,#12644,
#12645,#12646,#12647,#12648,#12649,#12650,#12651,#12652,#12653,#12654,#12655,
#12656,#12657,#12658,#12659,#12660,#12661,#12662,#12663,#12664,#12665,#12666,
#12667,#12668,#12669,#12670,#12671,#12672,#12673,#12674,#12675,#12676,#12677,
#12678,#12679,#12680,#12681,#12682,#12683,#12684,#12685,#12686,#12687,#12688,
#12689,#12690,#12691,#12692,#12693,#12694,#12695,#12696,#12697,#12698,#12699,
#12700,#12701,#12702,#12703,#12704,#12705,#12706),.UNSPECIFIED.,.F.,.F.,
(4,3,3,3,3,3,3,3,3,3,3,3,3,3,3,3,3,3,3,3,3,3,4),(0.,0.0975869658197039,
0.316224629921226,0.533974482508371,0.751791450250512,0.970571090053128,
0.983904149333616,1.18687637804593,1.40551330231184,1.62363563448458,1.84012907539297,
1.967779663268,2.05856366171448,2.27719954675489,2.49400168139467,2.71263709677618,
2.93000716182069,2.9516727955564,3.1476956812641,3.36438759275314,3.58302233313812,
3.80139773207559,3.93553521981785),.UNSPECIFIED.) ;
#3287 = B_SPLINE_CURVE_WITH_KNOTS('',3,(#12712,#12713,#12714,#12715,#12716,
#12717,#12718,#12719,#12720,#12721,#12722,#12723,#12724,#12725,#12726,#12727,
#12728,#12729,#12730,#12731,#12732,#12733,#12734,#12735,#12736,#12737,#12738,
#12739,#12740,#12741,#12742,#12743,#12744,#12745,#12746,#12747,#12748,#12749,
#12750,#12751,#12752,#12753,#12754,#12755,#12756,#12757,#12758,#12759,#12760,
#12761,#12762,#12763,#12764,#12765,#12766,#12767,#12768,#12769,#12770,#12771,
#12772,#12773,#12774,#12775,#12776,#12777,#12778),.UNSPECIFIED.,.F.,.F.,
(4,3,3,3,3,3,3,3,3,3,3,3,3,3,3,3,3,3,3,3,3,3,4),(3.93547251278037,4.06961094858131,
4.28798638030629,4.50662115468534,4.72331312294551,4.91933700306806,4.94100170508307,
5.15837184749187,5.37700734464929,5.59380956446693,5.8124455505454,5.90323061785796,
6.03088023023819,6.24737376267269,6.46549619232503,6.6841331895427,6.88710479223812,
6.90043854814402,7.11921826246268,7.33703527512716,7.55478517165104,7.77342285580172,
7.87100799512254),.UNSPECIFIED.) ;
#3288 = B_SPLINE_CURVE_WITH_KNOTS('',3,(#12779,#12780,#12781,#12782,#12783,
#12784,#12785,#12786,#12787,#12788,#12789,#12790,#12791,#12792,#12793,#12794,
#12795,#12796,#12797,#12798,#12799,#12800,#12801,#12802,#12803,#12804,#12805,
#12806,#12807,#12808,#12809,#12810,#12811,#12812,#12813,#12814,#12815,#12816,
#12817,#12818,#12819,#12820,#12821,#12822,#12823,#12824,#12825,#12826,#12827,
#12828,#12829,#12830,#12831,#12832,#12833,#12834,#12835,#12836,#12837,#12838,
#12839,#12840,#12841,#12842,#12843,#12844,#12845),.UNSPECIFIED.,.F.,.F.,
(4,3,3,3,3,3,3,3,3,3,3,3,3,3,3,3,3,3,3,3,3,3,4),(4.35954652862245E-7,0.119372163261154,
0.337345459789608,0.555020195428233,0.772262251650588,0.983893434075418,
0.990873877762923,1.2084306792763,1.42706758547165,1.64356117973995,1.86123472757703,
1.96779535009552,2.07966351227983,2.29690397078676,2.51539695630481,2.73254404906778,
2.95093109100352,2.95170382931863,3.16941983526542,3.38648900257636,3.60512375286946,
3.82170107768877,3.9356112509829),.UNSPECIFIED.) ;
#3289 = B_SPLINE_CURVE_WITH_KNOTS('',3,(#12847,#12848,#12849,#12850,#12851,
#12852,#12853,#12854,#12855,#12856,#12857,#12858,#12859,#12860,#12861,#12862,
#12863,#12864,#12865,#12866,#12867,#12868,#12869,#12870,#12871,#12872,#12873,
#12874,#12875,#12876,#12877,#12878,#12879,#12880,#12881,#12882,#12883,#12884,
#12885,#12886,#12887,#12888,#12889,#12890,#12891,#12892,#12893,#12894,#12895,
#12896,#12897,#12898,#12899,#12900,#12901,#12902,#12903,#12904,#12905,#12906,
#12907,#12908,#12909,#12910,#12911,#12912,#12913),.UNSPECIFIED.,.F.,.F.,
(4,3,3,3,3,3,3,3,3,3,3,3,3,3,3,3,3,3,3,3,3,3,4),(3.93553521981785,4.0186166507456,
4.237394066808,4.45524637685516,4.67168228798332,4.89031731534065,4.91942511752289,
5.10777744143641,5.32641286545437,5.54365324976844,5.76132642843505,5.90327971137444,
5.97977375285268,6.19626741280715,6.41490412589105,6.6327957250643,6.85047016051711,
6.88716122923848,7.06685121073668,7.28548870358118,7.5039832238531,7.72224969150007,
7.87100730541593),.UNSPECIFIED.) ;
#3290 = B_SPLINE_CURVE_WITH_KNOTS('',3,(#12914,#12915,#12916,#12917,#12918,
#12919,#12920,#12921,#12922,#12923,#12924,#12925,#12926,#12927,#12928,#12929,
#12930,#12931,#12932,#12933,#12934,#12935,#12936,#12937,#12938,#12939,#12940,
#12941,#12942,#12943,#12944,#12945,#12946,#12947,#12948,#12949,#12950,#12951,
#12952,#12953,#12954,#12955,#12956,#12957,#12958,#12959,#12960,#12961,#12962,
#12963,#12964,#12965,#12966,#12967,#12968,#12969,#12970,#12971,#12972,#12973,
#12974,#12975,#12976,#12977,#12978,#12979,#12980),.UNSPECIFIED.,.F.,.F.,
(4,3,3,3,3,3,3,3,3,3,3,3,3,3,3,3,3,3,3,3,3,3,4),(0.,0.0677050049383632,
0.286200456928864,0.504838070208805,0.721642294535249,0.940279670301964,
0.983887911634322,1.15752095782385,1.37528509523392,1.59197913143046,1.81061559832354,
1.96772752945778,2.02908413902557,2.24679594232941,2.46337476541722,2.6820102099624,
2.89990017557006,2.95160837635821,3.11728168426501,3.33539505176439,3.55269408023814,
3.77118616997486,3.9354465321173),.UNSPECIFIED.) ;
#3291 = B_SPLINE_CURVE_WITH_KNOTS('',3,(#12986,#12987,#12988,#12989,#12990,
#12991,#12992,#12993,#12994,#12995,#12996,#12997,#12998,#12999,#13000,#13001,
#13002,#13003,#13004,#13005,#13006,#13007,#13008,#13009,#13010,#13011,#13012,
#13013,#13014,#13015,#13016,#13017,#13018,#13019,#13020,#13021,#13022,#13023,
#13024,#13025,#13026,#13027,#13028,#13029,#13030,#13031,#13032,#13033,#13034,
#13035,#13036,#13037,#13038,#13039,#13040,#13041,#13042,#13043,#13044,#13045,
#13046,#13047,#13048,#13049,#13050,#13051,#13052,#13053,#13054,#13055,#13056,
#13057,#13058,#13059,#13060,#13061,#13062,#13063,#13064,#13065,#13066,#13067,
#13068,#13069,#13070,#13071,#13072,#13073,#13074,#13075,#13076,#13077,#13078,
#13079,#13080,#13081,#13082,#13083,#13084,#13085,#13086,#13087,#13088,#13089,
#13090,#13091,#13092,#13093,#13094,#13095,#13096,#13097,#13098,#13099,#13100,
#13101,#13102,#13103,#13104,#13105,#13106,#13107,#13108,#13109,#13110,#13111,
#13112,#13113,#13114,#13115,#13116,#13117,#13118,#13119,#13120,#13121,#13122,
#13123,#13124,#13125,#13126,#13127,#13128,#13129,#13130,#13131,#13132,#13133,
#13134,#13135,#13136,#13137,#13138,#13139,#13140,#13141,#13142,#13143,#13144,
#13145,#13146,#13147,#13148,#13149,#13150,#13151,#13152,#13153,#13154,#13155,
#13156,#13157,#13158,#13159,#13160,#13161,#13162,#13163,#13164,#13165,#13166,
#13167,#13168,#13169,#13170,#13171,#13172,#13173,#13174,#13175,#13176,#13177,
#13178,#13179,#13180,#13181,#13182,#13183,#13184,#13185,#13186,#13187,#13188,
#13189,#13190,#13191,#13192,#13193,#13194,#13195,#13196,#13197,#13198,#13199,
#13200,#13201,#13202,#13203,#13204,#13205,#13206,#13207,#13208,#13209,#13210,
#13211,#13212,#13213,#13214,#13215,#13216,#13217,#13218,#13219,#13220,#13221,
#13222,#13223,#13224,#13225,#13226,#13227,#13228,#13229,#13230,#13231,#13232,
#13233,#13234,#13235,#13236,#13237,#13238,#13239,#13240,#13241,#13242,#13243,
#13244,#13245,#13246,#13247,#13248,#13249,#13250,#13251,#13252,#13253,#13254,
#13255,#13256,#13257,#13258,#13259,#13260,#13261,#13262,#13263,#13264,#13265,
#13266,#13267,#13268,#13269,#13270,#13271,#13272,#13273,#13274,#13275,#13276,
#13277,#13278,#13279,#13280,#13281,#13282,#13283,#13284,#13285,#13286,#13287,
#13288,#13289,#13290,#13291,#13292,#13293,#13294,#13295,#13296,#13297,#13298,
#13299,#13300,#13301,#13302,#13303,#13304,#13305,#13306,#13307,#13308,#13309,
#13310,#13311,#13312,#13313,#13314,#13315,#13316,#13317,#13318,#13319,#13320,
#13321,#13322,#13323,#13324,#13325,#13326,#13327,#13328,#13329,#13330,#13331,
#13332,#13333,#13334,#13335,#13336,#13337,#13338,#13339,#13340,#13341,#13342,
#13343,#13344,#13345,#13346,#13347,#13348,#13349,#13350,#13351,#13352,#13353,
#13354,#13355,#13356,#13357,#13358,#13359,#13360,#13361,#13362,#13363,#13364,
#13365,#13366,#13367,#13368,#13369,#13370,#13371,#13372,#13373,#13374,#13375,
#13376,#13377,#13378,#13379,#13380,#13381,#13382,#13383,#13384,#13385,#13386,
#13387,#13388,#13389,#13390,#13391,#13392,#13393,#13394,#13395,#13396,#13397,
#13398,#13399,#13400,#13401,#13402,#13403,#13404,#13405,#13406,#13407,#13408,
#13409,#13410,#13411,#13412,#13413,#13414,#13415,#13416,#13417,#13418,#13419,
#13420,#13421,#13422,#13423,#13424,#13425,#13426,#13427,#13428,#13429,#13430,
#13431,#13432,#13433,#13434,#13435,#13436,#13437,#13438,#13439,#13440,#13441,
#13442,#13443,#13444,#13445,#13446,#13447,#13448,#13449,#13450,#13451,#13452,
#13453,#13454,#13455,#13456,#13457,#13458,#13459,#13460,#13461,#13462,#13463,
#13464,#13465,#13466,#13467,#13468,#13469,#13470,#13471,#13472,#13473,#13474,
#13475,#13476,#13477,#13478,#13479,#13480,#13481,#13482,#13483,#13484,#13485,
#13486,#13487,#13488,#13489,#13490,#13491,#13492,#13493,#13494,#13495,#13496,
#13497,#13498,#13499,#13500,#13501,#13502,#13503,#13504,#13505,#13506,#13507,
#13508,#13509,#13510,#13511,#13512,#13513,#13514,#13515,#13516,#13517,#13518,
#13519,#13520,#13521,#13522,#13523,#13524,#13525,#13526,#13527,#13528,#13529,
#13530,#13531,#13532,#13533,#13534,#13535,#13536,#13537,#13538,#13539,#13540,
#13541,#13542,#13543,#13544,#13545),.UNSPECIFIED.,.F.,.F.,(4,2,2,2,2,2,
2,2,2,2,2,2,2,2,2,2,2,2,2,2,2,2,2,2,2,2,2,2,2,2,2,2,2,2,2,2,2,2,2,2,2,2,
2,2,2,2,2,2,2,2,2,2,2,2,2,2,2,2,2,2,2,2,2,2,2,2,2,2,2,2,2,2,2,2,2,2,2,2,
2,2,2,2,2,2,2,2,2,2,2,2,2,2,2,2,2,2,2,2,2,2,2,2,2,2,2,2,2,2,2,2,2,2,2,2,
2,2,2,2,2,2,2,2,2,2,2,2,2,2,2,2,2,2,2,2,2,2,2,2,2,2,2,2,2,2,2,2,2,2,2,2,
2,2,2,2,2,2,2,2,2,2,2,2,2,2,2,2,2,2,2,2,2,2,2,2,2,2,2,2,2,2,2,2,2,2,2,2,
2,2,2,2,2,2,2,2,2,2,2,2,2,2,2,2,2,2,2,2,2,2,2,2,2,2,2,2,2,2,2,2,2,2,2,2,
2,2,2,2,2,2,2,2,2,2,2,2,2,2,2,2,2,2,2,2,2,2,2,2,2,2,2,2,2,2,2,2,2,2,2,2,
2,2,2,2,2,2,2,2,2,2,2,2,2,2,2,2,2,2,2,2,2,4),(-0.393137881593438,-0.389064719683897,
-0.386009163097905,-0.385981265578937,-0.385945108836368,-0.385909794020154,
-0.385875282553561,-0.385841538154784,-0.385808526670231,-0.385776215945061,
-0.385744575643447,-0.385713577137668,-0.385683193419207,-0.385653398899929,
-0.385624169353304,-0.3855954818173,-0.385567314554562,-0.385539646925394,
-0.385512459300206,-0.38548573304274,-0.385459450436866,-0.385433594604264,
-0.385408149413348,-0.38538309950479,-0.385358430245372,-0.385334127660716,
-0.385310178392478,-0.385286569649997,-0.385263289186791,-0.385240325295512,
-0.385217666806629,-0.385195302950154,-0.385173223392286,-0.385151418221862,
-0.385129877964114,-0.38510859346962,-0.385087555927281,-0.38506675688553,
-0.382193288159145,-0.378643776553383,-0.372987032673473,-0.370532901093016,
-0.367420038226476,-0.365735167603049,-0.364371223425476,-0.362805195776009,
-0.360769131760525,-0.357030669202214,-0.347953392087648,-0.345637025624622,
-0.343909370054482,-0.343898550497168,-0.343887881487955,-0.343877358895261,
-0.343866978617838,-0.343856737143705,-0.343846630668866,-0.342404946987773,
-0.342399739837498,-0.340389768977736,-0.337225312112191,-0.328012436212014,
-0.325339571894854,-0.323238491998288,-0.321074407389107,-0.312876297699838,
-0.309143304068466,-0.305494730244086,-0.292360872563278,-0.287021783224246,
-0.278556287551638,-0.276295069825672,-0.273635629426088,-0.273603569246504,
-0.273571755268592,-0.273540177451555,-0.273508826072954,-0.27347769171537,
-0.273446765245543,-0.273416037711126,-0.2733855003582,-0.27335514473055,
-0.273324962374537,-0.273294945231453,-0.273265085345797,-0.273235374864648,
-0.273205806152832,-0.273176371752135,-0.273147064283172,-0.273117876550817,
-0.273088801554495,-0.270488295678629,-0.267434391112323,-0.260733533799063,
-0.258124972448113,-0.25665576277279,-0.255967011402266,-0.254691877630724,
-0.253222721618945,-0.250969687319429,-0.245996994877722,-0.244458155047862,
-0.238929481981041,-0.237109779149582,-0.23562893190682,-0.235114669270249,
-0.23510527824484,-0.235095943200605,-0.23508666243864,-0.235077434592277,
-0.235068258329171,-0.23505913223512,-0.235050054796457,-0.235041024921968,
-0.23503204133481,-0.235023102795624,-0.23501420791345,-0.233317826364142,
-0.231331108821098,-0.227772701309594,-0.218656615672096,-0.215977453808853,
-0.215758282067611,-0.215512652033937,-0.215205754365662,-0.214758261696359,
-0.213155418319634,-0.210596281508668,-0.207035169697749,-0.19705905462199,
-0.191068766209985,-0.186517849648799,-0.182774919494473,-0.176531897491971,
-0.171684381933814,-0.169802781088252,-0.168531950096097,-0.167101615381119,
-0.165419900551934,-0.162807962076873,-0.156713689775964,-0.151097233777737,
-0.149355284868497,-0.147974374870866,-0.146676446306276,-0.146662048893367,
-0.146647590455199,-0.146633067451535,-0.146618476015309,-0.146603812396323,
-0.146589072896078,-0.1465742536766,-0.146559350880369,-0.146544360644392,
-0.146529279061066,-0.146514102176747,-0.146498826032116,-0.146483446528305,
-0.145022506404609,-0.1428831304497,-0.138743236588388,-0.130193530613127,
-0.128000750207622,-0.126822307669245,-0.125989676753377,-0.125972568843055,
-0.125957448615906,-0.12594411680296,-0.125932386946588,-0.125922086452357,
-0.125907945915367,-0.12589422147439,-0.125880906743579,-0.125867995017865,
-0.125855479563493,-0.125843353406085,-0.125831609296632,-0.124545889979032,
-0.123054230407459,-0.120618083045251,-0.114738096948853,-0.109085202066367,
-0.106461472196433,-0.104957436840786,-0.103756569812449,-0.103727129216677,
-0.103698167169185,-0.103669631891777,-0.103641475317349,-0.103613652549213,
-0.103586121444439,-0.103558842369885,-0.103531777824728,-0.10350489215023,
-0.103478151347447,-0.103451522768268,-0.10342497499356,-0.103398477630204,
-0.103372001174486,-0.103345516866451,-0.103318996425612,-0.10329241209262,
-0.10326573648879,-0.103238942402091,-0.103212002790916,-0.103184890572307,
-0.103157578580833,-0.103130039536487,-0.103102245868264,-0.103074169644922,
-0.103045782494817,-0.103017055491307,-0.102987959086974,-0.102958463062207,
-0.101523800085531,-0.0994324376486281,-0.0955430038437078,-0.0911201356083864,
-0.0854236788472147,-0.0839197154323816,-0.0830250946066951,-0.0821241714122678,
-0.0821135781755158,-0.0821031876279128,-0.0820929993889011,-0.0820830128687592,
-0.082073227467589,-0.0820636423483411,-0.0820542568396713,-0.0820450699627639,
-0.0820360806242098,-0.0820272876877643,-0.0807182497594875,-0.0792099620321136,
-0.0764044814883249,-0.0661392203353249,-0.0637492916655484,-0.0624181589015095,
-0.0613871859981794,-0.0612864336191271,-0.0612080546638962,-0.0611437934676291,
-0.0610891162320329,-0.0610412637399253,-0.0609984305477696,-0.0609593679774651,
-0.060923172538446,-0.0608891645204566,-0.060856814182384,-0.0608256946310408,
-0.0607954502793569,-0.0607657749375909,-0.0607363960142241,-0.0607070623707868,
-0.0606775346441359,-0.0606475771504467,-0.0606169504604617,-0.0605854041988785,
-0.060552669831555,-0.060518452696715,-0.0596102459314531,-0.0578951459211566,
-0.0547051042139423,-0.0471683111335125,-0.0440718493941549,-0.0424328101440815,
-0.0407738146829186,-0.0385041307164526,-0.0355007232875941,-0.0296701859213648,
-0.0284423965395485,-0.0274091206939878,-0.0259781110431152,-0.0245484004838547,
-0.0188048286315949,-0.0164738907366568,-0.0146236725297017,-0.0128934667137873,
-0.0108113783584484,-1.00000004499279E-6),.UNSPECIFIED.) ;
#3292 = B_SPLINE_CURVE_WITH_KNOTS('',3,(#13546,#13547,#13548,#13549,#13550,
#13551,#13552,#13553,#13554,#13555,#13556,#13557,#13558,#13559,#13560,#13561,
#13562,#13563,#13564,#13565,#13566,#13567,#13568,#13569,#13570,#13571,#13572,
#13573,#13574,#13575,#13576,#13577,#13578,#13579,#13580,#13581,#13582,#13583,
#13584,#13585,#13586,#13587,#13588,#13589,#13590,#13591,#13592,#13593,#13594,
#13595,#13596,#13597,#13598,#13599,#13600,#13601,#13602,#13603,#13604,#13605,
#13606,#13607,#13608,#13609,#13610,#13611,#13612),.UNSPECIFIED.,.F.,.F.,
(4,3,3,3,3,3,3,3,3,3,3,3,3,3,3,3,3,3,3,3,3,3,4),(8.59967866152634E-7,0.148759741016015,
0.367026201262003,0.585520705308296,0.804158161069697,0.983846684918452,
1.02053917198305,1.23821355501075,1.45610509475366,1.67474173516512,1.89123532545487,
1.96773238352147,2.10968257916154,2.32735567819506,2.5445960047733,2.76323136417574,
2.95158227043394,2.98069144299397,3.19932642889525,3.41576230303415,3.63361460867738,
3.85239201540518,3.93547251278037),.UNSPECIFIED.) ;
#3293 = B_SPLINE_CURVE_WITH_KNOTS('',3,(#13614,#13615,#13616,#13617,#13618,
#13619,#13620,#13621,#13622,#13623,#13624,#13625,#13626,#13627,#13628,#13629,
#13630,#13631,#13632,#13633,#13634,#13635,#13636,#13637,#13638,#13639,#13640,
#13641,#13642,#13643,#13644,#13645,#13646,#13647,#13648,#13649,#13650,#13651,
#13652,#13653,#13654,#13655,#13656,#13657,#13658,#13659,#13660,#13661,#13662,
#13663,#13664,#13665,#13666,#13667,#13668,#13669,#13670,#13671,#13672,#13673,
#13674,#13675,#13676,#13677),.UNSPECIFIED.,.F.,.F.,(4,3,3,3,3,3,3,3,3,3,
3,3,3,3,3,3,3,3,3,3,3,4),(3.9354465321173,3.98915356100037,4.20712406009794,
4.42428050568497,4.64267699059911,4.91961240864166,5.07847247943613,5.35085269365423,
5.51424929699302,5.73192619675865,5.90507510819469,5.95042577873663,6.16906217982155,
6.37457560045768,6.38686811203847,6.65623297772514,6.82404441772877,6.89060319718431,
7.2601083892678,7.53715824562949,7.69704795638202,7.87704726288776),
 .UNSPECIFIED.) ;
#3294 = B_SPLINE_CURVE_WITH_KNOTS('',3,(#13678,#13679,#13680,#13681,#13682,
#13683,#13684,#13685,#13686,#13687,#13688,#13689,#13690,#13691,#13692,#13693,
#13694,#13695,#13696,#13697,#13698,#13699,#13700,#13701,#13702,#13703,#13704,
#13705,#13706,#13707,#13708,#13709,#13710,#13711,#13712,#13713,#13714,#13715,
#13716,#13717,#13718,#13719,#13720,#13721,#13722,#13723,#13724,#13725,#13726,
#13727,#13728,#13729,#13730,#13731,#13732,#13733,#13734,#13735,#13736,#13737,
#13738,#13739,#13740,#13741,#13742,#13743,#13744,#13745,#13746,#13747,#13748,
#13749,#13750,#13751,#13752,#13753,#13754,#13755,#13756,#13757,#13758,#13759,
#13760,#13761,#13762,#13763,#13764,#13765,#13766,#13767,#13768,#13769,#13770,
#13771,#13772,#13773,#13774,#13775,#13776,#13777,#13778,#13779,#13780,#13781,
#13782,#13783,#13784,#13785,#13786,#13787,#13788,#13789,#13790,#13791,#13792,
#13793,#13794,#13795,#13796,#13797,#13798,#13799,#13800,#13801,#13802,#13803,
#13804,#13805,#13806,#13807,#13808,#13809,#13810,#13811,#13812,#13813,#13814,
#13815,#13816,#13817,#13818,#13819,#13820,#13821,#13822,#13823,#13824,#13825,
#13826,#13827,#13828,#13829,#13830,#13831,#13832,#13833,#13834,#13835,#13836,
#13837,#13838,#13839,#13840,#13841,#13842,#13843,#13844,#13845,#13846,#13847,
#13848,#13849,#13850,#13851,#13852,#13853,#13854,#13855,#13856,#13857,#13858,
#13859,#13860,#13861,#13862,#13863,#13864,#13865,#13866,#13867,#13868,#13869,
#13870,#13871,#13872,#13873,#13874,#13875,#13876,#13877,#13878,#13879,#13880,
#13881,#13882,#13883,#13884,#13885,#13886,#13887,#13888,#13889,#13890,#13891,
#13892,#13893,#13894,#13895,#13896,#13897,#13898,#13899,#13900,#13901,#13902,
#13903,#13904,#13905,#13906,#13907,#13908,#13909,#13910,#13911,#13912,#13913,
#13914,#13915,#13916,#13917,#13918,#13919,#13920,#13921,#13922,#13923,#13924,
#13925,#13926,#13927,#13928,#13929,#13930,#13931,#13932,#13933,#13934,#13935,
#13936,#13937,#13938,#13939,#13940,#13941,#13942,#13943,#13944,#13945,#13946,
#13947,#13948,#13949,#13950,#13951),.UNSPECIFIED.,.F.,.F.,(4,2,2,2,2,2,
2,2,2,2,2,2,2,2,2,2,2,2,2,2,2,2,2,2,2,2,2,2,2,2,2,2,2,2,2,2,2,2,2,2,2,2,
2,2,2,2,2,2,2,2,2,2,2,2,2,2,2,2,2,2,2,2,2,2,2,2,2,2,2,2,2,2,2,2,2,2,2,2,
2,2,2,2,2,2,2,2,2,2,2,2,2,2,2,2,2,2,2,2,2,2,2,2,2,2,2,2,2,2,2,2,2,2,2,2,
2,2,2,2,2,2,2,2,2,2,2,2,2,2,2,2,2,2,2,2,2,2,4),(-0.78638743863695,-0.783865136144057,
-0.781227861189557,-0.775152455613647,-0.766097510440291,-0.764097187693509,
-0.762309586971155,-0.760388178638292,-0.750981145966468,-0.742556535881132,
-0.740397682240013,-0.738484603898096,-0.736428582945787,-0.733875728280658,
-0.720932434032318,-0.717090859955029,-0.713389531042879,-0.710543028580515,
-0.693217343571822,-0.684636960856421,-0.680602460523877,-0.677007808154327,
-0.672649036269041,-0.661361827188727,-0.657367118065297,-0.654995127670715,
-0.653194778532826,-0.651398773584184,-0.649592474131525,-0.646251677215004,
-0.633032827345746,-0.62900903821384,-0.625374040640956,-0.62420154344307,
-0.617366718673342,-0.604222248212363,-0.597956446250104,-0.593485626003035,
-0.590208461213278,-0.585652486573894,-0.579451808375542,-0.572217577000446,
-0.569040010266564,-0.567102499947043,-0.565627562365034,-0.564173918933921,
-0.562517093097831,-0.559749200122382,-0.547987375366625,-0.540992348486649,
-0.53597161103656,-0.531601371432412,-0.530959041091284,-0.524707311709599,
-0.515867392725084,-0.507259310520406,-0.491002889787648,-0.486333349667312,
-0.483720612002522,-0.481821745073192,-0.480034700172722,-0.478257691761641,
-0.47576159989498,-0.465424549016278,-0.460609133799591,-0.458532191954113,
-0.457272245676355,-0.457266970231644,-0.457261751543754,-0.457256589587902,
-0.457251483390092,-0.457246432456842,-0.457241436079759,-0.457236493736514,
-0.457231604579641,-0.4572267678496,-0.457221983074196,-0.457217249922691,
-0.457212567335756,-0.457207935019405,-0.457203352445893,-0.457198818836132,
-0.457194333613499,-0.457189896411029,-0.457185506733976,-0.457181163236356,
-0.457176865874477,-0.457172614534079,-0.457168408126551,-0.457164246157086,
-0.45716012841437,-0.45715605432794,-0.457152023024765,-0.457148034407447,
-0.457144087795822,-0.457140182898109,-0.457136319059025,-0.457132495711979,
-0.457128712683886,-0.457124969589037,-0.457121265258414,-0.457117599629425,
-0.457113972289284,-0.45711038266605,-0.457106830488197,-0.45710331530434,
-0.457099836483116,-0.457096393787484,-0.457092987007351,-0.457089615480539,
-0.457086278913952,-0.457082976598086,-0.457079708498414,-0.457076474003513,
-0.457073272275524,-0.457070103696024,-0.457066968019619,-0.457063864356098,
-0.457060791889488,-0.457057751060048,-0.457054740955454,-0.45705176175811,
-0.457047854051728,-0.456092813665629,-0.455001710574267,-0.45314295087414,
-0.446964288888894,-0.441277563909847,-0.437106277410539,-0.434669623740107,
-0.432822778663546,-0.430965724317635,-0.428823650941757,-0.425037202595733,
-0.408253975266002,-0.39869121832428,-0.393164256152506),.UNSPECIFIED.) ;
#3295 = B_SPLINE_CURVE_WITH_KNOTS('',3,(#13957,#13958,#13959,#13960,#13961,
#13962,#13963,#13964,#13965,#13966,#13967,#13968,#13969,#13970,#13971,#13972,
#13973,#13974,#13975,#13976,#13977,#13978,#13979,#13980,#13981,#13982,#13983,
#13984,#13985,#13986,#13987,#13988,#13989,#13990,#13991,#13992,#13993,#13994,
#13995,#13996,#13997,#13998,#13999,#14000,#14001,#14002,#14003,#14004,#14005,
#14006,#14007,#14008,#14009,#14010,#14011,#14012,#14013,#14014,#14015,#14016,
#14017,#14018,#14019,#14020,#14021,#14022,#14023,#14024,#14025,#14026,#14027,
#14028,#14029,#14030,#14031,#14032,#14033,#14034,#14035,#14036,#14037,#14038,
#14039,#14040,#14041,#14042,#14043,#14044,#14045,#14046,#14047,#14048,#14049,
#14050,#14051,#14052,#14053,#14054,#14055,#14056,#14057,#14058,#14059,#14060,
#14061,#14062,#14063,#14064,#14065,#14066,#14067,#14068,#14069,#14070,#14071,
#14072,#14073,#14074,#14075,#14076,#14077,#14078,#14079,#14080,#14081,#14082,
#14083,#14084,#14085,#14086,#14087,#14088,#14089,#14090,#14091,#14092,#14093,
#14094,#14095,#14096,#14097,#14098,#14099,#14100,#14101,#14102,#14103,#14104,
#14105,#14106,#14107,#14108,#14109,#14110,#14111,#14112,#14113,#14114,#14115,
#14116,#14117,#14118,#14119,#14120,#14121,#14122,#14123,#14124,#14125,#14126,
#14127,#14128,#14129,#14130,#14131,#14132,#14133,#14134,#14135,#14136,#14137,
#14138,#14139,#14140,#14141,#14142,#14143,#14144,#14145,#14146,#14147,#14148,
#14149,#14150,#14151,#14152,#14153,#14154,#14155,#14156,#14157,#14158,#14159,
#14160,#14161,#14162,#14163,#14164,#14165,#14166,#14167,#14168,#14169,#14170,
#14171,#14172,#14173,#14174,#14175,#14176,#14177,#14178,#14179,#14180,#14181,
#14182,#14183,#14184,#14185,#14186,#14187,#14188,#14189,#14190,#14191,#14192,
#14193,#14194,#14195,#14196,#14197,#14198,#14199,#14200,#14201,#14202,#14203,
#14204,#14205,#14206,#14207,#14208,#14209,#14210,#14211,#14212,#14213,#14214,
#14215,#14216,#14217,#14218,#14219,#14220,#14221,#14222,#14223,#14224,#14225,
#14226,#14227,#14228,#14229,#14230),.UNSPECIFIED.,.F.,.F.,(4,2,2,2,2,2,
2,2,2,2,2,2,2,2,2,2,2,2,2,2,2,2,2,2,2,2,2,2,2,2,2,2,2,2,2,2,2,2,2,2,2,2,
2,2,2,2,2,2,2,2,2,2,2,2,2,2,2,2,2,2,2,2,2,2,2,2,2,2,2,2,2,2,2,2,2,2,2,2,
2,2,2,2,2,2,2,2,2,2,2,2,2,2,2,2,2,2,2,2,2,2,2,2,2,2,2,2,2,2,2,2,2,2,2,2,
2,2,2,2,2,2,2,2,2,2,2,2,2,2,2,2,2,2,2,2,2,2,4),(-0.393155650627907,-0.387629727924683,
-0.378068230731882,-0.361287776199656,-0.357500578681126,-0.355358535505596,
-0.353501602296624,-0.351655080524313,-0.349219040259675,-0.345049209213823,
-0.33936278735035,-0.333183989104826,-0.331325463430025,-0.3302344953374,
-0.329279567659575,-0.329275660740877,-0.329272683216366,-0.329269675131916,
-0.32926663546163,-0.32926356446945,-0.329260461873318,-0.329257326950647,
-0.329254159310184,-0.329250959069278,-0.329247725451569,-0.32924445849536,
-0.329241157598115,-0.329237822001912,-0.329234451827529,-0.329231046267257,
-0.329227605084572,-0.329224127780796,-0.329220614096719,-0.329217063471653,
-0.329213475265059,-0.329209849357973,-0.329206185080382,-0.329202481745933,
-0.329198739421806,-0.329194957807482,-0.329191135890187,-0.329187273587689,
-0.329183370094182,-0.329179424994815,-0.329175437803989,-0.329171407809548,
-0.329167335082706,-0.329163219015704,-0.329159058468777,-0.329154853485093,
-0.329150603751954,-0.329146308354663,-0.329141966379954,-0.329137577978438,
-0.329133142276796,-0.329128658730507,-0.329124126752042,-0.329119546000515,
-0.329114915761884,-0.329110235079655,-0.329105503478469,-0.329100720530011,
-0.329095885784316,-0.329090998346089,-0.329086057751377,-0.329081063161586,
-0.32907601396187,-0.329070909730608,-0.32906574975319,-0.329060533062429,
-0.329055259360269,-0.327795550975526,-0.325719003041814,-0.320904544524618,
-0.31056875890951,-0.30807314487149,-0.306296471718684,-0.304509772629784,
-0.302611272054989,-0.299999045073864,-0.29533043182203,-0.279076934495437,
-0.270470430520659,-0.261632120091862,-0.255381771120378,-0.254739617695096,
-0.250371737921051,-0.245351992063265,-0.238358876007113,-0.226596184096797,
-0.22382905230438,-0.222172585951009,-0.220719246692206,-0.219244572248415,
-0.217307373489516,-0.214130264922035,-0.206896736850026,-0.200696423966184,
-0.196142809980264,-0.192866381682365,-0.188395571634731,-0.182128464896467,
-0.168982401357977,-0.162153235280996,-0.16098254727699,-0.157348466548358,
-0.153324497182617,-0.140139096102638,-0.136783434587749,-0.134974848879064,
-0.133177422459453,-0.131378834625872,-0.12901199397723,-0.125031635429469,
-0.11386010124943,-0.10942740329141,-0.10584250125783,-0.101838714256601,
-0.0935015891921936,-0.0755843737492411,-0.0724654902868474,-0.0692767199008584,
-0.0654317269939601,-0.0525099573245685,-0.0499547679711224,-0.0478985120680001,
-0.0459856695307695,-0.0438283325047181,-0.0353950616692065,-0.0259975052079688,
-0.0240759710615349,-0.0222886006567847,-0.0202890763344258,-0.0112347913638698,
-0.00515985773145303,-0.00252293204832874,-1.00000001163059E-6),
 .UNSPECIFIED.) ;
#3296 = B_SPLINE_CURVE_WITH_KNOTS('',3,(#14231,#14232,#14233,#14234,#14235,
#14236,#14237,#14238,#14239,#14240,#14241,#14242,#14243,#14244,#14245,#14246,
#14247,#14248,#14249,#14250,#14251,#14252,#14253,#14254,#14255,#14256,#14257,
#14258,#14259,#14260,#14261,#14262,#14263,#14264,#14265,#14266,#14267,#14268,
#14269,#14270,#14271,#14272,#14273,#14274,#14275,#14276,#14277,#14278,#14279,
#14280,#14281,#14282,#14283,#14284,#14285,#14286,#14287,#14288,#14289,#14290,
#14291,#14292,#14293,#14294,#14295,#14296,#14297,#14298,#14299,#14300,#14301,
#14302,#14303,#14304,#14305,#14306,#14307,#14308,#14309,#14310,#14311,#14312,
#14313,#14314,#14315,#14316,#14317,#14318,#14319,#14320,#14321,#14322,#14323,
#14324,#14325,#14326,#14327,#14328,#14329,#14330,#14331,#14332,#14333,#14334,
#14335,#14336,#14337,#14338,#14339,#14340,#14341,#14342,#14343,#14344,#14345,
#14346,#14347,#14348,#14349,#14350,#14351,#14352,#14353,#14354,#14355,#14356,
#14357,#14358,#14359,#14360,#14361,#14362,#14363,#14364,#14365,#14366,#14367,
#14368,#14369,#14370,#14371,#14372,#14373,#14374,#14375,#14376,#14377,#14378,
#14379,#14380,#14381,#14382,#14383,#14384,#14385,#14386,#14387,#14388,#14389,
#14390,#14391,#14392,#14393,#14394,#14395,#14396,#14397,#14398,#14399,#14400,
#14401,#14402,#14403,#14404,#14405,#14406,#14407,#14408,#14409,#14410,#14411,
#14412,#14413,#14414,#14415,#14416,#14417,#14418,#14419,#14420,#14421,#14422,
#14423,#14424,#14425,#14426,#14427,#14428,#14429,#14430,#14431,#14432,#14433,
#14434,#14435,#14436,#14437,#14438,#14439,#14440,#14441,#14442,#14443,#14444,
#14445,#14446,#14447,#14448,#14449,#14450),.UNSPECIFIED.,.F.,.F.,(4,2,2,
2,2,2,2,2,2,2,2,2,2,2,2,2,2,2,2,2,2,2,2,2,2,2,2,2,2,2,2,2,2,2,2,2,2,2,2,
2,2,2,2,2,2,2,2,2,2,2,2,2,2,2,2,2,2,2,2,2,2,2,2,2,2,2,2,2,2,2,2,2,2,2,2,
2,2,2,2,2,2,2,2,2,2,2,2,2,2,2,2,2,2,2,2,2,2,2,2,2,2,2,2,2,2,2,2,2,2,4),
(-0.786273343435783,-0.773001471184209,-0.770573001975978,-0.768742355216508,
-0.766587767425843,-0.75899866934865,-0.75313139285783,-0.748699410766708,
-0.745705140539268,-0.742153195664726,-0.733428079293303,-0.728390926211773,
-0.726047785065597,-0.724277512874789,-0.722102272001067,-0.716420527903919,
-0.708093128085561,-0.704303759993659,-0.700288158954778,-0.691004273053775,
-0.686295144006975,-0.683880403467859,-0.682049599009929,-0.680014623759397,
-0.674617926078111,-0.667788657679692,-0.6643712859418,-0.661781895527913,
-0.65932165481377,-0.656051581552829,-0.647904383004953,-0.640525521808526,
-0.637756931237378,-0.635428184108743,-0.633020815526334,-0.631055785105423,
-0.6248745021367,-0.610275329302061,-0.606383693716128,-0.598297144223019,
-0.595215862502454,-0.592298706664051,-0.58606470101389,-0.581297788829462,
-0.569557635011832,-0.559040071782923,-0.55432033337968,-0.550634954450769,
-0.545470871844967,-0.537097023751534,-0.53129252517215,-0.526638712070383,
-0.515594536656462,-0.511360598200319,-0.508800616753945,-0.506335217761588,
-0.500095809376638,-0.493827715412358,-0.491575074254936,-0.491064556932098,
-0.487643095843383,-0.483876584508024,-0.475691649455891,-0.46980958524541,
-0.467180697532896,-0.465388922663278,-0.464200231400658,-0.462022156132893,
-0.455997116918477,-0.453227582516795,-0.453121577243071,-0.453023566146825,
-0.452932655182824,-0.452848051936698,-0.452769051778779,-0.452695026002403,
-0.452625411547095,-0.450412176489763,-0.447942918212535,-0.439410964102818,
-0.435408352651825,-0.432844648959021,-0.430509129130819,-0.427850578028832,
-0.422648173050742,-0.416008935206783,-0.414077849275576,-0.411778535426679,
-0.411736691025614,-0.411696134004543,-0.411656802430231,-0.411618637158931,
-0.411581581737191,-0.411545582241584,-0.411510587133983,-0.41147654712428,
-0.411443415053054,-0.411411145749891,-0.411379695948769,-0.411349024162954,
-0.411319090573825,-0.41128985691958,-0.411261286449138,-0.411233343753753,
-0.411205994709181,-0.409143892858475,-0.40678019535758,-0.398862602884172,
-0.393445365823776,-0.393137881593438),.UNSPECIFIED.) ;
#3297 = B_SPLINE_CURVE_WITH_KNOTS('',3,(#14452,#14453,#14454,#14455,#14456,
#14457,#14458,#14459,#14460,#14461,#14462,#14463,#14464,#14465,#14466,#14467,
#14468,#14469,#14470,#14471,#14472,#14473,#14474,#14475,#14476,#14477,#14478,
#14479,#14480,#14481,#14482,#14483,#14484,#14485,#14486,#14487,#14488,#14489,
#14490,#14491,#14492,#14493,#14494,#14495,#14496,#14497,#14498,#14499,#14500,
#14501,#14502,#14503,#14504,#14505,#14506,#14507,#14508,#14509,#14510,#14511,
#14512,#14513,#14514,#14515,#14516,#14517,#14518,#14519,#14520,#14521,#14522,
#14523,#14524,#14525,#14526,#14527,#14528,#14529,#14530,#14531,#14532,#14533,
#14534,#14535,#14536,#14537,#14538,#14539,#14540,#14541,#14542,#14543,#14544,
#14545,#14546,#14547,#14548,#14549,#14550,#14551,#14552,#14553,#14554,#14555,
#14556,#14557,#14558,#14559,#14560,#14561,#14562,#14563,#14564,#14565,#14566,
#14567,#14568,#14569,#14570,#14571,#14572,#14573,#14574,#14575,#14576,#14577,
#14578,#14579,#14580,#14581,#14582,#14583,#14584,#14585,#14586,#14587,#14588,
#14589,#14590,#14591,#14592,#14593,#14594,#14595,#14596,#14597,#14598,#14599,
#14600,#14601,#14602,#14603,#14604,#14605,#14606,#14607,#14608,#14609,#14610,
#14611,#14612,#14613,#14614,#14615,#14616,#14617,#14618,#14619,#14620,#14621,
#14622,#14623,#14624,#14625,#14626,#14627,#14628,#14629,#14630,#14631,#14632,
#14633,#14634,#14635,#14636,#14637,#14638,#14639,#14640,#14641,#14642,#14643,
#14644,#14645,#14646,#14647,#14648,#14649,#14650,#14651,#14652,#14653,#14654,
#14655,#14656,#14657,#14658,#14659,#14660,#14661,#14662,#14663,#14664,#14665,
#14666,#14667,#14668,#14669,#14670,#14671,#14672,#14673,#14674,#14675,#14676,
#14677,#14678,#14679,#14680,#14681,#14682,#14683,#14684,#14685,#14686,#14687,
#14688,#14689,#14690,#14691,#14692,#14693,#14694,#14695,#14696,#14697,#14698,
#14699,#14700,#14701,#14702,#14703,#14704,#14705,#14706,#14707,#14708,#14709,
#14710,#14711,#14712,#14713,#14714,#14715,#14716,#14717,#14718,#14719,#14720,
#14721,#14722,#14723),.UNSPECIFIED.,.F.,.F.,(4,2,2,2,2,2,2,2,2,2,2,2,2,
2,2,2,2,2,2,2,2,2,2,2,2,2,2,2,2,2,2,2,2,2,2,2,2,2,2,2,2,2,2,2,2,2,2,2,2,
2,2,2,2,2,2,2,2,2,2,2,2,2,2,2,2,2,2,2,2,2,2,2,2,2,2,2,2,2,2,2,2,2,2,2,2,
2,2,2,2,2,2,2,2,2,2,2,2,2,2,2,2,2,2,2,2,2,2,2,2,2,2,2,2,2,2,2,2,2,2,2,2,
2,2,2,2,2,2,2,2,2,2,2,2,2,2,4),(-0.393164256152506,-0.393156152264836,-0.388938949432386,
-0.386265586580309,-0.383320173841496,-0.380395963431555,-0.376729005749432,
-0.371225094645901,-0.360152076233212,-0.359495928794148,-0.358457912062503,
-0.350172848148019,-0.348316579230778,-0.347232091080918,-0.346281049832906,
-0.346279673121862,-0.346278295983329,-0.346276918614931,-0.346275541127419,
-0.346274163250002,-0.346272785147417,-0.346271406528979,-0.346270027636126,
-0.346268648580951,-0.346267269146959,-0.346265889522371,-0.346264509669902,
-0.346263129235698,-0.346261748432,-0.346260367379516,-0.346258985988669,
-0.346257604455402,-0.346256222575073,-0.346254840150813,-0.346253457297103,
-0.346252074157025,-0.346250690734408,-0.34624930702275,-0.346247922935139,
-0.346246538512013,-0.34624515358407,-0.346243768164284,-0.346242382584822,
-0.345151799848308,-0.343908139441378,-0.341920247788448,-0.337956361559221,
-0.325679469518384,-0.310845004075075,-0.306934033755646,-0.304680164208461,
-0.302801175364782,-0.300978183146279,-0.298749352050761,-0.295444848040455,
-0.28956265258177,-0.276417330167695,-0.275987654395813,-0.275612833232664,
-0.274946863498535,-0.27473675522648,-0.26425374347445,-0.262358110176394,
-0.261275001979622,-0.260436280330363,-0.259409419544499,-0.257693939132142,
-0.255516662923331,-0.250898764044614,-0.24098180353912,-0.240281267024552,
-0.230388301428365,-0.226809991025846,-0.224075699166215,-0.222030371261093,
-0.218905053144269,-0.21453036929629,-0.206387136316234,-0.189252459249222,
-0.181314015113157,-0.178316431191022,-0.176070457873785,-0.173676731992705,
-0.173570406462553,-0.173456483631081,-0.17333413848094,-0.17320245484236,
-0.173060415341428,-0.173015442866163,-0.169896516950465,-0.163995443686111,
-0.15590441049969,-0.154020787739337,-0.153227388479005,-0.152166946028985,
-0.151030334603398,-0.147191849426399,-0.139235580187801,-0.131672951160756,
-0.129497194643878,-0.12793351650616,-0.126359598583563,-0.126344644150439,
-0.126329505815758,-0.126314172451892,-0.126298632774915,-0.126282875117486,
-0.126266887628018,-0.126250657965286,-0.126234173291891,-0.126217420453576,
-0.126200385837139,-0.124081559057585,-0.121493031922308,-0.116659863047585,
-0.0969684848948,-0.0894745904169614,-0.0846281110938773,-0.0808440649500737,
-0.0771927026387058,-0.0730338453367011,-0.0673537441420915,-0.0575039506960627,
-0.0470669286143805,-0.0449139771380755,-0.0437353206561605,-0.0425621832511658,
-0.0414144769472923,-0.0399527651585903,-0.0335830466459723,-0.0263176670026784,
-0.0177262246232782,-0.0144866405770614,-0.01173305256724,-0.00884924094737548,
-1.00000003500078E-6),.UNSPECIFIED.) ;
#3298 = B_SPLINE_CURVE_WITH_KNOTS('',3,(#14724,#14725,#14726,#14727,#14728,
#14729,#14730,#14731,#14732,#14733,#14734,#14735,#14736,#14737,#14738,#14739,
#14740,#14741,#14742,#14743,#14744,#14745,#14746,#14747,#14748,#14749,#14750,
#14751,#14752,#14753,#14754,#14755,#14756,#14757,#14758,#14759,#14760,#14761,
#14762,#14763,#14764,#14765,#14766,#14767,#14768,#14769,#14770,#14771,#14772,
#14773,#14774,#14775,#14776,#14777,#14778,#14779,#14780,#14781,#14782,#14783,
#14784,#14785,#14786,#14787,#14788,#14789,#14790,#14791,#14792,#14793,#14794,
#14795,#14796,#14797,#14798,#14799,#14800,#14801,#14802,#14803,#14804,#14805,
#14806,#14807,#14808,#14809,#14810,#14811,#14812,#14813,#14814,#14815,#14816,
#14817,#14818,#14819,#14820,#14821,#14822,#14823,#14824,#14825,#14826,#14827,
#14828,#14829,#14830,#14831,#14832,#14833,#14834,#14835,#14836,#14837,#14838,
#14839,#14840,#14841,#14842,#14843,#14844,#14845,#14846,#14847,#14848,#14849,
#14850,#14851,#14852,#14853,#14854,#14855,#14856,#14857,#14858,#14859,#14860,
#14861,#14862,#14863,#14864,#14865,#14866,#14867,#14868,#14869,#14870,#14871,
#14872,#14873,#14874,#14875,#14876,#14877,#14878,#14879,#14880,#14881,#14882,
#14883,#14884,#14885,#14886,#14887,#14888,#14889,#14890,#14891,#14892,#14893,
#14894,#14895,#14896,#14897,#14898,#14899,#14900,#14901,#14902,#14903,#14904,
#14905,#14906,#14907,#14908,#14909,#14910,#14911,#14912,#14913,#14914,#14915,
#14916,#14917,#14918,#14919,#14920,#14921,#14922,#14923,#14924,#14925,#14926,
#14927,#14928,#14929,#14930,#14931,#14932,#14933,#14934,#14935,#14936,#14937,
#14938,#14939,#14940,#14941,#14942,#14943,#14944,#14945,#14946,#14947,#14948,
#14949,#14950,#14951,#14952,#14953,#14954,#14955,#14956,#14957,#14958,#14959,
#14960,#14961,#14962,#14963,#14964,#14965,#14966,#14967,#14968,#14969,#14970,
#14971,#14972,#14973,#14974,#14975,#14976,#14977,#14978,#14979,#14980,#14981,
#14982,#14983,#14984,#14985,#14986,#14987,#14988,#14989,#14990,#14991,#14992,
#14993,#14994,#14995,#14996,#14997,#14998,#14999,#15000,#15001,#15002,#15003,
#15004,#15005,#15006,#15007,#15008,#15009,#15010,#15011,#15012,#15013,#15014,
#15015),.UNSPECIFIED.,.F.,.F.,(4,2,2,2,2,2,2,2,2,2,2,2,2,2,2,2,2,2,2,2,
2,2,2,2,2,2,2,2,2,2,2,2,2,2,2,2,2,2,2,2,2,2,2,2,2,2,2,2,2,2,2,2,2,2,2,2,
2,2,2,2,2,2,2,2,2,2,2,2,2,2,2,2,2,2,2,2,2,2,2,2,2,2,2,2,2,2,2,2,2,2,2,2,
2,2,2,2,2,2,2,2,2,2,2,2,2,2,2,2,2,2,2,2,2,2,2,2,2,2,2,2,2,2,2,2,2,2,2,2,
2,2,2,2,2,2,2,2,2,2,2,2,2,2,2,2,2,4),(-0.786022802871508,-0.768208391277082,
-0.763296722099367,-0.757186840663637,-0.75093170811864,-0.747225332449611,
-0.743905579872729,-0.740546897014286,-0.73185450926267,-0.726296817827928,
-0.724605742925792,-0.722303472397469,-0.720646718297841,-0.718724450613038,
-0.711455389107924,-0.705359271837876,-0.702173637914158,-0.699807373883381,
-0.697387336668927,-0.694511206888103,-0.682603384706928,-0.679874821745708,
-0.676710642978271,-0.675083487318463,-0.673061951590874,-0.667330703143089,
-0.66053982472266,-0.656745501355214,-0.653484751976131,-0.650041026217191,
-0.642502460686856,-0.637046930977787,-0.634551112042692,-0.634475703136425,
-0.634422827534395,-0.634223891009373,-0.632239064452856,-0.629556314284553,
-0.620535120589472,-0.615777865121373,-0.61214503033578,-0.608261969470558,
-0.601555762042765,-0.594682091290462,-0.591844291769375,-0.591705496878947,
-0.591590627759353,-0.591494422149133,-0.591412906803809,-0.591343059299871,
-0.591282560900992,-0.591229616366297,-0.591182822316312,-0.591141070986382,
-0.591103479109329,-0.590996465223403,-0.58899879027378,-0.586182374600085,
-0.577064642147933,-0.572925971795207,-0.569140395517931,-0.56566768116009,
-0.55830252646824,-0.553871378565928,-0.551778210504473,-0.550396353791058,
-0.550323305434506,-0.550257444769354,-0.550197898458933,-0.55014391307928,
-0.550094837425834,-0.550050107588255,-0.550009234239916,-0.549971791816349,
-0.549937409460509,-0.549905763214133,-0.549876569464195,-0.549849579383786,
-0.549824574062461,-0.549801360514304,-0.549747414988473,-0.549695035134528,
-0.549644094807515,-0.54959447268028,-0.549546051397069,-0.549498717001692,
-0.549452358011198,-0.549406864822056,-0.54936212879158,-0.549318041362475,
-0.549274493079106,-0.549231372549108,-0.549188565089277,-0.549145951308499,
-0.549103405201313,-0.549060792152727,-0.549017966223606,-0.548974766892577,
-0.548931014636352,-0.548886505578638,-0.548841003937325,-0.548810962831153,
-0.548775373822835,-0.548732207959483,-0.548678123648267,-0.548606993145874,
-0.548541215849835,-0.546858935013925,-0.544928489758558,-0.539051063893007,
-0.533660931450951,-0.529338828586779,-0.526766798122483,-0.524756341531112,
-0.52283096277006,-0.520358847255927,-0.515244234843112,-0.505374289116286,
-0.502432187854402,-0.499446953973203,-0.49679495803258,-0.488455684056152,
-0.481023080017612,-0.467166537041728,-0.465270642042361,-0.462197285389915,
-0.459358861956419,-0.448994350869757,-0.44406330904248,-0.441103527746636,
-0.43868771315956,-0.436928935739463,-0.433877369930967,-0.426667677105355,
-0.418914757875739,-0.415739113566393,-0.414563685772318,-0.414553954324598,
-0.414544121933321,-0.414534185879021,-0.412512888141889,-0.407947107053795,
-0.400787576798566,-0.396835168124836,-0.393317147110158,-0.393065589708965),
 .UNSPECIFIED.) ;
#3299 = B_SPLINE_CURVE_WITH_KNOTS('',3,(#15021,#15022,#15023,#15024,#15025,
#15026,#15027,#15028,#15029,#15030,#15031,#15032,#15033,#15034,#15035,#15036,
#15037,#15038,#15039,#15040,#15041,#15042,#15043,#15044,#15045,#15046,#15047,
#15048,#15049,#15050,#15051,#15052,#15053,#15054,#15055,#15056,#15057,#15058,
#15059,#15060,#15061,#15062,#15063,#15064,#15065,#15066,#15067,#15068,#15069,
#15070,#15071,#15072,#15073,#15074,#15075,#15076,#15077,#15078,#15079,#15080,
#15081,#15082,#15083,#15084),.UNSPECIFIED.,.F.,.F.,(4,3,3,3,3,3,3,3,3,3,
3,3,3,3,3,3,3,3,3,3,3,4),(3.93630690328113,4.11724533165042,4.33575257891902,
4.55311970215515,4.77079199021923,4.9201517619774,4.98858562151644,5.20574250287809,
5.42437800924309,5.64193365524723,5.85917452767311,5.90403230788466,6.07767534345593,
6.29534921278535,6.51184332341465,6.73048034262916,6.88787068095903,6.94820765270011,
7.16588235847274,7.38437758735345,7.60101478480632,7.60494227637848),
 .UNSPECIFIED.) ;
#3300 = B_SPLINE_CURVE_WITH_KNOTS('',3,(#15086,#15087,#15088,#15089),
 .UNSPECIFIED.,.F.,.F.,(4,4),(0.25650513994809,0.329185416412502),
 .UNSPECIFIED.) ;
#3301 = B_SPLINE_CURVE_WITH_KNOTS('',3,(#15090,#15091,#15092,#15093,#15094,
#15095,#15096,#15097,#15098,#15099,#15100,#15101,#15102,#15103,#15104,#15105,
#15106,#15107,#15108,#15109,#15110,#15111,#15112,#15113,#15114,#15115,#15116,
#15117,#15118,#15119,#15120,#15121,#15122,#15123,#15124,#15125,#15126,#15127,
#15128,#15129,#15130,#15131,#15132,#15133,#15134,#15135,#15136,#15137,#15138,
#15139,#15140,#15141,#15142,#15143,#15144,#15145,#15146,#15147,#15148,#15149,
#15150,#15151,#15152,#15153),.UNSPECIFIED.,.F.,.F.,(4,3,3,3,3,3,3,3,3,3,
3,3,3,3,3,3,3,3,3,3,3,4),(0.22510769815198,0.240322510068551,0.457482031297778,
0.674954946885662,0.984379771580828,1.11093076282781,1.38674777666684,1.54798490231427,
1.76619070002112,1.9698969082463,1.98477429053038,2.20178016056029,2.40580968662646,
2.41912725698171,2.6950269478308,2.85804930678088,2.95545595902922,3.29359733834846,
3.57495096587053,3.73048057044676,3.92985084354011,3.94168901841607),
 .UNSPECIFIED.) ;
#3302 = B_SPLINE_CURVE_WITH_KNOTS('',3,(#15159,#15160,#15161,#15162,#15163,
#15164,#15165,#15166,#15167,#15168,#15169,#15170,#15171,#15172,#15173,#15174,
#15175,#15176,#15177,#15178,#15179,#15180,#15181,#15182,#15183,#15184,#15185,
#15186,#15187,#15188,#15189,#15190,#15191,#15192,#15193,#15194,#15195,#15196,
#15197,#15198,#15199,#15200,#15201,#15202,#15203,#15204,#15205,#15206,#15207,
#15208,#15209,#15210,#15211,#15212,#15213,#15214,#15215,#15216,#15217,#15218,
#15219,#15220,#15221,#15222,#15223,#15224,#15225,#15226,#15227,#15228,#15229,
#15230,#15231,#15232,#15233,#15234,#15235,#15236,#15237,#15238,#15239,#15240,
#15241,#15242,#15243,#15244,#15245,#15246,#15247,#15248,#15249,#15250,#15251,
#15252,#15253,#15254,#15255,#15256,#15257,#15258,#15259,#15260,#15261,#15262,
#15263,#15264,#15265,#15266,#15267,#15268,#15269,#15270,#15271,#15272,#15273,
#15274,#15275,#15276,#15277,#15278,#15279,#15280,#15281,#15282,#15283,#15284,
#15285,#15286,#15287,#15288,#15289,#15290,#15291,#15292,#15293,#15294,#15295,
#15296,#15297,#15298,#15299,#15300,#15301,#15302,#15303,#15304,#15305,#15306,
#15307,#15308,#15309,#15310,#15311,#15312,#15313,#15314,#15315,#15316,#15317,
#15318,#15319,#15320,#15321,#15322,#15323,#15324,#15325,#15326,#15327,#15328,
#15329,#15330,#15331,#15332,#15333,#15334,#15335,#15336,#15337,#15338,#15339,
#15340,#15341,#15342,#15343,#15344,#15345,#15346,#15347,#15348,#15349,#15350,
#15351,#15352,#15353,#15354,#15355,#15356,#15357,#15358,#15359,#15360,#15361,
#15362,#15363,#15364,#15365,#15366,#15367,#15368,#15369,#15370,#15371,#15372,
#15373,#15374,#15375,#15376,#15377,#15378,#15379,#15380,#15381,#15382,#15383,
#15384,#15385,#15386,#15387,#15388,#15389,#15390,#15391,#15392,#15393,#15394,
#15395,#15396,#15397,#15398,#15399,#15400,#15401,#15402,#15403,#15404,#15405,
#15406,#15407,#15408,#15409,#15410,#15411,#15412,#15413,#15414,#15415,#15416,
#15417,#15418,#15419,#15420,#15421,#15422,#15423,#15424,#15425,#15426,#15427,
#15428,#15429,#15430,#15431,#15432,#15433,#15434,#15435,#15436,#15437,#15438,
#15439,#15440,#15441,#15442,#15443,#15444,#15445,#15446,#15447,#15448,#15449,
#15450,#15451,#15452,#15453,#15454,#15455,#15456,#15457,#15458,#15459,#15460,
#15461,#15462,#15463,#15464,#15465,#15466,#15467,#15468,#15469,#15470,#15471,
#15472,#15473,#15474,#15475,#15476,#15477,#15478,#15479,#15480,#15481,#15482,
#15483,#15484,#15485,#15486,#15487,#15488,#15489,#15490,#15491,#15492,#15493,
#15494,#15495,#15496,#15497,#15498,#15499,#15500,#15501,#15502,#15503,#15504,
#15505,#15506,#15507,#15508,#15509,#15510,#15511,#15512,#15513,#15514,#15515,
#15516,#15517,#15518,#15519,#15520,#15521,#15522,#15523,#15524,#15525,#15526,
#15527,#15528,#15529,#15530,#15531,#15532,#15533,#15534,#15535,#15536,#15537,
#15538,#15539,#15540,#15541,#15542,#15543,#15544,#15545,#15546,#15547,#15548,
#15549,#15550,#15551,#15552,#15553,#15554,#15555,#15556,#15557,#15558,#15559,
#15560,#15561,#15562,#15563,#15564,#15565,#15566,#15567,#15568,#15569,#15570,
#15571,#15572,#15573,#15574,#15575,#15576,#15577,#15578,#15579,#15580,#15581,
#15582,#15583,#15584,#15585,#15586,#15587,#15588,#15589,#15590,#15591,#15592,
#15593,#15594,#15595,#15596,#15597,#15598,#15599,#15600,#15601,#15602,#15603,
#15604,#15605,#15606,#15607,#15608,#15609,#15610,#15611,#15612,#15613,#15614,
#15615,#15616,#15617,#15618,#15619,#15620,#15621,#15622,#15623,#15624,#15625,
#15626,#15627,#15628,#15629,#15630,#15631,#15632,#15633,#15634,#15635,#15636,
#15637,#15638,#15639,#15640,#15641,#15642,#15643,#15644,#15645,#15646,#15647,
#15648,#15649,#15650,#15651,#15652,#15653,#15654,#15655,#15656,#15657,#15658,
#15659,#15660,#15661,#15662,#15663,#15664),.UNSPECIFIED.,.F.,.F.,(4,2,2,
2,2,2,2,2,2,2,2,2,2,2,2,2,2,2,2,2,2,2,2,2,2,2,2,2,2,2,2,2,2,2,2,2,2,2,2,
2,2,2,2,2,2,2,2,2,2,2,2,2,2,2,2,2,2,2,2,2,2,2,2,2,2,2,2,2,2,2,2,2,2,2,2,
2,2,2,2,2,2,2,2,2,2,2,2,2,2,2,2,2,2,2,2,2,2,2,2,2,2,2,2,2,2,2,2,2,2,2,2,
2,2,2,2,2,2,2,2,2,2,2,2,2,2,2,2,2,2,2,2,2,2,2,2,2,2,2,2,2,2,2,2,2,2,2,2,
2,2,2,2,2,2,2,2,2,2,2,2,2,2,2,2,2,2,2,2,2,2,2,2,2,2,2,2,2,2,2,2,2,2,2,2,
2,2,2,2,2,2,2,2,2,2,2,2,2,2,2,2,2,2,2,2,2,2,2,2,2,2,2,2,2,2,2,2,2,2,2,2,
2,2,2,2,2,2,2,2,2,2,2,2,2,2,2,2,2,2,2,2,2,2,2,2,2,2,2,2,2,2,2,2,2,4),(1.00000003107423E-6,
0.00758606072509173,0.0108710041624833,0.0143247956209498,0.0208239252769082,
0.0238927515787191,0.025810946333015,0.0279968188605102,0.0322345528750677,
0.0395986954574018,0.0425303421829458,0.0444500125162114,0.0461115855658382,
0.0478838537588698,0.0500607856817371,0.0592963885234545,0.0627047199517135,
0.064622625326492,0.0648433029942763,0.0649485267661199,0.0652108824895925,
0.0664993508235049,0.0678956190543377,0.069811362557096,0.0756151563130678,
0.0786721051827159,0.080996393366047,0.0835317885474625,0.0863732180528683,
0.0869090580287054,0.0943028183611597,0.0972479917582445,0.0998375264261362,
0.103450546780153,0.105746011255335,0.109557527772641,0.111773137679787,
0.113627818652749,0.115575090925519,0.117914649082595,0.126168573624676,
0.129469211199501,0.13113763966929,0.13228382018154,0.132297312089743,0.13231060790101,
0.132323711586497,0.132336627190269,0.132349358728273,0.132361910085438,
0.132374285113824,0.132386487393706,0.132398520751075,0.132410388821155,
0.132422095081156,0.132433642971765,0.13244503604532,0.132456277667125,
0.132467371078024,0.132478319353107,0.132489125877747,0.13249979378649,
0.132510326272213,0.132520726360938,0.132530996921134,0.132541140947748,
0.1325511614019,0.13256106116734,0.132570842850748,0.132580509282205,0.13259006330926,
0.132599507761533,0.132608845029195,0.132618077622391,0.132627208339874,
0.132636239878902,0.132645174451087,0.132654014587419,0.132662762780079,
0.133613078114437,0.134551756083437,0.136110283322514,0.141852140131374,
0.148152804730228,0.150696769179636,0.152207144948827,0.153332525120183,
0.154409950910943,0.155483588439527,0.156995117321235,0.163049020974393,
0.163318457712006,0.163487701093404,0.164044551813098,0.164239980931453,
0.169149440464479,0.171578832349428,0.173224310715876,0.173251122196248,
0.173275938182836,0.173298920277962,0.173320215933595,0.173339959524006,
0.173358273909484,0.173375271145134,0.173391053637524,0.173405715092009,
0.173419341274785,0.173457076411221,0.173493888724844,0.173529818902391,
0.173564906375431,0.173599189408022,0.173632705162844,0.173665489762294,
0.173697578453696,0.173729005422107,0.173759804091931,0.173790007159945,
0.175268608390759,0.17678317453679,0.179789230807408,0.185554972527963,
0.187485508647762,0.189489597414659,0.192290189644725,0.195571422944641,
0.201512834159888,0.207699189548433,0.214772626482893,0.222893420645628,
0.231588205447433,0.239730868305575,0.247641715027393,0.250223966606402,
0.252707032278387,0.255056200826789,0.263002130010397,0.265124646036926,
0.266879034859959,0.266949731973928,0.267021738327771,0.267095384335621,
0.267171007261269,0.267248955942809,0.269253037243444,0.272675869547824,
0.280388839190857,0.283981695096317,0.28562709367168,0.286337355946282,
0.287405356306157,0.288739948714158,0.290511659225286,0.29343858183247,
0.300314970243317,0.305179804900724,0.306560366801992,0.307367316534436,
0.308143086373136,0.308147292379295,0.30815149937488,0.30815570830479,0.308159919595909,
0.308164134087966,0.308168352790471,0.308172576588967,0.308176806155979,
0.308181042011112,0.308185285035802,0.308189536275606,0.308193796370424,
0.308198065979394,0.308202345949028,0.308206637056553,0.308210940072838,
0.308215255698035,0.308219584583216,0.308223927699764,0.30822828584424,
0.308232659615481,0.308237050159465,0.308241458313446,0.308245884278854,
0.308250329065134,0.308254793672125,0.308259279029154,0.308263785619111,
0.308268314266151,0.308272865990642,0.308277441596114,0.308282041749382,
0.308286667336892,0.308291319331838,0.308295998550959,0.308300705727866,
0.30830544197662,0.308310208408059,0.308315005715939,0.308319834658204,
0.30832469627586,0.308329591497877,0.308334521189614,0.308339486557809,
0.308344488696937,0.308349528192487,0.308354606294887,0.308359724188747,
0.308364882756052,0.308370082986239,0.308375326102076,0.308380613269204,
0.308385945504728,0.309501917416463,0.310849978670979,0.313302695335476,
0.32009880250983,0.321329313609062,0.326371209895372,0.32780966818185,0.328628411435736,
0.329447103513662,0.330268560056833,0.331331652992355,0.333024686442496,
0.336492955832328,0.341319027081028,0.347789982837823,0.349234163989716,
0.350039436967057,0.350844033296672,0.351809623999787,0.353532641840576,
0.355968223308192,0.363358431133201,0.368385057144218,0.370026937325979,
0.371198454251677,0.37238817065583,0.373634585993347,0.375332328479082,
0.378325953913608,0.386222929491161,0.389566981420992,0.391526002698366,
0.393264196242751,0.395926836584615,0.399549882620271,0.404261552877088,
0.40553618279537,0.406849244156398,0.408634596324438,0.415419114930417),
 .UNSPECIFIED.) ;
#3303 = B_SPLINE_CURVE_WITH_KNOTS('',3,(#15667,#15668,#15669,#15670,#15671,
#15672,#15673,#15674,#15675,#15676,#15677,#15678,#15679,#15680,#15681,#15682,
#15683,#15684,#15685,#15686,#15687,#15688,#15689,#15690,#15691,#15692,#15693,
#15694,#15695,#15696,#15697,#15698,#15699,#15700,#15701,#15702,#15703,#15704,
#15705,#15706,#15707,#15708,#15709,#15710,#15711,#15712,#15713,#15714,#15715,
#15716,#15717,#15718,#15719,#15720,#15721,#15722,#15723,#15724,#15725,#15726,
#15727,#15728,#15729,#15730,#15731,#15732,#15733,#15734,#15735,#15736,#15737,
#15738,#15739,#15740,#15741,#15742,#15743,#15744,#15745,#15746,#15747,#15748,
#15749,#15750,#15751,#15752,#15753,#15754,#15755,#15756,#15757,#15758,#15759,
#15760),.UNSPECIFIED.,.F.,.F.,(4,3,3,3,3,3,3,3,3,3,3,3,3,3,3,3,3,3,3,3,
3,3,3,3,3,3,3,3,3,3,3,4),(0.,0.134125242113495,0.352509078655641,0.571152133448733,
0.78785206804089,0.983887078909349,1.00554836450288,1.22292581387916,1.44156822673879,
1.6583768279816,1.87701872585698,1.967805066204,2.0954587923726,2.31195714336637,
2.53008391262842,2.74872480101196,2.95170543670643,2.96503359632297,3.18381638618427,
3.40163618034529,3.61938862784145,3.83802875124856,3.9356342331213,4.05498887068103,
4.27296461086581,4.49064193752331,4.70788679226362,4.91955051441669,4.92650165651424,
5.144061943285,5.36270278817282,5.47192428281431),.UNSPECIFIED.) ;
#3304 = B_SPLINE_CURVE_WITH_KNOTS('',3,(#15765,#15766,#15767,#15768,#15769,
#15770,#15771,#15772,#15773,#15774,#15775,#15776,#15777,#15778,#15779,#15780,
#15781,#15782,#15783,#15784,#15785,#15786,#15787,#15788,#15789,#15790,#15791,
#15792,#15793,#15794,#15795,#15796,#15797,#15798,#15799,#15800,#15801,#15802,
#15803,#15804,#15805,#15806,#15807,#15808,#15809,#15810,#15811,#15812,#15813,
#15814,#15815,#15816,#15817,#15818,#15819,#15820,#15821,#15822,#15823,#15824,
#15825,#15826,#15827,#15828,#15829,#15830,#15831,#15832,#15833,#15834,#15835,
#15836,#15837,#15838,#15839,#15840,#15841,#15842,#15843,#15844,#15845,#15846,
#15847,#15848,#15849,#15850,#15851,#15852,#15853,#15854,#15855,#15856,#15857,
#15858,#15859,#15860,#15861,#15862,#15863,#15864,#15865,#15866,#15867,#15868,
#15869,#15870,#15871,#15872,#15873,#15874,#15875,#15876,#15877,#15878,#15879,
#15880,#15881,#15882,#15883,#15884,#15885,#15886,#15887,#15888,#15889,#15890,
#15891,#15892,#15893,#15894,#15895,#15896,#15897),.UNSPECIFIED.,.F.,.F.,
(4,3,3,3,3,3,3,3,3,3,3,3,3,3,3,3,3,3,3,3,3,3,3,3,3,3,3,3,3,3,3,3,3,3,3,
3,3,3,3,3,3,3,3,3,4),(2.23946037462874E-7,0.113928974459155,0.33050927421389,
0.549146903932351,0.766218720390714,0.98390723300321,0.984709727674719,
1.20309877951712,1.42024744924451,1.63874154934289,1.85598261279694,1.96781599695643,
2.07441147807449,2.29208458319818,2.50857722956503,2.72721269324237,2.94476761865918,
2.95171824854718,3.16337707976576,3.38061656346098,3.59828848338828,3.81625880634713,
3.93561230171815,4.03321351484648,4.25184816680328,4.4695951611072,4.68740947514502,
4.90618676612606,4.91951528184525,5.12249010119948,5.3411254552712,5.55924671538816,
5.77573958537857,5.90338904849895,5.99417411953157,6.21281048992181,6.42961360201299,
6.64825048695635,6.86562245257652,6.887282253509,7.08331326234648,7.30000775290474,
7.51864531750287,7.73702369701646,7.87114652979459),.UNSPECIFIED.) ;
#3305 = B_SPLINE_CURVE_WITH_KNOTS('',3,(#15898,#15899,#15900,#15901,#15902,
#15903,#15904,#15905,#15906,#15907,#15908,#15909,#15910,#15911,#15912,#15913,
#15914,#15915,#15916,#15917,#15918,#15919,#15920,#15921,#15922,#15923,#15924,
#15925,#15926,#15927,#15928,#15929,#15930,#15931,#15932,#15933,#15934,#15935,
#15936,#15937,#15938,#15939,#15940,#15941,#15942,#15943,#15944,#15945,#15946,
#15947,#15948,#15949,#15950,#15951,#15952,#15953,#15954,#15955,#15956,#15957,
#15958,#15959,#15960,#15961,#15962,#15963,#15964,#15965,#15966,#15967,#15968,
#15969,#15970,#15971,#15972,#15973,#15974,#15975,#15976,#15977,#15978,#15979,
#15980,#15981,#15982,#15983,#15984,#15985,#15986,#15987,#15988,#15989,#15990,
#15991,#15992,#15993,#15994,#15995,#15996,#15997,#15998,#15999,#16000,#16001,
#16002,#16003,#16004,#16005,#16006,#16007,#16008,#16009,#16010,#16011,#16012,
#16013,#16014,#16015,#16016,#16017,#16018,#16019,#16020,#16021,#16022,#16023,
#16024,#16025,#16026,#16027,#16028,#16029,#16030),.UNSPECIFIED.,.F.,.F.,
(4,3,3,3,3,3,3,3,3,3,3,3,3,3,3,3,3,3,3,3,3,3,3,3,3,3,3,3,3,3,3,3,3,3,3,
3,3,3,3,3,3,3,3,3,4),(0.,0.1642451678838,0.382740226136021,0.600042062652495,
0.81815801878653,0.983838204133042,1.03554180687826,1.25343367267224,1.4720705861592,
1.68865038754616,1.90636266602205,1.96771931508277,2.12483115640474,2.34346704485423,
2.56016000368955,2.7779225847442,2.95155919736311,2.99516190669561,3.2137969189207,
3.43059850228283,3.6492332319301,3.86772566803192,3.93544715914144,4.08418625839254,
4.30244973018225,4.5209413905342,4.73957624737208,4.9192941129049,4.95595506538896,
5.17362755082564,5.39151762976199,5.61015329739374,5.82664642703676,5.90317527296924,
6.04509370180904,6.2627673956939,6.48000880082162,6.69864573210573,6.88702953663498,
6.91610786953944,7.13474521426614,7.35118372095701,7.56903886818247,7.78781927394833,
7.8709187028199),.UNSPECIFIED.) ;
#3306 = B_SPLINE_CURVE_WITH_KNOTS('',3,(#16035,#16036,#16037,#16038,#16039,
#16040,#16041,#16042,#16043,#16044,#16045,#16046,#16047,#16048,#16049,#16050,
#16051,#16052,#16053,#16054,#16055,#16056,#16057,#16058,#16059,#16060,#16061,
#16062,#16063,#16064,#16065,#16066,#16067,#16068,#16069,#16070,#16071,#16072,
#16073,#16074,#16075,#16076,#16077,#16078,#16079,#16080,#16081,#16082,#16083,
#16084,#16085,#16086,#16087,#16088,#16089,#16090,#16091,#16092,#16093,#16094,
#16095,#16096,#16097,#16098,#16099,#16100,#16101,#16102,#16103,#16104,#16105,
#16106,#16107,#16108,#16109,#16110,#16111,#16112,#16113,#16114,#16115,#16116,
#16117,#16118,#16119,#16120,#16121,#16122,#16123,#16124,#16125,#16126,#16127,
#16128,#16129,#16130,#16131,#16132,#16133,#16134,#16135,#16136,#16137,#16138,
#16139,#16140,#16141,#16142,#16143,#16144,#16145,#16146,#16147,#16148,#16149,
#16150,#16151,#16152,#16153,#16154,#16155,#16156,#16157,#16158,#16159,#16160,
#16161,#16162,#16163,#16164,#16165,#16166,#16167),.UNSPECIFIED.,.F.,.F.,
(4,3,3,3,3,3,3,3,3,3,3,3,3,3,3,3,3,3,3,3,3,3,3,3,3,3,3,3,3,3,3,3,3,3,3,
3,3,3,3,3,3,3,3,3,4),(6.47843382475931E-7,0.0830984389275147,0.301878860860896,
0.519734057113125,0.736172606010294,0.954810013303583,0.983889730856414,
1.17227222785097,1.39090923664682,1.60815073803404,1.82582451472097,1.96773996380494,
2.04427188534893,2.26076510838228,2.47940086131416,2.6972910267807,2.91496358979538,
2.95162597969021,3.13134247828944,3.3499773857217,3.56846909158646,3.78673258995452,
3.93547366988932,4.00319319004644,4.22168561989418,4.44032034293354,4.65712189547432,
4.87575686542146,4.91936143024466,5.09299614077408,5.31075866271332,5.5274515595306,
5.74608737246715,5.90319990585872,5.96455578971764,6.1822680007672,6.39884773442802,
6.61748458072403,6.835376397882,6.88707997267627,7.0527601418454,7.27087606613454,
7.48817787698011,7.70667292996054,7.87091906976138),.UNSPECIFIED.) ;
#3307 = B_SPLINE_CURVE_WITH_KNOTS('',3,(#16168,#16169,#16170,#16171,#16172,
#16173,#16174,#16175,#16176,#16177,#16178,#16179,#16180,#16181,#16182,#16183,
#16184,#16185,#16186,#16187,#16188,#16189,#16190,#16191,#16192,#16193,#16194,
#16195,#16196,#16197,#16198,#16199,#16200,#16201,#16202,#16203,#16204,#16205,
#16206,#16207,#16208,#16209,#16210,#16211,#16212,#16213,#16214,#16215,#16216,
#16217,#16218,#16219,#16220,#16221,#16222,#16223,#16224,#16225,#16226,#16227,
#16228,#16229,#16230,#16231,#16232,#16233,#16234,#16235,#16236,#16237,#16238,
#16239,#16240,#16241,#16242,#16243,#16244,#16245,#16246,#16247,#16248,#16249,
#16250,#16251,#16252,#16253,#16254,#16255,#16256,#16257,#16258,#16259,#16260,
#16261,#16262,#16263,#16264,#16265,#16266,#16267,#16268,#16269,#16270,#16271,
#16272,#16273,#16274,#16275,#16276,#16277,#16278,#16279,#16280,#16281,#16282,
#16283,#16284,#16285),.UNSPECIFIED.,.F.,.F.,(4,3,3,3,3,3,3,3,3,3,3,3,3,
3,3,3,3,3,3,3,3,3,3,3,3,3,3,3,3,3,3,3,3,3,3,3,3,3,3,4),(0.,0.194263872696949,
0.474398180042492,0.631922336312114,0.986336477555327,1.06871325737457,
1.35894643553535,1.50494696278201,1.94274749763261,1.97350601102964,2.37925229361138,
2.66802896959778,2.81675030786879,2.96031018031642,3.25226766112055,3.52559369118093,
3.69031672560053,3.93266213911079,3.94639008315669,4.1263712743904,4.39764408223475,
4.56330498068008,4.93283600994182,4.99936437452894,5.25968459515218,5.43653729304416,
5.64205095182849,5.65434225145359,5.87297818907955,5.91836368727623,6.09147775928523,
6.30915524874002,6.58118775056185,6.74493474743988,6.90382603695033,7.18073446312476,
7.39913360227665,7.61629290065923,7.834266390535,7.88799015781433),
 .UNSPECIFIED.) ;
#3308 = B_SPLINE_CURVE_WITH_KNOTS('',3,(#16290,#16291,#16292,#16293,#16294,
#16295,#16296,#16297,#16298,#16299,#16300,#16301,#16302,#16303,#16304,#16305,
#16306,#16307,#16308,#16309,#16310,#16311,#16312,#16313,#16314,#16315,#16316,
#16317,#16318,#16319,#16320,#16321,#16322,#16323,#16324,#16325,#16326,#16327,
#16328,#16329,#16330,#16331,#16332,#16333,#16334,#16335,#16336,#16337,#16338,
#16339,#16340,#16341,#16342,#16343,#16344,#16345,#16346,#16347,#16348,#16349,
#16350,#16351,#16352,#16353,#16354,#16355,#16356,#16357,#16358,#16359,#16360,
#16361,#16362,#16363,#16364,#16365,#16366,#16367,#16368,#16369,#16370,#16371,
#16372,#16373,#16374,#16375,#16376,#16377,#16378,#16379,#16380,#16381,#16382,
#16383,#16384,#16385,#16386,#16387,#16388,#16389,#16390,#16391,#16392,#16393,
#16394,#16395,#16396,#16397,#16398,#16399,#16400,#16401,#16402,#16403,#16404,
#16405,#16406,#16407,#16408,#16409,#16410,#16411,#16412,#16413,#16414,#16415,
#16416,#16417,#16418,#16419,#16420,#16421,#16422,#16423,#16424,#16425,#16426,
#16427,#16428,#16429,#16430,#16431,#16432,#16433,#16434,#16435,#16436,#16437,
#16438,#16439,#16440,#16441,#16442,#16443,#16444,#16445,#16446,#16447,#16448,
#16449,#16450,#16451,#16452,#16453,#16454,#16455,#16456,#16457,#16458,#16459,
#16460,#16461,#16462,#16463,#16464,#16465,#16466,#16467,#16468,#16469,#16470,
#16471,#16472,#16473,#16474,#16475,#16476,#16477,#16478,#16479,#16480,#16481,
#16482,#16483,#16484,#16485,#16486,#16487,#16488,#16489,#16490,#16491,#16492,
#16493,#16494,#16495,#16496,#16497,#16498,#16499,#16500,#16501,#16502,#16503,
#16504,#16505,#16506,#16507,#16508,#16509,#16510,#16511,#16512,#16513,#16514,
#16515,#16516,#16517,#16518,#16519,#16520,#16521,#16522,#16523,#16524,#16525,
#16526,#16527,#16528,#16529,#16530,#16531,#16532,#16533,#16534,#16535,#16536,
#16537,#16538,#16539,#16540,#16541,#16542,#16543,#16544,#16545,#16546,#16547,
#16548,#16549,#16550,#16551,#16552,#16553,#16554,#16555,#16556,#16557,#16558,
#16559,#16560,#16561,#16562,#16563,#16564,#16565,#16566,#16567,#16568,#16569,
#16570,#16571,#16572,#16573,#16574,#16575,#16576,#16577,#16578,#16579,#16580,
#16581,#16582,#16583,#16584,#16585,#16586,#16587,#16588,#16589,#16590,#16591,
#16592,#16593,#16594,#16595,#16596,#16597,#16598,#16599,#16600,#16601,#16602,
#16603,#16604,#16605,#16606,#16607,#16608,#16609,#16610,#16611,#16612,#16613,
#16614,#16615,#16616,#16617,#16618,#16619,#16620,#16621,#16622,#16623,#16624,
#16625,#16626,#16627,#16628,#16629,#16630,#16631,#16632,#16633,#16634,#16635,
#16636,#16637,#16638,#16639,#16640,#16641,#16642,#16643,#16644,#16645,#16646,
#16647,#16648,#16649,#16650,#16651,#16652,#16653,#16654,#16655,#16656,#16657,
#16658,#16659,#16660,#16661,#16662,#16663,#16664,#16665,#16666,#16667,#16668,
#16669,#16670,#16671,#16672,#16673,#16674,#16675,#16676,#16677,#16678,#16679,
#16680,#16681,#16682,#16683,#16684,#16685,#16686,#16687,#16688,#16689,#16690,
#16691,#16692,#16693,#16694,#16695,#16696,#16697,#16698,#16699,#16700,#16701,
#16702,#16703,#16704,#16705,#16706,#16707,#16708,#16709,#16710,#16711,#16712,
#16713,#16714,#16715,#16716,#16717,#16718,#16719,#16720,#16721,#16722,#16723,
#16724,#16725,#16726,#16727,#16728,#16729,#16730,#16731,#16732,#16733,#16734,
#16735,#16736,#16737,#16738,#16739,#16740,#16741,#16742,#16743,#16744,#16745,
#16746,#16747,#16748,#16749,#16750,#16751,#16752,#16753,#16754,#16755,#16756,
#16757,#16758,#16759,#16760,#16761,#16762,#16763,#16764,#16765,#16766,#16767,
#16768,#16769,#16770,#16771,#16772,#16773,#16774,#16775,#16776,#16777,#16778,
#16779,#16780,#16781,#16782,#16783,#16784,#16785,#16786,#16787,#16788,#16789,
#16790,#16791,#16792,#16793,#16794,#16795,#16796,#16797,#16798,#16799,#16800,
#16801,#16802,#16803,#16804,#16805,#16806,#16807,#16808,#16809,#16810,#16811,
#16812,#16813,#16814,#16815,#16816,#16817,#16818,#16819,#16820,#16821,#16822,
#16823,#16824,#16825,#16826,#16827,#16828,#16829,#16830,#16831,#16832,#16833,
#16834,#16835,#16836,#16837,#16838,#16839,#16840,#16841,#16842,#16843,#16844,
#16845,#16846,#16847,#16848,#16849,#16850,#16851,#16852,#16853,#16854,#16855,
#16856,#16857,#16858,#16859,#16860,#16861,#16862,#16863,#16864,#16865,#16866,
#16867,#16868,#16869,#16870,#16871,#16872,#16873,#16874,#16875,#16876,#16877,
#16878,#16879,#16880,#16881,#16882,#16883,#16884,#16885,#16886,#16887,#16888,
#16889,#16890,#16891,#16892,#16893,#16894,#16895,#16896,#16897,#16898,#16899,
#16900,#16901,#16902,#16903,#16904,#16905,#16906,#16907,#16908,#16909,#16910,
#16911,#16912,#16913,#16914,#16915,#16916,#16917,#16918,#16919,#16920,#16921,
#16922,#16923,#16924,#16925,#16926,#16927,#16928,#16929,#16930,#16931,#16932,
#16933,#16934,#16935,#16936,#16937,#16938,#16939,#16940,#16941,#16942,#16943,
#16944,#16945,#16946,#16947,#16948,#16949,#16950,#16951,#16952,#16953,#16954,
#16955,#16956,#16957,#16958,#16959,#16960,#16961,#16962,#16963,#16964,#16965,
#16966,#16967,#16968,#16969,#16970,#16971,#16972,#16973,#16974,#16975,#16976,
#16977,#16978,#16979,#16980,#16981,#16982,#16983,#16984,#16985,#16986,#16987,
#16988,#16989,#16990,#16991,#16992,#16993,#16994,#16995,#16996,#16997,#16998,
#16999,#17000,#17001,#17002,#17003,#17004,#17005,#17006,#17007,#17008,#17009,
#17010,#17011,#17012,#17013,#17014,#17015,#17016,#17017,#17018,#17019,#17020,
#17021,#17022,#17023,#17024,#17025,#17026,#17027,#17028,#17029,#17030,#17031,
#17032,#17033,#17034,#17035,#17036,#17037,#17038,#17039,#17040,#17041,#17042,
#17043,#17044,#17045,#17046,#17047,#17048,#17049,#17050,#17051,#17052,#17053,
#17054,#17055,#17056,#17057,#17058,#17059,#17060,#17061,#17062,#17063,#17064,
#17065,#17066,#17067,#17068,#17069,#17070,#17071,#17072,#17073,#17074,#17075,
#17076,#17077,#17078,#17079,#17080,#17081,#17082,#17083),.UNSPECIFIED.,
 .F.,.F.,(4,2,2,2,2,2,2,2,2,2,2,2,2,2,2,2,2,2,2,2,2,2,2,2,2,2,2,2,2,2,2,
2,2,2,2,2,2,2,2,2,2,2,2,2,2,2,2,2,2,2,2,2,2,2,2,2,2,2,2,2,2,2,2,2,2,2,2,
2,2,2,2,2,2,2,2,2,2,2,2,2,2,2,2,2,2,2,2,2,2,2,2,2,2,2,2,2,2,2,2,2,2,2,2,
2,2,2,2,2,2,2,2,2,2,2,2,2,2,2,2,2,2,2,2,2,2,2,2,2,2,2,2,2,2,2,2,2,2,2,2,
2,2,2,2,2,2,2,2,2,2,2,2,2,2,2,2,2,2,2,2,2,2,2,2,2,2,2,2,2,2,2,2,2,2,2,2,
2,2,2,2,2,2,2,2,2,2,2,2,2,2,2,2,2,2,2,2,2,2,2,2,2,2,2,2,2,2,2,2,2,2,2,2,
2,2,2,2,2,2,2,2,2,2,2,2,2,2,2,2,2,2,2,2,2,2,2,2,2,2,2,2,2,2,2,2,2,2,2,2,
2,2,2,2,2,2,2,2,2,2,2,2,2,2,2,2,2,2,2,2,2,2,2,2,2,2,2,2,2,2,2,2,2,2,2,2,
2,2,2,2,2,2,2,2,2,2,2,2,2,2,2,2,2,2,2,2,2,2,2,2,2,2,2,2,2,2,2,2,2,2,2,2,
2,2,2,2,2,2,2,2,2,2,2,2,2,2,2,2,2,2,2,2,2,2,2,2,2,2,2,2,2,2,2,2,2,2,2,2,
2,2,2,2,2,2,2,2,2,2,2,2,2,2,2,2,2,2,2,2,2,2,2,2,2,2,2,2,2,2,2,2,2,2,2,2,
2,2,2,2,2,4),(1.00000004678006E-6,0.0117981715776559,0.0141765875756427,
0.0161778548407407,0.0183214071210216,0.0216752514139586,0.0301257972670827,
0.0348883544478171,0.0372044521983115,0.0396682123971428,0.0428351898584976,
0.0509548013683551,0.0540302919194078,0.0564902514800823,0.0569992489011105,
0.057287635005279,0.0596896934386391,0.0647023908037505,0.0685970451669697,
0.0703360089238731,0.0705977297608284,0.0708618611263078,0.071867870856269,
0.0720514717888028,0.0742827147117976,0.0805882325797279,0.0872943976943436,
0.091128938430779,0.0937663735205952,0.0974692052344555,0.104677080693303,
0.110711199443734,0.113344221830045,0.113646001252761,0.113916590354331,
0.114250483372622,0.116287598685056,0.117104608580213,0.124391044251081,
0.130776892737506,0.135721936028525,0.136240568959361,0.136626232832928,
0.137108340071238,0.142825704139786,0.153865841947984,0.157348106984969,
0.157506960055344,0.157710572204959,0.158010479345694,0.15850669968298,
0.158878674540749,0.159347000758451,0.161532073514973,0.1720516846647,0.186215337037974,
0.190388529976153,0.190614963879188,0.201007120766463,0.206502849534112,
0.212828239653974,0.216632075569862,0.231244010368758,0.236061569493539,
0.236281020116368,0.23645410139097,0.23659200928394,0.236702897493482,0.236792780489028,
0.236866152563208,0.237052886302177,0.237226032123925,0.23738759982428,
0.237539361728887,0.237682899697175,0.237819646663956,0.237950924855777,
0.238077982687932,0.238202032570825,0.238324292626211,0.238446036229072,
0.238568655782945,0.23869375107223,0.238823260437904,0.238959669574263,
0.239029954464892,0.239146602253067,0.239517792197664,0.242077886644829,
0.244485969598382,0.254160824240424,0.260059855551496,0.263362599291692,
0.266361995925271,0.267949647995184,0.271025158298437,0.278007528704527,
0.285633683849564,0.287605018779196,0.287613733831114,0.287622288629389,
0.287630687375141,0.287638934034966,0.287647032406389,0.287654986251203,
0.287662799264217,0.287670474845409,0.287678016451467,0.287685427327927,
0.28769271074535,0.287699869641961,0.287712045364945,0.287724131601217,
0.287736129806356,0.287748041536514,0.287759868211534,0.287771611400497,
0.28778327247071,0.287794852852654,0.287806354058216,0.28781777741181,0.287829124241842,
0.2878403959326,0.287851593861463,0.287862719306652,0.287873773675878,0.287884758248309,
0.287895674233595,0.287906522873875,0.287917305479812,0.287928023241506,
0.287938677551452,0.287949269494109,0.287959800296564,0.28797027113837,
0.287980683122077,0.287991037486362,0.288001335428267,0.288011578116628,
0.288021766660132,0.288031902186019,0.288041985818963,0.288052018663478,
0.288062001850122,0.288071936449968,0.288081823552528,0.288091664187382,
0.288101459456185,0.288111210684049,0.28812092061002,0.288130592218129,
0.288140228407355,0.288149832177158,0.28815940654576,0.288168954459302,
0.288178478887028,0.288187982703064,0.28819746885464,0.288206940299735,
0.288216443475015,0.288225985215775,0.28823556627346,0.288245187451109,
0.288254849694628,0.288264553892017,0.288274300984802,0.288284091802487,
0.288293927281936,0.288303808366235,0.288313735947895,0.288323711024387,
0.288333734690832,0.288343807933894,0.288353931706565,0.288364107083035,
0.288374335136366,0.288384617030569,0.288394953825097,0.288405346697891,
0.288415796846845,0.288426305396853,0.288436873568455,0.288447502560683,
0.288458193667055,0.288468948077633,0.288479767132306,0.288490652188274,
0.288501604697995,0.288512626015545,0.288523717528315,0.288532425454214,
0.288541351952106,0.288550504837793,0.288559892422303,0.2885695234194,0.288579406955357,
0.288589552524787,0.288599970218165,0.288610670750819,0.28862166529466,
0.288632965629541,0.288644584315021,0.28865653447984,0.288668830106218,
0.288681485909634,0.28869451761888,0.288707941849257,0.288721776254907,
0.288736039507445,0.288750751595507,0.288765933733784,0.288781608601664,
0.288797800313895,0.28881453475341,0.288831839572732,0.288849744441903,
0.288868281230161,0.288887484152688,0.288907390099895,0.288928038818334,
0.288949473235584,0.291126502648353,0.295963668354246,0.303254745760134,
0.308370978615938,0.312352732402771,0.318935052213715,0.328136385741887,
0.328169070943261,0.328199862403885,0.328228893261674,0.328256285487696,
0.328282150978216,0.32830659252777,0.328329704637812,0.32835157435535,0.328372281895868,
0.328391901306064,0.328410500993111,0.328428144189227,0.328444889484998,
0.328480976124107,0.328516301480781,0.32855089593913,0.328584788546575,
0.330847670834751,0.332832671674803,0.336802722254229,0.34519558457925,
0.349089120984497,0.352558092535757,0.353797947175991,0.357218607553165,
0.362990062524411,0.370451452940245,0.372381352886408,0.374933898929131,
0.374939788970267,0.374945669020018,0.374951539223768,0.374957399789569,
0.374963250868975,0.374969092572663,0.37497492509504,0.374980748617456,
0.374986563312461,0.374992369363712,0.374998166923447,0.375003956114768,
0.375009737085523,0.375015510117237,0.375021275344455,0.375027032882029,
0.375032782879761,0.37503852556205,0.37555694324117,0.375567269909854,0.377720868258857,
0.382365610442631,0.389375752076264,0.393379859296447,0.397296294500328,
0.401104978004888,0.406777661015277,0.407621523137426,0.410289752320065,
0.414582856926883,0.416603986028205,0.416614002572225,0.416623915413951,
0.416633726692027,0.416643438635818,0.416653053555611,0.416662573535574,
0.41667200056114,0.416681336581605,0.417485878291613,0.419087625363594,
0.421142700497735,0.42574136377725,0.436836636891112,0.439393831152882,
0.441472131292074,0.441660590835585,0.441686489525662,0.441710955310895,
0.441733714646402,0.441754835741431,0.441774391036881,0.441792456284458,
0.441809109423203,0.441824429579624,0.441838496273588,0.441851388648489,
0.441864292124513,0.441876924177411,0.4418892852421,0.441901377148708,0.441913200097161,
0.442256322994076,0.44419768240756,0.446645761483289,0.450636427945831,
0.46174540541876,0.465759700949354,0.469658104524871,0.49693467769608,0.50102995100839,
0.504817827829038,0.508390463552266,0.520691704899558,0.524782833308149,
0.526948147955865,0.528135983758028,0.528194582201978,0.528236735318638,
0.528272546690989,0.528302637777417,0.52832766942319,0.528348305856086,
0.528365185038294,0.528386703464043,0.528407214203401,0.528426731725113,
0.52844527322612,0.528462858526146,0.530200604517233,0.53232457793843,0.535618772997076,
0.542794734749739,0.549350793127886,0.553775944069864,0.558191678735382,
0.564327245393766,0.579709110085063,0.581430465521649,0.584689685628003,
0.588301379998283,0.593186366960729,0.606838048654737,0.611786897883082,
0.61365258879985,0.615185280153268,0.616555647458888,0.618102750025953,
0.620251819405073,0.623997558833745,0.633926477995027,0.642866787177593,
0.648363892796145,0.654054532993876,0.66300241029919,0.671853890072724,
0.681717989235355,0.69435239117764,0.697366964678845,0.699144929545757,
0.700941910234864,0.702848675596833,0.705486500230046,0.71031582254622,
0.720212043330027,0.722204552175948,0.723328187639032,0.724052318599337,
0.725114703915184,0.728173669291402,0.737248207422731,0.744046114323223,
0.746546722674751,0.748393098439738,0.750149368261651,0.75220221465179,
0.755246063676816,0.768062546023172,0.778797336791404,0.786297940368581),
 .UNSPECIFIED.) ;
#3309 = B_SPLINE_CURVE_WITH_KNOTS('',3,(#17084,#17085,#17086,#17087,#17088,
#17089,#17090,#17091,#17092,#17093,#17094,#17095,#17096,#17097,#17098,#17099,
#17100,#17101,#17102,#17103,#17104,#17105,#17106,#17107,#17108,#17109,#17110,
#17111,#17112,#17113,#17114,#17115,#17116,#17117,#17118,#17119,#17120,#17121,
#17122,#17123,#17124,#17125,#17126,#17127,#17128,#17129,#17130,#17131,#17132,
#17133,#17134,#17135,#17136,#17137,#17138,#17139,#17140,#17141,#17142,#17143,
#17144,#17145,#17146,#17147,#17148,#17149,#17150,#17151,#17152,#17153,#17154,
#17155,#17156,#17157,#17158,#17159,#17160,#17161,#17162,#17163,#17164,#17165,
#17166,#17167,#17168,#17169,#17170,#17171,#17172,#17173,#17174,#17175,#17176,
#17177,#17178,#17179,#17180,#17181,#17182,#17183,#17184,#17185,#17186,#17187,
#17188,#17189,#17190,#17191,#17192,#17193,#17194,#17195,#17196,#17197,#17198,
#17199,#17200,#17201,#17202,#17203,#17204,#17205,#17206,#17207,#17208,#17209,
#17210,#17211,#17212,#17213,#17214,#17215,#17216,#17217,#17218,#17219,#17220,
#17221,#17222,#17223,#17224,#17225,#17226,#17227,#17228,#17229,#17230,#17231,
#17232,#17233,#17234,#17235,#17236,#17237,#17238,#17239,#17240,#17241,#17242,
#17243,#17244,#17245,#17246,#17247,#17248,#17249,#17250,#17251,#17252,#17253,
#17254,#17255,#17256,#17257,#17258,#17259,#17260,#17261,#17262,#17263,#17264,
#17265,#17266,#17267,#17268,#17269,#17270,#17271,#17272,#17273,#17274,#17275,
#17276,#17277,#17278,#17279,#17280,#17281,#17282,#17283,#17284,#17285,#17286,
#17287,#17288,#17289,#17290,#17291,#17292,#17293,#17294,#17295,#17296,#17297,
#17298,#17299,#17300,#17301,#17302,#17303,#17304,#17305,#17306,#17307,#17308,
#17309,#17310,#17311,#17312,#17313,#17314,#17315,#17316,#17317,#17318,#17319,
#17320,#17321,#17322,#17323,#17324,#17325,#17326,#17327,#17328,#17329,#17330,
#17331,#17332,#17333,#17334,#17335,#17336,#17337,#17338,#17339,#17340,#17341,
#17342,#17343,#17344,#17345,#17346,#17347,#17348,#17349,#17350,#17351,#17352,
#17353,#17354,#17355,#17356,#17357,#17358,#17359,#17360,#17361,#17362,#17363,
#17364,#17365,#17366,#17367,#17368,#17369,#17370,#17371,#17372,#17373,#17374,
#17375,#17376,#17377,#17378,#17379,#17380,#17381,#17382,#17383,#17384,#17385,
#17386,#17387,#17388,#17389,#17390,#17391,#17392,#17393,#17394,#17395,#17396,
#17397,#17398,#17399,#17400,#17401,#17402,#17403,#17404,#17405,#17406,#17407,
#17408,#17409,#17410,#17411,#17412,#17413,#17414,#17415,#17416,#17417,#17418,
#17419,#17420,#17421,#17422,#17423,#17424,#17425,#17426,#17427,#17428,#17429,
#17430,#17431,#17432,#17433,#17434,#17435,#17436,#17437,#17438,#17439,#17440,
#17441,#17442,#17443,#17444,#17445,#17446,#17447,#17448,#17449,#17450,#17451,
#17452,#17453,#17454,#17455,#17456,#17457,#17458,#17459,#17460,#17461,#17462,
#17463,#17464,#17465,#17466,#17467,#17468,#17469,#17470,#17471,#17472,#17473,
#17474,#17475,#17476,#17477,#17478,#17479,#17480,#17481,#17482,#17483,#17484,
#17485,#17486,#17487,#17488,#17489,#17490,#17491,#17492,#17493,#17494,#17495,
#17496,#17497,#17498,#17499,#17500,#17501,#17502,#17503,#17504,#17505,#17506,
#17507,#17508,#17509,#17510,#17511,#17512,#17513,#17514,#17515,#17516,#17517,
#17518,#17519,#17520,#17521,#17522,#17523,#17524,#17525,#17526,#17527,#17528,
#17529,#17530,#17531,#17532,#17533,#17534,#17535,#17536,#17537,#17538,#17539,
#17540,#17541,#17542,#17543,#17544,#17545,#17546,#17547,#17548,#17549,#17550,
#17551,#17552,#17553,#17554,#17555,#17556,#17557,#17558,#17559,#17560,#17561,
#17562,#17563,#17564,#17565,#17566,#17567,#17568,#17569,#17570,#17571,#17572,
#17573,#17574,#17575,#17576,#17577,#17578,#17579,#17580,#17581,#17582,#17583,
#17584,#17585,#17586,#17587,#17588,#17589,#17590,#17591,#17592,#17593,#17594,
#17595,#17596,#17597,#17598,#17599,#17600,#17601,#17602,#17603,#17604,#17605,
#17606,#17607,#17608,#17609,#17610,#17611,#17612,#17613,#17614,#17615,#17616,
#17617,#17618,#17619,#17620,#17621,#17622,#17623,#17624,#17625,#17626,#17627,
#17628,#17629,#17630,#17631,#17632,#17633,#17634,#17635,#17636,#17637,#17638,
#17639,#17640,#17641,#17642,#17643,#17644,#17645,#17646,#17647,#17648,#17649,
#17650,#17651,#17652,#17653,#17654,#17655,#17656,#17657,#17658,#17659,#17660,
#17661,#17662,#17663,#17664,#17665,#17666,#17667,#17668,#17669,#17670,#17671,
#17672,#17673,#17674,#17675,#17676,#17677,#17678,#17679,#17680,#17681,#17682,
#17683,#17684,#17685,#17686,#17687,#17688,#17689,#17690,#17691,#17692,#17693,
#17694,#17695,#17696,#17697,#17698,#17699,#17700,#17701,#17702,#17703,#17704,
#17705,#17706,#17707,#17708,#17709,#17710,#17711,#17712,#17713,#17714,#17715,
#17716,#17717,#17718,#17719,#17720,#17721,#17722,#17723,#17724,#17725,#17726,
#17727,#17728,#17729,#17730,#17731,#17732,#17733,#17734,#17735,#17736,#17737,
#17738,#17739,#17740,#17741,#17742,#17743,#17744,#17745,#17746,#17747,#17748,
#17749,#17750,#17751,#17752,#17753,#17754,#17755,#17756,#17757,#17758,#17759,
#17760,#17761,#17762,#17763,#17764,#17765,#17766,#17767,#17768,#17769,#17770,
#17771,#17772,#17773,#17774,#17775,#17776,#17777,#17778,#17779,#17780,#17781,
#17782,#17783,#17784,#17785,#17786,#17787,#17788,#17789,#17790,#17791,#17792,
#17793,#17794,#17795,#17796,#17797,#17798,#17799,#17800,#17801,#17802,#17803,
#17804,#17805,#17806,#17807,#17808,#17809,#17810,#17811,#17812,#17813,#17814,
#17815,#17816,#17817,#17818,#17819,#17820,#17821,#17822,#17823,#17824,#17825,
#17826,#17827,#17828,#17829,#17830,#17831,#17832,#17833,#17834,#17835,#17836,
#17837,#17838,#17839,#17840,#17841,#17842,#17843,#17844,#17845,#17846,#17847,
#17848,#17849,#17850,#17851,#17852,#17853,#17854,#17855,#17856,#17857,#17858,
#17859,#17860,#17861,#17862,#17863,#17864,#17865,#17866,#17867,#17868,#17869,
#17870,#17871,#17872,#17873,#17874,#17875,#17876,#17877,#17878,#17879,#17880,
#17881,#17882,#17883,#17884,#17885,#17886,#17887,#17888,#17889,#17890,#17891,
#17892,#17893,#17894,#17895,#17896,#17897,#17898,#17899,#17900,#17901,#17902,
#17903,#17904,#17905,#17906,#17907),.UNSPECIFIED.,.F.,.F.,(4,2,2,2,2,2,
2,2,2,2,2,2,2,2,2,2,2,2,2,2,2,2,2,2,2,2,2,2,2,2,2,2,2,2,2,2,2,2,2,2,2,2,
2,2,2,2,2,2,2,2,2,2,2,2,2,2,2,2,2,2,2,2,2,2,2,2,2,2,2,2,2,2,2,2,2,2,2,2,
2,2,2,2,2,2,2,2,2,2,2,2,2,2,2,2,2,2,2,2,2,2,2,2,2,2,2,2,2,2,2,2,2,2,2,2,
2,2,2,2,2,2,2,2,2,2,2,2,2,2,2,2,2,2,2,2,2,2,2,2,2,2,2,2,2,2,2,2,2,2,2,2,
2,2,2,2,2,2,2,2,2,2,2,2,2,2,2,2,2,2,2,2,2,2,2,2,2,2,2,2,2,2,2,2,2,2,2,2,
2,2,2,2,2,2,2,2,2,2,2,2,2,2,2,2,2,2,2,2,2,2,2,2,2,2,2,2,2,2,2,2,2,2,2,2,
2,2,2,2,2,2,2,2,2,2,2,2,2,2,2,2,2,2,2,2,2,2,2,2,2,2,2,2,2,2,2,2,2,2,2,2,
2,2,2,2,2,2,2,2,2,2,2,2,2,2,2,2,2,2,2,2,2,2,2,2,2,2,2,2,2,2,2,2,2,2,2,2,
2,2,2,2,2,2,2,2,2,2,2,2,2,2,2,2,2,2,2,2,2,2,2,2,2,2,2,2,2,2,2,2,2,2,2,2,
2,2,2,2,2,2,2,2,2,2,2,2,2,2,2,2,2,2,2,2,2,2,2,2,2,2,2,2,2,2,2,2,2,2,2,2,
2,2,2,2,2,2,2,2,2,2,2,2,2,2,2,2,2,2,2,2,2,2,2,2,2,2,2,2,2,2,2,2,2,2,2,2,
2,2,2,2,2,2,2,2,2,4),(1.00000001482342E-6,0.00387989849434221,0.00965386819778096,
0.0176277349044153,0.0198228806392684,0.0215745100882533,0.0234954630887238,
0.0326569349317571,0.0381640880605481,0.0412771457430435,0.0437174423764869,
0.0460848193585393,0.0492269609407735,0.0597163419065942,0.0643745621454506,
0.0675782334901951,0.0706959462422394,0.0779496778758638,0.0854439807223627,
0.0967604007439808,0.1017462689883,0.104731705765129,0.107252769730566,
0.11050523777754,0.119128871523756,0.124155399590182,0.126948898947171,
0.129018506668542,0.13105495250947,0.133405969259583,0.137725506561563,
0.148374618351109,0.151398280693758,0.153022907801174,0.154584281070802,
0.156423523520727,0.159912810261316,0.168481393143192,0.172565032640693,
0.175979545017129,0.179474515418626,0.189923792638977,0.193606348045477,
0.195687984992599,0.197706494688502,0.201164926123051,0.210217465380377,
0.214516682735599,0.218161996317371,0.221575844802789,0.232859886545185,
0.236588502397511,0.237112183316485,0.237411445158013,0.237578601813748,
0.237812638940346,0.239669627823577,0.241846153267194,0.247729815668176,
0.254523650730061,0.258167238498117,0.261688169648363,0.265918859928784,
0.276015561687705,0.27919245215231,0.281131484656794,0.282764054070061,
0.28459325304176,0.29344444708349,0.29879950755727,0.301799582589062,0.304123994276168,
0.306331369678783,0.309271856388809,0.320388661309048,0.324406343497094,
0.326367042094413,0.327914004120641,0.329700603105548,0.332765620440067,
0.335628650198325,0.337586531364092,0.344251170297893,0.348039110161335,
0.351365114431158,0.35489880382105,0.367359725472494,0.371399937256882,
0.380412495938149,0.393134782655627,0.403099644508735,0.40508617683676,
0.407722466949874,0.411122928841098,0.413016861815729,0.417678939999058,
0.432169368736004,0.43460346715269,0.435986161393044,0.437055341926396,
0.438233032937166,0.440330685773129,0.44298732252709,0.448720658143859,
0.466783984856216,0.471891219704659,0.475893582739653,0.479540483978466,
0.483861659422546,0.489514996798002,0.497347682092197,0.50903104119785,
0.51682119557004,0.519348403601593,0.520899994807651,0.522427103623144,
0.522431787674928,0.52243647891577,0.522441177308973,0.522445883339716,
0.522450597559427,0.522455319884319,0.522460050461944,0.522464789274641,
0.522469536791856,0.522474293569499,0.522479059583391,0.522483834861456,
0.522488620124326,0.522493415196993,0.522498220428804,0.522503036158753,
0.522507862278447,0.522512699215363,0.522517547179921,0.522522406468298,
0.522527277271925,0.522532160166779,0.52253705511781,0.522541962203414,
0.52254688191372,0.522551814514536,0.522556759960928,0.522561718587701,
0.522566690784472,0.522571676669936,0.52257667669236,0.52258169111907,0.522586720088111,
0.52259176374344,0.52259682253021,0.52260189634087,0.522606985649322,0.522612090817191,
0.522617212052831,0.522622349747412,0.522627504114795,0.522632675210603,
0.522637863360016,0.522643068897424,0.522648292262694,0.522653533546729,
0.522658793019039,0.522664071057127,0.522669367992304,0.522674683784087,
0.522680018881375,0.522685373651308,0.522690748552824,0.522696143694737,
0.52270155933062,0.522706995583814,0.522712453088174,0.522717932181592,
0.522723432857887,0.522728955413582,0.522734500378407,0.522740068108535,
0.52274565865659,0.522751272301079,0.522756909715616,0.522762570965939,
0.52276825654844,0.522773966889108,0.522779702246598,0.522785462863514,
0.522791249089045,0.52279706110555,0.522802899318917,0.522808764336661,
0.522814656363363,0.522820575614543,0.522826522575855,0.5228324974654,0.522838500862241,
0.52284453302179,0.522850594541565,0.522856685652069,0.522862806491349,
0.522868957545056,0.522875139471389,0.522881352428205,0.52288759698738,
0.522893873361063,0.522900181887687,0.522906523096759,0.522912897641791,
0.522919305649913,0.522925747550841,0.522932223934683,0.522938735130323,
0.522945281471344,0.522951863499161,0.522958481746644,0.522965136549655,
0.522971828363516,0.522978557605635,0.522985324817749,0.522992130433628,
0.522998974720019,0.523005858407542,0.523012782263043,0.523019746339463,
0.523026751225562,0.523033797426523,0.52304088550161,0.523048016135177,
0.523055189612988,0.523062406526519,0.523069667487326,0.523076972971153,
0.523084323472904,0.523091719682342,0.523099162013879,0.523106651015868,
0.523114187409881,0.523121771672841,0.523129404352956,0.523137086141206,
0.523144817633374,0.523152599363097,0.523160432004689,0.523168316071842,
0.523176252241407,0.523184241238915,0.523192283561949,0.523200380014055,
0.523208531216622,0.523216737875416,0.523225000632802,0.52323332020029,
0.523241697237135,0.523250132351368,0.523258626267659,0.523267179883397,
0.523275793851081,0.523284468965726,0.523293205898434,0.523302005342351,
0.523310868144507,0.523319795135524,0.523328787112698,0.523337844609226,
0.525978329323283,0.52959315606768,0.539115577091703,0.543835608239035,
0.545295680478062,0.545809802699583,0.546175058277946,0.547035020420134,
0.5483658270704,0.552881944968185,0.5629338284468,0.567349268951828,0.569636419430082,
0.571432686149489,0.571460440690088,0.571488096926663,0.571515667013946,
0.571543162713895,0.571570595505927,0.57159797647101,0.571625316334739,
0.57165262571796,0.571679914952057,0.571707194185741,0.571734473230971,
0.571761761761505,0.571789069348269,0.571816405330517,0.571843778985032,
0.571871199411981,0.571898675640363,0.571926216664993,0.571953831241164,
0.571981528180434,0.572009316259056,0.572037204205928,0.572065200618897,
0.57209331418374,0.572121553515515,0.572149927236589,0.572178443919876,
0.57220711230649,0.572235941083895,0.57226493891177,0.572294114588136,0.572323476896052,
0.572353034710167,0.572382797035703,0.572412772774587,0.572426819780976,
0.572441086189964,0.57245558087268,0.572470312916514,0.572485292018211,
0.572500528125015,0.572516031533396,0.572531813070026,0.572547883881441,
0.572564255805886,0.57258094096377,0.572597952081772,0.572615302426087,
0.572633005952118,0.57265107696426,0.57266953071676,0.57268838302498,0.572707650473353,
0.572727350232543,0.572747500466581,0.572768120205924,0.572789229388394,
0.572810848881148,0.572833000584883,0.572855707402202,0.572878993504638,
0.572902884225224,0.572927406145922,0.572952587234879,0.572978456979052,
0.573005046218774,0.5730323875944,0.573060515399895,0.573089465738324,0.573119276593467,
0.573149988169945,0.573181642778997,0.573214284998644,0.573247961904776,
0.57328272327948,0.573318621533535,0.573355712098979,0.57339405364296,0.573433708146859,
0.573474741030373,0.573517221578279,0.57356122312896,0.573606823301819,
0.573654104213617,0.573703152837347,0.573754061329939,0.573806927315289,
0.573861854260396,0.57391895190319,0.57397833652038,0.574040131475568,0.574104467637211,
0.57417148389872,0.577309791806326,0.583080868621443,0.605652753316221,
0.612431293337457,0.615878906316043,0.618876085243178,0.622649759553554,
0.631024122802069,0.643566397937766,0.65091863530742,0.652711902868909,
0.653761218994568,0.654673164993293,0.655825679584042,0.658039015136198,
0.665059029463612,0.685081295501266,0.691942522026095,0.694517354357912,
0.69636003364943,0.698151941485855,0.700025555889807,0.702422402367053,
0.706124226071868,0.713014604662016,0.722224740795031,0.725099045298787,
0.736565942202035,0.738505519027787,0.739619753857818,0.740483629436549,
0.741391023405732,0.742497960887426,0.745906515753753,0.748912421752995,
0.759518825586065,0.766546640638556,0.773314070429204,0.776970573531812,
0.780124271143675,0.783011593288301,0.786304990770929),.UNSPECIFIED.) ;
#3310 = B_SPLINE_CURVE_WITH_KNOTS('',3,(#17913,#17914,#17915,#17916,#17917,
#17918,#17919,#17920,#17921,#17922,#17923,#17924,#17925,#17926,#17927,#17928,
#17929,#17930,#17931,#17932,#17933,#17934,#17935,#17936,#17937,#17938,#17939,
#17940,#17941,#17942,#17943,#17944,#17945,#17946,#17947,#17948,#17949,#17950,
#17951,#17952,#17953,#17954,#17955,#17956,#17957,#17958,#17959,#17960,#17961,
#17962,#17963,#17964,#17965,#17966,#17967,#17968,#17969,#17970,#17971,#17972,
#17973,#17974,#17975,#17976,#17977,#17978,#17979,#17980,#17981,#17982,#17983,
#17984,#17985,#17986,#17987,#17988,#17989,#17990,#17991,#17992,#17993,#17994,
#17995,#17996,#17997,#17998,#17999,#18000,#18001,#18002,#18003,#18004,#18005,
#18006,#18007,#18008,#18009,#18010,#18011,#18012,#18013,#18014,#18015,#18016,
#18017,#18018,#18019,#18020,#18021,#18022,#18023,#18024,#18025,#18026,#18027,
#18028,#18029,#18030,#18031,#18032,#18033,#18034,#18035,#18036,#18037,#18038,
#18039,#18040,#18041,#18042,#18043,#18044,#18045,#18046,#18047,#18048,#18049,
#18050,#18051,#18052,#18053,#18054,#18055,#18056,#18057,#18058,#18059,#18060,
#18061,#18062,#18063,#18064,#18065,#18066,#18067,#18068,#18069,#18070,#18071,
#18072,#18073,#18074,#18075,#18076,#18077,#18078,#18079,#18080,#18081,#18082,
#18083,#18084,#18085,#18086,#18087,#18088,#18089,#18090,#18091,#18092,#18093,
#18094,#18095,#18096,#18097,#18098,#18099,#18100,#18101,#18102,#18103,#18104,
#18105,#18106,#18107,#18108,#18109,#18110,#18111,#18112,#18113,#18114,#18115,
#18116,#18117,#18118,#18119,#18120,#18121,#18122,#18123,#18124,#18125,#18126,
#18127,#18128,#18129,#18130,#18131,#18132,#18133,#18134,#18135,#18136,#18137,
#18138,#18139,#18140,#18141,#18142,#18143,#18144,#18145,#18146,#18147,#18148,
#18149,#18150,#18151,#18152,#18153,#18154,#18155,#18156,#18157,#18158,#18159,
#18160,#18161,#18162,#18163,#18164,#18165,#18166,#18167,#18168,#18169,#18170,
#18171,#18172,#18173,#18174,#18175,#18176,#18177,#18178,#18179,#18180,#18181,
#18182,#18183,#18184),.UNSPECIFIED.,.F.,.F.,(4,2,2,2,2,2,2,2,2,2,2,2,2,
2,2,2,2,2,2,2,2,2,2,2,2,2,2,2,2,2,2,2,2,2,2,2,2,2,2,2,2,2,2,2,2,2,2,2,2,
2,2,2,2,2,2,2,2,2,2,2,2,2,2,2,2,2,2,2,2,2,2,2,2,2,2,2,2,2,2,2,2,2,2,2,2,
2,2,2,2,2,2,2,2,2,2,2,2,2,2,2,2,2,2,2,2,2,2,2,2,2,2,2,2,2,2,2,2,2,2,2,2,
2,2,2,2,2,2,2,2,2,2,2,2,2,2,4),(1.00045753387877E-6,0.00842574258640645,
0.00972187540196538,0.0107115335657187,0.0116939906523298,0.0128170038292646,
0.0147243601837294,0.0215802725329028,0.0218748824183406,0.0269639747780574,
0.0291600262320035,0.0309012301160614,0.0309974238262923,0.0319926874072608,
0.0329785506518943,0.034294784905869,0.0372283069439382,0.038495401808696,
0.0441001690701221,0.0470165251449591,0.0497371711014842,0.0514932927041807,
0.0524315775376868,0.0534223086733845,0.0620991752675434,0.0650098235845182,
0.0652392200391438,0.0655582062101748,0.0676666166423386,0.0725489952146196,
0.0792874801163711,0.082412773806087,0.0850633816542351,0.0921119307833907,
0.0951721742366237,0.0969128579231273,0.0969476794878039,0.0969817376180178,
0.0970150806129788,0.0970477543459423,0.0970798024757228,0.0971112666319582,
0.0971421865730741,0.0971726002560678,0.0972025441603608,0.0972320533420131,
0.0986070463085602,0.0998164535194011,0.101545167401429,0.104608187854877,
0.111301015631071,0.11464694352377,0.117315886137275,0.118995585269948,
0.119617034933218,0.119948992792079,0.122025190823821,0.129033278289205,
0.132916033136038,0.135637083878071,0.135730605089018,0.135825237093655,
0.135921367094742,0.136019410332923,0.138398653533622,0.141309989037906,
0.148182546878764,0.151303116506634,0.15307225252019,0.157548254583598,
0.161220813611117,0.161356628742213,0.161482682807114,0.161600697766164,
0.161712100649152,0.161818095844787,0.161919719087912,0.16201787898814,
0.162113389929729,0.162206999116378,0.162299409747552,0.162391301834548,
0.162483352012097,0.162576253731141,0.164998922977395,0.165350175185979,
0.165513711754882,0.166873479807214,0.17275334136621,0.179112615094698,
0.183240259013787,0.194097109397645,0.195675735372543,0.200127934149792,
0.208329337367673,0.209725031547082,0.21258176570396,0.212716443836338,
0.215791274067457,0.218730443793863,0.226421270971432,0.228229406166425,
0.229464330404538,0.230921769963285,0.232826206626257,0.235360160744058,
0.241566937320219,0.246786042138185,0.249039996753663,0.250651677162911,
0.252552014854883,0.252615301035394,0.252681953760395,0.252752366350411,
0.252826979118717,0.252906286511062,0.255250205896054,0.259565120371384,
0.267809753877705,0.270257819100499,0.272207478810114,0.274503758004808,
0.277516463423376,0.283377219011778,0.286962777096555,0.295636502516541,
0.327358048750501,0.338653043172959,0.344423924466601,0.34720348970197,
0.353062618927892,0.357882761955244,0.360027136520687,0.361867165314252,
0.363867606408137,0.366518801123044),.UNSPECIFIED.) ;
#3311 = B_SPLINE_CURVE_WITH_KNOTS('',3,(#18186,#18187,#18188,#18189),
 .UNSPECIFIED.,.F.,.F.,(4,4),(1.57753970984684,1.64973532704643),
 .UNSPECIFIED.) ;
#3312 = B_SPLINE_CURVE_WITH_KNOTS('',3,(#18190,#18191,#18192,#18193,#18194,
#18195,#18196,#18197,#18198,#18199,#18200,#18201,#18202,#18203,#18204,#18205,
#18206,#18207,#18208,#18209,#18210,#18211,#18212,#18213,#18214,#18215,#18216,
#18217,#18218,#18219,#18220,#18221,#18222,#18223,#18224,#18225,#18226,#18227,
#18228,#18229,#18230,#18231,#18232,#18233,#18234,#18235,#18236,#18237,#18238,
#18239,#18240,#18241,#18242,#18243,#18244,#18245,#18246,#18247,#18248,#18249,
#18250,#18251,#18252,#18253,#18254,#18255,#18256,#18257,#18258,#18259,#18260,
#18261,#18262,#18263,#18264,#18265,#18266,#18267,#18268,#18269,#18270,#18271,
#18272,#18273,#18274,#18275,#18276,#18277,#18278,#18279,#18280,#18281,#18282,
#18283,#18284,#18285,#18286,#18287,#18288,#18289,#18290,#18291,#18292,#18293,
#18294,#18295,#18296,#18297,#18298,#18299,#18300,#18301,#18302,#18303,#18304,
#18305,#18306,#18307,#18308,#18309,#18310,#18311,#18312,#18313,#18314,#18315,
#18316,#18317,#18318,#18319,#18320,#18321,#18322,#18323,#18324,#18325,#18326,
#18327,#18328,#18329,#18330,#18331,#18332,#18333,#18334,#18335,#18336,#18337,
#18338,#18339,#18340,#18341,#18342,#18343,#18344,#18345,#18346,#18347,#18348,
#18349,#18350,#18351,#18352,#18353,#18354,#18355,#18356,#18357,#18358,#18359,
#18360,#18361,#18362,#18363,#18364,#18365,#18366,#18367,#18368,#18369,#18370,
#18371,#18372,#18373,#18374,#18375,#18376,#18377,#18378,#18379,#18380,#18381,
#18382,#18383,#18384,#18385,#18386,#18387,#18388,#18389,#18390,#18391,#18392,
#18393,#18394,#18395,#18396,#18397,#18398,#18399,#18400,#18401,#18402,#18403,
#18404,#18405,#18406,#18407,#18408,#18409,#18410,#18411,#18412,#18413,#18414,
#18415,#18416,#18417,#18418,#18419,#18420,#18421,#18422,#18423,#18424,#18425,
#18426,#18427,#18428,#18429,#18430,#18431,#18432,#18433,#18434,#18435),
 .UNSPECIFIED.,.F.,.F.,(4,2,2,2,2,2,2,2,2,2,2,2,2,2,2,2,2,2,2,2,2,2,2,2,
2,2,2,2,2,2,2,2,2,2,2,2,2,2,2,2,2,2,2,2,2,2,2,2,2,2,2,2,2,2,2,2,2,2,2,2,
2,2,2,2,2,2,2,2,2,2,2,2,2,2,2,2,2,2,2,2,2,2,2,2,2,2,2,2,2,2,2,2,2,2,2,2,
2,2,2,2,2,2,2,2,2,2,2,2,2,2,2,2,2,2,2,2,2,2,2,2,2,2,4),(1.00000001215618E-6,
0.00318509854600134,0.0129825347919774,0.0161655928261109,0.0181412012449489,
0.0198749291596257,0.0217270011136096,0.027707503078466,0.0396795572268528,
0.0419643725085689,0.0439360536928425,0.0460388807219774,0.0485916927504747,
0.0564492253007152,0.0645252079856154,0.0726409997678784,0.0841201028158781,
0.0914142858167252,0.0972082175898708,0.102273990648958,0.11246729967127,
0.119786567755532,0.122835110716931,0.12464124579374,0.125528329059267,
0.125562447011711,0.125595423621323,0.125627296775938,0.125658103323062,
0.125687879117623,0.125716658934808,0.125744476687226,0.125771365263028,
0.125797356637172,0.125822481953175,0.125846771389411,0.125870254353946,
0.125892959249474,0.125914913765058,0.125936144796729,0.125956678238446,
0.125976539390029,0.125995752768358,0.12601434203994,0.127279720261118,
0.128529548359017,0.130252307020754,0.135073159299629,0.13562333022193,
0.147756262536827,0.150769938843763,0.152296404982632,0.153444191401216,
0.154524046101334,0.155740524253793,0.157326395380975,0.164922423718007,
0.171721896110145,0.173399919221211,0.175450903838611,0.181038689856756,
0.185234452374922,0.185944160403659,0.187391980760904,0.190317421502036,
0.193934746168347,0.198342189104919,0.203544452516594,0.205689344812316,
0.20587443456203,0.207753117213519,0.207766443193314,0.207779613291745,
0.207792636216129,0.207805520255973,0.20781827348019,0.207830903622127,
0.210936143326028,0.215230566120306,0.225185429159629,0.231109341320472,
0.235206707196223,0.237029262167199,0.248215449135854,0.255908396838854,
0.259423652157063,0.262992881970404,0.263559828116157,0.265002078884858,
0.270395037063474,0.278966392081394,0.27937082880019,0.279812755485324,
0.280328522021279,0.281237571128015,0.283215844598803,0.285602684967694,
0.291240687814322,0.298563836950327,0.301598944092377,0.304073300045832,
0.30475905916055,0.305444187575203,0.306030104505483,0.312713720904449,
0.317760280930702,0.323566375723472,0.32540416659242,0.326816560433781,
0.329048274516511,0.33418691579389,0.339295415530195,0.341572983271978,
0.343355722688849,0.346097461408071,0.347784540996557,0.353350479362486,
0.357419122602839,0.359260829175887,0.360777612445794,0.362205588068618,
0.363994474172703,0.370434870678895),.UNSPECIFIED.) ;
#3313 = B_SPLINE_CURVE_WITH_KNOTS('',3,(#18443,#18444,#18445,#18446,#18447,
#18448,#18449,#18450,#18451,#18452,#18453,#18454,#18455,#18456,#18457,#18458),
 .UNSPECIFIED.,.T.,.F.,(4,1,1,1,1,1,1,1,1,1,1,1,1,4),(0.,0.520304865070705,
0.709542561390409,0.804161409708611,0.898780258026813,1.15893269056541,
1.419085123104,1.67923755563226,1.93938998816052,2.03400883639567,2.12862768463082,
2.31786538114359,2.57801781366682,2.83817024619004),.UNSPECIFIED.) ;
#3314 = B_SPLINE_CURVE_WITH_KNOTS('',3,(#18460,#18461,#18462,#18463,#18464,
#18465,#18466,#18467,#18468,#18469,#18470,#18471,#18472,#18473,#18474,#18475),
 .UNSPECIFIED.,.T.,.F.,(4,1,1,1,1,1,1,1,1,1,1,1,1,4),(0.,0.520304865043955,
0.70954256158844,0.804161409794499,0.898780258000557,1.15893269054429,1.41908512308802,
1.67923755561058,1.93938998813313,2.03400883648099,2.12862768482886,2.3178653810957,
2.57801781365659,2.83817024621747),.UNSPECIFIED.) ;
#3315 = B_SPLINE_CURVE_WITH_KNOTS('',3,(#18477,#18478,#18479,#18480,#18481,
#18482,#18483,#18484,#18485,#18486,#18487,#18488,#18489,#18490,#18491,#18492),
 .UNSPECIFIED.,.T.,.F.,(4,1,1,1,1,1,1,1,1,1,1,1,1,4),(0.,0.520304864990006,
0.709542561256855,0.80416140961432,0.898780257971786,1.15893269048473,1.41908512299766,
1.67923755554141,1.93938998808516,2.03400883629124,2.12862768449733,2.31786538104175,
2.57801781362961,2.83817024621746),.UNSPECIFIED.) ;
#3316 = B_SPLINE_CURVE_WITH_KNOTS('',3,(#18494,#18495,#18496,#18497,#18498,
#18499,#18500,#18501,#18502,#18503,#18504,#18505,#18506,#18507,#18508,#18509),
 .UNSPECIFIED.,.T.,.F.,(4,1,1,1,1,1,1,1,1,1,1,1,1,4),(0.,0.520304865114576,
0.709542561608101,0.804161409843274,0.898780258078447,1.1589326906067,1.41908512313495,
1.67923755567353,1.9393899882121,2.03400883653032,2.12862768484853,2.31786538116822,
2.57801781373375,2.83817024629929),.UNSPECIFIED.) ;
#3317 = B_SPLINE_CURVE_WITH_KNOTS('',3,(#18512,#18513,#18514,#18515,#18516,
#18517,#18518,#18519,#18520,#18521,#18522,#18523,#18524,#18525,#18526,#18527,
#18528,#18529,#18530),.UNSPECIFIED.,.T.,.F.,(4,1,1,1,1,1,1,1,1,1,1,1,1,
1,1,1,4),(0.,0.667571568814075,1.33514313762815,2.00271471386764,2.67028629010714,
3.33785785892123,4.00542942773531,4.67300100397479,5.34057258021427,6.00814415645105,
6.67571573268784,7.34328730150191,8.01085887031598,8.67843044655548,9.34600202279497,
10.0135735916091,10.6811451604231),.UNSPECIFIED.) ;
#3318 = B_SPLINE_CURVE_WITH_KNOTS('',3,(#18532,#18533,#18534,#18535,#18536,
#18537,#18538,#18539,#18540,#18541,#18542,#18543,#18544,#18545,#18546,#18547,
#18548,#18549,#18550,#18551,#18552,#18553,#18554,#18555,#18556,#18557,#18558,
#18559,#18560,#18561,#18562,#18563,#18564,#18565,#18566,#18567,#18568,#18569,
#18570,#18571,#18572,#18573,#18574,#18575,#18576,#18577,#18578,#18579,#18580,
#18581,#18582,#18583,#18584,#18585,#18586,#18587,#18588,#18589,#18590,#18591,
#18592,#18593,#18594,#18595,#18596,#18597,#18598,#18599,#18600,#18601,#18602,
#18603,#18604,#18605,#18606,#18607),.UNSPECIFIED.,.F.,.F.,(4,3,3,3,3,3,
3,3,3,3,3,3,3,3,3,3,3,3,3,3,3,3,3,3,3,4),(0.645166102166136,0.779260260223949,
0.953432776292934,1.00087899502182,1.2245538215817,1.38792237623853,1.45262949361123,
1.68236582634801,1.91465733457253,2.07687507662671,2.15140541324293,2.35410717544614,
2.38890591237544,2.56658916175515,2.63160106806682,2.84272353227155,2.87721416966982,
3.12396628424627,3.34224298985172,3.37420303087565,3.57733400929029,3.62763142462921,
3.88309575096213,4.05946355048951,4.14300211392098,4.256701237387),
 .UNSPECIFIED.) ;
#3319 = B_SPLINE_CURVE_WITH_KNOTS('',3,(#18608,#18609,#18610,#18611,#18612,
#18613,#18614,#18615,#18616,#18617,#18618,#18619,#18620,#18621,#18622,#18623,
#18624,#18625,#18626,#18627,#18628,#18629,#18630,#18631,#18632,#18633,#18634,
#18635,#18636,#18637,#18638,#18639,#18640,#18641,#18642,#18643,#18644,#18645,
#18646,#18647,#18648,#18649,#18650,#18651,#18652,#18653,#18654,#18655,#18656,
#18657,#18658,#18659,#18660,#18661,#18662,#18663,#18664,#18665,#18666,#18667,
#18668,#18669,#18670,#18671,#18672,#18673,#18674,#18675,#18676,#18677,#18678,
#18679,#18680,#18681,#18682,#18683,#18684,#18685,#18686,#18687,#18688,#18689,
#18690,#18691,#18692,#18693,#18694,#18695,#18696,#18697,#18698),
 .UNSPECIFIED.,.F.,.F.,(4,3,3,3,3,3,3,3,3,3,3,3,3,3,3,3,3,3,3,3,3,3,3,3,
3,3,3,3,3,3,4),(2.65072463961435E-14,0.145660370872957,0.320807895379567,
0.40519534671499,0.64591367467841,0.660293540743808,0.857679476426317,0.913841563973973,
1.11044144600034,1.16384460786289,1.38186603893937,1.40950020307555,1.5735409420364,
1.65456863850231,1.8674834420843,1.89503815818863,2.07745338563794,2.13417126051133,
2.32367309259648,2.37029532866498,2.58949458425784,2.60221850258879,2.76061048665942,
2.83266354337296,3.04253537567105,3.05893725264363,3.22614498180073,3.28375110259138,
3.46729051496174,3.5046955288712,3.61218581593466),.UNSPECIFIED.) ;
#3320 = B_SPLINE_CURVE_WITH_KNOTS('',3,(#18701,#18702,#18703,#18704,#18705,
#18706,#18707,#18708,#18709,#18710,#18711,#18712,#18713,#18714,#18715,#18716,
#18717,#18718,#18719),.UNSPECIFIED.,.T.,.F.,(4,1,1,1,1,1,1,1,1,1,1,1,1,
1,1,1,4),(0.,0.66757156881407,1.33514313762814,2.00271471386764,2.67028629010714,
3.33785785892123,4.00542942773532,4.67300100397479,5.34057258021426,6.00814415645105,
6.67571573268784,7.34328730150192,8.01085887031599,8.67843044655547,9.34600202279495,
10.013573591609,10.6811451604231),.UNSPECIFIED.) ;
#3321 = B_SPLINE_CURVE_WITH_KNOTS('',3,(#18721,#18722,#18723,#18724,#18725,
#18726,#18727,#18728,#18729,#18730,#18731,#18732,#18733,#18734,#18735,#18736,
#18737,#18738,#18739,#18740,#18741,#18742,#18743,#18744,#18745,#18746,#18747,
#18748,#18749,#18750,#18751,#18752,#18753,#18754,#18755,#18756,#18757,#18758,
#18759,#18760,#18761,#18762,#18763,#18764,#18765,#18766,#18767,#18768,#18769,
#18770,#18771,#18772,#18773,#18774,#18775,#18776,#18777,#18778,#18779,#18780,
#18781,#18782,#18783,#18784,#18785,#18786,#18787,#18788,#18789,#18790,#18791,
#18792,#18793,#18794,#18795,#18796),.UNSPECIFIED.,.F.,.F.,(4,3,3,3,3,3,
3,3,3,3,3,3,3,3,3,3,3,3,3,3,3,3,3,3,3,4),(0.,0.113699105245172,0.290066601932432,
0.373605432506589,0.629069723752491,0.832200318202323,0.882498082698975,
1.10077464959384,1.13273479495996,1.37948687564694,1.59060880287217,1.62509994351725,
1.80278299829912,1.86779506587701,2.07049658686577,2.10529553239169,2.26751302289565,
2.34204357854793,2.5743350548707,2.80407135605698,2.96743995792939,3.03214699676444,
3.25582179260699,3.42999406441784,3.47744049697027,3.61176015724593),
 .UNSPECIFIED.) ;
#3322 = B_SPLINE_CURVE_WITH_KNOTS('',3,(#18797,#18798,#18799,#18800,#18801,
#18802,#18803,#18804,#18805,#18806,#18807,#18808,#18809,#18810,#18811,#18812,
#18813,#18814,#18815,#18816,#18817,#18818,#18819,#18820,#18821,#18822,#18823,
#18824,#18825,#18826,#18827,#18828,#18829,#18830,#18831,#18832,#18833,#18834,
#18835,#18836,#18837,#18838,#18839,#18840,#18841,#18842,#18843,#18844,#18845,
#18846,#18847,#18848,#18849,#18850,#18851,#18852,#18853,#18854,#18855,#18856,
#18857,#18858,#18859,#18860,#18861,#18862,#18863,#18864,#18865,#18866,#18867,
#18868,#18869,#18870,#18871,#18872,#18873,#18874,#18875,#18876,#18877,#18878,
#18879,#18880,#18881,#18882,#18883,#18884,#18885,#18886,#18887),
 .UNSPECIFIED.,.F.,.F.,(4,3,3,3,3,3,3,3,3,3,3,3,3,3,3,3,3,3,3,3,3,3,3,3,
3,3,3,3,3,3,4),(0.644441410779395,0.75200920201523,0.935549149058043,0.972953628075139,
1.14016174570414,1.1977674777995,1.40763894920845,1.4240411868457,1.58243323607625,
1.65448622740162,1.8736850500751,1.88640940109609,2.07591169111657,2.12253346901659,
2.3049493882588,2.36166657110351,2.57458028242975,2.6021360905531,2.76617690465824,
2.84720452573892,3.06522545761094,3.09286012071041,3.28946054370769,3.34286316435422,
3.54024970390616,3.59641118733614,3.8371274811361,3.85150938111551,4.02665714187106,
4.11104435670409,4.25670473004031),.UNSPECIFIED.) ;
#3323 = B_SPLINE_CURVE_WITH_KNOTS('',3,(#25952,#25953,#25954,#25955,#25956,
#25957,#25958,#25959,#25960,#25961,#25962,#25963,#25964),.UNSPECIFIED.,
 .F.,.F.,(4,3,3,3,4),(0.00254885090942774,0.0798589394093864,0.156372123655699,
0.227373986667402,0.232885307902011),.UNSPECIFIED.) ;
#3324 = B_SPLINE_CURVE_WITH_KNOTS('',3,(#25966,#25967,#25968,#25969,#25970,
#25971,#25972,#25973,#25974,#25975,#25976,#25977,#25978,#25979,#25980,#25981,
#25982,#25983,#25984,#25985,#25986,#25987,#25988,#25989,#25990,#25991,#25992,
#25993,#25994,#25995,#25996,#25997,#25998,#25999,#26000,#26001,#26002,#26003,
#26004,#26005,#26006,#26007,#26008,#26009,#26010,#26011,#26012,#26013,#26014,
#26015,#26016,#26017,#26018,#26019,#26020,#26021,#26022,#26023,#26024,#26025,
#26026,#26027,#26028,#26029,#26030,#26031,#26032),.UNSPECIFIED.,.F.,.F.,
(4,3,3,3,3,3,3,3,3,3,3,3,3,3,3,3,3,3,3,3,3,3,4),(0.827865437902791,0.969498970179885,
1.21799523287345,1.38410983938184,1.46526269189611,1.66145193054325,1.70762278107361,
1.87143425230401,1.94910503522581,2.16981824391288,2.18634151562757,2.36300905408328,
2.42204214196616,2.61858944195816,2.65392288419624,2.88181125820872,3.05474643104765,
3.10884237347622,3.2820669169133,3.33241696329946,3.53151864647208,3.55138037599939,
3.61142664742073),.UNSPECIFIED.) ;
#3325 = B_SPLINE_CURVE_WITH_KNOTS('',3,(#26033,#26034,#26035,#26036,#26037,
#26038,#26039,#26040,#26041,#26042,#26043,#26044,#26045,#26046,#26047,#26048,
#26049,#26050,#26051,#26052,#26053,#26054,#26055,#26056,#26057,#26058,#26059,
#26060,#26061,#26062,#26063,#26064,#26065,#26066,#26067,#26068,#26069,#26070,
#26071,#26072,#26073,#26074,#26075,#26076,#26077,#26078,#26079,#26080,#26081,
#26082,#26083,#26084,#26085,#26086,#26087,#26088,#26089,#26090,#26091,#26092,
#26093,#26094,#26095,#26096,#26097,#26098,#26099,#26100,#26101,#26102,#26103,
#26104,#26105,#26106,#26107,#26108,#26109,#26110,#26111,#26112,#26113,#26114,
#26115,#26116,#26117,#26118,#26119,#26120,#26121,#26122,#26123,#26124,#26125,
#26126,#26127,#26128,#26129,#26130,#26131,#26132,#26133,#26134,#26135,#26136,
#26137,#26138,#26139,#26140,#26141,#26142,#26143,#26144,#26145,#26146,#26147,
#26148,#26149,#26150,#26151,#26152,#26153,#26154,#26155,#26156,#26157,#26158,
#26159,#26160,#26161,#26162,#26163,#26164,#26165,#26166,#26167,#26168,#26169,
#26170,#26171,#26172,#26173,#26174,#26175,#26176,#26177,#26178,#26179,#26180,
#26181,#26182,#26183,#26184,#26185,#26186,#26187,#26188,#26189,#26190,#26191,
#26192,#26193,#26194,#26195,#26196,#26197,#26198,#26199,#26200,#26201,#26202,
#26203,#26204,#26205,#26206,#26207,#26208,#26209,#26210,#26211,#26212,#26213,
#26214,#26215,#26216,#26217,#26218,#26219,#26220,#26221,#26222,#26223,#26224,
#26225,#26226,#26227,#26228,#26229,#26230,#26231,#26232,#26233,#26234,#26235,
#26236,#26237,#26238,#26239,#26240,#26241,#26242,#26243,#26244,#26245,#26246,
#26247,#26248,#26249,#26250,#26251,#26252,#26253,#26254,#26255,#26256,#26257,
#26258,#26259,#26260,#26261,#26262,#26263,#26264,#26265,#26266),
 .UNSPECIFIED.,.F.,.F.,(4,2,2,2,2,2,2,2,2,2,2,2,2,2,2,2,2,2,2,2,2,2,2,2,
2,2,2,2,2,2,2,2,2,2,2,2,2,2,2,2,2,2,2,2,2,2,2,2,2,2,2,2,2,2,2,2,2,2,2,2,
2,2,2,2,2,2,2,2,2,2,2,2,2,2,2,2,2,2,2,2,2,2,2,2,2,2,2,2,2,2,2,2,2,2,2,2,
2,2,2,2,2,2,2,2,2,2,2,2,2,2,2,2,2,2,2,2,4),(1.00011841232436E-6,0.00211487568124348,
0.00573504524170948,0.0105552052984136,0.013206038817188,0.0149819498688102,
0.0165674239395606,0.0182978612274979,0.0210987487537411,0.0278207031606176,
0.0325576793304593,0.0349535909101199,0.0374295225247761,0.0441510043973029,
0.0467789452193183,0.0486016307238571,0.0500606344083361,0.0531874431833309,
0.0585847367877814,0.061095445986784,0.0630628385785719,0.0657374888256804,
0.0741503815625694,0.0773889156137434,0.0796579552177498,0.0807688356105725,
0.0831046581995265,0.0871216394910236,0.0924688277337361,0.0956070243899364,
0.0989528606039263,0.106157070817436,0.109664151060947,0.112189673083253,
0.114183844036864,0.120195774072755,0.123225376896897,0.125013914410265,
0.125072206216835,0.125127793145369,0.125180993795639,0.125232100146867,
0.125281381546994,0.125329088683266,0.125375457257543,0.125420711238155,
0.125465066274631,0.125508733230266,0.125551921586471,0.125594843368815,
0.125637717537804,0.125680774972013,0.125724264618053,0.125768461261691,
0.125813675253946,0.125860265868866,0.125908659536032,0.125959375243851,
0.126013062148227,0.126070556325349,0.126132970718823,0.126201845154774,
0.126259063080509,0.126393996284037,0.127819373950443,0.129258214424421,
0.131110074945505,0.134186015138983,0.143305528015856,0.146054540687782,
0.147480969448531,0.148562805052782,0.149680232155087,0.149737317074787,
0.149799262331264,0.149866431189701,0.149894352585556,0.149929710577313,
0.151384856346816,0.153687973533875,0.158498449384403,0.166624947623936,
0.168158596691493,0.168993930820365,0.16982272504412,0.170635089478444,
0.171279550802086,0.172645679114621,0.175150864479718,0.182316618022404,
0.182679082917977,0.188178400224613,0.18968495109763,0.190545811688084,
0.191407957865223,0.192485536340025,0.194677082028042,0.197748855900557,
0.2033441185278,0.209436941624861,0.210950745000197,0.211819874549075,0.21269313079068,
0.213580580305497,0.213868320544485,0.214583360312335,0.216366268847191,
0.220199054862944,0.228694348237006,0.230899224185619,0.232466907354201,
0.234074279046871,0.23578755192576,0.244157487005655,0.250074754468557,
0.25296313407621,0.255635388345462),.UNSPECIFIED.) ;
#3326 = B_SPLINE_CURVE_WITH_KNOTS('',3,(#33239,#33240,#33241,#33242,#33243,
#33244,#33245,#33246,#33247,#33248,#33249,#33250,#33251),.UNSPECIFIED.,
 .F.,.F.,(4,3,3,3,4),(0.,0.077810894493114,0.156406594156863,0.238224767252187,
0.302239126484708),.UNSPECIFIED.) ;
#3327 = B_SPLINE_CURVE_WITH_KNOTS('',3,(#33253,#33254,#33255,#33256,#33257,
#33258,#33259,#33260,#33261,#33262,#33263,#33264,#33265,#33266,#33267,#33268,
#33269,#33270,#33271,#33272,#33273,#33274,#33275,#33276,#33277,#33278,#33279,
#33280,#33281,#33282,#33283,#33284,#33285,#33286,#33287,#33288,#33289,#33290,
#33291,#33292,#33293,#33294,#33295,#33296,#33297,#33298,#33299,#33300,#33301,
#33302,#33303,#33304,#33305,#33306,#33307,#33308,#33309,#33310,#33311,#33312,
#33313,#33314,#33315,#33316,#33317,#33318,#33319,#33320,#33321,#33322,#33323,
#33324,#33325),.UNSPECIFIED.,.F.,.F.,(4,3,3,3,3,3,3,3,3,3,3,3,3,3,3,3,3,
3,3,3,3,3,3,3,4),(0.730465481580954,0.828645125064015,1.05028297683292,
1.25837815007314,1.27510983870171,1.45572385055039,1.50312162767456,1.73316624271265,
1.90167574230091,1.96765453876245,2.20387853992391,2.44262970595965,2.62527594874775,
2.68580352301486,2.90417726727137,2.9307933308959,3.16390700344848,3.17732285394432,
3.35312908465983,3.42916468918551,3.68305064914715,3.93956813737863,4.12212044382143,
4.19992860565306,4.25678609882998),.UNSPECIFIED.) ;
#3328 = B_SPLINE_CURVE_WITH_KNOTS('',3,(#33326,#33327,#33328,#33329,#33330,
#33331,#33332,#33333,#33334,#33335,#33336,#33337,#33338,#33339,#33340,#33341,
#33342,#33343,#33344),.UNSPECIFIED.,.F.,.F.,(4,1,1,1,1,1,1,1,1,1,1,1,1,
1,1,1,4),(87.336489761411,87.4317045853384,87.8665778926469,88.3014512000977,
88.7363245076919,89.1711978154302,89.6060711233134,90.0409444313423,90.4758177395175,
90.9106910478396,91.345564356309,91.7804376649263,92.2153109736917,92.6501842826055,
93.085057591668,93.5199309008791,93.8817096841969),.UNSPECIFIED.) ;
#3329 = B_SPLINE_CURVE_WITH_KNOTS('',3,(#33352,#33353,#33354,#33355,#33356,
#33357),.UNSPECIFIED.,.F.,.F.,(4,2,4),(-0.0221113024783476,-0.0110566426889343,
-1.00008409958761E-6),.UNSPECIFIED.) ;
#3330 = B_SPLINE_CURVE_WITH_KNOTS('',3,(#33359,#33360,#33361,#33362,#33363,
#33364,#33365,#33366,#33367,#33368,#33369,#33370,#33371,#33372,#33373,#33374,
#33375,#33376,#33377,#33378,#33379,#33380,#33381,#33382,#33383,#33384,#33385,
#33386,#33387,#33388,#33389,#33390,#33391,#33392,#33393,#33394,#33395,#33396,
#33397,#33398,#33399,#33400,#33401,#33402,#33403,#33404,#33405,#33406,#33407,
#33408,#33409,#33410,#33411,#33412,#33413,#33414,#33415,#33416,#33417,#33418,
#33419,#33420,#33421,#33422,#33423,#33424,#33425,#33426,#33427,#33428,#33429,
#33430,#33431,#33432,#33433,#33434,#33435,#33436,#33437,#33438,#33439,#33440,
#33441,#33442,#33443,#33444,#33445,#33446,#33447,#33448,#33449,#33450,#33451,
#33452,#33453,#33454,#33455,#33456,#33457,#33458,#33459,#33460,#33461,#33462,
#33463,#33464,#33465,#33466,#33467,#33468,#33469,#33470,#33471,#33472,#33473,
#33474,#33475,#33476,#33477,#33478,#33479,#33480,#33481,#33482,#33483,#33484,
#33485,#33486,#33487,#33488,#33489,#33490,#33491,#33492,#33493,#33494,#33495,
#33496,#33497,#33498,#33499,#33500,#33501,#33502,#33503,#33504,#33505,#33506,
#33507,#33508,#33509,#33510,#33511,#33512,#33513,#33514,#33515,#33516,#33517,
#33518,#33519,#33520,#33521,#33522,#33523,#33524,#33525,#33526,#33527,#33528,
#33529,#33530,#33531,#33532,#33533,#33534,#33535,#33536,#33537,#33538,#33539,
#33540,#33541,#33542,#33543,#33544,#33545,#33546,#33547,#33548,#33549,#33550,
#33551,#33552,#33553,#33554,#33555,#33556,#33557,#33558,#33559,#33560,#33561,
#33562,#33563,#33564,#33565,#33566,#33567,#33568,#33569,#33570,#33571,#33572,
#33573,#33574,#33575,#33576,#33577,#33578,#33579,#33580,#33581,#33582,#33583,
#33584,#33585,#33586,#33587,#33588,#33589,#33590,#33591,#33592,#33593,#33594,
#33595,#33596,#33597,#33598,#33599,#33600,#33601,#33602,#33603,#33604,#33605,
#33606,#33607,#33608,#33609,#33610,#33611,#33612,#33613,#33614,#33615,#33616,
#33617,#33618,#33619,#33620,#33621,#33622,#33623,#33624,#33625,#33626,#33627,
#33628,#33629,#33630,#33631,#33632,#33633,#33634,#33635,#33636,#33637,#33638,
#33639,#33640,#33641,#33642,#33643,#33644,#33645,#33646,#33647,#33648,#33649,
#33650,#33651,#33652,#33653,#33654,#33655,#33656,#33657,#33658,#33659,#33660,
#33661,#33662,#33663,#33664,#33665,#33666,#33667,#33668,#33669,#33670,#33671,
#33672,#33673,#33674,#33675,#33676,#33677,#33678,#33679,#33680,#33681,#33682,
#33683,#33684,#33685,#33686,#33687,#33688,#33689,#33690,#33691,#33692,#33693,
#33694,#33695,#33696,#33697,#33698,#33699,#33700,#33701,#33702,#33703,#33704,
#33705,#33706,#33707,#33708,#33709,#33710,#33711,#33712,#33713,#33714,#33715,
#33716,#33717,#33718,#33719,#33720,#33721,#33722,#33723,#33724,#33725,#33726,
#33727,#33728,#33729,#33730,#33731,#33732,#33733,#33734,#33735,#33736,#33737,
#33738,#33739,#33740,#33741,#33742,#33743,#33744,#33745,#33746,#33747,#33748,
#33749,#33750,#33751,#33752,#33753,#33754,#33755,#33756,#33757,#33758,#33759,
#33760,#33761,#33762,#33763,#33764,#33765,#33766,#33767,#33768,#33769,#33770,
#33771,#33772,#33773,#33774,#33775,#33776,#33777,#33778,#33779,#33780,#33781,
#33782,#33783,#33784,#33785,#33786,#33787,#33788,#33789,#33790,#33791,#33792,
#33793,#33794,#33795,#33796,#33797,#33798,#33799,#33800,#33801,#33802,#33803,
#33804,#33805,#33806,#33807,#33808,#33809,#33810,#33811,#33812,#33813,#33814,
#33815,#33816,#33817,#33818,#33819,#33820,#33821,#33822,#33823,#33824,#33825,
#33826,#33827,#33828,#33829,#33830,#33831,#33832,#33833,#33834,#33835,#33836,
#33837,#33838,#33839,#33840,#33841,#33842,#33843,#33844,#33845,#33846,#33847,
#33848,#33849,#33850,#33851,#33852,#33853,#33854,#33855,#33856,#33857,#33858,
#33859,#33860,#33861,#33862,#33863,#33864,#33865,#33866,#33867,#33868,#33869,
#33870,#33871,#33872,#33873,#33874,#33875,#33876,#33877,#33878,#33879,#33880,
#33881,#33882,#33883,#33884,#33885,#33886,#33887,#33888,#33889,#33890,#33891,
#33892,#33893,#33894,#33895,#33896,#33897,#33898,#33899,#33900,#33901,#33902,
#33903,#33904,#33905,#33906,#33907,#33908,#33909,#33910,#33911,#33912,#33913,
#33914,#33915,#33916,#33917,#33918,#33919,#33920,#33921,#33922,#33923,#33924,
#33925,#33926,#33927,#33928,#33929,#33930,#33931,#33932,#33933,#33934,#33935,
#33936,#33937,#33938,#33939,#33940,#33941,#33942,#33943,#33944,#33945,#33946,
#33947,#33948,#33949,#33950,#33951,#33952,#33953,#33954,#33955,#33956,#33957,
#33958,#33959,#33960,#33961,#33962,#33963,#33964,#33965,#33966,#33967,#33968,
#33969,#33970,#33971,#33972,#33973,#33974,#33975,#33976,#33977,#33978,#33979,
#33980,#33981,#33982,#33983,#33984,#33985,#33986,#33987,#33988,#33989,#33990,
#33991,#33992,#33993,#33994,#33995,#33996,#33997,#33998,#33999,#34000,#34001,
#34002,#34003,#34004,#34005,#34006,#34007,#34008,#34009,#34010,#34011,#34012,
#34013,#34014,#34015,#34016,#34017,#34018,#34019,#34020,#34021,#34022,#34023,
#34024,#34025,#34026,#34027,#34028,#34029,#34030,#34031,#34032,#34033,#34034,
#34035,#34036,#34037,#34038,#34039,#34040,#34041,#34042,#34043,#34044,#34045,
#34046,#34047,#34048,#34049,#34050,#34051,#34052,#34053,#34054,#34055,#34056,
#34057,#34058,#34059,#34060,#34061,#34062,#34063,#34064,#34065,#34066,#34067,
#34068,#34069,#34070,#34071,#34072,#34073,#34074,#34075,#34076,#34077,#34078,
#34079,#34080,#34081,#34082,#34083,#34084,#34085,#34086,#34087,#34088,#34089,
#34090,#34091,#34092,#34093,#34094,#34095,#34096,#34097,#34098,#34099,#34100,
#34101,#34102,#34103,#34104,#34105,#34106,#34107,#34108,#34109,#34110,#34111,
#34112,#34113,#34114,#34115,#34116,#34117,#34118,#34119,#34120,#34121,#34122,
#34123,#34124,#34125,#34126,#34127,#34128,#34129,#34130,#34131,#34132,#34133,
#34134,#34135,#34136,#34137,#34138,#34139,#34140,#34141,#34142),
 .UNSPECIFIED.,.F.,.F.,(4,2,2,2,2,2,2,2,2,2,2,2,2,2,2,2,2,2,2,2,2,2,2,2,
2,2,2,2,2,2,2,2,2,2,2,2,2,2,2,2,2,2,2,2,2,2,2,2,2,2,2,2,2,2,2,2,2,2,2,2,
2,2,2,2,2,2,2,2,2,2,2,2,2,2,2,2,2,2,2,2,2,2,2,2,2,2,2,2,2,2,2,2,2,2,2,2,
2,2,2,2,2,2,2,2,2,2,2,2,2,2,2,2,2,2,2,2,2,2,2,2,2,2,2,2,2,2,2,2,2,2,2,2,
2,2,2,2,2,2,2,2,2,2,2,2,2,2,2,2,2,2,2,2,2,2,2,2,2,2,2,2,2,2,2,2,2,2,2,2,
2,2,2,2,2,2,2,2,2,2,2,2,2,2,2,2,2,2,2,2,2,2,2,2,2,2,2,2,2,2,2,2,2,2,2,2,
2,2,2,2,2,2,2,2,2,2,2,2,2,2,2,2,2,2,2,2,2,2,2,2,2,2,2,2,2,2,2,2,2,2,2,2,
2,2,2,2,2,2,2,2,2,2,2,2,2,2,2,2,2,2,2,2,2,2,2,2,2,2,2,2,2,2,2,2,2,2,2,2,
2,2,2,2,2,2,2,2,2,2,2,2,2,2,2,2,2,2,2,2,2,2,2,2,2,2,2,2,2,2,2,2,2,2,2,2,
2,2,2,2,2,2,2,2,2,2,2,2,2,2,2,2,2,2,2,2,2,2,2,2,2,2,2,2,2,2,2,2,2,2,2,2,
2,2,2,2,2,2,2,2,2,2,2,2,2,2,2,2,2,2,2,2,2,2,2,2,2,2,2,2,2,2,2,2,2,2,2,2,
2,2,2,2,2,2,2,4),(1.00000001682088E-6,0.00412378435184989,0.00720393598231871,
0.0103717437260683,0.0145585560623559,0.0244680661083784,0.0329545253558829,
0.0425764562482095,0.0440725730601049,0.0451152033327152,0.0460124834422306,
0.046934990694426,0.0481632294947072,0.050724122983898,0.0630557572617355,
0.0756411641465513,0.0813714533000482,0.0846115376600266,0.0868137062066845,
0.0886335553345215,0.0903716139373155,0.0926078484500323,0.0964385758774219,
0.110549659029758,0.121459739409565,0.129033302174599,0.130760319639646,
0.131651475686724,0.13256791807344,0.133625596671386,0.135410993071053,
0.142996697469524,0.155349098660419,0.163677401609616,0.167444141957419,
0.170440984965391,0.173893558787823,0.180700035175655,0.203153850559646,
0.208964366471218,0.212113722160231,0.212181573822733,0.212246701945834,
0.212309247893573,0.212369344911492,0.212427118577817,0.212482687279601,
0.212536162672608,0.212587650052935,0.212637248730231,0.212685052495241,
0.212731149867509,0.212775624407095,0.212818555053062,0.212860016364252,
0.212900078783675,0.212938809005543,0.212976269956484,0.213012521237669,
0.213047619261203,0.213081617320833,0.213114566013228,0.213146513186833,
0.213177504145674,0.213207581900862,0.213236787245495,0.213265158841159,
0.213292733336209,0.213319545600158,0.213345628689971,0.213371014017961,
0.213395731397533,0.213419809318236,0.213443274783266,0.213466153519028,
0.213488469935302,0.213510247310883,0.213531507949612,0.213552272981879,
0.213572562581441,0.213592396070832,0.213611791795321,0.213630767294437,
0.213649339348355,0.21366752401514,0.213685336572033,0.213702791695819,
0.213719903515766,0.213736685484902,0.213753150432965,0.213769310728772,
0.21378517818009,0.21380076423114,0.213816079672839,0.213831134968361,0.213845940413858,
0.213860505553586,0.213874839687762,0.213888951851384,0.213902850598825,
0.213932756139912,0.213962451140244,0.213991944588857,0.214021245372558,
0.214050362396523,0.21407930444072,0.21410808025762,0.214136698534644,0.214165167899702,
0.214193497034036,0.214221694551859,0.2142497691563,0.216316764564342,0.21852724166571,
0.222391601619717,0.233412192448542,0.237938484265656,0.239269823749761,
0.240130520900268,0.240495793723779,0.241009367005868,0.242468317341029,
0.247176360858102,0.256709502061751,0.260325910001816,0.262967487383116,
0.262976550055926,0.262985547006863,0.262994478949593,0.263003346688414,
0.263012151095934,0.263020892846339,0.263029572691251,0.263038191357084,
0.263046749477224,0.263055247941868,0.263063687659736,0.263072069032241,
0.263080392853637,0.263088659913182,0.263096870891574,0.263105026435826,
0.263113127286558,0.263121173964806,0.263129167089014,0.263137107431365,
0.263144995519346,0.263152832068115,0.263160617799678,0.263168353033123,
0.263176038461129,0.263183674782712,0.26319126272822,0.263198802642571,
0.263206295194712,0.263213741094152,0.263221140664439,0.263228494507098,
0.263235803269919,0.263243067523899,0.263250287803804,0.263257464673431,
0.263264598540779,0.263271689890335,0.263278739290234,0.263285747295609,
0.263292714458167,0.263299641321257,0.263306528372713,0.26331337601404,
0.263320184523784,0.263326954678803,0.263333686681642,0.263340381199479,
0.263347038813512,0.263353659761591,0.263360244580434,0.263366793603721,
0.26337330735734,0.263379786216298,0.263386230638156,0.26339264105942,0.263399017864931,
0.263405361587141,0.263411672563466,0.263417951327975,0.263424198117529,
0.263430413386007,0.263436597660909,0.263442751083506,0.263448874031492,
0.263454967274796,0.263461030978515,0.263467065444312,0.263473071031463,
0.263479048115547,0.26348499719065,0.263490918600648,0.263496812378503,
0.263502679415271,0.263508519888591,0.263514334030613,0.263520121950217,
0.263525884178365,0.263531621317426,0.263537333562649,0.263543021217466,
0.263548684527306,0.26355432378257,0.263559939476474,0.26356553220086,0.263571101903078,
0.26357664882651,0.263582173188598,0.263587675623338,0.263593156231263,
0.263598615319778,0.263604053269746,0.263609470391771,0.263614866889543,
0.26362024322544,0.263625599643742,0.263630936585898,0.263636254096805,
0.263641552456102,0.263646831847872,0.263652092608879,0.263657335218632,
0.263662559954704,0.263667766857738,0.263672956340642,0.263678128674226,
0.263683284231555,0.263688422961633,0.263693545507355,0.263698652084501,
0.263703742717273,0.263708818049715,0.263713878119357,0.263718922833078,
0.26372395284085,0.26372896824138,0.263733969297089,0.263738956503716,0.263743929821177,
0.263748889334407,0.263753835587936,0.263758768884115,0.263763689325482,
0.263768597440996,0.263773493243255,0.263778377033001,0.263783249035293,
0.263788109318664,0.263792958270771,0.263797796190937,0.263802623000511,
0.263807439149299,0.263812244968126,0.263817040702161,0.263821826455816,
0.263826602693428,0.263831369545261,0.263836126972638,0.263840875287213,
0.2638456147326,0.263850345569688,0.263855068225747,0.263859782816834,0.263864489633565,
0.263869188717774,0.263873880213536,0.265401600255821,0.266952459355332,
0.269475389911629,0.277313206724315,0.28897782029383,0.29680510177015,0.302454562050922,
0.306773756205715,0.310418199298673,0.314420940817946,0.319531495145557,
0.337589015000251,0.343318491153592,0.345973977396469,0.348070856727646,
0.34924830229069,0.350317526017165,0.351700343117464,0.354135128192724,
0.368622453128095,0.37328553484783,0.375179706387552,0.378580431548132,
0.381216461170867,0.383203158061469,0.393168494486374,0.405892027088247,
0.414901388307961,0.418941628677775,0.431399265051532,0.434934023162209,
0.43826011895309,0.442047228602453,0.448707942327242,0.450636832431272,
0.455673185951709,0.457711421550039,0.459369612802801,0.459393312537367,
0.459418300524679,0.459444670008319,0.461107089664572,0.464102834781033,
0.474294649944849,0.478469544933861,0.480777478216863,0.483091943086908,
0.485584314396763,0.489201048388902,0.49743706517905,0.498560540151176,
0.502130853319476,0.503676616615559,0.505311218089556,0.507306934747305,
0.510681185550213,0.522412328781764,0.524853424365672,0.52832725682492,
0.532028675715041,0.538308483071323,0.544544439139152,0.546692055961045,
0.548563315398212,0.548816900362078,0.549061281778513,0.549493119504176,
0.552992927585461,0.565070061983992,0.568331469467836,0.57196600242079,
0.576351091695299,0.581912985310773,0.58757768752732,0.589810159141457,
0.591607083077002,0.591973682452946,0.592227919713621,0.595420724217392,
0.605818271537551,0.609795976107658,0.613252592277516,0.617136578941486,
0.624359334370696,0.629340571199528,0.631327527801954,0.632953647429156,
0.634520487477763,0.637129649028583,0.644471683708734,0.651701706861225,
0.654404126261276,0.656417672709504,0.658388187756684,0.660761646549056,
0.66447217565491,0.673649019142133,0.677975885884396,0.680721260710457,
0.683544414440198,0.68754435673873,0.700974075705117,0.708499933748802,
0.71587279908506,0.718924768869659,0.722413104893756,0.72800993542403,0.737282377918865,
0.740350329593211,0.742684396226621,0.745136271957237,0.748306111782994,
0.754030433416531,0.762682415799703,0.764638709251022,0.766387126543181,
0.768545119657253,0.776581200999748,0.782397828470698,0.786290042297251),
 .UNSPECIFIED.) ;
#3331 = B_SPLINE_CURVE_WITH_KNOTS('',3,(#34143,#34144,#34145,#34146,#34147,
#34148,#34149,#34150,#34151,#34152,#34153,#34154,#34155,#34156,#34157,#34158,
#34159,#34160,#34161,#34162,#34163,#34164,#34165,#34166,#34167,#34168,#34169,
#34170,#34171,#34172,#34173,#34174,#34175,#34176,#34177,#34178,#34179,#34180,
#34181,#34182,#34183,#34184,#34185,#34186,#34187,#34188,#34189,#34190,#34191,
#34192,#34193,#34194,#34195,#34196,#34197,#34198,#34199,#34200,#34201,#34202,
#34203,#34204,#34205,#34206,#34207,#34208,#34209,#34210,#34211,#34212,#34213,
#34214,#34215,#34216,#34217,#34218,#34219,#34220,#34221,#34222,#34223,#34224,
#34225,#34226,#34227,#34228,#34229,#34230,#34231,#34232,#34233,#34234,#34235,
#34236,#34237,#34238,#34239,#34240,#34241,#34242,#34243,#34244,#34245,#34246,
#34247,#34248,#34249,#34250,#34251,#34252,#34253,#34254,#34255,#34256,#34257),
 .UNSPECIFIED.,.F.,.F.,(4,3,3,3,3,3,3,3,3,3,3,3,3,3,3,3,3,3,3,3,3,3,3,3,
3,3,3,3,3,3,3,3,3,3,3,3,3,3,4),(0.,0.0377030535869255,0.254567771787473,
0.472814106637255,0.691451692099905,0.908523894195214,0.983882498076101,
1.12697364238926,1.34346828606356,1.5611425742692,1.7797791811067,1.96773553890813,
1.9969257592614,2.21556187156847,2.43217608081115,2.65081168252064,2.86814667737748,
2.95162325710805,3.30465282917188,3.52319094343164,3.74168240699446,3.93630861076791,
3.95797636096931,4.17661107076291,4.39376768198014,4.61123898216608,4.92068696075518,
5.04720928317926,5.48426176171593,5.70246546995195,5.90620613535479,5.92104893161303,
6.13805509181114,6.35540620614376,6.79432818927802,6.89176793866042,7.22988061248286,
7.66676952770389,7.87799350781472),.UNSPECIFIED.) ;
#3332 = B_SPLINE_CURVE_WITH_KNOTS('',3,(#41229,#41230,#41231,#41232,#41233,
#41234,#41235,#41236,#41237,#41238,#41239,#41240,#41241,#41242,#41243,#41244,
#41245,#41246,#41247,#41248,#41249,#41250,#41251,#41252,#41253,#41254,#41255,
#41256,#41257,#41258,#41259,#41260,#41261,#41262,#41263,#41264,#41265,#41266,
#41267,#41268,#41269,#41270,#41271,#41272),.UNSPECIFIED.,.F.,.F.,(4,2,2,
2,2,2,2,2,2,2,2,2,2,2,2,2,2,2,2,2,2,4),(0.,0.00971482468978479,0.0203872474063451,
0.0279236293697992,0.0332114727556085,0.0367480813478895,0.0382588296076648,
0.0385204656750401,0.0385321923580342,0.0385402608458808,0.0385454131009185,
0.0385482839226327,0.0385506929760014,0.0385535216348412,0.0385585725934473,
0.0385811991469328,0.0386219012951342,0.0407407599450427,0.0444803773101447,
0.0498412534615488,0.0574206915439498,0.0744461764183355),.UNSPECIFIED.) ;
#3333 = B_SPLINE_CURVE_WITH_KNOTS('',3,(#41273,#41274,#41275,#41276,#41277,
#41278),.UNSPECIFIED.,.F.,.F.,(4,2,4),(9.99929898480087E-7,0.0141909886738071,
0.027570872690399),.UNSPECIFIED.) ;
#3334 = B_SPLINE_CURVE_WITH_KNOTS('',3,(#41279,#41280,#41281,#41282,#41283,
#41284,#41285,#41286,#41287,#41288,#41289,#41290,#41291,#41292,#41293,#41294,
#41295,#41296,#41297,#41298,#41299,#41300,#41301,#41302,#41303,#41304,#41305,
#41306,#41307,#41308,#41309,#41310,#41311,#41312,#41313,#41314,#41315,#41316,
#41317,#41318,#41319,#41320,#41321,#41322,#41323,#41324,#41325,#41326,#41327,
#41328,#41329,#41330,#41331,#41332,#41333,#41334,#41335,#41336,#41337,#41338,
#41339,#41340,#41341,#41342,#41343,#41344,#41345,#41346,#41347,#41348,#41349,
#41350,#41351,#41352,#41353,#41354,#41355,#41356,#41357,#41358,#41359,#41360,
#41361,#41362,#41363,#41364,#41365,#41366,#41367,#41368,#41369,#41370,#41371,
#41372,#41373,#41374,#41375,#41376,#41377,#41378,#41379,#41380,#41381,#41382,
#41383,#41384,#41385,#41386,#41387,#41388,#41389,#41390,#41391,#41392,#41393,
#41394,#41395,#41396,#41397,#41398,#41399,#41400,#41401,#41402,#41403,#41404,
#41405,#41406,#41407,#41408,#41409,#41410,#41411,#41412,#41413,#41414,#41415,
#41416,#41417,#41418,#41419,#41420,#41421,#41422,#41423,#41424,#41425,#41426,
#41427),.UNSPECIFIED.,.F.,.F.,(4,1,1,1,1,1,1,1,1,1,1,1,1,1,1,1,1,1,1,1,
1,1,1,1,1,1,1,1,1,1,1,1,1,1,1,1,1,1,1,1,1,1,1,1,1,1,1,1,1,1,1,1,1,1,1,1,
1,1,1,1,1,1,1,1,1,1,1,1,1,1,1,1,1,1,1,1,1,1,1,1,1,1,1,1,1,1,1,1,1,1,1,1,
1,1,1,1,1,1,1,1,1,1,1,1,1,1,1,1,1,1,1,1,1,1,1,1,1,1,1,1,1,1,1,1,1,1,1,1,
1,1,1,1,1,1,1,1,1,1,1,1,1,1,1,1,1,1,4),(94.7323961409497,94.8262562134414,
95.2611295230986,95.6960028329042,96.1308761428578,96.5657494529591,97.0006227632077,
97.4354960736028,97.870369384144,98.3052426948304,98.7401160056612,99.1749893166354,
99.6098626277522,100.04473593901,100.915335253024,101.351061255639,101.785934567313,
102.220807879124,102.655681191068,103.090554503145,103.525427815353,104.395174440154,
105.264921065453,105.699794378283,106.134667691232,106.569541004295,107.004414317471,
107.8750136343,108.745612951339,109.615359578629,110.485106206296,111.354852834309,
112.224599462639,113.094346091254,113.964092720119,114.834692038763,115.705291357499,
116.575037986826,117.444784616267,118.314531245777,119.184277875311,120.054024504821,
120.923771134261,121.794370453112,122.66496977189,123.534716400968,124.404463029834,
125.274209658448,126.143956286779,127.013702914792,127.883449542458,128.754048859798,
129.624648176939,130.494394803617,131.364141429857,132.233888055637,133.103634680937,
133.973381305737,134.843127930023,135.71372724472,136.584326559147,137.019199870684,
137.454073182083,137.888946493341,138.323819804458,139.193566426263,140.063313047491,
140.498186357887,140.933059668136,141.367932978237,141.802806288191,142.237679597997,
142.673405599673,143.109131601348,143.544004910857,143.978878220217,144.413751529429,
144.848624838491,145.283498147405,145.718371456171,146.153244764789,146.588118073258,
147.022991381581,147.457864689756,147.892737997785,148.327611305669,148.762484613407,
149.197357921002,149.633083921574,150.068809922147,150.503683229455,150.938556536623,
151.37342984365,151.808303150538,152.243176457288,152.678049763901,153.112923070379,
153.547796376722,153.982669682934,154.417542989014,154.852416294964,155.287289600787,
155.722162906483,156.157036212055,156.592762211626,157.028488211198,157.463361516526,
157.898234821735,158.333108126826,158.767981431803,159.202854736666,159.637728041419,
160.072601346062,160.507474650599,160.94234795503,161.37722125936,161.812094563589,
162.246967867721,162.681841171757,163.1167144757,163.552440474473,163.988166473247,
164.423039777011,164.85791308069,165.292786384286,165.727659687801,166.162532991238,
166.597406294601,167.03227959789,167.46715290111,167.902026204262,168.33689950735,
168.771772810376,169.206646113343,169.641519416254,170.076392719112,170.512118717363,
170.947844715614,171.382718018374,171.817591321089,172.252464623762,172.687337926397,
173.122211228996,173.557084531561,173.991957834097,174.426831136606,174.671174277229),
 .UNSPECIFIED.) ;
#3335 = B_SPLINE_CURVE_WITH_KNOTS('',3,(#41434,#41435,#41436,#41437,#41438,
#41439,#41440,#41441,#41442,#41443,#41444,#41445,#41446,#41447,#41448,#41449,
#41450,#41451,#41452,#41453,#41454,#41455,#41456,#41457,#41458,#41459,#41460,
#41461,#41462,#41463,#41464,#41465,#41466,#41467,#41468,#41469,#41470,#41471,
#41472,#41473,#41474,#41475,#41476,#41477,#41478,#41479,#41480,#41481,#41482,
#41483,#41484,#41485,#41486,#41487,#41488,#41489,#41490,#41491),
 .UNSPECIFIED.,.F.,.F.,(4,3,3,3,3,3,3,3,3,3,3,3,3,3,3,3,3,3,3,4),(3.94168901841607,
4.15261423848637,4.16618665983574,4.44281737539361,4.60337687546477,4.92785564904694,
5.03898230867997,5.31950967594945,5.47698109930275,5.91441694228828,5.91506511246863,
6.35152427416674,6.66153035873348,6.78902235094994,6.90225579028163,7.22528631210598,
7.50348627263337,7.66193049212852,7.87484757961294,7.8884094762389),
 .UNSPECIFIED.) ;
#3336 = B_SPLINE_CURVE_WITH_KNOTS('',3,(#41492,#41493,#41494,#41495,#41496,
#41497,#41498,#41499,#41500,#41501,#41502,#41503,#41504,#41505,#41506,#41507,
#41508,#41509,#41510,#41511,#41512,#41513,#41514,#41515,#41516,#41517,#41518,
#41519,#41520,#41521,#41522,#41523,#41524,#41525,#41526,#41527,#41528,#41529,
#41530,#41531,#41532,#41533,#41534,#41535,#41536,#41537,#41538,#41539,#41540,
#41541,#41542,#41543,#41544,#41545,#41546,#41547,#41548,#41549,#41550,#41551,
#41552,#41553,#41554,#41555,#41556,#41557,#41558,#41559,#41560,#41561,#41562,
#41563,#41564,#41565,#41566,#41567,#41568,#41569,#41570,#41571,#41572,#41573,
#41574,#41575,#41576,#41577,#41578,#41579,#41580,#41581,#41582,#41583,#41584,
#41585,#41586,#41587,#41588,#41589,#41590,#41591,#41592,#41593,#41594,#41595,
#41596,#41597,#41598,#41599,#41600,#41601,#41602,#41603,#41604,#41605,#41606,
#41607,#41608,#41609,#41610,#41611,#41612,#41613,#41614,#41615,#41616,#41617,
#41618,#41619,#41620,#41621,#41622,#41623,#41624,#41625,#41626,#41627,#41628,
#41629,#41630,#41631,#41632,#41633,#41634,#41635,#41636,#41637,#41638,#41639,
#41640,#41641,#41642,#41643,#41644,#41645,#41646,#41647,#41648,#41649,#41650,
#41651,#41652,#41653,#41654,#41655,#41656,#41657,#41658,#41659,#41660,#41661,
#41662,#41663,#41664,#41665,#41666,#41667,#41668,#41669,#41670,#41671,#41672,
#41673,#41674,#41675,#41676,#41677,#41678,#41679,#41680,#41681,#41682,#41683,
#41684,#41685,#41686,#41687,#41688,#41689,#41690,#41691,#41692,#41693,#41694,
#41695,#41696,#41697,#41698,#41699,#41700,#41701,#41702,#41703,#41704,#41705,
#41706,#41707,#41708,#41709,#41710,#41711,#41712,#41713,#41714,#41715,#41716,
#41717,#41718,#41719,#41720,#41721,#41722,#41723,#41724,#41725,#41726,#41727,
#41728,#41729,#41730,#41731,#41732,#41733,#41734,#41735,#41736,#41737,#41738,
#41739,#41740,#41741,#41742,#41743,#41744,#41745,#41746,#41747,#41748,#41749,
#41750,#41751,#41752,#41753,#41754,#41755,#41756,#41757,#41758,#41759,#41760,
#41761,#41762,#41763,#41764,#41765,#41766,#41767,#41768,#41769,#41770,#41771,
#41772,#41773,#41774,#41775,#41776,#41777,#41778,#41779,#41780,#41781,#41782,
#41783,#41784,#41785,#41786,#41787,#41788,#41789,#41790,#41791,#41792,#41793,
#41794,#41795,#41796,#41797,#41798,#41799,#41800,#41801),.UNSPECIFIED.,
 .F.,.F.,(4,2,2,2,2,2,2,2,2,2,2,2,2,2,2,2,2,2,2,2,2,2,2,2,2,2,2,2,2,2,2,
2,2,2,2,2,2,2,2,2,2,2,2,2,2,2,2,2,2,2,2,2,2,2,2,2,2,2,2,2,2,2,2,2,2,2,2,
2,2,2,2,2,2,2,2,2,2,2,2,2,2,2,2,2,2,2,2,2,2,2,2,2,2,2,2,2,2,2,2,2,2,2,2,
2,2,2,2,2,2,2,2,2,2,2,2,2,2,2,2,2,2,2,2,2,2,2,2,2,2,2,2,2,2,2,2,2,2,2,2,
2,2,2,2,2,2,2,2,2,2,2,2,2,2,2,4),(-0.786310854402765,-0.777462697274128,
-0.774578872863381,-0.771825253196008,-0.768585597468488,-0.759993654801992,
-0.752727637017471,-0.7463579158524,-0.744896183621603,-0.743748465546371,
-0.742575316626439,-0.741396655378143,-0.739243693561859,-0.729650287374014,
-0.719309564515478,-0.713515223997535,-0.709308158995403,-0.705651448980889,
-0.701940572141836,-0.697184946732764,-0.689928898172377,-0.675431880047376,
-0.667047856015395,-0.661931638796638,-0.661855545681514,-0.661787040240191,
-0.66172535466873,-0.661669797262891,-0.661619745923069,-0.661574641880017,
-0.661533983714326,-0.661497321699181,-0.66146425256561,-0.661434414874798,
-0.661407484600269,-0.661383171233308,-0.66136121431376,-0.661341380105068,
-0.661323458728828,-0.661307261727949,-0.661292619899717,-0.661242260347798,
-0.661193672018736,-0.661146774937757,-0.661101492920444,-0.660256710115307,
-0.660237022592094,-0.660217738911895,-0.660198840980835,-0.660180311218699,
-0.660162132911044,-0.660144290023941,-0.660126766947141,-0.660109548839258,
-0.660092621243659,-0.660075970239275,-0.660059582355764,-0.660043444656213,
-0.660027544568104,-0.660011869881863,-0.659996408737286,-0.659981149545176,
-0.659966081292558,-0.659951193024744,-0.65993647410584,-0.659921913985125,
-0.658343782751553,-0.656773017784948,-0.654567106743606,-0.647058060570245,
-0.639120195852277,-0.63528599385772,-0.634149487673151,-0.633089154912727,
-0.632295462749806,-0.630410887711222,-0.622332241191278,-0.616425079464459,
-0.613304633882996,-0.613259122205537,-0.613116914942923,-0.612985080125594,
-0.6128625987091,-0.612748553021981,-0.612642116711313,-0.612542545427062,
-0.612449168349521,-0.612361380429204,-0.612278635424558,-0.612200439406071,
-0.612126344955206,-0.612055945993218,-0.611988872963505,-0.611924788505522,
-0.611863383584545,-0.611804373914465,-0.61174749668639,-0.611692507596376,
-0.611639177998426,-0.611587292280063,-0.611536645440485,-0.611487040473534,
-0.611438286141007,-0.611390194205315,-0.611342577007589,-0.611295244644771,
-0.609030554233093,-0.606771899712746,-0.602625644752582,-0.58350798549645,
-0.573412898727784,-0.568397100365427,-0.565069075724267,-0.564230906277338,
-0.5619812954031,-0.559213833044693,-0.554692116549716,-0.54296895675803,
-0.533313904284,-0.529881127000282,-0.528101707580342,-0.526672538331252,
-0.525674820049849,-0.524770311635361,-0.523580015442259,-0.521028765004709,
-0.509643894233779,-0.496661773228539,-0.490823463523767,-0.487536687466684,
-0.485315312582905,-0.483494100654152,-0.481615236879797,-0.479353551751606,
-0.475409067681439,-0.460110760829431,-0.448244360047109,-0.444342287175839,
-0.442375723309685,-0.441140763404031,-0.440041468532887,-0.439091864624069,
-0.437996200865361,-0.43614029059331,-0.427858512292576,-0.426819130476898,
-0.426163596147315,-0.415092050513689,-0.409588944069834,-0.405922479428505,
-0.402998655796344,-0.40005364938589,-0.397380628838706,-0.393164021180743,
-0.393155650627907),.UNSPECIFIED.) ;
#3337 = B_SPLINE_CURVE_WITH_KNOTS('',3,(#41803,#41804,#41805,#41806,#41807,
#41808,#41809,#41810,#41811,#41812,#41813,#41814,#41815,#41816,#41817,#41818,
#41819,#41820,#41821,#41822,#41823,#41824,#41825,#41826,#41827,#41828,#41829,
#41830,#41831,#41832,#41833,#41834,#41835,#41836,#41837,#41838,#41839,#41840,
#41841,#41842,#41843,#41844,#41845,#41846,#41847,#41848,#41849,#41850,#41851,
#41852,#41853,#41854,#41855,#41856,#41857,#41858,#41859,#41860,#41861,#41862,
#41863,#41864,#41865,#41866,#41867,#41868,#41869,#41870,#41871,#41872,#41873,
#41874,#41875,#41876,#41877,#41878,#41879,#41880,#41881,#41882,#41883,#41884,
#41885,#41886,#41887,#41888,#41889,#41890,#41891,#41892,#41893,#41894,#41895,
#41896,#41897,#41898,#41899,#41900,#41901,#41902,#41903,#41904,#41905,#41906,
#41907,#41908,#41909,#41910,#41911,#41912,#41913,#41914,#41915,#41916,#41917,
#41918,#41919,#41920,#41921,#41922,#41923,#41924,#41925,#41926,#41927,#41928,
#41929,#41930,#41931,#41932,#41933,#41934,#41935,#41936,#41937,#41938,#41939,
#41940,#41941,#41942,#41943,#41944,#41945,#41946,#41947,#41948,#41949,#41950,
#41951,#41952,#41953,#41954,#41955,#41956,#41957,#41958,#41959,#41960,#41961,
#41962,#41963,#41964,#41965,#41966,#41967,#41968,#41969,#41970,#41971,#41972,
#41973,#41974,#41975,#41976,#41977,#41978,#41979,#41980,#41981,#41982,#41983,
#41984,#41985,#41986,#41987,#41988,#41989,#41990,#41991,#41992,#41993,#41994,
#41995,#41996,#41997,#41998,#41999,#42000,#42001,#42002,#42003,#42004,#42005,
#42006,#42007,#42008,#42009,#42010,#42011,#42012,#42013,#42014,#42015,#42016,
#42017,#42018,#42019,#42020,#42021,#42022,#42023,#42024,#42025,#42026,#42027,
#42028,#42029,#42030,#42031,#42032,#42033,#42034,#42035,#42036,#42037,#42038,
#42039,#42040,#42041,#42042,#42043,#42044,#42045,#42046,#42047,#42048,#42049,
#42050,#42051,#42052,#42053,#42054,#42055,#42056,#42057,#42058,#42059,#42060,
#42061,#42062,#42063,#42064,#42065,#42066,#42067,#42068,#42069,#42070,#42071,
#42072,#42073,#42074,#42075,#42076,#42077,#42078,#42079,#42080,#42081,#42082,
#42083,#42084,#42085,#42086,#42087,#42088,#42089,#42090,#42091,#42092,#42093,
#42094,#42095,#42096,#42097,#42098,#42099,#42100,#42101,#42102,#42103,#42104,
#42105,#42106,#42107,#42108,#42109,#42110,#42111,#42112,#42113,#42114,#42115,
#42116,#42117,#42118,#42119,#42120,#42121,#42122,#42123,#42124,#42125,#42126,
#42127,#42128,#42129,#42130,#42131,#42132,#42133,#42134,#42135,#42136,#42137,
#42138,#42139,#42140,#42141,#42142,#42143,#42144,#42145,#42146,#42147,#42148,
#42149,#42150,#42151,#42152,#42153,#42154,#42155,#42156,#42157,#42158,#42159,
#42160,#42161,#42162,#42163,#42164,#42165,#42166,#42167,#42168,#42169,#42170,
#42171,#42172,#42173,#42174,#42175,#42176,#42177,#42178,#42179,#42180,#42181,
#42182,#42183,#42184,#42185,#42186,#42187,#42188,#42189,#42190,#42191,#42192,
#42193,#42194,#42195,#42196,#42197,#42198,#42199,#42200,#42201,#42202,#42203,
#42204,#42205,#42206,#42207,#42208,#42209,#42210,#42211,#42212,#42213,#42214,
#42215,#42216,#42217,#42218,#42219,#42220,#42221,#42222,#42223,#42224,#42225,
#42226,#42227,#42228,#42229,#42230,#42231,#42232,#42233,#42234,#42235,#42236,
#42237,#42238,#42239,#42240,#42241,#42242,#42243,#42244,#42245,#42246,#42247,
#42248,#42249,#42250,#42251,#42252,#42253,#42254,#42255,#42256,#42257,#42258,
#42259,#42260,#42261,#42262,#42263,#42264,#42265,#42266,#42267,#42268,#42269,
#42270,#42271,#42272,#42273,#42274,#42275,#42276,#42277,#42278,#42279,#42280,
#42281,#42282,#42283,#42284,#42285,#42286,#42287,#42288,#42289,#42290,#42291,
#42292,#42293,#42294,#42295,#42296,#42297,#42298,#42299,#42300,#42301,#42302,
#42303,#42304,#42305,#42306,#42307,#42308,#42309,#42310,#42311,#42312,#42313,
#42314,#42315,#42316,#42317,#42318,#42319,#42320,#42321,#42322,#42323,#42324,
#42325,#42326,#42327,#42328,#42329,#42330,#42331,#42332,#42333,#42334,#42335,
#42336,#42337,#42338,#42339,#42340,#42341,#42342,#42343,#42344,#42345,#42346,
#42347,#42348,#42349,#42350,#42351,#42352,#42353,#42354,#42355,#42356,#42357,
#42358,#42359,#42360,#42361,#42362,#42363,#42364,#42365,#42366,#42367,#42368,
#42369,#42370,#42371,#42372,#42373,#42374,#42375,#42376,#42377,#42378,#42379,
#42380,#42381,#42382,#42383,#42384,#42385,#42386,#42387,#42388,#42389,#42390,
#42391,#42392,#42393,#42394,#42395,#42396,#42397,#42398,#42399,#42400,#42401,
#42402,#42403,#42404,#42405,#42406,#42407,#42408,#42409,#42410,#42411,#42412,
#42413,#42414,#42415,#42416,#42417,#42418,#42419,#42420,#42421,#42422,#42423,
#42424,#42425,#42426,#42427,#42428,#42429,#42430,#42431,#42432,#42433,#42434,
#42435,#42436,#42437,#42438,#42439,#42440,#42441,#42442,#42443,#42444,#42445,
#42446,#42447,#42448,#42449,#42450,#42451,#42452,#42453,#42454,#42455,#42456),
 .UNSPECIFIED.,.F.,.F.,(4,2,2,2,2,2,2,2,2,2,2,2,2,2,2,2,2,2,2,2,2,2,2,2,
2,2,2,2,2,2,2,2,2,2,2,2,2,2,2,2,2,2,2,2,2,2,2,2,2,2,2,2,2,2,2,2,2,2,2,2,
2,2,2,2,2,2,2,2,2,2,2,2,2,2,2,2,2,2,2,2,2,2,2,2,2,2,2,2,2,2,2,2,2,2,2,2,
2,2,2,2,2,2,2,2,2,2,2,2,2,2,2,2,2,2,2,2,2,2,2,2,2,2,2,2,2,2,2,2,2,2,2,2,
2,2,2,2,2,2,2,2,2,2,2,2,2,2,2,2,2,2,2,2,2,2,2,2,2,2,2,2,2,2,2,2,2,2,2,2,
2,2,2,2,2,2,2,2,2,2,2,2,2,2,2,2,2,2,2,2,2,2,2,2,2,2,2,2,2,2,2,2,2,2,2,2,
2,2,2,2,2,2,2,2,2,2,2,2,2,2,2,2,2,2,2,2,2,2,2,2,2,2,2,2,2,2,2,2,2,2,2,2,
2,2,2,2,2,2,2,2,2,2,2,2,2,2,2,2,2,2,2,2,2,2,2,2,2,2,2,2,2,2,2,2,2,2,2,2,
2,2,2,2,2,2,2,2,2,2,2,2,2,2,2,2,2,2,2,2,2,2,2,2,2,2,2,2,2,2,2,2,2,2,2,2,
2,2,2,2,2,2,2,2,2,2,2,2,2,2,4),(-0.393065589708965,-0.388966566095848,-0.383448746522827,
-0.376179753135169,-0.374191610189867,-0.374158237312468,-0.374135335710637,
-0.374114778741838,-0.374096326457447,-0.37407976325486,-0.374064895468,
-0.374052707000776,-0.374040843322002,-0.374029295564849,-0.374018055142535,
-0.37400711363893,-0.373996462896227,-0.373986094955537,-0.373976002159433,
-0.373966176968725,-0.373956612117498,-0.373947300479584,-0.373938235136589,
-0.373929409439409,-0.373920816821315,-0.373912450941929,-0.373904305666952,
-0.373896374972697,-0.373888653100104,-0.373881134329663,-0.373873813111811,
-0.373866684166782,-0.373860607584359,-0.373854573307737,-0.373848580835059,
-0.373842629926712,-0.373836720268857,-0.373830851509131,-0.373825023272392,
-0.373819235235161,-0.373813487086501,-0.373807778489716,-0.373802109135364,
-0.373796478691675,-0.373790886896402,-0.373785333367384,-0.373779817875267,
-0.373774340096372,-0.373768899680037,-0.373763496322769,-0.37375812978838,
-0.373752799775776,-0.373747505962267,-0.373742248096514,-0.373737025860778,
-0.373731838925717,-0.373726687062818,-0.373721569958284,-0.373716487431612,
-0.373711439097369,-0.373706424692151,-0.37370144397626,-0.373696496687196,
-0.373691582474535,-0.37368670118131,-0.373681852575176,-0.373677036273045,
-0.37367225212438,-0.373667499855715,-0.37366277918764,-0.373658089812767,
-0.373653431609658,-0.37364880421959,-0.373644207441387,-0.37363964110511,
-0.373635104865037,-0.373630598506484,-0.373626121825299,-0.373621674617905,
-0.373617256638368,-0.373612867642864,-0.373608507324453,-0.373604175512244,
-0.373599872088644,-0.373595596695155,-0.373591349100151,-0.373587129240475,
-0.373582936840201,-0.373578771687893,-0.373574633522961,-0.373570522099672,
-0.373566437263598,-0.373562378858738,-0.373558346621176,-0.37355434033864,
-0.373550359894408,-0.373546404978224,-0.373542475498692,-0.373538571202167,
-0.373534691880213,-0.373530837433716,-0.373527007687636,-0.373523202332135,
-0.373519421188301,-0.373515664008997,-0.371762372943665,-0.367585412427757,
-0.358613561453349,-0.352598337538184,-0.349970187718555,-0.349783763189994,
-0.349399873062088,-0.348443704439419,-0.348420198822344,-0.348398319008721,
-0.348377956190562,-0.346350426019905,-0.342846265948606,-0.33837561685244,
-0.323747138385486,-0.314628245737323,-0.303306470593153,-0.29761714021614,
-0.29751154058311,-0.297420043127292,-0.297340718720898,-0.297271910531709,
-0.297212194441151,-0.297160345241728,-0.297115307808145,-0.297005477530411,
-0.296899735717524,-0.296797879150421,-0.296699715967274,-0.296605065040454,
-0.296513755385228,-0.296425625561051,-0.296340523124463,-0.296258304111954,
-0.296178832569933,-0.296101980046967,-0.291688624157727,-0.287195888750989,
-0.280948704889126,-0.270198282438431,-0.267725595730619,-0.266255559945261,
-0.265102789113086,-0.263494144148679,-0.261728698969323,-0.258807088843284,
-0.25228863854667,-0.243580587869969,-0.240698578544022,-0.239321581938187,
-0.23823237340428,-0.237044660585399,-0.237040800982266,-0.237036934285919,
-0.23703306143964,-0.237029181853243,-0.237025295974021,-0.237021403755482,
-0.237017504634154,-0.237013599004515,-0.237009686534246,-0.237005767298947,
-0.237001841459152,-0.236997908635496,-0.236993968801003,-0.236990021739105,
-0.236986067654262,-0.236982106044023,-0.236978137342861,-0.236974161392018,
-0.23697017760217,-0.236966186281581,-0.23696218752544,-0.236958181222895,
-0.236954166974552,-0.23695014457853,-0.236946114306944,-0.236942076447991,
-0.236938030398093,-0.236933975907316,-0.236929912896609,-0.236925841365424,
-0.236921761508152,-0.236917673035839,-0.236913575943062,-0.236909470398506,
-0.236905355729577,-0.236901231847539,-0.236897099020933,-0.236892957094873,
-0.236888806195107,-0.236884645778026,-0.236880475992086,-0.236876296995416,
-0.236872107931012,-0.236867909171639,-0.236863701105506,-0.236859483371062,
-0.236855255499268,-0.236851017540101,-0.236846769356363,-0.236842511046265,
-0.236838242439205,-0.236833963293048,-0.23682967368968,-0.236825373304639,
-0.236821062388024,-0.236816740610951,-0.236812407982378,-0.236808064449367,
-0.236803709763215,-0.236799343749095,-0.236794966459936,-0.236790577909174,
-0.236786177609795,-0.236781765590968,-0.23677734198399,-0.236772906440799,
-0.236768459118643,-0.236763999450378,-0.236759527756641,-0.236755043949369,
-0.236750547798447,-0.236746039176336,-0.236741517915517,-0.23673698380523,
-0.23673243739724,-0.236727877973662,-0.236723305538348,-0.236718719816909,
-0.236714120437942,-0.236709507749938,-0.236704881494466,-0.23670024166752,
-0.236695588310455,-0.236690921045407,-0.236686240032755,-0.236681544736176,
-0.236676835247036,-0.235042424229185,-0.232085425740897,-0.221287541399645,
-0.219367323172205,-0.217301279783494,-0.210208222778234,-0.205932429359203,
-0.203111120439414,-0.199409758631995,-0.195007879852957,-0.189557019084433,
-0.187373499785273,-0.186489280858067,-0.186279454516391,-0.184275899608854,
-0.181927580489253,-0.177430693699789,-0.169025708425269,-0.162822605197181,
-0.159080604885825,-0.158224549345706,-0.158068265860158,-0.157746773017292,
-0.157485494790619,-0.157270578554057,-0.157091971577553,-0.156942232166822,
-0.156815749634271,-0.151620017481765,-0.146505313209591,-0.13770255809697,
-0.13360939923471,-0.129750206181053,-0.120875262469577,-0.114559186246218,
-0.113039759143288,-0.111359459678535,-0.111298677526727,-0.111244279657613,
-0.111195464270134,-0.111151549741104,-0.111111953849125,-0.111076177036546,
-0.111043788777336,-0.111014416324963,-0.110987735641776,-0.110963464046509,
-0.110941353812947,-0.110921187251175,-0.109180491091203,-0.107596966103121,
-0.102160409383009,-0.0942720035046282,-0.0912491998483847,-0.088868421435765,
-0.0853546399509588,-0.0811656674535144,-0.0703065043256505,-0.0680660783932548,
-0.0667589626736305,-0.0651824959318863,-0.062996302784368,-0.0575869508532417,
-0.0535188263621436,-0.051050432989073,-0.0487233765368177,-0.0471473950526166,
-0.0441655697277461,-0.0359017938579531,-0.0339314541286829,-0.0324758421304942,
-0.0308070834985168,-0.0290307014167538,-0.0262848070699855,-0.0228410082915044,
-0.0151658803392792,-0.0136856958442221,-0.0128656229705687,-0.0120507563698123,
-0.0112427406305335,-0.0102043876099121,-0.00839362727804128,-1.00000003522283E-6),
 .UNSPECIFIED.) ;
#3338 = B_SPLINE_CURVE_WITH_KNOTS('',3,(#42457,#42458,#42459,#42460,#42461,
#42462,#42463,#42464,#42465,#42466,#42467,#42468,#42469,#42470,#42471,#42472,
#42473,#42474,#42475,#42476,#42477,#42478,#42479,#42480,#42481,#42482,#42483,
#42484,#42485,#42486,#42487,#42488,#42489,#42490,#42491,#42492,#42493,#42494,
#42495,#42496,#42497,#42498,#42499,#42500,#42501,#42502,#42503,#42504,#42505,
#42506,#42507,#42508,#42509,#42510,#42511,#42512,#42513,#42514,#42515,#42516,
#42517,#42518,#42519,#42520),.UNSPECIFIED.,.F.,.F.,(4,3,3,3,3,3,3,3,3,3,
3,3,3,3,3,3,3,3,3,3,3,4),(0.,0.194611379569939,0.413105731031986,0.631646549932974,
0.984685058974708,1.0681572847997,1.2854939556078,1.50413078441806,1.72074571686338,
1.93938203882708,1.96857224711482,2.15652830010514,2.37516406745792,2.59283702522495,
2.80932989456835,2.95242475684296,3.0277774580989,3.24484714263336,3.46348192766738,
3.68172528565085,3.89858695415034,3.93630690328113),.UNSPECIFIED.) ;
#3339 = B_SPLINE_CURVE_WITH_KNOTS('',3,(#42524,#42525,#42526,#42527,#42528,
#42529,#42530,#42531,#42532,#42533,#42534,#42535,#42536),.UNSPECIFIED.,
 .F.,.F.,(4,3,2,2,2,4),(-0.00235052512319675,0.,0.0113491260853101,0.0226982521706202,
0.034046050040237,0.0453938479098539),.UNSPECIFIED.) ;
#3340 = B_SPLINE_CURVE_WITH_KNOTS('',3,(#42538,#42539,#42540,#42541,#42542,
#42543,#42544,#42545,#42546,#42547,#42548,#42549,#42550,#42551,#42552,#42553,
#42554,#42555,#42556,#42557,#42558,#42559,#42560,#42561,#42562,#42563,#42564,
#42565,#42566,#42567,#42568,#42569,#42570,#42571,#42572,#42573,#42574,#42575,
#42576,#42577,#42578,#42579,#42580,#42581,#42582,#42583,#42584,#42585,#42586,
#42587,#42588,#42589,#42590,#42591,#42592,#42593,#42594,#42595,#42596,#42597,
#42598,#42599,#42600,#42601,#42602,#42603,#42604,#42605,#42606,#42607,#42608,
#42609,#42610,#42611,#42612,#42613,#42614,#42615,#42616,#42617,#42618,#42619,
#42620,#42621,#42622,#42623,#42624,#42625,#42626,#42627,#42628,#42629,#42630,
#42631,#42632,#42633,#42634,#42635,#42636,#42637,#42638,#42639,#42640,#42641,
#42642,#42643,#42644,#42645,#42646,#42647,#42648,#42649,#42650,#42651,#42652,
#42653,#42654,#42655,#42656,#42657,#42658,#42659,#42660,#42661,#42662,#42663,
#42664,#42665,#42666,#42667,#42668,#42669,#42670,#42671,#42672,#42673,#42674,
#42675,#42676,#42677,#42678,#42679,#42680,#42681,#42682,#42683,#42684,#42685,
#42686,#42687,#42688,#42689,#42690,#42691,#42692,#42693,#42694,#42695,#42696,
#42697,#42698,#42699,#42700,#42701,#42702,#42703,#42704,#42705,#42706,#42707,
#42708,#42709,#42710,#42711,#42712,#42713,#42714,#42715,#42716,#42717,#42718,
#42719,#42720,#42721,#42722,#42723,#42724,#42725,#42726,#42727,#42728,#42729,
#42730,#42731,#42732,#42733,#42734,#42735,#42736,#42737,#42738,#42739,#42740,
#42741,#42742,#42743,#42744,#42745,#42746,#42747,#42748,#42749,#42750,#42751,
#42752,#42753,#42754,#42755,#42756,#42757,#42758,#42759,#42760,#42761,#42762,
#42763,#42764,#42765,#42766,#42767,#42768,#42769,#42770,#42771,#42772,#42773,
#42774,#42775,#42776,#42777,#42778,#42779,#42780,#42781,#42782,#42783,#42784,
#42785,#42786,#42787,#42788,#42789,#42790,#42791,#42792,#42793,#42794,#42795,
#42796,#42797,#42798,#42799,#42800,#42801,#42802,#42803,#42804,#42805,#42806,
#42807,#42808,#42809,#42810,#42811,#42812,#42813,#42814,#42815,#42816,#42817,
#42818,#42819,#42820,#42821,#42822,#42823,#42824,#42825,#42826,#42827,#42828,
#42829,#42830,#42831,#42832,#42833,#42834,#42835,#42836,#42837,#42838,#42839,
#42840,#42841,#42842,#42843,#42844,#42845,#42846,#42847,#42848,#42849,#42850,
#42851,#42852,#42853,#42854,#42855,#42856,#42857,#42858,#42859,#42860,#42861,
#42862,#42863,#42864,#42865,#42866,#42867,#42868,#42869,#42870,#42871,#42872,
#42873,#42874,#42875,#42876,#42877,#42878,#42879,#42880,#42881,#42882,#42883,
#42884,#42885,#42886,#42887,#42888,#42889,#42890,#42891,#42892,#42893,#42894,
#42895,#42896,#42897,#42898,#42899,#42900,#42901,#42902,#42903,#42904,#42905,
#42906,#42907,#42908,#42909,#42910,#42911,#42912,#42913,#42914,#42915,#42916,
#42917,#42918,#42919,#42920,#42921,#42922,#42923,#42924,#42925,#42926,#42927,
#42928,#42929,#42930,#42931),.UNSPECIFIED.,.F.,.F.,(4,2,2,2,2,2,2,2,2,2,
2,2,2,2,2,2,2,2,2,2,2,2,2,2,2,2,2,2,2,2,2,2,2,2,2,2,2,2,2,2,2,2,2,2,2,2,
2,2,2,2,2,2,2,2,2,2,2,2,2,2,2,2,2,2,2,2,2,2,2,2,2,2,2,2,2,2,2,2,2,2,2,2,
2,2,2,2,2,2,2,2,2,2,2,2,2,2,2,2,2,2,2,2,2,2,2,2,2,2,2,2,2,2,2,2,2,2,2,2,
2,2,2,2,2,2,2,2,2,2,2,2,2,2,2,2,2,2,2,2,2,2,2,2,2,2,2,2,2,2,2,2,2,2,2,2,
2,2,2,2,2,2,2,2,2,2,2,2,2,2,2,2,2,2,2,2,2,2,2,2,2,2,2,2,2,2,2,2,2,2,2,2,
2,2,2,2,2,2,4),(-0.338631569254744,-0.336734654040014,-0.334665307627351,
-0.325963066244536,-0.324026710452822,-0.322380662939139,-0.320388042855082,
-0.314253169168998,-0.311839994745291,-0.310214874905825,-0.308693228330123,
-0.307237952438348,-0.305185045258803,-0.298034605265837,-0.293405752588105,
-0.290428016768423,-0.289077367253203,-0.28796560372676,-0.286852955957451,
-0.284806427012391,-0.274926628259733,-0.271422900114645,-0.269729797054094,
-0.268657672992355,-0.267816313919124,-0.266952036340973,-0.266079447166832,
-0.264447264494238,-0.257570040233546,-0.252592203538653,-0.250216384988825,
-0.248700949561993,-0.248632464842557,-0.248568481034681,-0.248508631189948,
-0.248452576601431,-0.24840000531737,-0.248350630439625,-0.248304188574536,
-0.248260438055414,-0.248219157208751,-0.248180142845309,-0.248143208779721,
-0.248108184287919,-0.248074912796556,-0.24804325071982,-0.248013066120397,
-0.247984237858192,-0.247956654237224,-0.247930212389863,-0.247904817474043,
-0.247880381581244,-0.24785682312758,-0.247834066309284,-0.24781204061228,
-0.247790679923397,-0.247769922152786,-0.247749708861411,-0.247729984556913,
-0.246507560424402,-0.24509133284851,-0.242593824359581,-0.235999289760559,
-0.232926352893635,-0.230688043389769,-0.228517290840238,-0.227039427442087,
-0.219388666888622,-0.217665456719758,-0.217019247371198,-0.216676122635613,
-0.216319358125661,-0.21470742327233,-0.213094110076598,-0.206648321242796,
-0.203826866646343,-0.202141702601408,-0.200788110338928,-0.199645563913887,
-0.197964777160737,-0.194655651619069,-0.186005871621098,-0.183252900996211,
-0.18169874370884,-0.180697396005963,-0.1806889464537,-0.180680594203109,
-0.180672336985844,-0.180664172571408,-0.180656098583319,-0.180648112706023,
-0.180640212914428,-0.180632396970588,-0.180624663069236,-0.180617008915489,
-0.180609432678236,-0.180601932391217,-0.180594505992267,-0.180587151886344,
-0.180579867992514,-0.180572652375439,-0.180565503195765,-0.180558418705696,
-0.180551397343621,-0.180544437198527,-0.180537536934857,-0.1805306943673,
-0.180523907902386,-0.18051717611988,-0.180510497480495,-0.180503870227966,
-0.180497293018481,-0.180490764023599,-0.180484281594919,-0.180477844687277,
-0.180471451615318,-0.180465100943189,-0.180458791043372,-0.180452520351895,
-0.180446287768797,-0.180440091869983,-0.180433931188036,-0.180427804187668,
-0.180421709398241,-0.180415645806202,-0.180409611787812,-0.180403605757985,
-0.180397626779217,-0.180391673454889,-0.180385744113069,-0.180379837431095,
-0.18037395189779,-0.180368086410412,-0.180362239526999,-0.180356409940254,
-0.179302518753018,-0.178256366520431,-0.176428224520422,-0.169274085184775,
-0.160721521229079,-0.15926326782659,-0.158400178395906,-0.157693395568019,
-0.156881584995432,-0.15590972122208,-0.154367141469796,-0.151240750842007,
-0.146109134458849,-0.139316786451658,-0.137868408683809,-0.137073205141669,
-0.136282115590371,-0.135380397820905,-0.133553731398204,-0.131159020760954,
-0.124761979671465,-0.123705062809495,-0.12237947135262,-0.117498075480047,
-0.116125649359041,-0.115350727199907,-0.11460597602389,-0.113633192853416,
-0.112559082792293,-0.110778577105945,-0.106872228035098,-0.0943360832791758,
-0.0919864445405689,-0.0905627277180745,-0.0893105960214068,-0.0878491374722877,
-0.0847657690986667,-0.0804642266826064,-0.0673398015862877,-0.0635702031269495,
-0.0616708223826233,-0.0604348086240259,-0.0593643263936798,-0.0570968745149313,
-0.0544573924190736,-0.0493100487068456,-0.0414061098843744,-0.0409465848615722,
-0.0358095315760844,-0.0335776201567591,-0.0318756311788981,-0.0302486677193898,
-0.0283707910132205,-0.0227320356787229,-0.014755322969727,-0.00882146644314774,
-0.00702341351978558,-0.00596810267110615,-0.00504964345917795,-0.00413109953237996,
-0.00245627375521964,-1.35388579686318E-6),.UNSPECIFIED.) ;
#3341 = B_SPLINE_CURVE_WITH_KNOTS('',3,(#42933,#42934,#42935,#42936),
 .UNSPECIFIED.,.F.,.F.,(4,4),(0.597204295884584,0.669364392781264),
 .UNSPECIFIED.) ;
#3342 = B_SPLINE_CURVE_WITH_KNOTS('',3,(#42938,#42939,#42940,#42941,#42942,
#42943,#42944,#42945,#42946,#42947,#42948,#42949,#42950,#42951,#42952,#42953,
#42954,#42955,#42956,#42957,#42958,#42959,#42960,#42961,#42962,#42963,#42964,
#42965,#42966,#42967,#42968,#42969,#42970,#42971,#42972,#42973,#42974,#42975,
#42976,#42977,#42978,#42979,#42980,#42981,#42982,#42983,#42984,#42985,#42986,
#42987,#42988,#42989,#42990,#42991,#42992,#42993,#42994,#42995,#42996,#42997,
#42998,#42999,#43000,#43001,#43002,#43003,#43004,#43005,#43006,#43007,#43008,
#43009,#43010,#43011,#43012,#43013,#43014,#43015,#43016,#43017,#43018,#43019,
#43020,#43021,#43022,#43023,#43024,#43025,#43026,#43027,#43028,#43029,#43030,
#43031,#43032,#43033,#43034,#43035,#43036,#43037,#43038,#43039,#43040,#43041,
#43042,#43043,#43044,#43045,#43046,#43047,#43048,#43049,#43050,#43051,#43052,
#43053,#43054,#43055,#43056,#43057,#43058,#43059,#43060,#43061,#43062,#43063,
#43064,#43065,#43066,#43067,#43068,#43069,#43070,#43071,#43072,#43073,#43074,
#43075,#43076,#43077,#43078,#43079,#43080,#43081,#43082,#43083,#43084,#43085,
#43086,#43087,#43088,#43089,#43090,#43091,#43092,#43093,#43094,#43095,#43096,
#43097,#43098,#43099,#43100,#43101,#43102,#43103,#43104,#43105,#43106,#43107,
#43108,#43109,#43110,#43111,#43112,#43113,#43114,#43115,#43116,#43117,#43118,
#43119,#43120,#43121,#43122,#43123,#43124,#43125,#43126,#43127,#43128,#43129,
#43130,#43131,#43132,#43133,#43134,#43135,#43136,#43137,#43138,#43139,#43140,
#43141,#43142,#43143,#43144,#43145,#43146,#43147,#43148,#43149,#43150,#43151,
#43152,#43153,#43154,#43155,#43156,#43157,#43158,#43159,#43160,#43161,#43162,
#43163,#43164,#43165,#43166,#43167,#43168,#43169,#43170,#43171,#43172,#43173,
#43174,#43175,#43176,#43177,#43178,#43179,#43180,#43181,#43182,#43183,#43184,
#43185,#43186,#43187,#43188,#43189,#43190,#43191,#43192,#43193,#43194,#43195,
#43196,#43197,#43198,#43199,#43200,#43201,#43202,#43203,#43204,#43205,#43206,
#43207,#43208,#43209,#43210,#43211,#43212,#43213,#43214,#43215),
 .UNSPECIFIED.,.F.,.F.,(4,2,2,2,2,2,2,2,2,2,2,2,2,2,2,2,2,2,2,2,2,2,2,2,
2,2,2,2,2,2,2,2,2,2,2,2,2,2,2,2,2,2,2,2,2,2,2,2,2,2,2,2,2,2,2,2,2,2,2,2,
2,2,2,2,2,2,2,2,2,2,2,2,2,2,2,2,2,2,2,2,2,2,2,2,2,2,2,2,2,2,2,2,2,2,2,2,
2,2,2,2,2,2,2,2,2,2,2,2,2,2,2,2,2,2,2,2,2,2,2,2,2,2,2,2,2,2,2,2,2,2,2,2,
2,2,2,2,2,2,4),(-0.255648930279346,-0.252997541914023,-0.250129508816139,
-0.244210307020476,-0.235916895314324,-0.234170956693684,-0.232581734776005,
-0.231043334138474,-0.228960848074572,-0.223018060278477,-0.217304903048903,
-0.215115149238904,-0.214045289292404,-0.213762778966205,-0.213544837882605,
-0.21267034927113,-0.211779906286584,-0.210886419354201,-0.209240569491487,
-0.200245314661032,-0.195659752547622,-0.193628747053223,-0.19199875282225,
-0.191155799364946,-0.190355763478676,-0.189321341453539,-0.187490259426295,
-0.178111063619884,-0.173947777970992,-0.172066662684669,-0.170719960522959,
-0.169907202828386,-0.169080407616088,-0.168125956034019,-0.166503868399372,
-0.159143686189377,-0.153892298833385,-0.151463180561509,-0.149957923478239,
-0.149923891593186,-0.149852516398666,-0.149787000180214,-0.149726927856389,
-0.149671902957905,-0.149621548601185,-0.149575508042802,-0.149533444910382,
-0.149495043241783,-0.149460007279618,-0.149428060969789,-0.149398947448583,
-0.149372428287741,-0.149348282727429,-0.149326306823944,-0.148216684864361,
-0.147036713161444,-0.145438572312611,-0.141547364205493,-0.133915278003247,
-0.131027999202793,-0.129244445564844,-0.127826135572844,-0.126440315731165,
-0.126372665632238,-0.126313570081502,-0.126260877382886,-0.126213119574936,
-0.12616924808184,-0.126128485907223,-0.126090239723491,-0.126054044534104,
-0.126019527514997,-0.125986383549398,-0.125954358172745,-0.12592323535276,
-0.125892828263452,-0.125862972666397,-0.125833521763597,-0.125804342006902,
-0.125775309964684,-0.125746309595708,-0.125717230067369,-0.125687963743893,
-0.125658404683168,-0.125628446977801,-0.125597983344769,-0.125566903782413,
-0.125535094159789,-0.12550243490758,-0.125468799508362,-0.125434053165129,
-0.125398051016836,-0.125360636381765,-0.125321638936169,-0.125280872491618,
-0.125238132559374,-0.125193193743492,-0.125145806626417,-0.125095694373013,
-0.12504254882899,-0.12498602602317,-0.123134106545598,-0.119878592254869,
-0.114023992805888,-0.111969741016468,-0.10916358533671,-0.10505083642492,
-0.100009585314172,-0.0968084810169616,-0.0931769772020695,-0.0889343467329334,
-0.0835736290368014,-0.0811284571804246,-0.0788395281498874,-0.076396123281033,
-0.0724625170395792,-0.0649643833672325,-0.0625961828505878,-0.060884501010045,
-0.058400734905096,-0.0550093093267712,-0.0499279043162481,-0.0484720480245992,
-0.0466014067838737,-0.0438229874809215,-0.0372914318420222,-0.03484561812626,
-0.032259227308613,-0.0307659861063578,-0.0287650324744632,-0.0222547659180821,
-0.0186956352932961,-0.0168281722189283,-0.0152082970564504,-0.0135169884610331,
-0.0111371344141474,-0.0062262270346876,-0.00219948967990509,-1.00011834170696E-6),
 .UNSPECIFIED.) ;
#3343 = B_SPLINE_CURVE_WITH_KNOTS('',3,(#43219,#43220,#43221,#43222,#43223,
#43224,#43225,#43226,#43227,#43228),.UNSPECIFIED.,.F.,.F.,(4,2,2,2,4),(-0.0453938479098542,
-0.034046050040237,-0.0226982521706198,-0.0113491260853099,0.),
 .UNSPECIFIED.) ;
#3344 = B_SPLINE_CURVE_WITH_KNOTS('',3,(#43230,#43231,#43232,#43233,#43234,
#43235,#43236,#43237,#43238,#43239),.UNSPECIFIED.,.F.,.F.,(4,2,2,2,4),(-0.0907876281662502,
-0.07943850588408,-0.0680893836019098,-0.056741615755882,-0.0453938479098542),
 .UNSPECIFIED.) ;
#3345 = B_SPLINE_CURVE_WITH_KNOTS('',3,(#43242,#43243,#43244,#43245,#43246,
#43247,#43248,#43249,#43250,#43251),.UNSPECIFIED.,.F.,.F.,(4,2,2,2,4),(0.0453964590725441,
0.0567416157558807,0.0680893836019074,0.0794385058840781,0.0907876281662487),
 .UNSPECIFIED.) ;
#3346 = B_SPLINE_CURVE_WITH_KNOTS('',3,(#50224,#50225,#50226,#50227,#50228,
#50229,#50230,#50231,#50232,#50233,#50234,#50235,#50236),.UNSPECIFIED.,
 .F.,.F.,(4,3,3,3,4),(0.00255363805101728,0.0798635693162218,0.156366831960307,
0.227369307234732,0.232870094604391),.UNSPECIFIED.) ;
#3347 = B_SPLINE_CURVE_WITH_KNOTS('',3,(#50237,#50238,#50239,#50240,#50241,
#50242,#50243,#50244,#50245,#50246,#50247,#50248,#50249,#50250,#50251,#50252,
#50253,#50254,#50255,#50256,#50257,#50258,#50259,#50260,#50261,#50262,#50263,
#50264,#50265,#50266,#50267,#50268,#50269,#50270,#50271,#50272,#50273,#50274,
#50275,#50276,#50277,#50278,#50279,#50280,#50281,#50282,#50283,#50284,#50285,
#50286,#50287,#50288,#50289,#50290,#50291,#50292,#50293,#50294,#50295,#50296,
#50297,#50298,#50299,#50300,#50301,#50302,#50303),.UNSPECIFIED.,.F.,.F.,
(4,3,3,3,3,3,3,3,3,3,3,3,3,3,3,3,3,3,3,3,3,3,4),(0.827865437902793,0.969498981235656,
1.21799526332659,1.38410988280274,1.4652627416507,1.66145199561158,1.70762284974659,
1.8714343337634,1.94910512274864,2.16981834865978,2.18634162166884,2.3630091739159,
2.42204226640599,2.61858958173905,2.65392302673644,2.88181141853766,3.05474660487823,
3.10884255152698,3.28206710848474,3.33241715880223,3.53151885752025,3.55138058859422,
3.61157274718876),.UNSPECIFIED.) ;
#3348 = B_SPLINE_CURVE_WITH_KNOTS('',3,(#57276,#57277,#57278,#57279,#57280,
#57281,#57282,#57283,#57284,#57285,#57286,#57287,#57288,#57289,#57290,#57291,
#57292,#57293,#57294,#57295,#57296,#57297,#57298,#57299,#57300,#57301,#57302,
#57303,#57304,#57305,#57306,#57307,#57308,#57309,#57310,#57311,#57312,#57313,
#57314,#57315,#57316,#57317,#57318,#57319),.UNSPECIFIED.,.F.,.F.,(4,2,2,
2,2,2,2,2,2,2,2,2,2,2,2,2,2,2,2,2,2,4),(0.,0.00971873963594822,0.0203964852574078,
0.0279299520213564,0.0332159680142414,0.0367507190487289,0.0382591314234756,
0.0385205125291013,0.0385320951859343,0.0385380775151796,0.0385445454156034,
0.0385477019368606,0.0385501373609749,0.0385527760503969,0.0385569787262409,
0.0385703376675416,0.0391296696114738,0.0414060512274473,0.0455043325938727,
0.051255059605876,0.0595245127263013,0.0750115373312587),.UNSPECIFIED.) ;
#3349 = B_SPLINE_CURVE_WITH_KNOTS('',3,(#57321,#57322,#57323,#57324,#57325,
#57326,#57327,#57328,#57329,#57330,#57331,#57332,#57333,#57334,#57335,#57336,
#57337,#57338,#57339),.UNSPECIFIED.,.F.,.F.,(4,1,1,1,1,1,1,1,1,1,1,1,1,
1,1,1,4),(87.336489761411,87.4317045853384,87.8665778926469,88.3014512000977,
88.7363245076919,89.1711978154302,89.6060711233134,90.0409444313423,90.4758177395175,
90.9106910478396,91.345564356309,91.7804376649263,92.2153109736917,92.6501842826055,
93.085057591668,93.5199309008791,93.8817096841969),.UNSPECIFIED.) ;
#3350 = B_SPLINE_CURVE_WITH_KNOTS('',3,(#57341,#57342,#57343,#57344,#57345,
#57346),.UNSPECIFIED.,.F.,.F.,(4,2,4),(-0.022111302478061,-0.0110566426887937,
-1.0000840920775E-6),.UNSPECIFIED.) ;
#3351 = B_SPLINE_CURVE_WITH_KNOTS('',3,(#57347,#57348,#57349,#57350,#57351,
#57352),.UNSPECIFIED.,.F.,.F.,(4,2,4),(9.99929897944746E-7,0.014189921283727,
0.0275689001028884),.UNSPECIFIED.) ;
#3352 = B_SPLINE_CURVE_WITH_KNOTS('',3,(#57353,#57354,#57355,#57356,#57357,
#57358,#57359,#57360,#57361,#57362,#57363,#57364,#57365,#57366,#57367,#57368,
#57369,#57370,#57371,#57372,#57373,#57374,#57375,#57376,#57377,#57378,#57379,
#57380,#57381,#57382,#57383,#57384,#57385,#57386,#57387,#57388,#57389,#57390,
#57391,#57392,#57393,#57394,#57395,#57396,#57397,#57398,#57399,#57400,#57401,
#57402,#57403,#57404,#57405,#57406,#57407,#57408,#57409,#57410,#57411,#57412,
#57413,#57414,#57415,#57416,#57417,#57418,#57419,#57420,#57421,#57422,#57423,
#57424,#57425,#57426,#57427,#57428,#57429,#57430,#57431,#57432,#57433,#57434,
#57435,#57436,#57437,#57438,#57439,#57440,#57441,#57442,#57443,#57444,#57445,
#57446,#57447,#57448,#57449,#57450,#57451,#57452,#57453,#57454,#57455,#57456,
#57457,#57458,#57459,#57460,#57461,#57462,#57463,#57464,#57465,#57466,#57467,
#57468,#57469,#57470,#57471,#57472,#57473,#57474,#57475,#57476,#57477,#57478,
#57479,#57480,#57481,#57482,#57483,#57484,#57485,#57486,#57487,#57488,#57489,
#57490,#57491,#57492,#57493,#57494,#57495,#57496,#57497,#57498,#57499,#57500,
#57501),.UNSPECIFIED.,.F.,.F.,(4,1,1,1,1,1,1,1,1,1,1,1,1,1,1,1,1,1,1,1,
1,1,1,1,1,1,1,1,1,1,1,1,1,1,1,1,1,1,1,1,1,1,1,1,1,1,1,1,1,1,1,1,1,1,1,1,
1,1,1,1,1,1,1,1,1,1,1,1,1,1,1,1,1,1,1,1,1,1,1,1,1,1,1,1,1,1,1,1,1,1,1,1,
1,1,1,1,1,1,1,1,1,1,1,1,1,1,1,1,1,1,1,1,1,1,1,1,1,1,1,1,1,1,1,1,1,1,1,1,
1,1,1,1,1,1,1,1,1,1,1,1,1,1,1,1,1,1,4),(94.7323961409497,94.8262562134414,
95.2611295230986,95.6960028329042,96.1308761428578,96.5657494529591,97.0006227632077,
97.4354960736028,97.870369384144,98.3052426948304,98.7401160056612,99.1749893166354,
99.6098626277522,100.04473593901,100.915335253024,101.351061255639,101.785934567313,
102.220807879124,102.655681191068,103.090554503145,103.525427815353,104.395174440154,
105.264921065453,105.699794378283,106.134667691232,106.569541004295,107.004414317471,
107.8750136343,108.745612951339,109.615359578629,110.485106206296,111.354852834309,
112.224599462639,113.094346091254,113.964092720119,114.834692038763,115.705291357499,
116.575037986826,117.444784616267,118.314531245777,119.184277875311,120.054024504821,
120.923771134261,121.794370453112,122.66496977189,123.534716400968,124.404463029834,
125.274209658448,126.143956286779,127.013702914792,127.883449542458,128.754048859798,
129.624648176939,130.494394803617,131.364141429857,132.233888055637,133.103634680937,
133.973381305737,134.843127930023,135.71372724472,136.584326559147,137.019199870684,
137.454073182083,137.888946493341,138.323819804458,139.193566426263,140.063313047491,
140.498186357887,140.933059668136,141.367932978237,141.802806288191,142.237679597997,
142.673405599673,143.109131601348,143.544004910857,143.978878220217,144.413751529429,
144.848624838491,145.283498147405,145.718371456171,146.153244764789,146.588118073258,
147.022991381581,147.457864689756,147.892737997785,148.327611305669,148.762484613407,
149.197357921002,149.633083921574,150.068809922147,150.503683229455,150.938556536623,
151.37342984365,151.808303150538,152.243176457288,152.678049763901,153.112923070379,
153.547796376722,153.982669682934,154.417542989014,154.852416294964,155.287289600787,
155.722162906483,156.157036212055,156.592762211626,157.028488211198,157.463361516526,
157.898234821735,158.333108126826,158.767981431803,159.202854736666,159.637728041419,
160.072601346062,160.507474650599,160.94234795503,161.37722125936,161.812094563589,
162.246967867721,162.681841171757,163.1167144757,163.552440474473,163.988166473247,
164.423039777011,164.85791308069,165.292786384286,165.727659687801,166.162532991238,
166.597406294601,167.03227959789,167.46715290111,167.902026204262,168.33689950735,
168.771772810376,169.206646113343,169.641519416254,170.076392719112,170.512118717363,
170.947844715614,171.382718018374,171.817591321089,172.252464623762,172.687337926397,
173.122211228996,173.557084531561,173.991957834097,174.426831136606,174.671174272867),
 .UNSPECIFIED.) ;
#3353 = B_SPLINE_CURVE_WITH_KNOTS('',3,(#64473,#64474,#64475,#64476,#64477,
#64478,#64479,#64480,#64481,#64482,#64483,#64484,#64485),.UNSPECIFIED.,
 .F.,.F.,(4,3,3,3,4),(0.,0.0778109650715507,0.156406745035681,0.238225011997873,
0.302239126480066),.UNSPECIFIED.) ;
#3354 = B_SPLINE_CURVE_WITH_KNOTS('',3,(#64486,#64487,#64488,#64489,#64490,
#64491,#64492,#64493,#64494,#64495,#64496,#64497,#64498,#64499,#64500,#64501,
#64502,#64503,#64504,#64505,#64506,#64507,#64508,#64509,#64510,#64511,#64512,
#64513,#64514,#64515,#64516,#64517,#64518,#64519,#64520,#64521,#64522,#64523,
#64524,#64525,#64526,#64527,#64528,#64529,#64530,#64531,#64532,#64533,#64534,
#64535,#64536,#64537,#64538,#64539,#64540,#64541,#64542,#64543,#64544,#64545,
#64546,#64547,#64548,#64549,#64550,#64551,#64552,#64553,#64554,#64555,#64556,
#64557,#64558),.UNSPECIFIED.,.F.,.F.,(4,3,3,3,3,3,3,3,3,3,3,3,3,3,3,3,3,
3,3,3,3,3,3,3,4),(0.730465481580952,0.828645125064031,1.05028297683293,
1.25837815006847,1.27510983870173,1.45572385054788,1.50312162767457,1.73316624271266,
1.90167574230222,1.96765453876246,2.20387853992392,2.44262970595966,2.62527594874715,
2.68580352301487,2.90417726726914,2.93079333089591,3.16390700345105,3.17732285394433,
3.35312908465868,3.42916468918551,3.68305064914715,3.93956813737864,4.1221204438191,
4.19992860565306,4.25678609882998),.UNSPECIFIED.) ;
#3355 = B_SPLINE_CURVE_WITH_KNOTS('',3,(#71535,#71536,#71537,#71538,#71539,
#71540,#71541,#71542,#71543,#71544,#71545,#71546,#71547,#71548,#71549,#71550),
 .UNSPECIFIED.,.F.,.F.,(4,3,3,3,3,4),(0.0598809947678152,0.135924535410352,
0.211078185367313,0.230755660513956,0.309208503339108,0.36825634451708),
 .UNSPECIFIED.) ;
#3356 = B_SPLINE_CURVE_WITH_KNOTS('',3,(#71552,#71553,#71554,#71555,#71556,
#71557,#71558,#71559,#71560,#71561,#71562,#71563,#71564,#71565,#71566,#71567,
#71568,#71569,#71570,#71571,#71572,#71573,#71574,#71575,#71576,#71577,#71578,
#71579,#71580,#71581,#71582,#71583,#71584,#71585,#71586,#71587,#71588,#71589,
#71590,#71591),.UNSPECIFIED.,.F.,.F.,(4,2,2,2,2,2,2,2,2,2,2,2,2,2,2,2,2,
2,2,4),(9.99997384787396E-7,0.0135018971911158,0.0220946867910526,0.027582782468828,
0.0313908326607115,0.0327527068279077,0.0343893874316741,0.0345526414539241,
0.0345596766530826,0.0345660072734853,0.0345689326430106,0.0345711188771073,
0.0345734204079688,0.0345769493878356,0.0345871620488376,0.0367578642760943,
0.040111326215381,0.0450373013211218,0.0525487888573377,0.0677449129025004),
 .UNSPECIFIED.) ;
#3357 = B_SPLINE_CURVE_WITH_KNOTS('',3,(#71592,#71593,#71594,#71595,#71596,
#71597,#71598,#71599,#71600,#71601,#71602,#71603,#71604,#71605,#71606,#71607,
#71608,#71609,#71610,#71611,#71612,#71613,#71614,#71615,#71616,#71617,#71618,
#71619,#71620,#71621,#71622,#71623,#71624,#71625,#71626,#71627,#71628,#71629,
#71630,#71631,#71632,#71633,#71634,#71635,#71636,#71637,#71638,#71639,#71640,
#71641,#71642,#71643,#71644,#71645,#71646,#71647,#71648,#71649,#71650,#71651,
#71652,#71653,#71654,#71655,#71656,#71657,#71658,#71659,#71660,#71661,#71662,
#71663,#71664,#71665,#71666,#71667,#71668,#71669,#71670,#71671,#71672,#71673,
#71674,#71675,#71676,#71677,#71678,#71679,#71680,#71681,#71682,#71683,#71684,
#71685,#71686,#71687,#71688,#71689,#71690,#71691,#71692,#71693,#71694,#71695,
#71696,#71697,#71698,#71699,#71700,#71701,#71702,#71703,#71704,#71705,#71706,
#71707,#71708,#71709,#71710,#71711,#71712,#71713,#71714,#71715,#71716,#71717,
#71718,#71719,#71720,#71721,#71722,#71723,#71724,#71725,#71726,#71727,#71728,
#71729,#71730,#71731,#71732,#71733,#71734,#71735,#71736,#71737,#71738,#71739,
#71740,#71741,#71742,#71743,#71744,#71745,#71746,#71747,#71748,#71749,#71750,
#71751,#71752,#71753,#71754,#71755,#71756,#71757,#71758,#71759,#71760,#71761,
#71762,#71763,#71764,#71765,#71766,#71767,#71768,#71769,#71770,#71771,#71772,
#71773,#71774,#71775,#71776,#71777,#71778,#71779,#71780,#71781,#71782,#71783,
#71784,#71785,#71786,#71787,#71788,#71789,#71790,#71791,#71792,#71793,#71794,
#71795,#71796,#71797,#71798,#71799,#71800,#71801,#71802,#71803,#71804,#71805,
#71806,#71807,#71808,#71809,#71810,#71811,#71812,#71813,#71814,#71815,#71816,
#71817,#71818,#71819,#71820,#71821,#71822,#71823,#71824,#71825,#71826,#71827,
#71828,#71829,#71830,#71831,#71832,#71833,#71834,#71835,#71836,#71837,#71838,
#71839,#71840,#71841,#71842,#71843,#71844,#71845,#71846,#71847,#71848,#71849,
#71850,#71851,#71852,#71853,#71854,#71855,#71856,#71857,#71858,#71859,#71860,
#71861,#71862,#71863,#71864,#71865,#71866,#71867,#71868,#71869,#71870,#71871,
#71872,#71873,#71874,#71875,#71876,#71877,#71878,#71879,#71880,#71881,#71882,
#71883,#71884,#71885,#71886,#71887,#71888,#71889,#71890,#71891,#71892,#71893,
#71894,#71895,#71896,#71897,#71898,#71899,#71900,#71901,#71902,#71903,#71904,
#71905,#71906,#71907,#71908,#71909,#71910,#71911,#71912,#71913,#71914,#71915,
#71916,#71917,#71918,#71919,#71920,#71921,#71922,#71923,#71924,#71925,#71926,
#71927,#71928,#71929,#71930,#71931,#71932,#71933,#71934,#71935,#71936,#71937,
#71938,#71939,#71940,#71941,#71942,#71943,#71944,#71945,#71946,#71947,#71948,
#71949,#71950,#71951,#71952,#71953,#71954,#71955,#71956,#71957,#71958,#71959),
 .UNSPECIFIED.,.F.,.F.,(4,2,2,2,2,2,2,2,2,2,2,2,2,2,2,2,2,2,2,2,2,2,2,2,
2,2,2,2,2,2,2,2,2,2,2,2,2,2,2,2,2,2,2,2,2,2,2,2,2,2,2,2,2,2,2,2,2,2,2,2,
2,2,2,2,2,2,2,2,2,2,2,2,2,2,2,2,2,2,2,2,2,2,2,2,2,2,2,2,2,2,2,2,2,2,2,2,
2,2,2,2,2,2,2,2,2,2,2,2,2,2,2,2,2,2,2,2,2,2,2,2,2,2,2,2,2,2,2,2,2,2,2,2,
2,2,2,2,2,2,2,2,2,2,2,2,2,2,2,2,2,2,2,2,2,2,2,2,2,2,2,2,2,2,2,2,2,2,2,2,
2,2,2,2,2,2,2,2,2,2,2,2,2,2,2,4),(1.35400733413699E-6,0.00247712615579827,
0.00416327824388871,0.00508094205146327,0.00600249339869984,0.00706335045674913,
0.00883969038701396,0.0148099473822476,0.0223717149096194,0.0282144997247987,
0.0301112620467383,0.0317402129382764,0.0334276492258154,0.035620968207884,
0.04014858204514,0.041818613145435,0.0446047361014287,0.0527583621791066,
0.056170953193112,0.0582260663201588,0.0600962810291678,0.0613627721698091,
0.062890447110422,0.0656053777468073,0.0781892490459218,0.0837716676672865,
0.0863815797603843,0.0884353175008502,0.0896926063713129,0.0909040769289953,
0.0925010147903435,0.0957213105472747,0.107315595210945,0.110987479881035,
0.112703162161221,0.113752244471158,0.114706885863388,0.115459320656402,
0.116244504662199,0.117671271441775,0.124286961621675,0.129221268253395,
0.132637342200675,0.134292593949302,0.135648728949349,0.136457286584393,
0.137217119793651,0.138224392156069,0.140288657651391,0.15170269218118,
0.154607426891558,0.156079206690623,0.157023151154972,0.157823017364658,
0.158553592630756,0.15932922122094,0.160778639609794,0.169274631208156,
0.17634068036209,0.178159353561367,0.17920223816847,0.180252674718397,0.180259238384283,
0.180265816165773,0.180272408897723,0.180279016995136,0.180285641276059,
0.180292281883292,0.180298939237232,0.180305613920904,0.180312306657082,
0.180319018096007,0.180325748485621,0.180332498553139,0.180339268810392,
0.180346059541105,0.180352871422257,0.180359704913109,0.18036656035672,
0.180373438439803,0.180380339998498,0.180387264920328,0.18039421413319,
0.180401188293552,0.180408187593391,0.180415212537324,0.180422263678796,
0.180429341619825,0.180433899500866,0.180438500021273,0.180443144549349,
0.180447833609563,0.180452567793726,0.180457348925566,0.18046217785813,
0.180467055297385,0.18047198255009,0.180476960905836,0.180481991429058,
0.180487075020832,0.180492212776601,0.180497405893481,0.180502655702569,
0.180507963598798,0.180513330421916,0.180518757821487,0.180524247036456,
0.180529799495268,0.18053541611957,0.180541098419139,0.1812540104352,0.182637078659382,
0.184907612682179,0.190264930962229,0.19721030750339,0.199018921921987,
0.200342886349612,0.201754309915285,0.203268702276234,0.205528536271081,
0.211010514357248,0.213215625083288,0.214788461835044,0.216383819945492,
0.216677045527393,0.217059609681938,0.21736670252085,0.218221242950562,
0.222644625572557,0.227038488681671,0.228286630614335,0.230499490647744,
0.233501249236801,0.236831559789177,0.243983859626164,0.245565587400414,
0.246852731705488,0.248082986420242,0.248115535241426,0.248150077301255,
0.248186785422691,0.24822584879476,0.248267474505976,0.248311889112464,
0.248359340307674,0.248410098749749,0.248464459771102,0.24852274514359,
0.248585304912807,0.248652519012008,0.248724798736779,0.250293175307972,
0.252802035704825,0.258274709663911,0.258524204270529,0.258641428066646,
0.264406706682384,0.266093408532013,0.267063302604525,0.267797752698992,
0.268629450310478,0.269666667475709,0.27127109378087,0.274485218599025,
0.28441766485709,0.286615027587656,0.287893040214175,0.289005127074856,
0.290350347390146,0.293262005179613,0.297735907724777,0.305254160455839,
0.307305008735793,0.308761349714037,0.310272174180748,0.311899572851342,
0.314318074144669,0.320539171758634,0.322438859760375,0.324064743577309,
0.330918118892867,0.335527404899377,0.33711098117137,0.338630983095817),
 .UNSPECIFIED.) ;
#3358 = B_SPLINE_CURVE_WITH_KNOTS('',3,(#71963,#71964,#71965,#71966,#71967,
#71968,#71969,#71970,#71971,#71972,#71973,#71974),.UNSPECIFIED.,.F.,.F.,
(4,2,2,2,2,4),(-0.0931391249568014,-0.0907876281662553,-0.0794385020809448,
-0.0680893759956343,-0.0567415781260163,-0.0453937802563982),
 .UNSPECIFIED.) ;
#3359 = B_SPLINE_CURVE_WITH_KNOTS('',3,(#71975,#71976,#71977,#71978),
 .UNSPECIFIED.,.F.,.F.,(4,4),(0.282642643684195,0.354822145847901),
 .UNSPECIFIED.) ;
#3360 = B_SPLINE_CURVE_WITH_KNOTS('',3,(#71980,#71981,#71982,#71983,#71984,
#71985,#71986,#71987,#71988,#71989),.UNSPECIFIED.,.F.,.F.,(4,2,2,2,4),(0.0907876281662566,
0.102136754251567,0.113485880336878,0.124833678206496,0.136181476076114),
 .UNSPECIFIED.) ;
#3361 = B_SPLINE_CURVE_WITH_KNOTS('',3,(#71990,#71991,#71992,#71993,#71994,
#71995,#71996,#71997,#71998,#71999),.UNSPECIFIED.,.F.,.F.,(4,2,2,2,4),(0.136181476076114,
0.147529243922143,0.158877011768171,0.170226134050342,0.181575256332513),
 .UNSPECIFIED.) ;
#3362 = B_SPLINE_CURVE_WITH_KNOTS('',3,(#72000,#72001,#72002,#72003,#72004,
#72005,#72006,#72007,#72008,#72009),.UNSPECIFIED.,.F.,.F.,(4,2,2,2,4),(-0.0453929098666937,
-0.0340453596051069,-0.02269780934352,-0.01134890467176,0.),
 .UNSPECIFIED.) ;
#3363 = B_SPLINE_CURVE_WITH_KNOTS('',3,(#78980,#78981,#78982,#78983,#78984,
#78985,#78986,#78987,#78988,#78989,#78990,#78991,#78992,#78993,#78994,#78995),
 .UNSPECIFIED.,.F.,.F.,(4,3,3,3,3,4),(0.0598607559016046,0.135904671484349,
0.211058386868452,0.230755571039204,0.309208126739232,0.368256344517073),
 .UNSPECIFIED.) ;
#3364 = B_SPLINE_CURVE_WITH_KNOTS('',3,(#78996,#78997,#78998,#78999,#79000,
#79001,#79002,#79003,#79004,#79005,#79006,#79007,#79008,#79009,#79010,#79011,
#79012,#79013,#79014,#79015,#79016,#79017,#79018,#79019,#79020,#79021,#79022,
#79023,#79024,#79025,#79026,#79027,#79028,#79029,#79030,#79031,#79032,#79033,
#79034,#79035),.UNSPECIFIED.,.F.,.F.,(4,2,2,2,2,2,2,2,2,2,2,2,2,2,2,2,2,
2,2,4),(8.8129793943429E-6,0.0135075679582764,0.0221000806739361,0.0275880663744416,
0.0313960477253353,0.0327588819471267,0.0343944713916458,0.0345576172666708,
0.0345645498592877,0.0345709399602103,0.0345738770438662,0.0345760653634415,
0.0345783628973854,0.0345818439872346,0.0345918197813435,0.0363912982801799,
0.0395253587707758,0.0441846088748481,0.051190397675679,0.0673693904034745),
 .UNSPECIFIED.) ;
#3365 = B_SPLINE_CURVE_WITH_KNOTS('',3,(#79039,#79040,#79041,#79042,#79043,
#79044,#79045,#79046,#79047),.UNSPECIFIED.,.F.,.F.,(4,1,1,1,1,1,4),(0.,
0.520304865070705,0.709542561390409,0.804161409708611,0.898780258026813,
1.15893269056541,1.419085123104),.UNSPECIFIED.) ;
#3366 = B_SPLINE_CURVE_WITH_KNOTS('',3,(#79049,#79050,#79051,#79052,#79053,
#79054,#79055,#79056,#79057,#79058),.UNSPECIFIED.,.F.,.F.,(4,1,1,1,1,1,
1,4),(1.419085123104,1.67923755563226,1.93938998816052,2.03400883639567,
2.12862768463082,2.31786538114359,2.57801781366682,2.83817024619004),
 .UNSPECIFIED.) ;
#3367 = B_SPLINE_CURVE_WITH_KNOTS('',3,(#79096,#79097,#79098,#79099,#79100,
#79101,#79102,#79103,#79104,#79105),.UNSPECIFIED.,.F.,.F.,(4,1,1,1,1,1,
1,4),(1.41908512308802,1.67923755561058,1.93938998813313,2.03400883648099,
2.12862768482886,2.3178653810957,2.57801781365659,2.83817024621747),
 .UNSPECIFIED.) ;
#3368 = B_SPLINE_CURVE_WITH_KNOTS('',3,(#79106,#79107,#79108,#79109,#79110,
#79111,#79112,#79113,#79114),.UNSPECIFIED.,.F.,.F.,(4,1,1,1,1,1,4),(0.,
0.520304865043955,0.70954256158844,0.804161409794499,0.898780258000557,
1.15893269054429,1.41908512308802),.UNSPECIFIED.) ;
#3369 = B_SPLINE_CURVE_WITH_KNOTS('',3,(#79152,#79153,#79154,#79155,#79156,
#79157,#79158,#79159,#79160,#79161),.UNSPECIFIED.,.F.,.F.,(4,1,1,1,1,1,
1,4),(1.41908512299766,1.67923755554141,1.93938998808516,2.03400883629124,
2.12862768449733,2.31786538104175,2.57801781362961,2.83817024621746),
 .UNSPECIFIED.) ;
#3370 = B_SPLINE_CURVE_WITH_KNOTS('',3,(#79162,#79163,#79164,#79165,#79166,
#79167,#79168,#79169,#79170),.UNSPECIFIED.,.F.,.F.,(4,1,1,1,1,1,4),(0.,
0.520304864990006,0.709542561256855,0.80416140961432,0.898780257971786,
1.15893269048473,1.41908512299766),.UNSPECIFIED.) ;
#3371 = B_SPLINE_CURVE_WITH_KNOTS('',3,(#79174,#79175,#79176,#79177,#79178,
#79179,#79180,#79181,#79182),.UNSPECIFIED.,.F.,.F.,(4,1,1,1,1,1,4),(0.,
0.520304865114576,0.709542561608101,0.804161409843274,0.898780258078447,
1.1589326906067,1.41908512313495),.UNSPECIFIED.) ;
#3372 = B_SPLINE_CURVE_WITH_KNOTS('',3,(#79184,#79185,#79186,#79187,#79188,
#79189,#79190,#79191,#79192,#79193),.UNSPECIFIED.,.F.,.F.,(4,1,1,1,1,1,
1,4),(1.41908512313495,1.67923755567353,1.9393899882121,2.03400883653032,
2.12862768484853,2.31786538116822,2.57801781373375,2.83817024629929),
 .UNSPECIFIED.) ;
#3373 = B_SPLINE_CURVE_WITH_KNOTS('',3,(#79271,#79272,#79273,#79274,#79275,
#79276,#79277,#79278,#79279,#79280,#79281),.UNSPECIFIED.,.T.,.F.,(4,1,1,
1,1,1,1,1,4),(0.,0.117806748710524,0.235613497421048,0.353420242239986,
0.471226987058923,0.58903373187812,0.706840476697317,0.824647225407855,
0.942453974118393),.UNSPECIFIED.) ;
#3374 = B_SPLINE_CURVE_WITH_KNOTS('',3,(#79318,#79319,#79320,#79321,#79322,
#79323,#79324,#79325,#79326,#79327,#79328,#79329,#79330,#79331,#79332,#79333,
#79334,#79335,#79336,#79337,#79338,#79339,#79340,#79341,#79342,#79343,#79344,
#79345,#79346,#79347,#79348,#79349,#79350,#79351,#79352,#79353,#79354,#79355,
#79356,#79357,#79358,#79359,#79360,#79361,#79362,#79363,#79364,#79365,#79366,
#79367,#79368,#79369,#79370,#79371,#79372,#79373,#79374,#79375,#79376,#79377,
#79378,#79379,#79380,#79381,#79382,#79383,#79384,#79385,#79386,#79387,#79388,
#79389,#79390,#79391,#79392,#79393,#79394,#79395,#79396,#79397,#79398,#79399,
#79400,#79401,#79402,#79403,#79404,#79405,#79406,#79407,#79408,#79409,#79410,
#79411,#79412,#79413,#79414,#79415,#79416,#79417,#79418,#79419,#79420,#79421,
#79422,#79423,#79424,#79425,#79426,#79427,#79428,#79429,#79430,#79431,#79432,
#79433,#79434,#79435,#79436,#79437,#79438,#79439,#79440,#79441,#79442,#79443,
#79444,#79445,#79446,#79447,#79448,#79449,#79450,#79451,#79452,#79453,#79454,
#79455,#79456,#79457,#79458,#79459,#79460,#79461,#79462,#79463,#79464,#79465,
#79466,#79467,#79468,#79469,#79470,#79471,#79472,#79473,#79474,#79475,#79476,
#79477,#79478,#79479,#79480,#79481,#79482,#79483,#79484,#79485),
 .UNSPECIFIED.,.F.,.F.,(4,2,2,2,2,2,2,2,2,2,2,2,2,2,2,2,2,2,2,2,2,2,2,2,
2,2,2,2,2,2,2,2,2,2,2,2,2,2,2,2,2,2,2,2,2,2,2,2,2,2,2,2,2,2,2,2,2,2,2,2,
2,2,2,2,2,2,2,2,2,2,2,2,2,2,2,2,2,2,2,2,2,2,2,4),(-0.220763983380471,-0.212810338743189,
-0.210826302908365,-0.209271007576308,-0.207760980376256,-0.205729488094328,
-0.198550181809563,-0.194693795352243,-0.191844661325702,-0.190288509145287,
-0.188362306697201,-0.184999537283139,-0.180416472909434,-0.177999557055194,
-0.176979917204659,-0.17545943341679,-0.169329841502711,-0.167326009010082,
-0.165010107168382,-0.163313661316864,-0.161023174884449,-0.15372738344787,
-0.149942801988463,-0.147940388957888,-0.146174507780922,-0.14492471603392,
-0.143254578734082,-0.139977364430561,-0.132761299778805,-0.129907182850962,
-0.12772776186146,-0.12769522261391,-0.127662280121649,-0.127628703111083,
-0.127594235626406,-0.127558587343492,-0.127521421133998,-0.127482336198394,
-0.125819004945782,-0.123790181619449,-0.118018980404149,-0.115257240279385,
-0.113532448213236,-0.112659152515239,-0.111622338612391,-0.110439445580995,
-0.105393490852793,-0.101142710955009,-0.0984836507689282,-0.0959423330614772,
-0.0924670231571394,-0.0856704509335571,-0.0830826422246745,-0.0810670415820549,
-0.0801905444928017,-0.0800237634118451,-0.0798508645920698,-0.0797151871859187,
-0.0796106920962894,-0.0765192041817014,-0.0724898724816029,-0.0649233609992019,
-0.0628333596238857,-0.0625221421103429,-0.0613894549744398,-0.0592211973507973,
-0.0578457591077455,-0.0536661847240215,-0.0503751810208162,-0.0488118397384947,
-0.0471863838408071,-0.0401191690844113,-0.036693088908186,-0.0347854974643231,
-0.0327365419518084,-0.0288818466209434,-0.0233041197359696,-0.0196358343583312,
-0.0180950601031717,-0.016951466256656,-0.0158400932091164,-0.0145364062440794,
-0.0126256867425368,-1.00000005442968E-6),.UNSPECIFIED.) ;
#3375 = B_SPLINE_CURVE_WITH_KNOTS('',3,(#79488,#79489,#79490,#79491,#79492,
#79493,#79494,#79495,#79496,#79497,#79498,#79499,#79500,#79501,#79502,#79503,
#79504,#79505,#79506,#79507,#79508,#79509,#79510,#79511,#79512,#79513,#79514,
#79515,#79516,#79517,#79518,#79519,#79520,#79521,#79522,#79523,#79524,#79525,
#79526,#79527,#79528,#79529,#79530,#79531,#79532,#79533,#79534,#79535,#79536,
#79537,#79538,#79539,#79540,#79541,#79542,#79543,#79544,#79545,#79546,#79547,
#79548,#79549,#79550,#79551,#79552,#79553,#79554,#79555,#79556,#79557,#79558,
#79559,#79560,#79561,#79562,#79563,#79564,#79565,#79566,#79567,#79568,#79569,
#79570,#79571,#79572,#79573,#79574,#79575,#79576,#79577,#79578,#79579,#79580,
#79581,#79582,#79583,#79584,#79585,#79586,#79587,#79588,#79589,#79590,#79591,
#79592,#79593,#79594,#79595,#79596,#79597,#79598,#79599,#79600,#79601,#79602,
#79603,#79604,#79605,#79606,#79607,#79608,#79609,#79610,#79611,#79612,#79613,
#79614,#79615,#79616,#79617,#79618,#79619,#79620,#79621,#79622,#79623,#79624,
#79625,#79626,#79627,#79628,#79629),.UNSPECIFIED.,.F.,.F.,(4,2,2,2,2,2,
2,2,2,2,2,2,2,2,2,2,2,2,2,2,2,2,2,2,2,2,2,2,2,2,2,2,2,2,2,2,2,2,2,2,2,2,
2,2,2,2,2,2,2,2,2,2,2,2,2,2,2,2,2,2,2,2,2,2,2,2,2,2,2,2,4),(-0.18252474525029,
-0.179400066977439,-0.175252692305652,-0.169924729691008,-0.168066528920694,
-0.166743109385763,-0.165501096667492,-0.164280350194813,-0.162567505415626,
-0.153584789316722,-0.149881802737214,-0.148075117524774,-0.147659331879399,
-0.147475574264912,-0.147253803230242,-0.147096076826089,-0.146984500314822,
-0.146905539465106,-0.146333073448781,-0.145369009076629,-0.144414998280596,
-0.142823355979458,-0.1369286174308,-0.132413903090164,-0.129285936821479,
-0.127635850380881,-0.12651547712041,-0.125561653504244,-0.124579822074233,
-0.123247741481105,-0.120332181776785,-0.114069642881635,-0.11110441261796,
-0.108953824687521,-0.106802809676022,-0.104459564364395,-0.0976458556504293,
-0.0940738777335949,-0.0913404381349576,-0.0885028731082607,-0.0798366421232186,
-0.0769226509456521,-0.074379646873931,-0.0720421619700198,-0.0689755666210176,
-0.0630996412878632,-0.0613131008382774,-0.0599974512973652,-0.0595480234483862,
-0.0594019673736506,-0.0592683762327051,-0.0591333251245316,-0.0589867853784717,
-0.0588186846865954,-0.0586168250482456,-0.0583652072776119,-0.0566822399161281,
-0.0538546350878509,-0.0440464063710776,-0.04191636283755,-0.0403248468776896,
-0.0387643875176817,-0.0368436467110806,-0.0336193237703689,-0.025875309571662,
-0.0229828527660033,-0.0202624149178314,-0.0102148474703489,-0.00824309809122128,
-0.00659087878765106,-6.19471680093315E-6),.UNSPECIFIED.) ;
#3376 = B_SPLINE_CURVE_WITH_KNOTS('',3,(#79634,#79635,#79636,#79637,#79638,
#79639,#79640,#79641,#79642,#79643,#79644,#79645,#79646,#79647,#79648,#79649,
#79650,#79651,#79652,#79653,#79654,#79655,#79656,#79657,#79658,#79659,#79660,
#79661,#79662,#79663,#79664,#79665,#79666,#79667,#79668,#79669,#79670,#79671,
#79672,#79673,#79674,#79675,#79676,#79677,#79678,#79679,#79680,#79681,#79682,
#79683,#79684,#79685,#79686,#79687,#79688,#79689,#79690,#79691,#79692,#79693,
#79694,#79695,#79696,#79697,#79698,#79699,#79700,#79701,#79702,#79703,#79704,
#79705,#79706,#79707,#79708,#79709,#79710,#79711,#79712,#79713,#79714,#79715,
#79716,#79717,#79718,#79719,#79720,#79721,#79722,#79723,#79724,#79725,#79726,
#79727,#79728,#79729,#79730,#79731,#79732,#79733,#79734,#79735,#79736,#79737,
#79738,#79739,#79740,#79741,#79742,#79743,#79744,#79745,#79746,#79747,#79748,
#79749,#79750,#79751,#79752,#79753,#79754,#79755,#79756,#79757,#79758,#79759,
#79760,#79761,#79762,#79763,#79764,#79765,#79766,#79767,#79768,#79769,#79770,
#79771,#79772,#79773,#79774,#79775,#79776,#79777,#79778,#79779,#79780,#79781,
#79782,#79783,#79784,#79785,#79786,#79787,#79788,#79789,#79790,#79791,#79792,
#79793,#79794,#79795,#79796,#79797,#79798,#79799,#79800,#79801,#79802,#79803,
#79804,#79805,#79806,#79807,#79808,#79809,#79810,#79811,#79812,#79813,#79814,
#79815,#79816,#79817,#79818,#79819,#79820,#79821,#79822,#79823,#79824,#79825,
#79826,#79827,#79828,#79829,#79830,#79831,#79832,#79833,#79834,#79835,#79836,
#79837,#79838,#79839,#79840,#79841,#79842,#79843,#79844,#79845,#79846,#79847,
#79848,#79849,#79850,#79851,#79852,#79853),.UNSPECIFIED.,.F.,.F.,(4,3,3,
3,3,3,3,3,3,3,3,3,3,3,3,3,3,3,3,3,3,3,3,3,3,3,3,3,3,3,3,3,3,3,3,3,3,3,3,
3,3,3,3,3,3,3,3,3,3,3,3,3,3,3,3,3,3,3,3,3,3,3,3,3,3,3,3,3,3,3,3,3,3,4),
(0.,0.114554107952554,0.219999579637262,0.40798083050021,0.571675274172504,
0.925887608273928,1.24364764883742,1.27682344199313,1.56513289539867,1.63103573085445,
1.92276380563121,1.98481039669498,2.30553261810542,2.33719940646081,2.68985168871465,
2.85597213219828,3.02278753371246,3.04298755913573,3.13367446983352,3.18807481875432,
3.3009537204216,3.39425414698803,3.57785099270887,3.7486975888156,4.10139086880436,
4.41302871221882,4.45537183311384,4.74928777620892,4.80732327925073,5.09839243438881,
5.16153555014084,5.47412129432304,5.51418781350788,5.86492791526386,6.04203405015412,
6.21914018504438,6.31436263900441,6.37615253991527,6.48557261069783,6.57181603734208,
6.75160383616011,6.92446829765038,7.27760414977274,7.59380314034735,7.6294205837199,
7.91857835915048,7.98363285125545,8.27582882629675,8.33593536794668,8.66001538388278,
8.6877517844213,9.04173195324679,9.21866661258249,9.39560127191819,9.49526269149975,
9.56422015730585,9.66918811922697,9.74731942042791,9.92430999212726,10.1013005638266,
10.4534629350241,10.7676564343516,10.8062607636447,11.0976054309995,11.1594970582837,
11.454185960616,11.5115370732495,11.8216297039995,11.8657493811883,12.2168162078705,
12.3939223660536,12.5710285242368,12.6749025971548,12.7522862024853),
 .UNSPECIFIED.) ;
#3377 = B_SPLINE_CURVE_WITH_KNOTS('',3,(#79854,#79855,#79856,#79857,#79858,
#79859,#79860,#79861,#79862,#79863,#79864,#79865,#79866,#79867,#79868,#79869,
#79870,#79871,#79872,#79873,#79874,#79875,#79876,#79877,#79878,#79879,#79880,
#79881,#79882,#79883,#79884,#79885,#79886,#79887,#79888,#79889,#79890,#79891,
#79892,#79893,#79894,#79895,#79896,#79897,#79898,#79899,#79900,#79901,#79902,
#79903,#79904,#79905,#79906,#79907,#79908,#79909,#79910,#79911,#79912,#79913,
#79914,#79915,#79916,#79917,#79918,#79919,#79920,#79921,#79922,#79923,#79924,
#79925,#79926,#79927,#79928,#79929,#79930,#79931,#79932,#79933,#79934,#79935,
#79936,#79937,#79938,#79939,#79940,#79941,#79942,#79943,#79944,#79945,#79946,
#79947,#79948,#79949,#79950,#79951,#79952,#79953,#79954,#79955,#79956,#79957,
#79958,#79959,#79960,#79961,#79962,#79963,#79964,#79965,#79966,#79967,#79968,
#79969,#79970,#79971,#79972,#79973,#79974,#79975,#79976,#79977,#79978,#79979,
#79980,#79981,#79982,#79983,#79984,#79985,#79986,#79987,#79988,#79989,#79990,
#79991,#79992,#79993,#79994,#79995,#79996,#79997,#79998,#79999,#80000,#80001,
#80002,#80003,#80004,#80005,#80006,#80007,#80008,#80009,#80010,#80011,#80012,
#80013,#80014,#80015,#80016,#80017,#80018,#80019,#80020,#80021,#80022,#80023,
#80024,#80025,#80026,#80027,#80028,#80029,#80030,#80031,#80032,#80033,#80034,
#80035,#80036,#80037,#80038,#80039,#80040,#80041,#80042,#80043,#80044,#80045,
#80046,#80047,#80048,#80049,#80050,#80051,#80052,#80053,#80054,#80055,#80056,
#80057,#80058,#80059,#80060,#80061,#80062,#80063,#80064,#80065,#80066,#80067,
#80068,#80069,#80070,#80071,#80072,#80073,#80074,#80075,#80076,#80077,#80078,
#80079,#80080,#80081,#80082,#80083,#80084,#80085),.UNSPECIFIED.,.F.,.F.,
(4,3,3,3,3,3,3,3,3,3,3,3,3,3,3,3,3,3,3,3,3,3,3,3,3,3,3,3,3,3,3,3,3,3,3,
3,3,3,3,3,3,3,3,3,3,3,3,3,3,3,3,3,3,3,3,3,3,3,3,3,3,3,3,3,3,3,3,3,3,3,3,
3,3,3,3,3,3,4),(0.,0.0894148861877891,0.133889678145916,0.297921036677569,
0.461212171674198,0.484629898594515,0.837282234412057,1.15861202910842,
1.19149448755028,1.48838290165772,1.54321518660845,1.8334631648485,1.89765827078402,
2.20002485219279,2.25210099027431,2.60280642166565,2.79655675959504,2.95701869061026,
3.07760215573877,3.18808892718112,3.26981110624916,3.31092626983993,3.47259185576712,
3.633470010557,3.6613092422968,4.01460245905827,4.34133219129516,4.36881472280183,
4.66775371996431,4.71935092585698,5.00902512576176,5.07356320109738,5.375729168866,
5.42777545310502,5.77865470103715,5.97878115250132,6.13136950553454,6.25595693487507,
6.37618626099941,6.4513335487717,6.483550843245,6.64287768424873,6.80133273686597,
6.83734305486834,7.19132473436349,7.52405859388823,7.5426224094343,7.8336538016193,
7.89706722798282,8.18493486313129,8.25104693288396,8.56343455351041,8.6015832902021,
8.95491331887032,9.16001611295106,9.30912556946611,9.4367215799293,9.56431759039249,
9.63444066958202,9.65993050174436,9.81702320746632,9.97319560073537,10.012728542287,
10.3669408040578,10.7013854790574,10.719103527886,11.0117551593669,11.0733158373996,
11.3671781532315,11.4245578244276,11.7283639906824,11.7787701291327,12.1305869844538,
12.3455036127973,12.4828898638758,12.6089564690771,12.7358311186926,12.7524660495637),
 .UNSPECIFIED.) ;
#3378 = B_SPLINE_CURVE_WITH_KNOTS('',3,(#80090,#80091,#80092,#80093,#80094,
#80095,#80096,#80097,#80098,#80099,#80100,#80101,#80102,#80103,#80104,#80105,
#80106,#80107,#80108,#80109,#80110,#80111,#80112,#80113,#80114,#80115,#80116,
#80117,#80118,#80119,#80120,#80121,#80122,#80123,#80124,#80125,#80126,#80127,
#80128,#80129,#80130,#80131,#80132,#80133,#80134,#80135,#80136,#80137,#80138,
#80139,#80140,#80141,#80142,#80143,#80144,#80145,#80146,#80147,#80148,#80149,
#80150,#80151,#80152,#80153,#80154,#80155,#80156,#80157,#80158,#80159,#80160,
#80161,#80162,#80163,#80164,#80165,#80166,#80167,#80168,#80169,#80170,#80171,
#80172,#80173,#80174,#80175,#80176,#80177,#80178,#80179,#80180,#80181,#80182,
#80183,#80184,#80185,#80186,#80187,#80188,#80189,#80190,#80191,#80192,#80193,
#80194,#80195,#80196,#80197,#80198,#80199,#80200,#80201,#80202,#80203,#80204,
#80205,#80206,#80207,#80208,#80209,#80210,#80211,#80212,#80213,#80214,#80215,
#80216,#80217,#80218,#80219,#80220,#80221,#80222,#80223,#80224,#80225,#80226,
#80227,#80228,#80229,#80230,#80231,#80232,#80233,#80234,#80235,#80236,#80237,
#80238,#80239,#80240,#80241,#80242,#80243,#80244,#80245,#80246,#80247,#80248,
#80249,#80250,#80251,#80252,#80253,#80254,#80255,#80256,#80257,#80258,#80259,
#80260,#80261,#80262,#80263,#80264,#80265,#80266,#80267,#80268,#80269,#80270,
#80271,#80272,#80273,#80274,#80275,#80276,#80277,#80278,#80279,#80280,#80281,
#80282,#80283,#80284,#80285,#80286,#80287,#80288,#80289,#80290,#80291,#80292,
#80293,#80294,#80295,#80296,#80297,#80298,#80299,#80300,#80301,#80302,#80303,
#80304,#80305,#80306,#80307,#80308,#80309,#80310,#80311,#80312),
 .UNSPECIFIED.,.F.,.F.,(4,3,3,3,3,3,3,3,3,3,3,3,3,3,3,3,3,3,3,3,3,3,3,3,
3,3,3,3,3,3,3,3,3,3,3,3,3,3,3,3,3,3,3,3,3,3,3,3,3,3,3,3,3,3,3,3,3,3,3,3,
3,3,3,3,3,3,3,3,3,3,3,3,3,3,4),(0.,0.100762857825756,0.17045455738185,0.347415762439074,
0.524376967496299,0.877381484509634,1.19821800653056,1.22826049812016,1.51697376328285,
1.58247279915011,1.87779658023047,1.93391776317192,2.25164505566527,2.28836068050304,
2.64280331320604,2.82167316119906,2.99350875161294,3.10266796924014,3.18807250430072,
3.28423663368526,3.34738831255791,3.5233640520366,3.69933979151529,4.05355206803615,
4.37985223749883,4.40620435589301,4.70171242540885,4.75694454204997,5.04601965453119,
5.11115683439866,5.42764767481781,5.46361882765795,5.81783110946781,6.00081498008659,
6.16978259404898,6.2828607180743,6.37613838180102,6.46714712814609,6.52211297837991,
6.68925611334493,6.85570174442494,6.87524886950579,7.22706540888955,7.5427802441183,
7.58104611352649,7.87520812138854,7.93428224769233,8.2234903967075,8.28872622840582,
8.59531361187601,8.64114684774855,8.99188712842038,9.18026879928742,9.34609939086034,
9.46276931651261,9.56422046408461,9.65091384739663,9.69916314071276,9.86319775131977,
10.0264998248966,10.0499034623499,10.4041157271119,10.7307046869009,10.7583279856935,
11.0558356759019,11.1095696963186,11.3979727180052,11.4637819917093,11.7745585768663,
11.8159445691956,12.1687425517332,12.3621786336217,12.5198069536285,12.6375810196589,
12.7523053453689),.UNSPECIFIED.) ;
#3379 = B_SPLINE_CURVE_WITH_KNOTS('',3,(#80313,#80314,#80315,#80316,#80317,
#80318,#80319,#80320,#80321,#80322,#80323,#80324,#80325,#80326,#80327,#80328,
#80329,#80330,#80331,#80332,#80333,#80334,#80335,#80336,#80337,#80338,#80339,
#80340,#80341,#80342,#80343,#80344,#80345,#80346,#80347,#80348,#80349,#80350,
#80351,#80352,#80353,#80354,#80355,#80356,#80357,#80358,#80359,#80360,#80361,
#80362,#80363,#80364,#80365,#80366,#80367,#80368,#80369,#80370,#80371,#80372,
#80373,#80374,#80375,#80376,#80377,#80378,#80379,#80380,#80381,#80382,#80383,
#80384,#80385,#80386,#80387,#80388,#80389,#80390,#80391,#80392,#80393,#80394,
#80395,#80396,#80397,#80398,#80399,#80400,#80401,#80402,#80403,#80404,#80405,
#80406,#80407,#80408,#80409,#80410,#80411,#80412,#80413,#80414,#80415,#80416,
#80417,#80418,#80419,#80420,#80421,#80422,#80423,#80424,#80425,#80426,#80427,
#80428,#80429,#80430,#80431,#80432,#80433,#80434,#80435,#80436,#80437,#80438,
#80439,#80440,#80441,#80442,#80443,#80444,#80445,#80446,#80447,#80448,#80449,
#80450,#80451,#80452,#80453,#80454,#80455,#80456,#80457,#80458,#80459,#80460,
#80461,#80462,#80463,#80464,#80465,#80466,#80467,#80468,#80469,#80470,#80471,
#80472,#80473,#80474,#80475,#80476,#80477,#80478,#80479,#80480,#80481,#80482,
#80483,#80484,#80485,#80486,#80487,#80488,#80489,#80490,#80491,#80492,#80493,
#80494,#80495,#80496,#80497,#80498,#80499,#80500,#80501,#80502,#80503,#80504,
#80505,#80506,#80507,#80508,#80509,#80510,#80511,#80512,#80513,#80514,#80515,
#80516,#80517,#80518,#80519,#80520,#80521,#80522,#80523,#80524,#80525,#80526,
#80527,#80528,#80529,#80530,#80531,#80532),.UNSPECIFIED.,.F.,.F.,(4,3,3,
3,3,3,3,3,3,3,3,3,3,3,3,3,3,3,3,3,3,3,3,3,3,3,3,3,3,3,3,3,3,3,3,3,3,3,3,
3,3,3,3,3,3,3,3,3,3,3,3,3,3,3,3,3,3,3,3,3,3,3,3,3,3,3,3,3,3,3,3,3,3,4),
(0.,0.103893003810878,0.181262498396716,0.358368655155245,0.535474811913774,
0.886541640300103,1.19673532348644,1.24075395493171,1.53528792411396,1.59279396171985,
1.88431414393547,1.94603026773208,2.25997509560389,2.29882808755841,2.65099046906085,
2.82798104483141,3.00497162060198,3.10991086391462,3.18806738078836,3.28775562074012,
3.35668976127941,3.5336244263954,3.71055909151139,4.06453925695613,4.38847961223419,
4.41635566929646,4.70870697419377,4.76865819735123,5.05774592416977,5.12287046168214,
5.43899161304988,5.47468689392592,5.82782275374672,6.00761036936649,6.18047500641398,
6.28988375072362,6.37613695915723,6.4713735827455,6.53315086103547,6.71025699441627,
6.88736312779706,7.23810322232236,7.55101366328478,7.59075550121641,7.88163753031553,
7.94496776270377,8.23896747477361,8.29691921461726,8.60855780948375,8.65090019138673,
9.00359345967117,9.18722179851666,9.35803689449882,9.47088359281189,9.56421233698863,
9.65492998924632,9.70930349363768,9.87612791713462,10.0422522333714,10.0624393716107,
10.4150916485022,10.7357912645928,10.7674806581858,11.0593569652461,11.1212553350823,
11.409386398908,11.4754676140256,11.7933709583769,11.826403454723,12.180615789613,
12.3685389651704,12.5322914820512,12.6468674178292,12.7522978599647),
 .UNSPECIFIED.) ;
#3380 = B_SPLINE_CURVE_WITH_KNOTS('',3,(#80537,#80538,#80539,#80540,#80541,
#80542,#80543,#80544,#80545,#80546,#80547,#80548,#80549,#80550,#80551,#80552,
#80553,#80554,#80555,#80556,#80557,#80558,#80559,#80560,#80561,#80562,#80563,
#80564,#80565,#80566,#80567,#80568,#80569,#80570,#80571,#80572,#80573,#80574,
#80575,#80576,#80577,#80578,#80579,#80580,#80581,#80582,#80583,#80584,#80585,
#80586,#80587,#80588,#80589,#80590,#80591,#80592,#80593,#80594,#80595,#80596,
#80597,#80598,#80599,#80600,#80601,#80602,#80603,#80604,#80605,#80606,#80607,
#80608,#80609,#80610,#80611,#80612,#80613,#80614,#80615,#80616,#80617,#80618,
#80619,#80620,#80621,#80622,#80623,#80624,#80625,#80626,#80627,#80628,#80629,
#80630,#80631,#80632,#80633,#80634,#80635,#80636,#80637,#80638,#80639,#80640,
#80641,#80642,#80643,#80644,#80645,#80646,#80647,#80648,#80649,#80650,#80651,
#80652,#80653,#80654,#80655,#80656,#80657,#80658,#80659,#80660,#80661,#80662,
#80663,#80664,#80665,#80666,#80667,#80668,#80669,#80670,#80671,#80672,#80673,
#80674,#80675,#80676,#80677,#80678,#80679,#80680,#80681,#80682,#80683,#80684,
#80685,#80686,#80687,#80688,#80689,#80690,#80691,#80692,#80693,#80694,#80695,
#80696,#80697,#80698,#80699,#80700,#80701,#80702,#80703,#80704,#80705,#80706,
#80707,#80708,#80709,#80710,#80711,#80712,#80713,#80714,#80715,#80716,#80717,
#80718,#80719,#80720,#80721,#80722,#80723,#80724,#80725,#80726,#80727,#80728,
#80729,#80730,#80731,#80732,#80733,#80734,#80735,#80736,#80737,#80738,#80739,
#80740,#80741,#80742,#80743,#80744,#80745,#80746,#80747,#80748,#80749,#80750,
#80751,#80752,#80753,#80754,#80755,#80756,#80757,#80758,#80759,#80760,#80761,
#80762,#80763,#80764,#80765),.UNSPECIFIED.,.F.,.F.,(4,3,3,3,3,3,3,3,3,3,
3,3,3,3,3,3,3,3,3,3,3,3,3,3,3,3,3,3,3,3,3,3,3,3,3,3,3,3,3,3,3,3,3,3,3,3,
3,3,3,3,3,3,3,3,3,3,3,3,3,3,3,3,3,3,3,3,3,3,3,3,3,3,3,3,3,3,4),(0.,0.0849567058115355,
0.121410866737072,0.283571067642219,0.444919421038145,0.475392252089173,
0.827665187221835,1.14808607613794,1.18210927518942,1.47839116596738,1.53459228457289,
1.82885507160418,1.88547168452342,2.19314502783543,2.23968397375804,2.59214615040927,
2.79038879486852,2.94635842870424,3.06998802803527,3.18810817019483,3.26440590431521,
3.29802675005529,3.45757822076252,3.61627514247094,3.65067925900212,4.00489154138233,
4.35563223002435,4.64617975589709,4.70984452935805,5.00046832574839,5.06284926268752,
5.36685554190499,5.41550181494416,5.76624256865231,5.97273593786443,6.1202225757179,
6.24822644256217,6.37623030940644,6.44733815583808,6.47439716292745,6.63221404230345,
6.78911562829056,6.82800759658552,7.18091231497168,7.51065136477143,7.53272928162441,
7.82487629705489,7.88694158774125,8.18083977413766,8.23818376656191,8.54281082978249,
8.59239607694621,8.94455897340147,9.1575282370111,9.2973571803608,9.4308647738549,
9.564372367349,9.62916114633184,9.64818402988998,9.80361159264067,9.95805838375808,
10.002396297147,10.3566085447957,10.5648455268548,10.7090424934517,10.9238830828392,
11.1385418510569,11.3532131814733,11.4174022576871,11.6640729394278,11.7698515234467,
12.1227348772726,12.3436966068405,12.4771776993501,12.6049451701728,12.7335676446473,
12.7552103037919),.UNSPECIFIED.) ;
#3381 = B_SPLINE_CURVE_WITH_KNOTS('',3,(#80766,#80767,#80768,#80769,#80770,
#80771,#80772,#80773,#80774,#80775,#80776,#80777,#80778,#80779,#80780,#80781,
#80782,#80783,#80784,#80785,#80786,#80787,#80788,#80789,#80790,#80791,#80792,
#80793,#80794,#80795,#80796,#80797,#80798,#80799,#80800,#80801,#80802,#80803,
#80804,#80805,#80806,#80807,#80808,#80809,#80810,#80811,#80812,#80813,#80814,
#80815,#80816,#80817,#80818,#80819,#80820,#80821,#80822,#80823,#80824,#80825,
#80826,#80827,#80828,#80829,#80830,#80831,#80832,#80833,#80834,#80835,#80836,
#80837,#80838,#80839,#80840,#80841,#80842,#80843,#80844,#80845,#80846,#80847,
#80848,#80849,#80850,#80851,#80852,#80853,#80854,#80855,#80856,#80857,#80858,
#80859,#80860,#80861,#80862,#80863,#80864,#80865,#80866,#80867,#80868,#80869,
#80870,#80871,#80872,#80873,#80874,#80875,#80876,#80877,#80878,#80879,#80880,
#80881,#80882,#80883,#80884,#80885,#80886,#80887,#80888,#80889,#80890,#80891,
#80892,#80893,#80894,#80895,#80896,#80897,#80898,#80899,#80900,#80901,#80902,
#80903,#80904,#80905,#80906,#80907,#80908,#80909,#80910,#80911,#80912,#80913,
#80914,#80915,#80916,#80917,#80918,#80919,#80920,#80921,#80922,#80923,#80924,
#80925,#80926,#80927,#80928,#80929,#80930,#80931,#80932,#80933,#80934,#80935,
#80936,#80937,#80938,#80939,#80940,#80941,#80942,#80943,#80944,#80945,#80946,
#80947,#80948,#80949,#80950,#80951,#80952,#80953,#80954,#80955,#80956,#80957,
#80958,#80959,#80960,#80961,#80962,#80963,#80964,#80965,#80966,#80967,#80968,
#80969,#80970,#80971,#80972,#80973,#80974,#80975,#80976,#80977,#80978,#80979,
#80980,#80981,#80982,#80983,#80984,#80985,#80986,#80987,#80988),
 .UNSPECIFIED.,.F.,.F.,(4,3,3,3,3,3,3,3,3,3,3,3,3,3,3,3,3,3,3,3,3,3,3,3,
3,3,3,3,3,3,3,3,3,3,3,3,3,3,3,3,3,3,3,3,3,3,3,3,3,3,3,3,3,3,3,3,3,3,3,3,
3,3,3,3,3,3,3,3,3,3,3,3,3,3,4),(0.,0.117766852480119,0.232496353538427,
0.425959269805488,0.58356076372737,0.936358747455187,1.24721516299566,1.28852133052573,
1.57691037403893,1.64273362456121,1.94009683856486,1.99397533075514,2.32101174159844,
2.34818760451099,2.70239985630971,2.86567318626521,3.02967152715542,3.05314018006163,
3.13984623840259,3.18808443459044,3.30474613545493,3.40620393305099,3.59458496913141,
3.76041618591283,4.11115646630507,4.4179620031712,4.46357709690046,4.75264568629906,
4.81802107035101,5.11225950860045,5.17125721849527,5.48698227134708,5.525237914481,
5.87705445117265,6.04348549182013,6.21060943622194,6.23019035170545,6.32120249042149,
6.37616561501542,6.4892370938465,6.58252073706138,6.76552124705007,6.93447223265948,
7.2886845102342,7.60525585812541,7.64114650722471,7.93025277521774,7.99535880099052,
8.29066722847324,8.34609897805127,8.67287428691527,8.69875128326739,9.05296354724675,
9.22893929137685,9.40491503550695,9.50113431130131,9.56423800268766,9.67334187672587,
9.75879459828048,9.93770082835329,10.109500019499,10.4639426784075,10.7812408318919,
10.8183855714955,11.1138898609533,11.1698305545815,11.4585507849351,11.5240428555817,
11.8445810390484,11.8749218597236,12.2279263926025,12.4048875910266,12.5818487894507,
12.6825950545204,12.7522985291244),.UNSPECIFIED.) ;
#3382 = B_SPLINE_CURVE_WITH_KNOTS('',3,(#80991,#80992,#80993,#80994,#80995,
#80996,#80997,#80998,#80999,#81000,#81001,#81002,#81003,#81004,#81005,#81006,
#81007,#81008,#81009,#81010,#81011,#81012,#81013,#81014,#81015,#81016,#81017,
#81018,#81019,#81020,#81021,#81022,#81023,#81024,#81025,#81026,#81027,#81028,
#81029,#81030,#81031,#81032,#81033,#81034,#81035,#81036,#81037,#81038,#81039,
#81040,#81041,#81042,#81043,#81044,#81045,#81046,#81047,#81048,#81049,#81050,
#81051,#81052,#81053,#81054,#81055,#81056,#81057,#81058,#81059,#81060,#81061,
#81062,#81063,#81064,#81065,#81066,#81067,#81068,#81069,#81070,#81071,#81072,
#81073,#81074,#81075,#81076,#81077,#81078,#81079,#81080,#81081,#81082,#81083,
#81084,#81085,#81086,#81087,#81088,#81089,#81090,#81091,#81092,#81093,#81094,
#81095,#81096,#81097,#81098,#81099,#81100,#81101,#81102,#81103,#81104,#81105,
#81106,#81107,#81108,#81109,#81110,#81111,#81112,#81113,#81114,#81115,#81116,
#81117,#81118,#81119,#81120,#81121,#81122,#81123,#81124,#81125,#81126,#81127,
#81128,#81129,#81130,#81131,#81132,#81133,#81134,#81135,#81136,#81137,#81138,
#81139,#81140,#81141,#81142,#81143,#81144,#81145,#81146,#81147,#81148,#81149,
#81150,#81151,#81152,#81153,#81154,#81155,#81156,#81157,#81158,#81159,#81160,
#81161,#81162,#81163,#81164,#81165,#81166,#81167,#81168,#81169,#81170,#81171,
#81172,#81173,#81174,#81175,#81176,#81177,#81178,#81179,#81180,#81181,#81182,
#81183,#81184,#81185,#81186,#81187,#81188,#81189,#81190,#81191,#81192,#81193,
#81194,#81195,#81196,#81197,#81198,#81199,#81200,#81201,#81202,#81203,#81204,
#81205,#81206,#81207,#81208,#81209,#81210,#81211,#81212,#81213,#81214,#81215,
#81216,#81217,#81218,#81219,#81220,#81221,#81222,#81223,#81224,#81225,#81226,
#81227,#81228,#81229,#81230,#81231,#81232,#81233,#81234,#81235,#81236,#81237,
#81238,#81239,#81240,#81241,#81242,#81243,#81244,#81245,#81246,#81247,#81248,
#81249,#81250,#81251,#81252,#81253,#81254,#81255,#81256,#81257,#81258,#81259,
#81260,#81261,#81262,#81263,#81264,#81265,#81266,#81267,#81268,#81269,#81270,
#81271,#81272,#81273,#81274,#81275,#81276,#81277,#81278,#81279,#81280,#81281,
#81282,#81283,#81284,#81285,#81286,#81287,#81288,#81289,#81290),
 .UNSPECIFIED.,.F.,.F.,(4,2,2,2,2,2,2,2,2,2,2,2,2,2,2,2,2,2,2,2,2,2,2,2,
2,2,2,2,2,2,2,2,2,2,2,2,2,2,2,2,2,2,2,2,2,2,2,2,2,2,2,2,2,2,2,2,2,2,2,2,
2,2,2,2,2,2,2,2,2,2,2,2,2,2,2,2,2,2,2,2,2,2,2,2,2,2,2,2,2,2,2,2,2,2,2,2,
2,2,2,2,2,2,2,2,2,2,2,2,2,2,2,2,2,2,2,2,2,2,2,2,2,2,2,2,2,2,2,2,2,2,2,2,
2,2,2,2,2,2,2,2,2,2,2,2,2,2,2,2,2,4),(-0.257894959744042,-0.253220611148935,
-0.252082519774515,-0.251189207858128,-0.2502706763012,-0.249204820691145,
-0.24734086125322,-0.238825211955683,-0.234956710782849,-0.232265582687393,
-0.232163656503359,-0.232079890411829,-0.232009429589355,-0.23194885477312,
-0.23189570103474,-0.231848145732546,-0.231804802747511,-0.231764583881055,
-0.231726602097676,-0.231690100812442,-0.231654398403906,-0.23161884023568,
-0.230646507521808,-0.229652146135218,-0.2283254697423,-0.225431560706624,
-0.219432808035315,-0.215918365425081,-0.213951525208257,-0.211667593912582,
-0.211297017030229,-0.210798316724895,-0.210069641212601,-0.209184079408535,
-0.20233480803109,-0.199071711636883,-0.196674826367858,-0.192673413721236,
-0.188338844281775,-0.185309143004634,-0.183063435515454,-0.180463010870351,
-0.172247574976944,-0.169227557805637,-0.166969106489589,-0.165718950597125,
-0.164550297675546,-0.162998755449737,-0.159450634129076,-0.151301404921013,
-0.148434861925196,-0.146764543296957,-0.145289493301241,-0.144420952767203,
-0.143261735333598,-0.141671941428281,-0.136953553242676,-0.134633536768281,
-0.129065614489829,-0.12586894668411,-0.124659009655095,-0.123667875186939,
-0.122712953941796,-0.122706902779335,-0.122700817345473,-0.122694696393175,
-0.122688538768037,-0.122682343223882,-0.122676108667069,-0.122669833751837,
-0.122663517479823,-0.122657158550683,-0.122650755298769,-0.122644306826007,
-0.122637811485778,-0.12263126801403,-0.122624675086352,-0.122618031304535,
-0.122611335124305,-0.122604585099646,-0.122597779832967,-0.122590917682396,
-0.122583997138402,-0.122577016970953,-0.122569975346635,-0.122562870404742,
-0.122555700497586,-0.122548464327288,-0.12254116008541,-0.122533785780757,
-0.122526339564397,-0.12251881963144,-0.122511223909231,-0.122503550667778,
-0.122495797889482,-0.122487963729255,-0.122480045927489,-0.122472042536743,
-0.122463951294876,-0.122455769992845,-0.122447496191321,-0.122439127884568,
-0.122430662619054,-0.1224220978723,-0.122413431228693,-0.121283105168391,
-0.119557604757718,-0.116062880165473,-0.107074205096058,-0.105202142314451,
-0.103854487638451,-0.102970526354438,-0.102907177308501,-0.102857423197713,
-0.101281612623738,-0.0993316703532008,-0.0956795824111655,-0.0888309643124724,
-0.0861370748464511,-0.0859955520258133,-0.0832106391533367,-0.0773048156889599,
-0.0731571830179152,-0.0730096294887505,-0.0728620764216494,-0.0727002874126334,
-0.0725018367868773,-0.0721447246476089,-0.0707043294314262,-0.0691077557991271,
-0.0654637854118928,-0.0610601613559754,-0.0589585948592443,-0.0572180043633603,
-0.0567189271384514,-0.0545935015097311,-0.0477781729190308,-0.0424783830991959,
-0.0401182720840394,-0.0381028158238574,-0.0355564513823461,-0.032173028311343,
-0.0238920353908075,-0.0211071460799632,-0.0181412510164185,-0.0145766045458494,
-0.00910418362044593,-0.00751977868442608,-0.00619932980695214,-1.00000002645206E-6),
 .UNSPECIFIED.) ;
#3383 = B_SPLINE_CURVE_WITH_KNOTS('',3,(#81293,#81294,#81295,#81296,#81297,
#81298,#81299,#81300,#81301,#81302,#81303,#81304,#81305,#81306,#81307,#81308,
#81309,#81310,#81311,#81312,#81313,#81314,#81315,#81316,#81317,#81318,#81319,
#81320,#81321,#81322,#81323,#81324,#81325,#81326,#81327,#81328,#81329,#81330,
#81331,#81332,#81333,#81334,#81335,#81336,#81337,#81338,#81339,#81340,#81341,
#81342,#81343,#81344,#81345,#81346,#81347,#81348,#81349,#81350,#81351,#81352,
#81353,#81354,#81355,#81356,#81357,#81358,#81359,#81360,#81361,#81362,#81363,
#81364,#81365,#81366,#81367,#81368,#81369,#81370,#81371,#81372,#81373,#81374,
#81375,#81376,#81377,#81378,#81379,#81380,#81381,#81382,#81383,#81384,#81385,
#81386,#81387,#81388,#81389,#81390,#81391,#81392,#81393,#81394,#81395,#81396,
#81397,#81398,#81399,#81400,#81401,#81402,#81403,#81404,#81405,#81406,#81407,
#81408,#81409,#81410,#81411,#81412,#81413,#81414,#81415,#81416,#81417,#81418,
#81419,#81420,#81421,#81422,#81423,#81424,#81425,#81426,#81427,#81428,#81429,
#81430,#81431,#81432,#81433,#81434,#81435,#81436,#81437,#81438,#81439,#81440,
#81441,#81442,#81443,#81444,#81445,#81446,#81447,#81448,#81449,#81450,#81451,
#81452,#81453,#81454,#81455,#81456,#81457,#81458,#81459,#81460,#81461,#81462,
#81463,#81464,#81465,#81466,#81467,#81468,#81469,#81470,#81471,#81472,#81473,
#81474,#81475,#81476,#81477,#81478,#81479,#81480,#81481,#81482,#81483,#81484,
#81485,#81486,#81487,#81488,#81489,#81490,#81491,#81492,#81493,#81494,#81495,
#81496,#81497,#81498,#81499,#81500,#81501,#81502,#81503,#81504,#81505,#81506,
#81507,#81508,#81509,#81510,#81511,#81512,#81513,#81514),.UNSPECIFIED.,
 .F.,.F.,(4,2,2,2,2,2,2,2,2,2,2,2,2,2,2,2,2,2,2,2,2,2,2,2,2,2,2,2,2,2,2,
2,2,2,2,2,2,2,2,2,2,2,2,2,2,2,2,2,2,2,2,2,2,2,2,2,2,2,2,2,2,2,2,2,2,2,2,
2,2,2,2,2,2,2,2,2,2,2,2,2,2,2,2,2,2,2,2,2,2,2,2,2,2,2,2,2,2,2,2,2,2,2,2,
2,2,2,2,2,2,2,4),(-0.21974730496944,-0.209497995751659,-0.207816227696814,
-0.206696348350822,-0.205767284698091,-0.20485397757947,-0.203644123970965,
-0.201163237535781,-0.199234334828623,-0.198913491876631,-0.192586005200389,
-0.188020363992073,-0.186092144364173,-0.185276519404618,-0.18332163303194,
-0.180721422658237,-0.173766453776646,-0.167938864952367,-0.166365261811103,
-0.163770327311883,-0.162358826389358,-0.160690850220444,-0.158448304110901,
-0.15228425029622,-0.144121818826867,-0.140893235816109,-0.138947282236318,
-0.138865006212637,-0.138785648892571,-0.138708812553493,-0.13863412632672,
-0.138561240968116,-0.138489823995273,-0.138419554947308,-0.138350120526013,
-0.138281209859491,-0.138212509414666,-0.138143697486611,-0.138074437950374,
-0.138004373215554,-0.137933115704807,-0.137860237518485,-0.137835732211627,
-0.136432771655794,-0.135030470253392,-0.133174489972427,-0.127354264807073,
-0.118311869408989,-0.114833620138255,-0.112062908143053,-0.111005128554945,
-0.110976089279789,-0.110945776024287,-0.110914132197716,-0.110881098781024,
-0.110846614335611,-0.110827740276134,-0.110804551101557,-0.110776089351518,
-0.11074120029057,-0.110698498801103,-0.110646335319223,-0.110582763233192,
-0.110521525369985,-0.110345951017164,-0.109869688106184,-0.108311784083106,
-0.10827868299426,-0.10824520687847,-0.10821132013487,-0.108176986417272,
-0.108142168373755,-0.108106827535724,-0.108070924329374,-0.108034417795035,
-0.10799726554041,-0.107959423681245,-0.107920846522564,-0.107881486501138,
-0.107841294113589,-0.10780021763837,-0.107758203039857,-0.107715193781533,
-0.104792570233929,-0.100834668518422,-0.0917717565902828,-0.0882811157453522,
-0.0867437366547149,-0.0853447743443662,-0.0838272385342882,-0.0790014398889958,
-0.0692014603300877,-0.0663858360611473,-0.0620178835475202,-0.0533675339317639,
-0.0502666772550644,-0.0473136918819925,-0.0441141213159802,-0.0372988874541403,
-0.0353544452877392,-0.0341090803360572,-0.0338991174967524,-0.032528273487166,
-0.030619718825037,-0.0274728686588918,-0.0176254071723615,-0.0155915957491533,
-0.0140813196430058,-0.0126105676500786,-0.0108387771806254,-5.22571535866158E-5),
 .UNSPECIFIED.) ;
#3384 = B_SPLINE_CURVE_WITH_KNOTS('',3,(#81522,#81523,#81524,#81525,#81526,
#81527,#81528,#81529,#81530,#81531,#81532,#81533,#81534,#81535,#81536,#81537,
#81538,#81539,#81540,#81541,#81542,#81543,#81544,#81545,#81546,#81547),
 .UNSPECIFIED.,.F.,.F.,(4,2,2,2,2,2,2,2,2,2,2,2,4),(9.99999996900801E-7,
0.0217536568115777,0.0435354891955391,0.0879397153262638,0.112564023697292,
0.137318935333563,0.162458662654742,0.187567234819558,0.213124132495112,
0.238695964082357,0.264191632957232,0.29041955787013,0.311836241868587),
 .UNSPECIFIED.) ;
#3385 = B_SPLINE_CURVE_WITH_KNOTS('',3,(#81549,#81550,#81551,#81552,#81553,
#81554,#81555,#81556),.UNSPECIFIED.,.F.,.F.,(4,2,2,4),(0.,0.0328258807040897,
0.0479820964185046,0.0625119124690952),.UNSPECIFIED.) ;
#3386 = B_SPLINE_CURVE_WITH_KNOTS('',3,(#81557,#81558,#81559,#81560,#81561,
#81562,#81563,#81564,#81565,#81566,#81567,#81568,#81569,#81570,#81571,#81572,
#81573,#81574,#81575,#81576,#81577,#81578,#81579,#81580,#81581,#81582,#81583,
#81584,#81585,#81586,#81587,#81588,#81589,#81590),.UNSPECIFIED.,.F.,.F.,
(4,2,2,2,2,2,2,2,2,2,2,2,2,2,2,2,4),(0.311836241868587,0.316507424623957,
0.342892888009964,0.369492419893424,0.396264677446643,0.409779859619715,
0.436779117207306,0.464022317104011,0.491926865768048,0.519205487048488,
0.547669956804294,0.575175692029193,0.603824409330207,0.632256986799627,
0.689732978983562,0.718666448865442,0.747725957477036),.UNSPECIFIED.) ;
#3387 = B_SPLINE_CURVE_WITH_KNOTS('',3,(#88563,#88564,#88565,#88566,#88567,
#88568,#88569,#88570,#88571,#88572,#88573,#88574,#88575,#88576,#88577,#88578,
#88579,#88580,#88581,#88582,#88583,#88584,#88585,#88586,#88587,#88588,#88589,
#88590,#88591,#88592,#88593,#88594,#88595,#88596,#88597,#88598,#88599,#88600,
#88601,#88602,#88603,#88604,#88605,#88606,#88607,#88608,#88609,#88610,#88611,
#88612,#88613,#88614,#88615,#88616,#88617,#88618,#88619,#88620,#88621,#88622,
#88623,#88624,#88625,#88626,#88627,#88628,#88629,#88630,#88631,#88632,#88633,
#88634,#88635,#88636,#88637,#88638,#88639,#88640,#88641,#88642,#88643,#88644,
#88645,#88646,#88647,#88648,#88649,#88650,#88651,#88652,#88653,#88654,#88655,
#88656,#88657,#88658,#88659,#88660,#88661,#88662,#88663,#88664,#88665,#88666),
 .UNSPECIFIED.,.F.,.F.,(4,1,1,1,1,1,1,1,1,1,1,1,1,1,1,1,1,1,1,1,1,1,1,1,
1,1,1,1,1,1,1,1,1,1,1,1,1,1,1,1,1,1,1,1,1,1,1,1,1,1,1,1,1,1,1,1,1,1,1,1,
1,1,1,1,1,1,1,1,1,1,1,1,1,1,1,1,1,1,1,1,1,1,1,1,1,1,1,1,1,1,1,1,1,1,1,1,
1,1,1,1,1,4),(32.7489697872148,33.0588984658616,33.4937717726112,33.928645079224,
34.3635183857014,34.7983916920448,35.2332649982556,35.6681383043353,36.1030116102854,
36.5378849161076,36.9727582218035,37.4076315273749,37.8425048328235,38.2782308323341,
38.7139568318446,39.1488301370532,39.5837034421446,40.0185767471208,40.4534500519838,
40.8883233567357,41.3231966613787,41.7580699659148,42.1929432703463,42.6278165746754,
43.0626898789044,43.4975631830356,43.9324364870714,44.3673097910142,44.8021830948664,
45.2379090935952,45.673635092324,46.1085083960024,46.5433816995978,46.9782550031127,
47.4131283065497,47.8480016099115,48.2828749132006,48.7177482164198,49.1526215195718,
49.5874948226593,50.0223681256851,50.457241428652,50.8921147315628,51.3269880344203,
51.7618613372274,52.197587335454,52.6333133336805,53.0681866363954,53.5030599390685,
53.9379332417027,54.3728065443011,54.8076798468664,55.2425531494018,55.6774264519101,
56.1122997543943,56.5471730568575,56.9820463593026,57.4169196617326,57.8517929641506,
58.2866662665595,58.7215395689624,59.157265567009,59.5929915650557,60.0278648674556,
60.4627381698584,60.8976114722673,61.3324847746853,61.7673580771153,62.2022313795604,
62.6371046820236,63.0719779845079,63.5068512870162,63.9417245895516,64.376597892117,
64.8114711947155,65.2463444973499,65.6812178000231,66.1169437982275,66.5526697964318,
66.9875430991915,67.4224164019987,67.8572897048563,68.2921630077673,68.7270363107343,
69.1619096137603,69.5967829168479,70.0316562200001,70.4665295232194,70.9014028265087,
71.3362761298705,71.7711494333077,72.2060227368227,72.6408960404182,73.0766220391044,
73.5123480377905,73.9472213415547,74.382094645407,74.8169679493499,75.2518412533859,
75.6867145575172,76.1215878617464,76.5237606401499),.UNSPECIFIED.) ;
#3388 = B_SPLINE_CURVE_WITH_KNOTS('',3,(#88667,#88668,#88669,#88670,#88671,
#88672,#88673,#88674,#88675,#88676),.UNSPECIFIED.,.F.,.F.,(4,2,2,2,4),(-0.0826694635875258,
-0.0593216231105862,-0.0376236853894878,-0.0193344026424728,0.),
 .UNSPECIFIED.) ;
#3389 = B_SPLINE_CURVE_WITH_KNOTS('',3,(#95648,#95649,#95650,#95651,#95652,
#95653,#95654,#95655,#95656,#95657),.UNSPECIFIED.,.F.,.F.,(4,2,2,2,4),(1.00000014359794E-6,
0.0360372518640473,0.0809925104139904,0.121401369748062,0.142937500220573),
 .UNSPECIFIED.) ;
#3390 = B_SPLINE_CURVE_WITH_KNOTS('',3,(#95658,#95659,#95660,#95661,#95662,
#95663,#95664,#95665,#95666,#95667,#95668,#95669,#95670,#95671,#95672,#95673,
#95674,#95675,#95676,#95677,#95678,#95679,#95680,#95681,#95682,#95683,#95684,
#95685,#95686,#95687,#95688,#95689,#95690,#95691,#95692,#95693,#95694,#95695,
#95696,#95697),.UNSPECIFIED.,.F.,.F.,(4,2,2,2,2,2,2,2,2,2,2,2,2,2,2,2,2,
2,2,4),(0.142937500220573,0.212621082019458,0.320815840090966,0.375504796790274,
0.430559656121251,0.485436696366515,0.542481778298955,0.598023802517587,
0.655309402277618,0.713243686022327,0.770798519845424,0.886328666912018,
0.944969358407582,1.06329674263614,1.1820699816098,1.24254840068009,1.30316653563122,
1.40054089198694,1.44934143852683,1.49830020415347),.UNSPECIFIED.) ;
#3391 = B_SPLINE_CURVE_WITH_KNOTS('',3,(#95745,#95746,#95747,#95748,#95749,
#95750,#95751,#95752,#95753,#95754,#95755,#95756,#95757,#95758,#95759,#95760,
#95761,#95762,#95763,#95764,#95765,#95766,#95767,#95768,#95769,#95770,#95771,
#95772,#95773,#95774,#95775,#95776,#95777,#95778,#95779,#95780,#95781,#95782,
#95783,#95784,#95785,#95786,#95787,#95788,#95789,#95790,#95791,#95792,#95793,
#95794,#95795,#95796,#95797,#95798,#95799,#95800,#95801,#95802,#95803,#95804,
#95805,#95806,#95807,#95808,#95809,#95810,#95811,#95812,#95813,#95814,#95815,
#95816,#95817,#95818,#95819,#95820,#95821,#95822,#95823,#95824,#95825,#95826,
#95827,#95828,#95829,#95830,#95831,#95832,#95833,#95834,#95835,#95836,#95837,
#95838,#95839,#95840,#95841,#95842,#95843,#95844,#95845,#95846,#95847,#95848,
#95849,#95850,#95851,#95852,#95853,#95854,#95855,#95856,#95857,#95858,#95859,
#95860,#95861,#95862,#95863,#95864,#95865,#95866,#95867,#95868,#95869,#95870,
#95871,#95872,#95873,#95874,#95875,#95876,#95877,#95878,#95879,#95880,#95881,
#95882,#95883,#95884,#95885,#95886,#95887,#95888,#95889,#95890,#95891,#95892,
#95893,#95894,#95895,#95896,#95897,#95898,#95899,#95900,#95901,#95902,#95903,
#95904,#95905,#95906,#95907,#95908,#95909,#95910,#95911,#95912),
 .UNSPECIFIED.,.F.,.F.,(4,2,2,2,2,2,2,2,2,2,2,2,2,2,2,2,2,2,2,2,2,2,2,2,
2,2,2,2,2,2,2,2,2,2,2,2,2,2,2,2,2,2,2,2,2,2,2,2,2,2,2,2,2,2,2,2,2,2,2,2,
2,2,2,2,2,2,2,2,2,2,2,2,2,2,2,2,2,2,2,2,2,2,2,4),(-0.220764104088801,-0.212810871540256,
-0.210826700499309,-0.209271377624256,-0.207761433718714,-0.205730133021802,
-0.198550410701793,-0.194693947563819,-0.191844768703672,-0.190288611310355,
-0.188362409929451,-0.184999676746538,-0.180416560353273,-0.177999628317623,
-0.176979986395151,-0.17545950163188,-0.169329901049086,-0.167326065798206,
-0.165010161095794,-0.163313713247872,-0.161023224140324,-0.153727427111349,
-0.149942839167921,-0.147940423218799,-0.146174539582342,-0.14492474623107,
-0.143254607113532,-0.139977390203118,-0.132761315345017,-0.129907194789166,
-0.127727771034509,-0.127695231772659,-0.127662289268986,-0.127628712263654,
-0.127594244771433,-0.127558596416708,-0.127521430120194,-0.127482345157773,
-0.125819013512314,-0.123790189778761,-0.118018986881696,-0.1152572462372,
-0.113532453832035,-0.112659157946268,-0.111622343809751,-0.110439450510491,
-0.105393494629594,-0.101142713766881,-0.0984836529757749,-0.0959423346846566,
-0.0924670239912303,-0.0856704502143524,-0.0830826409091052,-0.0810670398022107,
-0.0801905425616422,-0.0800237613922501,-0.0798508625343385,-0.0797151851007466,
-0.0796106899901649,-0.076519201508656,-0.0724898690735813,-0.0649233561618741,
-0.0628333544112901,-0.0625221368031416,-0.0613894493125142,-0.059221190827661,
-0.0578457520775916,-0.0536661754919154,-0.0503751719819521,-0.0488118303618613,
-0.0471863738239208,-0.0401191604475317,-0.0366930787710805,-0.0347854870478141,
-0.0327365310897468,-0.0288818358416986,-0.0233041138937386,-0.0196358217432888,
-0.0180786709312759,-0.0169397258617589,-0.0158280003179945,-0.0145205316222842,
-0.0125999707568532,-1.00000005423539E-6),.UNSPECIFIED.) ;
#3392 = B_SPLINE_CURVE_WITH_KNOTS('',3,(#95915,#95916,#95917,#95918,#95919,
#95920,#95921,#95922,#95923,#95924,#95925,#95926,#95927,#95928,#95929,#95930,
#95931,#95932,#95933,#95934,#95935,#95936,#95937,#95938,#95939,#95940,#95941,
#95942,#95943,#95944,#95945,#95946,#95947,#95948,#95949,#95950,#95951,#95952,
#95953,#95954,#95955,#95956,#95957,#95958,#95959,#95960,#95961,#95962,#95963,
#95964,#95965,#95966,#95967,#95968,#95969,#95970,#95971,#95972,#95973,#95974,
#95975,#95976,#95977,#95978,#95979,#95980,#95981,#95982,#95983,#95984,#95985,
#95986,#95987,#95988,#95989,#95990,#95991,#95992,#95993,#95994,#95995,#95996,
#95997,#95998,#95999,#96000,#96001,#96002,#96003,#96004,#96005,#96006,#96007,
#96008,#96009,#96010,#96011,#96012,#96013,#96014,#96015,#96016,#96017,#96018,
#96019,#96020,#96021,#96022,#96023,#96024,#96025,#96026,#96027,#96028,#96029,
#96030,#96031,#96032,#96033,#96034,#96035,#96036,#96037,#96038,#96039,#96040,
#96041,#96042,#96043,#96044,#96045,#96046,#96047,#96048,#96049,#96050,#96051,
#96052,#96053,#96054,#96055,#96056),.UNSPECIFIED.,.F.,.F.,(4,2,2,2,2,2,
2,2,2,2,2,2,2,2,2,2,2,2,2,2,2,2,2,2,2,2,2,2,2,2,2,2,2,2,2,2,2,2,2,2,2,2,
2,2,2,2,2,2,2,2,2,2,2,2,2,2,2,2,2,2,2,2,2,2,2,2,2,2,2,2,4),(-0.182524757410581,
-0.179400079255036,-0.17525270474638,-0.169924742343938,-0.168066541634283,
-0.166743122146313,-0.165501109476116,-0.164280363050201,-0.162567518341145,
-0.153584802508503,-0.149881816094398,-0.148075130957187,-0.147659345332695,
-0.14747558772853,-0.147253816704885,-0.147096090311417,-0.146984513812829,
-0.146905552966418,-0.146333086860246,-0.145369022341424,-0.144415011400128,
-0.142823368855438,-0.136928629403607,-0.132413914356333,-0.129285947625111,
-0.12763586093638,-0.126515487506062,-0.125561663743937,-0.124579832163949,
-0.123247751364027,-0.12033219120056,-0.114069651365153,-0.111104420647958,
-0.108953832387937,-0.106802817047256,-0.104459571378279,-0.0976458616205787,
-0.0940738831557366,-0.091340443134881,-0.0885028776720636,-0.0798366453627358,
-0.0769226537360381,-0.0743796492721717,-0.0720421640080332,-0.0689755681899533,
-0.0630996419380829,-0.0613131012176197,-0.0599974514768906,-0.0595480235572075,
-0.0594019674709208,-0.0592683763169184,-0.0591333251994762,-0.0589867854536884,
-0.0588186847538835,-0.0586168251107207,-0.0583652073408724,-0.0566822399868792,
-0.053854635167259,-0.0440464066436818,-0.0419163630190737,-0.0403248470153975,
-0.0387643876558876,-0.0368436468873608,-0.0336193240872738,-0.0258753093766691,
-0.0229828526112447,-0.0202624147686418,-0.0102148475350557,-0.0082430981455107,
-0.00659087887404097,-6.19471594258285E-6),.UNSPECIFIED.) ;
#3393 = B_SPLINE_CURVE_WITH_KNOTS('',3,(#96061,#96062,#96063,#96064,#96065,
#96066,#96067,#96068,#96069,#96070,#96071,#96072,#96073,#96074,#96075,#96076,
#96077,#96078,#96079,#96080,#96081,#96082,#96083,#96084,#96085,#96086,#96087,
#96088,#96089,#96090,#96091,#96092,#96093,#96094,#96095,#96096,#96097,#96098,
#96099,#96100,#96101,#96102,#96103,#96104,#96105,#96106,#96107,#96108,#96109,
#96110,#96111,#96112,#96113,#96114,#96115,#96116,#96117,#96118,#96119,#96120,
#96121,#96122,#96123,#96124,#96125,#96126,#96127,#96128,#96129,#96130,#96131,
#96132,#96133,#96134,#96135,#96136,#96137,#96138,#96139,#96140,#96141,#96142,
#96143,#96144,#96145,#96146,#96147,#96148,#96149,#96150,#96151,#96152,#96153,
#96154,#96155,#96156,#96157,#96158,#96159,#96160,#96161,#96162,#96163,#96164,
#96165,#96166,#96167,#96168,#96169,#96170,#96171,#96172,#96173,#96174,#96175,
#96176,#96177,#96178,#96179,#96180,#96181,#96182,#96183,#96184,#96185,#96186,
#96187,#96188,#96189,#96190,#96191,#96192,#96193,#96194,#96195,#96196,#96197,
#96198,#96199,#96200,#96201,#96202,#96203,#96204,#96205,#96206,#96207,#96208,
#96209,#96210,#96211,#96212,#96213,#96214,#96215,#96216,#96217,#96218,#96219,
#96220,#96221,#96222,#96223,#96224,#96225,#96226,#96227,#96228,#96229,#96230,
#96231,#96232,#96233,#96234,#96235,#96236,#96237,#96238,#96239,#96240,#96241,
#96242,#96243,#96244,#96245,#96246,#96247,#96248,#96249,#96250,#96251,#96252,
#96253,#96254,#96255,#96256,#96257,#96258,#96259,#96260,#96261,#96262,#96263,
#96264,#96265,#96266,#96267,#96268,#96269,#96270,#96271,#96272,#96273,#96274,
#96275,#96276,#96277,#96278,#96279,#96280),.UNSPECIFIED.,.F.,.F.,(4,3,3,
3,3,3,3,3,3,3,3,3,3,3,3,3,3,3,3,3,3,3,3,3,3,3,3,3,3,3,3,3,3,3,3,3,3,3,3,
3,3,3,3,3,3,3,3,3,3,3,3,3,3,3,3,3,3,3,3,3,3,3,3,3,3,3,3,3,3,3,3,3,3,4),
(0.,0.114554107952647,0.219999579637262,0.4079808305004,0.571675274172504,
0.925887608273928,1.24364764879026,1.27682344199313,1.56513289539198,1.63103573085445,
1.92276380563199,1.98481039669498,2.30553261811763,2.33719940646081,2.68985168871465,
2.85597213219783,3.02278753371137,3.04298755913573,3.13367446983363,3.18807481875432,
3.30095372042153,3.39425414698803,3.57785099270941,3.7486975888156,4.10139086880436,
4.41302871222335,4.45537183311384,4.74928777621505,4.80732327925073,5.0983924343693,
5.16153555014084,5.47412129432572,5.51418781350788,5.86492791526386,6.04203405015412,
6.21914018504438,6.31436263900473,6.37615253991527,6.4855726106983,6.57181603734208,
6.75160383615881,6.92446829765038,7.27760414977274,7.59380314037911,7.6294205837199,
7.91857835912354,7.98363285125545,8.27582882631628,8.33593536794668,8.66001538389398,
8.6877517844213,9.04173195324679,9.21866661258249,9.39560127191819,9.49526269149952,
9.56422015730585,9.66918811922683,9.74731942042791,9.92430999212726,10.1013005638266,
10.4534629350241,10.7676564343577,10.8062607636447,11.0976054309952,11.1594970582837,
11.4541859605988,11.5115370732495,11.8216297040439,11.8657493811883,12.2168162078705,
12.3939223660536,12.5710285242368,12.6749025971536,12.7522862024852),
 .UNSPECIFIED.) ;
#3394 = B_SPLINE_CURVE_WITH_KNOTS('',3,(#96281,#96282,#96283,#96284,#96285,
#96286,#96287,#96288,#96289,#96290,#96291,#96292,#96293,#96294,#96295,#96296,
#96297,#96298,#96299,#96300,#96301,#96302,#96303,#96304,#96305,#96306,#96307,
#96308,#96309,#96310,#96311,#96312,#96313,#96314,#96315,#96316,#96317,#96318,
#96319,#96320,#96321,#96322,#96323,#96324,#96325,#96326,#96327,#96328,#96329,
#96330,#96331,#96332,#96333,#96334,#96335,#96336,#96337,#96338,#96339,#96340,
#96341,#96342,#96343,#96344,#96345,#96346,#96347,#96348,#96349,#96350,#96351,
#96352,#96353,#96354,#96355,#96356,#96357,#96358,#96359,#96360,#96361,#96362,
#96363,#96364,#96365,#96366,#96367,#96368,#96369,#96370,#96371,#96372,#96373,
#96374,#96375,#96376,#96377,#96378,#96379,#96380,#96381,#96382,#96383,#96384,
#96385,#96386,#96387,#96388,#96389,#96390,#96391,#96392,#96393,#96394,#96395,
#96396,#96397,#96398,#96399,#96400,#96401,#96402,#96403,#96404,#96405,#96406,
#96407,#96408,#96409,#96410,#96411,#96412,#96413,#96414,#96415,#96416,#96417,
#96418,#96419,#96420,#96421,#96422,#96423,#96424,#96425,#96426,#96427,#96428,
#96429,#96430,#96431,#96432,#96433,#96434,#96435,#96436,#96437,#96438,#96439,
#96440,#96441,#96442,#96443,#96444,#96445,#96446,#96447,#96448,#96449,#96450,
#96451,#96452,#96453,#96454,#96455,#96456,#96457,#96458,#96459,#96460,#96461,
#96462,#96463,#96464,#96465,#96466,#96467,#96468,#96469,#96470,#96471,#96472,
#96473,#96474,#96475,#96476,#96477,#96478,#96479,#96480,#96481,#96482,#96483,
#96484,#96485,#96486,#96487,#96488,#96489,#96490,#96491,#96492,#96493,#96494,
#96495,#96496,#96497,#96498,#96499,#96500,#96501,#96502,#96503,#96504,#96505,
#96506,#96507,#96508,#96509,#96510,#96511,#96512,#96513,#96514,#96515,#96516,
#96517,#96518,#96519,#96520,#96521,#96522,#96523,#96524,#96525,#96526,#96527,
#96528,#96529,#96530,#96531,#96532,#96533,#96534,#96535,#96536,#96537,#96538,
#96539,#96540,#96541,#96542,#96543,#96544,#96545,#96546,#96547,#96548,#96549,
#96550,#96551,#96552,#96553,#96554,#96555,#96556,#96557,#96558,#96559,#96560,
#96561,#96562,#96563,#96564,#96565,#96566,#96567,#96568,#96569,#96570,#96571,
#96572,#96573,#96574,#96575,#96576,#96577,#96578,#96579,#96580,#96581,#96582,
#96583,#96584,#96585,#96586,#96587,#96588,#96589,#96590,#96591,#96592,#96593,
#96594,#96595,#96596,#96597,#96598,#96599,#96600,#96601,#96602,#96603,#96604,
#96605,#96606,#96607,#96608,#96609,#96610,#96611,#96612,#96613,#96614,#96615,
#96616,#96617,#96618,#96619,#96620,#96621,#96622,#96623,#96624,#96625,#96626,
#96627,#96628,#96629,#96630,#96631,#96632,#96633,#96634,#96635,#96636,#96637,
#96638,#96639,#96640,#96641,#96642,#96643,#96644,#96645,#96646,#96647,#96648,
#96649,#96650,#96651,#96652,#96653,#96654,#96655,#96656,#96657,#96658,#96659,
#96660,#96661,#96662,#96663,#96664,#96665,#96666,#96667,#96668,#96669,#96670,
#96671,#96672,#96673,#96674,#96675,#96676,#96677,#96678,#96679,#96680,#96681,
#96682,#96683,#96684,#96685,#96686,#96687,#96688,#96689,#96690,#96691,#96692,
#96693,#96694,#96695,#96696,#96697,#96698,#96699,#96700,#96701,#96702,#96703,
#96704,#96705,#96706,#96707,#96708,#96709,#96710,#96711,#96712,#96713,#96714,
#96715,#96716,#96717,#96718,#96719,#96720,#96721,#96722,#96723,#96724,#96725,
#96726,#96727,#96728,#96729,#96730,#96731,#96732,#96733,#96734,#96735,#96736,
#96737,#96738,#96739,#96740,#96741,#96742,#96743,#96744,#96745,#96746,#96747,
#96748,#96749,#96750,#96751,#96752,#96753,#96754,#96755,#96756,#96757,#96758,
#96759,#96760,#96761,#96762,#96763,#96764,#96765,#96766,#96767,#96768,#96769,
#96770,#96771,#96772,#96773,#96774,#96775,#96776,#96777,#96778,#96779,#96780,
#96781,#96782,#96783,#96784,#96785,#96786,#96787,#96788,#96789,#96790,#96791,
#96792,#96793,#96794,#96795,#96796,#96797,#96798,#96799,#96800,#96801,#96802,
#96803,#96804,#96805,#96806,#96807,#96808,#96809,#96810,#96811,#96812,#96813,
#96814,#96815,#96816,#96817,#96818,#96819,#96820,#96821,#96822,#96823,#96824,
#96825,#96826,#96827,#96828,#96829,#96830,#96831,#96832,#96833,#96834,#96835,
#96836,#96837,#96838,#96839,#96840,#96841,#96842,#96843,#96844,#96845,#96846,
#96847,#96848,#96849,#96850,#96851,#96852,#96853,#96854,#96855,#96856,#96857,
#96858,#96859,#96860,#96861,#96862,#96863,#96864,#96865,#96866,#96867,#96868,
#96869,#96870,#96871,#96872,#96873,#96874,#96875,#96876,#96877,#96878,#96879,
#96880,#96881,#96882,#96883,#96884,#96885,#96886,#96887,#96888,#96889,#96890,
#96891,#96892,#96893,#96894,#96895,#96896,#96897,#96898,#96899,#96900,#96901,
#96902,#96903,#96904,#96905,#96906,#96907,#96908,#96909,#96910,#96911,#96912,
#96913,#96914,#96915,#96916,#96917,#96918,#96919,#96920,#96921,#96922,#96923,
#96924,#96925,#96926,#96927,#96928,#96929,#96930,#96931,#96932,#96933,#96934,
#96935,#96936,#96937,#96938,#96939,#96940,#96941,#96942,#96943,#96944,#96945,
#96946,#96947,#96948,#96949,#96950,#96951,#96952,#96953,#96954,#96955,#96956,
#96957,#96958,#96959,#96960,#96961,#96962,#96963,#96964,#96965,#96966,#96967,
#96968,#96969,#96970,#96971,#96972,#96973,#96974,#96975,#96976,#96977,#96978,
#96979,#96980,#96981,#96982,#96983,#96984,#96985,#96986,#96987,#96988,#96989,
#96990,#96991,#96992,#96993,#96994,#96995,#96996,#96997,#96998,#96999,#97000,
#97001,#97002,#97003,#97004,#97005,#97006,#97007,#97008,#97009,#97010,#97011,
#97012,#97013,#97014,#97015,#97016,#97017,#97018,#97019,#97020,#97021,#97022,
#97023,#97024,#97025,#97026,#97027,#97028,#97029,#97030,#97031,#97032,#97033,
#97034,#97035,#97036,#97037,#97038,#97039,#97040,#97041,#97042,#97043,#97044,
#97045,#97046,#97047,#97048,#97049,#97050,#97051,#97052,#97053,#97054,#97055,
#97056,#97057,#97058,#97059,#97060,#97061,#97062,#97063,#97064,#97065,#97066,
#97067,#97068,#97069,#97070,#97071,#97072,#97073,#97074,#97075,#97076,#97077,
#97078,#97079,#97080,#97081,#97082,#97083,#97084,#97085,#97086,#97087,#97088,
#97089,#97090,#97091,#97092,#97093,#97094,#97095,#97096,#97097,#97098,#97099,
#97100,#97101,#97102,#97103,#97104,#97105,#97106,#97107,#97108,#97109,#97110,
#97111,#97112,#97113,#97114,#97115,#97116,#97117,#97118,#97119,#97120,#97121,
#97122,#97123,#97124,#97125,#97126,#97127,#97128,#97129,#97130,#97131,#97132,
#97133,#97134,#97135,#97136,#97137,#97138,#97139,#97140,#97141,#97142,#97143,
#97144,#97145,#97146,#97147,#97148,#97149,#97150,#97151,#97152,#97153,#97154,
#97155,#97156,#97157,#97158,#97159,#97160,#97161,#97162,#97163,#97164,#97165,
#97166,#97167,#97168,#97169,#97170,#97171,#97172,#97173,#97174,#97175,#97176,
#97177,#97178,#97179,#97180,#97181,#97182,#97183,#97184,#97185,#97186,#97187,
#97188,#97189,#97190,#97191,#97192,#97193,#97194,#97195,#97196,#97197,#97198,
#97199,#97200,#97201,#97202,#97203,#97204,#97205,#97206,#97207,#97208,#97209,
#97210,#97211,#97212,#97213,#97214,#97215,#97216,#97217,#97218,#97219,#97220,
#97221,#97222,#97223,#97224,#97225,#97226,#97227,#97228),.UNSPECIFIED.,
 .F.,.F.,(4,2,2,2,2,2,2,2,2,2,2,2,2,2,2,2,2,2,2,2,2,2,2,2,2,2,2,2,2,2,2,
2,2,2,2,2,2,2,2,2,2,2,2,2,2,2,2,2,2,2,2,2,2,2,2,2,2,2,2,2,2,2,2,2,2,2,2,
2,2,2,2,2,2,2,2,2,2,2,2,2,2,2,2,2,2,2,2,2,2,2,2,2,2,2,2,2,2,2,2,2,2,2,2,
2,2,2,2,2,2,2,2,2,2,2,2,2,2,2,2,2,2,2,2,2,2,2,2,2,2,2,2,2,2,2,2,2,2,2,2,
2,2,2,2,2,2,2,2,2,2,2,2,2,2,2,2,2,2,2,2,2,2,2,2,2,2,2,2,2,2,2,2,2,2,2,2,
2,2,2,2,2,2,2,2,2,2,2,2,2,2,2,2,2,2,2,2,2,2,2,2,2,2,2,2,2,2,2,2,2,2,2,2,
2,2,2,2,2,2,2,2,2,2,2,2,2,2,2,2,2,2,2,2,2,2,2,2,2,2,2,2,2,2,2,2,2,2,2,2,
2,2,2,2,2,2,2,2,2,2,2,2,2,2,2,2,2,2,2,2,2,2,2,2,2,2,2,2,2,2,2,2,2,2,2,2,
2,2,2,2,2,2,2,2,2,2,2,2,2,2,2,2,2,2,2,2,2,2,2,2,2,2,2,2,2,2,2,2,2,2,2,2,
2,2,2,2,2,2,2,2,2,2,2,2,2,2,2,2,2,2,2,2,2,2,2,2,2,2,2,2,2,2,2,2,2,2,2,2,
2,2,2,2,2,2,2,2,2,2,2,2,2,2,2,2,2,2,2,2,2,2,2,2,2,2,2,2,2,2,2,2,2,2,2,2,
2,2,2,2,2,2,2,2,2,2,2,2,2,2,2,2,2,2,2,2,2,2,2,2,2,2,2,2,2,2,2,2,2,2,2,2,
2,2,2,2,2,2,2,2,2,2,2,2,2,2,2,2,2,2,2,2,2,2,2,2,2,2,2,2,2,2,2,2,2,2,2,2,
2,2,2,2,2,2,2,2,2,2,4),(-0.764247471210668,-0.751743679523728,-0.749787349302028,
-0.748466170573943,-0.747353015576898,-0.746229888194009,-0.744705969654846,
-0.742042801572738,-0.735573867456227,-0.731599035226706,-0.729551225755541,
-0.727628551825557,-0.72429307565926,-0.71691825405121,-0.715319963117154,
-0.713752158702681,-0.708608552525963,-0.705537770035867,-0.703123628174905,
-0.701819340008528,-0.701457150876899,-0.699382833803033,-0.691744773922614,
-0.687727540938138,-0.684642066677351,-0.684536110788994,-0.684398664752154,
-0.68422368892437,-0.682267085929049,-0.679934930491743,-0.671990741585058,
-0.668436862044888,-0.665881117247485,-0.663217257250133,-0.659198808613844,
-0.652685204615345,-0.652533914973734,-0.65245118241893,-0.652302449152326,
-0.650842523847057,-0.648882336431947,-0.643460694478169,-0.64177287762435,
-0.639812161874024,-0.639732274774989,-0.639651729787625,-0.639569911247981,
-0.639486132208486,-0.638734001454006,-0.637077613810066,-0.634878942084535,
-0.627305526955079,-0.623486976014171,-0.621469617402936,-0.619690631731014,
-0.619675203404641,-0.619659397167634,-0.619643206678388,-0.619626625429433,
-0.619609647081108,-0.619592265438801,-0.619580360610218,-0.619567134202823,
-0.619552452451201,-0.619536170878834,-0.619518134345827,-0.619498176802242,
-0.619476121371885,-0.619451780953779,-0.619424958790796,-0.619395449422112,
-0.619363039920797,-0.619339594194662,-0.619303081702113,-0.617893108950745,
-0.615986126825558,-0.607568520154958,-0.605265027516251,-0.602031053370959,
-0.600933167430379,-0.600899078332022,-0.600864107171565,-0.600685194201412,
-0.600643494517834,-0.600618863935554,-0.60058963465784,-0.600554752212184,
-0.60051283765328,-0.600055981038067,-0.599755508282305,-0.597758365505696,
-0.593453273343866,-0.58837845402993,-0.587432039779253,-0.587421662489367,
-0.587410744853701,-0.587399259284741,-0.58738717681477,-0.587374467033305,
-0.587361098224912,-0.587347036777663,-0.58733224805926,-0.587315700780545,
-0.587294738679146,-0.58604872530786,-0.583570527120193,-0.578806017610902,
-0.575951442215166,-0.575917240039466,-0.57588284902638,-0.575848211361223,
-0.575813266743046,-0.575777951589565,-0.575742198696271,-0.575705936497424,
-0.575669088408267,-0.57563157188355,-0.575593297525791,-0.575554167891789,
-0.57551407621428,-0.575472904825173,-0.575430523338962,-0.575386786293546,
-0.575341530464242,-0.575314804902926,-0.575282441596471,-0.575242886292903,
-0.575193971047836,-0.575132559298258,-0.573617922583152,-0.571473185681082,
-0.56666188804757,-0.561213174936975,-0.557976488337323,-0.556248940259786,
-0.556234303419732,-0.55621901057048,-0.556203037864369,-0.556186360864792,
-0.556168954990762,-0.556150795432733,-0.556131857164985,-0.556112114829003,
-0.556093762689975,-0.556071807037008,-0.556045611582623,-0.555146889562833,
-0.553249080234159,-0.545543142497903,-0.542277133625629,-0.539549071161527,
-0.539527961353536,-0.539506410590843,-0.539484393166028,-0.537478254791286,
-0.534396939859279,-0.528389792761219,-0.525975385171115,-0.525950334205306,
-0.525919886593823,-0.525882858483798,-0.525818434103449,-0.524768379556028,
-0.523498792503296,-0.519527060031304,-0.51451371647883,-0.512990411388448,
-0.512985571119614,-0.51298073940741,-0.512975916047397,-0.512971100723961,
-0.512966293278019,-0.51296149320922,-0.512956700126011,-0.512951913903677,
-0.511533686684132,-0.51074103694245,-0.509075698376633,-0.505578465657056,
-0.498985700758375,-0.495984052245982,-0.49431865305602,-0.49347474134022,
-0.492447925254705,-0.492444741841439,-0.492441529986487,-0.492438289763827,
-0.492435021143763,-0.492431723884107,-0.492428397667622,-0.492425042141419,
-0.492421657251981,-0.492418243145725,-0.492414799298318,-0.492411325675055,
-0.492407822183086,-0.492404288454517,-0.492400724400314,-0.49239712971674,
-0.492393504309571,-0.492389847865722,-0.492386160569218,-0.492382441900127,
-0.492378691584599,-0.49237490968904,-0.492371096173412,-0.492367250332756,
-0.491212100946225,-0.489658668231368,-0.48579386383809,-0.479247024011673,
-0.476541896056154,-0.474240991892955,-0.473496884918386,-0.473492032853011,
-0.473487171877076,-0.473482301681109,-0.473477422598824,-0.472531671634839,
-0.470819598033998,-0.467496550271221,-0.462891280246222,-0.460594804555694,
-0.459579150359858,-0.459572594336455,-0.459565739815589,-0.459558575888467,
-0.459551091681993,-0.459543276259237,-0.459535118497733,-0.459526607327517,
-0.459517731602073,-0.459504728118507,-0.45948935708003,-0.459459911773783,
-0.457898811626963,-0.454146636974715,-0.44879963365633,-0.448782583811241,
-0.448765565490588,-0.448748572187319,-0.448731597359594,-0.448714634442148,
-0.448697676866893,-0.448680718021248,-0.44866375125925,-0.448646769824788,
-0.448629766958303,-0.448612735772892,-0.448595669336493,-0.448578560584644,
-0.448561402330495,-0.44854418730869,-0.448526908057938,-0.44850955695485,
-0.448492126230268,-0.448474607909694,-0.448456993824479,-0.448439275580402,
-0.448421444480109,-0.448403491668086,-0.448385407921326,-0.448367183739672,
-0.44834880927186,-0.448330274319018,-0.448311568261963,-0.448292680100457,
-0.448273598359855,-0.448254311073561,-0.448234805752344,-0.448215069359952,
-0.448195088218958,-0.448174847977606,-0.446498823840117,-0.444209675105915,
-0.440096269981153,-0.438612670832745,-0.433471678410112,-0.43105242545973,
-0.429081315189868,-0.427604986575227,-0.425942948455691,-0.422783439228443,
-0.414686064488075,-0.410544955223904,-0.408685120304353,-0.408680349430051,
-0.408675563585301,-0.408670762642213,-0.408665946448391,-0.408661114778539,
-0.408656267551759,-0.408651404514737,-0.408646525472597,-0.407180031046102,
-0.405160847915497,-0.398885138529577,-0.394827184160689,-0.391157229748051,
-0.387782172196992,-0.382119133251819,-0.371538992080939,-0.366674974245237,
-0.359492910150279,-0.356777429108173,-0.35469669248993,-0.352539612414606,
-0.346580265699802,-0.344141192861172,-0.342601973036691,-0.341195159870061,
-0.341185080766306,-0.341179279227765,-0.341173371117081,-0.341167354069549,
-0.341161225915604,-0.341154984427779,-0.341148627126594,-0.341142151588876,
-0.341135555270567,-0.341128835670544,-0.341121990175109,-0.341115016042629,
-0.341107910569127,-0.341100670812776,-0.34109329398637,-0.339488553499683,
-0.337100964130616,-0.331943480773202,-0.325973543825826,-0.3242649653731,
-0.323327136344219,-0.321983662699549,-0.320591621861973,-0.318681119126004,
-0.315127904949632,-0.30733571251182,-0.30502535251208,-0.303264954718732,
-0.301373168516209,-0.301330539132518,-0.298659107685882,-0.292153707163327,
-0.291167913599698,-0.290027782255832,-0.288548550475036,-0.28699609204701,
-0.280112499969877,-0.27810737232618,-0.276309322148879,-0.276270890762943,
-0.274217775393644,-0.27099881481407,-0.262322295726513,-0.26026993325124,
-0.259118191666412,-0.257531498350647,-0.255622309972626,-0.252492003430452,
-0.244299738980638,-0.241664490080971,-0.239328621772058,-0.239270801643195,
-0.239209267816936,-0.239142667100564,-0.239069398875907,-0.238987504118802,
-0.238894521700588,-0.238787295383387,-0.23866170859767,-0.238512313680558,
-0.238331805657696,-0.238110260907096,-0.237834000563045,-0.237730468280656,
-0.237537621407133,-0.237173459105306,-0.232786366078886,-0.229150918687028,
-0.227767912571321,-0.226477389477959,-0.221465127450128,-0.217366883738891,
-0.215227634545174,-0.213304274802974,-0.213220060681828,-0.213129818468827,
-0.210837382962062,-0.206830485926529,-0.206050186928971,-0.205848356940494,
-0.205558812609167,-0.199735382837687,-0.197168390117335,-0.194942299789501,
-0.192518372131756,-0.188519286600698,-0.182665514369018,-0.179430930361463,
-0.1759487406926,-0.167493640840597,-0.165422929828438,-0.163016914317639,
-0.159282584895954,-0.154570625643645,-0.152751981500879,-0.151249069802613,
-0.15121886468106,-0.151188329092347,-0.151157425891687,-0.151126118404242,
-0.151094370205691,-0.149639146972516,-0.147699964868839,-0.144332394789749,
-0.138049392543586,-0.134219702370753,-0.132635022309593,-0.131621746604662,
-0.130511202200971,-0.129274850574216,-0.127539473416974,-0.124480181543592,
-0.115529958994556,-0.112874792302332,-0.1118274726451,-0.110975117635325,
-0.110185271538753,-0.110181023981887,-0.110176712096691,-0.10911714467567,
-0.107808154915339,-0.105454165490774,-0.0990506249196755,-0.092819106367308,
-0.0912922977547633,-0.0904278445491569,-0.0895633488178997,-0.0886960865164723,
-0.0875709520751671,-0.0857663825379889,-0.0819690399160495,-0.0723457760579113,
-0.0706861327542463,-0.069790593161694,-0.0688988824995555,-0.0682206244844478,
-0.0681980213041179,-0.0681745958247813,-0.0681503130202285,-0.0681251364468912,
-0.0680990281743692,-0.0680904012106424,-0.0680808133760211,-0.0680701573783576,
-0.068058313900782,-0.0680451504167606,-0.0680305197492798,-0.0680142584983207,
-0.0661033948947557,-0.0635460144550783,-0.0543011430140782,-0.0514707434372014,
-0.0498660191763955,-0.048524465054405,-0.0468977105032776,-0.0447503169441138,
-0.0408288456754641,-0.0327801722920067,-0.0296337577175016,-0.0264024832468529,
-0.0139286036663535,-0.00444927623081447,-1.00000001590494E-6),
 .UNSPECIFIED.) ;
#3395 = B_SPLINE_CURVE_WITH_KNOTS('',3,(#97233,#97234,#97235,#97236,#97237,
#97238,#97239,#97240,#97241,#97242,#97243,#97244,#97245,#97246,#97247,#97248,
#97249,#97250,#97251,#97252,#97253,#97254,#97255,#97256,#97257,#97258,#97259,
#97260,#97261,#97262,#97263,#97264,#97265,#97266,#97267,#97268,#97269,#97270,
#97271,#97272,#97273,#97274,#97275,#97276,#97277,#97278,#97279,#97280,#97281,
#97282,#97283,#97284,#97285,#97286,#97287,#97288,#97289,#97290,#97291,#97292,
#97293,#97294,#97295,#97296,#97297,#97298,#97299,#97300,#97301,#97302,#97303,
#97304,#97305,#97306,#97307,#97308,#97309,#97310,#97311,#97312,#97313,#97314,
#97315,#97316,#97317,#97318,#97319,#97320,#97321,#97322,#97323,#97324,#97325,
#97326,#97327,#97328,#97329,#97330,#97331,#97332,#97333,#97334,#97335,#97336,
#97337,#97338,#97339,#97340,#97341,#97342,#97343,#97344,#97345,#97346,#97347,
#97348,#97349,#97350,#97351,#97352,#97353,#97354,#97355,#97356,#97357,#97358,
#97359,#97360,#97361,#97362,#97363,#97364,#97365,#97366,#97367,#97368,#97369,
#97370,#97371,#97372,#97373,#97374,#97375,#97376,#97377,#97378,#97379,#97380,
#97381,#97382,#97383,#97384,#97385,#97386,#97387,#97388,#97389,#97390,#97391,
#97392,#97393,#97394,#97395,#97396,#97397,#97398,#97399,#97400,#97401,#97402,
#97403,#97404,#97405,#97406,#97407,#97408,#97409,#97410,#97411,#97412,#97413,
#97414,#97415,#97416,#97417,#97418,#97419,#97420,#97421,#97422,#97423,#97424,
#97425,#97426,#97427,#97428,#97429,#97430,#97431,#97432,#97433,#97434,#97435,
#97436,#97437,#97438,#97439,#97440,#97441,#97442,#97443,#97444,#97445,#97446,
#97447,#97448,#97449,#97450,#97451,#97452,#97453,#97454,#97455),
 .UNSPECIFIED.,.F.,.F.,(4,3,3,3,3,3,3,3,3,3,3,3,3,3,3,3,3,3,3,3,3,3,3,3,
3,3,3,3,3,3,3,3,3,3,3,3,3,3,3,3,3,3,3,3,3,3,3,3,3,3,3,3,3,3,3,3,3,3,3,3,
3,3,3,3,3,3,3,3,3,3,3,3,3,3,4),(0.,0.100762857826657,0.17045455738185,0.347415762439074,
0.524376967496299,0.877381484509634,1.19821800652288,1.22826049812016,1.51697376328212,
1.58247279915011,1.87779658021693,1.93391776317192,2.25164505567423,2.28836068050304,
2.64280331320604,2.82167316119952,2.99350875161294,3.10266796923987,3.18807250430072,
3.28423663368536,3.34738831255791,3.5233640520366,3.69933979151529,4.05355206803615,
4.37985223748112,4.40620435589301,4.70171242541753,4.75694454204997,5.0460196545254,
5.11115683439866,5.42764767484474,5.46361882765795,5.81783110946781,6.00081498008586,
6.16978259404898,6.28286071807447,6.37613838180102,6.46714712814611,6.52211297837991,
6.68925611334469,6.8557017444244,6.87524886950579,7.22706540888955,7.54278024414005,
7.58104611352649,7.87520812139574,7.93428224769233,8.22349039670314,8.28872622840582,
8.59531361187982,8.64114684774855,8.99188712842038,9.18026879928553,9.34609939086034,
9.46276931651287,9.56422046408461,9.6509138473967,9.69916314071276,9.86319775131968,
10.0264998248963,10.0499034623499,10.4041157271119,10.7307046868919,10.7583279856935,
11.0558356759029,11.1095696963186,11.3979727180224,11.4637819917093,11.7745585768636,
11.8159445691956,12.1687425517332,12.3621786336201,12.5198069536285,12.6375810196581,
12.7523053453688),.UNSPECIFIED.) ;
#3396 = B_SPLINE_CURVE_WITH_KNOTS('',3,(#97456,#97457,#97458,#97459,#97460,
#97461,#97462,#97463,#97464,#97465,#97466,#97467,#97468,#97469,#97470,#97471,
#97472,#97473,#97474,#97475,#97476,#97477,#97478,#97479,#97480,#97481,#97482,
#97483,#97484,#97485,#97486,#97487,#97488,#97489,#97490,#97491,#97492,#97493,
#97494,#97495,#97496,#97497,#97498,#97499,#97500,#97501,#97502,#97503,#97504,
#97505,#97506,#97507,#97508,#97509,#97510,#97511,#97512,#97513,#97514,#97515,
#97516,#97517,#97518,#97519,#97520,#97521,#97522,#97523,#97524,#97525,#97526,
#97527,#97528,#97529,#97530,#97531,#97532,#97533,#97534,#97535,#97536,#97537,
#97538,#97539,#97540,#97541,#97542,#97543,#97544,#97545,#97546,#97547,#97548,
#97549,#97550,#97551,#97552,#97553,#97554,#97555,#97556,#97557,#97558,#97559,
#97560,#97561,#97562,#97563,#97564,#97565,#97566,#97567,#97568,#97569,#97570,
#97571,#97572,#97573,#97574,#97575,#97576,#97577,#97578,#97579,#97580,#97581,
#97582,#97583,#97584,#97585,#97586,#97587,#97588,#97589,#97590,#97591,#97592,
#97593,#97594,#97595,#97596,#97597,#97598,#97599,#97600,#97601,#97602,#97603,
#97604,#97605,#97606,#97607,#97608,#97609,#97610,#97611,#97612,#97613,#97614,
#97615,#97616,#97617,#97618,#97619,#97620,#97621,#97622,#97623,#97624,#97625,
#97626,#97627,#97628,#97629,#97630,#97631,#97632,#97633,#97634,#97635,#97636,
#97637,#97638,#97639,#97640,#97641,#97642,#97643,#97644,#97645,#97646,#97647,
#97648,#97649,#97650,#97651,#97652,#97653,#97654,#97655,#97656,#97657,#97658,
#97659,#97660,#97661,#97662,#97663,#97664,#97665,#97666,#97667,#97668,#97669,
#97670,#97671,#97672,#97673,#97674,#97675),.UNSPECIFIED.,.F.,.F.,(4,3,3,
3,3,3,3,3,3,3,3,3,3,3,3,3,3,3,3,3,3,3,3,3,3,3,3,3,3,3,3,3,3,3,3,3,3,3,3,
3,3,3,3,3,3,3,3,3,3,3,3,3,3,3,3,3,3,3,3,3,3,3,3,3,3,3,3,3,3,3,3,3,3,4),
(4.62398695583928E-14,0.103893003809472,0.181262498396716,0.358368655155245,
0.535474811913774,0.886541640300103,1.19673532348575,1.24075395493171,1.53528792411631,
1.59279396171985,1.88431414392228,1.94603026773208,2.25997509562812,2.29882808755841,
2.65099046906085,2.82798104483141,3.00497162060198,3.10991086391406,3.18806738078836,
3.28775562074052,3.35668976127941,3.5336244263954,3.71055909151139,4.06453925695613,
4.38847961221436,4.41635566929646,4.70870697420658,4.76865819735123,5.05774592416949,
5.12287046168214,5.43899161303812,5.47468689392592,5.82782275374672,6.0076103693676,
6.18047500641398,6.28988375072323,6.37613695915723,6.4713735827459,6.53315086103547,
6.71025699441627,6.88736312779706,7.23810322232236,7.55101366329053,7.59075550121641,
7.88163753032148,7.94496776270377,8.238967474758,8.29691921461726,8.60855780950479,
8.65090019138673,9.00359345967117,9.18722179851689,9.35803689449882,9.47088359281198,
9.56421233698863,9.65492998924665,9.70930349363768,9.87612791713392,10.0422522333702,
10.0624393716107,10.4150916485022,10.7357912646172,10.7674806581858,11.0593569652202,
11.1212553350823,11.4093863989005,11.4754676140256,11.793370958421,11.826403454723,
12.180615789613,12.3685389651718,12.5322914820512,12.6468674178297,12.7522978599647),
 .UNSPECIFIED.) ;
#3397 = B_SPLINE_CURVE_WITH_KNOTS('',3,(#97680,#97681,#97682,#97683,#97684,
#97685,#97686,#97687,#97688,#97689,#97690,#97691,#97692,#97693,#97694,#97695,
#97696,#97697,#97698,#97699,#97700,#97701,#97702,#97703,#97704,#97705,#97706,
#97707,#97708,#97709,#97710,#97711,#97712,#97713,#97714,#97715,#97716,#97717,
#97718,#97719,#97720,#97721,#97722,#97723,#97724,#97725,#97726,#97727,#97728,
#97729,#97730,#97731,#97732,#97733,#97734,#97735,#97736,#97737,#97738,#97739,
#97740,#97741,#97742,#97743,#97744,#97745,#97746,#97747,#97748,#97749,#97750,
#97751,#97752,#97753,#97754,#97755,#97756,#97757,#97758,#97759,#97760,#97761,
#97762,#97763,#97764,#97765,#97766,#97767,#97768,#97769,#97770,#97771,#97772,
#97773,#97774,#97775,#97776,#97777,#97778,#97779,#97780,#97781,#97782,#97783,
#97784,#97785,#97786,#97787,#97788,#97789,#97790,#97791,#97792,#97793,#97794,
#97795,#97796,#97797,#97798,#97799,#97800,#97801,#97802,#97803,#97804,#97805,
#97806,#97807,#97808,#97809,#97810,#97811,#97812,#97813,#97814,#97815,#97816,
#97817,#97818,#97819,#97820,#97821,#97822,#97823,#97824,#97825,#97826,#97827,
#97828,#97829,#97830,#97831,#97832,#97833,#97834,#97835,#97836,#97837,#97838,
#97839,#97840,#97841,#97842,#97843,#97844,#97845,#97846,#97847,#97848,#97849,
#97850,#97851,#97852,#97853,#97854,#97855,#97856,#97857,#97858,#97859,#97860,
#97861,#97862,#97863,#97864,#97865,#97866,#97867,#97868,#97869,#97870,#97871,
#97872,#97873,#97874,#97875,#97876,#97877,#97878,#97879,#97880,#97881,#97882,
#97883,#97884,#97885,#97886,#97887,#97888,#97889,#97890,#97891,#97892,#97893,
#97894,#97895,#97896,#97897,#97898,#97899,#97900,#97901,#97902,#97903,#97904,
#97905,#97906,#97907,#97908),.UNSPECIFIED.,.F.,.F.,(4,3,3,3,3,3,3,3,3,3,
3,3,3,3,3,3,3,3,3,3,3,3,3,3,3,3,3,3,3,3,3,3,3,3,3,3,3,3,3,3,3,3,3,3,3,3,
3,3,3,3,3,3,3,3,3,3,3,3,3,3,3,3,3,3,3,3,3,3,3,3,3,3,3,3,3,3,4),(0.,0.0849567058129364,
0.121410866737072,0.283571067641385,0.444919421036448,0.475392252089173,
0.827665187221835,1.14808607612973,1.18210927518942,1.47839116596226,1.53459228457289,
1.82885507160546,1.88547168452342,2.19314502784146,2.23968397375804,2.59214615040927,
2.79038879486884,2.94635842870424,3.06998802803508,3.18810817019483,3.26440590431514,
3.29802675005529,3.45757822076301,3.61627514247155,3.65067925900212,4.00489154138233,
4.35563223002435,4.64617975588607,4.70984452935805,5.00046832575526,5.06284926268752,
5.36685554187163,5.41550181494416,5.76624256865231,5.97273593786742,6.1202225757179,
6.24822644256217,6.37623030940644,6.44733815583888,6.47439716292745,6.63221404230216,
6.78911562828793,6.82800759658552,7.18091231497168,7.51065136471811,7.53272928162441,
7.82487629707621,7.88694158774125,8.18083977411295,8.23818376656191,8.5428108298148,
8.59239607694621,8.94455897340147,9.15752823700876,9.2973571803608,9.4308647738549,
9.564372367349,9.62916114633207,9.64818402988998,9.80361159264046,9.95805838375772,
10.002396297147,10.3566085447957,10.5648455268525,10.7090424934517,10.9238830828388,
11.1385418510563,11.3532131814724,11.4174022576871,11.6640729394265,11.7698515234467,
12.1227348772726,12.3436966068389,12.4771776993501,12.6049451701722,12.7335676446457,
12.7552103037919),.UNSPECIFIED.) ;
#3398 = B_SPLINE_CURVE_WITH_KNOTS('',3,(#97909,#97910,#97911,#97912,#97913,
#97914,#97915,#97916,#97917,#97918,#97919,#97920,#97921,#97922,#97923,#97924,
#97925,#97926,#97927,#97928,#97929,#97930,#97931,#97932,#97933,#97934,#97935,
#97936,#97937,#97938,#97939,#97940,#97941,#97942,#97943,#97944,#97945,#97946,
#97947,#97948,#97949,#97950,#97951,#97952,#97953,#97954,#97955,#97956,#97957,
#97958,#97959,#97960,#97961,#97962,#97963,#97964,#97965,#97966,#97967,#97968,
#97969,#97970,#97971,#97972,#97973,#97974,#97975,#97976,#97977,#97978,#97979,
#97980,#97981,#97982,#97983,#97984,#97985,#97986,#97987,#97988,#97989,#97990,
#97991,#97992,#97993,#97994,#97995,#97996,#97997,#97998,#97999,#98000,#98001,
#98002,#98003,#98004,#98005,#98006,#98007,#98008,#98009,#98010,#98011,#98012,
#98013,#98014,#98015,#98016,#98017,#98018,#98019,#98020,#98021,#98022,#98023,
#98024,#98025,#98026,#98027,#98028,#98029,#98030,#98031,#98032,#98033,#98034,
#98035,#98036,#98037,#98038,#98039,#98040,#98041,#98042,#98043,#98044,#98045,
#98046,#98047,#98048,#98049,#98050,#98051,#98052,#98053,#98054,#98055,#98056,
#98057,#98058,#98059,#98060,#98061,#98062,#98063,#98064,#98065,#98066,#98067,
#98068,#98069,#98070,#98071,#98072,#98073,#98074,#98075,#98076,#98077,#98078,
#98079,#98080,#98081,#98082,#98083,#98084,#98085,#98086,#98087,#98088,#98089,
#98090,#98091,#98092,#98093,#98094,#98095,#98096,#98097,#98098,#98099,#98100,
#98101,#98102,#98103,#98104,#98105,#98106,#98107,#98108,#98109,#98110,#98111,
#98112,#98113,#98114,#98115,#98116,#98117,#98118,#98119,#98120,#98121,#98122,
#98123,#98124,#98125,#98126,#98127,#98128,#98129,#98130,#98131),
 .UNSPECIFIED.,.F.,.F.,(4,3,3,3,3,3,3,3,3,3,3,3,3,3,3,3,3,3,3,3,3,3,3,3,
3,3,3,3,3,3,3,3,3,3,3,3,3,3,3,3,3,3,3,3,3,3,3,3,3,3,3,3,3,3,3,3,3,3,3,3,
3,3,3,3,3,3,3,3,3,3,3,3,3,3,4),(0.,0.117766852478915,0.232496353538427,
0.425959269809284,0.58356076372737,0.936358747455187,1.24721516302964,1.28852133052573,
1.57691037402851,1.64273362456121,1.94009683856461,1.99397533075514,2.32101174159414,
2.34818760451099,2.70239985630971,2.86567318626527,3.02967152715568,3.05314018006163,
3.13984623840255,3.18808443459044,3.30474613545452,3.40620393305099,3.59458496913247,
3.76041618591283,4.11115646630507,4.4179620031698,4.46357709690046,4.752645686315,
4.81802107035101,5.11225950859455,5.17125721849527,5.48698227134387,5.525237914481,
5.87705445117265,6.04348549182109,6.21060943622386,6.23019035170545,6.32120249042075,
6.37616561501542,6.48923709384672,6.58252073706138,6.7655212470504,6.93447223265948,
7.2886845102342,7.60525585810603,7.64114650722471,7.93025277521067,7.99535880099052,
8.29066722848746,8.34609897805127,8.67287428692262,8.69875128326739,9.05296354724675,
9.22893929137685,9.40491503550695,9.50113431130136,9.56423800268766,9.67334187672609,
9.75879459828048,9.93770082835262,10.109500019499,10.4639426784075,10.7812408319156,
10.8183855714955,11.1138898609681,11.1698305545815,11.4585507849166,11.5240428555817,
11.8445810390535,11.8749218597236,12.2279263926025,12.4048875910266,12.5818487894507,
12.6825950545208,12.7522985291244),.UNSPECIFIED.) ;
#3399 = B_SPLINE_CURVE_WITH_KNOTS('',3,(#98134,#98135,#98136,#98137,#98138,
#98139,#98140,#98141,#98142,#98143,#98144,#98145,#98146,#98147,#98148,#98149,
#98150,#98151,#98152,#98153,#98154,#98155,#98156,#98157,#98158,#98159,#98160,
#98161,#98162,#98163,#98164,#98165,#98166,#98167,#98168,#98169,#98170,#98171,
#98172,#98173,#98174,#98175,#98176,#98177,#98178,#98179,#98180,#98181,#98182,
#98183,#98184,#98185,#98186,#98187,#98188,#98189,#98190,#98191,#98192,#98193,
#98194,#98195,#98196,#98197,#98198,#98199,#98200,#98201,#98202,#98203,#98204,
#98205,#98206,#98207,#98208,#98209,#98210,#98211,#98212,#98213,#98214,#98215,
#98216,#98217,#98218,#98219,#98220,#98221,#98222,#98223,#98224,#98225,#98226,
#98227,#98228,#98229,#98230,#98231,#98232,#98233,#98234,#98235,#98236,#98237,
#98238,#98239,#98240,#98241,#98242,#98243,#98244,#98245,#98246,#98247,#98248,
#98249,#98250,#98251,#98252,#98253,#98254,#98255,#98256,#98257,#98258,#98259,
#98260,#98261,#98262,#98263,#98264,#98265,#98266,#98267,#98268,#98269,#98270,
#98271,#98272,#98273,#98274,#98275,#98276,#98277,#98278,#98279,#98280,#98281,
#98282,#98283,#98284,#98285,#98286,#98287,#98288,#98289,#98290,#98291,#98292,
#98293,#98294,#98295,#98296,#98297,#98298,#98299,#98300,#98301,#98302,#98303,
#98304,#98305,#98306,#98307,#98308,#98309,#98310,#98311,#98312,#98313,#98314,
#98315,#98316,#98317,#98318,#98319,#98320,#98321,#98322,#98323,#98324,#98325,
#98326,#98327,#98328,#98329,#98330,#98331,#98332,#98333,#98334,#98335,#98336,
#98337,#98338,#98339,#98340,#98341,#98342,#98343,#98344,#98345,#98346,#98347,
#98348,#98349,#98350,#98351,#98352,#98353,#98354,#98355,#98356,#98357,#98358,
#98359,#98360,#98361,#98362,#98363,#98364,#98365,#98366,#98367,#98368,#98369,
#98370,#98371,#98372,#98373,#98374,#98375,#98376,#98377,#98378,#98379,#98380,
#98381,#98382,#98383,#98384,#98385,#98386,#98387,#98388,#98389,#98390,#98391,
#98392,#98393,#98394,#98395,#98396,#98397,#98398,#98399,#98400,#98401,#98402,
#98403,#98404,#98405,#98406,#98407,#98408,#98409,#98410,#98411,#98412,#98413,
#98414,#98415,#98416,#98417,#98418,#98419,#98420,#98421,#98422,#98423,#98424,
#98425,#98426,#98427,#98428,#98429,#98430,#98431),.UNSPECIFIED.,.F.,.F.,
(4,2,2,2,2,2,2,2,2,2,2,2,2,2,2,2,2,2,2,2,2,2,2,2,2,2,2,2,2,2,2,2,2,2,2,
2,2,2,2,2,2,2,2,2,2,2,2,2,2,2,2,2,2,2,2,2,2,2,2,2,2,2,2,2,2,2,2,2,2,2,2,
2,2,2,2,2,2,2,2,2,2,2,2,2,2,2,2,2,2,2,2,2,2,2,2,2,2,2,2,2,2,2,2,2,2,2,2,
2,2,2,2,2,2,2,2,2,2,2,2,2,2,2,2,2,2,2,2,2,2,2,2,2,2,2,2,2,2,2,2,2,2,2,2,
2,2,2,2,2,4),(-0.257900755467309,-0.253216416734724,-0.252081122878548,
-0.251188581376995,-0.250268481007479,-0.249199690087404,-0.247321831903525,
-0.238759204638973,-0.234724908277334,-0.232196441579018,-0.232107868071063,
-0.232033864423124,-0.231970645036362,-0.231915500222983,-0.231866441938075,
-0.231821971305206,-0.231780923271327,-0.231742359395631,-0.231705490559752,
-0.231669618083719,-0.231634084187505,-0.230661352058559,-0.229670878231674,
-0.228329990486118,-0.225435956904153,-0.219436946684503,-0.215922353082132,
-0.213955428346512,-0.211671398913192,-0.211300806108947,-0.210802084382286,
-0.210073377562204,-0.209187777716023,-0.202338212115815,-0.199074975538359,
-0.196677987276589,-0.192676403012342,-0.188341647230444,-0.185311815741795,
-0.183066011781248,-0.180465475451871,-0.172249686430586,-0.169229539589126,
-0.166970991294384,-0.165720781707934,-0.164552078584456,-0.163000469703303,
-0.159452196243217,-0.151302616749568,-0.14843595058748,-0.146765560197486,
-0.145290446824941,-0.144421868974387,-0.143262601739533,-0.141672739536235,
-0.136954148649398,-0.1346340325145,-0.129065871038034,-0.125869065902798,
-0.124659076889791,-0.123667899831835,-0.122712937555569,-0.122706886177565,
-0.122700800497667,-0.122694679405855,-0.122688521605658,-0.122682326092311,
-0.122676091686211,-0.122669816895747,-0.122663500605786,-0.122657141585206,
-0.122650738405059,-0.122644289727925,-0.122637794294871,-0.122631250811736,
-0.122624657919335,-0.122618014052854,-0.122611317871009,-0.12260456775595,
-0.122597762378302,-0.122590900399232,-0.122583979898203,-0.122576999612479,
-0.122569957810855,-0.122562852868749,-0.122555683037884,-0.122548446726371,
-0.12254114229378,-0.122533767854874,-0.122526321434637,-0.122518801293772,
-0.122511205564072,-0.122503532259167,-0.122495779555185,-0.122487945279876,
-0.122480027554225,-0.122472024212396,-0.122463932904575,-0.122455751548302,
-0.122447477743975,-0.122439109319996,-0.122430643883141,-0.122422079074529,
-0.122413412433196,-0.121283087484751,-0.11955758875476,-0.116062867522551,
-0.10707420165302,-0.105202140685433,-0.103854487337308,-0.102970526980149,
-0.102907177979866,-0.102857423888435,-0.101281613267831,-0.0993316709483247,
-0.0956795830241013,-0.0888309635444944,-0.086137074043605,-0.0859955526366021,
-0.0832106401463704,-0.0773048160284202,-0.0731571835682499,-0.0730096300108956,
-0.0728620769714977,-0.0727002880618865,-0.0725018376578106,-0.0721447273630533,
-0.0707043405651774,-0.0691077748749713,-0.0654638461792568,-0.0610602370306744,
-0.0589586516625534,-0.0572180695927868,-0.056718927282375,-0.0545935016922846,
-0.0477781731658085,-0.0424783825520563,-0.0401182717033047,-0.0381028155134184,
-0.0355564509498019,-0.0321730274769302,-0.0238920357109913,-0.0211071463371678,
-0.018141251387123,-0.0145766051973008,-0.00910418335533362,-0.00751977848971695,
-0.0061993296316266,-1.00000002145606E-6),.UNSPECIFIED.) ;
#3400 = B_SPLINE_CURVE_WITH_KNOTS('',3,(#98434,#98435,#98436,#98437,#98438,
#98439,#98440,#98441,#98442,#98443,#98444,#98445,#98446,#98447,#98448,#98449,
#98450,#98451,#98452,#98453,#98454,#98455,#98456,#98457,#98458,#98459,#98460,
#98461,#98462,#98463,#98464,#98465,#98466,#98467,#98468,#98469,#98470,#98471,
#98472,#98473,#98474,#98475,#98476,#98477,#98478,#98479,#98480,#98481,#98482,
#98483,#98484,#98485,#98486,#98487,#98488,#98489,#98490,#98491,#98492,#98493,
#98494,#98495,#98496,#98497,#98498,#98499,#98500,#98501,#98502,#98503,#98504,
#98505,#98506,#98507,#98508,#98509,#98510,#98511,#98512,#98513,#98514,#98515,
#98516,#98517,#98518,#98519,#98520,#98521,#98522,#98523,#98524,#98525,#98526,
#98527,#98528,#98529,#98530,#98531,#98532,#98533,#98534,#98535,#98536,#98537,
#98538,#98539,#98540,#98541,#98542,#98543,#98544,#98545,#98546,#98547,#98548,
#98549,#98550,#98551,#98552,#98553,#98554,#98555,#98556,#98557,#98558,#98559,
#98560,#98561,#98562,#98563,#98564,#98565,#98566,#98567,#98568,#98569,#98570,
#98571,#98572,#98573,#98574,#98575,#98576,#98577,#98578,#98579,#98580,#98581,
#98582,#98583,#98584,#98585,#98586,#98587,#98588,#98589,#98590,#98591,#98592,
#98593,#98594,#98595,#98596,#98597,#98598,#98599,#98600,#98601,#98602,#98603,
#98604,#98605,#98606,#98607,#98608,#98609,#98610,#98611,#98612,#98613,#98614,
#98615,#98616,#98617,#98618,#98619,#98620,#98621,#98622,#98623,#98624,#98625,
#98626,#98627,#98628,#98629,#98630,#98631,#98632,#98633,#98634,#98635,#98636,
#98637,#98638,#98639,#98640,#98641,#98642,#98643,#98644,#98645,#98646,#98647,
#98648,#98649,#98650,#98651,#98652,#98653,#98654,#98655),.UNSPECIFIED.,
 .F.,.F.,(4,2,2,2,2,2,2,2,2,2,2,2,2,2,2,2,2,2,2,2,2,2,2,2,2,2,2,2,2,2,2,
2,2,2,2,2,2,2,2,2,2,2,2,2,2,2,2,2,2,2,2,2,2,2,2,2,2,2,2,2,2,2,2,2,2,2,2,
2,2,2,2,2,2,2,2,2,2,2,2,2,2,2,2,2,2,2,2,2,2,2,2,2,2,2,2,2,2,2,2,2,2,2,2,
2,2,2,2,2,2,2,4),(-0.219746869275165,-0.209394220478331,-0.207753239526596,
-0.206649108783921,-0.205722501184274,-0.204794843451096,-0.203555739165895,
-0.200894311177838,-0.198921158679466,-0.192588578659282,-0.188021143583113,
-0.186092785062327,-0.185276448909895,-0.183321587913198,-0.180721553559358,
-0.173767470654067,-0.167939033501986,-0.166365809517859,-0.163837166237039,
-0.163751776767129,-0.163601872210293,-0.16333609984235,-0.163198358840147,
-0.162183429560188,-0.160484216404485,-0.158438737394277,-0.15227047994801,
-0.144118005044246,-0.140891167696757,-0.138945836080856,-0.138863610757223,
-0.138784297455775,-0.13870749893918,-0.138632844736102,-0.138559985944405,
-0.138488590311582,-0.138418337492401,-0.138348914283941,-0.138280009818965,
-0.138211310482883,-0.138142494364349,-0.138073225083726,-0.138003144624901,
-0.136574115420871,-0.135030386981507,-0.133174412630518,-0.127354206019301,
-0.118311839564707,-0.114833601418337,-0.112062898284409,-0.111005122078999,
-0.110976082918538,-0.110945769834806,-0.110914126133238,-0.110881092843895,
-0.110846608552085,-0.110827734526394,-0.110804545330814,-0.110776083625737,
-0.110741194601781,-0.110698493158317,-0.110646329764849,-0.110582757773965,
-0.110521519984715,-0.110345945926127,-0.109869683740985,-0.108311782090756,
-0.108278681034145,-0.108245204934098,-0.108211318224594,-0.108176984518539,
-0.108142166467452,-0.108106825649253,-0.108070922435533,-0.108034415899468,
-0.107997263682651,-0.107959421830159,-0.107920844662558,-0.107881484651252,
-0.10784129228663,-0.107800215827085,-0.107758201241631,-0.107715191988349,
-0.104792568503729,-0.100834666872008,-0.0917717551230505,-0.0882811143143876,
-0.0867437352941089,-0.0853447730347683,-0.083827236203204,-0.0790014302681088,
-0.069201462111199,-0.0663858373919709,-0.062017901694425,-0.0533676094137269,
-0.0502667414139253,-0.0473137908608287,-0.0441142595304958,-0.037298863082803,
-0.0353544289087413,-0.0341090641924219,-0.0338990145187595,-0.0325276327465331,
-0.030618814017994,-0.0274711235000813,-0.0176209626715808,-0.015588847484666,
-0.0140793900248419,-0.0126085540006478,-0.0108360299783269,-5.22571551622377E-5),
 .UNSPECIFIED.) ;
#3401 = B_SPLINE_CURVE_WITH_KNOTS('',3,(#98664,#98665,#98666,#98667,#98668,
#98669,#98670,#98671,#98672,#98673,#98674,#98675,#98676,#98677,#98678,#98679,
#98680,#98681,#98682,#98683,#98684,#98685,#98686,#98687,#98688,#98689),
 .UNSPECIFIED.,.F.,.F.,(4,2,2,2,2,2,2,2,2,2,2,2,4),(9.99999999408653E-7,
0.0217536568113104,0.0435354891950078,0.0879397153249219,0.112564023696129,
0.137318935332534,0.162458662654022,0.187567234819067,0.213124132494857,
0.23869596408236,0.264191632957491,0.290419557870604,0.311836241869575),
 .UNSPECIFIED.) ;
#3402 = B_SPLINE_CURVE_WITH_KNOTS('',3,(#98691,#98692,#98693,#98694,#98695,
#98696,#98697,#98698),.UNSPECIFIED.,.F.,.F.,(4,2,2,4),(0.,0.032825880706413,
0.0479820964229119,0.0625119124755425),.UNSPECIFIED.) ;
#3403 = B_SPLINE_CURVE_WITH_KNOTS('',3,(#98699,#98700,#98701,#98702,#98703,
#98704,#98705,#98706,#98707,#98708,#98709,#98710,#98711,#98712,#98713,#98714,
#98715,#98716,#98717,#98718,#98719,#98720,#98721,#98722,#98723,#98724,#98725,
#98726,#98727,#98728,#98729,#98730,#98731,#98732),.UNSPECIFIED.,.F.,.F.,
(4,2,2,2,2,2,2,2,2,2,2,2,2,2,2,2,4),(0.311836241869575,0.316507424624442,
0.342892888010537,0.369492419894292,0.396264677447541,0.409779859620928,
0.436779117209232,0.464022317106864,0.491926865771247,0.519205487052424,
0.547669956809039,0.575175692034606,0.603824409336178,0.632256986806205,
0.68973297899141,0.718666448874189,0.74772595748679),.UNSPECIFIED.) ;
#3404 = B_SPLINE_CURVE_WITH_KNOTS('',3,(#105704,#105705,#105706,#105707,#105708,
#105709,#105710,#105711,#105712,#105713,#105714,#105715,#105716,#105717,
#105718,#105719,#105720,#105721,#105722,#105723,#105724,#105725,#105726,
#105727,#105728,#105729,#105730,#105731,#105732,#105733,#105734,#105735,
#105736,#105737,#105738,#105739,#105740,#105741,#105742,#105743,#105744,
#105745,#105746,#105747,#105748,#105749,#105750,#105751,#105752,#105753,
#105754,#105755,#105756,#105757,#105758,#105759,#105760,#105761,#105762,
#105763,#105764,#105765,#105766,#105767,#105768,#105769,#105770,#105771,
#105772,#105773,#105774,#105775,#105776,#105777,#105778,#105779,#105780,
#105781,#105782,#105783,#105784,#105785,#105786,#105787,#105788,#105789,
#105790,#105791,#105792,#105793,#105794,#105795,#105796,#105797,#105798,
#105799,#105800,#105801,#105802,#105803,#105804,#105805,#105806,#105807),
 .UNSPECIFIED.,.F.,.F.,(4,1,1,1,1,1,1,1,1,1,1,1,1,1,1,1,1,1,1,1,1,1,1,1,
1,1,1,1,1,1,1,1,1,1,1,1,1,1,1,1,1,1,1,1,1,1,1,1,1,1,1,1,1,1,1,1,1,1,1,1,
1,1,1,1,1,1,1,1,1,1,1,1,1,1,1,1,1,1,1,1,1,1,1,1,1,1,1,1,1,1,1,1,1,1,1,1,
1,1,1,1,1,4),(32.7489697872148,33.0588984658616,33.4937717726112,33.928645079224,
34.3635183857014,34.7983916920448,35.2332649982556,35.6681383043353,36.1030116102854,
36.5378849161076,36.9727582218035,37.4076315273749,37.8425048328235,38.2782308323341,
38.7139568318446,39.1488301370532,39.5837034421446,40.0185767471208,40.4534500519838,
40.8883233567357,41.3231966613787,41.7580699659148,42.1929432703463,42.6278165746754,
43.0626898789044,43.4975631830356,43.9324364870714,44.3673097910142,44.8021830948664,
45.2379090935952,45.673635092324,46.1085083960024,46.5433816995978,46.9782550031127,
47.4131283065497,47.8480016099115,48.2828749132006,48.7177482164198,49.1526215195718,
49.5874948226593,50.0223681256851,50.457241428652,50.8921147315628,51.3269880344203,
51.7618613372274,52.197587335454,52.6333133336805,53.0681866363954,53.5030599390685,
53.9379332417027,54.3728065443011,54.8076798468664,55.2425531494018,55.6774264519101,
56.1122997543943,56.5471730568575,56.9820463593026,57.4169196617326,57.8517929641506,
58.2866662665595,58.7215395689624,59.157265567009,59.5929915650557,60.0278648674556,
60.4627381698584,60.8976114722673,61.3324847746853,61.7673580771153,62.2022313795604,
62.6371046820236,63.0719779845079,63.5068512870162,63.9417245895516,64.376597892117,
64.8114711947155,65.2463444973499,65.6812178000231,66.1169437982275,66.5526697964318,
66.9875430991915,67.4224164019987,67.8572897048563,68.2921630077673,68.7270363107343,
69.1619096137603,69.5967829168479,70.0316562200001,70.4665295232194,70.9014028265087,
71.3362761298705,71.7711494333077,72.2060227368227,72.6408960404182,73.0766220391044,
73.5123480377905,73.9472213415547,74.382094645407,74.8169679493499,75.2518412533859,
75.6867145575172,76.1215878617464,76.5237606401499),.UNSPECIFIED.) ;
#3405 = B_SPLINE_CURVE_WITH_KNOTS('',3,(#105808,#105809,#105810,#105811,#105812,
#105813,#105814,#105815,#105816,#105817),.UNSPECIFIED.,.F.,.F.,(4,2,2,2,
4),(-0.0826694635853999,-0.0593216231081083,-0.0376236853870205,-0.0193344026412378,
0.),.UNSPECIFIED.) ;
#3406 = B_SPLINE_CURVE_WITH_KNOTS('',3,(#112789,#112790,#112791,#112792,#112793,
#112794,#112795,#112796,#112797,#112798),.UNSPECIFIED.,.F.,.F.,(4,2,2,2,
4),(1.00000014634402E-6,0.0360372518616826,0.080992510409305,0.121401369744557,
0.142937500227851),.UNSPECIFIED.) ;
#3407 = B_SPLINE_CURVE_WITH_KNOTS('',3,(#112799,#112800,#112801,#112802,#112803,
#112804,#112805,#112806,#112807,#112808,#112809,#112810,#112811,#112812,
#112813,#112814,#112815,#112816,#112817,#112818,#112819,#112820,#112821,
#112822,#112823,#112824,#112825,#112826,#112827,#112828,#112829,#112830,
#112831,#112832,#112833,#112834,#112835,#112836,#112837,#112838),
 .UNSPECIFIED.,.F.,.F.,(4,2,2,2,2,2,2,2,2,2,2,2,2,2,2,2,2,2,2,4),(0.142937500227851,
0.212621082022179,0.320815840109222,0.37550479681675,0.43055965615564,0.485436696409689,
0.542481778350213,0.598023802577391,0.655309402346842,0.713243686100983,
0.770798519932069,0.886328667015345,0.944969358519958,1.06329674276424,
1.18206998175586,1.24254840083446,1.30316653579448,1.4005408921717,1.44934143872188,
1.49830020435886),.UNSPECIFIED.) ;
#3408 = B_SPLINE_CURVE_WITH_KNOTS('',3,(#112934,#112935,#112936,#112937,#112938,
#112939,#112940,#112941,#112942,#112943,#112944,#112945,#112946,#112947,
#112948,#112949,#112950,#112951,#112952),.UNSPECIFIED.,.T.,.F.,(4,1,1,1,
1,1,1,1,1,1,1,1,1,1,1,1,4),(0.,2.69519445779221,5.61545499238393,8.53571552697323,
11.2309099847624,13.9261044425515,16.8463649771433,19.7666255117326,22.4618199695218,
25.1570144273109,28.0772749619002,30.9975354964919,33.6927299542811,36.3879244120703,
39.3081849466596,42.2284454812513,44.9236399390405),.UNSPECIFIED.) ;
#3409 = B_SPLINE_CURVE_WITH_KNOTS('',3,(#112955,#112956,#112957,#112958,#112959,
#112960,#112961,#112962,#112963,#112964,#112965),.UNSPECIFIED.,.F.,.F.,
(4,1,1,1,1,1,1,1,4),(0.,1.04064620349252,2.08129240698504,3.12193860703556,
4.16258480708607,5.2032310071414,6.24387720719673,7.28452341068926,8.32516961418179),
 .UNSPECIFIED.) ;
#3410 = B_SPLINE_CURVE_WITH_KNOTS('',3,(#112969,#112970,#112971,#112972,#112973,
#112974,#112975,#112976,#112977,#112978,#112979),.UNSPECIFIED.,.F.,.F.,
(4,1,1,1,1,1,1,1,4),(0.,1.04062614942685,2.0812522988537,3.12187844827608,
4.16250459769846,5.20313074711661,6.24375689653477,7.28438304596783,8.32500919540089),
 .UNSPECIFIED.) ;
#3411 = B_SPLINE_CURVE_WITH_KNOTS('',3,(#112985,#112986,#112987,#112988,#112989,
#112990,#112991,#112992,#112993,#112994,#112995,#112996,#112997,#112998,
#112999,#113000,#113001,#113002,#113003,#113004,#113005,#113006),
 .UNSPECIFIED.,.F.,.F.,(4,2,2,2,2,2,2,2,2,2,4),(-0.482562577818028,-0.447777673419887,
-0.413036999106612,-0.354121907354326,-0.297189647078672,-0.24122658651999,
-0.185260249381691,-0.128411301285868,-0.0694119365245573,-0.0347286016619977,
0.),.UNSPECIFIED.) ;
#3412 = B_SPLINE_CURVE_WITH_KNOTS('',3,(#113009,#113010,#113011,#113012,#113013,
#113014,#113015,#113016,#113017),.UNSPECIFIED.,.F.,.F.,(4,1,1,1,1,1,4),
(0.,1.29587422179682,1.94381133989722,2.59174845799762,3.23968557610065,
3.88762269420369,5.18349660704779),.UNSPECIFIED.) ;
#3413 = B_SPLINE_CURVE_WITH_KNOTS('',3,(#113019,#113020,#113021,#113022,#113023,
#113024,#113025,#113026,#113027,#113028,#113029,#113030,#113031,#113032,
#113033,#113034,#113035,#113036,#113037),.UNSPECIFIED.,.T.,.F.,(4,1,1,1,
1,1,1,1,1,1,1,1,1,1,1,1,4),(0.,0.84428169467316,1.68856338934632,2.53284508400807,
3.37712677866981,4.22140847333581,5.06569016800181,5.90997186266355,6.75425355732529,
7.5985352519836,8.44281694664192,9.28709864130792,10.1313803359739,10.9756620306322,
11.8199437252905,12.664225419956,13.5085071146214),.UNSPECIFIED.) ;
#3414 = B_SPLINE_CURVE_WITH_KNOTS('',3,(#113047,#113048,#113049,#113050,#113051,
#113052,#113053,#113054,#113055,#113056,#113057),.UNSPECIFIED.,.F.,.F.,
(4,1,1,1,1,1,1,1,4),(0.,1.04064620349252,2.08129240698504,3.12193860703556,
4.16258480708607,5.2032310071414,6.24387720719673,7.28452341068926,8.32516961418179),
 .UNSPECIFIED.) ;
#3415 = B_SPLINE_CURVE_WITH_KNOTS('',3,(#113065,#113066,#113067,#113068,#113069,
#113070,#113071,#113072,#113073,#113074,#113075),.UNSPECIFIED.,.F.,.F.,
(4,1,1,1,1,1,1,1,4),(0.,1.04062614942685,2.0812522988537,3.12187844827608,
4.16250459769846,5.20313074711661,6.24375689653477,7.28438304596783,8.32500919540089),
 .UNSPECIFIED.) ;
#3416 = B_SPLINE_CURVE_WITH_KNOTS('',3,(#113077,#113078,#113079,#113080,#113081,
#113082),.UNSPECIFIED.,.F.,.F.,(4,2,4),(0.,0.224505556318787,0.44901111263762),
 .UNSPECIFIED.) ;
#3417 = B_SPLINE_CURVE_WITH_KNOTS('',3,(#113092,#113093,#113094,#113095,#113096,
#113097),.UNSPECIFIED.,.F.,.F.,(4,2,4),(6.6871801508411E-9,0.167853757777579,
0.335707403334044),.UNSPECIFIED.) ;
#3418 = B_SPLINE_CURVE_WITH_KNOTS('',3,(#113107,#113108,#113109,#113110,#113111,
#113112,#113113,#113114,#113115),.UNSPECIFIED.,.F.,.F.,(4,1,1,1,1,1,4),
(1.11022302462516E-16,1.29587422179682,1.94381133989722,2.59174845799762,
3.23968557610065,3.88762269420369,5.18349660704779),.UNSPECIFIED.) ;
#3419 = B_SPLINE_CURVE_WITH_KNOTS('',3,(#113363,#113364,#113365,#113366,#113367,
#113368,#113369,#113370,#113371,#113372,#113373,#113374,#113375,#113376,
#113377,#113378,#113379,#113380,#113381),.UNSPECIFIED.,.T.,.F.,(4,1,1,1,
1,1,1,1,1,1,1,1,1,1,1,1,4),(0.,2.69519445779222,5.61545499238395,8.53571552697321,
11.2309099847624,13.9261044425516,16.8463649771433,19.7666255117326,22.4618199695217,
25.1570144273109,28.0772749619002,30.9975354964919,33.692729954281,36.3879244120702,
39.3081849466595,42.2284454812513,44.9236399390404),.UNSPECIFIED.) ;
#3420 = B_SPLINE_CURVE_WITH_KNOTS('',3,(#113384,#113385,#113386,#113387,#113388,
#113389,#113390,#113391,#113392,#113393,#113394),.UNSPECIFIED.,.F.,.F.,
(4,1,1,1,1,1,1,1,4),(0.,1.04064620349252,2.08129240698504,3.12193860704037,
4.16258480709569,5.20323100714621,6.24387720719672,7.28452341068925,8.32516961418178),
 .UNSPECIFIED.) ;
#3421 = B_SPLINE_CURVE_WITH_KNOTS('',3,(#113398,#113399,#113400,#113401,#113402,
#113403,#113404,#113405,#113406,#113407,#113408),.UNSPECIFIED.,.F.,.F.,
(4,1,1,1,1,1,1,1,4),(0.,1.04062614942688,2.08125229885376,3.12187844827613,
4.1625045976985,5.20313074711665,6.24375689653479,7.28438304596787,8.32500919540094),
 .UNSPECIFIED.) ;
#3422 = B_SPLINE_CURVE_WITH_KNOTS('',3,(#113411,#113412,#113413,#113414,#113415,
#113416,#113417,#113418,#113419,#113420,#113421),.UNSPECIFIED.,.T.,.F.,
(4,1,1,1,1,1,1,1,4),(0.,0.903185063809554,1.80637013757091,2.70955520128371,
3.61274027504511,4.51592534880276,5.4191104125156,6.32229548627704,7.22548054998985),
 .UNSPECIFIED.) ;
#3423 = B_SPLINE_CURVE_WITH_KNOTS('',3,(#113426,#113427,#113428,#113429,#113430,
#113431,#113432,#113433,#113434),.UNSPECIFIED.,.F.,.F.,(4,1,1,1,1,1,4),
(0.,1.2958739093245,1.94381087119137,2.59174783305825,3.23968479492247,
3.88762175678669,5.18349566611894),.UNSPECIFIED.) ;
#3424 = B_SPLINE_CURVE_WITH_KNOTS('',3,(#113437,#113438,#113439,#113440,#113441,
#113442,#113443,#113444,#113445),.UNSPECIFIED.,.F.,.F.,(4,1,1,1,1,1,4),
(0.,1.29587422179652,1.94381133989956,2.5917484580026,3.23968557610299,
3.88762269420339,5.18349691602093),.UNSPECIFIED.) ;
#3425 = B_SPLINE_CURVE_WITH_KNOTS('',3,(#113447,#113448,#113449,#113450,#113451,
#113452,#113453,#113454,#113455,#113456,#113457,#113458,#113459,#113460,
#113461,#113462,#113463,#113464,#113465),.UNSPECIFIED.,.T.,.F.,(4,1,1,1,
1,1,1,1,1,1,1,1,1,1,1,1,4),(0.,0.844281694673181,1.68856338934636,2.5328450840081,
3.37712677866985,4.22140847333585,5.06569016800186,5.90997186266359,6.75425355732532,
7.59853525198361,8.44281694664191,9.28709864130793,10.131380335974,10.9756620306357,
11.8199437252974,12.6642254199629,13.5085071146283),.UNSPECIFIED.) ;
#3426 = B_SPLINE_CURVE_WITH_KNOTS('',3,(#113475,#113476,#113477,#113478,#113479,
#113480,#113481,#113482,#113483,#113484,#113485),.UNSPECIFIED.,.F.,.F.,
(4,1,1,1,1,1,1,1,4),(0.,1.04064620349252,2.08129240698504,3.12193860704037,
4.16258480709569,5.20323100714621,6.24387720719672,7.28452341068925,8.32516961418178),
 .UNSPECIFIED.) ;
#3427 = B_SPLINE_CURVE_WITH_KNOTS('',3,(#113493,#113494,#113495,#113496,#113497,
#113498,#113499,#113500,#113501,#113502,#113503),.UNSPECIFIED.,.F.,.F.,
(4,1,1,1,1,1,1,1,4),(0.,1.04062614942688,2.08125229885376,3.12187844827613,
4.1625045976985,5.20313074711665,6.24375689653479,7.28438304596787,8.32500919540094),
 .UNSPECIFIED.) ;
#3428 = B_SPLINE_CURVE_WITH_KNOTS('',3,(#113505,#113506,#113507,#113508,#113509,
#113510),.UNSPECIFIED.,.F.,.F.,(4,2,4),(0.,0.224505556318748,0.449011112637672),
 .UNSPECIFIED.) ;
#3429 = B_SPLINE_CURVE_WITH_KNOTS('',3,(#113520,#113521,#113522,#113523,#113524,
#113525),.UNSPECIFIED.,.F.,.F.,(4,2,4),(0.,0.167853741155252,0.335707418129887),
 .UNSPECIFIED.) ;
#3430 = B_SPLINE_CURVE_WITH_KNOTS('',3,(#113529,#113530,#113531,#113532,#113533,
#113534,#113535,#113536,#113537),.UNSPECIFIED.,.F.,.F.,(4,1,1,1,1,1,4),
(1.46151310183612E-7,1.2958739093245,1.94381087119137,2.59174783305825,
3.23968479492247,3.88762175678669,5.18349566611894),.UNSPECIFIED.) ;
#3431 = B_SPLINE_CURVE_WITH_KNOTS('',3,(#113543,#113544,#113545,#113546,#113547,
#113548,#113549,#113550,#113551),.UNSPECIFIED.,.F.,.F.,(4,1,1,1,1,1,4),
(0.,1.29587422179652,1.94381133989956,2.5917484580026,3.23968557610299,
3.88762269420339,5.18349691602093),.UNSPECIFIED.) ;
#3432 = B_SPLINE_CURVE_WITH_KNOTS('',3,(#113554,#113555,#113556,#113557,#113558,
#113559,#113560,#113561,#113562,#113563,#113564),.UNSPECIFIED.,.T.,.F.,
(4,1,1,1,1,1,1,1,4),(0.,0.903185063809554,1.80637013757091,2.70955520128371,
3.61274027504511,4.51592534880276,5.4191104125156,6.32229548627704,7.22548054998985),
 .UNSPECIFIED.) ;
#3433 = B_SPLINE_CURVE_WITH_KNOTS('',3,(#113795,#113796,#113797,#113798,#113799,
#113800,#113801,#113802,#113803,#113804,#113805,#113806,#113807,#113808,
#113809,#113810,#113811,#113812,#113813),.UNSPECIFIED.,.T.,.F.,(4,1,1,1,
1,1,1,1,1,1,1,1,1,1,1,1,4),(0.,0.667571568814079,1.33514313762816,2.00271471386765,
2.67028629010715,3.33785785892125,4.00542942773535,4.67300100397484,5.34057258021434,
6.00814415645112,6.67571573268789,7.34328730150198,8.01085887031606,8.67843044655556,
9.34600202279505,10.0135735916092,10.6811451604233),.UNSPECIFIED.) ;
#3434 = B_SPLINE_CURVE_WITH_KNOTS('',3,(#113816,#113817,#113818,#113819,#113820,
#113821,#113822,#113823,#113824,#113825,#113826,#113827,#113828,#113829,
#113830,#113831,#113832,#113833,#113834),.UNSPECIFIED.,.T.,.F.,(4,1,1,1,
1,1,1,1,1,1,1,1,1,1,1,1,4),(0.,0.667571568814083,1.33514313762817,2.00271471386766,
2.67028629010715,3.33785785892125,4.00542942773535,4.67300100397484,5.34057258021433,
6.00814415645111,6.67571573268789,7.34328730150198,8.01085887031607,8.67843044655557,
9.34600202279507,10.0135735916092,10.6811451604233),.UNSPECIFIED.) ;
#3435 = B_SPLINE_CURVE_WITH_KNOTS('',3,(#133905,#133906,#133907,#133908,#133909,
#133910,#133911,#133912,#133913,#133914,#133915,#133916,#133917,#133918,
#133919,#133920,#133921,#133922,#133923,#133924,#133925,#133926,#133927,
#133928,#133929,#133930,#133931,#133932,#133933,#133934,#133935,#133936,
#133937,#133938,#133939,#133940,#133941,#133942,#133943,#133944,#133945,
#133946,#133947,#133948,#133949,#133950,#133951,#133952,#133953,#133954,
#133955,#133956,#133957,#133958,#133959,#133960,#133961,#133962,#133963,
#133964,#133965,#133966,#133967,#133968,#133969,#133970,#133971,#133972,
#133973,#133974,#133975,#133976,#133977,#133978,#133979,#133980,#133981,
#133982,#133983,#133984,#133985,#133986,#133987,#133988,#133989,#133990,
#133991,#133992,#133993,#133994,#133995),.UNSPECIFIED.,.F.,.F.,(4,3,3,3,
3,3,3,3,3,3,3,3,3,3,3,3,3,3,3,3,3,3,3,3,3,3,3,3,3,3,4),(5.88213542013056,
6.01172757014424,6.06553319243455,6.3179007861267,6.37548924090185,6.63206088097925,
6.68416207138069,6.92315601894786,6.99256132469663,7.21356160680289,7.29931351804432,
7.37778610342962,7.45630346085746,7.5348566545112,7.60445173491709,7.66483126169226,
7.72511131097227,7.78447083804811,7.84521114843021,7.9059514588123,7.94504552692403,
7.9844284737438,8.02381142056356,8.05269951431726,8.08176218026163,8.08494149672526,
8.10686730860061,8.11737739318286,8.13530591783441,8.14584296460486,8.16217407354799),
 .UNSPECIFIED.) ;
#3436 = B_SPLINE_CURVE_WITH_KNOTS('',3,(#133997,#133998,#133999,#134000,#134001,
#134002,#134003,#134004,#134005,#134006,#134007,#134008,#134009,#134010,
#134011,#134012,#134013,#134014,#134015,#134016,#134017,#134018,#134019,
#134020,#134021,#134022,#134023,#134024,#134025,#134026,#134027,#134028,
#134029,#134030,#134031,#134032,#134033,#134034,#134035,#134036),
 .UNSPECIFIED.,.F.,.F.,(4,2,2,2,2,2,2,2,2,2,2,2,2,2,2,2,2,2,2,4),(-0.39127659712415,
-0.362669068199835,-0.333777979412566,-0.298294797615378,-0.264279211558204,
-0.227335226972421,-0.209250043988191,-0.205161811504485,-0.20408201623579,
-0.203429602940516,-0.202882771686664,-0.202269768258323,-0.2012554462146,
-0.198930919322328,-0.191706051626658,-0.146438477798862,-0.104948460896364,
-0.0633681945290975,-0.0314897645765271,-1.00000011526991E-6),
 .UNSPECIFIED.) ;
#3437 = B_SPLINE_CURVE_WITH_KNOTS('',3,(#134037,#134038,#134039,#134040,#134041,
#134042,#134043,#134044,#134045,#134046,#134047,#134048,#134049,#134050,
#134051,#134052,#134053,#134054,#134055,#134056,#134057,#134058,#134059,
#134060),.UNSPECIFIED.,.F.,.F.,(4,2,2,2,2,2,2,2,2,2,2,4),(-0.201634045224376,
-0.201150550092067,-0.200600545085954,-0.19922381894873,-0.19585601760169,
-0.188262366788053,-0.170242357527641,-0.140254894616156,-0.102132640276839,
-0.061140945039494,-0.0300852443665849,-9.99700435461159E-7),
 .UNSPECIFIED.) ;
#3438 = B_SPLINE_CURVE_WITH_KNOTS('',3,(#153893,#153894,#153895,#153896,#153897,
#153898,#153899,#153900,#153901,#153902,#153903,#153904,#153905,#153906,
#153907,#153908,#153909,#153910,#153911,#153912,#153913,#153914,#153915,
#153916,#153917,#153918,#153919,#153920,#153921,#153922,#153923,#153924,
#153925,#153926,#153927,#153928,#153929,#153930,#153931,#153932,#153933,
#153934,#153935,#153936,#153937,#153938,#153939,#153940,#153941,#153942,
#153943,#153944,#153945,#153946,#153947,#153948,#153949,#153950,#153951,
#153952,#153953,#153954,#153955,#153956,#153957,#153958,#153959,#153960,
#153961,#153962,#153963,#153964,#153965,#153966,#153967,#153968,#153969,
#153970,#153971,#153972,#153973,#153974,#153975,#153976,#153977,#153978,
#153979,#153980,#153981,#153982,#153983),.UNSPECIFIED.,.F.,.F.,(4,3,3,3,
3,3,3,3,3,3,3,3,3,3,3,3,3,3,3,3,3,3,3,3,3,3,3,3,3,3,4),(5.88213542013066,
6.01172757014427,6.06553319243458,6.31790078613558,6.37548924090187,6.63206088096672,
6.68416207138071,6.92315601894749,6.99256132469664,7.21356160680676,7.29931351804433,
7.3777861034297,7.45630346085931,7.53485665450175,7.6044517349171,7.66483126169192,
7.72511131097202,7.78447083804736,7.84521114842983,7.90595145881231,7.94504552692402,
7.98442847374379,8.02381142056356,8.05269951431751,8.08176218026769,8.08494149672526,
8.10686730860063,8.11737739318286,8.13530591783441,8.14584296460486,8.16217407354799),
 .UNSPECIFIED.) ;
#3439 = B_SPLINE_CURVE_WITH_KNOTS('',3,(#153984,#153985,#153986,#153987,#153988,
#153989,#153990,#153991,#153992,#153993,#153994,#153995,#153996,#153997,
#153998,#153999,#154000,#154001,#154002,#154003,#154004,#154005,#154006,
#154007,#154008,#154009,#154010,#154011,#154012,#154013,#154014,#154015,
#154016,#154017,#154018,#154019,#154020,#154021,#154022,#154023),
 .UNSPECIFIED.,.F.,.F.,(4,2,2,2,2,2,2,2,2,2,2,2,2,2,2,2,2,2,2,4),(1.0000001190084E-6,
0.0314897645751662,0.0633681945262461,0.104948460893497,0.1464384777964,
0.191706051628097,0.198930919322058,0.201255446202256,0.202269768237498,
0.202882771658999,0.203429602908372,0.204082016198889,0.205161811456729,
0.209250043899134,0.227335226679599,0.264279210845935,0.298294796516944,
0.333777977911312,0.362669066370513,0.391276594970033),.UNSPECIFIED.) ;
#3440 = B_SPLINE_CURVE_WITH_KNOTS('',3,(#154024,#154025,#154026,#154027,#154028,
#154029,#154030,#154031,#154032,#154033,#154034,#154035,#154036,#154037,
#154038,#154039,#154040,#154041,#154042,#154043,#154044,#154045,#154046,
#154047),.UNSPECIFIED.,.F.,.F.,(4,2,2,2,2,2,2,2,2,2,2,4),(-0.2016340451575,
-0.201150550045475,-0.200600545062619,-0.1992238189524,-0.19585601759736,
-0.188262366785114,-0.170242357526105,-0.140254894616092,-0.10213264027677,
-0.061140945039477,-0.030085244366594,-9.99700430853734E-7),
 .UNSPECIFIED.) ;
#3441 = B_SPLINE_CURVE_WITH_KNOTS('',3,(#173197,#173198,#173199,#173200,#173201,
#173202,#173203,#173204,#173205,#173206,#173207,#173208,#173209,#173210,
#173211,#173212,#173213,#173214,#173215,#173216,#173217,#173218,#173219,
#173220),.UNSPECIFIED.,.F.,.F.,(4,2,2,2,2,2,2,2,2,2,2,4),(1.00031199612268E-6,
0.000119735576117112,0.000254804132751259,0.00059289635728083,0.00141995080467776,
0.00328477655390897,0.00771007580557226,0.0150743060490529,0.0244362537133422,
0.034502869975532,0.0421294348106346,0.0495174324242607),.UNSPECIFIED.) ;
#3442 = B_SPLINE_CURVE_WITH_KNOTS('',3,(#173222,#173223,#173224,#173225,#173226,
#173227,#173228,#173229,#173230,#173231,#173232,#173233,#173234,#173235,
#173236,#173237,#173238,#173239,#173240,#173241,#173242,#173243,#173244,
#173245,#173246,#173247,#173248,#173249,#173250,#173251,#173252,#173253,
#173254,#173255,#173256,#173257,#173258,#173259,#173260,#173261),
 .UNSPECIFIED.,.F.,.F.,(4,2,2,2,2,2,2,2,2,2,2,2,2,2,2,2,2,2,2,4),(1.00000084760866E-6,
0.0356408539522558,0.0716339726729334,0.115839657841778,0.158216981743479,
0.204242565336012,0.226773462184898,0.231866667251746,0.233211898655665,
0.234024688708034,0.23470594245746,0.235469634878188,0.236733298374843,
0.239629242314517,0.248630132692209,0.305025417214415,0.356714542868905,
0.408516103190126,0.448230914032676,0.487460271649596),.UNSPECIFIED.) ;
#3443 = B_SPLINE_CURVE_WITH_KNOTS('',3,(#173262,#173263,#173264,#173265,#173266,
#173267,#173268,#173269,#173270,#173271,#173272,#173273,#173274,#173275,
#173276,#173277,#173278,#173279,#173280,#173281,#173282,#173283,#173284,
#173285,#173286,#173287,#173288,#173289,#173290,#173291,#173292,#173293,
#173294,#173295,#173296,#173297,#173298,#173299,#173300,#173301,#173302,
#173303,#173304,#173305,#173306,#173307,#173308,#173309,#173310,#173311,
#173312,#173313,#173314,#173315,#173316,#173317,#173318,#173319,#173320,
#173321,#173322,#173323,#173324,#173325,#173326,#173327,#173328,#173329,
#173330,#173331,#173332,#173333,#173334,#173335,#173336,#173337,#173338,
#173339,#173340,#173341,#173342,#173343,#173344,#173345,#173346,#173347,
#173348,#173349,#173350,#173351,#173352),.UNSPECIFIED.,.F.,.F.,(4,3,3,3,
3,3,3,3,3,3,3,3,3,3,3,3,3,3,3,3,3,3,3,3,3,3,3,3,3,3,4),(5.88213542013056,
6.01172757014424,6.06553319243455,6.31789845245754,6.37548924090185,6.63205227957284,
6.68416207138069,6.92308957797642,6.99256132469663,7.21322502396329,7.29931351804432,
7.37778610061133,7.45630345780951,7.53485664750583,7.60445173491709,7.66483122117882,
7.72511128058719,7.78447080698424,7.84521113289827,7.9059514588123,7.9450455134496,
7.98442846700658,8.02381142056356,8.05269948781751,8.08176212724297,8.08494149672526,
8.10686730859982,8.11737739318286,8.13530591783441,8.14584296460486,8.16217407354799),
 .UNSPECIFIED.) ;
#3444 = B_SPLINE_CURVE_WITH_KNOTS('',3,(#193185,#193186,#193187,#193188,#193189,
#193190,#193191,#193192,#193193,#193194,#193195,#193196,#193197,#193198,
#193199,#193200,#193201,#193202,#193203,#193204,#193205,#193206,#193207,
#193208),.UNSPECIFIED.,.F.,.F.,(4,2,2,2,2,2,2,2,2,2,2,4),(1.00031199566413E-6,
0.000119735576065817,0.000254804132477893,0.000592896355756741,0.0014199507976843,
0.00328477653422319,0.00771007575652981,0.0150743059510554,0.0244362535529347,
0.0345028697479965,0.0421294345322319,0.0495174320965966),.UNSPECIFIED.) ;
#3445 = B_SPLINE_CURVE_WITH_KNOTS('',3,(#193209,#193210,#193211,#193212,#193213,
#193214,#193215,#193216,#193217,#193218,#193219,#193220,#193221,#193222,
#193223,#193224,#193225,#193226,#193227,#193228,#193229,#193230,#193231,
#193232,#193233,#193234,#193235,#193236,#193237,#193238,#193239,#193240,
#193241,#193242,#193243,#193244,#193245,#193246,#193247,#193248),
 .UNSPECIFIED.,.F.,.F.,(4,2,2,2,2,2,2,2,2,2,2,2,2,2,2,2,2,2,2,4),(-0.487460274297177,
-0.44823091626508,-0.408516105002165,-0.356714544130802,-0.305025417927037,
-0.248630132802184,-0.23962924233009,-0.236733298377342,-0.235469634879205,
-0.234705942460026,-0.234024688710982,-0.233211898657874,-0.231866667252239,
-0.22677346218541,-0.204242565336273,-0.158216981743476,-0.115839657841771,
-0.071633972672922,-0.0356408539523076,-1.00000084793567E-6),
 .UNSPECIFIED.) ;
#3446 = B_SPLINE_CURVE_WITH_KNOTS('',3,(#193249,#193250,#193251,#193252,#193253,
#193254,#193255,#193256,#193257,#193258,#193259,#193260,#193261,#193262,
#193263,#193264,#193265,#193266,#193267,#193268,#193269,#193270,#193271,
#193272,#193273,#193274,#193275,#193276,#193277,#193278,#193279,#193280,
#193281,#193282,#193283,#193284,#193285,#193286,#193287,#193288,#193289,
#193290,#193291,#193292,#193293,#193294,#193295,#193296,#193297,#193298,
#193299,#193300,#193301,#193302,#193303,#193304,#193305,#193306,#193307,
#193308,#193309,#193310,#193311,#193312,#193313,#193314,#193315,#193316,
#193317,#193318,#193319,#193320,#193321,#193322,#193323,#193324,#193325,
#193326,#193327,#193328,#193329,#193330,#193331,#193332,#193333,#193334,
#193335,#193336,#193337,#193338,#193339),.UNSPECIFIED.,.F.,.F.,(4,3,3,3,
3,3,3,3,3,3,3,3,3,3,3,3,3,3,3,3,3,3,3,3,3,3,3,3,3,3,4),(5.88213542013066,
6.01172757014427,6.06553319243458,6.31789845246383,6.37548924090187,6.63205227957771,
6.68416207138071,6.92308957798153,6.99256132469664,7.21322502396281,7.29931351804433,
7.37778610061136,7.45630345780724,7.53485664750453,7.6044517349171,7.66483122117873,
7.72511128058713,7.78447080698428,7.84521113289829,7.90595145881231,7.94504551344955,
7.98442846700656,8.02381142056356,8.05269948781744,8.08176212725545,8.08494149672526,
8.10686730859978,8.11737739318286,8.13530591783441,8.14584296460486,8.16217407354799),
 .UNSPECIFIED.) ;
#3447 = VERTEX_POINT('',#11579) ;
#3448 = VERTEX_POINT('',#11580) ;
#3449 = VERTEX_POINT('',#11651) ;
#3450 = VERTEX_POINT('',#11653) ;
#3451 = VERTEX_POINT('',#11853) ;
#3452 = VERTEX_POINT('',#11854) ;
#3453 = VERTEX_POINT('',#11925) ;
#3454 = VERTEX_POINT('',#11927) ;
#3455 = VERTEX_POINT('',#12156) ;
#3456 = VERTEX_POINT('',#12203) ;
#3457 = VERTEX_POINT('',#12250) ;
#3458 = VERTEX_POINT('',#12297) ;
#3459 = VERTEX_POINT('',#12315) ;
#3460 = VERTEX_POINT('',#12317) ;
#3461 = VERTEX_POINT('',#12321) ;
#3462 = VERTEX_POINT('',#12342) ;
#3463 = VERTEX_POINT('',#12441) ;
#3464 = VERTEX_POINT('',#12442) ;
#3465 = VERTEX_POINT('',#12444) ;
#3466 = VERTEX_POINT('',#12512) ;
#3467 = VERTEX_POINT('',#12523) ;
#3468 = VERTEX_POINT('',#12525) ;
#3469 = VERTEX_POINT('',#12708) ;
#3470 = VERTEX_POINT('',#12709) ;
#3471 = VERTEX_POINT('',#12711) ;
#3472 = VERTEX_POINT('',#12846) ;
#3473 = VERTEX_POINT('',#12982) ;
#3474 = VERTEX_POINT('',#12983) ;
#3475 = VERTEX_POINT('',#12985) ;
#3476 = VERTEX_POINT('',#13613) ;
#3477 = VERTEX_POINT('',#13953) ;
#3478 = VERTEX_POINT('',#13954) ;
#3479 = VERTEX_POINT('',#13956) ;
#3480 = VERTEX_POINT('',#14451) ;
#3481 = VERTEX_POINT('',#15017) ;
#3482 = VERTEX_POINT('',#15018) ;
#3483 = VERTEX_POINT('',#15020) ;
#3484 = VERTEX_POINT('',#15085) ;
#3485 = VERTEX_POINT('',#15155) ;
#3486 = VERTEX_POINT('',#15156) ;
#3487 = VERTEX_POINT('',#15158) ;
#3488 = VERTEX_POINT('',#15665) ;
#3489 = VERTEX_POINT('',#15762) ;
#3490 = VERTEX_POINT('',#15763) ;
#3491 = VERTEX_POINT('',#16032) ;
#3492 = VERTEX_POINT('',#16033) ;
#3493 = VERTEX_POINT('',#16287) ;
#3494 = VERTEX_POINT('',#16288) ;
#3495 = VERTEX_POINT('',#17909) ;
#3496 = VERTEX_POINT('',#17910) ;
#3497 = VERTEX_POINT('',#17912) ;
#3498 = VERTEX_POINT('',#18185) ;
#3499 = VERTEX_POINT('',#18437) ;
#3500 = VERTEX_POINT('',#18439) ;
#3501 = VERTEX_POINT('',#18442) ;
#3502 = VERTEX_POINT('',#18459) ;
#3503 = VERTEX_POINT('',#18476) ;
#3504 = VERTEX_POINT('',#18493) ;
#3505 = VERTEX_POINT('',#18511) ;
#3506 = VERTEX_POINT('',#18531) ;
#3507 = VERTEX_POINT('',#18700) ;
#3508 = VERTEX_POINT('',#18720) ;
#3509 = VERTEX_POINT('',#18967) ;
#3510 = VERTEX_POINT('',#18968) ;
#3511 = VERTEX_POINT('',#18970) ;
#3512 = VERTEX_POINT('',#18974) ;
#3513 = VERTEX_POINT('',#18975) ;
#3514 = VERTEX_POINT('',#18977) ;
#3515 = VERTEX_POINT('',#25950) ;
#3516 = VERTEX_POINT('',#25951) ;
#3517 = VERTEX_POINT('',#25965) ;
#3518 = VERTEX_POINT('',#33237) ;
#3519 = VERTEX_POINT('',#33238) ;
#3520 = VERTEX_POINT('',#33252) ;
#3521 = VERTEX_POINT('',#33346) ;
#3522 = VERTEX_POINT('',#33348) ;
#3523 = VERTEX_POINT('',#33350) ;
#3524 = VERTEX_POINT('',#41228) ;
#3525 = VERTEX_POINT('',#41429) ;
#3526 = VERTEX_POINT('',#41433) ;
#3527 = VERTEX_POINT('',#41802) ;
#3528 = VERTEX_POINT('',#42522) ;
#3529 = VERTEX_POINT('',#42523) ;
#3530 = VERTEX_POINT('',#42537) ;
#3531 = VERTEX_POINT('',#42932) ;
#3532 = VERTEX_POINT('',#42937) ;
#3533 = VERTEX_POINT('',#43216) ;
#3534 = VERTEX_POINT('',#43218) ;
#3535 = VERTEX_POINT('',#43229) ;
#3536 = VERTEX_POINT('',#43240) ;
#3537 = VERTEX_POINT('',#50223) ;
#3538 = VERTEX_POINT('',#57274) ;
#3539 = VERTEX_POINT('',#57275) ;
#3540 = VERTEX_POINT('',#57320) ;
#3541 = VERTEX_POINT('',#57340) ;
#3542 = VERTEX_POINT('',#64472) ;
#3543 = VERTEX_POINT('',#71534) ;
#3544 = VERTEX_POINT('',#71551) ;
#3545 = VERTEX_POINT('',#71961) ;
#3546 = VERTEX_POINT('',#71979) ;
#3547 = VERTEX_POINT('',#79037) ;
#3548 = VERTEX_POINT('',#79038) ;
#3549 = VERTEX_POINT('',#79093) ;
#3550 = VERTEX_POINT('',#79095) ;
#3551 = VERTEX_POINT('',#79149) ;
#3552 = VERTEX_POINT('',#79151) ;
#3553 = VERTEX_POINT('',#79172) ;
#3554 = VERTEX_POINT('',#79173) ;
#3555 = VERTEX_POINT('',#79261) ;
#3556 = VERTEX_POINT('',#79263) ;
#3557 = VERTEX_POINT('',#79265) ;
#3558 = VERTEX_POINT('',#79270) ;
#3559 = VERTEX_POINT('',#79306) ;
#3560 = VERTEX_POINT('',#79308) ;
#3561 = VERTEX_POINT('',#79314) ;
#3562 = VERTEX_POINT('',#79315) ;
#3563 = VERTEX_POINT('',#79317) ;
#3564 = VERTEX_POINT('',#79486) ;
#3565 = VERTEX_POINT('',#79631) ;
#3566 = VERTEX_POINT('',#79632) ;
#3567 = VERTEX_POINT('',#80087) ;
#3568 = VERTEX_POINT('',#80088) ;
#3569 = VERTEX_POINT('',#80534) ;
#3570 = VERTEX_POINT('',#80535) ;
#3571 = VERTEX_POINT('',#80990) ;
#3572 = VERTEX_POINT('',#81291) ;
#3573 = VERTEX_POINT('',#81516) ;
#3574 = VERTEX_POINT('',#81517) ;
#3575 = VERTEX_POINT('',#81521) ;
#3576 = VERTEX_POINT('',#81548) ;
#3577 = VERTEX_POINT('',#88562) ;
#3578 = VERTEX_POINT('',#95647) ;
#3579 = VERTEX_POINT('',#95699) ;
#3580 = VERTEX_POINT('',#95703) ;
#3581 = VERTEX_POINT('',#95704) ;
#3582 = VERTEX_POINT('',#95706) ;
#3583 = VERTEX_POINT('',#95708) ;
#3584 = VERTEX_POINT('',#95710) ;
#3585 = VERTEX_POINT('',#95712) ;
#3586 = VERTEX_POINT('',#95716) ;
#3587 = VERTEX_POINT('',#95718) ;
#3588 = VERTEX_POINT('',#95722) ;
#3589 = VERTEX_POINT('',#95726) ;
#3590 = VERTEX_POINT('',#95730) ;
#3591 = VERTEX_POINT('',#95734) ;
#3592 = VERTEX_POINT('',#95741) ;
#3593 = VERTEX_POINT('',#95742) ;
#3594 = VERTEX_POINT('',#95744) ;
#3595 = VERTEX_POINT('',#95913) ;
#3596 = VERTEX_POINT('',#96058) ;
#3597 = VERTEX_POINT('',#96059) ;
#3598 = VERTEX_POINT('',#97230) ;
#3599 = VERTEX_POINT('',#97231) ;
#3600 = VERTEX_POINT('',#97677) ;
#3601 = VERTEX_POINT('',#97678) ;
#3602 = VERTEX_POINT('',#98133) ;
#3603 = VERTEX_POINT('',#98432) ;
#3604 = VERTEX_POINT('',#98657) ;
#3605 = VERTEX_POINT('',#98659) ;
#3606 = VERTEX_POINT('',#98662) ;
#3607 = VERTEX_POINT('',#98690) ;
#3608 = VERTEX_POINT('',#105703) ;
#3609 = VERTEX_POINT('',#112788) ;
#3610 = VERTEX_POINT('',#112840) ;
#3611 = VERTEX_POINT('',#112844) ;
#3612 = VERTEX_POINT('',#112845) ;
#3613 = VERTEX_POINT('',#112847) ;
#3614 = VERTEX_POINT('',#112849) ;
#3615 = VERTEX_POINT('',#112851) ;
#3616 = VERTEX_POINT('',#112853) ;
#3617 = VERTEX_POINT('',#112857) ;
#3618 = VERTEX_POINT('',#112859) ;
#3619 = VERTEX_POINT('',#112863) ;
#3620 = VERTEX_POINT('',#112867) ;
#3621 = VERTEX_POINT('',#112871) ;
#3622 = VERTEX_POINT('',#112875) ;
#3623 = VERTEX_POINT('',#112882) ;
#3624 = VERTEX_POINT('',#112883) ;
#3625 = VERTEX_POINT('',#112885) ;
#3626 = VERTEX_POINT('',#112887) ;
#3627 = VERTEX_POINT('',#112891) ;
#3628 = VERTEX_POINT('',#112893) ;
#3629 = VERTEX_POINT('',#112897) ;
#3630 = VERTEX_POINT('',#112899) ;
#3631 = VERTEX_POINT('',#112906) ;
#3632 = VERTEX_POINT('',#112908) ;
#3633 = VERTEX_POINT('',#112912) ;
#3634 = VERTEX_POINT('',#112914) ;
#3635 = VERTEX_POINT('',#112915) ;
#3636 = VERTEX_POINT('',#112917) ;
#3637 = VERTEX_POINT('',#112919) ;
#3638 = VERTEX_POINT('',#112922) ;
#3639 = VERTEX_POINT('',#112924) ;
#3640 = VERTEX_POINT('',#112925) ;
#3641 = VERTEX_POINT('',#112927) ;
#3642 = VERTEX_POINT('',#112929) ;
#3643 = VERTEX_POINT('',#112933) ;
#3644 = VERTEX_POINT('',#112953) ;
#3645 = VERTEX_POINT('',#112954) ;
#3646 = VERTEX_POINT('',#112966) ;
#3647 = VERTEX_POINT('',#112968) ;
#3648 = VERTEX_POINT('',#112981) ;
#3649 = VERTEX_POINT('',#112982) ;
#3650 = VERTEX_POINT('',#112984) ;
#3651 = VERTEX_POINT('',#113007) ;
#3652 = VERTEX_POINT('',#113018) ;
#3653 = VERTEX_POINT('',#113039) ;
#3654 = VERTEX_POINT('',#113043) ;
#3655 = VERTEX_POINT('',#113045) ;
#3656 = VERTEX_POINT('',#113059) ;
#3657 = VERTEX_POINT('',#113063) ;
#3658 = VERTEX_POINT('',#113084) ;
#3659 = VERTEX_POINT('',#113088) ;
#3660 = VERTEX_POINT('',#113090) ;
#3661 = VERTEX_POINT('',#113099) ;
#3662 = VERTEX_POINT('',#113103) ;
#3663 = VERTEX_POINT('',#113315) ;
#3664 = VERTEX_POINT('',#113316) ;
#3665 = VERTEX_POINT('',#113318) ;
#3666 = VERTEX_POINT('',#113320) ;
#3667 = VERTEX_POINT('',#113324) ;
#3668 = VERTEX_POINT('',#113326) ;
#3669 = VERTEX_POINT('',#113330) ;
#3670 = VERTEX_POINT('',#113332) ;
#3671 = VERTEX_POINT('',#113339) ;
#3672 = VERTEX_POINT('',#113341) ;
#3673 = VERTEX_POINT('',#113342) ;
#3674 = VERTEX_POINT('',#113344) ;
#3675 = VERTEX_POINT('',#113346) ;
#3676 = VERTEX_POINT('',#113349) ;
#3677 = VERTEX_POINT('',#113351) ;
#3678 = VERTEX_POINT('',#113352) ;
#3679 = VERTEX_POINT('',#113354) ;
#3680 = VERTEX_POINT('',#113356) ;
#3681 = VERTEX_POINT('',#113359) ;
#3682 = VERTEX_POINT('',#113362) ;
#3683 = VERTEX_POINT('',#113382) ;
#3684 = VERTEX_POINT('',#113383) ;
#3685 = VERTEX_POINT('',#113395) ;
#3686 = VERTEX_POINT('',#113397) ;
#3687 = VERTEX_POINT('',#113410) ;
#3688 = VERTEX_POINT('',#113422) ;
#3689 = VERTEX_POINT('',#113423) ;
#3690 = VERTEX_POINT('',#113425) ;
#3691 = VERTEX_POINT('',#113435) ;
#3692 = VERTEX_POINT('',#113446) ;
#3693 = VERTEX_POINT('',#113467) ;
#3694 = VERTEX_POINT('',#113471) ;
#3695 = VERTEX_POINT('',#113473) ;
#3696 = VERTEX_POINT('',#113487) ;
#3697 = VERTEX_POINT('',#113491) ;
#3698 = VERTEX_POINT('',#113512) ;
#3699 = VERTEX_POINT('',#113516) ;
#3700 = VERTEX_POINT('',#113518) ;
#3701 = VERTEX_POINT('',#113527) ;
#3702 = VERTEX_POINT('',#113539) ;
#3703 = VERTEX_POINT('',#113553) ;
#3704 = VERTEX_POINT('',#113788) ;
#3705 = VERTEX_POINT('',#113790) ;
#3706 = VERTEX_POINT('',#113794) ;
#3707 = VERTEX_POINT('',#113815) ;
#3708 = VERTEX_POINT('',#113914) ;
#3709 = VERTEX_POINT('',#113915) ;
#3710 = VERTEX_POINT('',#113917) ;
#3711 = VERTEX_POINT('',#113919) ;
#3712 = VERTEX_POINT('',#113923) ;
#3713 = VERTEX_POINT('',#113925) ;
#3714 = VERTEX_POINT('',#113929) ;
#3715 = VERTEX_POINT('',#113931) ;
#3716 = VERTEX_POINT('',#113935) ;
#3717 = VERTEX_POINT('',#113937) ;
#3718 = VERTEX_POINT('',#113941) ;
#3719 = VERTEX_POINT('',#113943) ;
#3720 = VERTEX_POINT('',#113947) ;
#3721 = VERTEX_POINT('',#113949) ;
#3722 = VERTEX_POINT('',#113953) ;
#3723 = VERTEX_POINT('',#113955) ;
#3724 = VERTEX_POINT('',#113959) ;
#3725 = VERTEX_POINT('',#113961) ;
#3726 = VERTEX_POINT('',#113965) ;
#3727 = VERTEX_POINT('',#113967) ;
#3728 = VERTEX_POINT('',#113971) ;
#3729 = VERTEX_POINT('',#113973) ;
#3730 = VERTEX_POINT('',#113977) ;
#3731 = VERTEX_POINT('',#113979) ;
#3732 = VERTEX_POINT('',#113986) ;
#3733 = VERTEX_POINT('',#113988) ;
#3734 = VERTEX_POINT('',#113991) ;
#3735 = VERTEX_POINT('',#113993) ;
#3736 = VERTEX_POINT('',#114000) ;
#3737 = VERTEX_POINT('',#114001) ;
#3738 = VERTEX_POINT('',#114031) ;
#3739 = VERTEX_POINT('',#114033) ;
#3740 = VERTEX_POINT('',#114053) ;
#3741 = VERTEX_POINT('',#114137) ;
#3742 = VERTEX_POINT('',#114166) ;
#3743 = VERTEX_POINT('',#114189) ;
#3744 = VERTEX_POINT('',#114191) ;
#3745 = VERTEX_POINT('',#114220) ;
#3746 = VERTEX_POINT('',#114221) ;
#3747 = VERTEX_POINT('',#114242) ;
#3748 = VERTEX_POINT('',#114326) ;
#3749 = VERTEX_POINT('',#114355) ;
#3750 = VERTEX_POINT('',#114378) ;
#3751 = VERTEX_POINT('',#132839) ;
#3752 = VERTEX_POINT('',#132840) ;
#3753 = VERTEX_POINT('',#133899) ;
#3754 = VERTEX_POINT('',#133901) ;
#3755 = VERTEX_POINT('',#133904) ;
#3756 = VERTEX_POINT('',#133996) ;
#3757 = VERTEX_POINT('',#134124) ;
#3758 = VERTEX_POINT('',#134169) ;
#3759 = VERTEX_POINT('',#134171) ;
#3760 = VERTEX_POINT('',#134173) ;
#3761 = VERTEX_POINT('',#134367) ;
#3762 = VERTEX_POINT('',#152828) ;
#3763 = VERTEX_POINT('',#152829) ;
#3764 = VERTEX_POINT('',#153888) ;
#3765 = VERTEX_POINT('',#153890) ;
#3766 = VERTEX_POINT('',#154111) ;
#3767 = VERTEX_POINT('',#154156) ;
#3768 = VERTEX_POINT('',#154158) ;
#3769 = VERTEX_POINT('',#154160) ;
#3770 = VERTEX_POINT('',#154356) ;
#3771 = VERTEX_POINT('',#154358) ;
#3772 = VERTEX_POINT('',#154387) ;
#3773 = VERTEX_POINT('',#154388) ;
#3774 = VERTEX_POINT('',#154409) ;
#3775 = VERTEX_POINT('',#154493) ;
#3776 = VERTEX_POINT('',#154522) ;
#3777 = VERTEX_POINT('',#154545) ;
#3778 = VERTEX_POINT('',#154546) ;
#3779 = VERTEX_POINT('',#154576) ;
#3780 = VERTEX_POINT('',#154578) ;
#3781 = VERTEX_POINT('',#154598) ;
#3782 = VERTEX_POINT('',#154682) ;
#3783 = VERTEX_POINT('',#154711) ;
#3784 = VERTEX_POINT('',#154734) ;
#3785 = VERTEX_POINT('',#173195) ;
#3786 = VERTEX_POINT('',#173196) ;
#3787 = VERTEX_POINT('',#173221) ;
#3788 = VERTEX_POINT('',#173353) ;
#3789 = VERTEX_POINT('',#174412) ;
#3790 = VERTEX_POINT('',#174414) ;
#3791 = VERTEX_POINT('',#174480) ;
#3792 = VERTEX_POINT('',#174525) ;
#3793 = VERTEX_POINT('',#174527) ;
#3794 = VERTEX_POINT('',#174529) ;
#3795 = VERTEX_POINT('',#174723) ;
#3796 = VERTEX_POINT('',#193184) ;
#3797 = VERTEX_POINT('',#193340) ;
#3798 = VERTEX_POINT('',#194399) ;
#3799 = VERTEX_POINT('',#194401) ;
#3800 = VERTEX_POINT('',#194467) ;
#3801 = VERTEX_POINT('',#194512) ;
#3802 = VERTEX_POINT('',#194514) ;
#3803 = VERTEX_POINT('',#194516) ;
#3804 = VERTEX_POINT('',#194712) ;
#3805 = VERTEX_POINT('',#194713) ;
#3806 = VERTEX_POINT('',#194715) ;
#3807 = VERTEX_POINT('',#194717) ;
#3808 = VERTEX_POINT('',#194726) ;
#3809 = VERTEX_POINT('',#194728) ;
#3810 = VERTEX_POINT('',#194732) ;
#3811 = VERTEX_POINT('',#194734) ;
#3812 = VERTEX_POINT('',#194738) ;
#3813 = VERTEX_POINT('',#194740) ;
#3814 = VERTEX_POINT('',#194744) ;
#3815 = VERTEX_POINT('',#194746) ;
#3816 = VERTEX_POINT('',#194750) ;
#3817 = VERTEX_POINT('',#194752) ;
#3818 = VERTEX_POINT('',#194756) ;
#3819 = VERTEX_POINT('',#194758) ;
#3820 = VERTEX_POINT('',#194762) ;
#3821 = VERTEX_POINT('',#194764) ;
#3822 = VERTEX_POINT('',#194768) ;
#3823 = VERTEX_POINT('',#194770) ;
#3824 = VERTEX_POINT('',#194774) ;
#3825 = VERTEX_POINT('',#194776) ;
#3826 = VERTEX_POINT('',#194780) ;
#3827 = VERTEX_POINT('',#194782) ;
#3828 = VERTEX_POINT('',#194786) ;
#3829 = VERTEX_POINT('',#194788) ;
#3830 = VERTEX_POINT('',#194792) ;
#3831 = VERTEX_POINT('',#194794) ;
#3832 = VERTEX_POINT('',#194803) ;
#3833 = VERTEX_POINT('',#194805) ;
#3834 = VERTEX_POINT('',#194812) ;
#3835 = VERTEX_POINT('',#194814) ;
#3836 = VERTEX_POINT('',#194818) ;
#3837 = VERTEX_POINT('',#194820) ;
#3838 = VERTEX_POINT('',#194826) ;
#3839 = VERTEX_POINT('',#194828) ;
#3840 = VERTEX_POINT('',#194832) ;
#3841 = VERTEX_POINT('',#194834) ;
#3842 = VERTEX_POINT('',#194837) ;
#3843 = VERTEX_POINT('',#194840) ;
#3844 = VERTEX_POINT('',#194842) ;
#3845 = VERTEX_POINT('',#194846) ;
#3846 = VERTEX_POINT('',#194854) ;
#3847 = VERTEX_POINT('',#194855) ;
#3848 = VERTEX_POINT('',#194857) ;
#3849 = VERTEX_POINT('',#194859) ;
#3850 = VERTEX_POINT('',#194872) ;
#3851 = VERTEX_POINT('',#194874) ;
#3852 = VERTEX_POINT('',#194878) ;
#3853 = VERTEX_POINT('',#194880) ;
#3854 = VERTEX_POINT('',#194884) ;
#3855 = VERTEX_POINT('',#194886) ;
#3856 = VERTEX_POINT('',#194899) ;
#3857 = VERTEX_POINT('',#194901) ;
#3858 = VERTEX_POINT('',#194905) ;
#3859 = VERTEX_POINT('',#194907) ;
#3860 = VERTEX_POINT('',#194911) ;
#3861 = VERTEX_POINT('',#194913) ;
#3862 = VERTEX_POINT('',#194926) ;
#3863 = VERTEX_POINT('',#194928) ;
#3864 = VERTEX_POINT('',#194932) ;
#3865 = VERTEX_POINT('',#194934) ;
#3866 = VERTEX_POINT('',#194938) ;
#3867 = VERTEX_POINT('',#194940) ;
#3868 = VERTEX_POINT('',#194953) ;
#3869 = VERTEX_POINT('',#194955) ;
#3870 = VERTEX_POINT('',#194959) ;
#3871 = VERTEX_POINT('',#194961) ;
#3872 = VERTEX_POINT('',#194965) ;
#3873 = VERTEX_POINT('',#194967) ;
#3874 = VERTEX_POINT('',#194980) ;
#3875 = VERTEX_POINT('',#194982) ;
#3876 = VERTEX_POINT('',#194986) ;
#3877 = VERTEX_POINT('',#194988) ;
#3878 = VERTEX_POINT('',#194992) ;
#3879 = VERTEX_POINT('',#194994) ;
#3880 = VERTEX_POINT('',#195007) ;
#3881 = VERTEX_POINT('',#195009) ;
#3882 = VERTEX_POINT('',#195013) ;
#3883 = VERTEX_POINT('',#195015) ;
#3884 = VERTEX_POINT('',#195019) ;
#3885 = VERTEX_POINT('',#195021) ;
#3886 = VERTEX_POINT('',#195034) ;
#3887 = VERTEX_POINT('',#195036) ;
#3888 = VERTEX_POINT('',#195040) ;
#3889 = VERTEX_POINT('',#195042) ;
#3890 = VERTEX_POINT('',#195046) ;
#3891 = VERTEX_POINT('',#195048) ;
#3892 = VERTEX_POINT('',#195061) ;
#3893 = VERTEX_POINT('',#195063) ;
#3894 = VERTEX_POINT('',#195067) ;
#3895 = VERTEX_POINT('',#195069) ;
#3896 = VERTEX_POINT('',#195073) ;
#3897 = VERTEX_POINT('',#195075) ;
#3898 = VERTEX_POINT('',#195088) ;
#3899 = VERTEX_POINT('',#195090) ;
#3900 = VERTEX_POINT('',#195094) ;
#3901 = VERTEX_POINT('',#195096) ;
#3902 = VERTEX_POINT('',#195100) ;
#3903 = VERTEX_POINT('',#195102) ;
#3904 = VERTEX_POINT('',#195115) ;
#3905 = VERTEX_POINT('',#195117) ;
#3906 = VERTEX_POINT('',#195121) ;
#3907 = VERTEX_POINT('',#195123) ;
#3908 = VERTEX_POINT('',#195127) ;
#3909 = VERTEX_POINT('',#195129) ;
#3910 = VERTEX_POINT('',#195142) ;
#3911 = VERTEX_POINT('',#195144) ;
#3912 = VERTEX_POINT('',#195148) ;
#3913 = VERTEX_POINT('',#195150) ;
#3914 = VERTEX_POINT('',#195154) ;
#3915 = VERTEX_POINT('',#195156) ;
#3916 = VERTEX_POINT('',#195169) ;
#3917 = VERTEX_POINT('',#195171) ;
#3918 = VERTEX_POINT('',#195175) ;
#3919 = VERTEX_POINT('',#195177) ;
#3920 = VERTEX_POINT('',#195181) ;
#3921 = VERTEX_POINT('',#195183) ;
#3922 = VERTEX_POINT('',#195196) ;
#3923 = VERTEX_POINT('',#195198) ;
#3924 = VERTEX_POINT('',#195202) ;
#3925 = VERTEX_POINT('',#195204) ;
#3926 = VERTEX_POINT('',#195208) ;
#3927 = VERTEX_POINT('',#195210) ;
#3928 = VERTEX_POINT('',#195223) ;
#3929 = VERTEX_POINT('',#195225) ;
#3930 = VERTEX_POINT('',#195229) ;
#3931 = VERTEX_POINT('',#195231) ;
#3932 = VERTEX_POINT('',#195235) ;
#3933 = VERTEX_POINT('',#195237) ;
#3934 = VERTEX_POINT('',#195250) ;
#3935 = VERTEX_POINT('',#195252) ;
#3936 = VERTEX_POINT('',#195256) ;
#3937 = VERTEX_POINT('',#195258) ;
#3938 = VERTEX_POINT('',#195262) ;
#3939 = VERTEX_POINT('',#195264) ;
#3940 = VERTEX_POINT('',#195277) ;
#3941 = VERTEX_POINT('',#195279) ;
#3942 = VERTEX_POINT('',#195283) ;
#3943 = VERTEX_POINT('',#195285) ;
#3944 = VERTEX_POINT('',#195289) ;
#3945 = VERTEX_POINT('',#195291) ;
#3946 = VERTEX_POINT('',#195304) ;
#3947 = VERTEX_POINT('',#195306) ;
#3948 = VERTEX_POINT('',#195310) ;
#3949 = VERTEX_POINT('',#195312) ;
#3950 = VERTEX_POINT('',#195316) ;
#3951 = VERTEX_POINT('',#195318) ;
#3952 = VERTEX_POINT('',#195331) ;
#3953 = VERTEX_POINT('',#195333) ;
#3954 = VERTEX_POINT('',#195337) ;
#3955 = VERTEX_POINT('',#195339) ;
#3956 = VERTEX_POINT('',#195343) ;
#3957 = VERTEX_POINT('',#195345) ;
#3958 = VERTEX_POINT('',#195358) ;
#3959 = VERTEX_POINT('',#195360) ;
#3960 = VERTEX_POINT('',#195364) ;
#3961 = VERTEX_POINT('',#195366) ;
#3962 = VERTEX_POINT('',#195370) ;
#3963 = VERTEX_POINT('',#195372) ;
#3964 = VERTEX_POINT('',#195385) ;
#3965 = VERTEX_POINT('',#195387) ;
#3966 = VERTEX_POINT('',#195391) ;
#3967 = VERTEX_POINT('',#195393) ;
#3968 = VERTEX_POINT('',#195397) ;
#3969 = VERTEX_POINT('',#195399) ;
#3970 = VERTEX_POINT('',#195412) ;
#3971 = VERTEX_POINT('',#195414) ;
#3972 = VERTEX_POINT('',#195418) ;
#3973 = VERTEX_POINT('',#195420) ;
#3974 = VERTEX_POINT('',#195424) ;
#3975 = VERTEX_POINT('',#195426) ;
#3976 = VERTEX_POINT('',#195439) ;
#3977 = VERTEX_POINT('',#195441) ;
#3978 = VERTEX_POINT('',#195445) ;
#3979 = VERTEX_POINT('',#195447) ;
#3980 = VERTEX_POINT('',#195451) ;
#3981 = VERTEX_POINT('',#195453) ;
#3982 = VERTEX_POINT('',#195466) ;
#3983 = VERTEX_POINT('',#195468) ;
#3984 = VERTEX_POINT('',#195472) ;
#3985 = VERTEX_POINT('',#195474) ;
#3986 = VERTEX_POINT('',#195478) ;
#3987 = VERTEX_POINT('',#195480) ;
#3988 = VERTEX_POINT('',#195493) ;
#3989 = VERTEX_POINT('',#195495) ;
#3990 = VERTEX_POINT('',#195499) ;
#3991 = VERTEX_POINT('',#195501) ;
#3992 = VERTEX_POINT('',#195505) ;
#3993 = VERTEX_POINT('',#195507) ;
#3994 = VERTEX_POINT('',#195520) ;
#3995 = VERTEX_POINT('',#195522) ;
#3996 = VERTEX_POINT('',#195526) ;
#3997 = VERTEX_POINT('',#195528) ;
#3998 = VERTEX_POINT('',#195532) ;
#3999 = VERTEX_POINT('',#195534) ;
#4000 = VERTEX_POINT('',#195547) ;
#4001 = VERTEX_POINT('',#195549) ;
#4002 = VERTEX_POINT('',#195553) ;
#4003 = VERTEX_POINT('',#195555) ;
#4004 = VERTEX_POINT('',#195559) ;
#4005 = VERTEX_POINT('',#195561) ;
#4006 = VERTEX_POINT('',#195574) ;
#4007 = VERTEX_POINT('',#195576) ;
#4008 = VERTEX_POINT('',#195580) ;
#4009 = VERTEX_POINT('',#195582) ;
#4010 = VERTEX_POINT('',#195586) ;
#4011 = VERTEX_POINT('',#195588) ;
#4012 = VERTEX_POINT('',#195601) ;
#4013 = VERTEX_POINT('',#195603) ;
#4014 = VERTEX_POINT('',#195607) ;
#4015 = VERTEX_POINT('',#195609) ;
#4016 = VERTEX_POINT('',#195613) ;
#4017 = VERTEX_POINT('',#195615) ;
#4018 = VERTEX_POINT('',#195628) ;
#4019 = VERTEX_POINT('',#195630) ;
#4020 = VERTEX_POINT('',#195634) ;
#4021 = VERTEX_POINT('',#195636) ;
#4022 = VERTEX_POINT('',#195640) ;
#4023 = VERTEX_POINT('',#195642) ;
#4024 = VERTEX_POINT('',#195655) ;
#4025 = VERTEX_POINT('',#195657) ;
#4026 = VERTEX_POINT('',#195661) ;
#4027 = VERTEX_POINT('',#195663) ;
#4028 = VERTEX_POINT('',#195667) ;
#4029 = VERTEX_POINT('',#195669) ;
#4030 = VERTEX_POINT('',#195682) ;
#4031 = VERTEX_POINT('',#195684) ;
#4032 = VERTEX_POINT('',#195688) ;
#4033 = VERTEX_POINT('',#195690) ;
#4034 = VERTEX_POINT('',#195694) ;
#4035 = VERTEX_POINT('',#195696) ;
#4036 = VERTEX_POINT('',#195709) ;
#4037 = VERTEX_POINT('',#195711) ;
#4038 = VERTEX_POINT('',#195715) ;
#4039 = VERTEX_POINT('',#195717) ;
#4040 = VERTEX_POINT('',#195721) ;
#4041 = VERTEX_POINT('',#195723) ;
#4042 = VERTEX_POINT('',#195736) ;
#4043 = VERTEX_POINT('',#195738) ;
#4044 = VERTEX_POINT('',#195742) ;
#4045 = VERTEX_POINT('',#195744) ;
#4046 = VERTEX_POINT('',#195748) ;
#4047 = VERTEX_POINT('',#195750) ;
#4048 = VERTEX_POINT('',#195763) ;
#4049 = VERTEX_POINT('',#195765) ;
#4050 = VERTEX_POINT('',#195769) ;
#4051 = VERTEX_POINT('',#195771) ;
#4052 = VERTEX_POINT('',#195775) ;
#4053 = VERTEX_POINT('',#195777) ;
#4054 = VERTEX_POINT('',#195790) ;
#4055 = VERTEX_POINT('',#195792) ;
#4056 = VERTEX_POINT('',#195796) ;
#4057 = VERTEX_POINT('',#195798) ;
#4058 = VERTEX_POINT('',#195802) ;
#4059 = VERTEX_POINT('',#195804) ;
#4060 = VERTEX_POINT('',#195817) ;
#4061 = VERTEX_POINT('',#195819) ;
#4062 = VERTEX_POINT('',#195823) ;
#4063 = VERTEX_POINT('',#195825) ;
#4064 = VERTEX_POINT('',#195829) ;
#4065 = VERTEX_POINT('',#195831) ;
#4066 = VERTEX_POINT('',#195844) ;
#4067 = VERTEX_POINT('',#195846) ;
#4068 = VERTEX_POINT('',#195850) ;
#4069 = VERTEX_POINT('',#195852) ;
#4070 = VERTEX_POINT('',#195856) ;
#4071 = VERTEX_POINT('',#195858) ;
#4072 = VERTEX_POINT('',#195871) ;
#4073 = VERTEX_POINT('',#195873) ;
#4074 = VERTEX_POINT('',#195877) ;
#4075 = VERTEX_POINT('',#195879) ;
#4076 = VERTEX_POINT('',#195883) ;
#4077 = VERTEX_POINT('',#195885) ;
#4078 = VERTEX_POINT('',#195898) ;
#4079 = VERTEX_POINT('',#195900) ;
#4080 = VERTEX_POINT('',#195904) ;
#4081 = VERTEX_POINT('',#195906) ;
#4082 = VERTEX_POINT('',#195910) ;
#4083 = VERTEX_POINT('',#195912) ;
#4084 = VERTEX_POINT('',#195925) ;
#4085 = VERTEX_POINT('',#195927) ;
#4086 = VERTEX_POINT('',#195931) ;
#4087 = VERTEX_POINT('',#195933) ;
#4088 = VERTEX_POINT('',#195937) ;
#4089 = VERTEX_POINT('',#195939) ;
#4090 = VERTEX_POINT('',#195952) ;
#4091 = VERTEX_POINT('',#195954) ;
#4092 = VERTEX_POINT('',#195958) ;
#4093 = VERTEX_POINT('',#195960) ;
#4094 = VERTEX_POINT('',#195964) ;
#4095 = VERTEX_POINT('',#195966) ;
#4096 = VERTEX_POINT('',#195979) ;
#4097 = VERTEX_POINT('',#195981) ;
#4098 = VERTEX_POINT('',#195985) ;
#4099 = VERTEX_POINT('',#195987) ;
#4100 = VERTEX_POINT('',#195991) ;
#4101 = VERTEX_POINT('',#195993) ;
#4102 = VERTEX_POINT('',#196006) ;
#4103 = VERTEX_POINT('',#196008) ;
#4104 = VERTEX_POINT('',#196012) ;
#4105 = VERTEX_POINT('',#196014) ;
#4106 = VERTEX_POINT('',#196018) ;
#4107 = VERTEX_POINT('',#196020) ;
#4108 = VERTEX_POINT('',#196033) ;
#4109 = VERTEX_POINT('',#196035) ;
#4110 = VERTEX_POINT('',#196039) ;
#4111 = VERTEX_POINT('',#196041) ;
#4112 = VERTEX_POINT('',#196045) ;
#4113 = VERTEX_POINT('',#196047) ;
#4114 = VERTEX_POINT('',#196060) ;
#4115 = VERTEX_POINT('',#196062) ;
#4116 = VERTEX_POINT('',#196066) ;
#4117 = VERTEX_POINT('',#196068) ;
#4118 = VERTEX_POINT('',#196072) ;
#4119 = VERTEX_POINT('',#196074) ;
#4120 = VERTEX_POINT('',#196087) ;
#4121 = VERTEX_POINT('',#196089) ;
#4122 = VERTEX_POINT('',#196093) ;
#4123 = VERTEX_POINT('',#196095) ;
#4124 = VERTEX_POINT('',#196099) ;
#4125 = VERTEX_POINT('',#196101) ;
#4126 = VERTEX_POINT('',#196114) ;
#4127 = VERTEX_POINT('',#196116) ;
#4128 = VERTEX_POINT('',#196120) ;
#4129 = VERTEX_POINT('',#196122) ;
#4130 = VERTEX_POINT('',#196126) ;
#4131 = VERTEX_POINT('',#196128) ;
#4132 = VERTEX_POINT('',#196141) ;
#4133 = VERTEX_POINT('',#196143) ;
#4134 = VERTEX_POINT('',#196147) ;
#4135 = VERTEX_POINT('',#196149) ;
#4136 = VERTEX_POINT('',#196153) ;
#4137 = VERTEX_POINT('',#196155) ;
#4138 = VERTEX_POINT('',#196168) ;
#4139 = VERTEX_POINT('',#196170) ;
#4140 = VERTEX_POINT('',#196174) ;
#4141 = VERTEX_POINT('',#196176) ;
#4142 = VERTEX_POINT('',#196180) ;
#4143 = VERTEX_POINT('',#196182) ;
#4144 = VERTEX_POINT('',#196195) ;
#4145 = VERTEX_POINT('',#196197) ;
#4146 = VERTEX_POINT('',#196201) ;
#4147 = VERTEX_POINT('',#196203) ;
#4148 = VERTEX_POINT('',#196207) ;
#4149 = VERTEX_POINT('',#196209) ;
#4150 = VERTEX_POINT('',#196222) ;
#4151 = VERTEX_POINT('',#196224) ;
#4152 = VERTEX_POINT('',#196228) ;
#4153 = VERTEX_POINT('',#196230) ;
#4154 = VERTEX_POINT('',#196234) ;
#4155 = VERTEX_POINT('',#196236) ;
#4156 = VERTEX_POINT('',#196249) ;
#4157 = VERTEX_POINT('',#196251) ;
#4158 = VERTEX_POINT('',#196255) ;
#4159 = VERTEX_POINT('',#196257) ;
#4160 = VERTEX_POINT('',#196261) ;
#4161 = VERTEX_POINT('',#196263) ;
#4162 = VERTEX_POINT('',#196276) ;
#4163 = VERTEX_POINT('',#196278) ;
#4164 = VERTEX_POINT('',#196282) ;
#4165 = VERTEX_POINT('',#196284) ;
#4166 = VERTEX_POINT('',#196288) ;
#4167 = VERTEX_POINT('',#196290) ;
#4168 = VERTEX_POINT('',#196303) ;
#4169 = VERTEX_POINT('',#196305) ;
#4170 = VERTEX_POINT('',#196309) ;
#4171 = VERTEX_POINT('',#196311) ;
#4172 = VERTEX_POINT('',#196315) ;
#4173 = VERTEX_POINT('',#196317) ;
#4174 = VERTEX_POINT('',#196330) ;
#4175 = VERTEX_POINT('',#196332) ;
#4176 = VERTEX_POINT('',#196336) ;
#4177 = VERTEX_POINT('',#196338) ;
#4178 = VERTEX_POINT('',#196342) ;
#4179 = VERTEX_POINT('',#196344) ;
#4180 = VERTEX_POINT('',#196357) ;
#4181 = VERTEX_POINT('',#196359) ;
#4182 = VERTEX_POINT('',#196363) ;
#4183 = VERTEX_POINT('',#196365) ;
#4184 = VERTEX_POINT('',#196369) ;
#4185 = VERTEX_POINT('',#196371) ;
#4186 = VERTEX_POINT('',#196384) ;
#4187 = VERTEX_POINT('',#196386) ;
#4188 = VERTEX_POINT('',#196390) ;
#4189 = VERTEX_POINT('',#196392) ;
#4190 = VERTEX_POINT('',#196396) ;
#4191 = VERTEX_POINT('',#196398) ;
#4192 = VERTEX_POINT('',#196411) ;
#4193 = VERTEX_POINT('',#196413) ;
#4194 = VERTEX_POINT('',#196417) ;
#4195 = VERTEX_POINT('',#196419) ;
#4196 = VERTEX_POINT('',#196423) ;
#4197 = VERTEX_POINT('',#196425) ;
#4198 = VERTEX_POINT('',#196438) ;
#4199 = VERTEX_POINT('',#196440) ;
#4200 = VERTEX_POINT('',#196444) ;
#4201 = VERTEX_POINT('',#196446) ;
#4202 = VERTEX_POINT('',#196450) ;
#4203 = VERTEX_POINT('',#196452) ;
#4204 = VERTEX_POINT('',#196465) ;
#4205 = VERTEX_POINT('',#196467) ;
#4206 = VERTEX_POINT('',#196474) ;
#4207 = VERTEX_POINT('',#196475) ;
#4208 = VERTEX_POINT('',#196477) ;
#4209 = VERTEX_POINT('',#196479) ;
#4210 = VERTEX_POINT('',#196481) ;
#4211 = VERTEX_POINT('',#196483) ;
#4212 = VERTEX_POINT('',#196485) ;
#4213 = VERTEX_POINT('',#196487) ;
#4214 = VERTEX_POINT('',#196490) ;
#4215 = VERTEX_POINT('',#196492) ;
#4216 = VERTEX_POINT('',#196493) ;
#4217 = VERTEX_POINT('',#196495) ;
#4218 = VERTEX_POINT('',#196497) ;
#4219 = VERTEX_POINT('',#196499) ;
#4220 = VERTEX_POINT('',#196501) ;
#4221 = VERTEX_POINT('',#196503) ;
#4222 = VERTEX_POINT('',#196505) ;
#4223 = VERTEX_POINT('',#196508) ;
#4224 = VERTEX_POINT('',#196509) ;
#4225 = VERTEX_POINT('',#196511) ;
#4226 = VERTEX_POINT('',#196513) ;
#4227 = VERTEX_POINT('',#196515) ;
#4228 = VERTEX_POINT('',#196517) ;
#4229 = VERTEX_POINT('',#196519) ;
#4230 = VERTEX_POINT('',#196521) ;
#4231 = VERTEX_POINT('',#196524) ;
#4232 = VERTEX_POINT('',#196525) ;
#4233 = VERTEX_POINT('',#196527) ;
#4234 = VERTEX_POINT('',#196529) ;
#4235 = VERTEX_POINT('',#196531) ;
#4236 = VERTEX_POINT('',#196533) ;
#4237 = VERTEX_POINT('',#196535) ;
#4238 = VERTEX_POINT('',#196537) ;
#4239 = VERTEX_POINT('',#196540) ;
#4240 = VERTEX_POINT('',#196541) ;
#4241 = VERTEX_POINT('',#196543) ;
#4242 = VERTEX_POINT('',#196545) ;
#4243 = VERTEX_POINT('',#196547) ;
#4244 = VERTEX_POINT('',#196549) ;
#4245 = VERTEX_POINT('',#196551) ;
#4246 = VERTEX_POINT('',#196553) ;
#4247 = VERTEX_POINT('',#196557) ;
#4248 = VERTEX_POINT('',#196560) ;
#4249 = VERTEX_POINT('',#196562) ;
#4250 = VERTEX_POINT('',#196566) ;
#4251 = VERTEX_POINT('',#196570) ;
#4252 = VERTEX_POINT('',#196574) ;
#4253 = VERTEX_POINT('',#196578) ;
#4254 = VERTEX_POINT('',#196582) ;
#4255 = VERTEX_POINT('',#196586) ;
#4256 = VERTEX_POINT('',#196592) ;
#4257 = VERTEX_POINT('',#196596) ;
#4258 = VERTEX_POINT('',#196598) ;
#4259 = VERTEX_POINT('',#196602) ;
#4260 = VERTEX_POINT('',#196606) ;
#4261 = VERTEX_POINT('',#196610) ;
#4262 = VERTEX_POINT('',#196614) ;
#4263 = VERTEX_POINT('',#196618) ;
#4264 = VERTEX_POINT('',#196622) ;
#4265 = VERTEX_POINT('',#196628) ;
#4266 = VERTEX_POINT('',#196630) ;
#4267 = VERTEX_POINT('',#196634) ;
#4268 = VERTEX_POINT('',#196638) ;
#4269 = VERTEX_POINT('',#196642) ;
#4270 = VERTEX_POINT('',#196646) ;
#4271 = VERTEX_POINT('',#196650) ;
#4272 = VERTEX_POINT('',#196654) ;
#4273 = VERTEX_POINT('',#196660) ;
#4274 = VERTEX_POINT('',#196662) ;
#4275 = VERTEX_POINT('',#196666) ;
#4276 = VERTEX_POINT('',#196670) ;
#4277 = VERTEX_POINT('',#196674) ;
#4278 = VERTEX_POINT('',#196678) ;
#4279 = VERTEX_POINT('',#196682) ;
#4280 = VERTEX_POINT('',#196686) ;
#4281 = VERTEX_POINT('',#196692) ;
#4282 = VERTEX_POINT('',#196694) ;
#4283 = VERTEX_POINT('',#196698) ;
#4284 = VERTEX_POINT('',#196702) ;
#4285 = VERTEX_POINT('',#196706) ;
#4286 = VERTEX_POINT('',#196710) ;
#4287 = VERTEX_POINT('',#196714) ;
#4288 = VERTEX_POINT('',#196718) ;
#4289 = VERTEX_POINT('',#196724) ;
#4290 = VERTEX_POINT('',#196728) ;
#4291 = VERTEX_POINT('',#196730) ;
#4292 = EDGE_CURVE('',#3447,#3448,#3269,.T.) ;
#4293 = EDGE_CURVE('',#3448,#3449,#1863,.T.) ;
#4294 = EDGE_CURVE('',#3449,#3450,#3270,.T.) ;
#4295 = EDGE_CURVE('',#3450,#3449,#3271,.T.) ;
#4296 = EDGE_CURVE('',#3448,#3447,#3272,.T.) ;
#4297 = EDGE_CURVE('',#3451,#3452,#3273,.T.) ;
#4298 = EDGE_CURVE('',#3452,#3453,#1864,.T.) ;
#4299 = EDGE_CURVE('',#3453,#3454,#3274,.T.) ;
#4300 = EDGE_CURVE('',#3454,#3453,#3275,.T.) ;
#4301 = EDGE_CURVE('',#3452,#3451,#3276,.T.) ;
#4302 = EDGE_CURVE('',#3447,#3455,#1865,.T.) ;
#4303 = EDGE_CURVE('',#3455,#3455,#3277,.T.) ;
#4304 = EDGE_CURVE('',#3450,#3456,#1866,.T.) ;
#4305 = EDGE_CURVE('',#3456,#3456,#3278,.T.) ;
#4306 = EDGE_CURVE('',#3451,#3457,#1867,.T.) ;
#4307 = EDGE_CURVE('',#3457,#3457,#3279,.T.) ;
#4308 = EDGE_CURVE('',#3454,#3458,#1868,.T.) ;
#4309 = EDGE_CURVE('',#3458,#3458,#3280,.T.) ;
#4310 = EDGE_CURVE('',#3459,#3459,#612,.T.) ;
#4311 = EDGE_CURVE('',#3459,#3460,#1869,.T.) ;
#4312 = EDGE_CURVE('',#3460,#3460,#613,.T.) ;
#4313 = EDGE_CURVE('',#3461,#3461,#3281,.T.) ;
#4314 = EDGE_CURVE('',#3462,#3462,#3282,.T.) ;
#4315 = EDGE_CURVE('',#3459,#3461,#1870,.T.) ;
#4316 = EDGE_CURVE('',#3460,#3462,#1871,.T.) ;
#4317 = EDGE_CURVE('',#3463,#3464,#1872,.T.) ;
#4318 = EDGE_CURVE('',#3464,#3465,#3283,.T.) ;
#4319 = EDGE_CURVE('',#3465,#3466,#3284,.T.) ;
#4320 = EDGE_CURVE('',#3466,#3467,#614,.T.) ;
#4321 = EDGE_CURVE('',#3467,#3468,#3285,.T.) ;
#4322 = EDGE_CURVE('',#3468,#3463,#3286,.T.) ;
#4323 = EDGE_CURVE('',#3469,#3470,#1873,.T.) ;
#4324 = EDGE_CURVE('',#3470,#3471,#3287,.T.) ;
#4325 = EDGE_CURVE('',#3471,#3464,#3288,.T.) ;
#4326 = EDGE_CURVE('',#3463,#3472,#3289,.T.) ;
#4327 = EDGE_CURVE('',#3472,#3469,#3290,.T.) ;
#4328 = EDGE_CURVE('',#3473,#3474,#1874,.T.) ;
#4329 = EDGE_CURVE('',#3474,#3475,#3291,.T.) ;
#4330 = EDGE_CURVE('',#3475,#3470,#3292,.T.) ;
#4331 = EDGE_CURVE('',#3469,#3476,#3293,.T.) ;
#4332 = EDGE_CURVE('',#3476,#3473,#3294,.T.) ;
#4333 = EDGE_CURVE('',#3477,#3478,#1875,.T.) ;
#4334 = EDGE_CURVE('',#3478,#3479,#3295,.T.) ;
#4335 = EDGE_CURVE('',#3479,#3474,#3296,.T.) ;
#4336 = EDGE_CURVE('',#3473,#3480,#3297,.T.) ;
#4337 = EDGE_CURVE('',#3480,#3477,#3298,.T.) ;
#4338 = EDGE_CURVE('',#3481,#3482,#1876,.T.) ;
#4339 = EDGE_CURVE('',#3481,#3483,#3299,.T.) ;
#4340 = EDGE_CURVE('',#3484,#3483,#3300,.T.) ;
#4341 = EDGE_CURVE('',#3484,#3482,#3301,.T.) ;
#4342 = EDGE_CURVE('',#3485,#3486,#1877,.T.) ;
#4343 = EDGE_CURVE('',#3487,#3486,#3302,.T.) ;
#4344 = EDGE_CURVE('',#3487,#3488,#615,.T.) ;
#4345 = EDGE_CURVE('',#3485,#3488,#3303,.T.) ;
#4346 = EDGE_CURVE('',#3489,#3490,#1878,.T.) ;
#4347 = EDGE_CURVE('',#3486,#3490,#3304,.T.) ;
#4348 = EDGE_CURVE('',#3489,#3485,#3305,.T.) ;
#4349 = EDGE_CURVE('',#3491,#3492,#1879,.T.) ;
#4350 = EDGE_CURVE('',#3490,#3492,#3306,.T.) ;
#4351 = EDGE_CURVE('',#3491,#3489,#3307,.T.) ;
#4352 = EDGE_CURVE('',#3493,#3494,#1880,.T.) ;
#4353 = EDGE_CURVE('',#3492,#3494,#3308,.T.) ;
#4354 = EDGE_CURVE('',#3493,#3491,#3309,.T.) ;
#4355 = EDGE_CURVE('',#3495,#3496,#1881,.T.) ;
#4356 = EDGE_CURVE('',#3497,#3495,#3310,.T.) ;
#4357 = EDGE_CURVE('',#3497,#3498,#3311,.T.) ;
#4358 = EDGE_CURVE('',#3496,#3498,#3312,.T.) ;
#4359 = EDGE_CURVE('',#3499,#3499,#616,.T.) ;
#4360 = EDGE_CURVE('',#3499,#3500,#1882,.T.) ;
#4361 = EDGE_CURVE('',#3500,#3500,#617,.T.) ;
#4362 = EDGE_CURVE('',#3501,#3501,#3313,.T.) ;
#4363 = EDGE_CURVE('',#3502,#3502,#3314,.T.) ;
#4364 = EDGE_CURVE('',#3503,#3503,#3315,.T.) ;
#4365 = EDGE_CURVE('',#3504,#3504,#3316,.T.) ;
#4366 = EDGE_CURVE('',#3505,#3505,#3317,.T.) ;
#4367 = EDGE_CURVE('',#3466,#3506,#3318,.T.) ;
#4368 = EDGE_CURVE('',#3506,#3467,#3319,.T.) ;
#4369 = EDGE_CURVE('',#3507,#3507,#3320,.T.) ;
#4370 = EDGE_CURVE('',#3508,#3487,#3321,.T.) ;
#4371 = EDGE_CURVE('',#3488,#3508,#3322,.T.) ;
#4372 = EDGE_CURVE('',#3499,#3505,#1883,.T.) ;
#4373 = EDGE_CURVE('',#3500,#3507,#1884,.T.) ;
#4374 = EDGE_CURVE('',#3509,#3510,#1885,.T.) ;
#4375 = EDGE_CURVE('',#3511,#3510,#618,.T.) ;
#4376 = EDGE_CURVE('',#3510,#3511,#619,.T.) ;
#4377 = EDGE_CURVE('',#3512,#3513,#620,.T.) ;
#4378 = EDGE_CURVE('',#3513,#3514,#1886,.T.) ;
#4379 = EDGE_CURVE('',#3513,#3512,#621,.T.) ;
#4380 = EDGE_CURVE('',#3515,#3516,#3323,.T.) ;
#4381 = EDGE_CURVE('',#3516,#3517,#3324,.T.) ;
#4382 = EDGE_CURVE('',#3517,#3515,#3325,.T.) ;
#4383 = EDGE_CURVE('',#3518,#3519,#3326,.T.) ;
#4384 = EDGE_CURVE('',#3519,#3520,#3327,.T.) ;
#4385 = EDGE_CURVE('',#3520,#3518,#3328,.T.) ;
#4386 = EDGE_CURVE('',#3519,#3521,#1887,.T.) ;
#4387 = EDGE_CURVE('',#3521,#3522,#622,.T.) ;
#4388 = EDGE_CURVE('',#3522,#3523,#1888,.T.) ;
#4389 = EDGE_CURVE('',#3520,#3523,#3329,.T.) ;
#4390 = EDGE_CURVE('',#3494,#3496,#3330,.T.) ;
#4391 = EDGE_CURVE('',#3495,#3493,#3331,.T.) ;
#4392 = EDGE_CURVE('',#3524,#3518,#3332,.T.) ;
#4393 = EDGE_CURVE('',#3523,#3497,#3333,.T.) ;
#4394 = EDGE_CURVE('',#3524,#3508,#3334,.T.) ;
#4395 = EDGE_CURVE('',#3516,#3525,#1889,.T.) ;
#4396 = EDGE_CURVE('',#3525,#3517,#623,.T.) ;
#4397 = EDGE_CURVE('',#3482,#3526,#3335,.T.) ;
#4398 = EDGE_CURVE('',#3526,#3478,#3336,.T.) ;
#4399 = EDGE_CURVE('',#3477,#3527,#3337,.T.) ;
#4400 = EDGE_CURVE('',#3527,#3481,#3338,.T.) ;
#4401 = EDGE_CURVE('',#3528,#3529,#3339,.T.) ;
#4402 = EDGE_CURVE('',#3528,#3530,#3340,.T.) ;
#4403 = EDGE_CURVE('',#3531,#3530,#3341,.T.) ;
#4404 = EDGE_CURVE('',#3531,#3532,#3342,.T.) ;
#4405 = EDGE_CURVE('',#3532,#3533,#624,.T.) ;
#4406 = EDGE_CURVE('',#3534,#3533,#3343,.T.) ;
#4407 = EDGE_CURVE('',#3535,#3534,#3344,.T.) ;
#4408 = EDGE_CURVE('',#3535,#3536,#625,.T.) ;
#4409 = EDGE_CURVE('',#3529,#3536,#3345,.T.) ;
#4410 = EDGE_CURVE('',#3511,#3529,#1890,.T.) ;
#4411 = EDGE_CURVE('',#3531,#3537,#3346,.T.) ;
#4412 = EDGE_CURVE('',#3537,#3532,#3347,.T.) ;
#4413 = EDGE_CURVE('',#3538,#3539,#3348,.T.) ;
#4414 = EDGE_CURVE('',#3540,#3539,#3349,.T.) ;
#4415 = EDGE_CURVE('',#3540,#3541,#3350,.T.) ;
#4416 = EDGE_CURVE('',#3541,#3483,#3351,.T.) ;
#4417 = EDGE_CURVE('',#3538,#3506,#3352,.T.) ;
#4418 = EDGE_CURVE('',#3539,#3542,#3353,.T.) ;
#4419 = EDGE_CURVE('',#3542,#3540,#3354,.T.) ;
#4420 = EDGE_CURVE('',#3537,#3533,#1891,.T.) ;
#4421 = EDGE_CURVE('',#3542,#3536,#1892,.T.) ;
#4422 = EDGE_CURVE('',#3535,#3541,#1893,.T.) ;
#4423 = EDGE_CURVE('',#3543,#3524,#3355,.T.) ;
#4424 = EDGE_CURVE('',#3498,#3544,#3356,.T.) ;
#4425 = EDGE_CURVE('',#3544,#3543,#3357,.T.) ;
#4426 = EDGE_CURVE('',#3512,#3545,#1894,.T.) ;
#4427 = EDGE_CURVE('',#3545,#3543,#3358,.F.) ;
#4428 = EDGE_CURVE('',#3544,#3515,#3359,.T.) ;
#4429 = EDGE_CURVE('',#3525,#3546,#3360,.T.) ;
#4430 = EDGE_CURVE('',#3546,#3522,#3361,.T.) ;
#4431 = EDGE_CURVE('',#3521,#3545,#3362,.F.) ;
#4432 = EDGE_CURVE('',#3528,#3538,#3363,.T.) ;
#4433 = EDGE_CURVE('',#3484,#3530,#3364,.T.) ;
#4434 = EDGE_CURVE('',#3547,#3548,#3365,.T.) ;
#4435 = EDGE_CURVE('',#3548,#3545,#1895,.T.) ;
#4436 = EDGE_CURVE('',#3548,#3547,#3366,.T.) ;
#4437 = EDGE_CURVE('',#3547,#3501,#1896,.T.) ;
#4438 = EDGE_CURVE('',#3546,#3549,#1897,.T.) ;
#4439 = EDGE_CURVE('',#3549,#3550,#3367,.T.) ;
#4440 = EDGE_CURVE('',#3550,#3549,#3368,.T.) ;
#4441 = EDGE_CURVE('',#3550,#3502,#1898,.T.) ;
#4442 = EDGE_CURVE('',#3529,#3551,#1899,.T.) ;
#4443 = EDGE_CURVE('',#3551,#3552,#3369,.T.) ;
#4444 = EDGE_CURVE('',#3552,#3551,#3370,.T.) ;
#4445 = EDGE_CURVE('',#3553,#3554,#3371,.T.) ;
#4446 = EDGE_CURVE('',#3554,#3534,#1900,.T.) ;
#4447 = EDGE_CURVE('',#3554,#3553,#3372,.T.) ;
#4448 = EDGE_CURVE('',#3553,#3504,#1901,.T.) ;
#4449 = EDGE_CURVE('',#3552,#3503,#1902,.T.) ;
#4450 = EDGE_CURVE('',#3555,#3555,#626,.T.) ;
#4451 = EDGE_CURVE('',#3555,#3556,#1903,.T.) ;
#4452 = EDGE_CURVE('',#3557,#3556,#627,.T.) ;
#4453 = EDGE_CURVE('',#3556,#3557,#628,.T.) ;
#4454 = EDGE_CURVE('',#3558,#3558,#3373,.T.) ;
#4455 = EDGE_CURVE('',#3557,#3558,#1904,.T.) ;
#4456 = EDGE_CURVE('',#3559,#3559,#629,.T.) ;
#4457 = EDGE_CURVE('',#3559,#3560,#1905,.T.) ;
#4458 = EDGE_CURVE('',#3560,#3560,#630,.T.) ;
#4459 = EDGE_CURVE('',#3561,#3562,#1906,.T.) ;
#4460 = EDGE_CURVE('',#3563,#3561,#3374,.T.) ;
#4461 = EDGE_CURVE('',#3563,#3564,#631,.T.) ;
#4462 = EDGE_CURVE('',#3562,#3564,#3375,.T.) ;
#4463 = EDGE_CURVE('',#3565,#3566,#1907,.T.) ;
#4464 = EDGE_CURVE('',#3561,#3565,#3376,.T.) ;
#4465 = EDGE_CURVE('',#3566,#3562,#3377,.T.) ;
#4466 = EDGE_CURVE('',#3567,#3568,#1908,.T.) ;
#4467 = EDGE_CURVE('',#3565,#3567,#3378,.T.) ;
#4468 = EDGE_CURVE('',#3568,#3566,#3379,.T.) ;
#4469 = EDGE_CURVE('',#3569,#3570,#1909,.T.) ;
#4470 = EDGE_CURVE('',#3567,#3569,#3380,.T.) ;
#4471 = EDGE_CURVE('',#3570,#3568,#3381,.T.) ;
#4472 = EDGE_CURVE('',#3571,#3570,#3382,.T.) ;
#4473 = EDGE_CURVE('',#3572,#3571,#632,.T.) ;
#4474 = EDGE_CURVE('',#3569,#3572,#3383,.T.) ;
#4475 = EDGE_CURVE('',#3573,#3574,#1910,.T.) ;
#4476 = EDGE_CURVE('',#3574,#3574,#633,.T.) ;
#4477 = EDGE_CURVE('',#3572,#3575,#3384,.T.) ;
#4478 = EDGE_CURVE('',#3576,#3571,#3385,.T.) ;
#4479 = EDGE_CURVE('',#3575,#3576,#3386,.T.) ;
#4480 = EDGE_CURVE('',#3575,#3574,#1911,.T.) ;
#4481 = EDGE_CURVE('',#3576,#3577,#3387,.T.) ;
#4482 = EDGE_CURVE('',#3563,#3577,#3388,.T.) ;
#4483 = EDGE_CURVE('',#3578,#3564,#3389,.F.) ;
#4484 = EDGE_CURVE('',#3577,#3578,#3390,.F.) ;
#4485 = EDGE_CURVE('',#3579,#3579,#634,.T.) ;
#4486 = EDGE_CURVE('',#3579,#3578,#1912,.T.) ;
#4487 = EDGE_CURVE('',#3580,#3581,#1913,.T.) ;
#4488 = EDGE_CURVE('',#3581,#3582,#1914,.T.) ;
#4489 = EDGE_CURVE('',#3582,#3583,#1915,.T.) ;
#4490 = EDGE_CURVE('',#3583,#3584,#1916,.T.) ;
#4491 = EDGE_CURVE('',#3584,#3585,#1917,.T.) ;
#4492 = EDGE_CURVE('',#3585,#3580,#1918,.T.) ;
#4493 = EDGE_CURVE('',#3580,#3586,#1919,.T.) ;
#4494 = EDGE_CURVE('',#3586,#3587,#1920,.T.) ;
#4495 = EDGE_CURVE('',#3581,#3587,#1921,.T.) ;
#4496 = EDGE_CURVE('',#3587,#3588,#1922,.T.) ;
#4497 = EDGE_CURVE('',#3582,#3588,#1923,.T.) ;
#4498 = EDGE_CURVE('',#3588,#3589,#1924,.T.) ;
#4499 = EDGE_CURVE('',#3583,#3589,#1925,.T.) ;
#4500 = EDGE_CURVE('',#3589,#3590,#1926,.T.) ;
#4501 = EDGE_CURVE('',#3584,#3590,#1927,.T.) ;
#4502 = EDGE_CURVE('',#3590,#3591,#1928,.T.) ;
#4503 = EDGE_CURVE('',#3585,#3591,#1929,.T.) ;
#4504 = EDGE_CURVE('',#3591,#3586,#1930,.T.) ;
#4505 = EDGE_CURVE('',#3592,#3593,#1931,.T.) ;
#4506 = EDGE_CURVE('',#3594,#3592,#3391,.T.) ;
#4507 = EDGE_CURVE('',#3594,#3595,#635,.T.) ;
#4508 = EDGE_CURVE('',#3593,#3595,#3392,.T.) ;
#4509 = EDGE_CURVE('',#3596,#3597,#1932,.T.) ;
#4510 = EDGE_CURVE('',#3592,#3596,#3393,.T.) ;
#4511 = EDGE_CURVE('',#3597,#3593,#3394,.T.) ;
#4512 = EDGE_CURVE('',#3598,#3599,#1933,.T.) ;
#4513 = EDGE_CURVE('',#3596,#3598,#3395,.T.) ;
#4514 = EDGE_CURVE('',#3599,#3597,#3396,.T.) ;
#4515 = EDGE_CURVE('',#3600,#3601,#1934,.T.) ;
#4516 = EDGE_CURVE('',#3598,#3600,#3397,.T.) ;
#4517 = EDGE_CURVE('',#3601,#3599,#3398,.T.) ;
#4518 = EDGE_CURVE('',#3602,#3601,#3399,.T.) ;
#4519 = EDGE_CURVE('',#3603,#3602,#636,.T.) ;
#4520 = EDGE_CURVE('',#3600,#3603,#3400,.T.) ;
#4521 = EDGE_CURVE('',#3604,#3604,#637,.T.) ;
#4522 = EDGE_CURVE('',#3604,#3605,#1935,.T.) ;
#4523 = EDGE_CURVE('',#3604,#3606,#1936,.T.) ;
#4524 = EDGE_CURVE('',#3603,#3606,#3401,.T.) ;
#4525 = EDGE_CURVE('',#3607,#3602,#3402,.T.) ;
#4526 = EDGE_CURVE('',#3606,#3607,#3403,.T.) ;
#4527 = EDGE_CURVE('',#3607,#3608,#3404,.T.) ;
#4528 = EDGE_CURVE('',#3594,#3608,#3405,.T.) ;
#4529 = EDGE_CURVE('',#3609,#3595,#3406,.F.) ;
#4530 = EDGE_CURVE('',#3608,#3609,#3407,.F.) ;
#4531 = EDGE_CURVE('',#3609,#3610,#1937,.T.) ;
#4532 = EDGE_CURVE('',#3610,#3610,#638,.T.) ;
#4533 = EDGE_CURVE('',#3611,#3612,#1938,.T.) ;
#4534 = EDGE_CURVE('',#3612,#3613,#1939,.T.) ;
#4535 = EDGE_CURVE('',#3613,#3614,#1940,.T.) ;
#4536 = EDGE_CURVE('',#3614,#3615,#1941,.T.) ;
#4537 = EDGE_CURVE('',#3615,#3616,#1942,.T.) ;
#4538 = EDGE_CURVE('',#3616,#3611,#1943,.T.) ;
#4539 = EDGE_CURVE('',#3611,#3617,#1944,.T.) ;
#4540 = EDGE_CURVE('',#3617,#3618,#1945,.T.) ;
#4541 = EDGE_CURVE('',#3612,#3618,#1946,.T.) ;
#4542 = EDGE_CURVE('',#3618,#3619,#1947,.T.) ;
#4543 = EDGE_CURVE('',#3613,#3619,#1948,.T.) ;
#4544 = EDGE_CURVE('',#3619,#3620,#1949,.T.) ;
#4545 = EDGE_CURVE('',#3614,#3620,#1950,.T.) ;
#4546 = EDGE_CURVE('',#3620,#3621,#1951,.T.) ;
#4547 = EDGE_CURVE('',#3615,#3621,#1952,.T.) ;
#4548 = EDGE_CURVE('',#3621,#3622,#1953,.T.) ;
#4549 = EDGE_CURVE('',#3616,#3622,#1954,.T.) ;
#4550 = EDGE_CURVE('',#3622,#3617,#1955,.T.) ;
#4551 = EDGE_CURVE('',#3623,#3624,#639,.T.) ;
#4552 = EDGE_CURVE('',#3624,#3625,#1956,.T.) ;
#4553 = EDGE_CURVE('',#3626,#3625,#640,.T.) ;
#4554 = EDGE_CURVE('',#3623,#3626,#1957,.T.) ;
#4555 = EDGE_CURVE('',#3624,#3627,#641,.T.) ;
#4556 = EDGE_CURVE('',#3627,#3628,#1958,.T.) ;
#4557 = EDGE_CURVE('',#3625,#3628,#642,.T.) ;
#4558 = EDGE_CURVE('',#3627,#3629,#643,.T.) ;
#4559 = EDGE_CURVE('',#3629,#3630,#1959,.T.) ;
#4560 = EDGE_CURVE('',#3628,#3630,#644,.T.) ;
#4561 = EDGE_CURVE('',#3629,#3623,#645,.T.) ;
#4562 = EDGE_CURVE('',#3630,#3626,#646,.T.) ;
#4563 = EDGE_CURVE('',#3631,#3631,#647,.T.) ;
#4564 = EDGE_CURVE('',#3631,#3632,#1960,.T.) ;
#4565 = EDGE_CURVE('',#3632,#3632,#648,.T.) ;
#4566 = EDGE_CURVE('',#3633,#3633,#649,.T.) ;
#4567 = EDGE_CURVE('',#3634,#3635,#650,.T.) ;
#4568 = EDGE_CURVE('',#3636,#3634,#651,.T.) ;
#4569 = EDGE_CURVE('',#3637,#3636,#652,.T.) ;
#4570 = EDGE_CURVE('',#3635,#3637,#653,.T.) ;
#4571 = EDGE_CURVE('',#3638,#3638,#654,.T.) ;
#4572 = EDGE_CURVE('',#3639,#3640,#655,.T.) ;
#4573 = EDGE_CURVE('',#3641,#3639,#656,.T.) ;
#4574 = EDGE_CURVE('',#3642,#3641,#657,.T.) ;
#4575 = EDGE_CURVE('',#3640,#3642,#658,.T.) ;
#4576 = EDGE_CURVE('',#3643,#3643,#3408,.T.) ;
#4577 = EDGE_CURVE('',#3644,#3645,#3409,.T.) ;
#4578 = EDGE_CURVE('',#3645,#3646,#131,.T.) ;
#4579 = EDGE_CURVE('',#3646,#3647,#3410,.T.) ;
#4580 = EDGE_CURVE('',#3647,#3644,#132,.T.) ;
#4581 = EDGE_CURVE('',#3648,#3649,#133,.T.) ;
#4582 = EDGE_CURVE('',#3649,#3650,#3411,.T.) ;
#4583 = EDGE_CURVE('',#3650,#3651,#134,.T.) ;
#4584 = EDGE_CURVE('',#3651,#3648,#3412,.T.) ;
#4585 = EDGE_CURVE('',#3652,#3652,#3413,.T.) ;
#4586 = EDGE_CURVE('',#3653,#3653,#659,.T.) ;
#4587 = EDGE_CURVE('',#3653,#3633,#1961,.T.) ;
#4588 = EDGE_CURVE('',#3635,#3654,#1962,.T.) ;
#4589 = EDGE_CURVE('',#3637,#3655,#1963,.T.) ;
#4590 = EDGE_CURVE('',#3654,#3655,#3414,.T.) ;
#4591 = EDGE_CURVE('',#3636,#3656,#1964,.T.) ;
#4592 = EDGE_CURVE('',#3655,#3656,#660,.T.) ;
#4593 = EDGE_CURVE('',#3634,#3657,#1965,.T.) ;
#4594 = EDGE_CURVE('',#3656,#3657,#3415,.T.) ;
#4595 = EDGE_CURVE('',#3657,#3654,#3416,.T.) ;
#4596 = EDGE_CURVE('',#3658,#3658,#661,.T.) ;
#4597 = EDGE_CURVE('',#3658,#3638,#1966,.T.) ;
#4598 = EDGE_CURVE('',#3640,#3659,#1967,.T.) ;
#4599 = EDGE_CURVE('',#3642,#3660,#1968,.T.) ;
#4600 = EDGE_CURVE('',#3659,#3660,#3417,.T.) ;
#4601 = EDGE_CURVE('',#3641,#3661,#1969,.T.) ;
#4602 = EDGE_CURVE('',#3660,#3661,#662,.T.) ;
#4603 = EDGE_CURVE('',#3639,#3662,#1970,.T.) ;
#4604 = EDGE_CURVE('',#3661,#3662,#663,.T.) ;
#4605 = EDGE_CURVE('',#3662,#3659,#3418,.T.) ;
#4606 = EDGE_CURVE('',#3653,#3652,#1971,.T.) ;
#4607 = EDGE_CURVE('',#3655,#3645,#1972,.T.) ;
#4608 = EDGE_CURVE('',#3644,#3654,#1973,.T.) ;
#4609 = EDGE_CURVE('',#3646,#3656,#1974,.T.) ;
#4610 = EDGE_CURVE('',#3657,#3647,#1975,.T.) ;
#4611 = EDGE_CURVE('',#3658,#3643,#1976,.T.) ;
#4612 = EDGE_CURVE('',#3660,#3649,#1977,.T.) ;
#4613 = EDGE_CURVE('',#3648,#3659,#1978,.T.) ;
#4614 = EDGE_CURVE('',#3661,#3650,#1979,.T.) ;
#4615 = EDGE_CURVE('',#3651,#3662,#1980,.T.) ;
#4616 = EDGE_CURVE('',#3663,#3664,#664,.T.) ;
#4617 = EDGE_CURVE('',#3664,#3665,#1981,.T.) ;
#4618 = EDGE_CURVE('',#3666,#3665,#665,.T.) ;
#4619 = EDGE_CURVE('',#3663,#3666,#1982,.T.) ;
#4620 = EDGE_CURVE('',#3664,#3667,#666,.T.) ;
#4621 = EDGE_CURVE('',#3667,#3668,#1983,.T.) ;
#4622 = EDGE_CURVE('',#3665,#3668,#667,.T.) ;
#4623 = EDGE_CURVE('',#3667,#3669,#668,.T.) ;
#4624 = EDGE_CURVE('',#3669,#3670,#1984,.T.) ;
#4625 = EDGE_CURVE('',#3668,#3670,#669,.T.) ;
#4626 = EDGE_CURVE('',#3669,#3663,#670,.T.) ;
#4627 = EDGE_CURVE('',#3670,#3666,#671,.T.) ;
#4628 = EDGE_CURVE('',#3671,#3671,#672,.T.) ;
#4629 = EDGE_CURVE('',#3672,#3673,#673,.T.) ;
#4630 = EDGE_CURVE('',#3674,#3672,#674,.T.) ;
#4631 = EDGE_CURVE('',#3675,#3674,#675,.T.) ;
#4632 = EDGE_CURVE('',#3673,#3675,#676,.T.) ;
#4633 = EDGE_CURVE('',#3676,#3676,#677,.T.) ;
#4634 = EDGE_CURVE('',#3677,#3678,#678,.T.) ;
#4635 = EDGE_CURVE('',#3679,#3677,#679,.T.) ;
#4636 = EDGE_CURVE('',#3680,#3679,#680,.T.) ;
#4637 = EDGE_CURVE('',#3678,#3680,#681,.T.) ;
#4638 = EDGE_CURVE('',#3681,#3681,#682,.T.) ;
#4639 = EDGE_CURVE('',#3682,#3682,#3419,.T.) ;
#4640 = EDGE_CURVE('',#3683,#3684,#3420,.T.) ;
#4641 = EDGE_CURVE('',#3684,#3685,#135,.T.) ;
#4642 = EDGE_CURVE('',#3685,#3686,#3421,.T.) ;
#4643 = EDGE_CURVE('',#3686,#3683,#136,.T.) ;
#4644 = EDGE_CURVE('',#3687,#3687,#3422,.T.) ;
#4645 = EDGE_CURVE('',#3688,#3689,#137,.T.) ;
#4646 = EDGE_CURVE('',#3689,#3690,#3423,.T.) ;
#4647 = EDGE_CURVE('',#3690,#3691,#138,.T.) ;
#4648 = EDGE_CURVE('',#3691,#3688,#3424,.T.) ;
#4649 = EDGE_CURVE('',#3692,#3692,#3425,.T.) ;
#4650 = EDGE_CURVE('',#3693,#3693,#683,.T.) ;
#4651 = EDGE_CURVE('',#3693,#3671,#1985,.T.) ;
#4652 = EDGE_CURVE('',#3673,#3694,#1986,.T.) ;
#4653 = EDGE_CURVE('',#3675,#3695,#1987,.T.) ;
#4654 = EDGE_CURVE('',#3694,#3695,#3426,.T.) ;
#4655 = EDGE_CURVE('',#3674,#3696,#1988,.T.) ;
#4656 = EDGE_CURVE('',#3695,#3696,#684,.T.) ;
#4657 = EDGE_CURVE('',#3672,#3697,#1989,.T.) ;
#4658 = EDGE_CURVE('',#3696,#3697,#3427,.T.) ;
#4659 = EDGE_CURVE('',#3697,#3694,#3428,.T.) ;
#4660 = EDGE_CURVE('',#3698,#3698,#685,.T.) ;
#4661 = EDGE_CURVE('',#3698,#3676,#1990,.T.) ;
#4662 = EDGE_CURVE('',#3678,#3699,#1991,.T.) ;
#4663 = EDGE_CURVE('',#3680,#3700,#1992,.T.) ;
#4664 = EDGE_CURVE('',#3699,#3700,#3429,.T.) ;
#4665 = EDGE_CURVE('',#3679,#3701,#1993,.T.) ;
#4666 = EDGE_CURVE('',#3700,#3701,#3430,.T.) ;
#4667 = EDGE_CURVE('',#3677,#3702,#1994,.T.) ;
#4668 = EDGE_CURVE('',#3701,#3702,#686,.T.) ;
#4669 = EDGE_CURVE('',#3702,#3699,#3431,.T.) ;
#4670 = EDGE_CURVE('',#3703,#3703,#3432,.T.) ;
#4671 = EDGE_CURVE('',#3703,#3681,#1995,.T.) ;
#4672 = EDGE_CURVE('',#3693,#3692,#1996,.T.) ;
#4673 = EDGE_CURVE('',#3695,#3684,#1997,.T.) ;
#4674 = EDGE_CURVE('',#3683,#3694,#1998,.T.) ;
#4675 = EDGE_CURVE('',#3696,#3685,#1999,.T.) ;
#4676 = EDGE_CURVE('',#3697,#3686,#2000,.T.) ;
#4677 = EDGE_CURVE('',#3698,#3682,#2001,.T.) ;
#4678 = EDGE_CURVE('',#3700,#3689,#2002,.T.) ;
#4679 = EDGE_CURVE('',#3699,#3688,#2003,.T.) ;
#4680 = EDGE_CURVE('',#3701,#3690,#2004,.T.) ;
#4681 = EDGE_CURVE('',#3702,#3691,#2005,.T.) ;
#4682 = EDGE_CURVE('',#3703,#3687,#2006,.T.) ;
#4683 = EDGE_CURVE('',#3704,#3704,#687,.T.) ;
#4684 = EDGE_CURVE('',#3704,#3705,#2007,.T.) ;
#4685 = EDGE_CURVE('',#3705,#3705,#688,.T.) ;
#4686 = EDGE_CURVE('',#3706,#3706,#3433,.T.) ;
#4687 = EDGE_CURVE('',#3707,#3707,#3434,.T.) ;
#4688 = EDGE_CURVE('',#3704,#3706,#2008,.T.) ;
#4689 = EDGE_CURVE('',#3705,#3707,#2009,.T.) ;
#4690 = EDGE_CURVE('',#3708,#3709,#689,.T.) ;
#4691 = EDGE_CURVE('',#3709,#3710,#2010,.T.) ;
#4692 = EDGE_CURVE('',#3711,#3710,#690,.T.) ;
#4693 = EDGE_CURVE('',#3708,#3711,#2011,.T.) ;
#4694 = EDGE_CURVE('',#3709,#3712,#2012,.T.) ;
#4695 = EDGE_CURVE('',#3712,#3713,#2013,.T.) ;
#4696 = EDGE_CURVE('',#3710,#3713,#2014,.T.) ;
#4697 = EDGE_CURVE('',#3712,#3714,#691,.T.) ;
#4698 = EDGE_CURVE('',#3714,#3715,#2015,.T.) ;
#4699 = EDGE_CURVE('',#3713,#3715,#692,.T.) ;
#4700 = EDGE_CURVE('',#3714,#3716,#693,.T.) ;
#4701 = EDGE_CURVE('',#3716,#3717,#2016,.T.) ;
#4702 = EDGE_CURVE('',#3715,#3717,#694,.T.) ;
#4703 = EDGE_CURVE('',#3716,#3718,#2017,.T.) ;
#4704 = EDGE_CURVE('',#3718,#3719,#2018,.T.) ;
#4705 = EDGE_CURVE('',#3717,#3719,#2019,.T.) ;
#4706 = EDGE_CURVE('',#3718,#3720,#2020,.T.) ;
#4707 = EDGE_CURVE('',#3720,#3721,#2021,.T.) ;
#4708 = EDGE_CURVE('',#3719,#3721,#2022,.T.) ;
#4709 = EDGE_CURVE('',#3720,#3722,#695,.T.) ;
#4710 = EDGE_CURVE('',#3722,#3723,#2023,.T.) ;
#4711 = EDGE_CURVE('',#3721,#3723,#696,.T.) ;
#4712 = EDGE_CURVE('',#3722,#3724,#2024,.T.) ;
#4713 = EDGE_CURVE('',#3724,#3725,#2025,.T.) ;
#4714 = EDGE_CURVE('',#3723,#3725,#2026,.T.) ;
#4715 = EDGE_CURVE('',#3724,#3726,#697,.T.) ;
#4716 = EDGE_CURVE('',#3726,#3727,#2027,.T.) ;
#4717 = EDGE_CURVE('',#3725,#3727,#698,.T.) ;
#4718 = EDGE_CURVE('',#3726,#3728,#699,.T.) ;
#4719 = EDGE_CURVE('',#3728,#3729,#2028,.T.) ;
#4720 = EDGE_CURVE('',#3727,#3729,#700,.T.) ;
#4721 = EDGE_CURVE('',#3728,#3730,#2029,.T.) ;
#4722 = EDGE_CURVE('',#3730,#3731,#2030,.T.) ;
#4723 = EDGE_CURVE('',#3729,#3731,#2031,.T.) ;
#4724 = EDGE_CURVE('',#3730,#3708,#701,.T.) ;
#4725 = EDGE_CURVE('',#3731,#3711,#702,.T.) ;
#4726 = EDGE_CURVE('',#3732,#3732,#703,.T.) ;
#4727 = EDGE_CURVE('',#3733,#3733,#704,.T.) ;
#4728 = EDGE_CURVE('',#3734,#3734,#705,.T.) ;
#4729 = EDGE_CURVE('',#3735,#3735,#706,.T.) ;
#4730 = EDGE_CURVE('',#3734,#3732,#2032,.T.) ;
#4731 = EDGE_CURVE('',#3733,#3735,#2033,.T.) ;
#4732 = EDGE_CURVE('',#3736,#3737,#2034,.T.) ;
#4733 = EDGE_CURVE('',#3736,#3736,#139,.T.) ;
#4734 = EDGE_CURVE('',#3738,#3738,#140,.T.) ;
#4735 = EDGE_CURVE('',#3739,#3738,#707,.T.) ;
#4736 = EDGE_CURVE('',#3740,#3740,#141,.T.) ;
#4737 = EDGE_CURVE('',#3738,#3740,#2035,.T.) ;
#4738 = EDGE_CURVE('',#3741,#3741,#142,.T.) ;
#4739 = EDGE_CURVE('',#3740,#3741,#17,.T.) ;
#4740 = EDGE_CURVE('',#3742,#3742,#143,.T.) ;
#4741 = EDGE_CURVE('',#3741,#3742,#2036,.T.) ;
#4742 = EDGE_CURVE('',#3742,#3736,#2037,.T.) ;
#4743 = EDGE_CURVE('',#3743,#3743,#144,.T.) ;
#4744 = EDGE_CURVE('',#3743,#3744,#2038,.T.) ;
#4745 = EDGE_CURVE('',#3745,#3746,#708,.T.) ;
#4746 = EDGE_CURVE('',#3746,#3746,#145,.T.) ;
#4747 = EDGE_CURVE('',#3746,#3747,#2039,.T.) ;
#4748 = EDGE_CURVE('',#3747,#3747,#146,.T.) ;
#4749 = EDGE_CURVE('',#3747,#3748,#18,.T.) ;
#4750 = EDGE_CURVE('',#3748,#3748,#147,.T.) ;
#4751 = EDGE_CURVE('',#3748,#3749,#2040,.T.) ;
#4752 = EDGE_CURVE('',#3749,#3749,#148,.T.) ;
#4753 = EDGE_CURVE('',#3749,#3743,#2041,.T.) ;
#4754 = EDGE_CURVE('',#3750,#3750,#149,.T.) ;
#4755 = EDGE_CURVE('',#3751,#3752,#19,.T.) ;
#4756 = EDGE_CURVE('',#3753,#3751,#150,.T.) ;
#4757 = EDGE_CURVE('',#3754,#3753,#151,.T.) ;
#4758 = EDGE_CURVE('',#3751,#3754,#152,.T.) ;
#4759 = EDGE_CURVE('',#3755,#3752,#3435,.T.) ;
#4760 = EDGE_CURVE('',#3755,#3756,#3436,.T.) ;
#4761 = EDGE_CURVE('',#3752,#3756,#3437,.T.) ;
#4762 = EDGE_CURVE('',#3751,#3757,#20,.T.) ;
#4763 = EDGE_CURVE('',#3757,#3757,#153,.T.) ;
#4764 = EDGE_CURVE('',#3757,#3758,#2042,.T.) ;
#4765 = EDGE_CURVE('',#3758,#3759,#154,.T.) ;
#4766 = EDGE_CURVE('',#3759,#3760,#155,.T.) ;
#4767 = EDGE_CURVE('',#3760,#3758,#156,.T.) ;
#4768 = EDGE_CURVE('',#3758,#3750,#21,.T.) ;
#4769 = EDGE_CURVE('',#3761,#3761,#157,.T.) ;
#4770 = EDGE_CURVE('',#3762,#3763,#22,.T.) ;
#4771 = EDGE_CURVE('',#3764,#3762,#158,.T.) ;
#4772 = EDGE_CURVE('',#3765,#3764,#159,.T.) ;
#4773 = EDGE_CURVE('',#3762,#3765,#160,.T.) ;
#4774 = EDGE_CURVE('',#3755,#3763,#3438,.T.) ;
#4775 = EDGE_CURVE('',#3756,#3755,#3439,.T.) ;
#4776 = EDGE_CURVE('',#3763,#3756,#3440,.T.) ;
#4777 = EDGE_CURVE('',#3762,#3766,#23,.T.) ;
#4778 = EDGE_CURVE('',#3766,#3766,#161,.T.) ;
#4779 = EDGE_CURVE('',#3766,#3767,#2043,.T.) ;
#4780 = EDGE_CURVE('',#3767,#3768,#162,.T.) ;
#4781 = EDGE_CURVE('',#3768,#3769,#163,.T.) ;
#4782 = EDGE_CURVE('',#3769,#3767,#164,.T.) ;
#4783 = EDGE_CURVE('',#3767,#3761,#24,.T.) ;
#4784 = EDGE_CURVE('',#3770,#3770,#165,.T.) ;
#4785 = EDGE_CURVE('',#3770,#3771,#2044,.T.) ;
#4786 = EDGE_CURVE('',#3772,#3773,#709,.T.) ;
#4787 = EDGE_CURVE('',#3773,#3773,#166,.T.) ;
#4788 = EDGE_CURVE('',#3773,#3774,#2045,.T.) ;
#4789 = EDGE_CURVE('',#3774,#3774,#167,.T.) ;
#4790 = EDGE_CURVE('',#3774,#3775,#25,.T.) ;
#4791 = EDGE_CURVE('',#3775,#3775,#168,.T.) ;
#4792 = EDGE_CURVE('',#3775,#3776,#2046,.T.) ;
#4793 = EDGE_CURVE('',#3776,#3776,#169,.T.) ;
#4794 = EDGE_CURVE('',#3776,#3770,#2047,.T.) ;
#4795 = EDGE_CURVE('',#3777,#3778,#2048,.T.) ;
#4796 = EDGE_CURVE('',#3777,#3777,#170,.T.) ;
#4797 = EDGE_CURVE('',#3779,#3779,#171,.T.) ;
#4798 = EDGE_CURVE('',#3780,#3779,#710,.T.) ;
#4799 = EDGE_CURVE('',#3781,#3781,#172,.T.) ;
#4800 = EDGE_CURVE('',#3779,#3781,#2049,.T.) ;
#4801 = EDGE_CURVE('',#3782,#3782,#173,.T.) ;
#4802 = EDGE_CURVE('',#3781,#3782,#26,.T.) ;
#4803 = EDGE_CURVE('',#3783,#3783,#174,.T.) ;
#4804 = EDGE_CURVE('',#3782,#3783,#2050,.T.) ;
#4805 = EDGE_CURVE('',#3783,#3777,#2051,.T.) ;
#4806 = EDGE_CURVE('',#3784,#3784,#175,.T.) ;
#4807 = EDGE_CURVE('',#3785,#3786,#3441,.T.) ;
#4808 = EDGE_CURVE('',#3787,#3786,#3442,.T.) ;
#4809 = EDGE_CURVE('',#3787,#3785,#3443,.T.) ;
#4810 = EDGE_CURVE('',#3788,#3785,#27,.T.) ;
#4811 = EDGE_CURVE('',#3788,#3789,#176,.T.) ;
#4812 = EDGE_CURVE('',#3789,#3790,#177,.T.) ;
#4813 = EDGE_CURVE('',#3790,#3788,#178,.T.) ;
#4814 = EDGE_CURVE('',#3788,#3791,#28,.T.) ;
#4815 = EDGE_CURVE('',#3791,#3791,#179,.T.) ;
#4816 = EDGE_CURVE('',#3791,#3792,#2052,.T.) ;
#4817 = EDGE_CURVE('',#3793,#3792,#180,.T.) ;
#4818 = EDGE_CURVE('',#3794,#3793,#181,.T.) ;
#4819 = EDGE_CURVE('',#3792,#3794,#182,.T.) ;
#4820 = EDGE_CURVE('',#3792,#3784,#29,.T.) ;
#4821 = EDGE_CURVE('',#3795,#3795,#183,.T.) ;
#4822 = EDGE_CURVE('',#3796,#3786,#3444,.T.) ;
#4823 = EDGE_CURVE('',#3786,#3787,#3445,.T.) ;
#4824 = EDGE_CURVE('',#3787,#3796,#3446,.T.) ;
#4825 = EDGE_CURVE('',#3797,#3796,#30,.T.) ;
#4826 = EDGE_CURVE('',#3797,#3798,#184,.T.) ;
#4827 = EDGE_CURVE('',#3798,#3799,#185,.T.) ;
#4828 = EDGE_CURVE('',#3799,#3797,#186,.T.) ;
#4829 = EDGE_CURVE('',#3797,#3800,#31,.T.) ;
#4830 = EDGE_CURVE('',#3800,#3800,#187,.T.) ;
#4831 = EDGE_CURVE('',#3800,#3801,#2053,.T.) ;
#4832 = EDGE_CURVE('',#3802,#3801,#188,.T.) ;
#4833 = EDGE_CURVE('',#3803,#3802,#189,.T.) ;
#4834 = EDGE_CURVE('',#3801,#3803,#190,.T.) ;
#4835 = EDGE_CURVE('',#3801,#3795,#32,.T.) ;
#4836 = EDGE_CURVE('',#3804,#3805,#2054,.T.) ;
#4837 = EDGE_CURVE('',#3805,#3806,#2055,.T.) ;
#4838 = EDGE_CURVE('',#3807,#3806,#2056,.T.) ;
#4839 = EDGE_CURVE('',#3804,#3807,#2057,.T.) ;
#4840 = EDGE_CURVE('',#3805,#3808,#711,.T.) ;
#4841 = EDGE_CURVE('',#3808,#3809,#2058,.T.) ;
#4842 = EDGE_CURVE('',#3806,#3809,#712,.T.) ;
#4843 = EDGE_CURVE('',#3808,#3810,#713,.T.) ;
#4844 = EDGE_CURVE('',#3810,#3811,#2059,.T.) ;
#4845 = EDGE_CURVE('',#3809,#3811,#714,.T.) ;
#4846 = EDGE_CURVE('',#3810,#3812,#715,.T.) ;
#4847 = EDGE_CURVE('',#3812,#3813,#2060,.T.) ;
#4848 = EDGE_CURVE('',#3811,#3813,#716,.T.) ;
#4849 = EDGE_CURVE('',#3812,#3814,#717,.T.) ;
#4850 = EDGE_CURVE('',#3814,#3815,#2061,.T.) ;
#4851 = EDGE_CURVE('',#3813,#3815,#718,.T.) ;
#4852 = EDGE_CURVE('',#3814,#3816,#719,.T.) ;
#4853 = EDGE_CURVE('',#3816,#3817,#2062,.T.) ;
#4854 = EDGE_CURVE('',#3815,#3817,#720,.T.) ;
#4855 = EDGE_CURVE('',#3816,#3818,#721,.T.) ;
#4856 = EDGE_CURVE('',#3818,#3819,#2063,.T.) ;
#4857 = EDGE_CURVE('',#3817,#3819,#722,.T.) ;
#4858 = EDGE_CURVE('',#3818,#3820,#2064,.T.) ;
#4859 = EDGE_CURVE('',#3820,#3821,#2065,.T.) ;
#4860 = EDGE_CURVE('',#3819,#3821,#2066,.T.) ;
#4861 = EDGE_CURVE('',#3820,#3822,#723,.T.) ;
#4862 = EDGE_CURVE('',#3822,#3823,#2067,.T.) ;
#4863 = EDGE_CURVE('',#3821,#3823,#724,.T.) ;
#4864 = EDGE_CURVE('',#3822,#3824,#2068,.T.) ;
#4865 = EDGE_CURVE('',#3824,#3825,#2069,.T.) ;
#4866 = EDGE_CURVE('',#3823,#3825,#2070,.T.) ;
#4867 = EDGE_CURVE('',#3824,#3826,#725,.T.) ;
#4868 = EDGE_CURVE('',#3826,#3827,#2071,.T.) ;
#4869 = EDGE_CURVE('',#3825,#3827,#726,.T.) ;
#4870 = EDGE_CURVE('',#3826,#3828,#727,.T.) ;
#4871 = EDGE_CURVE('',#3828,#3829,#2072,.T.) ;
#4872 = EDGE_CURVE('',#3827,#3829,#728,.T.) ;
#4873 = EDGE_CURVE('',#3828,#3830,#729,.T.) ;
#4874 = EDGE_CURVE('',#3830,#3831,#2073,.T.) ;
#4875 = EDGE_CURVE('',#3829,#3831,#730,.T.) ;
#4876 = EDGE_CURVE('',#3830,#3832,#731,.T.) ;
#4877 = EDGE_CURVE('',#3832,#3833,#2074,.T.) ;
#4878 = EDGE_CURVE('',#3831,#3833,#732,.T.) ;
#4879 = EDGE_CURVE('',#3832,#3804,#2075,.T.) ;
#4880 = EDGE_CURVE('',#3833,#3807,#2076,.T.) ;
#4881 = EDGE_CURVE('',#3834,#3834,#733,.T.) ;
#4882 = EDGE_CURVE('',#3834,#3835,#2077,.T.) ;
#4883 = EDGE_CURVE('',#3835,#3835,#734,.T.) ;
#4884 = EDGE_CURVE('',#3836,#3836,#735,.T.) ;
#4885 = EDGE_CURVE('',#3836,#3837,#2078,.T.) ;
#4886 = EDGE_CURVE('',#3837,#3837,#736,.T.) ;
#4887 = EDGE_CURVE('',#3838,#3838,#737,.T.) ;
#4888 = EDGE_CURVE('',#3838,#3839,#2079,.T.) ;
#4889 = EDGE_CURVE('',#3839,#3839,#738,.T.) ;
#4890 = EDGE_CURVE('',#3840,#3840,#739,.T.) ;
#4891 = EDGE_CURVE('',#3841,#3841,#740,.T.) ;
#4892 = EDGE_CURVE('',#3842,#3842,#741,.T.) ;
#4893 = EDGE_CURVE('',#3843,#3843,#742,.T.) ;
#4894 = EDGE_CURVE('',#3843,#3844,#2080,.T.) ;
#4895 = EDGE_CURVE('',#3844,#3844,#743,.T.) ;
#4896 = EDGE_CURVE('',#3845,#3845,#744,.T.) ;
#4897 = EDGE_CURVE('',#3840,#3845,#2081,.T.) ;
#4898 = EDGE_CURVE('',#3842,#3841,#2082,.T.) ;
#4899 = EDGE_CURVE('',#3846,#3847,#2083,.T.) ;
#4900 = EDGE_CURVE('',#3847,#3848,#2084,.T.) ;
#4901 = EDGE_CURVE('',#3849,#3848,#2085,.T.) ;
#4902 = EDGE_CURVE('',#3846,#3849,#2086,.T.) ;
#4903 = EDGE_CURVE('',#3847,#3850,#191,.T.) ;
#4904 = EDGE_CURVE('',#3850,#3851,#2087,.T.) ;
#4905 = EDGE_CURVE('',#3848,#3851,#192,.T.) ;
#4906 = EDGE_CURVE('',#3850,#3852,#2088,.T.) ;
#4907 = EDGE_CURVE('',#3852,#3853,#2089,.T.) ;
#4908 = EDGE_CURVE('',#3851,#3853,#2090,.T.) ;
#4909 = EDGE_CURVE('',#3852,#3854,#2091,.T.) ;
#4910 = EDGE_CURVE('',#3854,#3855,#2092,.T.) ;
#4911 = EDGE_CURVE('',#3853,#3855,#2093,.T.) ;
#4912 = EDGE_CURVE('',#3854,#3856,#193,.T.) ;
#4913 = EDGE_CURVE('',#3856,#3857,#2094,.T.) ;
#4914 = EDGE_CURVE('',#3855,#3857,#194,.T.) ;
#4915 = EDGE_CURVE('',#3856,#3858,#2095,.T.) ;
#4916 = EDGE_CURVE('',#3858,#3859,#2096,.T.) ;
#4917 = EDGE_CURVE('',#3857,#3859,#2097,.T.) ;
#4918 = EDGE_CURVE('',#3858,#3860,#2098,.T.) ;
#4919 = EDGE_CURVE('',#3860,#3861,#2099,.T.) ;
#4920 = EDGE_CURVE('',#3859,#3861,#2100,.T.) ;
#4921 = EDGE_CURVE('',#3860,#3862,#195,.T.) ;
#4922 = EDGE_CURVE('',#3862,#3863,#2101,.T.) ;
#4923 = EDGE_CURVE('',#3861,#3863,#196,.T.) ;
#4924 = EDGE_CURVE('',#3862,#3864,#2102,.T.) ;
#4925 = EDGE_CURVE('',#3864,#3865,#2103,.T.) ;
#4926 = EDGE_CURVE('',#3863,#3865,#2104,.T.) ;
#4927 = EDGE_CURVE('',#3864,#3866,#2105,.T.) ;
#4928 = EDGE_CURVE('',#3866,#3867,#2106,.T.) ;
#4929 = EDGE_CURVE('',#3865,#3867,#2107,.T.) ;
#4930 = EDGE_CURVE('',#3866,#3868,#197,.T.) ;
#4931 = EDGE_CURVE('',#3868,#3869,#2108,.T.) ;
#4932 = EDGE_CURVE('',#3867,#3869,#198,.T.) ;
#4933 = EDGE_CURVE('',#3868,#3870,#2109,.T.) ;
#4934 = EDGE_CURVE('',#3870,#3871,#2110,.T.) ;
#4935 = EDGE_CURVE('',#3869,#3871,#2111,.T.) ;
#4936 = EDGE_CURVE('',#3870,#3872,#2112,.T.) ;
#4937 = EDGE_CURVE('',#3872,#3873,#2113,.T.) ;
#4938 = EDGE_CURVE('',#3871,#3873,#2114,.T.) ;
#4939 = EDGE_CURVE('',#3872,#3874,#199,.T.) ;
#4940 = EDGE_CURVE('',#3874,#3875,#2115,.T.) ;
#4941 = EDGE_CURVE('',#3873,#3875,#200,.T.) ;
#4942 = EDGE_CURVE('',#3874,#3876,#2116,.T.) ;
#4943 = EDGE_CURVE('',#3876,#3877,#2117,.T.) ;
#4944 = EDGE_CURVE('',#3875,#3877,#2118,.T.) ;
#4945 = EDGE_CURVE('',#3876,#3878,#2119,.T.) ;
#4946 = EDGE_CURVE('',#3878,#3879,#2120,.T.) ;
#4947 = EDGE_CURVE('',#3877,#3879,#2121,.T.) ;
#4948 = EDGE_CURVE('',#3878,#3880,#201,.T.) ;
#4949 = EDGE_CURVE('',#3880,#3881,#2122,.T.) ;
#4950 = EDGE_CURVE('',#3879,#3881,#202,.T.) ;
#4951 = EDGE_CURVE('',#3880,#3882,#2123,.T.) ;
#4952 = EDGE_CURVE('',#3882,#3883,#2124,.T.) ;
#4953 = EDGE_CURVE('',#3881,#3883,#2125,.T.) ;
#4954 = EDGE_CURVE('',#3882,#3884,#2126,.T.) ;
#4955 = EDGE_CURVE('',#3884,#3885,#2127,.T.) ;
#4956 = EDGE_CURVE('',#3883,#3885,#2128,.T.) ;
#4957 = EDGE_CURVE('',#3884,#3886,#203,.T.) ;
#4958 = EDGE_CURVE('',#3886,#3887,#2129,.T.) ;
#4959 = EDGE_CURVE('',#3885,#3887,#204,.T.) ;
#4960 = EDGE_CURVE('',#3886,#3888,#2130,.T.) ;
#4961 = EDGE_CURVE('',#3888,#3889,#2131,.T.) ;
#4962 = EDGE_CURVE('',#3887,#3889,#2132,.T.) ;
#4963 = EDGE_CURVE('',#3888,#3890,#2133,.T.) ;
#4964 = EDGE_CURVE('',#3890,#3891,#2134,.T.) ;
#4965 = EDGE_CURVE('',#3889,#3891,#2135,.T.) ;
#4966 = EDGE_CURVE('',#3890,#3892,#205,.T.) ;
#4967 = EDGE_CURVE('',#3892,#3893,#2136,.T.) ;
#4968 = EDGE_CURVE('',#3891,#3893,#206,.T.) ;
#4969 = EDGE_CURVE('',#3892,#3894,#2137,.T.) ;
#4970 = EDGE_CURVE('',#3894,#3895,#2138,.T.) ;
#4971 = EDGE_CURVE('',#3893,#3895,#2139,.T.) ;
#4972 = EDGE_CURVE('',#3894,#3896,#2140,.T.) ;
#4973 = EDGE_CURVE('',#3896,#3897,#2141,.T.) ;
#4974 = EDGE_CURVE('',#3895,#3897,#2142,.T.) ;
#4975 = EDGE_CURVE('',#3896,#3898,#207,.T.) ;
#4976 = EDGE_CURVE('',#3898,#3899,#2143,.T.) ;
#4977 = EDGE_CURVE('',#3897,#3899,#208,.T.) ;
#4978 = EDGE_CURVE('',#3898,#3900,#2144,.T.) ;
#4979 = EDGE_CURVE('',#3900,#3901,#2145,.T.) ;
#4980 = EDGE_CURVE('',#3899,#3901,#2146,.T.) ;
#4981 = EDGE_CURVE('',#3900,#3902,#2147,.T.) ;
#4982 = EDGE_CURVE('',#3902,#3903,#2148,.T.) ;
#4983 = EDGE_CURVE('',#3901,#3903,#2149,.T.) ;
#4984 = EDGE_CURVE('',#3902,#3904,#209,.T.) ;
#4985 = EDGE_CURVE('',#3904,#3905,#2150,.T.) ;
#4986 = EDGE_CURVE('',#3903,#3905,#210,.T.) ;
#4987 = EDGE_CURVE('',#3904,#3906,#2151,.T.) ;
#4988 = EDGE_CURVE('',#3906,#3907,#2152,.T.) ;
#4989 = EDGE_CURVE('',#3905,#3907,#2153,.T.) ;
#4990 = EDGE_CURVE('',#3906,#3908,#2154,.T.) ;
#4991 = EDGE_CURVE('',#3908,#3909,#2155,.T.) ;
#4992 = EDGE_CURVE('',#3907,#3909,#2156,.T.) ;
#4993 = EDGE_CURVE('',#3908,#3910,#211,.T.) ;
#4994 = EDGE_CURVE('',#3910,#3911,#2157,.T.) ;
#4995 = EDGE_CURVE('',#3909,#3911,#212,.T.) ;
#4996 = EDGE_CURVE('',#3910,#3912,#2158,.T.) ;
#4997 = EDGE_CURVE('',#3912,#3913,#2159,.T.) ;
#4998 = EDGE_CURVE('',#3911,#3913,#2160,.T.) ;
#4999 = EDGE_CURVE('',#3912,#3914,#2161,.T.) ;
#5000 = EDGE_CURVE('',#3914,#3915,#2162,.T.) ;
#5001 = EDGE_CURVE('',#3913,#3915,#2163,.T.) ;
#5002 = EDGE_CURVE('',#3914,#3916,#213,.T.) ;
#5003 = EDGE_CURVE('',#3916,#3917,#2164,.T.) ;
#5004 = EDGE_CURVE('',#3915,#3917,#214,.T.) ;
#5005 = EDGE_CURVE('',#3916,#3918,#2165,.T.) ;
#5006 = EDGE_CURVE('',#3918,#3919,#2166,.T.) ;
#5007 = EDGE_CURVE('',#3917,#3919,#2167,.T.) ;
#5008 = EDGE_CURVE('',#3918,#3920,#2168,.T.) ;
#5009 = EDGE_CURVE('',#3920,#3921,#2169,.T.) ;
#5010 = EDGE_CURVE('',#3919,#3921,#2170,.T.) ;
#5011 = EDGE_CURVE('',#3920,#3922,#215,.T.) ;
#5012 = EDGE_CURVE('',#3922,#3923,#2171,.T.) ;
#5013 = EDGE_CURVE('',#3921,#3923,#216,.T.) ;
#5014 = EDGE_CURVE('',#3922,#3924,#2172,.T.) ;
#5015 = EDGE_CURVE('',#3924,#3925,#2173,.T.) ;
#5016 = EDGE_CURVE('',#3923,#3925,#2174,.T.) ;
#5017 = EDGE_CURVE('',#3924,#3926,#2175,.T.) ;
#5018 = EDGE_CURVE('',#3926,#3927,#2176,.T.) ;
#5019 = EDGE_CURVE('',#3925,#3927,#2177,.T.) ;
#5020 = EDGE_CURVE('',#3926,#3928,#217,.T.) ;
#5021 = EDGE_CURVE('',#3928,#3929,#2178,.T.) ;
#5022 = EDGE_CURVE('',#3927,#3929,#218,.T.) ;
#5023 = EDGE_CURVE('',#3928,#3930,#2179,.T.) ;
#5024 = EDGE_CURVE('',#3930,#3931,#2180,.T.) ;
#5025 = EDGE_CURVE('',#3929,#3931,#2181,.T.) ;
#5026 = EDGE_CURVE('',#3930,#3932,#2182,.T.) ;
#5027 = EDGE_CURVE('',#3932,#3933,#2183,.T.) ;
#5028 = EDGE_CURVE('',#3931,#3933,#2184,.T.) ;
#5029 = EDGE_CURVE('',#3932,#3934,#219,.T.) ;
#5030 = EDGE_CURVE('',#3934,#3935,#2185,.T.) ;
#5031 = EDGE_CURVE('',#3933,#3935,#220,.T.) ;
#5032 = EDGE_CURVE('',#3934,#3936,#2186,.T.) ;
#5033 = EDGE_CURVE('',#3936,#3937,#2187,.T.) ;
#5034 = EDGE_CURVE('',#3935,#3937,#2188,.T.) ;
#5035 = EDGE_CURVE('',#3936,#3938,#2189,.T.) ;
#5036 = EDGE_CURVE('',#3938,#3939,#2190,.T.) ;
#5037 = EDGE_CURVE('',#3937,#3939,#2191,.T.) ;
#5038 = EDGE_CURVE('',#3938,#3940,#221,.T.) ;
#5039 = EDGE_CURVE('',#3940,#3941,#2192,.T.) ;
#5040 = EDGE_CURVE('',#3939,#3941,#222,.T.) ;
#5041 = EDGE_CURVE('',#3940,#3942,#2193,.T.) ;
#5042 = EDGE_CURVE('',#3942,#3943,#2194,.T.) ;
#5043 = EDGE_CURVE('',#3941,#3943,#2195,.T.) ;
#5044 = EDGE_CURVE('',#3942,#3944,#2196,.T.) ;
#5045 = EDGE_CURVE('',#3944,#3945,#2197,.T.) ;
#5046 = EDGE_CURVE('',#3943,#3945,#2198,.T.) ;
#5047 = EDGE_CURVE('',#3944,#3946,#223,.T.) ;
#5048 = EDGE_CURVE('',#3946,#3947,#2199,.T.) ;
#5049 = EDGE_CURVE('',#3945,#3947,#224,.T.) ;
#5050 = EDGE_CURVE('',#3946,#3948,#2200,.T.) ;
#5051 = EDGE_CURVE('',#3948,#3949,#2201,.T.) ;
#5052 = EDGE_CURVE('',#3947,#3949,#2202,.T.) ;
#5053 = EDGE_CURVE('',#3948,#3950,#2203,.T.) ;
#5054 = EDGE_CURVE('',#3950,#3951,#2204,.T.) ;
#5055 = EDGE_CURVE('',#3949,#3951,#2205,.T.) ;
#5056 = EDGE_CURVE('',#3950,#3952,#225,.T.) ;
#5057 = EDGE_CURVE('',#3952,#3953,#2206,.T.) ;
#5058 = EDGE_CURVE('',#3951,#3953,#226,.T.) ;
#5059 = EDGE_CURVE('',#3952,#3954,#2207,.T.) ;
#5060 = EDGE_CURVE('',#3954,#3955,#2208,.T.) ;
#5061 = EDGE_CURVE('',#3953,#3955,#2209,.T.) ;
#5062 = EDGE_CURVE('',#3954,#3956,#2210,.T.) ;
#5063 = EDGE_CURVE('',#3956,#3957,#2211,.T.) ;
#5064 = EDGE_CURVE('',#3955,#3957,#2212,.T.) ;
#5065 = EDGE_CURVE('',#3956,#3958,#227,.T.) ;
#5066 = EDGE_CURVE('',#3958,#3959,#2213,.T.) ;
#5067 = EDGE_CURVE('',#3957,#3959,#228,.T.) ;
#5068 = EDGE_CURVE('',#3958,#3960,#2214,.T.) ;
#5069 = EDGE_CURVE('',#3960,#3961,#2215,.T.) ;
#5070 = EDGE_CURVE('',#3959,#3961,#2216,.T.) ;
#5071 = EDGE_CURVE('',#3960,#3962,#2217,.T.) ;
#5072 = EDGE_CURVE('',#3962,#3963,#2218,.T.) ;
#5073 = EDGE_CURVE('',#3961,#3963,#2219,.T.) ;
#5074 = EDGE_CURVE('',#3962,#3964,#229,.T.) ;
#5075 = EDGE_CURVE('',#3964,#3965,#2220,.T.) ;
#5076 = EDGE_CURVE('',#3963,#3965,#230,.T.) ;
#5077 = EDGE_CURVE('',#3964,#3966,#2221,.T.) ;
#5078 = EDGE_CURVE('',#3966,#3967,#2222,.T.) ;
#5079 = EDGE_CURVE('',#3965,#3967,#2223,.T.) ;
#5080 = EDGE_CURVE('',#3966,#3968,#2224,.T.) ;
#5081 = EDGE_CURVE('',#3968,#3969,#2225,.T.) ;
#5082 = EDGE_CURVE('',#3967,#3969,#2226,.T.) ;
#5083 = EDGE_CURVE('',#3968,#3970,#231,.T.) ;
#5084 = EDGE_CURVE('',#3970,#3971,#2227,.T.) ;
#5085 = EDGE_CURVE('',#3969,#3971,#232,.T.) ;
#5086 = EDGE_CURVE('',#3970,#3972,#2228,.T.) ;
#5087 = EDGE_CURVE('',#3972,#3973,#2229,.T.) ;
#5088 = EDGE_CURVE('',#3971,#3973,#2230,.T.) ;
#5089 = EDGE_CURVE('',#3972,#3974,#2231,.T.) ;
#5090 = EDGE_CURVE('',#3974,#3975,#2232,.T.) ;
#5091 = EDGE_CURVE('',#3973,#3975,#2233,.T.) ;
#5092 = EDGE_CURVE('',#3974,#3976,#233,.T.) ;
#5093 = EDGE_CURVE('',#3976,#3977,#2234,.T.) ;
#5094 = EDGE_CURVE('',#3975,#3977,#234,.T.) ;
#5095 = EDGE_CURVE('',#3976,#3978,#2235,.T.) ;
#5096 = EDGE_CURVE('',#3978,#3979,#2236,.T.) ;
#5097 = EDGE_CURVE('',#3977,#3979,#2237,.T.) ;
#5098 = EDGE_CURVE('',#3978,#3980,#2238,.T.) ;
#5099 = EDGE_CURVE('',#3980,#3981,#2239,.T.) ;
#5100 = EDGE_CURVE('',#3979,#3981,#2240,.T.) ;
#5101 = EDGE_CURVE('',#3980,#3982,#235,.T.) ;
#5102 = EDGE_CURVE('',#3982,#3983,#2241,.T.) ;
#5103 = EDGE_CURVE('',#3981,#3983,#236,.T.) ;
#5104 = EDGE_CURVE('',#3982,#3984,#2242,.T.) ;
#5105 = EDGE_CURVE('',#3984,#3985,#2243,.T.) ;
#5106 = EDGE_CURVE('',#3983,#3985,#2244,.T.) ;
#5107 = EDGE_CURVE('',#3984,#3986,#2245,.T.) ;
#5108 = EDGE_CURVE('',#3986,#3987,#2246,.T.) ;
#5109 = EDGE_CURVE('',#3985,#3987,#2247,.T.) ;
#5110 = EDGE_CURVE('',#3986,#3988,#237,.T.) ;
#5111 = EDGE_CURVE('',#3988,#3989,#2248,.T.) ;
#5112 = EDGE_CURVE('',#3987,#3989,#238,.T.) ;
#5113 = EDGE_CURVE('',#3988,#3990,#2249,.T.) ;
#5114 = EDGE_CURVE('',#3990,#3991,#2250,.T.) ;
#5115 = EDGE_CURVE('',#3989,#3991,#2251,.T.) ;
#5116 = EDGE_CURVE('',#3990,#3992,#2252,.T.) ;
#5117 = EDGE_CURVE('',#3992,#3993,#2253,.T.) ;
#5118 = EDGE_CURVE('',#3991,#3993,#2254,.T.) ;
#5119 = EDGE_CURVE('',#3992,#3994,#239,.T.) ;
#5120 = EDGE_CURVE('',#3994,#3995,#2255,.T.) ;
#5121 = EDGE_CURVE('',#3993,#3995,#240,.T.) ;
#5122 = EDGE_CURVE('',#3994,#3996,#2256,.T.) ;
#5123 = EDGE_CURVE('',#3996,#3997,#2257,.T.) ;
#5124 = EDGE_CURVE('',#3995,#3997,#2258,.T.) ;
#5125 = EDGE_CURVE('',#3996,#3998,#2259,.T.) ;
#5126 = EDGE_CURVE('',#3998,#3999,#2260,.T.) ;
#5127 = EDGE_CURVE('',#3997,#3999,#2261,.T.) ;
#5128 = EDGE_CURVE('',#3998,#4000,#241,.T.) ;
#5129 = EDGE_CURVE('',#4000,#4001,#2262,.T.) ;
#5130 = EDGE_CURVE('',#3999,#4001,#242,.T.) ;
#5131 = EDGE_CURVE('',#4000,#4002,#2263,.T.) ;
#5132 = EDGE_CURVE('',#4002,#4003,#2264,.T.) ;
#5133 = EDGE_CURVE('',#4001,#4003,#2265,.T.) ;
#5134 = EDGE_CURVE('',#4002,#4004,#2266,.T.) ;
#5135 = EDGE_CURVE('',#4004,#4005,#2267,.T.) ;
#5136 = EDGE_CURVE('',#4003,#4005,#2268,.T.) ;
#5137 = EDGE_CURVE('',#4004,#4006,#243,.T.) ;
#5138 = EDGE_CURVE('',#4006,#4007,#2269,.T.) ;
#5139 = EDGE_CURVE('',#4005,#4007,#244,.T.) ;
#5140 = EDGE_CURVE('',#4006,#4008,#2270,.T.) ;
#5141 = EDGE_CURVE('',#4008,#4009,#2271,.T.) ;
#5142 = EDGE_CURVE('',#4007,#4009,#2272,.T.) ;
#5143 = EDGE_CURVE('',#4008,#4010,#2273,.T.) ;
#5144 = EDGE_CURVE('',#4010,#4011,#2274,.T.) ;
#5145 = EDGE_CURVE('',#4009,#4011,#2275,.T.) ;
#5146 = EDGE_CURVE('',#4010,#4012,#245,.T.) ;
#5147 = EDGE_CURVE('',#4012,#4013,#2276,.T.) ;
#5148 = EDGE_CURVE('',#4011,#4013,#246,.T.) ;
#5149 = EDGE_CURVE('',#4012,#4014,#2277,.T.) ;
#5150 = EDGE_CURVE('',#4014,#4015,#2278,.T.) ;
#5151 = EDGE_CURVE('',#4013,#4015,#2279,.T.) ;
#5152 = EDGE_CURVE('',#4014,#4016,#2280,.T.) ;
#5153 = EDGE_CURVE('',#4016,#4017,#2281,.T.) ;
#5154 = EDGE_CURVE('',#4015,#4017,#2282,.T.) ;
#5155 = EDGE_CURVE('',#4016,#4018,#247,.T.) ;
#5156 = EDGE_CURVE('',#4018,#4019,#2283,.T.) ;
#5157 = EDGE_CURVE('',#4017,#4019,#248,.T.) ;
#5158 = EDGE_CURVE('',#4018,#4020,#2284,.T.) ;
#5159 = EDGE_CURVE('',#4020,#4021,#2285,.T.) ;
#5160 = EDGE_CURVE('',#4019,#4021,#2286,.T.) ;
#5161 = EDGE_CURVE('',#4020,#4022,#2287,.T.) ;
#5162 = EDGE_CURVE('',#4022,#4023,#2288,.T.) ;
#5163 = EDGE_CURVE('',#4021,#4023,#2289,.T.) ;
#5164 = EDGE_CURVE('',#4022,#4024,#249,.T.) ;
#5165 = EDGE_CURVE('',#4024,#4025,#2290,.T.) ;
#5166 = EDGE_CURVE('',#4023,#4025,#250,.T.) ;
#5167 = EDGE_CURVE('',#4024,#4026,#2291,.T.) ;
#5168 = EDGE_CURVE('',#4026,#4027,#2292,.T.) ;
#5169 = EDGE_CURVE('',#4025,#4027,#2293,.T.) ;
#5170 = EDGE_CURVE('',#4026,#4028,#2294,.T.) ;
#5171 = EDGE_CURVE('',#4028,#4029,#2295,.T.) ;
#5172 = EDGE_CURVE('',#4027,#4029,#2296,.T.) ;
#5173 = EDGE_CURVE('',#4028,#4030,#251,.T.) ;
#5174 = EDGE_CURVE('',#4030,#4031,#2297,.T.) ;
#5175 = EDGE_CURVE('',#4029,#4031,#252,.T.) ;
#5176 = EDGE_CURVE('',#4030,#4032,#2298,.T.) ;
#5177 = EDGE_CURVE('',#4032,#4033,#2299,.T.) ;
#5178 = EDGE_CURVE('',#4031,#4033,#2300,.T.) ;
#5179 = EDGE_CURVE('',#4032,#4034,#2301,.T.) ;
#5180 = EDGE_CURVE('',#4034,#4035,#2302,.T.) ;
#5181 = EDGE_CURVE('',#4033,#4035,#2303,.T.) ;
#5182 = EDGE_CURVE('',#4034,#4036,#253,.T.) ;
#5183 = EDGE_CURVE('',#4036,#4037,#2304,.T.) ;
#5184 = EDGE_CURVE('',#4035,#4037,#254,.T.) ;
#5185 = EDGE_CURVE('',#4036,#4038,#2305,.T.) ;
#5186 = EDGE_CURVE('',#4038,#4039,#2306,.T.) ;
#5187 = EDGE_CURVE('',#4037,#4039,#2307,.T.) ;
#5188 = EDGE_CURVE('',#4038,#4040,#2308,.T.) ;
#5189 = EDGE_CURVE('',#4040,#4041,#2309,.T.) ;
#5190 = EDGE_CURVE('',#4039,#4041,#2310,.T.) ;
#5191 = EDGE_CURVE('',#4040,#4042,#255,.T.) ;
#5192 = EDGE_CURVE('',#4042,#4043,#2311,.T.) ;
#5193 = EDGE_CURVE('',#4041,#4043,#256,.T.) ;
#5194 = EDGE_CURVE('',#4042,#4044,#2312,.T.) ;
#5195 = EDGE_CURVE('',#4044,#4045,#2313,.T.) ;
#5196 = EDGE_CURVE('',#4043,#4045,#2314,.T.) ;
#5197 = EDGE_CURVE('',#4044,#4046,#2315,.T.) ;
#5198 = EDGE_CURVE('',#4046,#4047,#2316,.T.) ;
#5199 = EDGE_CURVE('',#4045,#4047,#2317,.T.) ;
#5200 = EDGE_CURVE('',#4046,#4048,#257,.T.) ;
#5201 = EDGE_CURVE('',#4048,#4049,#2318,.T.) ;
#5202 = EDGE_CURVE('',#4047,#4049,#258,.T.) ;
#5203 = EDGE_CURVE('',#4048,#4050,#2319,.T.) ;
#5204 = EDGE_CURVE('',#4050,#4051,#2320,.T.) ;
#5205 = EDGE_CURVE('',#4049,#4051,#2321,.T.) ;
#5206 = EDGE_CURVE('',#4050,#4052,#2322,.T.) ;
#5207 = EDGE_CURVE('',#4052,#4053,#2323,.T.) ;
#5208 = EDGE_CURVE('',#4051,#4053,#2324,.T.) ;
#5209 = EDGE_CURVE('',#4052,#4054,#259,.T.) ;
#5210 = EDGE_CURVE('',#4054,#4055,#2325,.T.) ;
#5211 = EDGE_CURVE('',#4053,#4055,#260,.T.) ;
#5212 = EDGE_CURVE('',#4054,#4056,#2326,.T.) ;
#5213 = EDGE_CURVE('',#4056,#4057,#2327,.T.) ;
#5214 = EDGE_CURVE('',#4055,#4057,#2328,.T.) ;
#5215 = EDGE_CURVE('',#4056,#4058,#2329,.T.) ;
#5216 = EDGE_CURVE('',#4058,#4059,#2330,.T.) ;
#5217 = EDGE_CURVE('',#4057,#4059,#2331,.T.) ;
#5218 = EDGE_CURVE('',#4058,#4060,#261,.T.) ;
#5219 = EDGE_CURVE('',#4060,#4061,#2332,.T.) ;
#5220 = EDGE_CURVE('',#4059,#4061,#262,.T.) ;
#5221 = EDGE_CURVE('',#4060,#4062,#2333,.T.) ;
#5222 = EDGE_CURVE('',#4062,#4063,#2334,.T.) ;
#5223 = EDGE_CURVE('',#4061,#4063,#2335,.T.) ;
#5224 = EDGE_CURVE('',#4062,#4064,#2336,.T.) ;
#5225 = EDGE_CURVE('',#4064,#4065,#2337,.T.) ;
#5226 = EDGE_CURVE('',#4063,#4065,#2338,.T.) ;
#5227 = EDGE_CURVE('',#4064,#4066,#263,.T.) ;
#5228 = EDGE_CURVE('',#4066,#4067,#2339,.T.) ;
#5229 = EDGE_CURVE('',#4065,#4067,#264,.T.) ;
#5230 = EDGE_CURVE('',#4066,#4068,#2340,.T.) ;
#5231 = EDGE_CURVE('',#4068,#4069,#2341,.T.) ;
#5232 = EDGE_CURVE('',#4067,#4069,#2342,.T.) ;
#5233 = EDGE_CURVE('',#4068,#4070,#2343,.T.) ;
#5234 = EDGE_CURVE('',#4070,#4071,#2344,.T.) ;
#5235 = EDGE_CURVE('',#4069,#4071,#2345,.T.) ;
#5236 = EDGE_CURVE('',#4070,#4072,#265,.T.) ;
#5237 = EDGE_CURVE('',#4072,#4073,#2346,.T.) ;
#5238 = EDGE_CURVE('',#4071,#4073,#266,.T.) ;
#5239 = EDGE_CURVE('',#4072,#4074,#2347,.T.) ;
#5240 = EDGE_CURVE('',#4074,#4075,#2348,.T.) ;
#5241 = EDGE_CURVE('',#4073,#4075,#2349,.T.) ;
#5242 = EDGE_CURVE('',#4074,#4076,#2350,.T.) ;
#5243 = EDGE_CURVE('',#4076,#4077,#2351,.T.) ;
#5244 = EDGE_CURVE('',#4075,#4077,#2352,.T.) ;
#5245 = EDGE_CURVE('',#4076,#4078,#267,.T.) ;
#5246 = EDGE_CURVE('',#4078,#4079,#2353,.T.) ;
#5247 = EDGE_CURVE('',#4077,#4079,#268,.T.) ;
#5248 = EDGE_CURVE('',#4078,#4080,#2354,.T.) ;
#5249 = EDGE_CURVE('',#4080,#4081,#2355,.T.) ;
#5250 = EDGE_CURVE('',#4079,#4081,#2356,.T.) ;
#5251 = EDGE_CURVE('',#4080,#4082,#2357,.T.) ;
#5252 = EDGE_CURVE('',#4082,#4083,#2358,.T.) ;
#5253 = EDGE_CURVE('',#4081,#4083,#2359,.T.) ;
#5254 = EDGE_CURVE('',#4082,#4084,#269,.T.) ;
#5255 = EDGE_CURVE('',#4084,#4085,#2360,.T.) ;
#5256 = EDGE_CURVE('',#4083,#4085,#270,.T.) ;
#5257 = EDGE_CURVE('',#4084,#4086,#2361,.T.) ;
#5258 = EDGE_CURVE('',#4086,#4087,#2362,.T.) ;
#5259 = EDGE_CURVE('',#4085,#4087,#2363,.T.) ;
#5260 = EDGE_CURVE('',#4086,#4088,#2364,.T.) ;
#5261 = EDGE_CURVE('',#4088,#4089,#2365,.T.) ;
#5262 = EDGE_CURVE('',#4087,#4089,#2366,.T.) ;
#5263 = EDGE_CURVE('',#4088,#4090,#271,.T.) ;
#5264 = EDGE_CURVE('',#4090,#4091,#2367,.T.) ;
#5265 = EDGE_CURVE('',#4089,#4091,#272,.T.) ;
#5266 = EDGE_CURVE('',#4090,#4092,#2368,.T.) ;
#5267 = EDGE_CURVE('',#4092,#4093,#2369,.T.) ;
#5268 = EDGE_CURVE('',#4091,#4093,#2370,.T.) ;
#5269 = EDGE_CURVE('',#4092,#4094,#2371,.T.) ;
#5270 = EDGE_CURVE('',#4094,#4095,#2372,.T.) ;
#5271 = EDGE_CURVE('',#4093,#4095,#2373,.T.) ;
#5272 = EDGE_CURVE('',#4094,#4096,#273,.T.) ;
#5273 = EDGE_CURVE('',#4096,#4097,#2374,.T.) ;
#5274 = EDGE_CURVE('',#4095,#4097,#274,.T.) ;
#5275 = EDGE_CURVE('',#4096,#4098,#2375,.T.) ;
#5276 = EDGE_CURVE('',#4098,#4099,#2376,.T.) ;
#5277 = EDGE_CURVE('',#4097,#4099,#2377,.T.) ;
#5278 = EDGE_CURVE('',#4098,#4100,#2378,.T.) ;
#5279 = EDGE_CURVE('',#4100,#4101,#2379,.T.) ;
#5280 = EDGE_CURVE('',#4099,#4101,#2380,.T.) ;
#5281 = EDGE_CURVE('',#4100,#4102,#275,.T.) ;
#5282 = EDGE_CURVE('',#4102,#4103,#2381,.T.) ;
#5283 = EDGE_CURVE('',#4101,#4103,#276,.T.) ;
#5284 = EDGE_CURVE('',#4102,#4104,#2382,.T.) ;
#5285 = EDGE_CURVE('',#4104,#4105,#2383,.T.) ;
#5286 = EDGE_CURVE('',#4103,#4105,#2384,.T.) ;
#5287 = EDGE_CURVE('',#4104,#4106,#2385,.T.) ;
#5288 = EDGE_CURVE('',#4106,#4107,#2386,.T.) ;
#5289 = EDGE_CURVE('',#4105,#4107,#2387,.T.) ;
#5290 = EDGE_CURVE('',#4106,#4108,#277,.T.) ;
#5291 = EDGE_CURVE('',#4108,#4109,#2388,.T.) ;
#5292 = EDGE_CURVE('',#4107,#4109,#278,.T.) ;
#5293 = EDGE_CURVE('',#4108,#4110,#2389,.T.) ;
#5294 = EDGE_CURVE('',#4110,#4111,#2390,.T.) ;
#5295 = EDGE_CURVE('',#4109,#4111,#2391,.T.) ;
#5296 = EDGE_CURVE('',#4110,#4112,#2392,.T.) ;
#5297 = EDGE_CURVE('',#4112,#4113,#2393,.T.) ;
#5298 = EDGE_CURVE('',#4111,#4113,#2394,.T.) ;
#5299 = EDGE_CURVE('',#4112,#4114,#279,.T.) ;
#5300 = EDGE_CURVE('',#4114,#4115,#2395,.T.) ;
#5301 = EDGE_CURVE('',#4113,#4115,#280,.T.) ;
#5302 = EDGE_CURVE('',#4114,#4116,#2396,.T.) ;
#5303 = EDGE_CURVE('',#4116,#4117,#2397,.T.) ;
#5304 = EDGE_CURVE('',#4115,#4117,#2398,.T.) ;
#5305 = EDGE_CURVE('',#4116,#4118,#2399,.T.) ;
#5306 = EDGE_CURVE('',#4118,#4119,#2400,.T.) ;
#5307 = EDGE_CURVE('',#4117,#4119,#2401,.T.) ;
#5308 = EDGE_CURVE('',#4118,#4120,#281,.T.) ;
#5309 = EDGE_CURVE('',#4120,#4121,#2402,.T.) ;
#5310 = EDGE_CURVE('',#4119,#4121,#282,.T.) ;
#5311 = EDGE_CURVE('',#4120,#4122,#2403,.T.) ;
#5312 = EDGE_CURVE('',#4122,#4123,#2404,.T.) ;
#5313 = EDGE_CURVE('',#4121,#4123,#2405,.T.) ;
#5314 = EDGE_CURVE('',#4122,#4124,#2406,.T.) ;
#5315 = EDGE_CURVE('',#4124,#4125,#2407,.T.) ;
#5316 = EDGE_CURVE('',#4123,#4125,#2408,.T.) ;
#5317 = EDGE_CURVE('',#4124,#4126,#283,.T.) ;
#5318 = EDGE_CURVE('',#4126,#4127,#2409,.T.) ;
#5319 = EDGE_CURVE('',#4125,#4127,#284,.T.) ;
#5320 = EDGE_CURVE('',#4126,#4128,#2410,.T.) ;
#5321 = EDGE_CURVE('',#4128,#4129,#2411,.T.) ;
#5322 = EDGE_CURVE('',#4127,#4129,#2412,.T.) ;
#5323 = EDGE_CURVE('',#4128,#4130,#2413,.T.) ;
#5324 = EDGE_CURVE('',#4130,#4131,#2414,.T.) ;
#5325 = EDGE_CURVE('',#4129,#4131,#2415,.T.) ;
#5326 = EDGE_CURVE('',#4130,#4132,#285,.T.) ;
#5327 = EDGE_CURVE('',#4132,#4133,#2416,.T.) ;
#5328 = EDGE_CURVE('',#4131,#4133,#286,.T.) ;
#5329 = EDGE_CURVE('',#4132,#4134,#2417,.T.) ;
#5330 = EDGE_CURVE('',#4134,#4135,#2418,.T.) ;
#5331 = EDGE_CURVE('',#4133,#4135,#2419,.T.) ;
#5332 = EDGE_CURVE('',#4134,#4136,#2420,.T.) ;
#5333 = EDGE_CURVE('',#4136,#4137,#2421,.T.) ;
#5334 = EDGE_CURVE('',#4135,#4137,#2422,.T.) ;
#5335 = EDGE_CURVE('',#4136,#4138,#287,.T.) ;
#5336 = EDGE_CURVE('',#4138,#4139,#2423,.T.) ;
#5337 = EDGE_CURVE('',#4137,#4139,#288,.T.) ;
#5338 = EDGE_CURVE('',#4138,#4140,#2424,.T.) ;
#5339 = EDGE_CURVE('',#4140,#4141,#2425,.T.) ;
#5340 = EDGE_CURVE('',#4139,#4141,#2426,.T.) ;
#5341 = EDGE_CURVE('',#4140,#4142,#2427,.T.) ;
#5342 = EDGE_CURVE('',#4142,#4143,#2428,.T.) ;
#5343 = EDGE_CURVE('',#4141,#4143,#2429,.T.) ;
#5344 = EDGE_CURVE('',#4142,#4144,#289,.T.) ;
#5345 = EDGE_CURVE('',#4144,#4145,#2430,.T.) ;
#5346 = EDGE_CURVE('',#4143,#4145,#290,.T.) ;
#5347 = EDGE_CURVE('',#4144,#4146,#2431,.T.) ;
#5348 = EDGE_CURVE('',#4146,#4147,#2432,.T.) ;
#5349 = EDGE_CURVE('',#4145,#4147,#2433,.T.) ;
#5350 = EDGE_CURVE('',#4146,#4148,#2434,.T.) ;
#5351 = EDGE_CURVE('',#4148,#4149,#2435,.T.) ;
#5352 = EDGE_CURVE('',#4147,#4149,#2436,.T.) ;
#5353 = EDGE_CURVE('',#4148,#4150,#291,.T.) ;
#5354 = EDGE_CURVE('',#4150,#4151,#2437,.T.) ;
#5355 = EDGE_CURVE('',#4149,#4151,#292,.T.) ;
#5356 = EDGE_CURVE('',#4150,#4152,#2438,.T.) ;
#5357 = EDGE_CURVE('',#4152,#4153,#2439,.T.) ;
#5358 = EDGE_CURVE('',#4151,#4153,#2440,.T.) ;
#5359 = EDGE_CURVE('',#4152,#4154,#2441,.T.) ;
#5360 = EDGE_CURVE('',#4154,#4155,#2442,.T.) ;
#5361 = EDGE_CURVE('',#4153,#4155,#2443,.T.) ;
#5362 = EDGE_CURVE('',#4154,#4156,#293,.T.) ;
#5363 = EDGE_CURVE('',#4156,#4157,#2444,.T.) ;
#5364 = EDGE_CURVE('',#4155,#4157,#294,.T.) ;
#5365 = EDGE_CURVE('',#4156,#4158,#2445,.T.) ;
#5366 = EDGE_CURVE('',#4158,#4159,#2446,.T.) ;
#5367 = EDGE_CURVE('',#4157,#4159,#2447,.T.) ;
#5368 = EDGE_CURVE('',#4158,#4160,#2448,.T.) ;
#5369 = EDGE_CURVE('',#4160,#4161,#2449,.T.) ;
#5370 = EDGE_CURVE('',#4159,#4161,#2450,.T.) ;
#5371 = EDGE_CURVE('',#4160,#4162,#295,.T.) ;
#5372 = EDGE_CURVE('',#4162,#4163,#2451,.T.) ;
#5373 = EDGE_CURVE('',#4161,#4163,#296,.T.) ;
#5374 = EDGE_CURVE('',#4162,#4164,#2452,.T.) ;
#5375 = EDGE_CURVE('',#4164,#4165,#2453,.T.) ;
#5376 = EDGE_CURVE('',#4163,#4165,#2454,.T.) ;
#5377 = EDGE_CURVE('',#4164,#4166,#2455,.T.) ;
#5378 = EDGE_CURVE('',#4166,#4167,#2456,.T.) ;
#5379 = EDGE_CURVE('',#4165,#4167,#2457,.T.) ;
#5380 = EDGE_CURVE('',#4166,#4168,#297,.T.) ;
#5381 = EDGE_CURVE('',#4168,#4169,#2458,.T.) ;
#5382 = EDGE_CURVE('',#4167,#4169,#298,.T.) ;
#5383 = EDGE_CURVE('',#4168,#4170,#2459,.T.) ;
#5384 = EDGE_CURVE('',#4170,#4171,#2460,.T.) ;
#5385 = EDGE_CURVE('',#4169,#4171,#2461,.T.) ;
#5386 = EDGE_CURVE('',#4170,#4172,#2462,.T.) ;
#5387 = EDGE_CURVE('',#4172,#4173,#2463,.T.) ;
#5388 = EDGE_CURVE('',#4171,#4173,#2464,.T.) ;
#5389 = EDGE_CURVE('',#4172,#4174,#299,.T.) ;
#5390 = EDGE_CURVE('',#4174,#4175,#2465,.T.) ;
#5391 = EDGE_CURVE('',#4173,#4175,#300,.T.) ;
#5392 = EDGE_CURVE('',#4174,#4176,#2466,.T.) ;
#5393 = EDGE_CURVE('',#4176,#4177,#2467,.T.) ;
#5394 = EDGE_CURVE('',#4175,#4177,#2468,.T.) ;
#5395 = EDGE_CURVE('',#4176,#4178,#2469,.T.) ;
#5396 = EDGE_CURVE('',#4178,#4179,#2470,.T.) ;
#5397 = EDGE_CURVE('',#4177,#4179,#2471,.T.) ;
#5398 = EDGE_CURVE('',#4178,#4180,#301,.T.) ;
#5399 = EDGE_CURVE('',#4180,#4181,#2472,.T.) ;
#5400 = EDGE_CURVE('',#4179,#4181,#302,.T.) ;
#5401 = EDGE_CURVE('',#4180,#4182,#2473,.T.) ;
#5402 = EDGE_CURVE('',#4182,#4183,#2474,.T.) ;
#5403 = EDGE_CURVE('',#4181,#4183,#2475,.T.) ;
#5404 = EDGE_CURVE('',#4182,#4184,#2476,.T.) ;
#5405 = EDGE_CURVE('',#4184,#4185,#2477,.T.) ;
#5406 = EDGE_CURVE('',#4183,#4185,#2478,.T.) ;
#5407 = EDGE_CURVE('',#4184,#4186,#303,.T.) ;
#5408 = EDGE_CURVE('',#4186,#4187,#2479,.T.) ;
#5409 = EDGE_CURVE('',#4185,#4187,#304,.T.) ;
#5410 = EDGE_CURVE('',#4186,#4188,#2480,.T.) ;
#5411 = EDGE_CURVE('',#4188,#4189,#2481,.T.) ;
#5412 = EDGE_CURVE('',#4187,#4189,#2482,.T.) ;
#5413 = EDGE_CURVE('',#4188,#4190,#2483,.T.) ;
#5414 = EDGE_CURVE('',#4190,#4191,#2484,.T.) ;
#5415 = EDGE_CURVE('',#4189,#4191,#2485,.T.) ;
#5416 = EDGE_CURVE('',#4190,#4192,#305,.T.) ;
#5417 = EDGE_CURVE('',#4192,#4193,#2486,.T.) ;
#5418 = EDGE_CURVE('',#4191,#4193,#306,.T.) ;
#5419 = EDGE_CURVE('',#4192,#4194,#2487,.T.) ;
#5420 = EDGE_CURVE('',#4194,#4195,#2488,.T.) ;
#5421 = EDGE_CURVE('',#4193,#4195,#2489,.T.) ;
#5422 = EDGE_CURVE('',#4194,#4196,#2490,.T.) ;
#5423 = EDGE_CURVE('',#4196,#4197,#2491,.T.) ;
#5424 = EDGE_CURVE('',#4195,#4197,#2492,.T.) ;
#5425 = EDGE_CURVE('',#4196,#4198,#307,.T.) ;
#5426 = EDGE_CURVE('',#4198,#4199,#2493,.T.) ;
#5427 = EDGE_CURVE('',#4197,#4199,#308,.T.) ;
#5428 = EDGE_CURVE('',#4198,#4200,#2494,.T.) ;
#5429 = EDGE_CURVE('',#4200,#4201,#2495,.T.) ;
#5430 = EDGE_CURVE('',#4199,#4201,#2496,.T.) ;
#5431 = EDGE_CURVE('',#4200,#4202,#2497,.T.) ;
#5432 = EDGE_CURVE('',#4202,#4203,#2498,.T.) ;
#5433 = EDGE_CURVE('',#4201,#4203,#2499,.T.) ;
#5434 = EDGE_CURVE('',#4202,#4204,#309,.T.) ;
#5435 = EDGE_CURVE('',#4204,#4205,#2500,.T.) ;
#5436 = EDGE_CURVE('',#4203,#4205,#310,.T.) ;
#5437 = EDGE_CURVE('',#4204,#3846,#2501,.T.) ;
#5438 = EDGE_CURVE('',#4205,#3849,#2502,.T.) ;
#5439 = EDGE_CURVE('',#4206,#4207,#2503,.T.) ;
#5440 = EDGE_CURVE('',#4208,#4206,#745,.T.) ;
#5441 = EDGE_CURVE('',#4209,#4208,#746,.T.) ;
#5442 = EDGE_CURVE('',#4210,#4209,#747,.T.) ;
#5443 = EDGE_CURVE('',#4211,#4210,#2504,.T.) ;
#5444 = EDGE_CURVE('',#4212,#4211,#748,.T.) ;
#5445 = EDGE_CURVE('',#4213,#4212,#749,.T.) ;
#5446 = EDGE_CURVE('',#4207,#4213,#750,.T.) ;
#5447 = EDGE_CURVE('',#4214,#4214,#751,.T.) ;
#5448 = EDGE_CURVE('',#4215,#4216,#2505,.T.) ;
#5449 = EDGE_CURVE('',#4217,#4215,#752,.T.) ;
#5450 = EDGE_CURVE('',#4218,#4217,#753,.T.) ;
#5451 = EDGE_CURVE('',#4219,#4218,#754,.T.) ;
#5452 = EDGE_CURVE('',#4220,#4219,#2506,.T.) ;
#5453 = EDGE_CURVE('',#4221,#4220,#755,.T.) ;
#5454 = EDGE_CURVE('',#4222,#4221,#756,.T.) ;
#5455 = EDGE_CURVE('',#4216,#4222,#757,.T.) ;
#5456 = EDGE_CURVE('',#4223,#4224,#2507,.T.) ;
#5457 = EDGE_CURVE('',#4225,#4223,#758,.T.) ;
#5458 = EDGE_CURVE('',#4226,#4225,#759,.T.) ;
#5459 = EDGE_CURVE('',#4227,#4226,#760,.T.) ;
#5460 = EDGE_CURVE('',#4228,#4227,#2508,.T.) ;
#5461 = EDGE_CURVE('',#4229,#4228,#761,.T.) ;
#5462 = EDGE_CURVE('',#4230,#4229,#762,.T.) ;
#5463 = EDGE_CURVE('',#4224,#4230,#763,.T.) ;
#5464 = EDGE_CURVE('',#4231,#4232,#2509,.T.) ;
#5465 = EDGE_CURVE('',#4233,#4231,#764,.T.) ;
#5466 = EDGE_CURVE('',#4234,#4233,#765,.T.) ;
#5467 = EDGE_CURVE('',#4235,#4234,#766,.T.) ;
#5468 = EDGE_CURVE('',#4236,#4235,#2510,.T.) ;
#5469 = EDGE_CURVE('',#4237,#4236,#767,.T.) ;
#5470 = EDGE_CURVE('',#4238,#4237,#768,.T.) ;
#5471 = EDGE_CURVE('',#4232,#4238,#769,.T.) ;
#5472 = EDGE_CURVE('',#4239,#4240,#2511,.T.) ;
#5473 = EDGE_CURVE('',#4241,#4239,#770,.T.) ;
#5474 = EDGE_CURVE('',#4242,#4241,#771,.T.) ;
#5475 = EDGE_CURVE('',#4243,#4242,#772,.T.) ;
#5476 = EDGE_CURVE('',#4244,#4243,#2512,.T.) ;
#5477 = EDGE_CURVE('',#4245,#4244,#773,.T.) ;
#5478 = EDGE_CURVE('',#4246,#4245,#774,.T.) ;
#5479 = EDGE_CURVE('',#4240,#4246,#775,.T.) ;
#5480 = EDGE_CURVE('',#4247,#4247,#776,.T.) ;
#5481 = EDGE_CURVE('',#4212,#4248,#2513,.T.) ;
#5482 = EDGE_CURVE('',#4249,#4248,#777,.T.) ;
#5483 = EDGE_CURVE('',#4213,#4249,#2514,.T.) ;
#5484 = EDGE_CURVE('',#4250,#4249,#778,.T.) ;
#5485 = EDGE_CURVE('',#4207,#4250,#2515,.T.) ;
#5486 = EDGE_CURVE('',#4206,#4251,#2516,.T.) ;
#5487 = EDGE_CURVE('',#4251,#4250,#2517,.T.) ;
#5488 = EDGE_CURVE('',#4252,#4251,#779,.T.) ;
#5489 = EDGE_CURVE('',#4208,#4252,#2518,.T.) ;
#5490 = EDGE_CURVE('',#4253,#4252,#780,.T.) ;
#5491 = EDGE_CURVE('',#4209,#4253,#2519,.T.) ;
#5492 = EDGE_CURVE('',#4254,#4253,#781,.T.) ;
#5493 = EDGE_CURVE('',#4210,#4254,#2520,.T.) ;
#5494 = EDGE_CURVE('',#4255,#4254,#2521,.T.) ;
#5495 = EDGE_CURVE('',#4211,#4255,#2522,.T.) ;
#5496 = EDGE_CURVE('',#4248,#4255,#782,.T.) ;
#5497 = EDGE_CURVE('',#4256,#4256,#783,.T.) ;
#5498 = EDGE_CURVE('',#4256,#4214,#2523,.T.) ;
#5499 = EDGE_CURVE('',#4221,#4257,#2524,.T.) ;
#5500 = EDGE_CURVE('',#4258,#4257,#784,.T.) ;
#5501 = EDGE_CURVE('',#4222,#4258,#2525,.T.) ;
#5502 = EDGE_CURVE('',#4259,#4258,#785,.T.) ;
#5503 = EDGE_CURVE('',#4216,#4259,#2526,.T.) ;
#5504 = EDGE_CURVE('',#4215,#4260,#2527,.T.) ;
#5505 = EDGE_CURVE('',#4260,#4259,#2528,.T.) ;
#5506 = EDGE_CURVE('',#4261,#4260,#786,.T.) ;
#5507 = EDGE_CURVE('',#4217,#4261,#2529,.T.) ;
#5508 = EDGE_CURVE('',#4262,#4261,#787,.T.) ;
#5509 = EDGE_CURVE('',#4218,#4262,#2530,.T.) ;
#5510 = EDGE_CURVE('',#4263,#4262,#788,.T.) ;
#5511 = EDGE_CURVE('',#4219,#4263,#2531,.T.) ;
#5512 = EDGE_CURVE('',#4264,#4263,#2532,.T.) ;
#5513 = EDGE_CURVE('',#4220,#4264,#2533,.T.) ;
#5514 = EDGE_CURVE('',#4257,#4264,#789,.T.) ;
#5515 = EDGE_CURVE('',#4229,#4265,#2534,.T.) ;
#5516 = EDGE_CURVE('',#4266,#4265,#790,.T.) ;
#5517 = EDGE_CURVE('',#4230,#4266,#2535,.T.) ;
#5518 = EDGE_CURVE('',#4267,#4266,#791,.T.) ;
#5519 = EDGE_CURVE('',#4224,#4267,#2536,.T.) ;
#5520 = EDGE_CURVE('',#4223,#4268,#2537,.T.) ;
#5521 = EDGE_CURVE('',#4268,#4267,#2538,.T.) ;
#5522 = EDGE_CURVE('',#4269,#4268,#792,.T.) ;
#5523 = EDGE_CURVE('',#4225,#4269,#2539,.T.) ;
#5524 = EDGE_CURVE('',#4270,#4269,#793,.T.) ;
#5525 = EDGE_CURVE('',#4226,#4270,#2540,.T.) ;
#5526 = EDGE_CURVE('',#4271,#4270,#794,.T.) ;
#5527 = EDGE_CURVE('',#4227,#4271,#2541,.T.) ;
#5528 = EDGE_CURVE('',#4272,#4271,#2542,.T.) ;
#5529 = EDGE_CURVE('',#4228,#4272,#2543,.T.) ;
#5530 = EDGE_CURVE('',#4265,#4272,#795,.T.) ;
#5531 = EDGE_CURVE('',#4237,#4273,#2544,.T.) ;
#5532 = EDGE_CURVE('',#4274,#4273,#796,.T.) ;
#5533 = EDGE_CURVE('',#4238,#4274,#2545,.T.) ;
#5534 = EDGE_CURVE('',#4275,#4274,#797,.T.) ;
#5535 = EDGE_CURVE('',#4232,#4275,#2546,.T.) ;
#5536 = EDGE_CURVE('',#4231,#4276,#2547,.T.) ;
#5537 = EDGE_CURVE('',#4276,#4275,#2548,.T.) ;
#5538 = EDGE_CURVE('',#4277,#4276,#798,.T.) ;
#5539 = EDGE_CURVE('',#4233,#4277,#2549,.T.) ;
#5540 = EDGE_CURVE('',#4278,#4277,#799,.T.) ;
#5541 = EDGE_CURVE('',#4234,#4278,#2550,.T.) ;
#5542 = EDGE_CURVE('',#4279,#4278,#800,.T.) ;
#5543 = EDGE_CURVE('',#4235,#4279,#2551,.T.) ;
#5544 = EDGE_CURVE('',#4280,#4279,#2552,.T.) ;
#5545 = EDGE_CURVE('',#4236,#4280,#2553,.T.) ;
#5546 = EDGE_CURVE('',#4273,#4280,#801,.T.) ;
#5547 = EDGE_CURVE('',#4245,#4281,#2554,.T.) ;
#5548 = EDGE_CURVE('',#4282,#4281,#802,.T.) ;
#5549 = EDGE_CURVE('',#4246,#4282,#2555,.T.) ;
#5550 = EDGE_CURVE('',#4283,#4282,#803,.T.) ;
#5551 = EDGE_CURVE('',#4240,#4283,#2556,.T.) ;
#5552 = EDGE_CURVE('',#4239,#4284,#2557,.T.) ;
#5553 = EDGE_CURVE('',#4284,#4283,#2558,.T.) ;
#5554 = EDGE_CURVE('',#4285,#4284,#804,.T.) ;
#5555 = EDGE_CURVE('',#4241,#4285,#2559,.T.) ;
#5556 = EDGE_CURVE('',#4286,#4285,#805,.T.) ;
#5557 = EDGE_CURVE('',#4242,#4286,#2560,.T.) ;
#5558 = EDGE_CURVE('',#4287,#4286,#806,.T.) ;
#5559 = EDGE_CURVE('',#4243,#4287,#2561,.T.) ;
#5560 = EDGE_CURVE('',#4288,#4287,#2562,.T.) ;
#5561 = EDGE_CURVE('',#4244,#4288,#2563,.T.) ;
#5562 = EDGE_CURVE('',#4281,#4288,#807,.T.) ;
#5563 = EDGE_CURVE('',#4247,#4289,#2564,.T.) ;
#5564 = EDGE_CURVE('',#4289,#4289,#808,.T.) ;
#5565 = EDGE_CURVE('',#4290,#4290,#809,.T.) ;
#5566 = EDGE_CURVE('',#4290,#4291,#2565,.T.) ;
#5567 = EDGE_CURVE('',#4291,#4291,#810,.T.) ;
#5568 = ORIENTED_EDGE('',*,*,#4292,.T.) ;
#5569 = ORIENTED_EDGE('',*,*,#4293,.T.) ;
#5570 = ORIENTED_EDGE('',*,*,#4294,.T.) ;
#5571 = ORIENTED_EDGE('',*,*,#4295,.T.) ;
#5572 = ORIENTED_EDGE('',*,*,#4293,.F.) ;
#5573 = ORIENTED_EDGE('',*,*,#4296,.T.) ;
#5574 = ORIENTED_EDGE('',*,*,#4297,.T.) ;
#5575 = ORIENTED_EDGE('',*,*,#4298,.T.) ;
#5576 = ORIENTED_EDGE('',*,*,#4299,.T.) ;
#5577 = ORIENTED_EDGE('',*,*,#4300,.T.) ;
#5578 = ORIENTED_EDGE('',*,*,#4298,.F.) ;
#5579 = ORIENTED_EDGE('',*,*,#4301,.T.) ;
#5580 = ORIENTED_EDGE('',*,*,#4302,.T.) ;
#5581 = ORIENTED_EDGE('',*,*,#4303,.T.) ;
#5582 = ORIENTED_EDGE('',*,*,#4302,.F.) ;
#5583 = ORIENTED_EDGE('',*,*,#4296,.F.) ;
#5584 = ORIENTED_EDGE('',*,*,#4292,.F.) ;
#5585 = ORIENTED_EDGE('',*,*,#4304,.T.) ;
#5586 = ORIENTED_EDGE('',*,*,#4305,.T.) ;
#5587 = ORIENTED_EDGE('',*,*,#4304,.F.) ;
#5588 = ORIENTED_EDGE('',*,*,#4294,.F.) ;
#5589 = ORIENTED_EDGE('',*,*,#4295,.F.) ;
#5590 = ORIENTED_EDGE('',*,*,#4306,.T.) ;
#5591 = ORIENTED_EDGE('',*,*,#4307,.T.) ;
#5592 = ORIENTED_EDGE('',*,*,#4306,.F.) ;
#5593 = ORIENTED_EDGE('',*,*,#4301,.F.) ;
#5594 = ORIENTED_EDGE('',*,*,#4297,.F.) ;
#5595 = ORIENTED_EDGE('',*,*,#4308,.T.) ;
#5596 = ORIENTED_EDGE('',*,*,#4309,.T.) ;
#5597 = ORIENTED_EDGE('',*,*,#4308,.F.) ;
#5598 = ORIENTED_EDGE('',*,*,#4299,.F.) ;
#5599 = ORIENTED_EDGE('',*,*,#4300,.F.) ;
#5600 = ORIENTED_EDGE('',*,*,#4310,.T.) ;
#5601 = ORIENTED_EDGE('',*,*,#4311,.T.) ;
#5602 = ORIENTED_EDGE('',*,*,#4312,.F.) ;
#5603 = ORIENTED_EDGE('',*,*,#4311,.F.) ;
#5604 = ORIENTED_EDGE('',*,*,#4307,.F.) ;
#5605 = ORIENTED_EDGE('',*,*,#4305,.F.) ;
#5606 = ORIENTED_EDGE('',*,*,#4303,.F.) ;
#5607 = ORIENTED_EDGE('',*,*,#4309,.F.) ;
#5608 = ORIENTED_EDGE('',*,*,#4313,.F.) ;
#5609 = ORIENTED_EDGE('',*,*,#4314,.T.) ;
#5610 = ORIENTED_EDGE('',*,*,#4315,.T.) ;
#5611 = ORIENTED_EDGE('',*,*,#4313,.T.) ;
#5612 = ORIENTED_EDGE('',*,*,#4315,.F.) ;
#5613 = ORIENTED_EDGE('',*,*,#4310,.F.) ;
#5614 = ORIENTED_EDGE('',*,*,#4312,.T.) ;
#5615 = ORIENTED_EDGE('',*,*,#4316,.T.) ;
#5616 = ORIENTED_EDGE('',*,*,#4314,.F.) ;
#5617 = ORIENTED_EDGE('',*,*,#4316,.F.) ;
#5618 = ORIENTED_EDGE('',*,*,#4317,.T.) ;
#5619 = ORIENTED_EDGE('',*,*,#4318,.T.) ;
#5620 = ORIENTED_EDGE('',*,*,#4319,.T.) ;
#5621 = ORIENTED_EDGE('',*,*,#4320,.T.) ;
#5622 = ORIENTED_EDGE('',*,*,#4321,.T.) ;
#5623 = ORIENTED_EDGE('',*,*,#4322,.T.) ;
#5624 = ORIENTED_EDGE('',*,*,#4323,.T.) ;
#5625 = ORIENTED_EDGE('',*,*,#4324,.T.) ;
#5626 = ORIENTED_EDGE('',*,*,#4325,.T.) ;
#5627 = ORIENTED_EDGE('',*,*,#4317,.F.) ;
#5628 = ORIENTED_EDGE('',*,*,#4326,.T.) ;
#5629 = ORIENTED_EDGE('',*,*,#4327,.T.) ;
#5630 = ORIENTED_EDGE('',*,*,#4328,.T.) ;
#5631 = ORIENTED_EDGE('',*,*,#4329,.T.) ;
#5632 = ORIENTED_EDGE('',*,*,#4330,.T.) ;
#5633 = ORIENTED_EDGE('',*,*,#4323,.F.) ;
#5634 = ORIENTED_EDGE('',*,*,#4331,.T.) ;
#5635 = ORIENTED_EDGE('',*,*,#4332,.T.) ;
#5636 = ORIENTED_EDGE('',*,*,#4333,.T.) ;
#5637 = ORIENTED_EDGE('',*,*,#4334,.T.) ;
#5638 = ORIENTED_EDGE('',*,*,#4335,.T.) ;
#5639 = ORIENTED_EDGE('',*,*,#4328,.F.) ;
#5640 = ORIENTED_EDGE('',*,*,#4336,.T.) ;
#5641 = ORIENTED_EDGE('',*,*,#4337,.T.) ;
#5642 = ORIENTED_EDGE('',*,*,#4338,.F.) ;
#5643 = ORIENTED_EDGE('',*,*,#4339,.T.) ;
#5644 = ORIENTED_EDGE('',*,*,#4340,.F.) ;
#5645 = ORIENTED_EDGE('',*,*,#4341,.T.) ;
#5646 = ORIENTED_EDGE('',*,*,#4342,.T.) ;
#5647 = ORIENTED_EDGE('',*,*,#4343,.F.) ;
#5648 = ORIENTED_EDGE('',*,*,#4344,.T.) ;
#5649 = ORIENTED_EDGE('',*,*,#4345,.F.) ;
#5650 = ORIENTED_EDGE('',*,*,#4346,.T.) ;
#5651 = ORIENTED_EDGE('',*,*,#4347,.F.) ;
#5652 = ORIENTED_EDGE('',*,*,#4342,.F.) ;
#5653 = ORIENTED_EDGE('',*,*,#4348,.F.) ;
#5654 = ORIENTED_EDGE('',*,*,#4349,.T.) ;
#5655 = ORIENTED_EDGE('',*,*,#4350,.F.) ;
#5656 = ORIENTED_EDGE('',*,*,#4346,.F.) ;
#5657 = ORIENTED_EDGE('',*,*,#4351,.F.) ;
#5658 = ORIENTED_EDGE('',*,*,#4352,.T.) ;
#5659 = ORIENTED_EDGE('',*,*,#4353,.F.) ;
#5660 = ORIENTED_EDGE('',*,*,#4349,.F.) ;
#5661 = ORIENTED_EDGE('',*,*,#4354,.F.) ;
#5662 = ORIENTED_EDGE('',*,*,#4355,.F.) ;
#5663 = ORIENTED_EDGE('',*,*,#4356,.F.) ;
#5664 = ORIENTED_EDGE('',*,*,#4357,.T.) ;
#5665 = ORIENTED_EDGE('',*,*,#4358,.F.) ;
#5666 = ORIENTED_EDGE('',*,*,#4359,.T.) ;
#5667 = ORIENTED_EDGE('',*,*,#4360,.T.) ;
#5668 = ORIENTED_EDGE('',*,*,#4361,.F.) ;
#5669 = ORIENTED_EDGE('',*,*,#4360,.F.) ;
#5670 = ORIENTED_EDGE('',*,*,#4362,.F.) ;
#5671 = ORIENTED_EDGE('',*,*,#4363,.F.) ;
#5672 = ORIENTED_EDGE('',*,*,#4364,.F.) ;
#5673 = ORIENTED_EDGE('',*,*,#4365,.F.) ;
#5674 = ORIENTED_EDGE('',*,*,#4366,.F.) ;
#5675 = ORIENTED_EDGE('',*,*,#4367,.T.) ;
#5676 = ORIENTED_EDGE('',*,*,#4368,.T.) ;
#5677 = ORIENTED_EDGE('',*,*,#4320,.F.) ;
#5678 = ORIENTED_EDGE('',*,*,#4369,.T.) ;
#5679 = ORIENTED_EDGE('',*,*,#4344,.F.) ;
#5680 = ORIENTED_EDGE('',*,*,#4370,.F.) ;
#5681 = ORIENTED_EDGE('',*,*,#4371,.F.) ;
#5682 = ORIENTED_EDGE('',*,*,#4372,.T.) ;
#5683 = ORIENTED_EDGE('',*,*,#4366,.T.) ;
#5684 = ORIENTED_EDGE('',*,*,#4372,.F.) ;
#5685 = ORIENTED_EDGE('',*,*,#4359,.F.) ;
#5686 = ORIENTED_EDGE('',*,*,#4361,.T.) ;
#5687 = ORIENTED_EDGE('',*,*,#4373,.T.) ;
#5688 = ORIENTED_EDGE('',*,*,#4369,.F.) ;
#5689 = ORIENTED_EDGE('',*,*,#4373,.F.) ;
#5690 = ORIENTED_EDGE('',*,*,#4374,.T.) ;
#5691 = ORIENTED_EDGE('',*,*,#4375,.F.) ;
#5692 = ORIENTED_EDGE('',*,*,#4376,.F.) ;
#5693 = ORIENTED_EDGE('',*,*,#4374,.F.) ;
#5694 = ORIENTED_EDGE('',*,*,#4377,.T.) ;
#5695 = ORIENTED_EDGE('',*,*,#4378,.T.) ;
#5696 = ORIENTED_EDGE('',*,*,#4378,.F.) ;
#5697 = ORIENTED_EDGE('',*,*,#4379,.T.) ;
#5698 = ORIENTED_EDGE('',*,*,#4380,.T.) ;
#5699 = ORIENTED_EDGE('',*,*,#4381,.T.) ;
#5700 = ORIENTED_EDGE('',*,*,#4382,.T.) ;
#5701 = ORIENTED_EDGE('',*,*,#4383,.T.) ;
#5702 = ORIENTED_EDGE('',*,*,#4384,.T.) ;
#5703 = ORIENTED_EDGE('',*,*,#4385,.T.) ;
#5704 = ORIENTED_EDGE('',*,*,#4386,.T.) ;
#5705 = ORIENTED_EDGE('',*,*,#4387,.T.) ;
#5706 = ORIENTED_EDGE('',*,*,#4388,.T.) ;
#5707 = ORIENTED_EDGE('',*,*,#4389,.F.) ;
#5708 = ORIENTED_EDGE('',*,*,#4384,.F.) ;
#5709 = ORIENTED_EDGE('',*,*,#4355,.T.) ;
#5710 = ORIENTED_EDGE('',*,*,#4390,.F.) ;
#5711 = ORIENTED_EDGE('',*,*,#4352,.F.) ;
#5712 = ORIENTED_EDGE('',*,*,#4391,.F.) ;
#5713 = ORIENTED_EDGE('',*,*,#4392,.T.) ;
#5714 = ORIENTED_EDGE('',*,*,#4385,.F.) ;
#5715 = ORIENTED_EDGE('',*,*,#4389,.T.) ;
#5716 = ORIENTED_EDGE('',*,*,#4393,.T.) ;
#5717 = ORIENTED_EDGE('',*,*,#4356,.T.) ;
#5718 = ORIENTED_EDGE('',*,*,#4391,.T.) ;
#5719 = ORIENTED_EDGE('',*,*,#4354,.T.) ;
#5720 = ORIENTED_EDGE('',*,*,#4351,.T.) ;
#5721 = ORIENTED_EDGE('',*,*,#4348,.T.) ;
#5722 = ORIENTED_EDGE('',*,*,#4345,.T.) ;
#5723 = ORIENTED_EDGE('',*,*,#4371,.T.) ;
#5724 = ORIENTED_EDGE('',*,*,#4394,.F.) ;
#5725 = ORIENTED_EDGE('',*,*,#4395,.T.) ;
#5726 = ORIENTED_EDGE('',*,*,#4396,.T.) ;
#5727 = ORIENTED_EDGE('',*,*,#4381,.F.) ;
#5728 = ORIENTED_EDGE('',*,*,#4338,.T.) ;
#5729 = ORIENTED_EDGE('',*,*,#4397,.T.) ;
#5730 = ORIENTED_EDGE('',*,*,#4398,.T.) ;
#5731 = ORIENTED_EDGE('',*,*,#4333,.F.) ;
#5732 = ORIENTED_EDGE('',*,*,#4399,.T.) ;
#5733 = ORIENTED_EDGE('',*,*,#4400,.T.) ;
#5734 = ORIENTED_EDGE('',*,*,#4401,.F.) ;
#5735 = ORIENTED_EDGE('',*,*,#4402,.T.) ;
#5736 = ORIENTED_EDGE('',*,*,#4403,.F.) ;
#5737 = ORIENTED_EDGE('',*,*,#4404,.T.) ;
#5738 = ORIENTED_EDGE('',*,*,#4405,.T.) ;
#5739 = ORIENTED_EDGE('',*,*,#4406,.F.) ;
#5740 = ORIENTED_EDGE('',*,*,#4407,.F.) ;
#5741 = ORIENTED_EDGE('',*,*,#4408,.T.) ;
#5742 = ORIENTED_EDGE('',*,*,#4409,.F.) ;
#5743 = ORIENTED_EDGE('',*,*,#4410,.F.) ;
#5744 = ORIENTED_EDGE('',*,*,#4375,.T.) ;
#5745 = ORIENTED_EDGE('',*,*,#4376,.T.) ;
#5746 = ORIENTED_EDGE('',*,*,#4410,.T.) ;
#5747 = ORIENTED_EDGE('',*,*,#4411,.T.) ;
#5748 = ORIENTED_EDGE('',*,*,#4412,.T.) ;
#5749 = ORIENTED_EDGE('',*,*,#4404,.F.) ;
#5750 = ORIENTED_EDGE('',*,*,#4413,.T.) ;
#5751 = ORIENTED_EDGE('',*,*,#4414,.F.) ;
#5752 = ORIENTED_EDGE('',*,*,#4415,.T.) ;
#5753 = ORIENTED_EDGE('',*,*,#4416,.T.) ;
#5754 = ORIENTED_EDGE('',*,*,#4339,.F.) ;
#5755 = ORIENTED_EDGE('',*,*,#4400,.F.) ;
#5756 = ORIENTED_EDGE('',*,*,#4399,.F.) ;
#5757 = ORIENTED_EDGE('',*,*,#4337,.F.) ;
#5758 = ORIENTED_EDGE('',*,*,#4336,.F.) ;
#5759 = ORIENTED_EDGE('',*,*,#4332,.F.) ;
#5760 = ORIENTED_EDGE('',*,*,#4331,.F.) ;
#5761 = ORIENTED_EDGE('',*,*,#4327,.F.) ;
#5762 = ORIENTED_EDGE('',*,*,#4326,.F.) ;
#5763 = ORIENTED_EDGE('',*,*,#4322,.F.) ;
#5764 = ORIENTED_EDGE('',*,*,#4321,.F.) ;
#5765 = ORIENTED_EDGE('',*,*,#4368,.F.) ;
#5766 = ORIENTED_EDGE('',*,*,#4417,.F.) ;
#5767 = ORIENTED_EDGE('',*,*,#4418,.T.) ;
#5768 = ORIENTED_EDGE('',*,*,#4419,.T.) ;
#5769 = ORIENTED_EDGE('',*,*,#4414,.T.) ;
#5770 = ORIENTED_EDGE('',*,*,#4420,.T.) ;
#5771 = ORIENTED_EDGE('',*,*,#4405,.F.) ;
#5772 = ORIENTED_EDGE('',*,*,#4412,.F.) ;
#5773 = ORIENTED_EDGE('',*,*,#4421,.T.) ;
#5774 = ORIENTED_EDGE('',*,*,#4408,.F.) ;
#5775 = ORIENTED_EDGE('',*,*,#4422,.T.) ;
#5776 = ORIENTED_EDGE('',*,*,#4415,.F.) ;
#5777 = ORIENTED_EDGE('',*,*,#4419,.F.) ;
#5778 = ORIENTED_EDGE('',*,*,#4423,.T.) ;
#5779 = ORIENTED_EDGE('',*,*,#4394,.T.) ;
#5780 = ORIENTED_EDGE('',*,*,#4370,.T.) ;
#5781 = ORIENTED_EDGE('',*,*,#4343,.T.) ;
#5782 = ORIENTED_EDGE('',*,*,#4347,.T.) ;
#5783 = ORIENTED_EDGE('',*,*,#4350,.T.) ;
#5784 = ORIENTED_EDGE('',*,*,#4353,.T.) ;
#5785 = ORIENTED_EDGE('',*,*,#4390,.T.) ;
#5786 = ORIENTED_EDGE('',*,*,#4358,.T.) ;
#5787 = ORIENTED_EDGE('',*,*,#4424,.T.) ;
#5788 = ORIENTED_EDGE('',*,*,#4425,.T.) ;
#5789 = ORIENTED_EDGE('',*,*,#4377,.F.) ;
#5790 = ORIENTED_EDGE('',*,*,#4426,.T.) ;
#5791 = ORIENTED_EDGE('',*,*,#4427,.T.) ;
#5792 = ORIENTED_EDGE('',*,*,#4425,.F.) ;
#5793 = ORIENTED_EDGE('',*,*,#4428,.T.) ;
#5794 = ORIENTED_EDGE('',*,*,#4382,.F.) ;
#5795 = ORIENTED_EDGE('',*,*,#4396,.F.) ;
#5796 = ORIENTED_EDGE('',*,*,#4429,.T.) ;
#5797 = ORIENTED_EDGE('',*,*,#4430,.T.) ;
#5798 = ORIENTED_EDGE('',*,*,#4387,.F.) ;
#5799 = ORIENTED_EDGE('',*,*,#4431,.T.) ;
#5800 = ORIENTED_EDGE('',*,*,#4426,.F.) ;
#5801 = ORIENTED_EDGE('',*,*,#4379,.F.) ;
#5802 = ORIENTED_EDGE('',*,*,#4432,.T.) ;
#5803 = ORIENTED_EDGE('',*,*,#4417,.T.) ;
#5804 = ORIENTED_EDGE('',*,*,#4367,.F.) ;
#5805 = ORIENTED_EDGE('',*,*,#4319,.F.) ;
#5806 = ORIENTED_EDGE('',*,*,#4318,.F.) ;
#5807 = ORIENTED_EDGE('',*,*,#4325,.F.) ;
#5808 = ORIENTED_EDGE('',*,*,#4324,.F.) ;
#5809 = ORIENTED_EDGE('',*,*,#4330,.F.) ;
#5810 = ORIENTED_EDGE('',*,*,#4329,.F.) ;
#5811 = ORIENTED_EDGE('',*,*,#4335,.F.) ;
#5812 = ORIENTED_EDGE('',*,*,#4334,.F.) ;
#5813 = ORIENTED_EDGE('',*,*,#4398,.F.) ;
#5814 = ORIENTED_EDGE('',*,*,#4397,.F.) ;
#5815 = ORIENTED_EDGE('',*,*,#4341,.F.) ;
#5816 = ORIENTED_EDGE('',*,*,#4433,.T.) ;
#5817 = ORIENTED_EDGE('',*,*,#4402,.F.) ;
#5818 = ORIENTED_EDGE('',*,*,#4434,.T.) ;
#5819 = ORIENTED_EDGE('',*,*,#4435,.T.) ;
#5820 = ORIENTED_EDGE('',*,*,#4431,.F.) ;
#5821 = ORIENTED_EDGE('',*,*,#4386,.F.) ;
#5822 = ORIENTED_EDGE('',*,*,#4383,.F.) ;
#5823 = ORIENTED_EDGE('',*,*,#4392,.F.) ;
#5824 = ORIENTED_EDGE('',*,*,#4423,.F.) ;
#5825 = ORIENTED_EDGE('',*,*,#4427,.F.) ;
#5826 = ORIENTED_EDGE('',*,*,#4435,.F.) ;
#5827 = ORIENTED_EDGE('',*,*,#4436,.T.) ;
#5828 = ORIENTED_EDGE('',*,*,#4437,.T.) ;
#5829 = ORIENTED_EDGE('',*,*,#4362,.T.) ;
#5830 = ORIENTED_EDGE('',*,*,#4437,.F.) ;
#5831 = ORIENTED_EDGE('',*,*,#4436,.F.) ;
#5832 = ORIENTED_EDGE('',*,*,#4434,.F.) ;
#5833 = ORIENTED_EDGE('',*,*,#4424,.F.) ;
#5834 = ORIENTED_EDGE('',*,*,#4357,.F.) ;
#5835 = ORIENTED_EDGE('',*,*,#4393,.F.) ;
#5836 = ORIENTED_EDGE('',*,*,#4388,.F.) ;
#5837 = ORIENTED_EDGE('',*,*,#4430,.F.) ;
#5838 = ORIENTED_EDGE('',*,*,#4438,.T.) ;
#5839 = ORIENTED_EDGE('',*,*,#4439,.T.) ;
#5840 = ORIENTED_EDGE('',*,*,#4440,.T.) ;
#5841 = ORIENTED_EDGE('',*,*,#4438,.F.) ;
#5842 = ORIENTED_EDGE('',*,*,#4429,.F.) ;
#5843 = ORIENTED_EDGE('',*,*,#4395,.F.) ;
#5844 = ORIENTED_EDGE('',*,*,#4380,.F.) ;
#5845 = ORIENTED_EDGE('',*,*,#4428,.F.) ;
#5846 = ORIENTED_EDGE('',*,*,#4441,.T.) ;
#5847 = ORIENTED_EDGE('',*,*,#4363,.T.) ;
#5848 = ORIENTED_EDGE('',*,*,#4441,.F.) ;
#5849 = ORIENTED_EDGE('',*,*,#4439,.F.) ;
#5850 = ORIENTED_EDGE('',*,*,#4440,.F.) ;
#5851 = ORIENTED_EDGE('',*,*,#4409,.T.) ;
#5852 = ORIENTED_EDGE('',*,*,#4421,.F.) ;
#5853 = ORIENTED_EDGE('',*,*,#4418,.F.) ;
#5854 = ORIENTED_EDGE('',*,*,#4413,.F.) ;
#5855 = ORIENTED_EDGE('',*,*,#4432,.F.) ;
#5856 = ORIENTED_EDGE('',*,*,#4401,.T.) ;
#5857 = ORIENTED_EDGE('',*,*,#4442,.T.) ;
#5858 = ORIENTED_EDGE('',*,*,#4443,.T.) ;
#5859 = ORIENTED_EDGE('',*,*,#4444,.T.) ;
#5860 = ORIENTED_EDGE('',*,*,#4442,.F.) ;
#5861 = ORIENTED_EDGE('',*,*,#4445,.T.) ;
#5862 = ORIENTED_EDGE('',*,*,#4446,.T.) ;
#5863 = ORIENTED_EDGE('',*,*,#4406,.T.) ;
#5864 = ORIENTED_EDGE('',*,*,#4420,.F.) ;
#5865 = ORIENTED_EDGE('',*,*,#4411,.F.) ;
#5866 = ORIENTED_EDGE('',*,*,#4403,.T.) ;
#5867 = ORIENTED_EDGE('',*,*,#4433,.F.) ;
#5868 = ORIENTED_EDGE('',*,*,#4340,.T.) ;
#5869 = ORIENTED_EDGE('',*,*,#4416,.F.) ;
#5870 = ORIENTED_EDGE('',*,*,#4422,.F.) ;
#5871 = ORIENTED_EDGE('',*,*,#4407,.T.) ;
#5872 = ORIENTED_EDGE('',*,*,#4446,.F.) ;
#5873 = ORIENTED_EDGE('',*,*,#4447,.T.) ;
#5874 = ORIENTED_EDGE('',*,*,#4448,.T.) ;
#5875 = ORIENTED_EDGE('',*,*,#4365,.T.) ;
#5876 = ORIENTED_EDGE('',*,*,#4448,.F.) ;
#5877 = ORIENTED_EDGE('',*,*,#4447,.F.) ;
#5878 = ORIENTED_EDGE('',*,*,#4445,.F.) ;
#5879 = ORIENTED_EDGE('',*,*,#4449,.T.) ;
#5880 = ORIENTED_EDGE('',*,*,#4364,.T.) ;
#5881 = ORIENTED_EDGE('',*,*,#4449,.F.) ;
#5882 = ORIENTED_EDGE('',*,*,#4443,.F.) ;
#5883 = ORIENTED_EDGE('',*,*,#4444,.F.) ;
#5884 = ORIENTED_EDGE('',*,*,#4450,.F.) ;
#5885 = ORIENTED_EDGE('',*,*,#4451,.T.) ;
#5886 = ORIENTED_EDGE('',*,*,#4452,.F.) ;
#5887 = ORIENTED_EDGE('',*,*,#4453,.F.) ;
#5888 = ORIENTED_EDGE('',*,*,#4451,.F.) ;
#5889 = ORIENTED_EDGE('',*,*,#4450,.T.) ;
#5890 = ORIENTED_EDGE('',*,*,#4454,.T.) ;
#5891 = ORIENTED_EDGE('',*,*,#4452,.T.) ;
#5892 = ORIENTED_EDGE('',*,*,#4453,.T.) ;
#5893 = ORIENTED_EDGE('',*,*,#4455,.T.) ;
#5894 = ORIENTED_EDGE('',*,*,#4454,.F.) ;
#5895 = ORIENTED_EDGE('',*,*,#4455,.F.) ;
#5896 = ORIENTED_EDGE('',*,*,#4456,.T.) ;
#5897 = ORIENTED_EDGE('',*,*,#4457,.T.) ;
#5898 = ORIENTED_EDGE('',*,*,#4458,.F.) ;
#5899 = ORIENTED_EDGE('',*,*,#4457,.F.) ;
#5900 = ORIENTED_EDGE('',*,*,#4458,.T.) ;
#5901 = ORIENTED_EDGE('',*,*,#4456,.F.) ;
#5902 = ORIENTED_EDGE('',*,*,#4459,.F.) ;
#5903 = ORIENTED_EDGE('',*,*,#4460,.F.) ;
#5904 = ORIENTED_EDGE('',*,*,#4461,.T.) ;
#5905 = ORIENTED_EDGE('',*,*,#4462,.F.) ;
#5906 = ORIENTED_EDGE('',*,*,#4463,.F.) ;
#5907 = ORIENTED_EDGE('',*,*,#4464,.F.) ;
#5908 = ORIENTED_EDGE('',*,*,#4459,.T.) ;
#5909 = ORIENTED_EDGE('',*,*,#4465,.F.) ;
#5910 = ORIENTED_EDGE('',*,*,#4466,.F.) ;
#5911 = ORIENTED_EDGE('',*,*,#4467,.F.) ;
#5912 = ORIENTED_EDGE('',*,*,#4463,.T.) ;
#5913 = ORIENTED_EDGE('',*,*,#4468,.F.) ;
#5914 = ORIENTED_EDGE('',*,*,#4469,.F.) ;
#5915 = ORIENTED_EDGE('',*,*,#4470,.F.) ;
#5916 = ORIENTED_EDGE('',*,*,#4466,.T.) ;
#5917 = ORIENTED_EDGE('',*,*,#4471,.F.) ;
#5918 = ORIENTED_EDGE('',*,*,#4469,.T.) ;
#5919 = ORIENTED_EDGE('',*,*,#4472,.F.) ;
#5920 = ORIENTED_EDGE('',*,*,#4473,.F.) ;
#5921 = ORIENTED_EDGE('',*,*,#4474,.F.) ;
#5922 = ORIENTED_EDGE('',*,*,#4475,.T.) ;
#5923 = ORIENTED_EDGE('',*,*,#4476,.T.) ;
#5924 = ORIENTED_EDGE('',*,*,#4475,.F.) ;
#5925 = ORIENTED_EDGE('',*,*,#4477,.F.) ;
#5926 = ORIENTED_EDGE('',*,*,#4473,.T.) ;
#5927 = ORIENTED_EDGE('',*,*,#4478,.F.) ;
#5928 = ORIENTED_EDGE('',*,*,#4479,.F.) ;
#5929 = ORIENTED_EDGE('',*,*,#4480,.T.) ;
#5930 = ORIENTED_EDGE('',*,*,#4476,.F.) ;
#5931 = ORIENTED_EDGE('',*,*,#4480,.F.) ;
#5932 = ORIENTED_EDGE('',*,*,#4460,.T.) ;
#5933 = ORIENTED_EDGE('',*,*,#4464,.T.) ;
#5934 = ORIENTED_EDGE('',*,*,#4467,.T.) ;
#5935 = ORIENTED_EDGE('',*,*,#4470,.T.) ;
#5936 = ORIENTED_EDGE('',*,*,#4474,.T.) ;
#5937 = ORIENTED_EDGE('',*,*,#4477,.T.) ;
#5938 = ORIENTED_EDGE('',*,*,#4479,.T.) ;
#5939 = ORIENTED_EDGE('',*,*,#4481,.T.) ;
#5940 = ORIENTED_EDGE('',*,*,#4482,.F.) ;
#5941 = ORIENTED_EDGE('',*,*,#4481,.F.) ;
#5942 = ORIENTED_EDGE('',*,*,#4478,.T.) ;
#5943 = ORIENTED_EDGE('',*,*,#4472,.T.) ;
#5944 = ORIENTED_EDGE('',*,*,#4471,.T.) ;
#5945 = ORIENTED_EDGE('',*,*,#4468,.T.) ;
#5946 = ORIENTED_EDGE('',*,*,#4465,.T.) ;
#5947 = ORIENTED_EDGE('',*,*,#4462,.T.) ;
#5948 = ORIENTED_EDGE('',*,*,#4483,.F.) ;
#5949 = ORIENTED_EDGE('',*,*,#4484,.F.) ;
#5950 = ORIENTED_EDGE('',*,*,#4485,.F.) ;
#5951 = ORIENTED_EDGE('',*,*,#4486,.T.) ;
#5952 = ORIENTED_EDGE('',*,*,#4483,.T.) ;
#5953 = ORIENTED_EDGE('',*,*,#4461,.F.) ;
#5954 = ORIENTED_EDGE('',*,*,#4482,.T.) ;
#5955 = ORIENTED_EDGE('',*,*,#4484,.T.) ;
#5956 = ORIENTED_EDGE('',*,*,#4486,.F.) ;
#5957 = ORIENTED_EDGE('',*,*,#4485,.T.) ;
#5958 = ORIENTED_EDGE('',*,*,#4487,.T.) ;
#5959 = ORIENTED_EDGE('',*,*,#4488,.T.) ;
#5960 = ORIENTED_EDGE('',*,*,#4489,.T.) ;
#5961 = ORIENTED_EDGE('',*,*,#4490,.T.) ;
#5962 = ORIENTED_EDGE('',*,*,#4491,.T.) ;
#5963 = ORIENTED_EDGE('',*,*,#4492,.T.) ;
#5964 = ORIENTED_EDGE('',*,*,#4493,.T.) ;
#5965 = ORIENTED_EDGE('',*,*,#4494,.T.) ;
#5966 = ORIENTED_EDGE('',*,*,#4495,.F.) ;
#5967 = ORIENTED_EDGE('',*,*,#4487,.F.) ;
#5968 = ORIENTED_EDGE('',*,*,#4495,.T.) ;
#5969 = ORIENTED_EDGE('',*,*,#4496,.T.) ;
#5970 = ORIENTED_EDGE('',*,*,#4497,.F.) ;
#5971 = ORIENTED_EDGE('',*,*,#4488,.F.) ;
#5972 = ORIENTED_EDGE('',*,*,#4497,.T.) ;
#5973 = ORIENTED_EDGE('',*,*,#4498,.T.) ;
#5974 = ORIENTED_EDGE('',*,*,#4499,.F.) ;
#5975 = ORIENTED_EDGE('',*,*,#4489,.F.) ;
#5976 = ORIENTED_EDGE('',*,*,#4499,.T.) ;
#5977 = ORIENTED_EDGE('',*,*,#4500,.T.) ;
#5978 = ORIENTED_EDGE('',*,*,#4501,.F.) ;
#5979 = ORIENTED_EDGE('',*,*,#4490,.F.) ;
#5980 = ORIENTED_EDGE('',*,*,#4501,.T.) ;
#5981 = ORIENTED_EDGE('',*,*,#4502,.T.) ;
#5982 = ORIENTED_EDGE('',*,*,#4503,.F.) ;
#5983 = ORIENTED_EDGE('',*,*,#4491,.F.) ;
#5984 = ORIENTED_EDGE('',*,*,#4503,.T.) ;
#5985 = ORIENTED_EDGE('',*,*,#4504,.T.) ;
#5986 = ORIENTED_EDGE('',*,*,#4493,.F.) ;
#5987 = ORIENTED_EDGE('',*,*,#4492,.F.) ;
#5988 = ORIENTED_EDGE('',*,*,#4504,.F.) ;
#5989 = ORIENTED_EDGE('',*,*,#4502,.F.) ;
#5990 = ORIENTED_EDGE('',*,*,#4500,.F.) ;
#5991 = ORIENTED_EDGE('',*,*,#4498,.F.) ;
#5992 = ORIENTED_EDGE('',*,*,#4496,.F.) ;
#5993 = ORIENTED_EDGE('',*,*,#4494,.F.) ;
#5994 = ORIENTED_EDGE('',*,*,#4505,.F.) ;
#5995 = ORIENTED_EDGE('',*,*,#4506,.F.) ;
#5996 = ORIENTED_EDGE('',*,*,#4507,.T.) ;
#5997 = ORIENTED_EDGE('',*,*,#4508,.F.) ;
#5998 = ORIENTED_EDGE('',*,*,#4509,.F.) ;
#5999 = ORIENTED_EDGE('',*,*,#4510,.F.) ;
#6000 = ORIENTED_EDGE('',*,*,#4505,.T.) ;
#6001 = ORIENTED_EDGE('',*,*,#4511,.F.) ;
#6002 = ORIENTED_EDGE('',*,*,#4512,.F.) ;
#6003 = ORIENTED_EDGE('',*,*,#4513,.F.) ;
#6004 = ORIENTED_EDGE('',*,*,#4509,.T.) ;
#6005 = ORIENTED_EDGE('',*,*,#4514,.F.) ;
#6006 = ORIENTED_EDGE('',*,*,#4515,.F.) ;
#6007 = ORIENTED_EDGE('',*,*,#4516,.F.) ;
#6008 = ORIENTED_EDGE('',*,*,#4512,.T.) ;
#6009 = ORIENTED_EDGE('',*,*,#4517,.F.) ;
#6010 = ORIENTED_EDGE('',*,*,#4515,.T.) ;
#6011 = ORIENTED_EDGE('',*,*,#4518,.F.) ;
#6012 = ORIENTED_EDGE('',*,*,#4519,.F.) ;
#6013 = ORIENTED_EDGE('',*,*,#4520,.F.) ;
#6014 = ORIENTED_EDGE('',*,*,#4521,.T.) ;
#6015 = ORIENTED_EDGE('',*,*,#4522,.T.) ;
#6016 = ORIENTED_EDGE('',*,*,#4522,.F.) ;
#6017 = ORIENTED_EDGE('',*,*,#4521,.F.) ;
#6018 = ORIENTED_EDGE('',*,*,#4523,.T.) ;
#6019 = ORIENTED_EDGE('',*,*,#4524,.F.) ;
#6020 = ORIENTED_EDGE('',*,*,#4519,.T.) ;
#6021 = ORIENTED_EDGE('',*,*,#4525,.F.) ;
#6022 = ORIENTED_EDGE('',*,*,#4526,.F.) ;
#6023 = ORIENTED_EDGE('',*,*,#4523,.F.) ;
#6024 = ORIENTED_EDGE('',*,*,#4506,.T.) ;
#6025 = ORIENTED_EDGE('',*,*,#4510,.T.) ;
#6026 = ORIENTED_EDGE('',*,*,#4513,.T.) ;
#6027 = ORIENTED_EDGE('',*,*,#4516,.T.) ;
#6028 = ORIENTED_EDGE('',*,*,#4520,.T.) ;
#6029 = ORIENTED_EDGE('',*,*,#4524,.T.) ;
#6030 = ORIENTED_EDGE('',*,*,#4526,.T.) ;
#6031 = ORIENTED_EDGE('',*,*,#4527,.T.) ;
#6032 = ORIENTED_EDGE('',*,*,#4528,.F.) ;
#6033 = ORIENTED_EDGE('',*,*,#4527,.F.) ;
#6034 = ORIENTED_EDGE('',*,*,#4525,.T.) ;
#6035 = ORIENTED_EDGE('',*,*,#4518,.T.) ;
#6036 = ORIENTED_EDGE('',*,*,#4517,.T.) ;
#6037 = ORIENTED_EDGE('',*,*,#4514,.T.) ;
#6038 = ORIENTED_EDGE('',*,*,#4511,.T.) ;
#6039 = ORIENTED_EDGE('',*,*,#4508,.T.) ;
#6040 = ORIENTED_EDGE('',*,*,#4529,.F.) ;
#6041 = ORIENTED_EDGE('',*,*,#4530,.F.) ;
#6042 = ORIENTED_EDGE('',*,*,#4530,.T.) ;
#6043 = ORIENTED_EDGE('',*,*,#4531,.T.) ;
#6044 = ORIENTED_EDGE('',*,*,#4532,.F.) ;
#6045 = ORIENTED_EDGE('',*,*,#4531,.F.) ;
#6046 = ORIENTED_EDGE('',*,*,#4529,.T.) ;
#6047 = ORIENTED_EDGE('',*,*,#4507,.F.) ;
#6048 = ORIENTED_EDGE('',*,*,#4528,.T.) ;
#6049 = ORIENTED_EDGE('',*,*,#4532,.T.) ;
#6050 = ORIENTED_EDGE('',*,*,#4533,.T.) ;
#6051 = ORIENTED_EDGE('',*,*,#4534,.T.) ;
#6052 = ORIENTED_EDGE('',*,*,#4535,.T.) ;
#6053 = ORIENTED_EDGE('',*,*,#4536,.T.) ;
#6054 = ORIENTED_EDGE('',*,*,#4537,.T.) ;
#6055 = ORIENTED_EDGE('',*,*,#4538,.T.) ;
#6056 = ORIENTED_EDGE('',*,*,#4539,.T.) ;
#6057 = ORIENTED_EDGE('',*,*,#4540,.T.) ;
#6058 = ORIENTED_EDGE('',*,*,#4541,.F.) ;
#6059 = ORIENTED_EDGE('',*,*,#4533,.F.) ;
#6060 = ORIENTED_EDGE('',*,*,#4541,.T.) ;
#6061 = ORIENTED_EDGE('',*,*,#4542,.T.) ;
#6062 = ORIENTED_EDGE('',*,*,#4543,.F.) ;
#6063 = ORIENTED_EDGE('',*,*,#4534,.F.) ;
#6064 = ORIENTED_EDGE('',*,*,#4543,.T.) ;
#6065 = ORIENTED_EDGE('',*,*,#4544,.T.) ;
#6066 = ORIENTED_EDGE('',*,*,#4545,.F.) ;
#6067 = ORIENTED_EDGE('',*,*,#4535,.F.) ;
#6068 = ORIENTED_EDGE('',*,*,#4545,.T.) ;
#6069 = ORIENTED_EDGE('',*,*,#4546,.T.) ;
#6070 = ORIENTED_EDGE('',*,*,#4547,.F.) ;
#6071 = ORIENTED_EDGE('',*,*,#4536,.F.) ;
#6072 = ORIENTED_EDGE('',*,*,#4547,.T.) ;
#6073 = ORIENTED_EDGE('',*,*,#4548,.T.) ;
#6074 = ORIENTED_EDGE('',*,*,#4549,.F.) ;
#6075 = ORIENTED_EDGE('',*,*,#4537,.F.) ;
#6076 = ORIENTED_EDGE('',*,*,#4549,.T.) ;
#6077 = ORIENTED_EDGE('',*,*,#4550,.T.) ;
#6078 = ORIENTED_EDGE('',*,*,#4539,.F.) ;
#6079 = ORIENTED_EDGE('',*,*,#4538,.F.) ;
#6080 = ORIENTED_EDGE('',*,*,#4550,.F.) ;
#6081 = ORIENTED_EDGE('',*,*,#4548,.F.) ;
#6082 = ORIENTED_EDGE('',*,*,#4546,.F.) ;
#6083 = ORIENTED_EDGE('',*,*,#4544,.F.) ;
#6084 = ORIENTED_EDGE('',*,*,#4542,.F.) ;
#6085 = ORIENTED_EDGE('',*,*,#4540,.F.) ;
#6086 = ORIENTED_EDGE('',*,*,#4551,.T.) ;
#6087 = ORIENTED_EDGE('',*,*,#4552,.T.) ;
#6088 = ORIENTED_EDGE('',*,*,#4553,.F.) ;
#6089 = ORIENTED_EDGE('',*,*,#4554,.F.) ;
#6090 = ORIENTED_EDGE('',*,*,#4555,.T.) ;
#6091 = ORIENTED_EDGE('',*,*,#4556,.T.) ;
#6092 = ORIENTED_EDGE('',*,*,#4557,.F.) ;
#6093 = ORIENTED_EDGE('',*,*,#4552,.F.) ;
#6094 = ORIENTED_EDGE('',*,*,#4558,.T.) ;
#6095 = ORIENTED_EDGE('',*,*,#4559,.T.) ;
#6096 = ORIENTED_EDGE('',*,*,#4560,.F.) ;
#6097 = ORIENTED_EDGE('',*,*,#4556,.F.) ;
#6098 = ORIENTED_EDGE('',*,*,#4561,.T.) ;
#6099 = ORIENTED_EDGE('',*,*,#4554,.T.) ;
#6100 = ORIENTED_EDGE('',*,*,#4562,.F.) ;
#6101 = ORIENTED_EDGE('',*,*,#4559,.F.) ;
#6102 = ORIENTED_EDGE('',*,*,#4563,.F.) ;
#6103 = ORIENTED_EDGE('',*,*,#4564,.T.) ;
#6104 = ORIENTED_EDGE('',*,*,#4565,.T.) ;
#6105 = ORIENTED_EDGE('',*,*,#4564,.F.) ;
#6106 = ORIENTED_EDGE('',*,*,#4561,.F.) ;
#6107 = ORIENTED_EDGE('',*,*,#4558,.F.) ;
#6108 = ORIENTED_EDGE('',*,*,#4555,.F.) ;
#6109 = ORIENTED_EDGE('',*,*,#4551,.F.) ;
#6110 = ORIENTED_EDGE('',*,*,#4566,.F.) ;
#6111 = ORIENTED_EDGE('',*,*,#4567,.F.) ;
#6112 = ORIENTED_EDGE('',*,*,#4568,.F.) ;
#6113 = ORIENTED_EDGE('',*,*,#4569,.F.) ;
#6114 = ORIENTED_EDGE('',*,*,#4570,.F.) ;
#6115 = ORIENTED_EDGE('',*,*,#4571,.F.) ;
#6116 = ORIENTED_EDGE('',*,*,#4572,.F.) ;
#6117 = ORIENTED_EDGE('',*,*,#4573,.F.) ;
#6118 = ORIENTED_EDGE('',*,*,#4574,.F.) ;
#6119 = ORIENTED_EDGE('',*,*,#4575,.F.) ;
#6120 = ORIENTED_EDGE('',*,*,#4565,.F.) ;
#6121 = ORIENTED_EDGE('',*,*,#4553,.T.) ;
#6122 = ORIENTED_EDGE('',*,*,#4557,.T.) ;
#6123 = ORIENTED_EDGE('',*,*,#4560,.T.) ;
#6124 = ORIENTED_EDGE('',*,*,#4562,.T.) ;
#6125 = ORIENTED_EDGE('',*,*,#4563,.T.) ;
#6126 = ORIENTED_EDGE('',*,*,#4576,.T.) ;
#6127 = ORIENTED_EDGE('',*,*,#4577,.T.) ;
#6128 = ORIENTED_EDGE('',*,*,#4578,.T.) ;
#6129 = ORIENTED_EDGE('',*,*,#4579,.T.) ;
#6130 = ORIENTED_EDGE('',*,*,#4580,.T.) ;
#6131 = ORIENTED_EDGE('',*,*,#4581,.T.) ;
#6132 = ORIENTED_EDGE('',*,*,#4582,.T.) ;
#6133 = ORIENTED_EDGE('',*,*,#4583,.T.) ;
#6134 = ORIENTED_EDGE('',*,*,#4584,.T.) ;
#6135 = ORIENTED_EDGE('',*,*,#4585,.T.) ;
#6136 = ORIENTED_EDGE('',*,*,#4586,.F.) ;
#6137 = ORIENTED_EDGE('',*,*,#4587,.T.) ;
#6138 = ORIENTED_EDGE('',*,*,#4566,.T.) ;
#6139 = ORIENTED_EDGE('',*,*,#4587,.F.) ;
#6140 = ORIENTED_EDGE('',*,*,#4588,.F.) ;
#6141 = ORIENTED_EDGE('',*,*,#4570,.T.) ;
#6142 = ORIENTED_EDGE('',*,*,#4589,.T.) ;
#6143 = ORIENTED_EDGE('',*,*,#4590,.F.) ;
#6144 = ORIENTED_EDGE('',*,*,#4589,.F.) ;
#6145 = ORIENTED_EDGE('',*,*,#4569,.T.) ;
#6146 = ORIENTED_EDGE('',*,*,#4591,.T.) ;
#6147 = ORIENTED_EDGE('',*,*,#4592,.F.) ;
#6148 = ORIENTED_EDGE('',*,*,#4591,.F.) ;
#6149 = ORIENTED_EDGE('',*,*,#4568,.T.) ;
#6150 = ORIENTED_EDGE('',*,*,#4593,.T.) ;
#6151 = ORIENTED_EDGE('',*,*,#4594,.F.) ;
#6152 = ORIENTED_EDGE('',*,*,#4593,.F.) ;
#6153 = ORIENTED_EDGE('',*,*,#4567,.T.) ;
#6154 = ORIENTED_EDGE('',*,*,#4588,.T.) ;
#6155 = ORIENTED_EDGE('',*,*,#4595,.F.) ;
#6156 = ORIENTED_EDGE('',*,*,#4596,.F.) ;
#6157 = ORIENTED_EDGE('',*,*,#4597,.T.) ;
#6158 = ORIENTED_EDGE('',*,*,#4571,.T.) ;
#6159 = ORIENTED_EDGE('',*,*,#4597,.F.) ;
#6160 = ORIENTED_EDGE('',*,*,#4598,.F.) ;
#6161 = ORIENTED_EDGE('',*,*,#4575,.T.) ;
#6162 = ORIENTED_EDGE('',*,*,#4599,.T.) ;
#6163 = ORIENTED_EDGE('',*,*,#4600,.F.) ;
#6164 = ORIENTED_EDGE('',*,*,#4599,.F.) ;
#6165 = ORIENTED_EDGE('',*,*,#4574,.T.) ;
#6166 = ORIENTED_EDGE('',*,*,#4601,.T.) ;
#6167 = ORIENTED_EDGE('',*,*,#4602,.F.) ;
#6168 = ORIENTED_EDGE('',*,*,#4601,.F.) ;
#6169 = ORIENTED_EDGE('',*,*,#4573,.T.) ;
#6170 = ORIENTED_EDGE('',*,*,#4603,.T.) ;
#6171 = ORIENTED_EDGE('',*,*,#4604,.F.) ;
#6172 = ORIENTED_EDGE('',*,*,#4603,.F.) ;
#6173 = ORIENTED_EDGE('',*,*,#4572,.T.) ;
#6174 = ORIENTED_EDGE('',*,*,#4598,.T.) ;
#6175 = ORIENTED_EDGE('',*,*,#4605,.F.) ;
#6176 = ORIENTED_EDGE('',*,*,#4586,.T.) ;
#6177 = ORIENTED_EDGE('',*,*,#4606,.T.) ;
#6178 = ORIENTED_EDGE('',*,*,#4585,.F.) ;
#6179 = ORIENTED_EDGE('',*,*,#4606,.F.) ;
#6180 = ORIENTED_EDGE('',*,*,#4590,.T.) ;
#6181 = ORIENTED_EDGE('',*,*,#4607,.T.) ;
#6182 = ORIENTED_EDGE('',*,*,#4577,.F.) ;
#6183 = ORIENTED_EDGE('',*,*,#4608,.T.) ;
#6184 = ORIENTED_EDGE('',*,*,#4592,.T.) ;
#6185 = ORIENTED_EDGE('',*,*,#4609,.F.) ;
#6186 = ORIENTED_EDGE('',*,*,#4578,.F.) ;
#6187 = ORIENTED_EDGE('',*,*,#4607,.F.) ;
#6188 = ORIENTED_EDGE('',*,*,#4594,.T.) ;
#6189 = ORIENTED_EDGE('',*,*,#4610,.T.) ;
#6190 = ORIENTED_EDGE('',*,*,#4579,.F.) ;
#6191 = ORIENTED_EDGE('',*,*,#4609,.T.) ;
#6192 = ORIENTED_EDGE('',*,*,#4595,.T.) ;
#6193 = ORIENTED_EDGE('',*,*,#4608,.F.) ;
#6194 = ORIENTED_EDGE('',*,*,#4580,.F.) ;
#6195 = ORIENTED_EDGE('',*,*,#4610,.F.) ;
#6196 = ORIENTED_EDGE('',*,*,#4596,.T.) ;
#6197 = ORIENTED_EDGE('',*,*,#4611,.T.) ;
#6198 = ORIENTED_EDGE('',*,*,#4576,.F.) ;
#6199 = ORIENTED_EDGE('',*,*,#4611,.F.) ;
#6200 = ORIENTED_EDGE('',*,*,#4600,.T.) ;
#6201 = ORIENTED_EDGE('',*,*,#4612,.T.) ;
#6202 = ORIENTED_EDGE('',*,*,#4581,.F.) ;
#6203 = ORIENTED_EDGE('',*,*,#4613,.T.) ;
#6204 = ORIENTED_EDGE('',*,*,#4602,.T.) ;
#6205 = ORIENTED_EDGE('',*,*,#4614,.T.) ;
#6206 = ORIENTED_EDGE('',*,*,#4582,.F.) ;
#6207 = ORIENTED_EDGE('',*,*,#4612,.F.) ;
#6208 = ORIENTED_EDGE('',*,*,#4604,.T.) ;
#6209 = ORIENTED_EDGE('',*,*,#4615,.F.) ;
#6210 = ORIENTED_EDGE('',*,*,#4583,.F.) ;
#6211 = ORIENTED_EDGE('',*,*,#4614,.F.) ;
#6212 = ORIENTED_EDGE('',*,*,#4605,.T.) ;
#6213 = ORIENTED_EDGE('',*,*,#4613,.F.) ;
#6214 = ORIENTED_EDGE('',*,*,#4584,.F.) ;
#6215 = ORIENTED_EDGE('',*,*,#4615,.T.) ;
#6216 = ORIENTED_EDGE('',*,*,#4616,.T.) ;
#6217 = ORIENTED_EDGE('',*,*,#4617,.T.) ;
#6218 = ORIENTED_EDGE('',*,*,#4618,.F.) ;
#6219 = ORIENTED_EDGE('',*,*,#4619,.F.) ;
#6220 = ORIENTED_EDGE('',*,*,#4620,.T.) ;
#6221 = ORIENTED_EDGE('',*,*,#4621,.T.) ;
#6222 = ORIENTED_EDGE('',*,*,#4622,.F.) ;
#6223 = ORIENTED_EDGE('',*,*,#4617,.F.) ;
#6224 = ORIENTED_EDGE('',*,*,#4623,.T.) ;
#6225 = ORIENTED_EDGE('',*,*,#4624,.T.) ;
#6226 = ORIENTED_EDGE('',*,*,#4625,.F.) ;
#6227 = ORIENTED_EDGE('',*,*,#4621,.F.) ;
#6228 = ORIENTED_EDGE('',*,*,#4626,.T.) ;
#6229 = ORIENTED_EDGE('',*,*,#4619,.T.) ;
#6230 = ORIENTED_EDGE('',*,*,#4627,.F.) ;
#6231 = ORIENTED_EDGE('',*,*,#4624,.F.) ;
#6232 = ORIENTED_EDGE('',*,*,#4626,.F.) ;
#6233 = ORIENTED_EDGE('',*,*,#4623,.F.) ;
#6234 = ORIENTED_EDGE('',*,*,#4620,.F.) ;
#6235 = ORIENTED_EDGE('',*,*,#4616,.F.) ;
#6236 = ORIENTED_EDGE('',*,*,#4628,.F.) ;
#6237 = ORIENTED_EDGE('',*,*,#4629,.F.) ;
#6238 = ORIENTED_EDGE('',*,*,#4630,.F.) ;
#6239 = ORIENTED_EDGE('',*,*,#4631,.F.) ;
#6240 = ORIENTED_EDGE('',*,*,#4632,.F.) ;
#6241 = ORIENTED_EDGE('',*,*,#4633,.F.) ;
#6242 = ORIENTED_EDGE('',*,*,#4634,.F.) ;
#6243 = ORIENTED_EDGE('',*,*,#4635,.F.) ;
#6244 = ORIENTED_EDGE('',*,*,#4636,.F.) ;
#6245 = ORIENTED_EDGE('',*,*,#4637,.F.) ;
#6246 = ORIENTED_EDGE('',*,*,#4638,.F.) ;
#6247 = ORIENTED_EDGE('',*,*,#4618,.T.) ;
#6248 = ORIENTED_EDGE('',*,*,#4622,.T.) ;
#6249 = ORIENTED_EDGE('',*,*,#4625,.T.) ;
#6250 = ORIENTED_EDGE('',*,*,#4627,.T.) ;
#6251 = ORIENTED_EDGE('',*,*,#4639,.T.) ;
#6252 = ORIENTED_EDGE('',*,*,#4640,.T.) ;
#6253 = ORIENTED_EDGE('',*,*,#4641,.T.) ;
#6254 = ORIENTED_EDGE('',*,*,#4642,.T.) ;
#6255 = ORIENTED_EDGE('',*,*,#4643,.T.) ;
#6256 = ORIENTED_EDGE('',*,*,#4644,.T.) ;
#6257 = ORIENTED_EDGE('',*,*,#4645,.T.) ;
#6258 = ORIENTED_EDGE('',*,*,#4646,.T.) ;
#6259 = ORIENTED_EDGE('',*,*,#4647,.T.) ;
#6260 = ORIENTED_EDGE('',*,*,#4648,.T.) ;
#6261 = ORIENTED_EDGE('',*,*,#4649,.T.) ;
#6262 = ORIENTED_EDGE('',*,*,#4650,.F.) ;
#6263 = ORIENTED_EDGE('',*,*,#4651,.T.) ;
#6264 = ORIENTED_EDGE('',*,*,#4628,.T.) ;
#6265 = ORIENTED_EDGE('',*,*,#4651,.F.) ;
#6266 = ORIENTED_EDGE('',*,*,#4652,.F.) ;
#6267 = ORIENTED_EDGE('',*,*,#4632,.T.) ;
#6268 = ORIENTED_EDGE('',*,*,#4653,.T.) ;
#6269 = ORIENTED_EDGE('',*,*,#4654,.F.) ;
#6270 = ORIENTED_EDGE('',*,*,#4653,.F.) ;
#6271 = ORIENTED_EDGE('',*,*,#4631,.T.) ;
#6272 = ORIENTED_EDGE('',*,*,#4655,.T.) ;
#6273 = ORIENTED_EDGE('',*,*,#4656,.F.) ;
#6274 = ORIENTED_EDGE('',*,*,#4655,.F.) ;
#6275 = ORIENTED_EDGE('',*,*,#4630,.T.) ;
#6276 = ORIENTED_EDGE('',*,*,#4657,.T.) ;
#6277 = ORIENTED_EDGE('',*,*,#4658,.F.) ;
#6278 = ORIENTED_EDGE('',*,*,#4657,.F.) ;
#6279 = ORIENTED_EDGE('',*,*,#4629,.T.) ;
#6280 = ORIENTED_EDGE('',*,*,#4652,.T.) ;
#6281 = ORIENTED_EDGE('',*,*,#4659,.F.) ;
#6282 = ORIENTED_EDGE('',*,*,#4660,.F.) ;
#6283 = ORIENTED_EDGE('',*,*,#4661,.T.) ;
#6284 = ORIENTED_EDGE('',*,*,#4633,.T.) ;
#6285 = ORIENTED_EDGE('',*,*,#4661,.F.) ;
#6286 = ORIENTED_EDGE('',*,*,#4662,.F.) ;
#6287 = ORIENTED_EDGE('',*,*,#4637,.T.) ;
#6288 = ORIENTED_EDGE('',*,*,#4663,.T.) ;
#6289 = ORIENTED_EDGE('',*,*,#4664,.F.) ;
#6290 = ORIENTED_EDGE('',*,*,#4663,.F.) ;
#6291 = ORIENTED_EDGE('',*,*,#4636,.T.) ;
#6292 = ORIENTED_EDGE('',*,*,#4665,.T.) ;
#6293 = ORIENTED_EDGE('',*,*,#4666,.F.) ;
#6294 = ORIENTED_EDGE('',*,*,#4665,.F.) ;
#6295 = ORIENTED_EDGE('',*,*,#4635,.T.) ;
#6296 = ORIENTED_EDGE('',*,*,#4667,.T.) ;
#6297 = ORIENTED_EDGE('',*,*,#4668,.F.) ;
#6298 = ORIENTED_EDGE('',*,*,#4667,.F.) ;
#6299 = ORIENTED_EDGE('',*,*,#4634,.T.) ;
#6300 = ORIENTED_EDGE('',*,*,#4662,.T.) ;
#6301 = ORIENTED_EDGE('',*,*,#4669,.F.) ;
#6302 = ORIENTED_EDGE('',*,*,#4670,.F.) ;
#6303 = ORIENTED_EDGE('',*,*,#4671,.T.) ;
#6304 = ORIENTED_EDGE('',*,*,#4638,.T.) ;
#6305 = ORIENTED_EDGE('',*,*,#4671,.F.) ;
#6306 = ORIENTED_EDGE('',*,*,#4650,.T.) ;
#6307 = ORIENTED_EDGE('',*,*,#4672,.T.) ;
#6308 = ORIENTED_EDGE('',*,*,#4649,.F.) ;
#6309 = ORIENTED_EDGE('',*,*,#4672,.F.) ;
#6310 = ORIENTED_EDGE('',*,*,#4654,.T.) ;
#6311 = ORIENTED_EDGE('',*,*,#4673,.T.) ;
#6312 = ORIENTED_EDGE('',*,*,#4640,.F.) ;
#6313 = ORIENTED_EDGE('',*,*,#4674,.T.) ;
#6314 = ORIENTED_EDGE('',*,*,#4656,.T.) ;
#6315 = ORIENTED_EDGE('',*,*,#4675,.T.) ;
#6316 = ORIENTED_EDGE('',*,*,#4641,.F.) ;
#6317 = ORIENTED_EDGE('',*,*,#4673,.F.) ;
#6318 = ORIENTED_EDGE('',*,*,#4658,.T.) ;
#6319 = ORIENTED_EDGE('',*,*,#4676,.T.) ;
#6320 = ORIENTED_EDGE('',*,*,#4642,.F.) ;
#6321 = ORIENTED_EDGE('',*,*,#4675,.F.) ;
#6322 = ORIENTED_EDGE('',*,*,#4659,.T.) ;
#6323 = ORIENTED_EDGE('',*,*,#4674,.F.) ;
#6324 = ORIENTED_EDGE('',*,*,#4643,.F.) ;
#6325 = ORIENTED_EDGE('',*,*,#4676,.F.) ;
#6326 = ORIENTED_EDGE('',*,*,#4660,.T.) ;
#6327 = ORIENTED_EDGE('',*,*,#4677,.T.) ;
#6328 = ORIENTED_EDGE('',*,*,#4639,.F.) ;
#6329 = ORIENTED_EDGE('',*,*,#4677,.F.) ;
#6330 = ORIENTED_EDGE('',*,*,#4664,.T.) ;
#6331 = ORIENTED_EDGE('',*,*,#4678,.T.) ;
#6332 = ORIENTED_EDGE('',*,*,#4645,.F.) ;
#6333 = ORIENTED_EDGE('',*,*,#4679,.F.) ;
#6334 = ORIENTED_EDGE('',*,*,#4666,.T.) ;
#6335 = ORIENTED_EDGE('',*,*,#4680,.T.) ;
#6336 = ORIENTED_EDGE('',*,*,#4646,.F.) ;
#6337 = ORIENTED_EDGE('',*,*,#4678,.F.) ;
#6338 = ORIENTED_EDGE('',*,*,#4668,.T.) ;
#6339 = ORIENTED_EDGE('',*,*,#4681,.T.) ;
#6340 = ORIENTED_EDGE('',*,*,#4647,.F.) ;
#6341 = ORIENTED_EDGE('',*,*,#4680,.F.) ;
#6342 = ORIENTED_EDGE('',*,*,#4669,.T.) ;
#6343 = ORIENTED_EDGE('',*,*,#4679,.T.) ;
#6344 = ORIENTED_EDGE('',*,*,#4648,.F.) ;
#6345 = ORIENTED_EDGE('',*,*,#4681,.F.) ;
#6346 = ORIENTED_EDGE('',*,*,#4670,.T.) ;
#6347 = ORIENTED_EDGE('',*,*,#4682,.T.) ;
#6348 = ORIENTED_EDGE('',*,*,#4644,.F.) ;
#6349 = ORIENTED_EDGE('',*,*,#4682,.F.) ;
#6350 = ORIENTED_EDGE('',*,*,#4683,.T.) ;
#6351 = ORIENTED_EDGE('',*,*,#4684,.T.) ;
#6352 = ORIENTED_EDGE('',*,*,#4685,.F.) ;
#6353 = ORIENTED_EDGE('',*,*,#4684,.F.) ;
#6354 = ORIENTED_EDGE('',*,*,#4686,.F.) ;
#6355 = ORIENTED_EDGE('',*,*,#4687,.T.) ;
#6356 = ORIENTED_EDGE('',*,*,#4688,.T.) ;
#6357 = ORIENTED_EDGE('',*,*,#4686,.T.) ;
#6358 = ORIENTED_EDGE('',*,*,#4688,.F.) ;
#6359 = ORIENTED_EDGE('',*,*,#4683,.F.) ;
#6360 = ORIENTED_EDGE('',*,*,#4685,.T.) ;
#6361 = ORIENTED_EDGE('',*,*,#4689,.T.) ;
#6362 = ORIENTED_EDGE('',*,*,#4687,.F.) ;
#6363 = ORIENTED_EDGE('',*,*,#4689,.F.) ;
#6364 = ORIENTED_EDGE('',*,*,#4690,.T.) ;
#6365 = ORIENTED_EDGE('',*,*,#4691,.T.) ;
#6366 = ORIENTED_EDGE('',*,*,#4692,.F.) ;
#6367 = ORIENTED_EDGE('',*,*,#4693,.F.) ;
#6368 = ORIENTED_EDGE('',*,*,#4694,.T.) ;
#6369 = ORIENTED_EDGE('',*,*,#4695,.T.) ;
#6370 = ORIENTED_EDGE('',*,*,#4696,.F.) ;
#6371 = ORIENTED_EDGE('',*,*,#4691,.F.) ;
#6372 = ORIENTED_EDGE('',*,*,#4697,.T.) ;
#6373 = ORIENTED_EDGE('',*,*,#4698,.T.) ;
#6374 = ORIENTED_EDGE('',*,*,#4699,.F.) ;
#6375 = ORIENTED_EDGE('',*,*,#4695,.F.) ;
#6376 = ORIENTED_EDGE('',*,*,#4700,.T.) ;
#6377 = ORIENTED_EDGE('',*,*,#4701,.T.) ;
#6378 = ORIENTED_EDGE('',*,*,#4702,.F.) ;
#6379 = ORIENTED_EDGE('',*,*,#4698,.F.) ;
#6380 = ORIENTED_EDGE('',*,*,#4703,.T.) ;
#6381 = ORIENTED_EDGE('',*,*,#4704,.T.) ;
#6382 = ORIENTED_EDGE('',*,*,#4705,.F.) ;
#6383 = ORIENTED_EDGE('',*,*,#4701,.F.) ;
#6384 = ORIENTED_EDGE('',*,*,#4706,.T.) ;
#6385 = ORIENTED_EDGE('',*,*,#4707,.T.) ;
#6386 = ORIENTED_EDGE('',*,*,#4708,.F.) ;
#6387 = ORIENTED_EDGE('',*,*,#4704,.F.) ;
#6388 = ORIENTED_EDGE('',*,*,#4709,.T.) ;
#6389 = ORIENTED_EDGE('',*,*,#4710,.T.) ;
#6390 = ORIENTED_EDGE('',*,*,#4711,.F.) ;
#6391 = ORIENTED_EDGE('',*,*,#4707,.F.) ;
#6392 = ORIENTED_EDGE('',*,*,#4712,.T.) ;
#6393 = ORIENTED_EDGE('',*,*,#4713,.T.) ;
#6394 = ORIENTED_EDGE('',*,*,#4714,.F.) ;
#6395 = ORIENTED_EDGE('',*,*,#4710,.F.) ;
#6396 = ORIENTED_EDGE('',*,*,#4715,.T.) ;
#6397 = ORIENTED_EDGE('',*,*,#4716,.T.) ;
#6398 = ORIENTED_EDGE('',*,*,#4717,.F.) ;
#6399 = ORIENTED_EDGE('',*,*,#4713,.F.) ;
#6400 = ORIENTED_EDGE('',*,*,#4718,.T.) ;
#6401 = ORIENTED_EDGE('',*,*,#4719,.T.) ;
#6402 = ORIENTED_EDGE('',*,*,#4720,.F.) ;
#6403 = ORIENTED_EDGE('',*,*,#4716,.F.) ;
#6404 = ORIENTED_EDGE('',*,*,#4721,.T.) ;
#6405 = ORIENTED_EDGE('',*,*,#4722,.T.) ;
#6406 = ORIENTED_EDGE('',*,*,#4723,.F.) ;
#6407 = ORIENTED_EDGE('',*,*,#4719,.F.) ;
#6408 = ORIENTED_EDGE('',*,*,#4724,.T.) ;
#6409 = ORIENTED_EDGE('',*,*,#4693,.T.) ;
#6410 = ORIENTED_EDGE('',*,*,#4725,.F.) ;
#6411 = ORIENTED_EDGE('',*,*,#4722,.F.) ;
#6412 = ORIENTED_EDGE('',*,*,#4724,.F.) ;
#6413 = ORIENTED_EDGE('',*,*,#4721,.F.) ;
#6414 = ORIENTED_EDGE('',*,*,#4718,.F.) ;
#6415 = ORIENTED_EDGE('',*,*,#4715,.F.) ;
#6416 = ORIENTED_EDGE('',*,*,#4712,.F.) ;
#6417 = ORIENTED_EDGE('',*,*,#4709,.F.) ;
#6418 = ORIENTED_EDGE('',*,*,#4706,.F.) ;
#6419 = ORIENTED_EDGE('',*,*,#4703,.F.) ;
#6420 = ORIENTED_EDGE('',*,*,#4700,.F.) ;
#6421 = ORIENTED_EDGE('',*,*,#4697,.F.) ;
#6422 = ORIENTED_EDGE('',*,*,#4694,.F.) ;
#6423 = ORIENTED_EDGE('',*,*,#4690,.F.) ;
#6424 = ORIENTED_EDGE('',*,*,#4726,.F.) ;
#6425 = ORIENTED_EDGE('',*,*,#4727,.F.) ;
#6426 = ORIENTED_EDGE('',*,*,#4692,.T.) ;
#6427 = ORIENTED_EDGE('',*,*,#4696,.T.) ;
#6428 = ORIENTED_EDGE('',*,*,#4699,.T.) ;
#6429 = ORIENTED_EDGE('',*,*,#4702,.T.) ;
#6430 = ORIENTED_EDGE('',*,*,#4705,.T.) ;
#6431 = ORIENTED_EDGE('',*,*,#4708,.T.) ;
#6432 = ORIENTED_EDGE('',*,*,#4711,.T.) ;
#6433 = ORIENTED_EDGE('',*,*,#4714,.T.) ;
#6434 = ORIENTED_EDGE('',*,*,#4717,.T.) ;
#6435 = ORIENTED_EDGE('',*,*,#4720,.T.) ;
#6436 = ORIENTED_EDGE('',*,*,#4723,.T.) ;
#6437 = ORIENTED_EDGE('',*,*,#4725,.T.) ;
#6438 = ORIENTED_EDGE('',*,*,#4728,.T.) ;
#6439 = ORIENTED_EDGE('',*,*,#4729,.T.) ;
#6440 = ORIENTED_EDGE('',*,*,#4728,.F.) ;
#6441 = ORIENTED_EDGE('',*,*,#4730,.T.) ;
#6442 = ORIENTED_EDGE('',*,*,#4726,.T.) ;
#6443 = ORIENTED_EDGE('',*,*,#4730,.F.) ;
#6444 = ORIENTED_EDGE('',*,*,#4727,.T.) ;
#6445 = ORIENTED_EDGE('',*,*,#4731,.T.) ;
#6446 = ORIENTED_EDGE('',*,*,#4729,.F.) ;
#6447 = ORIENTED_EDGE('',*,*,#4731,.F.) ;
#6448 = ORIENTED_EDGE('',*,*,#4732,.T.) ;
#6449 = ORIENTED_EDGE('',*,*,#4732,.F.) ;
#6450 = ORIENTED_EDGE('',*,*,#4733,.F.) ;
#6451 = ORIENTED_EDGE('',*,*,#4734,.T.) ;
#6452 = ORIENTED_EDGE('',*,*,#4735,.F.) ;
#6453 = ORIENTED_EDGE('',*,*,#4735,.T.) ;
#6454 = ORIENTED_EDGE('',*,*,#4736,.T.) ;
#6455 = ORIENTED_EDGE('',*,*,#4737,.F.) ;
#6456 = ORIENTED_EDGE('',*,*,#4734,.F.) ;
#6457 = ORIENTED_EDGE('',*,*,#4737,.T.) ;
#6458 = ORIENTED_EDGE('',*,*,#4738,.T.) ;
#6459 = ORIENTED_EDGE('',*,*,#4739,.F.) ;
#6460 = ORIENTED_EDGE('',*,*,#4736,.F.) ;
#6461 = ORIENTED_EDGE('',*,*,#4739,.T.) ;
#6462 = ORIENTED_EDGE('',*,*,#4740,.T.) ;
#6463 = ORIENTED_EDGE('',*,*,#4741,.F.) ;
#6464 = ORIENTED_EDGE('',*,*,#4738,.F.) ;
#6465 = ORIENTED_EDGE('',*,*,#4741,.T.) ;
#6466 = ORIENTED_EDGE('',*,*,#4733,.T.) ;
#6467 = ORIENTED_EDGE('',*,*,#4742,.F.) ;
#6468 = ORIENTED_EDGE('',*,*,#4740,.F.) ;
#6469 = ORIENTED_EDGE('',*,*,#4742,.T.) ;
#6470 = ORIENTED_EDGE('',*,*,#4743,.T.) ;
#6471 = ORIENTED_EDGE('',*,*,#4744,.T.) ;
#6472 = ORIENTED_EDGE('',*,*,#4744,.F.) ;
#6473 = ORIENTED_EDGE('',*,*,#4745,.F.) ;
#6474 = ORIENTED_EDGE('',*,*,#4745,.T.) ;
#6475 = ORIENTED_EDGE('',*,*,#4746,.F.) ;
#6476 = ORIENTED_EDGE('',*,*,#4747,.F.) ;
#6477 = ORIENTED_EDGE('',*,*,#4746,.T.) ;
#6478 = ORIENTED_EDGE('',*,*,#4747,.T.) ;
#6479 = ORIENTED_EDGE('',*,*,#4748,.F.) ;
#6480 = ORIENTED_EDGE('',*,*,#4749,.F.) ;
#6481 = ORIENTED_EDGE('',*,*,#4748,.T.) ;
#6482 = ORIENTED_EDGE('',*,*,#4749,.T.) ;
#6483 = ORIENTED_EDGE('',*,*,#4750,.F.) ;
#6484 = ORIENTED_EDGE('',*,*,#4751,.F.) ;
#6485 = ORIENTED_EDGE('',*,*,#4750,.T.) ;
#6486 = ORIENTED_EDGE('',*,*,#4751,.T.) ;
#6487 = ORIENTED_EDGE('',*,*,#4752,.F.) ;
#6488 = ORIENTED_EDGE('',*,*,#4753,.F.) ;
#6489 = ORIENTED_EDGE('',*,*,#4752,.T.) ;
#6490 = ORIENTED_EDGE('',*,*,#4753,.T.) ;
#6491 = ORIENTED_EDGE('',*,*,#4743,.F.) ;
#6492 = ORIENTED_EDGE('',*,*,#4754,.F.) ;
#6493 = ORIENTED_EDGE('',*,*,#4755,.F.) ;
#6494 = ORIENTED_EDGE('',*,*,#4756,.F.) ;
#6495 = ORIENTED_EDGE('',*,*,#4757,.F.) ;
#6496 = ORIENTED_EDGE('',*,*,#4758,.F.) ;
#6497 = ORIENTED_EDGE('',*,*,#4755,.T.) ;
#6498 = ORIENTED_EDGE('',*,*,#4759,.F.) ;
#6499 = ORIENTED_EDGE('',*,*,#4760,.T.) ;
#6500 = ORIENTED_EDGE('',*,*,#4761,.F.) ;
#6501 = ORIENTED_EDGE('',*,*,#4762,.T.) ;
#6502 = ORIENTED_EDGE('',*,*,#4763,.T.) ;
#6503 = ORIENTED_EDGE('',*,*,#4762,.F.) ;
#6504 = ORIENTED_EDGE('',*,*,#4758,.T.) ;
#6505 = ORIENTED_EDGE('',*,*,#4757,.T.) ;
#6506 = ORIENTED_EDGE('',*,*,#4756,.T.) ;
#6507 = ORIENTED_EDGE('',*,*,#4764,.T.) ;
#6508 = ORIENTED_EDGE('',*,*,#4765,.T.) ;
#6509 = ORIENTED_EDGE('',*,*,#4766,.T.) ;
#6510 = ORIENTED_EDGE('',*,*,#4767,.T.) ;
#6511 = ORIENTED_EDGE('',*,*,#4764,.F.) ;
#6512 = ORIENTED_EDGE('',*,*,#4763,.F.) ;
#6513 = ORIENTED_EDGE('',*,*,#4768,.T.) ;
#6514 = ORIENTED_EDGE('',*,*,#4754,.T.) ;
#6515 = ORIENTED_EDGE('',*,*,#4768,.F.) ;
#6516 = ORIENTED_EDGE('',*,*,#4767,.F.) ;
#6517 = ORIENTED_EDGE('',*,*,#4766,.F.) ;
#6518 = ORIENTED_EDGE('',*,*,#4765,.F.) ;
#6519 = ORIENTED_EDGE('',*,*,#4769,.F.) ;
#6520 = ORIENTED_EDGE('',*,*,#4770,.F.) ;
#6521 = ORIENTED_EDGE('',*,*,#4771,.F.) ;
#6522 = ORIENTED_EDGE('',*,*,#4772,.F.) ;
#6523 = ORIENTED_EDGE('',*,*,#4773,.F.) ;
#6524 = ORIENTED_EDGE('',*,*,#4770,.T.) ;
#6525 = ORIENTED_EDGE('',*,*,#4774,.F.) ;
#6526 = ORIENTED_EDGE('',*,*,#4775,.F.) ;
#6527 = ORIENTED_EDGE('',*,*,#4776,.F.) ;
#6528 = ORIENTED_EDGE('',*,*,#4777,.T.) ;
#6529 = ORIENTED_EDGE('',*,*,#4778,.T.) ;
#6530 = ORIENTED_EDGE('',*,*,#4777,.F.) ;
#6531 = ORIENTED_EDGE('',*,*,#4773,.T.) ;
#6532 = ORIENTED_EDGE('',*,*,#4772,.T.) ;
#6533 = ORIENTED_EDGE('',*,*,#4771,.T.) ;
#6534 = ORIENTED_EDGE('',*,*,#4779,.T.) ;
#6535 = ORIENTED_EDGE('',*,*,#4780,.T.) ;
#6536 = ORIENTED_EDGE('',*,*,#4781,.T.) ;
#6537 = ORIENTED_EDGE('',*,*,#4782,.T.) ;
#6538 = ORIENTED_EDGE('',*,*,#4779,.F.) ;
#6539 = ORIENTED_EDGE('',*,*,#4778,.F.) ;
#6540 = ORIENTED_EDGE('',*,*,#4783,.T.) ;
#6541 = ORIENTED_EDGE('',*,*,#4769,.T.) ;
#6542 = ORIENTED_EDGE('',*,*,#4783,.F.) ;
#6543 = ORIENTED_EDGE('',*,*,#4782,.F.) ;
#6544 = ORIENTED_EDGE('',*,*,#4781,.F.) ;
#6545 = ORIENTED_EDGE('',*,*,#4780,.F.) ;
#6546 = ORIENTED_EDGE('',*,*,#4774,.T.) ;
#6547 = ORIENTED_EDGE('',*,*,#4776,.T.) ;
#6548 = ORIENTED_EDGE('',*,*,#4760,.F.) ;
#6549 = ORIENTED_EDGE('',*,*,#4775,.T.) ;
#6550 = ORIENTED_EDGE('',*,*,#4759,.T.) ;
#6551 = ORIENTED_EDGE('',*,*,#4761,.T.) ;
#6552 = ORIENTED_EDGE('',*,*,#4784,.T.) ;
#6553 = ORIENTED_EDGE('',*,*,#4785,.T.) ;
#6554 = ORIENTED_EDGE('',*,*,#4785,.F.) ;
#6555 = ORIENTED_EDGE('',*,*,#4786,.F.) ;
#6556 = ORIENTED_EDGE('',*,*,#4786,.T.) ;
#6557 = ORIENTED_EDGE('',*,*,#4787,.F.) ;
#6558 = ORIENTED_EDGE('',*,*,#4788,.F.) ;
#6559 = ORIENTED_EDGE('',*,*,#4787,.T.) ;
#6560 = ORIENTED_EDGE('',*,*,#4788,.T.) ;
#6561 = ORIENTED_EDGE('',*,*,#4789,.F.) ;
#6562 = ORIENTED_EDGE('',*,*,#4790,.F.) ;
#6563 = ORIENTED_EDGE('',*,*,#4789,.T.) ;
#6564 = ORIENTED_EDGE('',*,*,#4790,.T.) ;
#6565 = ORIENTED_EDGE('',*,*,#4791,.F.) ;
#6566 = ORIENTED_EDGE('',*,*,#4792,.F.) ;
#6567 = ORIENTED_EDGE('',*,*,#4791,.T.) ;
#6568 = ORIENTED_EDGE('',*,*,#4792,.T.) ;
#6569 = ORIENTED_EDGE('',*,*,#4793,.F.) ;
#6570 = ORIENTED_EDGE('',*,*,#4794,.F.) ;
#6571 = ORIENTED_EDGE('',*,*,#4793,.T.) ;
#6572 = ORIENTED_EDGE('',*,*,#4794,.T.) ;
#6573 = ORIENTED_EDGE('',*,*,#4784,.F.) ;
#6574 = ORIENTED_EDGE('',*,*,#4795,.T.) ;
#6575 = ORIENTED_EDGE('',*,*,#4795,.F.) ;
#6576 = ORIENTED_EDGE('',*,*,#4796,.F.) ;
#6577 = ORIENTED_EDGE('',*,*,#4797,.T.) ;
#6578 = ORIENTED_EDGE('',*,*,#4798,.F.) ;
#6579 = ORIENTED_EDGE('',*,*,#4798,.T.) ;
#6580 = ORIENTED_EDGE('',*,*,#4799,.T.) ;
#6581 = ORIENTED_EDGE('',*,*,#4800,.F.) ;
#6582 = ORIENTED_EDGE('',*,*,#4797,.F.) ;
#6583 = ORIENTED_EDGE('',*,*,#4800,.T.) ;
#6584 = ORIENTED_EDGE('',*,*,#4801,.T.) ;
#6585 = ORIENTED_EDGE('',*,*,#4802,.F.) ;
#6586 = ORIENTED_EDGE('',*,*,#4799,.F.) ;
#6587 = ORIENTED_EDGE('',*,*,#4802,.T.) ;
#6588 = ORIENTED_EDGE('',*,*,#4803,.T.) ;
#6589 = ORIENTED_EDGE('',*,*,#4804,.F.) ;
#6590 = ORIENTED_EDGE('',*,*,#4801,.F.) ;
#6591 = ORIENTED_EDGE('',*,*,#4804,.T.) ;
#6592 = ORIENTED_EDGE('',*,*,#4796,.T.) ;
#6593 = ORIENTED_EDGE('',*,*,#4805,.F.) ;
#6594 = ORIENTED_EDGE('',*,*,#4803,.F.) ;
#6595 = ORIENTED_EDGE('',*,*,#4805,.T.) ;
#6596 = ORIENTED_EDGE('',*,*,#4806,.T.) ;
#6597 = ORIENTED_EDGE('',*,*,#4807,.T.) ;
#6598 = ORIENTED_EDGE('',*,*,#4808,.F.) ;
#6599 = ORIENTED_EDGE('',*,*,#4809,.T.) ;
#6600 = ORIENTED_EDGE('',*,*,#4810,.F.) ;
#6601 = ORIENTED_EDGE('',*,*,#4811,.T.) ;
#6602 = ORIENTED_EDGE('',*,*,#4812,.T.) ;
#6603 = ORIENTED_EDGE('',*,*,#4813,.T.) ;
#6604 = ORIENTED_EDGE('',*,*,#4810,.T.) ;
#6605 = ORIENTED_EDGE('',*,*,#4811,.F.) ;
#6606 = ORIENTED_EDGE('',*,*,#4814,.T.) ;
#6607 = ORIENTED_EDGE('',*,*,#4815,.F.) ;
#6608 = ORIENTED_EDGE('',*,*,#4814,.F.) ;
#6609 = ORIENTED_EDGE('',*,*,#4813,.F.) ;
#6610 = ORIENTED_EDGE('',*,*,#4812,.F.) ;
#6611 = ORIENTED_EDGE('',*,*,#4815,.T.) ;
#6612 = ORIENTED_EDGE('',*,*,#4816,.T.) ;
#6613 = ORIENTED_EDGE('',*,*,#4817,.F.) ;
#6614 = ORIENTED_EDGE('',*,*,#4818,.F.) ;
#6615 = ORIENTED_EDGE('',*,*,#4819,.F.) ;
#6616 = ORIENTED_EDGE('',*,*,#4816,.F.) ;
#6617 = ORIENTED_EDGE('',*,*,#4819,.T.) ;
#6618 = ORIENTED_EDGE('',*,*,#4818,.T.) ;
#6619 = ORIENTED_EDGE('',*,*,#4817,.T.) ;
#6620 = ORIENTED_EDGE('',*,*,#4820,.T.) ;
#6621 = ORIENTED_EDGE('',*,*,#4806,.F.) ;
#6622 = ORIENTED_EDGE('',*,*,#4820,.F.) ;
#6623 = ORIENTED_EDGE('',*,*,#4821,.T.) ;
#6624 = ORIENTED_EDGE('',*,*,#4822,.T.) ;
#6625 = ORIENTED_EDGE('',*,*,#4823,.T.) ;
#6626 = ORIENTED_EDGE('',*,*,#4824,.T.) ;
#6627 = ORIENTED_EDGE('',*,*,#4825,.F.) ;
#6628 = ORIENTED_EDGE('',*,*,#4826,.T.) ;
#6629 = ORIENTED_EDGE('',*,*,#4827,.T.) ;
#6630 = ORIENTED_EDGE('',*,*,#4828,.T.) ;
#6631 = ORIENTED_EDGE('',*,*,#4825,.T.) ;
#6632 = ORIENTED_EDGE('',*,*,#4826,.F.) ;
#6633 = ORIENTED_EDGE('',*,*,#4829,.T.) ;
#6634 = ORIENTED_EDGE('',*,*,#4830,.F.) ;
#6635 = ORIENTED_EDGE('',*,*,#4829,.F.) ;
#6636 = ORIENTED_EDGE('',*,*,#4828,.F.) ;
#6637 = ORIENTED_EDGE('',*,*,#4827,.F.) ;
#6638 = ORIENTED_EDGE('',*,*,#4830,.T.) ;
#6639 = ORIENTED_EDGE('',*,*,#4831,.T.) ;
#6640 = ORIENTED_EDGE('',*,*,#4832,.F.) ;
#6641 = ORIENTED_EDGE('',*,*,#4833,.F.) ;
#6642 = ORIENTED_EDGE('',*,*,#4834,.F.) ;
#6643 = ORIENTED_EDGE('',*,*,#4831,.F.) ;
#6644 = ORIENTED_EDGE('',*,*,#4834,.T.) ;
#6645 = ORIENTED_EDGE('',*,*,#4833,.T.) ;
#6646 = ORIENTED_EDGE('',*,*,#4832,.T.) ;
#6647 = ORIENTED_EDGE('',*,*,#4835,.T.) ;
#6648 = ORIENTED_EDGE('',*,*,#4821,.F.) ;
#6649 = ORIENTED_EDGE('',*,*,#4835,.F.) ;
#6650 = ORIENTED_EDGE('',*,*,#4808,.T.) ;
#6651 = ORIENTED_EDGE('',*,*,#4822,.F.) ;
#6652 = ORIENTED_EDGE('',*,*,#4824,.F.) ;
#6653 = ORIENTED_EDGE('',*,*,#4807,.F.) ;
#6654 = ORIENTED_EDGE('',*,*,#4809,.F.) ;
#6655 = ORIENTED_EDGE('',*,*,#4823,.F.) ;
#6656 = ORIENTED_EDGE('',*,*,#4836,.T.) ;
#6657 = ORIENTED_EDGE('',*,*,#4837,.T.) ;
#6658 = ORIENTED_EDGE('',*,*,#4838,.F.) ;
#6659 = ORIENTED_EDGE('',*,*,#4839,.F.) ;
#6660 = ORIENTED_EDGE('',*,*,#4840,.T.) ;
#6661 = ORIENTED_EDGE('',*,*,#4841,.T.) ;
#6662 = ORIENTED_EDGE('',*,*,#4842,.F.) ;
#6663 = ORIENTED_EDGE('',*,*,#4837,.F.) ;
#6664 = ORIENTED_EDGE('',*,*,#4843,.T.) ;
#6665 = ORIENTED_EDGE('',*,*,#4844,.T.) ;
#6666 = ORIENTED_EDGE('',*,*,#4845,.F.) ;
#6667 = ORIENTED_EDGE('',*,*,#4841,.F.) ;
#6668 = ORIENTED_EDGE('',*,*,#4846,.T.) ;
#6669 = ORIENTED_EDGE('',*,*,#4847,.T.) ;
#6670 = ORIENTED_EDGE('',*,*,#4848,.F.) ;
#6671 = ORIENTED_EDGE('',*,*,#4844,.F.) ;
#6672 = ORIENTED_EDGE('',*,*,#4849,.T.) ;
#6673 = ORIENTED_EDGE('',*,*,#4850,.T.) ;
#6674 = ORIENTED_EDGE('',*,*,#4851,.F.) ;
#6675 = ORIENTED_EDGE('',*,*,#4847,.F.) ;
#6676 = ORIENTED_EDGE('',*,*,#4852,.T.) ;
#6677 = ORIENTED_EDGE('',*,*,#4853,.T.) ;
#6678 = ORIENTED_EDGE('',*,*,#4854,.F.) ;
#6679 = ORIENTED_EDGE('',*,*,#4850,.F.) ;
#6680 = ORIENTED_EDGE('',*,*,#4855,.T.) ;
#6681 = ORIENTED_EDGE('',*,*,#4856,.T.) ;
#6682 = ORIENTED_EDGE('',*,*,#4857,.F.) ;
#6683 = ORIENTED_EDGE('',*,*,#4853,.F.) ;
#6684 = ORIENTED_EDGE('',*,*,#4858,.T.) ;
#6685 = ORIENTED_EDGE('',*,*,#4859,.T.) ;
#6686 = ORIENTED_EDGE('',*,*,#4860,.F.) ;
#6687 = ORIENTED_EDGE('',*,*,#4856,.F.) ;
#6688 = ORIENTED_EDGE('',*,*,#4861,.T.) ;
#6689 = ORIENTED_EDGE('',*,*,#4862,.T.) ;
#6690 = ORIENTED_EDGE('',*,*,#4863,.F.) ;
#6691 = ORIENTED_EDGE('',*,*,#4859,.F.) ;
#6692 = ORIENTED_EDGE('',*,*,#4864,.T.) ;
#6693 = ORIENTED_EDGE('',*,*,#4865,.T.) ;
#6694 = ORIENTED_EDGE('',*,*,#4866,.F.) ;
#6695 = ORIENTED_EDGE('',*,*,#4862,.F.) ;
#6696 = ORIENTED_EDGE('',*,*,#4867,.T.) ;
#6697 = ORIENTED_EDGE('',*,*,#4868,.T.) ;
#6698 = ORIENTED_EDGE('',*,*,#4869,.F.) ;
#6699 = ORIENTED_EDGE('',*,*,#4865,.F.) ;
#6700 = ORIENTED_EDGE('',*,*,#4870,.T.) ;
#6701 = ORIENTED_EDGE('',*,*,#4871,.T.) ;
#6702 = ORIENTED_EDGE('',*,*,#4872,.F.) ;
#6703 = ORIENTED_EDGE('',*,*,#4868,.F.) ;
#6704 = ORIENTED_EDGE('',*,*,#4873,.T.) ;
#6705 = ORIENTED_EDGE('',*,*,#4874,.T.) ;
#6706 = ORIENTED_EDGE('',*,*,#4875,.F.) ;
#6707 = ORIENTED_EDGE('',*,*,#4871,.F.) ;
#6708 = ORIENTED_EDGE('',*,*,#4876,.T.) ;
#6709 = ORIENTED_EDGE('',*,*,#4877,.T.) ;
#6710 = ORIENTED_EDGE('',*,*,#4878,.F.) ;
#6711 = ORIENTED_EDGE('',*,*,#4874,.F.) ;
#6712 = ORIENTED_EDGE('',*,*,#4879,.T.) ;
#6713 = ORIENTED_EDGE('',*,*,#4839,.T.) ;
#6714 = ORIENTED_EDGE('',*,*,#4880,.F.) ;
#6715 = ORIENTED_EDGE('',*,*,#4877,.F.) ;
#6716 = ORIENTED_EDGE('',*,*,#4881,.F.) ;
#6717 = ORIENTED_EDGE('',*,*,#4882,.T.) ;
#6718 = ORIENTED_EDGE('',*,*,#4883,.T.) ;
#6719 = ORIENTED_EDGE('',*,*,#4882,.F.) ;
#6720 = ORIENTED_EDGE('',*,*,#4884,.F.) ;
#6721 = ORIENTED_EDGE('',*,*,#4885,.T.) ;
#6722 = ORIENTED_EDGE('',*,*,#4886,.T.) ;
#6723 = ORIENTED_EDGE('',*,*,#4885,.F.) ;
#6724 = ORIENTED_EDGE('',*,*,#4879,.F.) ;
#6725 = ORIENTED_EDGE('',*,*,#4876,.F.) ;
#6726 = ORIENTED_EDGE('',*,*,#4873,.F.) ;
#6727 = ORIENTED_EDGE('',*,*,#4870,.F.) ;
#6728 = ORIENTED_EDGE('',*,*,#4867,.F.) ;
#6729 = ORIENTED_EDGE('',*,*,#4864,.F.) ;
#6730 = ORIENTED_EDGE('',*,*,#4861,.F.) ;
#6731 = ORIENTED_EDGE('',*,*,#4858,.F.) ;
#6732 = ORIENTED_EDGE('',*,*,#4855,.F.) ;
#6733 = ORIENTED_EDGE('',*,*,#4852,.F.) ;
#6734 = ORIENTED_EDGE('',*,*,#4849,.F.) ;
#6735 = ORIENTED_EDGE('',*,*,#4846,.F.) ;
#6736 = ORIENTED_EDGE('',*,*,#4843,.F.) ;
#6737 = ORIENTED_EDGE('',*,*,#4840,.F.) ;
#6738 = ORIENTED_EDGE('',*,*,#4836,.F.) ;
#6739 = ORIENTED_EDGE('',*,*,#4883,.F.) ;
#6740 = ORIENTED_EDGE('',*,*,#4886,.F.) ;
#6741 = ORIENTED_EDGE('',*,*,#4838,.T.) ;
#6742 = ORIENTED_EDGE('',*,*,#4842,.T.) ;
#6743 = ORIENTED_EDGE('',*,*,#4845,.T.) ;
#6744 = ORIENTED_EDGE('',*,*,#4848,.T.) ;
#6745 = ORIENTED_EDGE('',*,*,#4851,.T.) ;
#6746 = ORIENTED_EDGE('',*,*,#4854,.T.) ;
#6747 = ORIENTED_EDGE('',*,*,#4857,.T.) ;
#6748 = ORIENTED_EDGE('',*,*,#4860,.T.) ;
#6749 = ORIENTED_EDGE('',*,*,#4863,.T.) ;
#6750 = ORIENTED_EDGE('',*,*,#4866,.T.) ;
#6751 = ORIENTED_EDGE('',*,*,#4869,.T.) ;
#6752 = ORIENTED_EDGE('',*,*,#4872,.T.) ;
#6753 = ORIENTED_EDGE('',*,*,#4875,.T.) ;
#6754 = ORIENTED_EDGE('',*,*,#4878,.T.) ;
#6755 = ORIENTED_EDGE('',*,*,#4880,.T.) ;
#6756 = ORIENTED_EDGE('',*,*,#4881,.T.) ;
#6757 = ORIENTED_EDGE('',*,*,#4884,.T.) ;
#6758 = ORIENTED_EDGE('',*,*,#4887,.T.) ;
#6759 = ORIENTED_EDGE('',*,*,#4888,.T.) ;
#6760 = ORIENTED_EDGE('',*,*,#4889,.F.) ;
#6761 = ORIENTED_EDGE('',*,*,#4888,.F.) ;
#6762 = ORIENTED_EDGE('',*,*,#4890,.F.) ;
#6763 = ORIENTED_EDGE('',*,*,#4891,.F.) ;
#6764 = ORIENTED_EDGE('',*,*,#4889,.T.) ;
#6765 = ORIENTED_EDGE('',*,*,#4892,.T.) ;
#6766 = ORIENTED_EDGE('',*,*,#4893,.T.) ;
#6767 = ORIENTED_EDGE('',*,*,#4894,.T.) ;
#6768 = ORIENTED_EDGE('',*,*,#4895,.F.) ;
#6769 = ORIENTED_EDGE('',*,*,#4894,.F.) ;
#6770 = ORIENTED_EDGE('',*,*,#4893,.F.) ;
#6771 = ORIENTED_EDGE('',*,*,#4896,.T.) ;
#6772 = ORIENTED_EDGE('',*,*,#4895,.T.) ;
#6773 = ORIENTED_EDGE('',*,*,#4887,.F.) ;
#6774 = ORIENTED_EDGE('',*,*,#4890,.T.) ;
#6775 = ORIENTED_EDGE('',*,*,#4897,.T.) ;
#6776 = ORIENTED_EDGE('',*,*,#4896,.F.) ;
#6777 = ORIENTED_EDGE('',*,*,#4897,.F.) ;
#6778 = ORIENTED_EDGE('',*,*,#4892,.F.) ;
#6779 = ORIENTED_EDGE('',*,*,#4898,.T.) ;
#6780 = ORIENTED_EDGE('',*,*,#4891,.T.) ;
#6781 = ORIENTED_EDGE('',*,*,#4898,.F.) ;
#6782 = ORIENTED_EDGE('',*,*,#4899,.T.) ;
#6783 = ORIENTED_EDGE('',*,*,#4900,.T.) ;
#6784 = ORIENTED_EDGE('',*,*,#4901,.F.) ;
#6785 = ORIENTED_EDGE('',*,*,#4902,.F.) ;
#6786 = ORIENTED_EDGE('',*,*,#4903,.T.) ;
#6787 = ORIENTED_EDGE('',*,*,#4904,.T.) ;
#6788 = ORIENTED_EDGE('',*,*,#4905,.F.) ;
#6789 = ORIENTED_EDGE('',*,*,#4900,.F.) ;
#6790 = ORIENTED_EDGE('',*,*,#4906,.T.) ;
#6791 = ORIENTED_EDGE('',*,*,#4907,.T.) ;
#6792 = ORIENTED_EDGE('',*,*,#4908,.F.) ;
#6793 = ORIENTED_EDGE('',*,*,#4904,.F.) ;
#6794 = ORIENTED_EDGE('',*,*,#4909,.T.) ;
#6795 = ORIENTED_EDGE('',*,*,#4910,.T.) ;
#6796 = ORIENTED_EDGE('',*,*,#4911,.F.) ;
#6797 = ORIENTED_EDGE('',*,*,#4907,.F.) ;
#6798 = ORIENTED_EDGE('',*,*,#4912,.T.) ;
#6799 = ORIENTED_EDGE('',*,*,#4913,.T.) ;
#6800 = ORIENTED_EDGE('',*,*,#4914,.F.) ;
#6801 = ORIENTED_EDGE('',*,*,#4910,.F.) ;
#6802 = ORIENTED_EDGE('',*,*,#4915,.T.) ;
#6803 = ORIENTED_EDGE('',*,*,#4916,.T.) ;
#6804 = ORIENTED_EDGE('',*,*,#4917,.F.) ;
#6805 = ORIENTED_EDGE('',*,*,#4913,.F.) ;
#6806 = ORIENTED_EDGE('',*,*,#4918,.T.) ;
#6807 = ORIENTED_EDGE('',*,*,#4919,.T.) ;
#6808 = ORIENTED_EDGE('',*,*,#4920,.F.) ;
#6809 = ORIENTED_EDGE('',*,*,#4916,.F.) ;
#6810 = ORIENTED_EDGE('',*,*,#4921,.T.) ;
#6811 = ORIENTED_EDGE('',*,*,#4922,.T.) ;
#6812 = ORIENTED_EDGE('',*,*,#4923,.F.) ;
#6813 = ORIENTED_EDGE('',*,*,#4919,.F.) ;
#6814 = ORIENTED_EDGE('',*,*,#4924,.T.) ;
#6815 = ORIENTED_EDGE('',*,*,#4925,.T.) ;
#6816 = ORIENTED_EDGE('',*,*,#4926,.F.) ;
#6817 = ORIENTED_EDGE('',*,*,#4922,.F.) ;
#6818 = ORIENTED_EDGE('',*,*,#4927,.T.) ;
#6819 = ORIENTED_EDGE('',*,*,#4928,.T.) ;
#6820 = ORIENTED_EDGE('',*,*,#4929,.F.) ;
#6821 = ORIENTED_EDGE('',*,*,#4925,.F.) ;
#6822 = ORIENTED_EDGE('',*,*,#4930,.T.) ;
#6823 = ORIENTED_EDGE('',*,*,#4931,.T.) ;
#6824 = ORIENTED_EDGE('',*,*,#4932,.F.) ;
#6825 = ORIENTED_EDGE('',*,*,#4928,.F.) ;
#6826 = ORIENTED_EDGE('',*,*,#4933,.T.) ;
#6827 = ORIENTED_EDGE('',*,*,#4934,.T.) ;
#6828 = ORIENTED_EDGE('',*,*,#4935,.F.) ;
#6829 = ORIENTED_EDGE('',*,*,#4931,.F.) ;
#6830 = ORIENTED_EDGE('',*,*,#4936,.T.) ;
#6831 = ORIENTED_EDGE('',*,*,#4937,.T.) ;
#6832 = ORIENTED_EDGE('',*,*,#4938,.F.) ;
#6833 = ORIENTED_EDGE('',*,*,#4934,.F.) ;
#6834 = ORIENTED_EDGE('',*,*,#4939,.T.) ;
#6835 = ORIENTED_EDGE('',*,*,#4940,.T.) ;
#6836 = ORIENTED_EDGE('',*,*,#4941,.F.) ;
#6837 = ORIENTED_EDGE('',*,*,#4937,.F.) ;
#6838 = ORIENTED_EDGE('',*,*,#4942,.T.) ;
#6839 = ORIENTED_EDGE('',*,*,#4943,.T.) ;
#6840 = ORIENTED_EDGE('',*,*,#4944,.F.) ;
#6841 = ORIENTED_EDGE('',*,*,#4940,.F.) ;
#6842 = ORIENTED_EDGE('',*,*,#4945,.T.) ;
#6843 = ORIENTED_EDGE('',*,*,#4946,.T.) ;
#6844 = ORIENTED_EDGE('',*,*,#4947,.F.) ;
#6845 = ORIENTED_EDGE('',*,*,#4943,.F.) ;
#6846 = ORIENTED_EDGE('',*,*,#4948,.T.) ;
#6847 = ORIENTED_EDGE('',*,*,#4949,.T.) ;
#6848 = ORIENTED_EDGE('',*,*,#4950,.F.) ;
#6849 = ORIENTED_EDGE('',*,*,#4946,.F.) ;
#6850 = ORIENTED_EDGE('',*,*,#4951,.T.) ;
#6851 = ORIENTED_EDGE('',*,*,#4952,.T.) ;
#6852 = ORIENTED_EDGE('',*,*,#4953,.F.) ;
#6853 = ORIENTED_EDGE('',*,*,#4949,.F.) ;
#6854 = ORIENTED_EDGE('',*,*,#4954,.T.) ;
#6855 = ORIENTED_EDGE('',*,*,#4955,.T.) ;
#6856 = ORIENTED_EDGE('',*,*,#4956,.F.) ;
#6857 = ORIENTED_EDGE('',*,*,#4952,.F.) ;
#6858 = ORIENTED_EDGE('',*,*,#4957,.T.) ;
#6859 = ORIENTED_EDGE('',*,*,#4958,.T.) ;
#6860 = ORIENTED_EDGE('',*,*,#4959,.F.) ;
#6861 = ORIENTED_EDGE('',*,*,#4955,.F.) ;
#6862 = ORIENTED_EDGE('',*,*,#4960,.T.) ;
#6863 = ORIENTED_EDGE('',*,*,#4961,.T.) ;
#6864 = ORIENTED_EDGE('',*,*,#4962,.F.) ;
#6865 = ORIENTED_EDGE('',*,*,#4958,.F.) ;
#6866 = ORIENTED_EDGE('',*,*,#4963,.T.) ;
#6867 = ORIENTED_EDGE('',*,*,#4964,.T.) ;
#6868 = ORIENTED_EDGE('',*,*,#4965,.F.) ;
#6869 = ORIENTED_EDGE('',*,*,#4961,.F.) ;
#6870 = ORIENTED_EDGE('',*,*,#4966,.T.) ;
#6871 = ORIENTED_EDGE('',*,*,#4967,.T.) ;
#6872 = ORIENTED_EDGE('',*,*,#4968,.F.) ;
#6873 = ORIENTED_EDGE('',*,*,#4964,.F.) ;
#6874 = ORIENTED_EDGE('',*,*,#4969,.T.) ;
#6875 = ORIENTED_EDGE('',*,*,#4970,.T.) ;
#6876 = ORIENTED_EDGE('',*,*,#4971,.F.) ;
#6877 = ORIENTED_EDGE('',*,*,#4967,.F.) ;
#6878 = ORIENTED_EDGE('',*,*,#4972,.T.) ;
#6879 = ORIENTED_EDGE('',*,*,#4973,.T.) ;
#6880 = ORIENTED_EDGE('',*,*,#4974,.F.) ;
#6881 = ORIENTED_EDGE('',*,*,#4970,.F.) ;
#6882 = ORIENTED_EDGE('',*,*,#4975,.T.) ;
#6883 = ORIENTED_EDGE('',*,*,#4976,.T.) ;
#6884 = ORIENTED_EDGE('',*,*,#4977,.F.) ;
#6885 = ORIENTED_EDGE('',*,*,#4973,.F.) ;
#6886 = ORIENTED_EDGE('',*,*,#4978,.T.) ;
#6887 = ORIENTED_EDGE('',*,*,#4979,.T.) ;
#6888 = ORIENTED_EDGE('',*,*,#4980,.F.) ;
#6889 = ORIENTED_EDGE('',*,*,#4976,.F.) ;
#6890 = ORIENTED_EDGE('',*,*,#4981,.T.) ;
#6891 = ORIENTED_EDGE('',*,*,#4982,.T.) ;
#6892 = ORIENTED_EDGE('',*,*,#4983,.F.) ;
#6893 = ORIENTED_EDGE('',*,*,#4979,.F.) ;
#6894 = ORIENTED_EDGE('',*,*,#4984,.T.) ;
#6895 = ORIENTED_EDGE('',*,*,#4985,.T.) ;
#6896 = ORIENTED_EDGE('',*,*,#4986,.F.) ;
#6897 = ORIENTED_EDGE('',*,*,#4982,.F.) ;
#6898 = ORIENTED_EDGE('',*,*,#4987,.T.) ;
#6899 = ORIENTED_EDGE('',*,*,#4988,.T.) ;
#6900 = ORIENTED_EDGE('',*,*,#4989,.F.) ;
#6901 = ORIENTED_EDGE('',*,*,#4985,.F.) ;
#6902 = ORIENTED_EDGE('',*,*,#4990,.T.) ;
#6903 = ORIENTED_EDGE('',*,*,#4991,.T.) ;
#6904 = ORIENTED_EDGE('',*,*,#4992,.F.) ;
#6905 = ORIENTED_EDGE('',*,*,#4988,.F.) ;
#6906 = ORIENTED_EDGE('',*,*,#4993,.T.) ;
#6907 = ORIENTED_EDGE('',*,*,#4994,.T.) ;
#6908 = ORIENTED_EDGE('',*,*,#4995,.F.) ;
#6909 = ORIENTED_EDGE('',*,*,#4991,.F.) ;
#6910 = ORIENTED_EDGE('',*,*,#4996,.T.) ;
#6911 = ORIENTED_EDGE('',*,*,#4997,.T.) ;
#6912 = ORIENTED_EDGE('',*,*,#4998,.F.) ;
#6913 = ORIENTED_EDGE('',*,*,#4994,.F.) ;
#6914 = ORIENTED_EDGE('',*,*,#4999,.T.) ;
#6915 = ORIENTED_EDGE('',*,*,#5000,.T.) ;
#6916 = ORIENTED_EDGE('',*,*,#5001,.F.) ;
#6917 = ORIENTED_EDGE('',*,*,#4997,.F.) ;
#6918 = ORIENTED_EDGE('',*,*,#5002,.T.) ;
#6919 = ORIENTED_EDGE('',*,*,#5003,.T.) ;
#6920 = ORIENTED_EDGE('',*,*,#5004,.F.) ;
#6921 = ORIENTED_EDGE('',*,*,#5000,.F.) ;
#6922 = ORIENTED_EDGE('',*,*,#5005,.T.) ;
#6923 = ORIENTED_EDGE('',*,*,#5006,.T.) ;
#6924 = ORIENTED_EDGE('',*,*,#5007,.F.) ;
#6925 = ORIENTED_EDGE('',*,*,#5003,.F.) ;
#6926 = ORIENTED_EDGE('',*,*,#5008,.T.) ;
#6927 = ORIENTED_EDGE('',*,*,#5009,.T.) ;
#6928 = ORIENTED_EDGE('',*,*,#5010,.F.) ;
#6929 = ORIENTED_EDGE('',*,*,#5006,.F.) ;
#6930 = ORIENTED_EDGE('',*,*,#5011,.T.) ;
#6931 = ORIENTED_EDGE('',*,*,#5012,.T.) ;
#6932 = ORIENTED_EDGE('',*,*,#5013,.F.) ;
#6933 = ORIENTED_EDGE('',*,*,#5009,.F.) ;
#6934 = ORIENTED_EDGE('',*,*,#5014,.T.) ;
#6935 = ORIENTED_EDGE('',*,*,#5015,.T.) ;
#6936 = ORIENTED_EDGE('',*,*,#5016,.F.) ;
#6937 = ORIENTED_EDGE('',*,*,#5012,.F.) ;
#6938 = ORIENTED_EDGE('',*,*,#5017,.T.) ;
#6939 = ORIENTED_EDGE('',*,*,#5018,.T.) ;
#6940 = ORIENTED_EDGE('',*,*,#5019,.F.) ;
#6941 = ORIENTED_EDGE('',*,*,#5015,.F.) ;
#6942 = ORIENTED_EDGE('',*,*,#5020,.T.) ;
#6943 = ORIENTED_EDGE('',*,*,#5021,.T.) ;
#6944 = ORIENTED_EDGE('',*,*,#5022,.F.) ;
#6945 = ORIENTED_EDGE('',*,*,#5018,.F.) ;
#6946 = ORIENTED_EDGE('',*,*,#5023,.T.) ;
#6947 = ORIENTED_EDGE('',*,*,#5024,.T.) ;
#6948 = ORIENTED_EDGE('',*,*,#5025,.F.) ;
#6949 = ORIENTED_EDGE('',*,*,#5021,.F.) ;
#6950 = ORIENTED_EDGE('',*,*,#5026,.T.) ;
#6951 = ORIENTED_EDGE('',*,*,#5027,.T.) ;
#6952 = ORIENTED_EDGE('',*,*,#5028,.F.) ;
#6953 = ORIENTED_EDGE('',*,*,#5024,.F.) ;
#6954 = ORIENTED_EDGE('',*,*,#5029,.T.) ;
#6955 = ORIENTED_EDGE('',*,*,#5030,.T.) ;
#6956 = ORIENTED_EDGE('',*,*,#5031,.F.) ;
#6957 = ORIENTED_EDGE('',*,*,#5027,.F.) ;
#6958 = ORIENTED_EDGE('',*,*,#5032,.T.) ;
#6959 = ORIENTED_EDGE('',*,*,#5033,.T.) ;
#6960 = ORIENTED_EDGE('',*,*,#5034,.F.) ;
#6961 = ORIENTED_EDGE('',*,*,#5030,.F.) ;
#6962 = ORIENTED_EDGE('',*,*,#5035,.T.) ;
#6963 = ORIENTED_EDGE('',*,*,#5036,.T.) ;
#6964 = ORIENTED_EDGE('',*,*,#5037,.F.) ;
#6965 = ORIENTED_EDGE('',*,*,#5033,.F.) ;
#6966 = ORIENTED_EDGE('',*,*,#5038,.T.) ;
#6967 = ORIENTED_EDGE('',*,*,#5039,.T.) ;
#6968 = ORIENTED_EDGE('',*,*,#5040,.F.) ;
#6969 = ORIENTED_EDGE('',*,*,#5036,.F.) ;
#6970 = ORIENTED_EDGE('',*,*,#5041,.T.) ;
#6971 = ORIENTED_EDGE('',*,*,#5042,.T.) ;
#6972 = ORIENTED_EDGE('',*,*,#5043,.F.) ;
#6973 = ORIENTED_EDGE('',*,*,#5039,.F.) ;
#6974 = ORIENTED_EDGE('',*,*,#5044,.T.) ;
#6975 = ORIENTED_EDGE('',*,*,#5045,.T.) ;
#6976 = ORIENTED_EDGE('',*,*,#5046,.F.) ;
#6977 = ORIENTED_EDGE('',*,*,#5042,.F.) ;
#6978 = ORIENTED_EDGE('',*,*,#5047,.T.) ;
#6979 = ORIENTED_EDGE('',*,*,#5048,.T.) ;
#6980 = ORIENTED_EDGE('',*,*,#5049,.F.) ;
#6981 = ORIENTED_EDGE('',*,*,#5045,.F.) ;
#6982 = ORIENTED_EDGE('',*,*,#5050,.T.) ;
#6983 = ORIENTED_EDGE('',*,*,#5051,.T.) ;
#6984 = ORIENTED_EDGE('',*,*,#5052,.F.) ;
#6985 = ORIENTED_EDGE('',*,*,#5048,.F.) ;
#6986 = ORIENTED_EDGE('',*,*,#5053,.T.) ;
#6987 = ORIENTED_EDGE('',*,*,#5054,.T.) ;
#6988 = ORIENTED_EDGE('',*,*,#5055,.F.) ;
#6989 = ORIENTED_EDGE('',*,*,#5051,.F.) ;
#6990 = ORIENTED_EDGE('',*,*,#5056,.T.) ;
#6991 = ORIENTED_EDGE('',*,*,#5057,.T.) ;
#6992 = ORIENTED_EDGE('',*,*,#5058,.F.) ;
#6993 = ORIENTED_EDGE('',*,*,#5054,.F.) ;
#6994 = ORIENTED_EDGE('',*,*,#5059,.T.) ;
#6995 = ORIENTED_EDGE('',*,*,#5060,.T.) ;
#6996 = ORIENTED_EDGE('',*,*,#5061,.F.) ;
#6997 = ORIENTED_EDGE('',*,*,#5057,.F.) ;
#6998 = ORIENTED_EDGE('',*,*,#5062,.T.) ;
#6999 = ORIENTED_EDGE('',*,*,#5063,.T.) ;
#7000 = ORIENTED_EDGE('',*,*,#5064,.F.) ;
#7001 = ORIENTED_EDGE('',*,*,#5060,.F.) ;
#7002 = ORIENTED_EDGE('',*,*,#5065,.T.) ;
#7003 = ORIENTED_EDGE('',*,*,#5066,.T.) ;
#7004 = ORIENTED_EDGE('',*,*,#5067,.F.) ;
#7005 = ORIENTED_EDGE('',*,*,#5063,.F.) ;
#7006 = ORIENTED_EDGE('',*,*,#5068,.T.) ;
#7007 = ORIENTED_EDGE('',*,*,#5069,.T.) ;
#7008 = ORIENTED_EDGE('',*,*,#5070,.F.) ;
#7009 = ORIENTED_EDGE('',*,*,#5066,.F.) ;
#7010 = ORIENTED_EDGE('',*,*,#5071,.T.) ;
#7011 = ORIENTED_EDGE('',*,*,#5072,.T.) ;
#7012 = ORIENTED_EDGE('',*,*,#5073,.F.) ;
#7013 = ORIENTED_EDGE('',*,*,#5069,.F.) ;
#7014 = ORIENTED_EDGE('',*,*,#5074,.T.) ;
#7015 = ORIENTED_EDGE('',*,*,#5075,.T.) ;
#7016 = ORIENTED_EDGE('',*,*,#5076,.F.) ;
#7017 = ORIENTED_EDGE('',*,*,#5072,.F.) ;
#7018 = ORIENTED_EDGE('',*,*,#5077,.T.) ;
#7019 = ORIENTED_EDGE('',*,*,#5078,.T.) ;
#7020 = ORIENTED_EDGE('',*,*,#5079,.F.) ;
#7021 = ORIENTED_EDGE('',*,*,#5075,.F.) ;
#7022 = ORIENTED_EDGE('',*,*,#5080,.T.) ;
#7023 = ORIENTED_EDGE('',*,*,#5081,.T.) ;
#7024 = ORIENTED_EDGE('',*,*,#5082,.F.) ;
#7025 = ORIENTED_EDGE('',*,*,#5078,.F.) ;
#7026 = ORIENTED_EDGE('',*,*,#5083,.T.) ;
#7027 = ORIENTED_EDGE('',*,*,#5084,.T.) ;
#7028 = ORIENTED_EDGE('',*,*,#5085,.F.) ;
#7029 = ORIENTED_EDGE('',*,*,#5081,.F.) ;
#7030 = ORIENTED_EDGE('',*,*,#5086,.T.) ;
#7031 = ORIENTED_EDGE('',*,*,#5087,.T.) ;
#7032 = ORIENTED_EDGE('',*,*,#5088,.F.) ;
#7033 = ORIENTED_EDGE('',*,*,#5084,.F.) ;
#7034 = ORIENTED_EDGE('',*,*,#5089,.T.) ;
#7035 = ORIENTED_EDGE('',*,*,#5090,.T.) ;
#7036 = ORIENTED_EDGE('',*,*,#5091,.F.) ;
#7037 = ORIENTED_EDGE('',*,*,#5087,.F.) ;
#7038 = ORIENTED_EDGE('',*,*,#5092,.T.) ;
#7039 = ORIENTED_EDGE('',*,*,#5093,.T.) ;
#7040 = ORIENTED_EDGE('',*,*,#5094,.F.) ;
#7041 = ORIENTED_EDGE('',*,*,#5090,.F.) ;
#7042 = ORIENTED_EDGE('',*,*,#5095,.T.) ;
#7043 = ORIENTED_EDGE('',*,*,#5096,.T.) ;
#7044 = ORIENTED_EDGE('',*,*,#5097,.F.) ;
#7045 = ORIENTED_EDGE('',*,*,#5093,.F.) ;
#7046 = ORIENTED_EDGE('',*,*,#5098,.T.) ;
#7047 = ORIENTED_EDGE('',*,*,#5099,.T.) ;
#7048 = ORIENTED_EDGE('',*,*,#5100,.F.) ;
#7049 = ORIENTED_EDGE('',*,*,#5096,.F.) ;
#7050 = ORIENTED_EDGE('',*,*,#5101,.T.) ;
#7051 = ORIENTED_EDGE('',*,*,#5102,.T.) ;
#7052 = ORIENTED_EDGE('',*,*,#5103,.F.) ;
#7053 = ORIENTED_EDGE('',*,*,#5099,.F.) ;
#7054 = ORIENTED_EDGE('',*,*,#5104,.T.) ;
#7055 = ORIENTED_EDGE('',*,*,#5105,.T.) ;
#7056 = ORIENTED_EDGE('',*,*,#5106,.F.) ;
#7057 = ORIENTED_EDGE('',*,*,#5102,.F.) ;
#7058 = ORIENTED_EDGE('',*,*,#5107,.T.) ;
#7059 = ORIENTED_EDGE('',*,*,#5108,.T.) ;
#7060 = ORIENTED_EDGE('',*,*,#5109,.F.) ;
#7061 = ORIENTED_EDGE('',*,*,#5105,.F.) ;
#7062 = ORIENTED_EDGE('',*,*,#5110,.T.) ;
#7063 = ORIENTED_EDGE('',*,*,#5111,.T.) ;
#7064 = ORIENTED_EDGE('',*,*,#5112,.F.) ;
#7065 = ORIENTED_EDGE('',*,*,#5108,.F.) ;
#7066 = ORIENTED_EDGE('',*,*,#5113,.T.) ;
#7067 = ORIENTED_EDGE('',*,*,#5114,.T.) ;
#7068 = ORIENTED_EDGE('',*,*,#5115,.F.) ;
#7069 = ORIENTED_EDGE('',*,*,#5111,.F.) ;
#7070 = ORIENTED_EDGE('',*,*,#5116,.T.) ;
#7071 = ORIENTED_EDGE('',*,*,#5117,.T.) ;
#7072 = ORIENTED_EDGE('',*,*,#5118,.F.) ;
#7073 = ORIENTED_EDGE('',*,*,#5114,.F.) ;
#7074 = ORIENTED_EDGE('',*,*,#5119,.T.) ;
#7075 = ORIENTED_EDGE('',*,*,#5120,.T.) ;
#7076 = ORIENTED_EDGE('',*,*,#5121,.F.) ;
#7077 = ORIENTED_EDGE('',*,*,#5117,.F.) ;
#7078 = ORIENTED_EDGE('',*,*,#5122,.T.) ;
#7079 = ORIENTED_EDGE('',*,*,#5123,.T.) ;
#7080 = ORIENTED_EDGE('',*,*,#5124,.F.) ;
#7081 = ORIENTED_EDGE('',*,*,#5120,.F.) ;
#7082 = ORIENTED_EDGE('',*,*,#5125,.T.) ;
#7083 = ORIENTED_EDGE('',*,*,#5126,.T.) ;
#7084 = ORIENTED_EDGE('',*,*,#5127,.F.) ;
#7085 = ORIENTED_EDGE('',*,*,#5123,.F.) ;
#7086 = ORIENTED_EDGE('',*,*,#5128,.T.) ;
#7087 = ORIENTED_EDGE('',*,*,#5129,.T.) ;
#7088 = ORIENTED_EDGE('',*,*,#5130,.F.) ;
#7089 = ORIENTED_EDGE('',*,*,#5126,.F.) ;
#7090 = ORIENTED_EDGE('',*,*,#5131,.T.) ;
#7091 = ORIENTED_EDGE('',*,*,#5132,.T.) ;
#7092 = ORIENTED_EDGE('',*,*,#5133,.F.) ;
#7093 = ORIENTED_EDGE('',*,*,#5129,.F.) ;
#7094 = ORIENTED_EDGE('',*,*,#5134,.T.) ;
#7095 = ORIENTED_EDGE('',*,*,#5135,.T.) ;
#7096 = ORIENTED_EDGE('',*,*,#5136,.F.) ;
#7097 = ORIENTED_EDGE('',*,*,#5132,.F.) ;
#7098 = ORIENTED_EDGE('',*,*,#5137,.T.) ;
#7099 = ORIENTED_EDGE('',*,*,#5138,.T.) ;
#7100 = ORIENTED_EDGE('',*,*,#5139,.F.) ;
#7101 = ORIENTED_EDGE('',*,*,#5135,.F.) ;
#7102 = ORIENTED_EDGE('',*,*,#5140,.T.) ;
#7103 = ORIENTED_EDGE('',*,*,#5141,.T.) ;
#7104 = ORIENTED_EDGE('',*,*,#5142,.F.) ;
#7105 = ORIENTED_EDGE('',*,*,#5138,.F.) ;
#7106 = ORIENTED_EDGE('',*,*,#5143,.T.) ;
#7107 = ORIENTED_EDGE('',*,*,#5144,.T.) ;
#7108 = ORIENTED_EDGE('',*,*,#5145,.F.) ;
#7109 = ORIENTED_EDGE('',*,*,#5141,.F.) ;
#7110 = ORIENTED_EDGE('',*,*,#5146,.T.) ;
#7111 = ORIENTED_EDGE('',*,*,#5147,.T.) ;
#7112 = ORIENTED_EDGE('',*,*,#5148,.F.) ;
#7113 = ORIENTED_EDGE('',*,*,#5144,.F.) ;
#7114 = ORIENTED_EDGE('',*,*,#5149,.T.) ;
#7115 = ORIENTED_EDGE('',*,*,#5150,.T.) ;
#7116 = ORIENTED_EDGE('',*,*,#5151,.F.) ;
#7117 = ORIENTED_EDGE('',*,*,#5147,.F.) ;
#7118 = ORIENTED_EDGE('',*,*,#5152,.T.) ;
#7119 = ORIENTED_EDGE('',*,*,#5153,.T.) ;
#7120 = ORIENTED_EDGE('',*,*,#5154,.F.) ;
#7121 = ORIENTED_EDGE('',*,*,#5150,.F.) ;
#7122 = ORIENTED_EDGE('',*,*,#5155,.T.) ;
#7123 = ORIENTED_EDGE('',*,*,#5156,.T.) ;
#7124 = ORIENTED_EDGE('',*,*,#5157,.F.) ;
#7125 = ORIENTED_EDGE('',*,*,#5153,.F.) ;
#7126 = ORIENTED_EDGE('',*,*,#5158,.T.) ;
#7127 = ORIENTED_EDGE('',*,*,#5159,.T.) ;
#7128 = ORIENTED_EDGE('',*,*,#5160,.F.) ;
#7129 = ORIENTED_EDGE('',*,*,#5156,.F.) ;
#7130 = ORIENTED_EDGE('',*,*,#5161,.T.) ;
#7131 = ORIENTED_EDGE('',*,*,#5162,.T.) ;
#7132 = ORIENTED_EDGE('',*,*,#5163,.F.) ;
#7133 = ORIENTED_EDGE('',*,*,#5159,.F.) ;
#7134 = ORIENTED_EDGE('',*,*,#5164,.T.) ;
#7135 = ORIENTED_EDGE('',*,*,#5165,.T.) ;
#7136 = ORIENTED_EDGE('',*,*,#5166,.F.) ;
#7137 = ORIENTED_EDGE('',*,*,#5162,.F.) ;
#7138 = ORIENTED_EDGE('',*,*,#5167,.T.) ;
#7139 = ORIENTED_EDGE('',*,*,#5168,.T.) ;
#7140 = ORIENTED_EDGE('',*,*,#5169,.F.) ;
#7141 = ORIENTED_EDGE('',*,*,#5165,.F.) ;
#7142 = ORIENTED_EDGE('',*,*,#5170,.T.) ;
#7143 = ORIENTED_EDGE('',*,*,#5171,.T.) ;
#7144 = ORIENTED_EDGE('',*,*,#5172,.F.) ;
#7145 = ORIENTED_EDGE('',*,*,#5168,.F.) ;
#7146 = ORIENTED_EDGE('',*,*,#5173,.T.) ;
#7147 = ORIENTED_EDGE('',*,*,#5174,.T.) ;
#7148 = ORIENTED_EDGE('',*,*,#5175,.F.) ;
#7149 = ORIENTED_EDGE('',*,*,#5171,.F.) ;
#7150 = ORIENTED_EDGE('',*,*,#5176,.T.) ;
#7151 = ORIENTED_EDGE('',*,*,#5177,.T.) ;
#7152 = ORIENTED_EDGE('',*,*,#5178,.F.) ;
#7153 = ORIENTED_EDGE('',*,*,#5174,.F.) ;
#7154 = ORIENTED_EDGE('',*,*,#5179,.T.) ;
#7155 = ORIENTED_EDGE('',*,*,#5180,.T.) ;
#7156 = ORIENTED_EDGE('',*,*,#5181,.F.) ;
#7157 = ORIENTED_EDGE('',*,*,#5177,.F.) ;
#7158 = ORIENTED_EDGE('',*,*,#5182,.T.) ;
#7159 = ORIENTED_EDGE('',*,*,#5183,.T.) ;
#7160 = ORIENTED_EDGE('',*,*,#5184,.F.) ;
#7161 = ORIENTED_EDGE('',*,*,#5180,.F.) ;
#7162 = ORIENTED_EDGE('',*,*,#5185,.T.) ;
#7163 = ORIENTED_EDGE('',*,*,#5186,.T.) ;
#7164 = ORIENTED_EDGE('',*,*,#5187,.F.) ;
#7165 = ORIENTED_EDGE('',*,*,#5183,.F.) ;
#7166 = ORIENTED_EDGE('',*,*,#5188,.T.) ;
#7167 = ORIENTED_EDGE('',*,*,#5189,.T.) ;
#7168 = ORIENTED_EDGE('',*,*,#5190,.F.) ;
#7169 = ORIENTED_EDGE('',*,*,#5186,.F.) ;
#7170 = ORIENTED_EDGE('',*,*,#5191,.T.) ;
#7171 = ORIENTED_EDGE('',*,*,#5192,.T.) ;
#7172 = ORIENTED_EDGE('',*,*,#5193,.F.) ;
#7173 = ORIENTED_EDGE('',*,*,#5189,.F.) ;
#7174 = ORIENTED_EDGE('',*,*,#5194,.T.) ;
#7175 = ORIENTED_EDGE('',*,*,#5195,.T.) ;
#7176 = ORIENTED_EDGE('',*,*,#5196,.F.) ;
#7177 = ORIENTED_EDGE('',*,*,#5192,.F.) ;
#7178 = ORIENTED_EDGE('',*,*,#5197,.T.) ;
#7179 = ORIENTED_EDGE('',*,*,#5198,.T.) ;
#7180 = ORIENTED_EDGE('',*,*,#5199,.F.) ;
#7181 = ORIENTED_EDGE('',*,*,#5195,.F.) ;
#7182 = ORIENTED_EDGE('',*,*,#5200,.T.) ;
#7183 = ORIENTED_EDGE('',*,*,#5201,.T.) ;
#7184 = ORIENTED_EDGE('',*,*,#5202,.F.) ;
#7185 = ORIENTED_EDGE('',*,*,#5198,.F.) ;
#7186 = ORIENTED_EDGE('',*,*,#5203,.T.) ;
#7187 = ORIENTED_EDGE('',*,*,#5204,.T.) ;
#7188 = ORIENTED_EDGE('',*,*,#5205,.F.) ;
#7189 = ORIENTED_EDGE('',*,*,#5201,.F.) ;
#7190 = ORIENTED_EDGE('',*,*,#5206,.T.) ;
#7191 = ORIENTED_EDGE('',*,*,#5207,.T.) ;
#7192 = ORIENTED_EDGE('',*,*,#5208,.F.) ;
#7193 = ORIENTED_EDGE('',*,*,#5204,.F.) ;
#7194 = ORIENTED_EDGE('',*,*,#5209,.T.) ;
#7195 = ORIENTED_EDGE('',*,*,#5210,.T.) ;
#7196 = ORIENTED_EDGE('',*,*,#5211,.F.) ;
#7197 = ORIENTED_EDGE('',*,*,#5207,.F.) ;
#7198 = ORIENTED_EDGE('',*,*,#5212,.T.) ;
#7199 = ORIENTED_EDGE('',*,*,#5213,.T.) ;
#7200 = ORIENTED_EDGE('',*,*,#5214,.F.) ;
#7201 = ORIENTED_EDGE('',*,*,#5210,.F.) ;
#7202 = ORIENTED_EDGE('',*,*,#5215,.T.) ;
#7203 = ORIENTED_EDGE('',*,*,#5216,.T.) ;
#7204 = ORIENTED_EDGE('',*,*,#5217,.F.) ;
#7205 = ORIENTED_EDGE('',*,*,#5213,.F.) ;
#7206 = ORIENTED_EDGE('',*,*,#5218,.T.) ;
#7207 = ORIENTED_EDGE('',*,*,#5219,.T.) ;
#7208 = ORIENTED_EDGE('',*,*,#5220,.F.) ;
#7209 = ORIENTED_EDGE('',*,*,#5216,.F.) ;
#7210 = ORIENTED_EDGE('',*,*,#5221,.T.) ;
#7211 = ORIENTED_EDGE('',*,*,#5222,.T.) ;
#7212 = ORIENTED_EDGE('',*,*,#5223,.F.) ;
#7213 = ORIENTED_EDGE('',*,*,#5219,.F.) ;
#7214 = ORIENTED_EDGE('',*,*,#5224,.T.) ;
#7215 = ORIENTED_EDGE('',*,*,#5225,.T.) ;
#7216 = ORIENTED_EDGE('',*,*,#5226,.F.) ;
#7217 = ORIENTED_EDGE('',*,*,#5222,.F.) ;
#7218 = ORIENTED_EDGE('',*,*,#5227,.T.) ;
#7219 = ORIENTED_EDGE('',*,*,#5228,.T.) ;
#7220 = ORIENTED_EDGE('',*,*,#5229,.F.) ;
#7221 = ORIENTED_EDGE('',*,*,#5225,.F.) ;
#7222 = ORIENTED_EDGE('',*,*,#5230,.T.) ;
#7223 = ORIENTED_EDGE('',*,*,#5231,.T.) ;
#7224 = ORIENTED_EDGE('',*,*,#5232,.F.) ;
#7225 = ORIENTED_EDGE('',*,*,#5228,.F.) ;
#7226 = ORIENTED_EDGE('',*,*,#5233,.T.) ;
#7227 = ORIENTED_EDGE('',*,*,#5234,.T.) ;
#7228 = ORIENTED_EDGE('',*,*,#5235,.F.) ;
#7229 = ORIENTED_EDGE('',*,*,#5231,.F.) ;
#7230 = ORIENTED_EDGE('',*,*,#5236,.T.) ;
#7231 = ORIENTED_EDGE('',*,*,#5237,.T.) ;
#7232 = ORIENTED_EDGE('',*,*,#5238,.F.) ;
#7233 = ORIENTED_EDGE('',*,*,#5234,.F.) ;
#7234 = ORIENTED_EDGE('',*,*,#5239,.T.) ;
#7235 = ORIENTED_EDGE('',*,*,#5240,.T.) ;
#7236 = ORIENTED_EDGE('',*,*,#5241,.F.) ;
#7237 = ORIENTED_EDGE('',*,*,#5237,.F.) ;
#7238 = ORIENTED_EDGE('',*,*,#5242,.T.) ;
#7239 = ORIENTED_EDGE('',*,*,#5243,.T.) ;
#7240 = ORIENTED_EDGE('',*,*,#5244,.F.) ;
#7241 = ORIENTED_EDGE('',*,*,#5240,.F.) ;
#7242 = ORIENTED_EDGE('',*,*,#5245,.T.) ;
#7243 = ORIENTED_EDGE('',*,*,#5246,.T.) ;
#7244 = ORIENTED_EDGE('',*,*,#5247,.F.) ;
#7245 = ORIENTED_EDGE('',*,*,#5243,.F.) ;
#7246 = ORIENTED_EDGE('',*,*,#5248,.T.) ;
#7247 = ORIENTED_EDGE('',*,*,#5249,.T.) ;
#7248 = ORIENTED_EDGE('',*,*,#5250,.F.) ;
#7249 = ORIENTED_EDGE('',*,*,#5246,.F.) ;
#7250 = ORIENTED_EDGE('',*,*,#5251,.T.) ;
#7251 = ORIENTED_EDGE('',*,*,#5252,.T.) ;
#7252 = ORIENTED_EDGE('',*,*,#5253,.F.) ;
#7253 = ORIENTED_EDGE('',*,*,#5249,.F.) ;
#7254 = ORIENTED_EDGE('',*,*,#5254,.T.) ;
#7255 = ORIENTED_EDGE('',*,*,#5255,.T.) ;
#7256 = ORIENTED_EDGE('',*,*,#5256,.F.) ;
#7257 = ORIENTED_EDGE('',*,*,#5252,.F.) ;
#7258 = ORIENTED_EDGE('',*,*,#5257,.T.) ;
#7259 = ORIENTED_EDGE('',*,*,#5258,.T.) ;
#7260 = ORIENTED_EDGE('',*,*,#5259,.F.) ;
#7261 = ORIENTED_EDGE('',*,*,#5255,.F.) ;
#7262 = ORIENTED_EDGE('',*,*,#5260,.T.) ;
#7263 = ORIENTED_EDGE('',*,*,#5261,.T.) ;
#7264 = ORIENTED_EDGE('',*,*,#5262,.F.) ;
#7265 = ORIENTED_EDGE('',*,*,#5258,.F.) ;
#7266 = ORIENTED_EDGE('',*,*,#5263,.T.) ;
#7267 = ORIENTED_EDGE('',*,*,#5264,.T.) ;
#7268 = ORIENTED_EDGE('',*,*,#5265,.F.) ;
#7269 = ORIENTED_EDGE('',*,*,#5261,.F.) ;
#7270 = ORIENTED_EDGE('',*,*,#5266,.T.) ;
#7271 = ORIENTED_EDGE('',*,*,#5267,.T.) ;
#7272 = ORIENTED_EDGE('',*,*,#5268,.F.) ;
#7273 = ORIENTED_EDGE('',*,*,#5264,.F.) ;
#7274 = ORIENTED_EDGE('',*,*,#5269,.T.) ;
#7275 = ORIENTED_EDGE('',*,*,#5270,.T.) ;
#7276 = ORIENTED_EDGE('',*,*,#5271,.F.) ;
#7277 = ORIENTED_EDGE('',*,*,#5267,.F.) ;
#7278 = ORIENTED_EDGE('',*,*,#5272,.T.) ;
#7279 = ORIENTED_EDGE('',*,*,#5273,.T.) ;
#7280 = ORIENTED_EDGE('',*,*,#5274,.F.) ;
#7281 = ORIENTED_EDGE('',*,*,#5270,.F.) ;
#7282 = ORIENTED_EDGE('',*,*,#5275,.T.) ;
#7283 = ORIENTED_EDGE('',*,*,#5276,.T.) ;
#7284 = ORIENTED_EDGE('',*,*,#5277,.F.) ;
#7285 = ORIENTED_EDGE('',*,*,#5273,.F.) ;
#7286 = ORIENTED_EDGE('',*,*,#5278,.T.) ;
#7287 = ORIENTED_EDGE('',*,*,#5279,.T.) ;
#7288 = ORIENTED_EDGE('',*,*,#5280,.F.) ;
#7289 = ORIENTED_EDGE('',*,*,#5276,.F.) ;
#7290 = ORIENTED_EDGE('',*,*,#5281,.T.) ;
#7291 = ORIENTED_EDGE('',*,*,#5282,.T.) ;
#7292 = ORIENTED_EDGE('',*,*,#5283,.F.) ;
#7293 = ORIENTED_EDGE('',*,*,#5279,.F.) ;
#7294 = ORIENTED_EDGE('',*,*,#5284,.T.) ;
#7295 = ORIENTED_EDGE('',*,*,#5285,.T.) ;
#7296 = ORIENTED_EDGE('',*,*,#5286,.F.) ;
#7297 = ORIENTED_EDGE('',*,*,#5282,.F.) ;
#7298 = ORIENTED_EDGE('',*,*,#5287,.T.) ;
#7299 = ORIENTED_EDGE('',*,*,#5288,.T.) ;
#7300 = ORIENTED_EDGE('',*,*,#5289,.F.) ;
#7301 = ORIENTED_EDGE('',*,*,#5285,.F.) ;
#7302 = ORIENTED_EDGE('',*,*,#5290,.T.) ;
#7303 = ORIENTED_EDGE('',*,*,#5291,.T.) ;
#7304 = ORIENTED_EDGE('',*,*,#5292,.F.) ;
#7305 = ORIENTED_EDGE('',*,*,#5288,.F.) ;
#7306 = ORIENTED_EDGE('',*,*,#5293,.T.) ;
#7307 = ORIENTED_EDGE('',*,*,#5294,.T.) ;
#7308 = ORIENTED_EDGE('',*,*,#5295,.F.) ;
#7309 = ORIENTED_EDGE('',*,*,#5291,.F.) ;
#7310 = ORIENTED_EDGE('',*,*,#5296,.T.) ;
#7311 = ORIENTED_EDGE('',*,*,#5297,.T.) ;
#7312 = ORIENTED_EDGE('',*,*,#5298,.F.) ;
#7313 = ORIENTED_EDGE('',*,*,#5294,.F.) ;
#7314 = ORIENTED_EDGE('',*,*,#5299,.T.) ;
#7315 = ORIENTED_EDGE('',*,*,#5300,.T.) ;
#7316 = ORIENTED_EDGE('',*,*,#5301,.F.) ;
#7317 = ORIENTED_EDGE('',*,*,#5297,.F.) ;
#7318 = ORIENTED_EDGE('',*,*,#5302,.T.) ;
#7319 = ORIENTED_EDGE('',*,*,#5303,.T.) ;
#7320 = ORIENTED_EDGE('',*,*,#5304,.F.) ;
#7321 = ORIENTED_EDGE('',*,*,#5300,.F.) ;
#7322 = ORIENTED_EDGE('',*,*,#5305,.T.) ;
#7323 = ORIENTED_EDGE('',*,*,#5306,.T.) ;
#7324 = ORIENTED_EDGE('',*,*,#5307,.F.) ;
#7325 = ORIENTED_EDGE('',*,*,#5303,.F.) ;
#7326 = ORIENTED_EDGE('',*,*,#5308,.T.) ;
#7327 = ORIENTED_EDGE('',*,*,#5309,.T.) ;
#7328 = ORIENTED_EDGE('',*,*,#5310,.F.) ;
#7329 = ORIENTED_EDGE('',*,*,#5306,.F.) ;
#7330 = ORIENTED_EDGE('',*,*,#5311,.T.) ;
#7331 = ORIENTED_EDGE('',*,*,#5312,.T.) ;
#7332 = ORIENTED_EDGE('',*,*,#5313,.F.) ;
#7333 = ORIENTED_EDGE('',*,*,#5309,.F.) ;
#7334 = ORIENTED_EDGE('',*,*,#5314,.T.) ;
#7335 = ORIENTED_EDGE('',*,*,#5315,.T.) ;
#7336 = ORIENTED_EDGE('',*,*,#5316,.F.) ;
#7337 = ORIENTED_EDGE('',*,*,#5312,.F.) ;
#7338 = ORIENTED_EDGE('',*,*,#5317,.T.) ;
#7339 = ORIENTED_EDGE('',*,*,#5318,.T.) ;
#7340 = ORIENTED_EDGE('',*,*,#5319,.F.) ;
#7341 = ORIENTED_EDGE('',*,*,#5315,.F.) ;
#7342 = ORIENTED_EDGE('',*,*,#5320,.T.) ;
#7343 = ORIENTED_EDGE('',*,*,#5321,.T.) ;
#7344 = ORIENTED_EDGE('',*,*,#5322,.F.) ;
#7345 = ORIENTED_EDGE('',*,*,#5318,.F.) ;
#7346 = ORIENTED_EDGE('',*,*,#5323,.T.) ;
#7347 = ORIENTED_EDGE('',*,*,#5324,.T.) ;
#7348 = ORIENTED_EDGE('',*,*,#5325,.F.) ;
#7349 = ORIENTED_EDGE('',*,*,#5321,.F.) ;
#7350 = ORIENTED_EDGE('',*,*,#5326,.T.) ;
#7351 = ORIENTED_EDGE('',*,*,#5327,.T.) ;
#7352 = ORIENTED_EDGE('',*,*,#5328,.F.) ;
#7353 = ORIENTED_EDGE('',*,*,#5324,.F.) ;
#7354 = ORIENTED_EDGE('',*,*,#5329,.T.) ;
#7355 = ORIENTED_EDGE('',*,*,#5330,.T.) ;
#7356 = ORIENTED_EDGE('',*,*,#5331,.F.) ;
#7357 = ORIENTED_EDGE('',*,*,#5327,.F.) ;
#7358 = ORIENTED_EDGE('',*,*,#5332,.T.) ;
#7359 = ORIENTED_EDGE('',*,*,#5333,.T.) ;
#7360 = ORIENTED_EDGE('',*,*,#5334,.F.) ;
#7361 = ORIENTED_EDGE('',*,*,#5330,.F.) ;
#7362 = ORIENTED_EDGE('',*,*,#5335,.T.) ;
#7363 = ORIENTED_EDGE('',*,*,#5336,.T.) ;
#7364 = ORIENTED_EDGE('',*,*,#5337,.F.) ;
#7365 = ORIENTED_EDGE('',*,*,#5333,.F.) ;
#7366 = ORIENTED_EDGE('',*,*,#5338,.T.) ;
#7367 = ORIENTED_EDGE('',*,*,#5339,.T.) ;
#7368 = ORIENTED_EDGE('',*,*,#5340,.F.) ;
#7369 = ORIENTED_EDGE('',*,*,#5336,.F.) ;
#7370 = ORIENTED_EDGE('',*,*,#5341,.T.) ;
#7371 = ORIENTED_EDGE('',*,*,#5342,.T.) ;
#7372 = ORIENTED_EDGE('',*,*,#5343,.F.) ;
#7373 = ORIENTED_EDGE('',*,*,#5339,.F.) ;
#7374 = ORIENTED_EDGE('',*,*,#5344,.T.) ;
#7375 = ORIENTED_EDGE('',*,*,#5345,.T.) ;
#7376 = ORIENTED_EDGE('',*,*,#5346,.F.) ;
#7377 = ORIENTED_EDGE('',*,*,#5342,.F.) ;
#7378 = ORIENTED_EDGE('',*,*,#5347,.T.) ;
#7379 = ORIENTED_EDGE('',*,*,#5348,.T.) ;
#7380 = ORIENTED_EDGE('',*,*,#5349,.F.) ;
#7381 = ORIENTED_EDGE('',*,*,#5345,.F.) ;
#7382 = ORIENTED_EDGE('',*,*,#5350,.T.) ;
#7383 = ORIENTED_EDGE('',*,*,#5351,.T.) ;
#7384 = ORIENTED_EDGE('',*,*,#5352,.F.) ;
#7385 = ORIENTED_EDGE('',*,*,#5348,.F.) ;
#7386 = ORIENTED_EDGE('',*,*,#5353,.T.) ;
#7387 = ORIENTED_EDGE('',*,*,#5354,.T.) ;
#7388 = ORIENTED_EDGE('',*,*,#5355,.F.) ;
#7389 = ORIENTED_EDGE('',*,*,#5351,.F.) ;
#7390 = ORIENTED_EDGE('',*,*,#5356,.T.) ;
#7391 = ORIENTED_EDGE('',*,*,#5357,.T.) ;
#7392 = ORIENTED_EDGE('',*,*,#5358,.F.) ;
#7393 = ORIENTED_EDGE('',*,*,#5354,.F.) ;
#7394 = ORIENTED_EDGE('',*,*,#5359,.T.) ;
#7395 = ORIENTED_EDGE('',*,*,#5360,.T.) ;
#7396 = ORIENTED_EDGE('',*,*,#5361,.F.) ;
#7397 = ORIENTED_EDGE('',*,*,#5357,.F.) ;
#7398 = ORIENTED_EDGE('',*,*,#5362,.T.) ;
#7399 = ORIENTED_EDGE('',*,*,#5363,.T.) ;
#7400 = ORIENTED_EDGE('',*,*,#5364,.F.) ;
#7401 = ORIENTED_EDGE('',*,*,#5360,.F.) ;
#7402 = ORIENTED_EDGE('',*,*,#5365,.T.) ;
#7403 = ORIENTED_EDGE('',*,*,#5366,.T.) ;
#7404 = ORIENTED_EDGE('',*,*,#5367,.F.) ;
#7405 = ORIENTED_EDGE('',*,*,#5363,.F.) ;
#7406 = ORIENTED_EDGE('',*,*,#5368,.T.) ;
#7407 = ORIENTED_EDGE('',*,*,#5369,.T.) ;
#7408 = ORIENTED_EDGE('',*,*,#5370,.F.) ;
#7409 = ORIENTED_EDGE('',*,*,#5366,.F.) ;
#7410 = ORIENTED_EDGE('',*,*,#5371,.T.) ;
#7411 = ORIENTED_EDGE('',*,*,#5372,.T.) ;
#7412 = ORIENTED_EDGE('',*,*,#5373,.F.) ;
#7413 = ORIENTED_EDGE('',*,*,#5369,.F.) ;
#7414 = ORIENTED_EDGE('',*,*,#5374,.T.) ;
#7415 = ORIENTED_EDGE('',*,*,#5375,.T.) ;
#7416 = ORIENTED_EDGE('',*,*,#5376,.F.) ;
#7417 = ORIENTED_EDGE('',*,*,#5372,.F.) ;
#7418 = ORIENTED_EDGE('',*,*,#5377,.T.) ;
#7419 = ORIENTED_EDGE('',*,*,#5378,.T.) ;
#7420 = ORIENTED_EDGE('',*,*,#5379,.F.) ;
#7421 = ORIENTED_EDGE('',*,*,#5375,.F.) ;
#7422 = ORIENTED_EDGE('',*,*,#5380,.T.) ;
#7423 = ORIENTED_EDGE('',*,*,#5381,.T.) ;
#7424 = ORIENTED_EDGE('',*,*,#5382,.F.) ;
#7425 = ORIENTED_EDGE('',*,*,#5378,.F.) ;
#7426 = ORIENTED_EDGE('',*,*,#5383,.T.) ;
#7427 = ORIENTED_EDGE('',*,*,#5384,.T.) ;
#7428 = ORIENTED_EDGE('',*,*,#5385,.F.) ;
#7429 = ORIENTED_EDGE('',*,*,#5381,.F.) ;
#7430 = ORIENTED_EDGE('',*,*,#5386,.T.) ;
#7431 = ORIENTED_EDGE('',*,*,#5387,.T.) ;
#7432 = ORIENTED_EDGE('',*,*,#5388,.F.) ;
#7433 = ORIENTED_EDGE('',*,*,#5384,.F.) ;
#7434 = ORIENTED_EDGE('',*,*,#5389,.T.) ;
#7435 = ORIENTED_EDGE('',*,*,#5390,.T.) ;
#7436 = ORIENTED_EDGE('',*,*,#5391,.F.) ;
#7437 = ORIENTED_EDGE('',*,*,#5387,.F.) ;
#7438 = ORIENTED_EDGE('',*,*,#5392,.T.) ;
#7439 = ORIENTED_EDGE('',*,*,#5393,.T.) ;
#7440 = ORIENTED_EDGE('',*,*,#5394,.F.) ;
#7441 = ORIENTED_EDGE('',*,*,#5390,.F.) ;
#7442 = ORIENTED_EDGE('',*,*,#5395,.T.) ;
#7443 = ORIENTED_EDGE('',*,*,#5396,.T.) ;
#7444 = ORIENTED_EDGE('',*,*,#5397,.F.) ;
#7445 = ORIENTED_EDGE('',*,*,#5393,.F.) ;
#7446 = ORIENTED_EDGE('',*,*,#5398,.T.) ;
#7447 = ORIENTED_EDGE('',*,*,#5399,.T.) ;
#7448 = ORIENTED_EDGE('',*,*,#5400,.F.) ;
#7449 = ORIENTED_EDGE('',*,*,#5396,.F.) ;
#7450 = ORIENTED_EDGE('',*,*,#5401,.T.) ;
#7451 = ORIENTED_EDGE('',*,*,#5402,.T.) ;
#7452 = ORIENTED_EDGE('',*,*,#5403,.F.) ;
#7453 = ORIENTED_EDGE('',*,*,#5399,.F.) ;
#7454 = ORIENTED_EDGE('',*,*,#5404,.T.) ;
#7455 = ORIENTED_EDGE('',*,*,#5405,.T.) ;
#7456 = ORIENTED_EDGE('',*,*,#5406,.F.) ;
#7457 = ORIENTED_EDGE('',*,*,#5402,.F.) ;
#7458 = ORIENTED_EDGE('',*,*,#5407,.T.) ;
#7459 = ORIENTED_EDGE('',*,*,#5408,.T.) ;
#7460 = ORIENTED_EDGE('',*,*,#5409,.F.) ;
#7461 = ORIENTED_EDGE('',*,*,#5405,.F.) ;
#7462 = ORIENTED_EDGE('',*,*,#5410,.T.) ;
#7463 = ORIENTED_EDGE('',*,*,#5411,.T.) ;
#7464 = ORIENTED_EDGE('',*,*,#5412,.F.) ;
#7465 = ORIENTED_EDGE('',*,*,#5408,.F.) ;
#7466 = ORIENTED_EDGE('',*,*,#5413,.T.) ;
#7467 = ORIENTED_EDGE('',*,*,#5414,.T.) ;
#7468 = ORIENTED_EDGE('',*,*,#5415,.F.) ;
#7469 = ORIENTED_EDGE('',*,*,#5411,.F.) ;
#7470 = ORIENTED_EDGE('',*,*,#5416,.T.) ;
#7471 = ORIENTED_EDGE('',*,*,#5417,.T.) ;
#7472 = ORIENTED_EDGE('',*,*,#5418,.F.) ;
#7473 = ORIENTED_EDGE('',*,*,#5414,.F.) ;
#7474 = ORIENTED_EDGE('',*,*,#5419,.T.) ;
#7475 = ORIENTED_EDGE('',*,*,#5420,.T.) ;
#7476 = ORIENTED_EDGE('',*,*,#5421,.F.) ;
#7477 = ORIENTED_EDGE('',*,*,#5417,.F.) ;
#7478 = ORIENTED_EDGE('',*,*,#5422,.T.) ;
#7479 = ORIENTED_EDGE('',*,*,#5423,.T.) ;
#7480 = ORIENTED_EDGE('',*,*,#5424,.F.) ;
#7481 = ORIENTED_EDGE('',*,*,#5420,.F.) ;
#7482 = ORIENTED_EDGE('',*,*,#5425,.T.) ;
#7483 = ORIENTED_EDGE('',*,*,#5426,.T.) ;
#7484 = ORIENTED_EDGE('',*,*,#5427,.F.) ;
#7485 = ORIENTED_EDGE('',*,*,#5423,.F.) ;
#7486 = ORIENTED_EDGE('',*,*,#5428,.T.) ;
#7487 = ORIENTED_EDGE('',*,*,#5429,.T.) ;
#7488 = ORIENTED_EDGE('',*,*,#5430,.F.) ;
#7489 = ORIENTED_EDGE('',*,*,#5426,.F.) ;
#7490 = ORIENTED_EDGE('',*,*,#5431,.T.) ;
#7491 = ORIENTED_EDGE('',*,*,#5432,.T.) ;
#7492 = ORIENTED_EDGE('',*,*,#5433,.F.) ;
#7493 = ORIENTED_EDGE('',*,*,#5429,.F.) ;
#7494 = ORIENTED_EDGE('',*,*,#5434,.T.) ;
#7495 = ORIENTED_EDGE('',*,*,#5435,.T.) ;
#7496 = ORIENTED_EDGE('',*,*,#5436,.F.) ;
#7497 = ORIENTED_EDGE('',*,*,#5432,.F.) ;
#7498 = ORIENTED_EDGE('',*,*,#5437,.T.) ;
#7499 = ORIENTED_EDGE('',*,*,#4902,.T.) ;
#7500 = ORIENTED_EDGE('',*,*,#5438,.F.) ;
#7501 = ORIENTED_EDGE('',*,*,#5435,.F.) ;
#7502 = ORIENTED_EDGE('',*,*,#5437,.F.) ;
#7503 = ORIENTED_EDGE('',*,*,#5434,.F.) ;
#7504 = ORIENTED_EDGE('',*,*,#5431,.F.) ;
#7505 = ORIENTED_EDGE('',*,*,#5428,.F.) ;
#7506 = ORIENTED_EDGE('',*,*,#5425,.F.) ;
#7507 = ORIENTED_EDGE('',*,*,#5422,.F.) ;
#7508 = ORIENTED_EDGE('',*,*,#5419,.F.) ;
#7509 = ORIENTED_EDGE('',*,*,#5416,.F.) ;
#7510 = ORIENTED_EDGE('',*,*,#5413,.F.) ;
#7511 = ORIENTED_EDGE('',*,*,#5410,.F.) ;
#7512 = ORIENTED_EDGE('',*,*,#5407,.F.) ;
#7513 = ORIENTED_EDGE('',*,*,#5404,.F.) ;
#7514 = ORIENTED_EDGE('',*,*,#5401,.F.) ;
#7515 = ORIENTED_EDGE('',*,*,#5398,.F.) ;
#7516 = ORIENTED_EDGE('',*,*,#5395,.F.) ;
#7517 = ORIENTED_EDGE('',*,*,#5392,.F.) ;
#7518 = ORIENTED_EDGE('',*,*,#5389,.F.) ;
#7519 = ORIENTED_EDGE('',*,*,#5386,.F.) ;
#7520 = ORIENTED_EDGE('',*,*,#5383,.F.) ;
#7521 = ORIENTED_EDGE('',*,*,#5380,.F.) ;
#7522 = ORIENTED_EDGE('',*,*,#5377,.F.) ;
#7523 = ORIENTED_EDGE('',*,*,#5374,.F.) ;
#7524 = ORIENTED_EDGE('',*,*,#5371,.F.) ;
#7525 = ORIENTED_EDGE('',*,*,#5368,.F.) ;
#7526 = ORIENTED_EDGE('',*,*,#5365,.F.) ;
#7527 = ORIENTED_EDGE('',*,*,#5362,.F.) ;
#7528 = ORIENTED_EDGE('',*,*,#5359,.F.) ;
#7529 = ORIENTED_EDGE('',*,*,#5356,.F.) ;
#7530 = ORIENTED_EDGE('',*,*,#5353,.F.) ;
#7531 = ORIENTED_EDGE('',*,*,#5350,.F.) ;
#7532 = ORIENTED_EDGE('',*,*,#5347,.F.) ;
#7533 = ORIENTED_EDGE('',*,*,#5344,.F.) ;
#7534 = ORIENTED_EDGE('',*,*,#5341,.F.) ;
#7535 = ORIENTED_EDGE('',*,*,#5338,.F.) ;
#7536 = ORIENTED_EDGE('',*,*,#5335,.F.) ;
#7537 = ORIENTED_EDGE('',*,*,#5332,.F.) ;
#7538 = ORIENTED_EDGE('',*,*,#5329,.F.) ;
#7539 = ORIENTED_EDGE('',*,*,#5326,.F.) ;
#7540 = ORIENTED_EDGE('',*,*,#5323,.F.) ;
#7541 = ORIENTED_EDGE('',*,*,#5320,.F.) ;
#7542 = ORIENTED_EDGE('',*,*,#5317,.F.) ;
#7543 = ORIENTED_EDGE('',*,*,#5314,.F.) ;
#7544 = ORIENTED_EDGE('',*,*,#5311,.F.) ;
#7545 = ORIENTED_EDGE('',*,*,#5308,.F.) ;
#7546 = ORIENTED_EDGE('',*,*,#5305,.F.) ;
#7547 = ORIENTED_EDGE('',*,*,#5302,.F.) ;
#7548 = ORIENTED_EDGE('',*,*,#5299,.F.) ;
#7549 = ORIENTED_EDGE('',*,*,#5296,.F.) ;
#7550 = ORIENTED_EDGE('',*,*,#5293,.F.) ;
#7551 = ORIENTED_EDGE('',*,*,#5290,.F.) ;
#7552 = ORIENTED_EDGE('',*,*,#5287,.F.) ;
#7553 = ORIENTED_EDGE('',*,*,#5284,.F.) ;
#7554 = ORIENTED_EDGE('',*,*,#5281,.F.) ;
#7555 = ORIENTED_EDGE('',*,*,#5278,.F.) ;
#7556 = ORIENTED_EDGE('',*,*,#5275,.F.) ;
#7557 = ORIENTED_EDGE('',*,*,#5272,.F.) ;
#7558 = ORIENTED_EDGE('',*,*,#5269,.F.) ;
#7559 = ORIENTED_EDGE('',*,*,#5266,.F.) ;
#7560 = ORIENTED_EDGE('',*,*,#5263,.F.) ;
#7561 = ORIENTED_EDGE('',*,*,#5260,.F.) ;
#7562 = ORIENTED_EDGE('',*,*,#5257,.F.) ;
#7563 = ORIENTED_EDGE('',*,*,#5254,.F.) ;
#7564 = ORIENTED_EDGE('',*,*,#5251,.F.) ;
#7565 = ORIENTED_EDGE('',*,*,#5248,.F.) ;
#7566 = ORIENTED_EDGE('',*,*,#5245,.F.) ;
#7567 = ORIENTED_EDGE('',*,*,#5242,.F.) ;
#7568 = ORIENTED_EDGE('',*,*,#5239,.F.) ;
#7569 = ORIENTED_EDGE('',*,*,#5236,.F.) ;
#7570 = ORIENTED_EDGE('',*,*,#5233,.F.) ;
#7571 = ORIENTED_EDGE('',*,*,#5230,.F.) ;
#7572 = ORIENTED_EDGE('',*,*,#5227,.F.) ;
#7573 = ORIENTED_EDGE('',*,*,#5224,.F.) ;
#7574 = ORIENTED_EDGE('',*,*,#5221,.F.) ;
#7575 = ORIENTED_EDGE('',*,*,#5218,.F.) ;
#7576 = ORIENTED_EDGE('',*,*,#5215,.F.) ;
#7577 = ORIENTED_EDGE('',*,*,#5212,.F.) ;
#7578 = ORIENTED_EDGE('',*,*,#5209,.F.) ;
#7579 = ORIENTED_EDGE('',*,*,#5206,.F.) ;
#7580 = ORIENTED_EDGE('',*,*,#5203,.F.) ;
#7581 = ORIENTED_EDGE('',*,*,#5200,.F.) ;
#7582 = ORIENTED_EDGE('',*,*,#5197,.F.) ;
#7583 = ORIENTED_EDGE('',*,*,#5194,.F.) ;
#7584 = ORIENTED_EDGE('',*,*,#5191,.F.) ;
#7585 = ORIENTED_EDGE('',*,*,#5188,.F.) ;
#7586 = ORIENTED_EDGE('',*,*,#5185,.F.) ;
#7587 = ORIENTED_EDGE('',*,*,#5182,.F.) ;
#7588 = ORIENTED_EDGE('',*,*,#5179,.F.) ;
#7589 = ORIENTED_EDGE('',*,*,#5176,.F.) ;
#7590 = ORIENTED_EDGE('',*,*,#5173,.F.) ;
#7591 = ORIENTED_EDGE('',*,*,#5170,.F.) ;
#7592 = ORIENTED_EDGE('',*,*,#5167,.F.) ;
#7593 = ORIENTED_EDGE('',*,*,#5164,.F.) ;
#7594 = ORIENTED_EDGE('',*,*,#5161,.F.) ;
#7595 = ORIENTED_EDGE('',*,*,#5158,.F.) ;
#7596 = ORIENTED_EDGE('',*,*,#5155,.F.) ;
#7597 = ORIENTED_EDGE('',*,*,#5152,.F.) ;
#7598 = ORIENTED_EDGE('',*,*,#5149,.F.) ;
#7599 = ORIENTED_EDGE('',*,*,#5146,.F.) ;
#7600 = ORIENTED_EDGE('',*,*,#5143,.F.) ;
#7601 = ORIENTED_EDGE('',*,*,#5140,.F.) ;
#7602 = ORIENTED_EDGE('',*,*,#5137,.F.) ;
#7603 = ORIENTED_EDGE('',*,*,#5134,.F.) ;
#7604 = ORIENTED_EDGE('',*,*,#5131,.F.) ;
#7605 = ORIENTED_EDGE('',*,*,#5128,.F.) ;
#7606 = ORIENTED_EDGE('',*,*,#5125,.F.) ;
#7607 = ORIENTED_EDGE('',*,*,#5122,.F.) ;
#7608 = ORIENTED_EDGE('',*,*,#5119,.F.) ;
#7609 = ORIENTED_EDGE('',*,*,#5116,.F.) ;
#7610 = ORIENTED_EDGE('',*,*,#5113,.F.) ;
#7611 = ORIENTED_EDGE('',*,*,#5110,.F.) ;
#7612 = ORIENTED_EDGE('',*,*,#5107,.F.) ;
#7613 = ORIENTED_EDGE('',*,*,#5104,.F.) ;
#7614 = ORIENTED_EDGE('',*,*,#5101,.F.) ;
#7615 = ORIENTED_EDGE('',*,*,#5098,.F.) ;
#7616 = ORIENTED_EDGE('',*,*,#5095,.F.) ;
#7617 = ORIENTED_EDGE('',*,*,#5092,.F.) ;
#7618 = ORIENTED_EDGE('',*,*,#5089,.F.) ;
#7619 = ORIENTED_EDGE('',*,*,#5086,.F.) ;
#7620 = ORIENTED_EDGE('',*,*,#5083,.F.) ;
#7621 = ORIENTED_EDGE('',*,*,#5080,.F.) ;
#7622 = ORIENTED_EDGE('',*,*,#5077,.F.) ;
#7623 = ORIENTED_EDGE('',*,*,#5074,.F.) ;
#7624 = ORIENTED_EDGE('',*,*,#5071,.F.) ;
#7625 = ORIENTED_EDGE('',*,*,#5068,.F.) ;
#7626 = ORIENTED_EDGE('',*,*,#5065,.F.) ;
#7627 = ORIENTED_EDGE('',*,*,#5062,.F.) ;
#7628 = ORIENTED_EDGE('',*,*,#5059,.F.) ;
#7629 = ORIENTED_EDGE('',*,*,#5056,.F.) ;
#7630 = ORIENTED_EDGE('',*,*,#5053,.F.) ;
#7631 = ORIENTED_EDGE('',*,*,#5050,.F.) ;
#7632 = ORIENTED_EDGE('',*,*,#5047,.F.) ;
#7633 = ORIENTED_EDGE('',*,*,#5044,.F.) ;
#7634 = ORIENTED_EDGE('',*,*,#5041,.F.) ;
#7635 = ORIENTED_EDGE('',*,*,#5038,.F.) ;
#7636 = ORIENTED_EDGE('',*,*,#5035,.F.) ;
#7637 = ORIENTED_EDGE('',*,*,#5032,.F.) ;
#7638 = ORIENTED_EDGE('',*,*,#5029,.F.) ;
#7639 = ORIENTED_EDGE('',*,*,#5026,.F.) ;
#7640 = ORIENTED_EDGE('',*,*,#5023,.F.) ;
#7641 = ORIENTED_EDGE('',*,*,#5020,.F.) ;
#7642 = ORIENTED_EDGE('',*,*,#5017,.F.) ;
#7643 = ORIENTED_EDGE('',*,*,#5014,.F.) ;
#7644 = ORIENTED_EDGE('',*,*,#5011,.F.) ;
#7645 = ORIENTED_EDGE('',*,*,#5008,.F.) ;
#7646 = ORIENTED_EDGE('',*,*,#5005,.F.) ;
#7647 = ORIENTED_EDGE('',*,*,#5002,.F.) ;
#7648 = ORIENTED_EDGE('',*,*,#4999,.F.) ;
#7649 = ORIENTED_EDGE('',*,*,#4996,.F.) ;
#7650 = ORIENTED_EDGE('',*,*,#4993,.F.) ;
#7651 = ORIENTED_EDGE('',*,*,#4990,.F.) ;
#7652 = ORIENTED_EDGE('',*,*,#4987,.F.) ;
#7653 = ORIENTED_EDGE('',*,*,#4984,.F.) ;
#7654 = ORIENTED_EDGE('',*,*,#4981,.F.) ;
#7655 = ORIENTED_EDGE('',*,*,#4978,.F.) ;
#7656 = ORIENTED_EDGE('',*,*,#4975,.F.) ;
#7657 = ORIENTED_EDGE('',*,*,#4972,.F.) ;
#7658 = ORIENTED_EDGE('',*,*,#4969,.F.) ;
#7659 = ORIENTED_EDGE('',*,*,#4966,.F.) ;
#7660 = ORIENTED_EDGE('',*,*,#4963,.F.) ;
#7661 = ORIENTED_EDGE('',*,*,#4960,.F.) ;
#7662 = ORIENTED_EDGE('',*,*,#4957,.F.) ;
#7663 = ORIENTED_EDGE('',*,*,#4954,.F.) ;
#7664 = ORIENTED_EDGE('',*,*,#4951,.F.) ;
#7665 = ORIENTED_EDGE('',*,*,#4948,.F.) ;
#7666 = ORIENTED_EDGE('',*,*,#4945,.F.) ;
#7667 = ORIENTED_EDGE('',*,*,#4942,.F.) ;
#7668 = ORIENTED_EDGE('',*,*,#4939,.F.) ;
#7669 = ORIENTED_EDGE('',*,*,#4936,.F.) ;
#7670 = ORIENTED_EDGE('',*,*,#4933,.F.) ;
#7671 = ORIENTED_EDGE('',*,*,#4930,.F.) ;
#7672 = ORIENTED_EDGE('',*,*,#4927,.F.) ;
#7673 = ORIENTED_EDGE('',*,*,#4924,.F.) ;
#7674 = ORIENTED_EDGE('',*,*,#4921,.F.) ;
#7675 = ORIENTED_EDGE('',*,*,#4918,.F.) ;
#7676 = ORIENTED_EDGE('',*,*,#4915,.F.) ;
#7677 = ORIENTED_EDGE('',*,*,#4912,.F.) ;
#7678 = ORIENTED_EDGE('',*,*,#4909,.F.) ;
#7679 = ORIENTED_EDGE('',*,*,#4906,.F.) ;
#7680 = ORIENTED_EDGE('',*,*,#4903,.F.) ;
#7681 = ORIENTED_EDGE('',*,*,#4899,.F.) ;
#7682 = ORIENTED_EDGE('',*,*,#5439,.F.) ;
#7683 = ORIENTED_EDGE('',*,*,#5440,.F.) ;
#7684 = ORIENTED_EDGE('',*,*,#5441,.F.) ;
#7685 = ORIENTED_EDGE('',*,*,#5442,.F.) ;
#7686 = ORIENTED_EDGE('',*,*,#5443,.F.) ;
#7687 = ORIENTED_EDGE('',*,*,#5444,.F.) ;
#7688 = ORIENTED_EDGE('',*,*,#5445,.F.) ;
#7689 = ORIENTED_EDGE('',*,*,#5446,.F.) ;
#7690 = ORIENTED_EDGE('',*,*,#5447,.F.) ;
#7691 = ORIENTED_EDGE('',*,*,#5448,.F.) ;
#7692 = ORIENTED_EDGE('',*,*,#5449,.F.) ;
#7693 = ORIENTED_EDGE('',*,*,#5450,.F.) ;
#7694 = ORIENTED_EDGE('',*,*,#5451,.F.) ;
#7695 = ORIENTED_EDGE('',*,*,#5452,.F.) ;
#7696 = ORIENTED_EDGE('',*,*,#5453,.F.) ;
#7697 = ORIENTED_EDGE('',*,*,#5454,.F.) ;
#7698 = ORIENTED_EDGE('',*,*,#5455,.F.) ;
#7699 = ORIENTED_EDGE('',*,*,#5456,.F.) ;
#7700 = ORIENTED_EDGE('',*,*,#5457,.F.) ;
#7701 = ORIENTED_EDGE('',*,*,#5458,.F.) ;
#7702 = ORIENTED_EDGE('',*,*,#5459,.F.) ;
#7703 = ORIENTED_EDGE('',*,*,#5460,.F.) ;
#7704 = ORIENTED_EDGE('',*,*,#5461,.F.) ;
#7705 = ORIENTED_EDGE('',*,*,#5462,.F.) ;
#7706 = ORIENTED_EDGE('',*,*,#5463,.F.) ;
#7707 = ORIENTED_EDGE('',*,*,#5464,.F.) ;
#7708 = ORIENTED_EDGE('',*,*,#5465,.F.) ;
#7709 = ORIENTED_EDGE('',*,*,#5466,.F.) ;
#7710 = ORIENTED_EDGE('',*,*,#5467,.F.) ;
#7711 = ORIENTED_EDGE('',*,*,#5468,.F.) ;
#7712 = ORIENTED_EDGE('',*,*,#5469,.F.) ;
#7713 = ORIENTED_EDGE('',*,*,#5470,.F.) ;
#7714 = ORIENTED_EDGE('',*,*,#5471,.F.) ;
#7715 = ORIENTED_EDGE('',*,*,#5472,.F.) ;
#7716 = ORIENTED_EDGE('',*,*,#5473,.F.) ;
#7717 = ORIENTED_EDGE('',*,*,#5474,.F.) ;
#7718 = ORIENTED_EDGE('',*,*,#5475,.F.) ;
#7719 = ORIENTED_EDGE('',*,*,#5476,.F.) ;
#7720 = ORIENTED_EDGE('',*,*,#5477,.F.) ;
#7721 = ORIENTED_EDGE('',*,*,#5478,.F.) ;
#7722 = ORIENTED_EDGE('',*,*,#5479,.F.) ;
#7723 = ORIENTED_EDGE('',*,*,#4901,.T.) ;
#7724 = ORIENTED_EDGE('',*,*,#4905,.T.) ;
#7725 = ORIENTED_EDGE('',*,*,#4908,.T.) ;
#7726 = ORIENTED_EDGE('',*,*,#4911,.T.) ;
#7727 = ORIENTED_EDGE('',*,*,#4914,.T.) ;
#7728 = ORIENTED_EDGE('',*,*,#4917,.T.) ;
#7729 = ORIENTED_EDGE('',*,*,#4920,.T.) ;
#7730 = ORIENTED_EDGE('',*,*,#4923,.T.) ;
#7731 = ORIENTED_EDGE('',*,*,#4926,.T.) ;
#7732 = ORIENTED_EDGE('',*,*,#4929,.T.) ;
#7733 = ORIENTED_EDGE('',*,*,#4932,.T.) ;
#7734 = ORIENTED_EDGE('',*,*,#4935,.T.) ;
#7735 = ORIENTED_EDGE('',*,*,#4938,.T.) ;
#7736 = ORIENTED_EDGE('',*,*,#4941,.T.) ;
#7737 = ORIENTED_EDGE('',*,*,#4944,.T.) ;
#7738 = ORIENTED_EDGE('',*,*,#4947,.T.) ;
#7739 = ORIENTED_EDGE('',*,*,#4950,.T.) ;
#7740 = ORIENTED_EDGE('',*,*,#4953,.T.) ;
#7741 = ORIENTED_EDGE('',*,*,#4956,.T.) ;
#7742 = ORIENTED_EDGE('',*,*,#4959,.T.) ;
#7743 = ORIENTED_EDGE('',*,*,#4962,.T.) ;
#7744 = ORIENTED_EDGE('',*,*,#4965,.T.) ;
#7745 = ORIENTED_EDGE('',*,*,#4968,.T.) ;
#7746 = ORIENTED_EDGE('',*,*,#4971,.T.) ;
#7747 = ORIENTED_EDGE('',*,*,#4974,.T.) ;
#7748 = ORIENTED_EDGE('',*,*,#4977,.T.) ;
#7749 = ORIENTED_EDGE('',*,*,#4980,.T.) ;
#7750 = ORIENTED_EDGE('',*,*,#4983,.T.) ;
#7751 = ORIENTED_EDGE('',*,*,#4986,.T.) ;
#7752 = ORIENTED_EDGE('',*,*,#4989,.T.) ;
#7753 = ORIENTED_EDGE('',*,*,#4992,.T.) ;
#7754 = ORIENTED_EDGE('',*,*,#4995,.T.) ;
#7755 = ORIENTED_EDGE('',*,*,#4998,.T.) ;
#7756 = ORIENTED_EDGE('',*,*,#5001,.T.) ;
#7757 = ORIENTED_EDGE('',*,*,#5004,.T.) ;
#7758 = ORIENTED_EDGE('',*,*,#5007,.T.) ;
#7759 = ORIENTED_EDGE('',*,*,#5010,.T.) ;
#7760 = ORIENTED_EDGE('',*,*,#5013,.T.) ;
#7761 = ORIENTED_EDGE('',*,*,#5016,.T.) ;
#7762 = ORIENTED_EDGE('',*,*,#5019,.T.) ;
#7763 = ORIENTED_EDGE('',*,*,#5022,.T.) ;
#7764 = ORIENTED_EDGE('',*,*,#5025,.T.) ;
#7765 = ORIENTED_EDGE('',*,*,#5028,.T.) ;
#7766 = ORIENTED_EDGE('',*,*,#5031,.T.) ;
#7767 = ORIENTED_EDGE('',*,*,#5034,.T.) ;
#7768 = ORIENTED_EDGE('',*,*,#5037,.T.) ;
#7769 = ORIENTED_EDGE('',*,*,#5040,.T.) ;
#7770 = ORIENTED_EDGE('',*,*,#5043,.T.) ;
#7771 = ORIENTED_EDGE('',*,*,#5046,.T.) ;
#7772 = ORIENTED_EDGE('',*,*,#5049,.T.) ;
#7773 = ORIENTED_EDGE('',*,*,#5052,.T.) ;
#7774 = ORIENTED_EDGE('',*,*,#5055,.T.) ;
#7775 = ORIENTED_EDGE('',*,*,#5058,.T.) ;
#7776 = ORIENTED_EDGE('',*,*,#5061,.T.) ;
#7777 = ORIENTED_EDGE('',*,*,#5064,.T.) ;
#7778 = ORIENTED_EDGE('',*,*,#5067,.T.) ;
#7779 = ORIENTED_EDGE('',*,*,#5070,.T.) ;
#7780 = ORIENTED_EDGE('',*,*,#5073,.T.) ;
#7781 = ORIENTED_EDGE('',*,*,#5076,.T.) ;
#7782 = ORIENTED_EDGE('',*,*,#5079,.T.) ;
#7783 = ORIENTED_EDGE('',*,*,#5082,.T.) ;
#7784 = ORIENTED_EDGE('',*,*,#5085,.T.) ;
#7785 = ORIENTED_EDGE('',*,*,#5088,.T.) ;
#7786 = ORIENTED_EDGE('',*,*,#5091,.T.) ;
#7787 = ORIENTED_EDGE('',*,*,#5094,.T.) ;
#7788 = ORIENTED_EDGE('',*,*,#5097,.T.) ;
#7789 = ORIENTED_EDGE('',*,*,#5100,.T.) ;
#7790 = ORIENTED_EDGE('',*,*,#5103,.T.) ;
#7791 = ORIENTED_EDGE('',*,*,#5106,.T.) ;
#7792 = ORIENTED_EDGE('',*,*,#5109,.T.) ;
#7793 = ORIENTED_EDGE('',*,*,#5112,.T.) ;
#7794 = ORIENTED_EDGE('',*,*,#5115,.T.) ;
#7795 = ORIENTED_EDGE('',*,*,#5118,.T.) ;
#7796 = ORIENTED_EDGE('',*,*,#5121,.T.) ;
#7797 = ORIENTED_EDGE('',*,*,#5124,.T.) ;
#7798 = ORIENTED_EDGE('',*,*,#5127,.T.) ;
#7799 = ORIENTED_EDGE('',*,*,#5130,.T.) ;
#7800 = ORIENTED_EDGE('',*,*,#5133,.T.) ;
#7801 = ORIENTED_EDGE('',*,*,#5136,.T.) ;
#7802 = ORIENTED_EDGE('',*,*,#5139,.T.) ;
#7803 = ORIENTED_EDGE('',*,*,#5142,.T.) ;
#7804 = ORIENTED_EDGE('',*,*,#5145,.T.) ;
#7805 = ORIENTED_EDGE('',*,*,#5148,.T.) ;
#7806 = ORIENTED_EDGE('',*,*,#5151,.T.) ;
#7807 = ORIENTED_EDGE('',*,*,#5154,.T.) ;
#7808 = ORIENTED_EDGE('',*,*,#5157,.T.) ;
#7809 = ORIENTED_EDGE('',*,*,#5160,.T.) ;
#7810 = ORIENTED_EDGE('',*,*,#5163,.T.) ;
#7811 = ORIENTED_EDGE('',*,*,#5166,.T.) ;
#7812 = ORIENTED_EDGE('',*,*,#5169,.T.) ;
#7813 = ORIENTED_EDGE('',*,*,#5172,.T.) ;
#7814 = ORIENTED_EDGE('',*,*,#5175,.T.) ;
#7815 = ORIENTED_EDGE('',*,*,#5178,.T.) ;
#7816 = ORIENTED_EDGE('',*,*,#5181,.T.) ;
#7817 = ORIENTED_EDGE('',*,*,#5184,.T.) ;
#7818 = ORIENTED_EDGE('',*,*,#5187,.T.) ;
#7819 = ORIENTED_EDGE('',*,*,#5190,.T.) ;
#7820 = ORIENTED_EDGE('',*,*,#5193,.T.) ;
#7821 = ORIENTED_EDGE('',*,*,#5196,.T.) ;
#7822 = ORIENTED_EDGE('',*,*,#5199,.T.) ;
#7823 = ORIENTED_EDGE('',*,*,#5202,.T.) ;
#7824 = ORIENTED_EDGE('',*,*,#5205,.T.) ;
#7825 = ORIENTED_EDGE('',*,*,#5208,.T.) ;
#7826 = ORIENTED_EDGE('',*,*,#5211,.T.) ;
#7827 = ORIENTED_EDGE('',*,*,#5214,.T.) ;
#7828 = ORIENTED_EDGE('',*,*,#5217,.T.) ;
#7829 = ORIENTED_EDGE('',*,*,#5220,.T.) ;
#7830 = ORIENTED_EDGE('',*,*,#5223,.T.) ;
#7831 = ORIENTED_EDGE('',*,*,#5226,.T.) ;
#7832 = ORIENTED_EDGE('',*,*,#5229,.T.) ;
#7833 = ORIENTED_EDGE('',*,*,#5232,.T.) ;
#7834 = ORIENTED_EDGE('',*,*,#5235,.T.) ;
#7835 = ORIENTED_EDGE('',*,*,#5238,.T.) ;
#7836 = ORIENTED_EDGE('',*,*,#5241,.T.) ;
#7837 = ORIENTED_EDGE('',*,*,#5244,.T.) ;
#7838 = ORIENTED_EDGE('',*,*,#5247,.T.) ;
#7839 = ORIENTED_EDGE('',*,*,#5250,.T.) ;
#7840 = ORIENTED_EDGE('',*,*,#5253,.T.) ;
#7841 = ORIENTED_EDGE('',*,*,#5256,.T.) ;
#7842 = ORIENTED_EDGE('',*,*,#5259,.T.) ;
#7843 = ORIENTED_EDGE('',*,*,#5262,.T.) ;
#7844 = ORIENTED_EDGE('',*,*,#5265,.T.) ;
#7845 = ORIENTED_EDGE('',*,*,#5268,.T.) ;
#7846 = ORIENTED_EDGE('',*,*,#5271,.T.) ;
#7847 = ORIENTED_EDGE('',*,*,#5274,.T.) ;
#7848 = ORIENTED_EDGE('',*,*,#5277,.T.) ;
#7849 = ORIENTED_EDGE('',*,*,#5280,.T.) ;
#7850 = ORIENTED_EDGE('',*,*,#5283,.T.) ;
#7851 = ORIENTED_EDGE('',*,*,#5286,.T.) ;
#7852 = ORIENTED_EDGE('',*,*,#5289,.T.) ;
#7853 = ORIENTED_EDGE('',*,*,#5292,.T.) ;
#7854 = ORIENTED_EDGE('',*,*,#5295,.T.) ;
#7855 = ORIENTED_EDGE('',*,*,#5298,.T.) ;
#7856 = ORIENTED_EDGE('',*,*,#5301,.T.) ;
#7857 = ORIENTED_EDGE('',*,*,#5304,.T.) ;
#7858 = ORIENTED_EDGE('',*,*,#5307,.T.) ;
#7859 = ORIENTED_EDGE('',*,*,#5310,.T.) ;
#7860 = ORIENTED_EDGE('',*,*,#5313,.T.) ;
#7861 = ORIENTED_EDGE('',*,*,#5316,.T.) ;
#7862 = ORIENTED_EDGE('',*,*,#5319,.T.) ;
#7863 = ORIENTED_EDGE('',*,*,#5322,.T.) ;
#7864 = ORIENTED_EDGE('',*,*,#5325,.T.) ;
#7865 = ORIENTED_EDGE('',*,*,#5328,.T.) ;
#7866 = ORIENTED_EDGE('',*,*,#5331,.T.) ;
#7867 = ORIENTED_EDGE('',*,*,#5334,.T.) ;
#7868 = ORIENTED_EDGE('',*,*,#5337,.T.) ;
#7869 = ORIENTED_EDGE('',*,*,#5340,.T.) ;
#7870 = ORIENTED_EDGE('',*,*,#5343,.T.) ;
#7871 = ORIENTED_EDGE('',*,*,#5346,.T.) ;
#7872 = ORIENTED_EDGE('',*,*,#5349,.T.) ;
#7873 = ORIENTED_EDGE('',*,*,#5352,.T.) ;
#7874 = ORIENTED_EDGE('',*,*,#5355,.T.) ;
#7875 = ORIENTED_EDGE('',*,*,#5358,.T.) ;
#7876 = ORIENTED_EDGE('',*,*,#5361,.T.) ;
#7877 = ORIENTED_EDGE('',*,*,#5364,.T.) ;
#7878 = ORIENTED_EDGE('',*,*,#5367,.T.) ;
#7879 = ORIENTED_EDGE('',*,*,#5370,.T.) ;
#7880 = ORIENTED_EDGE('',*,*,#5373,.T.) ;
#7881 = ORIENTED_EDGE('',*,*,#5376,.T.) ;
#7882 = ORIENTED_EDGE('',*,*,#5379,.T.) ;
#7883 = ORIENTED_EDGE('',*,*,#5382,.T.) ;
#7884 = ORIENTED_EDGE('',*,*,#5385,.T.) ;
#7885 = ORIENTED_EDGE('',*,*,#5388,.T.) ;
#7886 = ORIENTED_EDGE('',*,*,#5391,.T.) ;
#7887 = ORIENTED_EDGE('',*,*,#5394,.T.) ;
#7888 = ORIENTED_EDGE('',*,*,#5397,.T.) ;
#7889 = ORIENTED_EDGE('',*,*,#5400,.T.) ;
#7890 = ORIENTED_EDGE('',*,*,#5403,.T.) ;
#7891 = ORIENTED_EDGE('',*,*,#5406,.T.) ;
#7892 = ORIENTED_EDGE('',*,*,#5409,.T.) ;
#7893 = ORIENTED_EDGE('',*,*,#5412,.T.) ;
#7894 = ORIENTED_EDGE('',*,*,#5415,.T.) ;
#7895 = ORIENTED_EDGE('',*,*,#5418,.T.) ;
#7896 = ORIENTED_EDGE('',*,*,#5421,.T.) ;
#7897 = ORIENTED_EDGE('',*,*,#5424,.T.) ;
#7898 = ORIENTED_EDGE('',*,*,#5427,.T.) ;
#7899 = ORIENTED_EDGE('',*,*,#5430,.T.) ;
#7900 = ORIENTED_EDGE('',*,*,#5433,.T.) ;
#7901 = ORIENTED_EDGE('',*,*,#5436,.T.) ;
#7902 = ORIENTED_EDGE('',*,*,#5438,.T.) ;
#7903 = ORIENTED_EDGE('',*,*,#5480,.T.) ;
#7904 = ORIENTED_EDGE('',*,*,#5445,.T.) ;
#7905 = ORIENTED_EDGE('',*,*,#5481,.T.) ;
#7906 = ORIENTED_EDGE('',*,*,#5482,.F.) ;
#7907 = ORIENTED_EDGE('',*,*,#5483,.F.) ;
#7908 = ORIENTED_EDGE('',*,*,#5446,.T.) ;
#7909 = ORIENTED_EDGE('',*,*,#5483,.T.) ;
#7910 = ORIENTED_EDGE('',*,*,#5484,.F.) ;
#7911 = ORIENTED_EDGE('',*,*,#5485,.F.) ;
#7912 = ORIENTED_EDGE('',*,*,#5486,.F.) ;
#7913 = ORIENTED_EDGE('',*,*,#5439,.T.) ;
#7914 = ORIENTED_EDGE('',*,*,#5485,.T.) ;
#7915 = ORIENTED_EDGE('',*,*,#5487,.F.) ;
#7916 = ORIENTED_EDGE('',*,*,#5440,.T.) ;
#7917 = ORIENTED_EDGE('',*,*,#5486,.T.) ;
#7918 = ORIENTED_EDGE('',*,*,#5488,.F.) ;
#7919 = ORIENTED_EDGE('',*,*,#5489,.F.) ;
#7920 = ORIENTED_EDGE('',*,*,#5441,.T.) ;
#7921 = ORIENTED_EDGE('',*,*,#5489,.T.) ;
#7922 = ORIENTED_EDGE('',*,*,#5490,.F.) ;
#7923 = ORIENTED_EDGE('',*,*,#5491,.F.) ;
#7924 = ORIENTED_EDGE('',*,*,#5442,.T.) ;
#7925 = ORIENTED_EDGE('',*,*,#5491,.T.) ;
#7926 = ORIENTED_EDGE('',*,*,#5492,.F.) ;
#7927 = ORIENTED_EDGE('',*,*,#5493,.F.) ;
#7928 = ORIENTED_EDGE('',*,*,#5443,.T.) ;
#7929 = ORIENTED_EDGE('',*,*,#5493,.T.) ;
#7930 = ORIENTED_EDGE('',*,*,#5494,.F.) ;
#7931 = ORIENTED_EDGE('',*,*,#5495,.F.) ;
#7932 = ORIENTED_EDGE('',*,*,#5444,.T.) ;
#7933 = ORIENTED_EDGE('',*,*,#5495,.T.) ;
#7934 = ORIENTED_EDGE('',*,*,#5496,.F.) ;
#7935 = ORIENTED_EDGE('',*,*,#5481,.F.) ;
#7936 = ORIENTED_EDGE('',*,*,#5497,.F.) ;
#7937 = ORIENTED_EDGE('',*,*,#5498,.T.) ;
#7938 = ORIENTED_EDGE('',*,*,#5447,.T.) ;
#7939 = ORIENTED_EDGE('',*,*,#5498,.F.) ;
#7940 = ORIENTED_EDGE('',*,*,#5454,.T.) ;
#7941 = ORIENTED_EDGE('',*,*,#5499,.T.) ;
#7942 = ORIENTED_EDGE('',*,*,#5500,.F.) ;
#7943 = ORIENTED_EDGE('',*,*,#5501,.F.) ;
#7944 = ORIENTED_EDGE('',*,*,#5455,.T.) ;
#7945 = ORIENTED_EDGE('',*,*,#5501,.T.) ;
#7946 = ORIENTED_EDGE('',*,*,#5502,.F.) ;
#7947 = ORIENTED_EDGE('',*,*,#5503,.F.) ;
#7948 = ORIENTED_EDGE('',*,*,#5504,.F.) ;
#7949 = ORIENTED_EDGE('',*,*,#5448,.T.) ;
#7950 = ORIENTED_EDGE('',*,*,#5503,.T.) ;
#7951 = ORIENTED_EDGE('',*,*,#5505,.F.) ;
#7952 = ORIENTED_EDGE('',*,*,#5449,.T.) ;
#7953 = ORIENTED_EDGE('',*,*,#5504,.T.) ;
#7954 = ORIENTED_EDGE('',*,*,#5506,.F.) ;
#7955 = ORIENTED_EDGE('',*,*,#5507,.F.) ;
#7956 = ORIENTED_EDGE('',*,*,#5450,.T.) ;
#7957 = ORIENTED_EDGE('',*,*,#5507,.T.) ;
#7958 = ORIENTED_EDGE('',*,*,#5508,.F.) ;
#7959 = ORIENTED_EDGE('',*,*,#5509,.F.) ;
#7960 = ORIENTED_EDGE('',*,*,#5451,.T.) ;
#7961 = ORIENTED_EDGE('',*,*,#5509,.T.) ;
#7962 = ORIENTED_EDGE('',*,*,#5510,.F.) ;
#7963 = ORIENTED_EDGE('',*,*,#5511,.F.) ;
#7964 = ORIENTED_EDGE('',*,*,#5452,.T.) ;
#7965 = ORIENTED_EDGE('',*,*,#5511,.T.) ;
#7966 = ORIENTED_EDGE('',*,*,#5512,.F.) ;
#7967 = ORIENTED_EDGE('',*,*,#5513,.F.) ;
#7968 = ORIENTED_EDGE('',*,*,#5453,.T.) ;
#7969 = ORIENTED_EDGE('',*,*,#5513,.T.) ;
#7970 = ORIENTED_EDGE('',*,*,#5514,.F.) ;
#7971 = ORIENTED_EDGE('',*,*,#5499,.F.) ;
#7972 = ORIENTED_EDGE('',*,*,#5462,.T.) ;
#7973 = ORIENTED_EDGE('',*,*,#5515,.T.) ;
#7974 = ORIENTED_EDGE('',*,*,#5516,.F.) ;
#7975 = ORIENTED_EDGE('',*,*,#5517,.F.) ;
#7976 = ORIENTED_EDGE('',*,*,#5463,.T.) ;
#7977 = ORIENTED_EDGE('',*,*,#5517,.T.) ;
#7978 = ORIENTED_EDGE('',*,*,#5518,.F.) ;
#7979 = ORIENTED_EDGE('',*,*,#5519,.F.) ;
#7980 = ORIENTED_EDGE('',*,*,#5520,.F.) ;
#7981 = ORIENTED_EDGE('',*,*,#5456,.T.) ;
#7982 = ORIENTED_EDGE('',*,*,#5519,.T.) ;
#7983 = ORIENTED_EDGE('',*,*,#5521,.F.) ;
#7984 = ORIENTED_EDGE('',*,*,#5457,.T.) ;
#7985 = ORIENTED_EDGE('',*,*,#5520,.T.) ;
#7986 = ORIENTED_EDGE('',*,*,#5522,.F.) ;
#7987 = ORIENTED_EDGE('',*,*,#5523,.F.) ;
#7988 = ORIENTED_EDGE('',*,*,#5458,.T.) ;
#7989 = ORIENTED_EDGE('',*,*,#5523,.T.) ;
#7990 = ORIENTED_EDGE('',*,*,#5524,.F.) ;
#7991 = ORIENTED_EDGE('',*,*,#5525,.F.) ;
#7992 = ORIENTED_EDGE('',*,*,#5459,.T.) ;
#7993 = ORIENTED_EDGE('',*,*,#5525,.T.) ;
#7994 = ORIENTED_EDGE('',*,*,#5526,.F.) ;
#7995 = ORIENTED_EDGE('',*,*,#5527,.F.) ;
#7996 = ORIENTED_EDGE('',*,*,#5460,.T.) ;
#7997 = ORIENTED_EDGE('',*,*,#5527,.T.) ;
#7998 = ORIENTED_EDGE('',*,*,#5528,.F.) ;
#7999 = ORIENTED_EDGE('',*,*,#5529,.F.) ;
#8000 = ORIENTED_EDGE('',*,*,#5461,.T.) ;
#8001 = ORIENTED_EDGE('',*,*,#5529,.T.) ;
#8002 = ORIENTED_EDGE('',*,*,#5530,.F.) ;
#8003 = ORIENTED_EDGE('',*,*,#5515,.F.) ;
#8004 = ORIENTED_EDGE('',*,*,#5470,.T.) ;
#8005 = ORIENTED_EDGE('',*,*,#5531,.T.) ;
#8006 = ORIENTED_EDGE('',*,*,#5532,.F.) ;
#8007 = ORIENTED_EDGE('',*,*,#5533,.F.) ;
#8008 = ORIENTED_EDGE('',*,*,#5471,.T.) ;
#8009 = ORIENTED_EDGE('',*,*,#5533,.T.) ;
#8010 = ORIENTED_EDGE('',*,*,#5534,.F.) ;
#8011 = ORIENTED_EDGE('',*,*,#5535,.F.) ;
#8012 = ORIENTED_EDGE('',*,*,#5536,.F.) ;
#8013 = ORIENTED_EDGE('',*,*,#5464,.T.) ;
#8014 = ORIENTED_EDGE('',*,*,#5535,.T.) ;
#8015 = ORIENTED_EDGE('',*,*,#5537,.F.) ;
#8016 = ORIENTED_EDGE('',*,*,#5465,.T.) ;
#8017 = ORIENTED_EDGE('',*,*,#5536,.T.) ;
#8018 = ORIENTED_EDGE('',*,*,#5538,.F.) ;
#8019 = ORIENTED_EDGE('',*,*,#5539,.F.) ;
#8020 = ORIENTED_EDGE('',*,*,#5466,.T.) ;
#8021 = ORIENTED_EDGE('',*,*,#5539,.T.) ;
#8022 = ORIENTED_EDGE('',*,*,#5540,.F.) ;
#8023 = ORIENTED_EDGE('',*,*,#5541,.F.) ;
#8024 = ORIENTED_EDGE('',*,*,#5467,.T.) ;
#8025 = ORIENTED_EDGE('',*,*,#5541,.T.) ;
#8026 = ORIENTED_EDGE('',*,*,#5542,.F.) ;
#8027 = ORIENTED_EDGE('',*,*,#5543,.F.) ;
#8028 = ORIENTED_EDGE('',*,*,#5468,.T.) ;
#8029 = ORIENTED_EDGE('',*,*,#5543,.T.) ;
#8030 = ORIENTED_EDGE('',*,*,#5544,.F.) ;
#8031 = ORIENTED_EDGE('',*,*,#5545,.F.) ;
#8032 = ORIENTED_EDGE('',*,*,#5469,.T.) ;
#8033 = ORIENTED_EDGE('',*,*,#5545,.T.) ;
#8034 = ORIENTED_EDGE('',*,*,#5546,.F.) ;
#8035 = ORIENTED_EDGE('',*,*,#5531,.F.) ;
#8036 = ORIENTED_EDGE('',*,*,#5478,.T.) ;
#8037 = ORIENTED_EDGE('',*,*,#5547,.T.) ;
#8038 = ORIENTED_EDGE('',*,*,#5548,.F.) ;
#8039 = ORIENTED_EDGE('',*,*,#5549,.F.) ;
#8040 = ORIENTED_EDGE('',*,*,#5479,.T.) ;
#8041 = ORIENTED_EDGE('',*,*,#5549,.T.) ;
#8042 = ORIENTED_EDGE('',*,*,#5550,.F.) ;
#8043 = ORIENTED_EDGE('',*,*,#5551,.F.) ;
#8044 = ORIENTED_EDGE('',*,*,#5552,.F.) ;
#8045 = ORIENTED_EDGE('',*,*,#5472,.T.) ;
#8046 = ORIENTED_EDGE('',*,*,#5551,.T.) ;
#8047 = ORIENTED_EDGE('',*,*,#5553,.F.) ;
#8048 = ORIENTED_EDGE('',*,*,#5473,.T.) ;
#8049 = ORIENTED_EDGE('',*,*,#5552,.T.) ;
#8050 = ORIENTED_EDGE('',*,*,#5554,.F.) ;
#8051 = ORIENTED_EDGE('',*,*,#5555,.F.) ;
#8052 = ORIENTED_EDGE('',*,*,#5474,.T.) ;
#8053 = ORIENTED_EDGE('',*,*,#5555,.T.) ;
#8054 = ORIENTED_EDGE('',*,*,#5556,.F.) ;
#8055 = ORIENTED_EDGE('',*,*,#5557,.F.) ;
#8056 = ORIENTED_EDGE('',*,*,#5475,.T.) ;
#8057 = ORIENTED_EDGE('',*,*,#5557,.T.) ;
#8058 = ORIENTED_EDGE('',*,*,#5558,.F.) ;
#8059 = ORIENTED_EDGE('',*,*,#5559,.F.) ;
#8060 = ORIENTED_EDGE('',*,*,#5476,.T.) ;
#8061 = ORIENTED_EDGE('',*,*,#5559,.T.) ;
#8062 = ORIENTED_EDGE('',*,*,#5560,.F.) ;
#8063 = ORIENTED_EDGE('',*,*,#5561,.F.) ;
#8064 = ORIENTED_EDGE('',*,*,#5477,.T.) ;
#8065 = ORIENTED_EDGE('',*,*,#5561,.T.) ;
#8066 = ORIENTED_EDGE('',*,*,#5562,.F.) ;
#8067 = ORIENTED_EDGE('',*,*,#5547,.F.) ;
#8068 = ORIENTED_EDGE('',*,*,#5480,.F.) ;
#8069 = ORIENTED_EDGE('',*,*,#5563,.T.) ;
#8070 = ORIENTED_EDGE('',*,*,#5564,.F.) ;
#8071 = ORIENTED_EDGE('',*,*,#5563,.F.) ;
#8072 = ORIENTED_EDGE('',*,*,#5565,.F.) ;
#8073 = ORIENTED_EDGE('',*,*,#5566,.T.) ;
#8074 = ORIENTED_EDGE('',*,*,#5567,.F.) ;
#8075 = ORIENTED_EDGE('',*,*,#5566,.F.) ;
#8076 = ORIENTED_EDGE('',*,*,#5564,.T.) ;
#8077 = ORIENTED_EDGE('',*,*,#5565,.T.) ;
#8078 = ORIENTED_EDGE('',*,*,#5567,.T.) ;
#8079 = ORIENTED_EDGE('',*,*,#5496,.T.) ;
#8080 = ORIENTED_EDGE('',*,*,#5494,.T.) ;
#8081 = ORIENTED_EDGE('',*,*,#5492,.T.) ;
#8082 = ORIENTED_EDGE('',*,*,#5490,.T.) ;
#8083 = ORIENTED_EDGE('',*,*,#5488,.T.) ;
#8084 = ORIENTED_EDGE('',*,*,#5487,.T.) ;
#8085 = ORIENTED_EDGE('',*,*,#5484,.T.) ;
#8086 = ORIENTED_EDGE('',*,*,#5482,.T.) ;
#8087 = ORIENTED_EDGE('',*,*,#5497,.T.) ;
#8088 = ORIENTED_EDGE('',*,*,#5514,.T.) ;
#8089 = ORIENTED_EDGE('',*,*,#5512,.T.) ;
#8090 = ORIENTED_EDGE('',*,*,#5510,.T.) ;
#8091 = ORIENTED_EDGE('',*,*,#5508,.T.) ;
#8092 = ORIENTED_EDGE('',*,*,#5506,.T.) ;
#8093 = ORIENTED_EDGE('',*,*,#5505,.T.) ;
#8094 = ORIENTED_EDGE('',*,*,#5502,.T.) ;
#8095 = ORIENTED_EDGE('',*,*,#5500,.T.) ;
#8096 = ORIENTED_EDGE('',*,*,#5530,.T.) ;
#8097 = ORIENTED_EDGE('',*,*,#5528,.T.) ;
#8098 = ORIENTED_EDGE('',*,*,#5526,.T.) ;
#8099 = ORIENTED_EDGE('',*,*,#5524,.T.) ;
#8100 = ORIENTED_EDGE('',*,*,#5522,.T.) ;
#8101 = ORIENTED_EDGE('',*,*,#5521,.T.) ;
#8102 = ORIENTED_EDGE('',*,*,#5518,.T.) ;
#8103 = ORIENTED_EDGE('',*,*,#5516,.T.) ;
#8104 = ORIENTED_EDGE('',*,*,#5546,.T.) ;
#8105 = ORIENTED_EDGE('',*,*,#5544,.T.) ;
#8106 = ORIENTED_EDGE('',*,*,#5542,.T.) ;
#8107 = ORIENTED_EDGE('',*,*,#5540,.T.) ;
#8108 = ORIENTED_EDGE('',*,*,#5538,.T.) ;
#8109 = ORIENTED_EDGE('',*,*,#5537,.T.) ;
#8110 = ORIENTED_EDGE('',*,*,#5534,.T.) ;
#8111 = ORIENTED_EDGE('',*,*,#5532,.T.) ;
#8112 = ORIENTED_EDGE('',*,*,#5562,.T.) ;
#8113 = ORIENTED_EDGE('',*,*,#5560,.T.) ;
#8114 = ORIENTED_EDGE('',*,*,#5558,.T.) ;
#8115 = ORIENTED_EDGE('',*,*,#5556,.T.) ;
#8116 = ORIENTED_EDGE('',*,*,#5554,.T.) ;
#8117 = ORIENTED_EDGE('',*,*,#5553,.T.) ;
#8118 = ORIENTED_EDGE('',*,*,#5550,.T.) ;
#8119 = ORIENTED_EDGE('',*,*,#5548,.T.) ;
#8120 = CYLINDRICAL_SURFACE('',#8748,0.300000000000011) ;
#8121 = CYLINDRICAL_SURFACE('',#8749,0.299999999999991) ;
#8122 = CYLINDRICAL_SURFACE('',#8750,3.00000000000003) ;
#8123 = CYLINDRICAL_SURFACE('',#8755,1.2500000000303) ;
#8124 = CYLINDRICAL_SURFACE('',#8757,1.2500000000303) ;
#8125 = CYLINDRICAL_SURFACE('',#8758,1.2500000000303) ;
#8126 = CYLINDRICAL_SURFACE('',#8759,1.2500000000303) ;
#8127 = CYLINDRICAL_SURFACE('',#8760,1.2500000000303) ;
#8128 = CYLINDRICAL_SURFACE('',#8761,1.25000000003033) ;
#8129 = CYLINDRICAL_SURFACE('',#8763,1.25000000003033) ;
#8130 = CYLINDRICAL_SURFACE('',#8764,1.25000000003033) ;
#8131 = CYLINDRICAL_SURFACE('',#8765,1.25000000003033) ;
#8132 = CYLINDRICAL_SURFACE('',#8766,1.25000000003033) ;
#8133 = CYLINDRICAL_SURFACE('',#8767,2.00000000000006) ;
#8134 = CYLINDRICAL_SURFACE('',#8780,1.25000000003033) ;
#8135 = CYLINDRICAL_SURFACE('',#8783,1.2500000000303) ;
#8136 = CYLINDRICAL_SURFACE('',#8784,1.2500000000303) ;
#8137 = CYLINDRICAL_SURFACE('',#8789,1.25000000003033) ;
#8138 = CYLINDRICAL_SURFACE('',#8790,0.300000000000011) ;
#8139 = CYLINDRICAL_SURFACE('',#8791,0.300000000000011) ;
#8140 = CYLINDRICAL_SURFACE('',#8792,0.299999999999991) ;
#8141 = CYLINDRICAL_SURFACE('',#8793,0.299999999999991) ;
#8142 = CYLINDRICAL_SURFACE('',#8794,0.299999999999991) ;
#8143 = CYLINDRICAL_SURFACE('',#8800,0.300000000000007) ;
#8144 = CYLINDRICAL_SURFACE('',#8805,1.21492629244945) ;
#8145 = CYLINDRICAL_SURFACE('',#8807,1.21492629244945) ;
#8146 = CYLINDRICAL_SURFACE('',#8808,1.21492629244945) ;
#8147 = CYLINDRICAL_SURFACE('',#8809,1.21492629244945) ;
#8148 = CYLINDRICAL_SURFACE('',#8810,1.21492629244945) ;
#8149 = CYLINDRICAL_SURFACE('',#8825,1.21492629244947) ;
#8150 = CYLINDRICAL_SURFACE('',#8827,1.21492629244947) ;
#8151 = CYLINDRICAL_SURFACE('',#8828,1.21492629244947) ;
#8152 = CYLINDRICAL_SURFACE('',#8829,1.21492629244947) ;
#8153 = CYLINDRICAL_SURFACE('',#8830,1.21492629244947) ;
#8154 = CYLINDRICAL_SURFACE('',#8845,28.7407375552551) ;
#8155 = CYLINDRICAL_SURFACE('',#8848,15.) ;
#8156 = CYLINDRICAL_SURFACE('',#8851,28.7407375552569) ;
#8157 = CYLINDRICAL_SURFACE('',#8854,10.3432265401782) ;
#8158 = CYLINDRICAL_SURFACE('',#8857,1.00000000000001) ;
#8159 = CYLINDRICAL_SURFACE('',#8876,2.00000000000002) ;
#8160 = CYLINDRICAL_SURFACE('',#8878,2.4999999999999) ;
#8161 = CYLINDRICAL_SURFACE('',#8879,18.0149881946833) ;
#8162 = CYLINDRICAL_SURFACE('',#8881,2.49999999999991) ;
#8163 = CYLINDRICAL_SURFACE('',#8882,23.0149881946373) ;
#8164 = CYLINDRICAL_SURFACE('',#8883,6.99999999999997) ;
#8165 = CYLINDRICAL_SURFACE('',#8885,9.6716132700902) ;
#8166 = CYLINDRICAL_SURFACE('',#8886,1.49999999999984) ;
#8167 = CYLINDRICAL_SURFACE('',#8888,6.67161327010488) ;
#8168 = CYLINDRICAL_SURFACE('',#8890,1.50000000000001) ;
#8169 = CYLINDRICAL_SURFACE('',#8891,28.7407375552557) ;
#8170 = CYLINDRICAL_SURFACE('',#8894,14.9999999999999) ;
#8171 = CYLINDRICAL_SURFACE('',#8897,28.7407375552568) ;
#8172 = CYLINDRICAL_SURFACE('',#8900,10.3432265401782) ;
#8173 = CYLINDRICAL_SURFACE('',#8920,2.) ;
#8174 = CYLINDRICAL_SURFACE('',#8922,2.49999999999952) ;
#8175 = CYLINDRICAL_SURFACE('',#8923,18.014988194682) ;
#8176 = CYLINDRICAL_SURFACE('',#8925,2.49999999999988) ;
#8177 = CYLINDRICAL_SURFACE('',#8926,23.0149881946396) ;
#8178 = CYLINDRICAL_SURFACE('',#8927,6.99999999999998) ;
#8179 = CYLINDRICAL_SURFACE('',#8929,9.67161327008889) ;
#8180 = CYLINDRICAL_SURFACE('',#8930,1.49999999999977) ;
#8181 = CYLINDRICAL_SURFACE('',#8931,6.6716132701054) ;
#8182 = CYLINDRICAL_SURFACE('',#8933,1.50000000000005) ;
#8183 = CYLINDRICAL_SURFACE('',#8934,0.999999999999981) ;
#8184 = CYLINDRICAL_SURFACE('',#8935,2.00000000000003) ;
#8185 = CYLINDRICAL_SURFACE('',#8940,5.99999999999987) ;
#8186 = CYLINDRICAL_SURFACE('',#8944,2.17161327008925) ;
#8187 = CYLINDRICAL_SURFACE('',#8947,2.49999999999937) ;
#8188 = CYLINDRICAL_SURFACE('',#8952,3.50000000000016) ;
#8189 = CYLINDRICAL_SURFACE('',#8956,2.50000000000004) ;
#8190 = CYLINDRICAL_SURFACE('',#8959,5.99999999999939) ;
#8191 = CYLINDRICAL_SURFACE('',#8963,2.49999999999973) ;
#8192 = CYLINDRICAL_SURFACE('',#8972,1.00000000000007) ;
#8193 = CYLINDRICAL_SURFACE('',#8973,2.00000000000001) ;
#8194 = CYLINDRICAL_SURFACE('',#9045,2.49999999999961) ;
#8195 = CYLINDRICAL_SURFACE('',#9048,5.99999999999934) ;
#8196 = CYLINDRICAL_SURFACE('',#9051,2.50000000000003) ;
#8197 = CYLINDRICAL_SURFACE('',#9054,2.17161327008909) ;
#8198 = CYLINDRICAL_SURFACE('',#9057,2.5000000000001) ;
#8199 = CYLINDRICAL_SURFACE('',#9061,5.99999999999993) ;
#8200 = CYLINDRICAL_SURFACE('',#9065,2.5) ;
#8201 = CYLINDRICAL_SURFACE('',#9068,6.00000000000019) ;
#8202 = CYLINDRICAL_SURFACE('',#9071,2.50000000000021) ;
#8203 = CYLINDRICAL_SURFACE('',#9077,2.00000000000001) ;
#8204 = CYLINDRICAL_SURFACE('',#9080,0.999999999999978) ;
#8205 = CYLINDRICAL_SURFACE('',#9085,7.00000000000021) ;
#8206 = CYLINDRICAL_SURFACE('',#9093,13.7469842874597) ;
#8207 = CYLINDRICAL_SURFACE('',#9099,7.00000000000021) ;
#8208 = CYLINDRICAL_SURFACE('',#9100,3.00000000000005) ;
#8209 = CYLINDRICAL_SURFACE('',#9375,17.4999999999914) ;
#8210 = CYLINDRICAL_SURFACE('',#9377,2.49999999999958) ;
#8211 = CYLINDRICAL_SURFACE('',#9380,2.50000000000016) ;
#8212 = CYLINDRICAL_SURFACE('',#9382,78.9146368237) ;
#8213 = CYLINDRICAL_SURFACE('',#9384,2.50000000000029) ;
#8214 = CYLINDRICAL_SURFACE('',#9387,2.50000000000002) ;
#8215 = CYLINDRICAL_SURFACE('',#9389,8.00000000000007) ;
#8216 = CYLINDRICAL_SURFACE('',#9391,17.4999999999863) ;
#8217 = CYLINDRICAL_SURFACE('',#9393,2.50000000000002) ;
#8218 = CYLINDRICAL_SURFACE('',#9396,2.50000000000046) ;
#8219 = CYLINDRICAL_SURFACE('',#9398,78.9146368237003) ;
#8220 = CYLINDRICAL_SURFACE('',#9400,2.50000000000052) ;
#8221 = CYLINDRICAL_SURFACE('',#9403,2.49999999999964) ;
#8222 = CYLINDRICAL_SURFACE('',#9405,17.4999999999883) ;
#8223 = CYLINDRICAL_SURFACE('',#9407,2.49999999999957) ;
#8224 = CYLINDRICAL_SURFACE('',#9410,2.50000000000006) ;
#8225 = CYLINDRICAL_SURFACE('',#9412,78.9146368237002) ;
#8226 = CYLINDRICAL_SURFACE('',#9414,2.50000000000021) ;
#8227 = CYLINDRICAL_SURFACE('',#9417,2.49999999999936) ;
#8228 = CYLINDRICAL_SURFACE('',#9419,17.4999999999923) ;
#8229 = CYLINDRICAL_SURFACE('',#9421,2.49999999999936) ;
#8230 = CYLINDRICAL_SURFACE('',#9424,2.5000000000007) ;
#8231 = CYLINDRICAL_SURFACE('',#9426,78.9146368237008) ;
#8232 = CYLINDRICAL_SURFACE('',#9428,2.50000000000029) ;
#8233 = CYLINDRICAL_SURFACE('',#9431,2.49999999999924) ;
#8234 = CYLINDRICAL_SURFACE('',#9433,17.4999999999921) ;
#8235 = CYLINDRICAL_SURFACE('',#9435,2.49999999999967) ;
#8236 = CYLINDRICAL_SURFACE('',#9438,2.50000000000017) ;
#8237 = CYLINDRICAL_SURFACE('',#9440,78.9146368237003) ;
#8238 = CYLINDRICAL_SURFACE('',#9442,2.49999999999996) ;
#8239 = CYLINDRICAL_SURFACE('',#9445,2.499999999999) ;
#8240 = CYLINDRICAL_SURFACE('',#9447,83.3146368237019) ;
#8241 = CYLINDRICAL_SURFACE('',#9449,81.1146368237021) ;
#8242 = ADVANCED_FACE('',(#859),#8120,.F.) ;
#8243 = ADVANCED_FACE('',(#860),#8121,.F.) ;
#8244 = ADVANCED_FACE('',(#861),#811,.T.) ;
#8245 = ADVANCED_FACE('',(#862),#812,.T.) ;
#8246 = ADVANCED_FACE('',(#863),#813,.T.) ;
#8247 = ADVANCED_FACE('',(#864),#814,.T.) ;
#8248 = ADVANCED_FACE('',(#865,#554,#555,#556,#557),#8122,.T.) ;
#8249 = ADVANCED_FACE('',(#866),#357,.T.) ;
#8250 = ADVANCED_FACE('',(#867),#358,.T.) ;
#8251 = ADVANCED_FACE('',(#868),#815,.T.) ;
#8252 = ADVANCED_FACE('',(#869),#816,.T.) ;
#8253 = ADVANCED_FACE('',(#870),#8123,.F.) ;
#8254 = ADVANCED_FACE('',(#871),#8124,.F.) ;
#8255 = ADVANCED_FACE('',(#872),#8125,.F.) ;
#8256 = ADVANCED_FACE('',(#873),#8126,.F.) ;
#8257 = ADVANCED_FACE('',(#874),#8127,.F.) ;
#8258 = ADVANCED_FACE('',(#875),#8128,.F.) ;
#8259 = ADVANCED_FACE('',(#876),#8129,.F.) ;
#8260 = ADVANCED_FACE('',(#877),#8130,.F.) ;
#8261 = ADVANCED_FACE('',(#878),#8131,.F.) ;
#8262 = ADVANCED_FACE('',(#879),#8132,.F.) ;
#8263 = ADVANCED_FACE('',(#880,#558,#559,#560,#561),#8133,.T.) ;
#8264 = ADVANCED_FACE('',(#881,#562),#359,.T.) ;
#8265 = ADVANCED_FACE('',(#882,#563),#360,.T.) ;
#8266 = ADVANCED_FACE('',(#883),#817,.T.) ;
#8267 = ADVANCED_FACE('',(#884),#818,.T.) ;
#8268 = ADVANCED_FACE('',(#885),#311,.F.) ;
#8269 = ADVANCED_FACE('',(#886),#312,.F.) ;
#8270 = ADVANCED_FACE('',(#887),#819,.T.) ;
#8271 = ADVANCED_FACE('',(#888),#820,.T.) ;
#8272 = ADVANCED_FACE('',(#889),#361,.T.) ;
#8273 = ADVANCED_FACE('',(#890),#8134,.F.) ;
#8274 = ADVANCED_FACE('',(#891),#821,.T.) ;
#8275 = ADVANCED_FACE('',(#892),#362,.T.) ;
#8276 = ADVANCED_FACE('',(#893),#8135,.F.) ;
#8277 = ADVANCED_FACE('',(#894),#8136,.F.) ;
#8278 = ADVANCED_FACE('',(#895),#822,.T.) ;
#8279 = ADVANCED_FACE('',(#896),#823,.T.) ;
#8280 = ADVANCED_FACE('',(#897),#824,.T.) ;
#8281 = ADVANCED_FACE('',(#898),#363,.T.) ;
#8282 = ADVANCED_FACE('',(#899),#364,.T.) ;
#8283 = ADVANCED_FACE('',(#900),#825,.T.) ;
#8284 = ADVANCED_FACE('',(#901),#8137,.F.) ;
#8285 = ADVANCED_FACE('',(#902),#826,.T.) ;
#8286 = ADVANCED_FACE('',(#903),#8138,.F.) ;
#8287 = ADVANCED_FACE('',(#904),#827,.T.) ;
#8288 = ADVANCED_FACE('',(#905),#8139,.F.) ;
#8289 = ADVANCED_FACE('',(#906),#828,.T.) ;
#8290 = ADVANCED_FACE('',(#907),#8140,.F.) ;
#8291 = ADVANCED_FACE('',(#908),#8141,.F.) ;
#8292 = ADVANCED_FACE('',(#909),#829,.T.) ;
#8293 = ADVANCED_FACE('',(#910),#830,.T.) ;
#8294 = ADVANCED_FACE('',(#911),#8142,.T.) ;
#8295 = ADVANCED_FACE('',(#912),#365,.T.) ;
#8296 = ADVANCED_FACE('',(#913),#366,.T.) ;
#8297 = ADVANCED_FACE('',(#914),#831,.T.) ;
#8298 = ADVANCED_FACE('',(#915),#8143,.T.) ;
#8299 = ADVANCED_FACE('',(#916),#367,.T.) ;
#8300 = ADVANCED_FACE('',(#917),#368,.T.) ;
#8301 = ADVANCED_FACE('',(#918),#8144,.T.) ;
#8302 = ADVANCED_FACE('',(#919),#8145,.T.) ;
#8303 = ADVANCED_FACE('',(#920),#8146,.T.) ;
#8304 = ADVANCED_FACE('',(#921),#8147,.T.) ;
#8305 = ADVANCED_FACE('',(#922),#8148,.T.) ;
#8306 = ADVANCED_FACE('',(#923),#313,.F.) ;
#8307 = ADVANCED_FACE('',(#924),#314,.T.) ;
#8308 = ADVANCED_FACE('',(#925),#832,.T.) ;
#8309 = ADVANCED_FACE('',(#926),#833,.T.) ;
#8310 = ADVANCED_FACE('',(#927),#315,.T.) ;
#8311 = ADVANCED_FACE('',(#928,#564),#369,.T.) ;
#8312 = ADVANCED_FACE('',(#929),#370,.T.) ;
#8313 = ADVANCED_FACE('',(#930),#371,.T.) ;
#8314 = ADVANCED_FACE('',(#931),#372,.T.) ;
#8315 = ADVANCED_FACE('',(#932),#373,.T.) ;
#8316 = ADVANCED_FACE('',(#933),#374,.T.) ;
#8317 = ADVANCED_FACE('',(#934),#375,.T.) ;
#8318 = ADVANCED_FACE('',(#935),#376,.T.) ;
#8319 = ADVANCED_FACE('',(#936),#8149,.T.) ;
#8320 = ADVANCED_FACE('',(#937),#8150,.T.) ;
#8321 = ADVANCED_FACE('',(#938),#8151,.T.) ;
#8322 = ADVANCED_FACE('',(#939),#8152,.T.) ;
#8323 = ADVANCED_FACE('',(#940),#8153,.T.) ;
#8324 = ADVANCED_FACE('',(#941),#316,.F.) ;
#8325 = ADVANCED_FACE('',(#942),#317,.T.) ;
#8326 = ADVANCED_FACE('',(#943),#834,.T.) ;
#8327 = ADVANCED_FACE('',(#944),#835,.T.) ;
#8328 = ADVANCED_FACE('',(#945),#318,.T.) ;
#8329 = ADVANCED_FACE('',(#946,#565),#377,.T.) ;
#8330 = ADVANCED_FACE('',(#947),#378,.T.) ;
#8331 = ADVANCED_FACE('',(#948),#379,.T.) ;
#8332 = ADVANCED_FACE('',(#949),#380,.T.) ;
#8333 = ADVANCED_FACE('',(#950),#381,.T.) ;
#8334 = ADVANCED_FACE('',(#951),#382,.T.) ;
#8335 = ADVANCED_FACE('',(#952),#383,.T.) ;
#8336 = ADVANCED_FACE('',(#953),#384,.T.) ;
#8337 = ADVANCED_FACE('',(#954),#8154,.F.) ;
#8338 = ADVANCED_FACE('',(#955),#8155,.T.) ;
#8339 = ADVANCED_FACE('',(#956),#8156,.F.) ;
#8340 = ADVANCED_FACE('',(#957),#8157,.T.) ;
#8341 = ADVANCED_FACE('',(#958),#8158,.F.) ;
#8342 = ADVANCED_FACE('',(#959,#566,#567,#568,#569,#570),#385,.T.) ;
#8343 = ADVANCED_FACE('',(#960,#571,#572,#573,#574,#575),#386,.T.) ;
#8344 = ADVANCED_FACE('',(#961),#8159,.F.) ;
#8345 = ADVANCED_FACE('',(#962),#8160,.F.) ;
#8346 = ADVANCED_FACE('',(#963),#8161,.T.) ;
#8347 = ADVANCED_FACE('',(#964),#8162,.F.) ;
#8348 = ADVANCED_FACE('',(#965),#8163,.F.) ;
#8349 = ADVANCED_FACE('',(#966),#8164,.F.) ;
#8350 = ADVANCED_FACE('',(#967),#8165,.F.) ;
#8351 = ADVANCED_FACE('',(#968),#8166,.F.) ;
#8352 = ADVANCED_FACE('',(#969),#8167,.T.) ;
#8353 = ADVANCED_FACE('',(#970),#8168,.F.) ;
#8354 = ADVANCED_FACE('',(#971),#836,.T.) ;
#8355 = ADVANCED_FACE('',(#972),#837,.T.) ;
#8356 = ADVANCED_FACE('',(#973),#838,.T.) ;
#8357 = ADVANCED_FACE('',(#974),#839,.T.) ;
#8358 = ADVANCED_FACE('',(#975),#840,.T.) ;
#8359 = ADVANCED_FACE('',(#976),#841,.T.) ;
#8360 = ADVANCED_FACE('',(#977),#842,.T.) ;
#8361 = ADVANCED_FACE('',(#978),#843,.T.) ;
#8362 = ADVANCED_FACE('',(#979),#844,.T.) ;
#8363 = ADVANCED_FACE('',(#980),#845,.T.) ;
#8364 = ADVANCED_FACE('',(#981),#8169,.F.) ;
#8365 = ADVANCED_FACE('',(#982),#8170,.T.) ;
#8366 = ADVANCED_FACE('',(#983),#8171,.F.) ;
#8367 = ADVANCED_FACE('',(#984),#8172,.T.) ;
#8368 = ADVANCED_FACE('',(#985,#576,#577,#578,#579,#580),#387,.T.) ;
#8369 = ADVANCED_FACE('',(#986,#581,#582,#583,#584,#585),#388,.T.) ;
#8370 = ADVANCED_FACE('',(#987),#8173,.F.) ;
#8371 = ADVANCED_FACE('',(#988),#8174,.F.) ;
#8372 = ADVANCED_FACE('',(#989),#8175,.T.) ;
#8373 = ADVANCED_FACE('',(#990),#8176,.F.) ;
#8374 = ADVANCED_FACE('',(#991),#8177,.F.) ;
#8375 = ADVANCED_FACE('',(#992),#8178,.F.) ;
#8376 = ADVANCED_FACE('',(#993),#8179,.F.) ;
#8377 = ADVANCED_FACE('',(#994),#8180,.F.) ;
#8378 = ADVANCED_FACE('',(#995),#8181,.T.) ;
#8379 = ADVANCED_FACE('',(#996),#8182,.F.) ;
#8380 = ADVANCED_FACE('',(#997),#8183,.F.) ;
#8381 = ADVANCED_FACE('',(#998),#846,.T.) ;
#8382 = ADVANCED_FACE('',(#999),#847,.T.) ;
#8383 = ADVANCED_FACE('',(#1000),#848,.T.) ;
#8384 = ADVANCED_FACE('',(#1001),#849,.T.) ;
#8385 = ADVANCED_FACE('',(#1002),#850,.T.) ;
#8386 = ADVANCED_FACE('',(#1003),#851,.T.) ;
#8387 = ADVANCED_FACE('',(#1004),#852,.T.) ;
#8388 = ADVANCED_FACE('',(#1005),#853,.T.) ;
#8389 = ADVANCED_FACE('',(#1006),#854,.T.) ;
#8390 = ADVANCED_FACE('',(#1007),#855,.T.) ;
#8391 = ADVANCED_FACE('',(#1008),#856,.T.) ;
#8392 = ADVANCED_FACE('',(#1009),#8184,.T.) ;
#8393 = ADVANCED_FACE('',(#1010),#389,.T.) ;
#8394 = ADVANCED_FACE('',(#1011),#390,.T.) ;
#8395 = ADVANCED_FACE('',(#1012),#857,.T.) ;
#8396 = ADVANCED_FACE('',(#1013),#858,.T.) ;
#8397 = ADVANCED_FACE('',(#1014),#8185,.T.) ;
#8398 = ADVANCED_FACE('',(#1015),#391,.T.) ;
#8399 = ADVANCED_FACE('',(#1016),#8186,.T.) ;
#8400 = ADVANCED_FACE('',(#1017),#8187,.F.) ;
#8401 = ADVANCED_FACE('',(#1018),#392,.T.) ;
#8402 = ADVANCED_FACE('',(#1019),#393,.T.) ;
#8403 = ADVANCED_FACE('',(#1020),#8188,.T.) ;
#8404 = ADVANCED_FACE('',(#1021),#394,.T.) ;
#8405 = ADVANCED_FACE('',(#1022),#8189,.F.) ;
#8406 = ADVANCED_FACE('',(#1023),#8190,.T.) ;
#8407 = ADVANCED_FACE('',(#1024),#395,.T.) ;
#8408 = ADVANCED_FACE('',(#1025),#8191,.F.) ;
#8409 = ADVANCED_FACE('',(#1026,#586,#587),#396,.T.) ;
#8410 = ADVANCED_FACE('',(#1027,#588,#589),#397,.T.) ;
#8411 = ADVANCED_FACE('',(#1028),#8192,.F.) ;
#8412 = ADVANCED_FACE('',(#1029),#8193,.F.) ;
#8413 = ADVANCED_FACE('',(#1030),#398,.T.) ;
#8414 = ADVANCED_FACE('',(#1031),#33,.T.) ;
#8415 = ADVANCED_FACE('',(#1032),#34,.F.) ;
#8416 = ADVANCED_FACE('',(#1033),#35,.T.) ;
#8417 = ADVANCED_FACE('',(#1034),#36,.F.) ;
#8418 = ADVANCED_FACE('',(#1035),#37,.T.) ;
#8419 = ADVANCED_FACE('',(#1036),#399,.T.) ;
#8420 = ADVANCED_FACE('',(#1037),#38,.T.) ;
#8421 = ADVANCED_FACE('',(#1038),#39,.T.) ;
#8422 = ADVANCED_FACE('',(#1039),#40,.T.) ;
#8423 = ADVANCED_FACE('',(#1040),#41,.T.) ;
#8424 = ADVANCED_FACE('',(#1041),#42,.T.) ;
#8425 = ADVANCED_FACE('',(#1042),#400,.T.) ;
#8426 = ADVANCED_FACE('',(#1043),#43,.T.) ;
#8427 = ADVANCED_FACE('',(#1044),#44,.T.) ;
#8428 = ADVANCED_FACE('',(#1045),#45,.T.) ;
#8429 = ADVANCED_FACE('',(#1046),#46,.T.) ;
#8430 = ADVANCED_FACE('',(#1047),#401,.T.) ;
#8431 = ADVANCED_FACE('',(#1048),#47,.T.) ;
#8432 = ADVANCED_FACE('',(#1049),#48,.T.) ;
#8433 = ADVANCED_FACE('',(#1050),#49,.T.) ;
#8434 = ADVANCED_FACE('',(#1051),#50,.T.) ;
#8435 = ADVANCED_FACE('',(#1052),#402,.T.) ;
#8436 = ADVANCED_FACE('',(#1053),#403,.T.) ;
#8437 = ADVANCED_FACE('',(#1054),#404,.T.) ;
#8438 = ADVANCED_FACE('',(#1055),#51,.T.) ;
#8439 = ADVANCED_FACE('',(#1056),#52,.T.) ;
#8440 = ADVANCED_FACE('',(#1057),#53,.T.) ;
#8441 = ADVANCED_FACE('',(#1058),#54,.T.) ;
#8442 = ADVANCED_FACE('',(#1059),#55,.T.) ;
#8443 = ADVANCED_FACE('',(#1060),#405,.T.) ;
#8444 = ADVANCED_FACE('',(#1061),#56,.T.) ;
#8445 = ADVANCED_FACE('',(#1062),#57,.F.) ;
#8446 = ADVANCED_FACE('',(#1063),#58,.T.) ;
#8447 = ADVANCED_FACE('',(#1064),#59,.F.) ;
#8448 = ADVANCED_FACE('',(#1065),#60,.T.) ;
#8449 = ADVANCED_FACE('',(#1066),#406,.T.) ;
#8450 = ADVANCED_FACE('',(#1067),#61,.T.) ;
#8451 = ADVANCED_FACE('',(#1068),#62,.T.) ;
#8452 = ADVANCED_FACE('',(#1069),#63,.T.) ;
#8453 = ADVANCED_FACE('',(#1070),#64,.T.) ;
#8454 = ADVANCED_FACE('',(#1071),#407,.T.) ;
#8455 = ADVANCED_FACE('',(#1072),#65,.T.) ;
#8456 = ADVANCED_FACE('',(#1073),#66,.T.) ;
#8457 = ADVANCED_FACE('',(#1074),#67,.T.) ;
#8458 = ADVANCED_FACE('',(#1075),#68,.T.) ;
#8459 = ADVANCED_FACE('',(#1076),#408,.T.) ;
#8460 = ADVANCED_FACE('',(#1077),#409,.T.) ;
#8461 = ADVANCED_FACE('',(#1078),#410,.T.) ;
#8462 = ADVANCED_FACE('',(#1079),#69,.T.) ;
#8463 = ADVANCED_FACE('',(#1080),#8194,.F.) ;
#8464 = ADVANCED_FACE('',(#1081),#8195,.T.) ;
#8465 = ADVANCED_FACE('',(#1082),#8196,.F.) ;
#8466 = ADVANCED_FACE('',(#1083),#8197,.T.) ;
#8467 = ADVANCED_FACE('',(#1084),#8198,.F.) ;
#8468 = ADVANCED_FACE('',(#1085),#411,.T.) ;
#8469 = ADVANCED_FACE('',(#1086),#8199,.T.) ;
#8470 = ADVANCED_FACE('',(#1087),#412,.T.) ;
#8471 = ADVANCED_FACE('',(#1088),#8200,.F.) ;
#8472 = ADVANCED_FACE('',(#1089),#8201,.T.) ;
#8473 = ADVANCED_FACE('',(#1090),#8202,.F.) ;
#8474 = ADVANCED_FACE('',(#1091),#70,.T.) ;
#8475 = ADVANCED_FACE('',(#1092),#413,.T.) ;
#8476 = ADVANCED_FACE('',(#1093),#8203,.F.) ;
#8477 = ADVANCED_FACE('',(#1094),#8204,.F.) ;
#8478 = ADVANCED_FACE('',(#1095,#590,#591),#414,.T.) ;
#8479 = ADVANCED_FACE('',(#1096,#592,#593),#415,.T.) ;
#8480 = ADVANCED_FACE('',(#1097),#8205,.T.) ;
#8481 = ADVANCED_FACE('',(#1098,#594),#416,.T.) ;
#8482 = ADVANCED_FACE('',(#1099,#595),#417,.T.) ;
#8483 = ADVANCED_FACE('',(#1100),#8206,.T.) ;
#8484 = ADVANCED_FACE('',(#1101,#596),#418,.T.) ;
#8485 = ADVANCED_FACE('',(#1102,#597),#419,.T.) ;
#8486 = ADVANCED_FACE('',(#1103),#8207,.T.) ;
#8487 = ADVANCED_FACE('',(#1104),#8208,.F.) ;
#8488 = ADVANCED_FACE('',(#1105),#420,.T.) ;
#8489 = ADVANCED_FACE('',(#1106),#71,.T.) ;
#8490 = ADVANCED_FACE('',(#1107),#421,.T.) ;
#8491 = ADVANCED_FACE('',(#1108),#422,.T.) ;
#8492 = ADVANCED_FACE('',(#1109),#72,.T.) ;
#8493 = ADVANCED_FACE('',(#1110),#423,.T.) ;
#8494 = ADVANCED_FACE('',(#1111),#424,.T.) ;
#8495 = ADVANCED_FACE('',(#1112),#73,.T.) ;
#8496 = ADVANCED_FACE('',(#1113),#425,.T.) ;
#8497 = ADVANCED_FACE('',(#1114),#426,.T.) ;
#8498 = ADVANCED_FACE('',(#1115),#74,.T.) ;
#8499 = ADVANCED_FACE('',(#1116),#427,.T.) ;
#8500 = ADVANCED_FACE('',(#1117),#428,.T.) ;
#8501 = ADVANCED_FACE('',(#1118),#75,.T.) ;
#8502 = ADVANCED_FACE('',(#1119),#429,.T.) ;
#8503 = ADVANCED_FACE('',(#1120),#430,.T.) ;
#8504 = ADVANCED_FACE('',(#1121),#76,.T.) ;
#8505 = ADVANCED_FACE('',(#1122),#431,.T.) ;
#8506 = ADVANCED_FACE('',(#1123),#432,.T.) ;
#8507 = ADVANCED_FACE('',(#1124),#77,.T.) ;
#8508 = ADVANCED_FACE('',(#1125),#433,.T.) ;
#8509 = ADVANCED_FACE('',(#1126),#434,.T.) ;
#8510 = ADVANCED_FACE('',(#1127),#78,.T.) ;
#8511 = ADVANCED_FACE('',(#1128),#435,.T.) ;
#8512 = ADVANCED_FACE('',(#1129),#436,.T.) ;
#8513 = ADVANCED_FACE('',(#1130),#79,.T.) ;
#8514 = ADVANCED_FACE('',(#1131),#437,.T.) ;
#8515 = ADVANCED_FACE('',(#1132),#438,.T.) ;
#8516 = ADVANCED_FACE('',(#1133),#80,.T.) ;
#8517 = ADVANCED_FACE('',(#1134),#439,.T.) ;
#8518 = ADVANCED_FACE('',(#1135),#440,.T.) ;
#8519 = ADVANCED_FACE('',(#1136),#81,.T.) ;
#8520 = ADVANCED_FACE('',(#1137),#441,.T.) ;
#8521 = ADVANCED_FACE('',(#1138),#442,.T.) ;
#8522 = ADVANCED_FACE('',(#1139),#82,.T.) ;
#8523 = ADVANCED_FACE('',(#1140),#443,.T.) ;
#8524 = ADVANCED_FACE('',(#1141),#444,.T.) ;
#8525 = ADVANCED_FACE('',(#1142),#83,.T.) ;
#8526 = ADVANCED_FACE('',(#1143),#445,.T.) ;
#8527 = ADVANCED_FACE('',(#1144),#446,.T.) ;
#8528 = ADVANCED_FACE('',(#1145),#84,.T.) ;
#8529 = ADVANCED_FACE('',(#1146),#447,.T.) ;
#8530 = ADVANCED_FACE('',(#1147),#448,.T.) ;
#8531 = ADVANCED_FACE('',(#1148),#85,.T.) ;
#8532 = ADVANCED_FACE('',(#1149),#449,.T.) ;
#8533 = ADVANCED_FACE('',(#1150),#450,.T.) ;
#8534 = ADVANCED_FACE('',(#1151),#86,.T.) ;
#8535 = ADVANCED_FACE('',(#1152),#451,.T.) ;
#8536 = ADVANCED_FACE('',(#1153),#452,.T.) ;
#8537 = ADVANCED_FACE('',(#1154),#87,.T.) ;
#8538 = ADVANCED_FACE('',(#1155),#453,.T.) ;
#8539 = ADVANCED_FACE('',(#1156),#454,.T.) ;
#8540 = ADVANCED_FACE('',(#1157),#88,.T.) ;
#8541 = ADVANCED_FACE('',(#1158),#455,.T.) ;
#8542 = ADVANCED_FACE('',(#1159),#456,.T.) ;
#8543 = ADVANCED_FACE('',(#1160),#89,.T.) ;
#8544 = ADVANCED_FACE('',(#1161),#457,.T.) ;
#8545 = ADVANCED_FACE('',(#1162),#458,.T.) ;
#8546 = ADVANCED_FACE('',(#1163),#90,.T.) ;
#8547 = ADVANCED_FACE('',(#1164),#459,.T.) ;
#8548 = ADVANCED_FACE('',(#1165),#460,.T.) ;
#8549 = ADVANCED_FACE('',(#1166),#91,.T.) ;
#8550 = ADVANCED_FACE('',(#1167),#461,.T.) ;
#8551 = ADVANCED_FACE('',(#1168),#462,.T.) ;
#8552 = ADVANCED_FACE('',(#1169),#92,.T.) ;
#8553 = ADVANCED_FACE('',(#1170),#463,.T.) ;
#8554 = ADVANCED_FACE('',(#1171),#464,.T.) ;
#8555 = ADVANCED_FACE('',(#1172),#93,.T.) ;
#8556 = ADVANCED_FACE('',(#1173),#465,.T.) ;
#8557 = ADVANCED_FACE('',(#1174),#466,.T.) ;
#8558 = ADVANCED_FACE('',(#1175),#94,.T.) ;
#8559 = ADVANCED_FACE('',(#1176),#467,.T.) ;
#8560 = ADVANCED_FACE('',(#1177),#468,.T.) ;
#8561 = ADVANCED_FACE('',(#1178),#95,.T.) ;
#8562 = ADVANCED_FACE('',(#1179),#469,.T.) ;
#8563 = ADVANCED_FACE('',(#1180),#470,.T.) ;
#8564 = ADVANCED_FACE('',(#1181),#96,.T.) ;
#8565 = ADVANCED_FACE('',(#1182),#471,.T.) ;
#8566 = ADVANCED_FACE('',(#1183),#472,.T.) ;
#8567 = ADVANCED_FACE('',(#1184),#97,.T.) ;
#8568 = ADVANCED_FACE('',(#1185),#473,.T.) ;
#8569 = ADVANCED_FACE('',(#1186),#474,.T.) ;
#8570 = ADVANCED_FACE('',(#1187),#98,.T.) ;
#8571 = ADVANCED_FACE('',(#1188),#475,.T.) ;
#8572 = ADVANCED_FACE('',(#1189),#476,.T.) ;
#8573 = ADVANCED_FACE('',(#1190),#99,.T.) ;
#8574 = ADVANCED_FACE('',(#1191),#477,.T.) ;
#8575 = ADVANCED_FACE('',(#1192),#478,.T.) ;
#8576 = ADVANCED_FACE('',(#1193),#100,.T.) ;
#8577 = ADVANCED_FACE('',(#1194),#479,.T.) ;
#8578 = ADVANCED_FACE('',(#1195),#480,.T.) ;
#8579 = ADVANCED_FACE('',(#1196),#101,.T.) ;
#8580 = ADVANCED_FACE('',(#1197),#481,.T.) ;
#8581 = ADVANCED_FACE('',(#1198),#482,.T.) ;
#8582 = ADVANCED_FACE('',(#1199),#102,.T.) ;
#8583 = ADVANCED_FACE('',(#1200),#483,.T.) ;
#8584 = ADVANCED_FACE('',(#1201),#484,.T.) ;
#8585 = ADVANCED_FACE('',(#1202),#103,.T.) ;
#8586 = ADVANCED_FACE('',(#1203),#485,.T.) ;
#8587 = ADVANCED_FACE('',(#1204),#486,.T.) ;
#8588 = ADVANCED_FACE('',(#1205),#104,.T.) ;
#8589 = ADVANCED_FACE('',(#1206),#487,.T.) ;
#8590 = ADVANCED_FACE('',(#1207),#488,.T.) ;
#8591 = ADVANCED_FACE('',(#1208),#105,.T.) ;
#8592 = ADVANCED_FACE('',(#1209),#489,.T.) ;
#8593 = ADVANCED_FACE('',(#1210),#490,.T.) ;
#8594 = ADVANCED_FACE('',(#1211),#106,.T.) ;
#8595 = ADVANCED_FACE('',(#1212),#491,.T.) ;
#8596 = ADVANCED_FACE('',(#1213),#492,.T.) ;
#8597 = ADVANCED_FACE('',(#1214),#107,.T.) ;
#8598 = ADVANCED_FACE('',(#1215),#493,.T.) ;
#8599 = ADVANCED_FACE('',(#1216),#494,.T.) ;
#8600 = ADVANCED_FACE('',(#1217),#108,.T.) ;
#8601 = ADVANCED_FACE('',(#1218),#495,.T.) ;
#8602 = ADVANCED_FACE('',(#1219),#496,.T.) ;
#8603 = ADVANCED_FACE('',(#1220),#109,.T.) ;
#8604 = ADVANCED_FACE('',(#1221),#497,.T.) ;
#8605 = ADVANCED_FACE('',(#1222),#498,.T.) ;
#8606 = ADVANCED_FACE('',(#1223),#110,.T.) ;
#8607 = ADVANCED_FACE('',(#1224),#499,.T.) ;
#8608 = ADVANCED_FACE('',(#1225),#500,.T.) ;
#8609 = ADVANCED_FACE('',(#1226),#111,.T.) ;
#8610 = ADVANCED_FACE('',(#1227),#501,.T.) ;
#8611 = ADVANCED_FACE('',(#1228),#502,.T.) ;
#8612 = ADVANCED_FACE('',(#1229),#112,.T.) ;
#8613 = ADVANCED_FACE('',(#1230),#503,.T.) ;
#8614 = ADVANCED_FACE('',(#1231),#504,.T.) ;
#8615 = ADVANCED_FACE('',(#1232),#113,.T.) ;
#8616 = ADVANCED_FACE('',(#1233),#505,.T.) ;
#8617 = ADVANCED_FACE('',(#1234),#506,.T.) ;
#8618 = ADVANCED_FACE('',(#1235),#114,.T.) ;
#8619 = ADVANCED_FACE('',(#1236),#507,.T.) ;
#8620 = ADVANCED_FACE('',(#1237),#508,.T.) ;
#8621 = ADVANCED_FACE('',(#1238),#115,.T.) ;
#8622 = ADVANCED_FACE('',(#1239),#509,.T.) ;
#8623 = ADVANCED_FACE('',(#1240),#510,.T.) ;
#8624 = ADVANCED_FACE('',(#1241),#116,.T.) ;
#8625 = ADVANCED_FACE('',(#1242),#511,.T.) ;
#8626 = ADVANCED_FACE('',(#1243),#512,.T.) ;
#8627 = ADVANCED_FACE('',(#1244),#117,.T.) ;
#8628 = ADVANCED_FACE('',(#1245),#513,.T.) ;
#8629 = ADVANCED_FACE('',(#1246),#514,.T.) ;
#8630 = ADVANCED_FACE('',(#1247),#118,.T.) ;
#8631 = ADVANCED_FACE('',(#1248),#515,.T.) ;
#8632 = ADVANCED_FACE('',(#1249),#516,.T.) ;
#8633 = ADVANCED_FACE('',(#1250),#119,.T.) ;
#8634 = ADVANCED_FACE('',(#1251),#517,.T.) ;
#8635 = ADVANCED_FACE('',(#1252),#518,.T.) ;
#8636 = ADVANCED_FACE('',(#1253),#120,.T.) ;
#8637 = ADVANCED_FACE('',(#1254),#519,.T.) ;
#8638 = ADVANCED_FACE('',(#1255),#520,.T.) ;
#8639 = ADVANCED_FACE('',(#1256),#121,.T.) ;
#8640 = ADVANCED_FACE('',(#1257),#521,.T.) ;
#8641 = ADVANCED_FACE('',(#1258),#522,.T.) ;
#8642 = ADVANCED_FACE('',(#1259),#122,.T.) ;
#8643 = ADVANCED_FACE('',(#1260),#523,.T.) ;
#8644 = ADVANCED_FACE('',(#1261),#524,.T.) ;
#8645 = ADVANCED_FACE('',(#1262),#123,.T.) ;
#8646 = ADVANCED_FACE('',(#1263),#525,.T.) ;
#8647 = ADVANCED_FACE('',(#1264),#526,.T.) ;
#8648 = ADVANCED_FACE('',(#1265),#124,.T.) ;
#8649 = ADVANCED_FACE('',(#1266),#527,.T.) ;
#8650 = ADVANCED_FACE('',(#1267),#528,.T.) ;
#8651 = ADVANCED_FACE('',(#1268),#125,.T.) ;
#8652 = ADVANCED_FACE('',(#1269),#529,.T.) ;
#8653 = ADVANCED_FACE('',(#1270),#530,.T.) ;
#8654 = ADVANCED_FACE('',(#1271),#126,.T.) ;
#8655 = ADVANCED_FACE('',(#1272),#531,.T.) ;
#8656 = ADVANCED_FACE('',(#1273),#532,.T.) ;
#8657 = ADVANCED_FACE('',(#1274),#127,.T.) ;
#8658 = ADVANCED_FACE('',(#1275),#533,.T.) ;
#8659 = ADVANCED_FACE('',(#1276),#534,.T.) ;
#8660 = ADVANCED_FACE('',(#1277),#128,.T.) ;
#8661 = ADVANCED_FACE('',(#1278),#535,.T.) ;
#8662 = ADVANCED_FACE('',(#1279),#536,.T.) ;
#8663 = ADVANCED_FACE('',(#1280),#129,.T.) ;
#8664 = ADVANCED_FACE('',(#1281),#537,.T.) ;
#8665 = ADVANCED_FACE('',(#1282),#538,.T.) ;
#8666 = ADVANCED_FACE('',(#1283),#130,.T.) ;
#8667 = ADVANCED_FACE('',(#1284),#539,.T.) ;
#8668 = ADVANCED_FACE('',(#1285,#598,#599,#600,#601,#602,#603),#540,.T.) ;
#8669 = ADVANCED_FACE('',(#1286,#604),#541,.T.) ;
#8670 = ADVANCED_FACE('',(#1287),#8209,.T.) ;
#8671 = ADVANCED_FACE('',(#1288),#8210,.F.) ;
#8672 = ADVANCED_FACE('',(#1289),#542,.T.) ;
#8673 = ADVANCED_FACE('',(#1290),#8211,.F.) ;
#8674 = ADVANCED_FACE('',(#1291),#8212,.F.) ;
#8675 = ADVANCED_FACE('',(#1292),#8213,.F.) ;
#8676 = ADVANCED_FACE('',(#1293),#543,.T.) ;
#8677 = ADVANCED_FACE('',(#1294),#8214,.F.) ;
#8678 = ADVANCED_FACE('',(#1295),#8215,.F.) ;
#8679 = ADVANCED_FACE('',(#1296),#8216,.T.) ;
#8680 = ADVANCED_FACE('',(#1297),#8217,.F.) ;
#8681 = ADVANCED_FACE('',(#1298),#544,.T.) ;
#8682 = ADVANCED_FACE('',(#1299),#8218,.F.) ;
#8683 = ADVANCED_FACE('',(#1300),#8219,.F.) ;
#8684 = ADVANCED_FACE('',(#1301),#8220,.F.) ;
#8685 = ADVANCED_FACE('',(#1302),#545,.T.) ;
#8686 = ADVANCED_FACE('',(#1303),#8221,.F.) ;
#8687 = ADVANCED_FACE('',(#1304),#8222,.T.) ;
#8688 = ADVANCED_FACE('',(#1305),#8223,.F.) ;
#8689 = ADVANCED_FACE('',(#1306),#546,.T.) ;
#8690 = ADVANCED_FACE('',(#1307),#8224,.F.) ;
#8691 = ADVANCED_FACE('',(#1308),#8225,.F.) ;
#8692 = ADVANCED_FACE('',(#1309),#8226,.F.) ;
#8693 = ADVANCED_FACE('',(#1310),#547,.T.) ;
#8694 = ADVANCED_FACE('',(#1311),#8227,.F.) ;
#8695 = ADVANCED_FACE('',(#1312),#8228,.T.) ;
#8696 = ADVANCED_FACE('',(#1313),#8229,.F.) ;
#8697 = ADVANCED_FACE('',(#1314),#548,.T.) ;
#8698 = ADVANCED_FACE('',(#1315),#8230,.F.) ;
#8699 = ADVANCED_FACE('',(#1316),#8231,.F.) ;
#8700 = ADVANCED_FACE('',(#1317),#8232,.F.) ;
#8701 = ADVANCED_FACE('',(#1318),#549,.T.) ;
#8702 = ADVANCED_FACE('',(#1319),#8233,.F.) ;
#8703 = ADVANCED_FACE('',(#1320),#8234,.T.) ;
#8704 = ADVANCED_FACE('',(#1321),#8235,.F.) ;
#8705 = ADVANCED_FACE('',(#1322),#550,.T.) ;
#8706 = ADVANCED_FACE('',(#1323),#8236,.F.) ;
#8707 = ADVANCED_FACE('',(#1324),#8237,.F.) ;
#8708 = ADVANCED_FACE('',(#1325),#8238,.F.) ;
#8709 = ADVANCED_FACE('',(#1326),#551,.T.) ;
#8710 = ADVANCED_FACE('',(#1327),#8239,.F.) ;
#8711 = ADVANCED_FACE('',(#1328),#8240,.F.) ;
#8712 = ADVANCED_FACE('',(#1329),#8241,.T.) ;
#8713 = ADVANCED_FACE('',(#1330,#605),#552,.T.) ;
#8714 = ADVANCED_FACE('',(#1331,#606,#607,#608,#609,#610,#611),#553,.T.) ;
#8715 = CLOSED_SHELL('',(#8242,#8243,#8244,#8245,#8246,#8247,#8248,#8249,
#8250,#8251,#8252)) ;
#8716 = CLOSED_SHELL('',(#8253,#8254,#8255,#8256,#8257,#8258,#8259,#8260,
#8261,#8262,#8263,#8264,#8265,#8266,#8267,#8268,#8269,#8270,#8271,#8272,
#8273,#8274,#8275,#8276,#8277,#8278,#8279,#8280,#8281,#8282,#8283,#8284,
#8285,#8286,#8287,#8288,#8289,#8290,#8291,#8292,#8293)) ;
#8717 = CLOSED_SHELL('',(#8294,#8295,#8296,#8297)) ;
#8718 = CLOSED_SHELL('',(#8298,#8299,#8300)) ;
#8719 = CLOSED_SHELL('',(#8301,#8302,#8303,#8304,#8305,#8306,#8307,#8308,
#8309,#8310,#8311,#8312,#8313,#8314,#8315,#8316,#8317,#8318)) ;
#8720 = CLOSED_SHELL('',(#8319,#8320,#8321,#8322,#8323,#8324,#8325,#8326,
#8327,#8328,#8329,#8330,#8331,#8332,#8333,#8334,#8335,#8336)) ;
#8721 = CLOSED_SHELL('',(#8337,#8338,#8339,#8340,#8341,#8342,#8343,#8344,
#8345,#8346,#8347,#8348,#8349,#8350,#8351,#8352,#8353,#8354,#8355,#8356,
#8357,#8358,#8359,#8360,#8361,#8362,#8363)) ;
#8722 = CLOSED_SHELL('',(#8364,#8365,#8366,#8367,#8368,#8369,#8370,#8371,
#8372,#8373,#8374,#8375,#8376,#8377,#8378,#8379,#8380,#8381,#8382,#8383,
#8384,#8385,#8386,#8387,#8388,#8389,#8390,#8391)) ;
#8723 = CLOSED_SHELL('',(#8392,#8393,#8394,#8395,#8396)) ;
#8724 = CLOSED_SHELL('',(#8397,#8398,#8399,#8400,#8401,#8402,#8403,#8404,
#8405,#8406,#8407,#8408,#8409,#8410,#8411,#8412)) ;
#8725 = CLOSED_SHELL('',(#8413,#8414,#8415,#8416,#8417,#8418)) ;
#8726 = CLOSED_SHELL('',(#8419,#8420,#8421,#8422,#8423,#8424)) ;
#8727 = CLOSED_SHELL('',(#8425,#8426,#8427,#8428,#8429,#8430,#8431,#8432,
#8433,#8434,#8435,#8436)) ;
#8728 = CLOSED_SHELL('',(#8437,#8438,#8439,#8440,#8441,#8442)) ;
#8729 = CLOSED_SHELL('',(#8443,#8444,#8445,#8446,#8447,#8448)) ;
#8730 = CLOSED_SHELL('',(#8449,#8450,#8451,#8452,#8453,#8454,#8455,#8456,
#8457,#8458,#8459,#8460)) ;
#8731 = CLOSED_SHELL('',(#8461,#8462,#8463,#8464,#8465,#8466,#8467,#8468,
#8469,#8470,#8471,#8472,#8473,#8474,#8475,#8476,#8477,#8478,#8479)) ;
#8732 = CLOSED_SHELL('',(#8480,#8481,#8482,#8483,#8484,#8485,#8486,#8487)) ;
#8733 = CLOSED_SHELL('',(#8488,#8489,#8490,#8491,#8492,#8493,#8494,#8495,
#8496,#8497,#8498,#8499,#8500,#8501,#8502,#8503,#8504,#8505,#8506,#8507,
#8508,#8509,#8510,#8511,#8512,#8513,#8514,#8515,#8516,#8517,#8518,#8519,
#8520,#8521,#8522,#8523,#8524,#8525,#8526,#8527,#8528,#8529,#8530,#8531,
#8532,#8533,#8534,#8535,#8536,#8537,#8538,#8539,#8540,#8541,#8542,#8543,
#8544,#8545,#8546,#8547,#8548,#8549,#8550,#8551,#8552,#8553,#8554,#8555,
#8556,#8557,#8558,#8559,#8560,#8561,#8562,#8563,#8564,#8565,#8566,#8567,
#8568,#8569,#8570,#8571,#8572,#8573,#8574,#8575,#8576,#8577,#8578,#8579,
#8580,#8581,#8582,#8583,#8584,#8585,#8586,#8587,#8588,#8589,#8590,#8591,
#8592,#8593,#8594,#8595,#8596,#8597,#8598,#8599,#8600,#8601,#8602,#8603,
#8604,#8605,#8606,#8607,#8608,#8609,#8610,#8611,#8612,#8613,#8614,#8615,
#8616,#8617,#8618,#8619,#8620,#8621,#8622,#8623,#8624,#8625,#8626,#8627,
#8628,#8629,#8630,#8631,#8632,#8633,#8634,#8635,#8636,#8637,#8638,#8639,
#8640,#8641,#8642,#8643,#8644,#8645,#8646,#8647,#8648,#8649,#8650,#8651,
#8652,#8653,#8654,#8655,#8656,#8657,#8658,#8659,#8660,#8661,#8662,#8663,
#8664,#8665,#8666,#8667,#8668,#8669,#8670,#8671,#8672,#8673,#8674,#8675,
#8676,#8677,#8678,#8679,#8680,#8681,#8682,#8683,#8684,#8685,#8686,#8687,
#8688,#8689,#8690,#8691,#8692,#8693,#8694,#8695,#8696,#8697,#8698,#8699,
#8700,#8701,#8702,#8703,#8704,#8705,#8706,#8707,#8708,#8709,#8710,#8711,
#8712,#8713,#8714)) ;
#8734 = DERIVED_UNIT_ELEMENT(#8736,1.) ;
#8735 = DERIVED_UNIT_ELEMENT(#196743,-3.) ;
#8736 = (
MASS_UNIT()
NAMED_UNIT(*)
SI_UNIT(.KILO.,.GRAM.)
) ;
#8737 = DERIVED_UNIT((#8734,#8735)) ;
#8738 = MEASURE_REPRESENTATION_ITEM('density measure',
POSITIVE_RATIO_MEASURE(7850.),#8737) ;
#8739 = PROPERTY_DEFINITION_REPRESENTATION(#8744,#8741) ;
#8740 = PROPERTY_DEFINITION_REPRESENTATION(#8745,#8742) ;
#8741 = REPRESENTATION('material name',(#8743),#196740) ;
#8742 = REPRESENTATION('density',(#8738),#196740) ;
#8743 = DESCRIPTIVE_REPRESENTATION_ITEM('Steel','Steel') ;
#8744 = PROPERTY_DEFINITION('material property','material name') ;
#8745 = PROPERTY_DEFINITION('material property','density of part') ;
#8746 = AXIS2_PLACEMENT_3D('',#11576,#9455,#9456) ;
#8748 = AXIS2_PLACEMENT_3D('',#11578,#9459,#9460) ;
#8749 = AXIS2_PLACEMENT_3D('',#11852,#9462,#9463) ;
#8750 = AXIS2_PLACEMENT_3D('',#12314,#9469,#9470) ;
#8751 = AXIS2_PLACEMENT_3D('',#12316,#9471,#9472) ;
#8752 = AXIS2_PLACEMENT_3D('',#12319,#9474,#9475) ;
#8753 = AXIS2_PLACEMENT_3D('',#12320,#9476,#9477) ;
#8754 = AXIS2_PLACEMENT_3D('',#12341,#9478,#9479) ;
#8755 = AXIS2_PLACEMENT_3D('',#12440,#9482,#9483) ;
#8756 = AXIS2_PLACEMENT_3D('',#12524,#9485,#9486) ;
#8757 = AXIS2_PLACEMENT_3D('',#12707,#9487,#9488) ;
#8758 = AXIS2_PLACEMENT_3D('',#12981,#9490,#9491) ;
#8759 = AXIS2_PLACEMENT_3D('',#13952,#9493,#9494) ;
#8760 = AXIS2_PLACEMENT_3D('',#15016,#9496,#9497) ;
#8761 = AXIS2_PLACEMENT_3D('',#15154,#9499,#9500) ;
#8762 = AXIS2_PLACEMENT_3D('',#15666,#9502,#9503) ;
#8763 = AXIS2_PLACEMENT_3D('',#15761,#9504,#9505) ;
#8764 = AXIS2_PLACEMENT_3D('',#16031,#9507,#9508) ;
#8765 = AXIS2_PLACEMENT_3D('',#16286,#9510,#9511) ;
#8766 = AXIS2_PLACEMENT_3D('',#17908,#9513,#9514) ;
#8767 = AXIS2_PLACEMENT_3D('',#18436,#9516,#9517) ;
#8768 = AXIS2_PLACEMENT_3D('',#18438,#9518,#9519) ;
#8769 = AXIS2_PLACEMENT_3D('',#18441,#9521,#9522) ;
#8770 = AXIS2_PLACEMENT_3D('',#18510,#9523,#9524) ;
#8771 = AXIS2_PLACEMENT_3D('',#18699,#9525,#9526) ;
#8772 = AXIS2_PLACEMENT_3D('',#18966,#9529,#9530) ;
#8773 = AXIS2_PLACEMENT_3D('',#18971,#9532,#9533) ;
#8774 = AXIS2_PLACEMENT_3D('',#18972,#9534,#9535) ;
#8775 = AXIS2_PLACEMENT_3D('',#18973,#9536,#9537) ;
#8776 = AXIS2_PLACEMENT_3D('',#18976,#9538,#9539) ;
#8777 = AXIS2_PLACEMENT_3D('',#18979,#9541,#9542) ;
#8778 = AXIS2_PLACEMENT_3D('',#33345,#9543,#9544) ;
#8779 = AXIS2_PLACEMENT_3D('',#33349,#9546,#9547) ;
#8780 = AXIS2_PLACEMENT_3D('',#33358,#9549,#9550) ;
#8781 = AXIS2_PLACEMENT_3D('',#41428,#9551,#9552) ;
#8782 = AXIS2_PLACEMENT_3D('',#41431,#9554,#9555) ;
#8783 = AXIS2_PLACEMENT_3D('',#41432,#9556,#9557) ;
#8784 = AXIS2_PLACEMENT_3D('',#42521,#9558,#9559) ;
#8785 = AXIS2_PLACEMENT_3D('',#43217,#9560,#9561) ;
#8786 = AXIS2_PLACEMENT_3D('',#43241,#9562,#9563) ;
#8787 = AXIS2_PLACEMENT_3D('',#64559,#9565,#9566) ;
#8788 = AXIS2_PLACEMENT_3D('',#64561,#9568,#9569) ;
#8789 = AXIS2_PLACEMENT_3D('',#71960,#9572,#9573) ;
#8790 = AXIS2_PLACEMENT_3D('',#79036,#9575,#9576) ;
#8791 = AXIS2_PLACEMENT_3D('',#79092,#9579,#9580) ;
#8792 = AXIS2_PLACEMENT_3D('',#79148,#9583,#9584) ;
#8793 = AXIS2_PLACEMENT_3D('',#79171,#9586,#9587) ;
#8794 = AXIS2_PLACEMENT_3D('',#79260,#9591,#9592) ;
#8795 = AXIS2_PLACEMENT_3D('',#79262,#9593,#9594) ;
#8796 = AXIS2_PLACEMENT_3D('',#79266,#9596,#9597) ;
#8797 = AXIS2_PLACEMENT_3D('',#79267,#9598,#9599) ;
#8798 = AXIS2_PLACEMENT_3D('',#79268,#9600,#9601) ;
#8799 = AXIS2_PLACEMENT_3D('',#79269,#9602,#9603) ;
#8800 = AXIS2_PLACEMENT_3D('',#79305,#9605,#9606) ;
#8801 = AXIS2_PLACEMENT_3D('',#79307,#9607,#9608) ;
#8802 = AXIS2_PLACEMENT_3D('',#79310,#9610,#9611) ;
#8803 = AXIS2_PLACEMENT_3D('',#79311,#9612,#9613) ;
#8804 = AXIS2_PLACEMENT_3D('',#79312,#9614,#9615) ;
#8805 = AXIS2_PLACEMENT_3D('',#79313,#9616,#9617) ;
#8806 = AXIS2_PLACEMENT_3D('',#79487,#9619,#9620) ;
#8807 = AXIS2_PLACEMENT_3D('',#79630,#9621,#9622) ;
#8808 = AXIS2_PLACEMENT_3D('',#80086,#9624,#9625) ;
#8809 = AXIS2_PLACEMENT_3D('',#80533,#9627,#9628) ;
#8810 = AXIS2_PLACEMENT_3D('',#80989,#9630,#9631) ;
#8811 = AXIS2_PLACEMENT_3D('',#81292,#9632,#9633) ;
#8812 = AXIS2_PLACEMENT_3D('',#81515,#9634,#9635) ;
#8813 = AXIS2_PLACEMENT_3D('',#81519,#9637,#9638) ;
#8814 = AXIS2_PLACEMENT_3D('',#81520,#9639,#9640) ;
#8815 = AXIS2_PLACEMENT_3D('',#95698,#9642,#9643) ;
#8816 = AXIS2_PLACEMENT_3D('',#95700,#9644,#9645) ;
#8817 = AXIS2_PLACEMENT_3D('',#95702,#9647,#9648) ;
#8818 = AXIS2_PLACEMENT_3D('',#95715,#9655,#9656) ;
#8819 = AXIS2_PLACEMENT_3D('',#95721,#9660,#9661) ;
#8820 = AXIS2_PLACEMENT_3D('',#95725,#9664,#9665) ;
#8821 = AXIS2_PLACEMENT_3D('',#95729,#9668,#9669) ;
#8822 = AXIS2_PLACEMENT_3D('',#95733,#9672,#9673) ;
#8823 = AXIS2_PLACEMENT_3D('',#95737,#9676,#9677) ;
#8824 = AXIS2_PLACEMENT_3D('',#95739,#9679,#9680) ;
#8825 = AXIS2_PLACEMENT_3D('',#95740,#9681,#9682) ;
#8826 = AXIS2_PLACEMENT_3D('',#95914,#9684,#9685) ;
#8827 = AXIS2_PLACEMENT_3D('',#96057,#9686,#9687) ;
#8828 = AXIS2_PLACEMENT_3D('',#97229,#9689,#9690) ;
#8829 = AXIS2_PLACEMENT_3D('',#97676,#9692,#9693) ;
#8830 = AXIS2_PLACEMENT_3D('',#98132,#9695,#9696) ;
#8831 = AXIS2_PLACEMENT_3D('',#98433,#9697,#9698) ;
#8832 = AXIS2_PLACEMENT_3D('',#98656,#9699,#9700) ;
#8833 = AXIS2_PLACEMENT_3D('',#98658,#9701,#9702) ;
#8834 = AXIS2_PLACEMENT_3D('',#98661,#9704,#9705) ;
#8835 = AXIS2_PLACEMENT_3D('',#112839,#9707,#9708) ;
#8836 = AXIS2_PLACEMENT_3D('',#112842,#9710,#9711) ;
#8837 = AXIS2_PLACEMENT_3D('',#112843,#9712,#9713) ;
#8838 = AXIS2_PLACEMENT_3D('',#112856,#9720,#9721) ;
#8839 = AXIS2_PLACEMENT_3D('',#112862,#9725,#9726) ;
#8840 = AXIS2_PLACEMENT_3D('',#112866,#9729,#9730) ;
#8841 = AXIS2_PLACEMENT_3D('',#112870,#9733,#9734) ;
#8842 = AXIS2_PLACEMENT_3D('',#112874,#9737,#9738) ;
#8843 = AXIS2_PLACEMENT_3D('',#112878,#9741,#9742) ;
#8844 = AXIS2_PLACEMENT_3D('',#112880,#9744,#9745) ;
#8845 = AXIS2_PLACEMENT_3D('',#112881,#9746,#9747) ;
#8846 = AXIS2_PLACEMENT_3D('',#112884,#9748,#9749) ;
#8847 = AXIS2_PLACEMENT_3D('',#112888,#9751,#9752) ;
#8848 = AXIS2_PLACEMENT_3D('',#112890,#9754,#9755) ;
#8849 = AXIS2_PLACEMENT_3D('',#112892,#9756,#9757) ;
#8850 = AXIS2_PLACEMENT_3D('',#112895,#9759,#9760) ;
#8851 = AXIS2_PLACEMENT_3D('',#112896,#9761,#9762) ;
#8852 = AXIS2_PLACEMENT_3D('',#112898,#9763,#9764) ;
#8853 = AXIS2_PLACEMENT_3D('',#112901,#9766,#9767) ;
#8854 = AXIS2_PLACEMENT_3D('',#112902,#9768,#9769) ;
#8855 = AXIS2_PLACEMENT_3D('',#112903,#9770,#9771) ;
#8856 = AXIS2_PLACEMENT_3D('',#112904,#9772,#9773) ;
#8857 = AXIS2_PLACEMENT_3D('',#112905,#9774,#9775) ;
#8858 = AXIS2_PLACEMENT_3D('',#112907,#9776,#9777) ;
#8859 = AXIS2_PLACEMENT_3D('',#112910,#9779,#9780) ;
#8860 = AXIS2_PLACEMENT_3D('',#112911,#9781,#9782) ;
#8861 = AXIS2_PLACEMENT_3D('',#112913,#9783,#9784) ;
#8862 = AXIS2_PLACEMENT_3D('',#112916,#9785,#9786) ;
#8863 = AXIS2_PLACEMENT_3D('',#112918,#9787,#9788) ;
#8864 = AXIS2_PLACEMENT_3D('',#112920,#9789,#9790) ;
#8865 = AXIS2_PLACEMENT_3D('',#112921,#9791,#9792) ;
#8866 = AXIS2_PLACEMENT_3D('',#112923,#9793,#9794) ;
#8867 = AXIS2_PLACEMENT_3D('',#112926,#9795,#9796) ;
#8868 = AXIS2_PLACEMENT_3D('',#112928,#9797,#9798) ;
#8869 = AXIS2_PLACEMENT_3D('',#112930,#9799,#9800) ;
#8870 = AXIS2_PLACEMENT_3D('',#112931,#9801,#9802) ;
#8871 = AXIS2_PLACEMENT_3D('',#112932,#9803,#9804) ;
#8872 = AXIS2_PLACEMENT_3D('',#112967,#9805,#9806) ;
#8873 = AXIS2_PLACEMENT_3D('',#112980,#9807,#9808) ;
#8874 = AXIS2_PLACEMENT_3D('',#112983,#9809,#9810) ;
#8875 = AXIS2_PLACEMENT_3D('',#113008,#9811,#9812) ;
#8876 = AXIS2_PLACEMENT_3D('',#113038,#9813,#9814) ;
#8877 = AXIS2_PLACEMENT_3D('',#113040,#9815,#9816) ;
#8878 = AXIS2_PLACEMENT_3D('',#113042,#9818,#9819) ;
#8879 = AXIS2_PLACEMENT_3D('',#113058,#9822,#9823) ;
#8880 = AXIS2_PLACEMENT_3D('',#113061,#9825,#9826) ;
#8881 = AXIS2_PLACEMENT_3D('',#113062,#9827,#9828) ;
#8882 = AXIS2_PLACEMENT_3D('',#113076,#9830,#9831) ;
#8883 = AXIS2_PLACEMENT_3D('',#113083,#9832,#9833) ;
#8884 = AXIS2_PLACEMENT_3D('',#113085,#9834,#9835) ;
#8885 = AXIS2_PLACEMENT_3D('',#113087,#9837,#9838) ;
#8886 = AXIS2_PLACEMENT_3D('',#113098,#9841,#9842) ;
#8887 = AXIS2_PLACEMENT_3D('',#113101,#9844,#9845) ;
#8888 = AXIS2_PLACEMENT_3D('',#113102,#9846,#9847) ;
#8889 = AXIS2_PLACEMENT_3D('',#113105,#9849,#9850) ;
#8890 = AXIS2_PLACEMENT_3D('',#113106,#9851,#9852) ;
#8891 = AXIS2_PLACEMENT_3D('',#113314,#9863,#9864) ;
#8892 = AXIS2_PLACEMENT_3D('',#113317,#9865,#9866) ;
#8893 = AXIS2_PLACEMENT_3D('',#113321,#9868,#9869) ;
#8894 = AXIS2_PLACEMENT_3D('',#113323,#9871,#9872) ;
#8895 = AXIS2_PLACEMENT_3D('',#113325,#9873,#9874) ;
#8896 = AXIS2_PLACEMENT_3D('',#113328,#9876,#9877) ;
#8897 = AXIS2_PLACEMENT_3D('',#113329,#9878,#9879) ;
#8898 = AXIS2_PLACEMENT_3D('',#113331,#9880,#9881) ;
#8899 = AXIS2_PLACEMENT_3D('',#113334,#9883,#9884) ;
#8900 = AXIS2_PLACEMENT_3D('',#113335,#9885,#9886) ;
#8901 = AXIS2_PLACEMENT_3D('',#113336,#9887,#9888) ;
#8902 = AXIS2_PLACEMENT_3D('',#113337,#9889,#9890) ;
#8903 = AXIS2_PLACEMENT_3D('',#113338,#9891,#9892) ;
#8904 = AXIS2_PLACEMENT_3D('',#113340,#9893,#9894) ;
#8905 = AXIS2_PLACEMENT_3D('',#113343,#9895,#9896) ;
#8906 = AXIS2_PLACEMENT_3D('',#113345,#9897,#9898) ;
#8907 = AXIS2_PLACEMENT_3D('',#113347,#9899,#9900) ;
#8908 = AXIS2_PLACEMENT_3D('',#113348,#9901,#9902) ;
#8909 = AXIS2_PLACEMENT_3D('',#113350,#9903,#9904) ;
#8910 = AXIS2_PLACEMENT_3D('',#113353,#9905,#9906) ;
#8911 = AXIS2_PLACEMENT_3D('',#113355,#9907,#9908) ;
#8912 = AXIS2_PLACEMENT_3D('',#113357,#9909,#9910) ;
#8913 = AXIS2_PLACEMENT_3D('',#113358,#9911,#9912) ;
#8914 = AXIS2_PLACEMENT_3D('',#113360,#9913,#9914) ;
#8915 = AXIS2_PLACEMENT_3D('',#113361,#9915,#9916) ;
#8916 = AXIS2_PLACEMENT_3D('',#113396,#9917,#9918) ;
#8917 = AXIS2_PLACEMENT_3D('',#113409,#9919,#9920) ;
#8918 = AXIS2_PLACEMENT_3D('',#113424,#9921,#9922) ;
#8919 = AXIS2_PLACEMENT_3D('',#113436,#9923,#9924) ;
#8920 = AXIS2_PLACEMENT_3D('',#113466,#9925,#9926) ;
#8921 = AXIS2_PLACEMENT_3D('',#113468,#9927,#9928) ;
#8922 = AXIS2_PLACEMENT_3D('',#113470,#9930,#9931) ;
#8923 = AXIS2_PLACEMENT_3D('',#113486,#9934,#9935) ;
#8924 = AXIS2_PLACEMENT_3D('',#113489,#9937,#9938) ;
#8925 = AXIS2_PLACEMENT_3D('',#113490,#9939,#9940) ;
#8926 = AXIS2_PLACEMENT_3D('',#113504,#9942,#9943) ;
#8927 = AXIS2_PLACEMENT_3D('',#113511,#9944,#9945) ;
#8928 = AXIS2_PLACEMENT_3D('',#113513,#9946,#9947) ;
#8929 = AXIS2_PLACEMENT_3D('',#113515,#9949,#9950) ;
#8930 = AXIS2_PLACEMENT_3D('',#113526,#9953,#9954) ;
#8931 = AXIS2_PLACEMENT_3D('',#113538,#9956,#9957) ;
#8932 = AXIS2_PLACEMENT_3D('',#113541,#9959,#9960) ;
#8933 = AXIS2_PLACEMENT_3D('',#113542,#9961,#9962) ;
#8934 = AXIS2_PLACEMENT_3D('',#113552,#9963,#9964) ;
#8935 = AXIS2_PLACEMENT_3D('',#113787,#9977,#9978) ;
#8936 = AXIS2_PLACEMENT_3D('',#113789,#9979,#9980) ;
#8937 = AXIS2_PLACEMENT_3D('',#113792,#9982,#9983) ;
#8938 = AXIS2_PLACEMENT_3D('',#113793,#9984,#9985) ;
#8939 = AXIS2_PLACEMENT_3D('',#113814,#9986,#9987) ;
#8940 = AXIS2_PLACEMENT_3D('',#113913,#9990,#9991) ;
#8941 = AXIS2_PLACEMENT_3D('',#113916,#9992,#9993) ;
#8942 = AXIS2_PLACEMENT_3D('',#113920,#9995,#9996) ;
#8943 = AXIS2_PLACEMENT_3D('',#113922,#9998,#9999) ;
#8944 = AXIS2_PLACEMENT_3D('',#113928,#10003,#10004) ;
#8945 = AXIS2_PLACEMENT_3D('',#113930,#10005,#10006) ;
#8946 = AXIS2_PLACEMENT_3D('',#113933,#10008,#10009) ;
#8947 = AXIS2_PLACEMENT_3D('',#113934,#10010,#10011) ;
#8948 = AXIS2_PLACEMENT_3D('',#113936,#10012,#10013) ;
#8949 = AXIS2_PLACEMENT_3D('',#113939,#10015,#10016) ;
#8950 = AXIS2_PLACEMENT_3D('',#113940,#10017,#10018) ;
#8951 = AXIS2_PLACEMENT_3D('',#113946,#10022,#10023) ;
#8952 = AXIS2_PLACEMENT_3D('',#113952,#10027,#10028) ;
#8953 = AXIS2_PLACEMENT_3D('',#113954,#10029,#10030) ;
#8954 = AXIS2_PLACEMENT_3D('',#113957,#10032,#10033) ;
#8955 = AXIS2_PLACEMENT_3D('',#113958,#10034,#10035) ;
#8956 = AXIS2_PLACEMENT_3D('',#113964,#10039,#10040) ;
#8957 = AXIS2_PLACEMENT_3D('',#113966,#10041,#10042) ;
#8958 = AXIS2_PLACEMENT_3D('',#113969,#10044,#10045) ;
#8959 = AXIS2_PLACEMENT_3D('',#113970,#10046,#10047) ;
#8960 = AXIS2_PLACEMENT_3D('',#113972,#10048,#10049) ;
#8961 = AXIS2_PLACEMENT_3D('',#113975,#10051,#10052) ;
#8962 = AXIS2_PLACEMENT_3D('',#113976,#10053,#10054) ;
#8963 = AXIS2_PLACEMENT_3D('',#113982,#10058,#10059) ;
#8964 = AXIS2_PLACEMENT_3D('',#113983,#10060,#10061) ;
#8965 = AXIS2_PLACEMENT_3D('',#113984,#10062,#10063) ;
#8966 = AXIS2_PLACEMENT_3D('',#113985,#10064,#10065) ;
#8967 = AXIS2_PLACEMENT_3D('',#113987,#10066,#10067) ;
#8968 = AXIS2_PLACEMENT_3D('',#113989,#10068,#10069) ;
#8969 = AXIS2_PLACEMENT_3D('',#113990,#10070,#10071) ;
#8970 = AXIS2_PLACEMENT_3D('',#113992,#10072,#10073) ;
#8971 = AXIS2_PLACEMENT_3D('',#113994,#10074,#10075) ;
#8972 = AXIS2_PLACEMENT_3D('',#113995,#10076,#10077) ;
#8973 = AXIS2_PLACEMENT_3D('',#113997,#10079,#10080) ;
#8974 = AXIS2_PLACEMENT_3D('',#113999,#10082,#10083) ;
#8975 = AXIS2_PLACEMENT_3D('',#114003,#10085,#10086) ;
#8976 = AXIS2_PLACEMENT_3D('',#114032,#10087,#10088) ;
#8977 = AXIS2_PLACEMENT_3D('',#114034,#10089,#10090) ;
#8978 = AXIS2_PLACEMENT_3D('',#114054,#10091,#10092) ;
#8979 = AXIS2_PLACEMENT_3D('',#114138,#10094,#10095) ;
#8980 = AXIS2_PLACEMENT_3D('',#114167,#10096,#10097) ;
#8981 = AXIS2_PLACEMENT_3D('',#114188,#10100,#10101) ;
#8982 = AXIS2_PLACEMENT_3D('',#114190,#10102,#10103) ;
#8983 = AXIS2_PLACEMENT_3D('',#114222,#10105,#10106) ;
#8984 = AXIS2_PLACEMENT_3D('',#114223,#10107,#10108) ;
#8985 = AXIS2_PLACEMENT_3D('',#114244,#10110,#10111) ;
#8986 = AXIS2_PLACEMENT_3D('',#114336,#10112,#10113) ;
#8987 = AXIS2_PLACEMENT_3D('',#114357,#10115,#10116) ;
#8988 = AXIS2_PLACEMENT_3D('',#114377,#10118,#10119) ;
#8989 = AXIS2_PLACEMENT_3D('',#114379,#10120,#10121) ;
#8990 = AXIS2_PLACEMENT_3D('',#133900,#10122,#10123) ;
#8991 = AXIS2_PLACEMENT_3D('',#133902,#10124,#10125) ;
#8992 = AXIS2_PLACEMENT_3D('',#133903,#10126,#10127) ;
#8993 = AXIS2_PLACEMENT_3D('',#134132,#10128,#10129) ;
#8994 = AXIS2_PLACEMENT_3D('',#134172,#10131,#10132) ;
#8995 = AXIS2_PLACEMENT_3D('',#134174,#10133,#10134) ;
#8996 = AXIS2_PLACEMENT_3D('',#134175,#10135,#10136) ;
#8997 = AXIS2_PLACEMENT_3D('',#134366,#10137,#10138) ;
#8998 = AXIS2_PLACEMENT_3D('',#134368,#10139,#10140) ;
#8999 = AXIS2_PLACEMENT_3D('',#153889,#10141,#10142) ;
#9000 = AXIS2_PLACEMENT_3D('',#153891,#10143,#10144) ;
#9001 = AXIS2_PLACEMENT_3D('',#153892,#10145,#10146) ;
#9002 = AXIS2_PLACEMENT_3D('',#154119,#10147,#10148) ;
#9003 = AXIS2_PLACEMENT_3D('',#154159,#10150,#10151) ;
#9004 = AXIS2_PLACEMENT_3D('',#154161,#10152,#10153) ;
#9005 = AXIS2_PLACEMENT_3D('',#154162,#10154,#10155) ;
#9006 = AXIS2_PLACEMENT_3D('',#154353,#10156,#10157) ;
#9007 = AXIS2_PLACEMENT_3D('',#154354,#10158,#10159) ;
#9008 = AXIS2_PLACEMENT_3D('',#154355,#10160,#10161) ;
#9009 = AXIS2_PLACEMENT_3D('',#154357,#10162,#10163) ;
#9010 = AXIS2_PLACEMENT_3D('',#154389,#10165,#10166) ;
#9011 = AXIS2_PLACEMENT_3D('',#154390,#10167,#10168) ;
#9012 = AXIS2_PLACEMENT_3D('',#154411,#10170,#10171) ;
#9013 = AXIS2_PLACEMENT_3D('',#154503,#10172,#10173) ;
#9014 = AXIS2_PLACEMENT_3D('',#154524,#10175,#10176) ;
#9015 = AXIS2_PLACEMENT_3D('',#154544,#10178,#10179) ;
#9016 = AXIS2_PLACEMENT_3D('',#154548,#10181,#10182) ;
#9017 = AXIS2_PLACEMENT_3D('',#154577,#10183,#10184) ;
#9018 = AXIS2_PLACEMENT_3D('',#154579,#10185,#10186) ;
#9019 = AXIS2_PLACEMENT_3D('',#154599,#10187,#10188) ;
#9020 = AXIS2_PLACEMENT_3D('',#154683,#10190,#10191) ;
#9021 = AXIS2_PLACEMENT_3D('',#154712,#10192,#10193) ;
#9022 = AXIS2_PLACEMENT_3D('',#154733,#10196,#10197) ;
#9023 = AXIS2_PLACEMENT_3D('',#154735,#10198,#10199) ;
#9024 = AXIS2_PLACEMENT_3D('',#174413,#10200,#10201) ;
#9025 = AXIS2_PLACEMENT_3D('',#174415,#10202,#10203) ;
#9026 = AXIS2_PLACEMENT_3D('',#174416,#10204,#10205) ;
#9027 = AXIS2_PLACEMENT_3D('',#174488,#10206,#10207) ;
#9028 = AXIS2_PLACEMENT_3D('',#174528,#10209,#10210) ;
#9029 = AXIS2_PLACEMENT_3D('',#174530,#10211,#10212) ;
#9030 = AXIS2_PLACEMENT_3D('',#174531,#10213,#10214) ;
#9031 = AXIS2_PLACEMENT_3D('',#174722,#10215,#10216) ;
#9032 = AXIS2_PLACEMENT_3D('',#174724,#10217,#10218) ;
#9033 = AXIS2_PLACEMENT_3D('',#194400,#10219,#10220) ;
#9034 = AXIS2_PLACEMENT_3D('',#194402,#10221,#10222) ;
#9035 = AXIS2_PLACEMENT_3D('',#194403,#10223,#10224) ;
#9036 = AXIS2_PLACEMENT_3D('',#194475,#10225,#10226) ;
#9037 = AXIS2_PLACEMENT_3D('',#194515,#10228,#10229) ;
#9038 = AXIS2_PLACEMENT_3D('',#194517,#10230,#10231) ;
#9039 = AXIS2_PLACEMENT_3D('',#194518,#10232,#10233) ;
#9040 = AXIS2_PLACEMENT_3D('',#194709,#10234,#10235) ;
#9041 = AXIS2_PLACEMENT_3D('',#194710,#10236,#10237) ;
#9042 = AXIS2_PLACEMENT_3D('',#194711,#10238,#10239) ;
#9043 = AXIS2_PLACEMENT_3D('',#194727,#10244,#10245) ;
#9044 = AXIS2_PLACEMENT_3D('',#194730,#10247,#10248) ;
#9045 = AXIS2_PLACEMENT_3D('',#194731,#10249,#10250) ;
#9046 = AXIS2_PLACEMENT_3D('',#194733,#10251,#10252) ;
#9047 = AXIS2_PLACEMENT_3D('',#194736,#10254,#10255) ;
#9048 = AXIS2_PLACEMENT_3D('',#194737,#10256,#10257) ;
#9049 = AXIS2_PLACEMENT_3D('',#194739,#10258,#10259) ;
#9050 = AXIS2_PLACEMENT_3D('',#194742,#10261,#10262) ;
#9051 = AXIS2_PLACEMENT_3D('',#194743,#10263,#10264) ;
#9052 = AXIS2_PLACEMENT_3D('',#194745,#10265,#10266) ;
#9053 = AXIS2_PLACEMENT_3D('',#194748,#10268,#10269) ;
#9054 = AXIS2_PLACEMENT_3D('',#194749,#10270,#10271) ;
#9055 = AXIS2_PLACEMENT_3D('',#194751,#10272,#10273) ;
#9056 = AXIS2_PLACEMENT_3D('',#194754,#10275,#10276) ;
#9057 = AXIS2_PLACEMENT_3D('',#194755,#10277,#10278) ;
#9058 = AXIS2_PLACEMENT_3D('',#194757,#10279,#10280) ;
#9059 = AXIS2_PLACEMENT_3D('',#194760,#10282,#10283) ;
#9060 = AXIS2_PLACEMENT_3D('',#194761,#10284,#10285) ;
#9061 = AXIS2_PLACEMENT_3D('',#194767,#10289,#10290) ;
#9062 = AXIS2_PLACEMENT_3D('',#194769,#10291,#10292) ;
#9063 = AXIS2_PLACEMENT_3D('',#194772,#10294,#10295) ;
#9064 = AXIS2_PLACEMENT_3D('',#194773,#10296,#10297) ;
#9065 = AXIS2_PLACEMENT_3D('',#194779,#10301,#10302) ;
#9066 = AXIS2_PLACEMENT_3D('',#194781,#10303,#10304) ;
#9067 = AXIS2_PLACEMENT_3D('',#194784,#10306,#10307) ;
#9068 = AXIS2_PLACEMENT_3D('',#194785,#10308,#10309) ;
#9069 = AXIS2_PLACEMENT_3D('',#194787,#10310,#10311) ;
#9070 = AXIS2_PLACEMENT_3D('',#194790,#10313,#10314) ;
#9071 = AXIS2_PLACEMENT_3D('',#194791,#10315,#10316) ;
#9072 = AXIS2_PLACEMENT_3D('',#194793,#10317,#10318) ;
#9073 = AXIS2_PLACEMENT_3D('',#194796,#10320,#10321) ;
#9074 = AXIS2_PLACEMENT_3D('',#194804,#10322,#10323) ;
#9075 = AXIS2_PLACEMENT_3D('',#194807,#10325,#10326) ;
#9076 = AXIS2_PLACEMENT_3D('',#194808,#10327,#10328) ;
#9077 = AXIS2_PLACEMENT_3D('',#194811,#10331,#10332) ;
#9078 = AXIS2_PLACEMENT_3D('',#194813,#10333,#10334) ;
#9079 = AXIS2_PLACEMENT_3D('',#194816,#10336,#10337) ;
#9080 = AXIS2_PLACEMENT_3D('',#194817,#10338,#10339) ;
#9081 = AXIS2_PLACEMENT_3D('',#194819,#10340,#10341) ;
#9082 = AXIS2_PLACEMENT_3D('',#194822,#10343,#10344) ;
#9083 = AXIS2_PLACEMENT_3D('',#194823,#10345,#10346) ;
#9084 = AXIS2_PLACEMENT_3D('',#194824,#10347,#10348) ;
#9085 = AXIS2_PLACEMENT_3D('',#194825,#10349,#10350) ;
#9086 = AXIS2_PLACEMENT_3D('',#194827,#10351,#10352) ;
#9087 = AXIS2_PLACEMENT_3D('',#194830,#10354,#10355) ;
#9088 = AXIS2_PLACEMENT_3D('',#194831,#10356,#10357) ;
#9089 = AXIS2_PLACEMENT_3D('',#194833,#10358,#10359) ;
#9090 = AXIS2_PLACEMENT_3D('',#194835,#10360,#10361) ;
#9091 = AXIS2_PLACEMENT_3D('',#194836,#10362,#10363) ;
#9092 = AXIS2_PLACEMENT_3D('',#194838,#10364,#10365) ;
#9093 = AXIS2_PLACEMENT_3D('',#194839,#10366,#10367) ;
#9094 = AXIS2_PLACEMENT_3D('',#194841,#10368,#10369) ;
#9095 = AXIS2_PLACEMENT_3D('',#194844,#10371,#10372) ;
#9096 = AXIS2_PLACEMENT_3D('',#194845,#10373,#10374) ;
#9097 = AXIS2_PLACEMENT_3D('',#194847,#10375,#10376) ;
#9098 = AXIS2_PLACEMENT_3D('',#194848,#10377,#10378) ;
#9099 = AXIS2_PLACEMENT_3D('',#194849,#10379,#10380) ;
#9100 = AXIS2_PLACEMENT_3D('',#194851,#10382,#10383) ;
#9101 = AXIS2_PLACEMENT_3D('',#194853,#10385,#10386) ;
#9102 = AXIS2_PLACEMENT_3D('',#194873,#10391,#10392) ;
#9103 = AXIS2_PLACEMENT_3D('',#194876,#10394,#10395) ;
#9104 = AXIS2_PLACEMENT_3D('',#194877,#10396,#10397) ;
#9105 = AXIS2_PLACEMENT_3D('',#194883,#10401,#10402) ;
#9106 = AXIS2_PLACEMENT_3D('',#194900,#10406,#10407) ;
#9107 = AXIS2_PLACEMENT_3D('',#194903,#10409,#10410) ;
#9108 = AXIS2_PLACEMENT_3D('',#194904,#10411,#10412) ;
#9109 = AXIS2_PLACEMENT_3D('',#194910,#10416,#10417) ;
#9110 = AXIS2_PLACEMENT_3D('',#194927,#10421,#10422) ;
#9111 = AXIS2_PLACEMENT_3D('',#194930,#10424,#10425) ;
#9112 = AXIS2_PLACEMENT_3D('',#194931,#10426,#10427) ;
#9113 = AXIS2_PLACEMENT_3D('',#194937,#10431,#10432) ;
#9114 = AXIS2_PLACEMENT_3D('',#194954,#10436,#10437) ;
#9115 = AXIS2_PLACEMENT_3D('',#194957,#10439,#10440) ;
#9116 = AXIS2_PLACEMENT_3D('',#194958,#10441,#10442) ;
#9117 = AXIS2_PLACEMENT_3D('',#194964,#10446,#10447) ;
#9118 = AXIS2_PLACEMENT_3D('',#194981,#10451,#10452) ;
#9119 = AXIS2_PLACEMENT_3D('',#194984,#10454,#10455) ;
#9120 = AXIS2_PLACEMENT_3D('',#194985,#10456,#10457) ;
#9121 = AXIS2_PLACEMENT_3D('',#194991,#10461,#10462) ;
#9122 = AXIS2_PLACEMENT_3D('',#195008,#10466,#10467) ;
#9123 = AXIS2_PLACEMENT_3D('',#195011,#10469,#10470) ;
#9124 = AXIS2_PLACEMENT_3D('',#195012,#10471,#10472) ;
#9125 = AXIS2_PLACEMENT_3D('',#195018,#10476,#10477) ;
#9126 = AXIS2_PLACEMENT_3D('',#195035,#10481,#10482) ;
#9127 = AXIS2_PLACEMENT_3D('',#195038,#10484,#10485) ;
#9128 = AXIS2_PLACEMENT_3D('',#195039,#10486,#10487) ;
#9129 = AXIS2_PLACEMENT_3D('',#195045,#10491,#10492) ;
#9130 = AXIS2_PLACEMENT_3D('',#195062,#10496,#10497) ;
#9131 = AXIS2_PLACEMENT_3D('',#195065,#10499,#10500) ;
#9132 = AXIS2_PLACEMENT_3D('',#195066,#10501,#10502) ;
#9133 = AXIS2_PLACEMENT_3D('',#195072,#10506,#10507) ;
#9134 = AXIS2_PLACEMENT_3D('',#195089,#10511,#10512) ;
#9135 = AXIS2_PLACEMENT_3D('',#195092,#10514,#10515) ;
#9136 = AXIS2_PLACEMENT_3D('',#195093,#10516,#10517) ;
#9137 = AXIS2_PLACEMENT_3D('',#195099,#10521,#10522) ;
#9138 = AXIS2_PLACEMENT_3D('',#195116,#10526,#10527) ;
#9139 = AXIS2_PLACEMENT_3D('',#195119,#10529,#10530) ;
#9140 = AXIS2_PLACEMENT_3D('',#195120,#10531,#10532) ;
#9141 = AXIS2_PLACEMENT_3D('',#195126,#10536,#10537) ;
#9142 = AXIS2_PLACEMENT_3D('',#195143,#10541,#10542) ;
#9143 = AXIS2_PLACEMENT_3D('',#195146,#10544,#10545) ;
#9144 = AXIS2_PLACEMENT_3D('',#195147,#10546,#10547) ;
#9145 = AXIS2_PLACEMENT_3D('',#195153,#10551,#10552) ;
#9146 = AXIS2_PLACEMENT_3D('',#195170,#10556,#10557) ;
#9147 = AXIS2_PLACEMENT_3D('',#195173,#10559,#10560) ;
#9148 = AXIS2_PLACEMENT_3D('',#195174,#10561,#10562) ;
#9149 = AXIS2_PLACEMENT_3D('',#195180,#10566,#10567) ;
#9150 = AXIS2_PLACEMENT_3D('',#195197,#10571,#10572) ;
#9151 = AXIS2_PLACEMENT_3D('',#195200,#10574,#10575) ;
#9152 = AXIS2_PLACEMENT_3D('',#195201,#10576,#10577) ;
#9153 = AXIS2_PLACEMENT_3D('',#195207,#10581,#10582) ;
#9154 = AXIS2_PLACEMENT_3D('',#195224,#10586,#10587) ;
#9155 = AXIS2_PLACEMENT_3D('',#195227,#10589,#10590) ;
#9156 = AXIS2_PLACEMENT_3D('',#195228,#10591,#10592) ;
#9157 = AXIS2_PLACEMENT_3D('',#195234,#10596,#10597) ;
#9158 = AXIS2_PLACEMENT_3D('',#195251,#10601,#10602) ;
#9159 = AXIS2_PLACEMENT_3D('',#195254,#10604,#10605) ;
#9160 = AXIS2_PLACEMENT_3D('',#195255,#10606,#10607) ;
#9161 = AXIS2_PLACEMENT_3D('',#195261,#10611,#10612) ;
#9162 = AXIS2_PLACEMENT_3D('',#195278,#10616,#10617) ;
#9163 = AXIS2_PLACEMENT_3D('',#195281,#10619,#10620) ;
#9164 = AXIS2_PLACEMENT_3D('',#195282,#10621,#10622) ;
#9165 = AXIS2_PLACEMENT_3D('',#195288,#10626,#10627) ;
#9166 = AXIS2_PLACEMENT_3D('',#195305,#10631,#10632) ;
#9167 = AXIS2_PLACEMENT_3D('',#195308,#10634,#10635) ;
#9168 = AXIS2_PLACEMENT_3D('',#195309,#10636,#10637) ;
#9169 = AXIS2_PLACEMENT_3D('',#195315,#10641,#10642) ;
#9170 = AXIS2_PLACEMENT_3D('',#195332,#10646,#10647) ;
#9171 = AXIS2_PLACEMENT_3D('',#195335,#10649,#10650) ;
#9172 = AXIS2_PLACEMENT_3D('',#195336,#10651,#10652) ;
#9173 = AXIS2_PLACEMENT_3D('',#195342,#10656,#10657) ;
#9174 = AXIS2_PLACEMENT_3D('',#195359,#10661,#10662) ;
#9175 = AXIS2_PLACEMENT_3D('',#195362,#10664,#10665) ;
#9176 = AXIS2_PLACEMENT_3D('',#195363,#10666,#10667) ;
#9177 = AXIS2_PLACEMENT_3D('',#195369,#10671,#10672) ;
#9178 = AXIS2_PLACEMENT_3D('',#195386,#10676,#10677) ;
#9179 = AXIS2_PLACEMENT_3D('',#195389,#10679,#10680) ;
#9180 = AXIS2_PLACEMENT_3D('',#195390,#10681,#10682) ;
#9181 = AXIS2_PLACEMENT_3D('',#195396,#10686,#10687) ;
#9182 = AXIS2_PLACEMENT_3D('',#195413,#10691,#10692) ;
#9183 = AXIS2_PLACEMENT_3D('',#195416,#10694,#10695) ;
#9184 = AXIS2_PLACEMENT_3D('',#195417,#10696,#10697) ;
#9185 = AXIS2_PLACEMENT_3D('',#195423,#10701,#10702) ;
#9186 = AXIS2_PLACEMENT_3D('',#195440,#10706,#10707) ;
#9187 = AXIS2_PLACEMENT_3D('',#195443,#10709,#10710) ;
#9188 = AXIS2_PLACEMENT_3D('',#195444,#10711,#10712) ;
#9189 = AXIS2_PLACEMENT_3D('',#195450,#10716,#10717) ;
#9190 = AXIS2_PLACEMENT_3D('',#195467,#10721,#10722) ;
#9191 = AXIS2_PLACEMENT_3D('',#195470,#10724,#10725) ;
#9192 = AXIS2_PLACEMENT_3D('',#195471,#10726,#10727) ;
#9193 = AXIS2_PLACEMENT_3D('',#195477,#10731,#10732) ;
#9194 = AXIS2_PLACEMENT_3D('',#195494,#10736,#10737) ;
#9195 = AXIS2_PLACEMENT_3D('',#195497,#10739,#10740) ;
#9196 = AXIS2_PLACEMENT_3D('',#195498,#10741,#10742) ;
#9197 = AXIS2_PLACEMENT_3D('',#195504,#10746,#10747) ;
#9198 = AXIS2_PLACEMENT_3D('',#195521,#10751,#10752) ;
#9199 = AXIS2_PLACEMENT_3D('',#195524,#10754,#10755) ;
#9200 = AXIS2_PLACEMENT_3D('',#195525,#10756,#10757) ;
#9201 = AXIS2_PLACEMENT_3D('',#195531,#10761,#10762) ;
#9202 = AXIS2_PLACEMENT_3D('',#195548,#10766,#10767) ;
#9203 = AXIS2_PLACEMENT_3D('',#195551,#10769,#10770) ;
#9204 = AXIS2_PLACEMENT_3D('',#195552,#10771,#10772) ;
#9205 = AXIS2_PLACEMENT_3D('',#195558,#10776,#10777) ;
#9206 = AXIS2_PLACEMENT_3D('',#195575,#10781,#10782) ;
#9207 = AXIS2_PLACEMENT_3D('',#195578,#10784,#10785) ;
#9208 = AXIS2_PLACEMENT_3D('',#195579,#10786,#10787) ;
#9209 = AXIS2_PLACEMENT_3D('',#195585,#10791,#10792) ;
#9210 = AXIS2_PLACEMENT_3D('',#195602,#10796,#10797) ;
#9211 = AXIS2_PLACEMENT_3D('',#195605,#10799,#10800) ;
#9212 = AXIS2_PLACEMENT_3D('',#195606,#10801,#10802) ;
#9213 = AXIS2_PLACEMENT_3D('',#195612,#10806,#10807) ;
#9214 = AXIS2_PLACEMENT_3D('',#195629,#10811,#10812) ;
#9215 = AXIS2_PLACEMENT_3D('',#195632,#10814,#10815) ;
#9216 = AXIS2_PLACEMENT_3D('',#195633,#10816,#10817) ;
#9217 = AXIS2_PLACEMENT_3D('',#195639,#10821,#10822) ;
#9218 = AXIS2_PLACEMENT_3D('',#195656,#10826,#10827) ;
#9219 = AXIS2_PLACEMENT_3D('',#195659,#10829,#10830) ;
#9220 = AXIS2_PLACEMENT_3D('',#195660,#10831,#10832) ;
#9221 = AXIS2_PLACEMENT_3D('',#195666,#10836,#10837) ;
#9222 = AXIS2_PLACEMENT_3D('',#195683,#10841,#10842) ;
#9223 = AXIS2_PLACEMENT_3D('',#195686,#10844,#10845) ;
#9224 = AXIS2_PLACEMENT_3D('',#195687,#10846,#10847) ;
#9225 = AXIS2_PLACEMENT_3D('',#195693,#10851,#10852) ;
#9226 = AXIS2_PLACEMENT_3D('',#195710,#10856,#10857) ;
#9227 = AXIS2_PLACEMENT_3D('',#195713,#10859,#10860) ;
#9228 = AXIS2_PLACEMENT_3D('',#195714,#10861,#10862) ;
#9229 = AXIS2_PLACEMENT_3D('',#195720,#10866,#10867) ;
#9230 = AXIS2_PLACEMENT_3D('',#195737,#10871,#10872) ;
#9231 = AXIS2_PLACEMENT_3D('',#195740,#10874,#10875) ;
#9232 = AXIS2_PLACEMENT_3D('',#195741,#10876,#10877) ;
#9233 = AXIS2_PLACEMENT_3D('',#195747,#10881,#10882) ;
#9234 = AXIS2_PLACEMENT_3D('',#195764,#10886,#10887) ;
#9235 = AXIS2_PLACEMENT_3D('',#195767,#10889,#10890) ;
#9236 = AXIS2_PLACEMENT_3D('',#195768,#10891,#10892) ;
#9237 = AXIS2_PLACEMENT_3D('',#195774,#10896,#10897) ;
#9238 = AXIS2_PLACEMENT_3D('',#195791,#10901,#10902) ;
#9239 = AXIS2_PLACEMENT_3D('',#195794,#10904,#10905) ;
#9240 = AXIS2_PLACEMENT_3D('',#195795,#10906,#10907) ;
#9241 = AXIS2_PLACEMENT_3D('',#195801,#10911,#10912) ;
#9242 = AXIS2_PLACEMENT_3D('',#195818,#10916,#10917) ;
#9243 = AXIS2_PLACEMENT_3D('',#195821,#10919,#10920) ;
#9244 = AXIS2_PLACEMENT_3D('',#195822,#10921,#10922) ;
#9245 = AXIS2_PLACEMENT_3D('',#195828,#10926,#10927) ;
#9246 = AXIS2_PLACEMENT_3D('',#195845,#10931,#10932) ;
#9247 = AXIS2_PLACEMENT_3D('',#195848,#10934,#10935) ;
#9248 = AXIS2_PLACEMENT_3D('',#195849,#10936,#10937) ;
#9249 = AXIS2_PLACEMENT_3D('',#195855,#10941,#10942) ;
#9250 = AXIS2_PLACEMENT_3D('',#195872,#10946,#10947) ;
#9251 = AXIS2_PLACEMENT_3D('',#195875,#10949,#10950) ;
#9252 = AXIS2_PLACEMENT_3D('',#195876,#10951,#10952) ;
#9253 = AXIS2_PLACEMENT_3D('',#195882,#10956,#10957) ;
#9254 = AXIS2_PLACEMENT_3D('',#195899,#10961,#10962) ;
#9255 = AXIS2_PLACEMENT_3D('',#195902,#10964,#10965) ;
#9256 = AXIS2_PLACEMENT_3D('',#195903,#10966,#10967) ;
#9257 = AXIS2_PLACEMENT_3D('',#195909,#10971,#10972) ;
#9258 = AXIS2_PLACEMENT_3D('',#195926,#10976,#10977) ;
#9259 = AXIS2_PLACEMENT_3D('',#195929,#10979,#10980) ;
#9260 = AXIS2_PLACEMENT_3D('',#195930,#10981,#10982) ;
#9261 = AXIS2_PLACEMENT_3D('',#195936,#10986,#10987) ;
#9262 = AXIS2_PLACEMENT_3D('',#195953,#10991,#10992) ;
#9263 = AXIS2_PLACEMENT_3D('',#195956,#10994,#10995) ;
#9264 = AXIS2_PLACEMENT_3D('',#195957,#10996,#10997) ;
#9265 = AXIS2_PLACEMENT_3D('',#195963,#11001,#11002) ;
#9266 = AXIS2_PLACEMENT_3D('',#195980,#11006,#11007) ;
#9267 = AXIS2_PLACEMENT_3D('',#195983,#11009,#11010) ;
#9268 = AXIS2_PLACEMENT_3D('',#195984,#11011,#11012) ;
#9269 = AXIS2_PLACEMENT_3D('',#195990,#11016,#11017) ;
#9270 = AXIS2_PLACEMENT_3D('',#196007,#11021,#11022) ;
#9271 = AXIS2_PLACEMENT_3D('',#196010,#11024,#11025) ;
#9272 = AXIS2_PLACEMENT_3D('',#196011,#11026,#11027) ;
#9273 = AXIS2_PLACEMENT_3D('',#196017,#11031,#11032) ;
#9274 = AXIS2_PLACEMENT_3D('',#196034,#11036,#11037) ;
#9275 = AXIS2_PLACEMENT_3D('',#196037,#11039,#11040) ;
#9276 = AXIS2_PLACEMENT_3D('',#196038,#11041,#11042) ;
#9277 = AXIS2_PLACEMENT_3D('',#196044,#11046,#11047) ;
#9278 = AXIS2_PLACEMENT_3D('',#196061,#11051,#11052) ;
#9279 = AXIS2_PLACEMENT_3D('',#196064,#11054,#11055) ;
#9280 = AXIS2_PLACEMENT_3D('',#196065,#11056,#11057) ;
#9281 = AXIS2_PLACEMENT_3D('',#196071,#11061,#11062) ;
#9282 = AXIS2_PLACEMENT_3D('',#196088,#11066,#11067) ;
#9283 = AXIS2_PLACEMENT_3D('',#196091,#11069,#11070) ;
#9284 = AXIS2_PLACEMENT_3D('',#196092,#11071,#11072) ;
#9285 = AXIS2_PLACEMENT_3D('',#196098,#11076,#11077) ;
#9286 = AXIS2_PLACEMENT_3D('',#196115,#11081,#11082) ;
#9287 = AXIS2_PLACEMENT_3D('',#196118,#11084,#11085) ;
#9288 = AXIS2_PLACEMENT_3D('',#196119,#11086,#11087) ;
#9289 = AXIS2_PLACEMENT_3D('',#196125,#11091,#11092) ;
#9290 = AXIS2_PLACEMENT_3D('',#196142,#11096,#11097) ;
#9291 = AXIS2_PLACEMENT_3D('',#196145,#11099,#11100) ;
#9292 = AXIS2_PLACEMENT_3D('',#196146,#11101,#11102) ;
#9293 = AXIS2_PLACEMENT_3D('',#196152,#11106,#11107) ;
#9294 = AXIS2_PLACEMENT_3D('',#196169,#11111,#11112) ;
#9295 = AXIS2_PLACEMENT_3D('',#196172,#11114,#11115) ;
#9296 = AXIS2_PLACEMENT_3D('',#196173,#11116,#11117) ;
#9297 = AXIS2_PLACEMENT_3D('',#196179,#11121,#11122) ;
#9298 = AXIS2_PLACEMENT_3D('',#196196,#11126,#11127) ;
#9299 = AXIS2_PLACEMENT_3D('',#196199,#11129,#11130) ;
#9300 = AXIS2_PLACEMENT_3D('',#196200,#11131,#11132) ;
#9301 = AXIS2_PLACEMENT_3D('',#196206,#11136,#11137) ;
#9302 = AXIS2_PLACEMENT_3D('',#196223,#11141,#11142) ;
#9303 = AXIS2_PLACEMENT_3D('',#196226,#11144,#11145) ;
#9304 = AXIS2_PLACEMENT_3D('',#196227,#11146,#11147) ;
#9305 = AXIS2_PLACEMENT_3D('',#196233,#11151,#11152) ;
#9306 = AXIS2_PLACEMENT_3D('',#196250,#11156,#11157) ;
#9307 = AXIS2_PLACEMENT_3D('',#196253,#11159,#11160) ;
#9308 = AXIS2_PLACEMENT_3D('',#196254,#11161,#11162) ;
#9309 = AXIS2_PLACEMENT_3D('',#196260,#11166,#11167) ;
#9310 = AXIS2_PLACEMENT_3D('',#196277,#11171,#11172) ;
#9311 = AXIS2_PLACEMENT_3D('',#196280,#11174,#11175) ;
#9312 = AXIS2_PLACEMENT_3D('',#196281,#11176,#11177) ;
#9313 = AXIS2_PLACEMENT_3D('',#196287,#11181,#11182) ;
#9314 = AXIS2_PLACEMENT_3D('',#196304,#11186,#11187) ;
#9315 = AXIS2_PLACEMENT_3D('',#196307,#11189,#11190) ;
#9316 = AXIS2_PLACEMENT_3D('',#196308,#11191,#11192) ;
#9317 = AXIS2_PLACEMENT_3D('',#196314,#11196,#11197) ;
#9318 = AXIS2_PLACEMENT_3D('',#196331,#11201,#11202) ;
#9319 = AXIS2_PLACEMENT_3D('',#196334,#11204,#11205) ;
#9320 = AXIS2_PLACEMENT_3D('',#196335,#11206,#11207) ;
#9321 = AXIS2_PLACEMENT_3D('',#196341,#11211,#11212) ;
#9322 = AXIS2_PLACEMENT_3D('',#196358,#11216,#11217) ;
#9323 = AXIS2_PLACEMENT_3D('',#196361,#11219,#11220) ;
#9324 = AXIS2_PLACEMENT_3D('',#196362,#11221,#11222) ;
#9325 = AXIS2_PLACEMENT_3D('',#196368,#11226,#11227) ;
#9326 = AXIS2_PLACEMENT_3D('',#196385,#11231,#11232) ;
#9327 = AXIS2_PLACEMENT_3D('',#196388,#11234,#11235) ;
#9328 = AXIS2_PLACEMENT_3D('',#196389,#11236,#11237) ;
#9329 = AXIS2_PLACEMENT_3D('',#196395,#11241,#11242) ;
#9330 = AXIS2_PLACEMENT_3D('',#196412,#11246,#11247) ;
#9331 = AXIS2_PLACEMENT_3D('',#196415,#11249,#11250) ;
#9332 = AXIS2_PLACEMENT_3D('',#196416,#11251,#11252) ;
#9333 = AXIS2_PLACEMENT_3D('',#196422,#11256,#11257) ;
#9334 = AXIS2_PLACEMENT_3D('',#196439,#11261,#11262) ;
#9335 = AXIS2_PLACEMENT_3D('',#196442,#11264,#11265) ;
#9336 = AXIS2_PLACEMENT_3D('',#196443,#11266,#11267) ;
#9337 = AXIS2_PLACEMENT_3D('',#196449,#11271,#11272) ;
#9338 = AXIS2_PLACEMENT_3D('',#196466,#11276,#11277) ;
#9339 = AXIS2_PLACEMENT_3D('',#196469,#11279,#11280) ;
#9340 = AXIS2_PLACEMENT_3D('',#196470,#11281,#11282) ;
#9341 = AXIS2_PLACEMENT_3D('',#196473,#11285,#11286) ;
#9342 = AXIS2_PLACEMENT_3D('',#196478,#11288,#11289) ;
#9343 = AXIS2_PLACEMENT_3D('',#196480,#11290,#11291) ;
#9344 = AXIS2_PLACEMENT_3D('',#196482,#11292,#11293) ;
#9345 = AXIS2_PLACEMENT_3D('',#196486,#11295,#11296) ;
#9346 = AXIS2_PLACEMENT_3D('',#196488,#11297,#11298) ;
#9347 = AXIS2_PLACEMENT_3D('',#196489,#11299,#11300) ;
#9348 = AXIS2_PLACEMENT_3D('',#196491,#11301,#11302) ;
#9349 = AXIS2_PLACEMENT_3D('',#196496,#11304,#11305) ;
#9350 = AXIS2_PLACEMENT_3D('',#196498,#11306,#11307) ;
#9351 = AXIS2_PLACEMENT_3D('',#196500,#11308,#11309) ;
#9352 = AXIS2_PLACEMENT_3D('',#196504,#11311,#11312) ;
#9353 = AXIS2_PLACEMENT_3D('',#196506,#11313,#11314) ;
#9354 = AXIS2_PLACEMENT_3D('',#196507,#11315,#11316) ;
#9355 = AXIS2_PLACEMENT_3D('',#196512,#11318,#11319) ;
#9356 = AXIS2_PLACEMENT_3D('',#196514,#11320,#11321) ;
#9357 = AXIS2_PLACEMENT_3D('',#196516,#11322,#11323) ;
#9358 = AXIS2_PLACEMENT_3D('',#196520,#11325,#11326) ;
#9359 = AXIS2_PLACEMENT_3D('',#196522,#11327,#11328) ;
#9360 = AXIS2_PLACEMENT_3D('',#196523,#11329,#11330) ;
#9361 = AXIS2_PLACEMENT_3D('',#196528,#11332,#11333) ;
#9362 = AXIS2_PLACEMENT_3D('',#196530,#11334,#11335) ;
#9363 = AXIS2_PLACEMENT_3D('',#196532,#11336,#11337) ;
#9364 = AXIS2_PLACEMENT_3D('',#196536,#11339,#11340) ;
#9365 = AXIS2_PLACEMENT_3D('',#196538,#11341,#11342) ;
#9366 = AXIS2_PLACEMENT_3D('',#196539,#11343,#11344) ;
#9367 = AXIS2_PLACEMENT_3D('',#196544,#11346,#11347) ;
#9368 = AXIS2_PLACEMENT_3D('',#196546,#11348,#11349) ;
#9369 = AXIS2_PLACEMENT_3D('',#196548,#11350,#11351) ;
#9370 = AXIS2_PLACEMENT_3D('',#196552,#11353,#11354) ;
#9371 = AXIS2_PLACEMENT_3D('',#196554,#11355,#11356) ;
#9372 = AXIS2_PLACEMENT_3D('',#196555,#11357,#11358) ;
#9373 = AXIS2_PLACEMENT_3D('',#196556,#11359,#11360) ;
#9374 = AXIS2_PLACEMENT_3D('',#196558,#11361,#11362) ;
#9375 = AXIS2_PLACEMENT_3D('',#196559,#11363,#11364) ;
#9376 = AXIS2_PLACEMENT_3D('',#196563,#11366,#11367) ;
#9377 = AXIS2_PLACEMENT_3D('',#196565,#11369,#11370) ;
#9378 = AXIS2_PLACEMENT_3D('',#196567,#11371,#11372) ;
#9379 = AXIS2_PLACEMENT_3D('',#196569,#11374,#11375) ;
#9380 = AXIS2_PLACEMENT_3D('',#196573,#11378,#11379) ;
#9381 = AXIS2_PLACEMENT_3D('',#196575,#11380,#11381) ;
#9382 = AXIS2_PLACEMENT_3D('',#196577,#11383,#11384) ;
#9383 = AXIS2_PLACEMENT_3D('',#196579,#11385,#11386) ;
#9384 = AXIS2_PLACEMENT_3D('',#196581,#11388,#11389) ;
#9385 = AXIS2_PLACEMENT_3D('',#196583,#11390,#11391) ;
#9386 = AXIS2_PLACEMENT_3D('',#196585,#11393,#11394) ;
#9387 = AXIS2_PLACEMENT_3D('',#196589,#11397,#11398) ;
#9388 = AXIS2_PLACEMENT_3D('',#196590,#11399,#11400) ;
#9389 = AXIS2_PLACEMENT_3D('',#196591,#11401,#11402) ;
#9390 = AXIS2_PLACEMENT_3D('',#196593,#11403,#11404) ;
#9391 = AXIS2_PLACEMENT_3D('',#196595,#11406,#11407) ;
#9392 = AXIS2_PLACEMENT_3D('',#196599,#11409,#11410) ;
#9393 = AXIS2_PLACEMENT_3D('',#196601,#11412,#11413) ;
#9394 = AXIS2_PLACEMENT_3D('',#196603,#11414,#11415) ;
#9395 = AXIS2_PLACEMENT_3D('',#196605,#11417,#11418) ;
#9396 = AXIS2_PLACEMENT_3D('',#196609,#11421,#11422) ;
#9397 = AXIS2_PLACEMENT_3D('',#196611,#11423,#11424) ;
#9398 = AXIS2_PLACEMENT_3D('',#196613,#11426,#11427) ;
#9399 = AXIS2_PLACEMENT_3D('',#196615,#11428,#11429) ;
#9400 = AXIS2_PLACEMENT_3D('',#196617,#11431,#11432) ;
#9401 = AXIS2_PLACEMENT_3D('',#196619,#11433,#11434) ;
#9402 = AXIS2_PLACEMENT_3D('',#196621,#11436,#11437) ;
#9403 = AXIS2_PLACEMENT_3D('',#196625,#11440,#11441) ;
#9404 = AXIS2_PLACEMENT_3D('',#196626,#11442,#11443) ;
#9405 = AXIS2_PLACEMENT_3D('',#196627,#11444,#11445) ;
#9406 = AXIS2_PLACEMENT_3D('',#196631,#11447,#11448) ;
#9407 = AXIS2_PLACEMENT_3D('',#196633,#11450,#11451) ;
#9408 = AXIS2_PLACEMENT_3D('',#196635,#11452,#11453) ;
#9409 = AXIS2_PLACEMENT_3D('',#196637,#11455,#11456) ;
#9410 = AXIS2_PLACEMENT_3D('',#196641,#11459,#11460) ;
#9411 = AXIS2_PLACEMENT_3D('',#196643,#11461,#11462) ;
#9412 = AXIS2_PLACEMENT_3D('',#196645,#11464,#11465) ;
#9413 = AXIS2_PLACEMENT_3D('',#196647,#11466,#11467) ;
#9414 = AXIS2_PLACEMENT_3D('',#196649,#11469,#11470) ;
#9415 = AXIS2_PLACEMENT_3D('',#196651,#11471,#11472) ;
#9416 = AXIS2_PLACEMENT_3D('',#196653,#11474,#11475) ;
#9417 = AXIS2_PLACEMENT_3D('',#196657,#11478,#11479) ;
#9418 = AXIS2_PLACEMENT_3D('',#196658,#11480,#11481) ;
#9419 = AXIS2_PLACEMENT_3D('',#196659,#11482,#11483) ;
#9420 = AXIS2_PLACEMENT_3D('',#196663,#11485,#11486) ;
#9421 = AXIS2_PLACEMENT_3D('',#196665,#11488,#11489) ;
#9422 = AXIS2_PLACEMENT_3D('',#196667,#11490,#11491) ;
#9423 = AXIS2_PLACEMENT_3D('',#196669,#11493,#11494) ;
#9424 = AXIS2_PLACEMENT_3D('',#196673,#11497,#11498) ;
#9425 = AXIS2_PLACEMENT_3D('',#196675,#11499,#11500) ;
#9426 = AXIS2_PLACEMENT_3D('',#196677,#11502,#11503) ;
#9427 = AXIS2_PLACEMENT_3D('',#196679,#11504,#11505) ;
#9428 = AXIS2_PLACEMENT_3D('',#196681,#11507,#11508) ;
#9429 = AXIS2_PLACEMENT_3D('',#196683,#11509,#11510) ;
#9430 = AXIS2_PLACEMENT_3D('',#196685,#11512,#11513) ;
#9431 = AXIS2_PLACEMENT_3D('',#196689,#11516,#11517) ;
#9432 = AXIS2_PLACEMENT_3D('',#196690,#11518,#11519) ;
#9433 = AXIS2_PLACEMENT_3D('',#196691,#11520,#11521) ;
#9434 = AXIS2_PLACEMENT_3D('',#196695,#11523,#11524) ;
#9435 = AXIS2_PLACEMENT_3D('',#196697,#11526,#11527) ;
#9436 = AXIS2_PLACEMENT_3D('',#196699,#11528,#11529) ;
#9437 = AXIS2_PLACEMENT_3D('',#196701,#11531,#11532) ;
#9438 = AXIS2_PLACEMENT_3D('',#196705,#11535,#11536) ;
#9439 = AXIS2_PLACEMENT_3D('',#196707,#11537,#11538) ;
#9440 = AXIS2_PLACEMENT_3D('',#196709,#11540,#11541) ;
#9441 = AXIS2_PLACEMENT_3D('',#196711,#11542,#11543) ;
#9442 = AXIS2_PLACEMENT_3D('',#196713,#11545,#11546) ;
#9443 = AXIS2_PLACEMENT_3D('',#196715,#11547,#11548) ;
#9444 = AXIS2_PLACEMENT_3D('',#196717,#11550,#11551) ;
#9445 = AXIS2_PLACEMENT_3D('',#196721,#11554,#11555) ;
#9446 = AXIS2_PLACEMENT_3D('',#196722,#11556,#11557) ;
#9447 = AXIS2_PLACEMENT_3D('',#196723,#11558,#11559) ;
#9448 = AXIS2_PLACEMENT_3D('',#196726,#11561,#11562) ;
#9449 = AXIS2_PLACEMENT_3D('',#196727,#11563,#11564) ;
#9450 = AXIS2_PLACEMENT_3D('',#196729,#11565,#11566) ;
#9451 = AXIS2_PLACEMENT_3D('',#196732,#11568,#11569) ;
#9452 = AXIS2_PLACEMENT_3D('',#196733,#11570,#11571) ;
#9453 = AXIS2_PLACEMENT_3D('',#196734,#11572,#11573) ;
#9454 = AXIS2_PLACEMENT_3D('',#196735,#11574,#11575) ;
#9455 = DIRECTION('axis',(0.,0.,1.)) ;
#9456 = DIRECTION('refdir',(1.,0.,0.)) ;
#9459 = DIRECTION('center_axis',(-0.946101641249535,-2.18705461187032E-30,
-0.323869857234255)) ;
#9460 = DIRECTION('ref_axis',(1.6950188065742E-15,1.,0.)) ;
#9461 = DIRECTION('',(0.946101641249535,2.18705461187032E-30,0.323869857234254)) ;
#9462 = DIRECTION('center_axis',(-0.946101641249535,-1.74964368949631E-30,
-0.323869857234254)) ;
#9463 = DIRECTION('ref_axis',(-1.69501880657431E-15,-1.,0.)) ;
#9464 = DIRECTION('',(0.946101641249535,1.74964368949631E-30,0.323869857234254)) ;
#9465 = DIRECTION('',(-0.668996284986547,0.707106781199264,-0.229006486057089)) ;
#9466 = DIRECTION('',(0.66899348741416,0.707106781186561,0.229014658477182)) ;
#9467 = DIRECTION('',(-0.668996284988301,-0.707106781199269,-0.229006486051948)) ;
#9468 = DIRECTION('',(0.668993487414155,-0.707106781186567,0.22901465847718)) ;
#9469 = DIRECTION('center_axis',(0.,1.,0.)) ;
#9470 = DIRECTION('ref_axis',(-0.21434215188659,0.,-0.976758640568194)) ;
#9471 = DIRECTION('center_axis',(0.,-1.,0.)) ;
#9472 = DIRECTION('ref_axis',(0.742040051540844,0.,0.670355548876312)) ;
#9473 = DIRECTION('',(0.,-1.,0.)) ;
#9474 = DIRECTION('center_axis',(0.,-1.,0.)) ;
#9475 = DIRECTION('ref_axis',(0.742040051540844,0.,0.670355548876312)) ;
#9476 = DIRECTION('center_axis',(0.,1.,0.)) ;
#9477 = DIRECTION('ref_axis',(0.,0.,1.)) ;
#9478 = DIRECTION('center_axis',(0.,-1.,0.)) ;
#9479 = DIRECTION('ref_axis',(0.,0.,-1.)) ;
#9480 = DIRECTION('',(-0.151562789093119,0.707106781186684,-0.690672658328185)) ;
#9481 = DIRECTION('',(-0.15156278909311,-0.707106781186643,-0.690672658328229)) ;
#9482 = DIRECTION('center_axis',(0.,1.,0.)) ;
#9483 = DIRECTION('ref_axis',(-0.946103896364967,0.,-0.323863269425582)) ;
#9484 = DIRECTION('',(0.,-1.,0.)) ;
#9485 = DIRECTION('center_axis',(1.35769304206411E-14,-1.,2.27077106269489E-14)) ;
#9486 = DIRECTION('ref_axis',(-0.0146228552552955,-2.30926389116428E-14,-0.999893080336184)) ;
#9487 = DIRECTION('center_axis',(0.,1.,0.)) ;
#9488 = DIRECTION('ref_axis',(-0.946103896364967,0.,-0.323863269425582)) ;
#9489 = DIRECTION('',(0.,-1.,0.)) ;
#9490 = DIRECTION('center_axis',(0.,1.,0.)) ;
#9491 = DIRECTION('ref_axis',(-0.946103896364967,0.,-0.323863269425582)) ;
#9492 = DIRECTION('',(0.,-1.,0.)) ;
#9493 = DIRECTION('center_axis',(0.,1.,0.)) ;
#9494 = DIRECTION('ref_axis',(-0.946103896364967,0.,-0.323863269425582)) ;
#9495 = DIRECTION('',(0.,-1.,0.)) ;
#9496 = DIRECTION('center_axis',(0.,1.,0.)) ;
#9497 = DIRECTION('ref_axis',(-0.946103896364967,0.,-0.323863269425582)) ;
#9498 = DIRECTION('',(0.,-1.,0.)) ;
#9499 = DIRECTION('center_axis',(0.,-1.,0.)) ;
#9500 = DIRECTION('ref_axis',(0.94610389636497,0.,0.323863269425573)) ;
#9501 = DIRECTION('',(0.,1.,0.)) ;
#9502 = DIRECTION('center_axis',(-1.2327844441336E-14,1.,4.81473066124874E-15)) ;
#9503 = DIRECTION('ref_axis',(0.624375708152623,1.06581410361413E-14,-0.781124173911492)) ;
#9504 = DIRECTION('center_axis',(0.,-1.,0.)) ;
#9505 = DIRECTION('ref_axis',(0.94610389636497,0.,0.323863269425573)) ;
#9506 = DIRECTION('',(0.,1.,0.)) ;
#9507 = DIRECTION('center_axis',(0.,-1.,0.)) ;
#9508 = DIRECTION('ref_axis',(0.94610389636497,0.,0.323863269425573)) ;
#9509 = DIRECTION('',(0.,1.,0.)) ;
#9510 = DIRECTION('center_axis',(0.,-1.,0.)) ;
#9511 = DIRECTION('ref_axis',(0.94610389636497,0.,0.323863269425573)) ;
#9512 = DIRECTION('',(0.,1.,0.)) ;
#9513 = DIRECTION('center_axis',(0.,-1.,0.)) ;
#9514 = DIRECTION('ref_axis',(0.94610389636497,0.,0.323863269425573)) ;
#9515 = DIRECTION('',(0.,1.,0.)) ;
#9516 = DIRECTION('center_axis',(0.,-1.,0.)) ;
#9517 = DIRECTION('ref_axis',(-0.999901327181056,0.,0.014047629748903)) ;
#9518 = DIRECTION('center_axis',(0.,1.,0.)) ;
#9519 = DIRECTION('ref_axis',(0.821908931733379,0.,0.569618914658647)) ;
#9520 = DIRECTION('',(0.,1.,0.)) ;
#9521 = DIRECTION('center_axis',(-5.43957754046731E-16,1.,-1.6588297649198E-16)) ;
#9522 = DIRECTION('ref_axis',(0.821908931733384,0.,0.569618914658641)) ;
#9523 = DIRECTION('center_axis',(0.,-1.,0.)) ;
#9524 = DIRECTION('ref_axis',(0.,0.,-1.)) ;
#9525 = DIRECTION('center_axis',(0.,1.,0.)) ;
#9526 = DIRECTION('ref_axis',(0.,0.,1.)) ;
#9527 = DIRECTION('',(-0.707037008967148,-0.707106781186553,0.00993317425505793)) ;
#9528 = DIRECTION('',(-0.707037008967142,0.707106781186558,0.00993317425505808)) ;
#9529 = DIRECTION('center_axis',(-8.17256413651962E-16,-1.,-6.22886289721765E-15)) ;
#9530 = DIRECTION('ref_axis',(-0.958163708642318,-9.99764261907128E-16,0.286220732024778)) ;
#9531 = DIRECTION('',(0.878436458273725,-0.399365905228251,-0.262404768471792)) ;
#9532 = DIRECTION('center_axis',(1.34449450164033E-15,1.,4.60237386928538E-16)) ;
#9533 = DIRECTION('ref_axis',(-0.946103896364975,1.42108547148575E-15,-0.32386326942556)) ;
#9534 = DIRECTION('center_axis',(1.34449450164033E-15,1.,4.60237386928538E-16)) ;
#9535 = DIRECTION('ref_axis',(-0.946103896364975,1.42108547148575E-15,-0.32386326942556)) ;
#9536 = DIRECTION('center_axis',(-2.00418059528623E-15,1.,-4.42697272393356E-15)) ;
#9537 = DIRECTION('ref_axis',(-0.958163708642327,-6.53241738270602E-16,0.286220732024745)) ;
#9538 = DIRECTION('center_axis',(-1.34449450164033E-15,1.,-4.60237386928538E-16)) ;
#9539 = DIRECTION('ref_axis',(-0.946103896364975,-1.42108547148575E-15,-0.32386326942556)) ;
#9540 = DIRECTION('',(-0.878436458273733,-0.399365905228253,0.262404768471762)) ;
#9541 = DIRECTION('center_axis',(-1.34449450164033E-15,1.,-4.60237386928538E-16)) ;
#9542 = DIRECTION('ref_axis',(-0.946103896364975,-1.42108547148575E-15,-0.32386326942556)) ;
#9543 = DIRECTION('center_axis',(0.,1.,0.)) ;
#9544 = DIRECTION('ref_axis',(0.,0.,1.)) ;
#9545 = DIRECTION('',(0.946101641249305,0.,0.323869857234926)) ;
#9546 = DIRECTION('center_axis',(-6.39729583226389E-16,-1.,-3.91154895135122E-16)) ;
#9547 = DIRECTION('ref_axis',(0.996177335286308,-1.42108547148575E-15,0.0873539733605267)) ;
#9548 = DIRECTION('',(0.946101641249524,1.83728335216313E-14,0.323869857234287)) ;
#9549 = DIRECTION('center_axis',(0.,-1.,0.)) ;
#9550 = DIRECTION('ref_axis',(0.94610389636497,0.,0.323863269425573)) ;
#9551 = DIRECTION('center_axis',(0.,1.,0.)) ;
#9552 = DIRECTION('ref_axis',(0.,0.,1.)) ;
#9553 = DIRECTION('',(-0.946101641249542,0.,-0.323869857234233)) ;
#9554 = DIRECTION('center_axis',(8.666064370551E-16,-1.,-2.17100603559229E-15)) ;
#9555 = DIRECTION('ref_axis',(-0.85456353911045,-2.84217094297147E-15,0.51934685675666)) ;
#9556 = DIRECTION('center_axis',(0.,1.,0.)) ;
#9557 = DIRECTION('ref_axis',(-0.946103896364967,0.,-0.323863269425582)) ;
#9558 = DIRECTION('center_axis',(0.,1.,0.)) ;
#9559 = DIRECTION('ref_axis',(-0.946103896364967,0.,-0.323863269425582)) ;
#9560 = DIRECTION('center_axis',(-8.0112472999825E-16,-1.,2.45282936024342E-15)) ;
#9561 = DIRECTION('ref_axis',(-0.996179841145295,0.,-0.087325392044553)) ;
#9562 = DIRECTION('center_axis',(4.89721590946324E-33,-1.,-1.43059439030947E-32)) ;
#9563 = DIRECTION('ref_axis',(-0.840728824371145,0.,-0.541456409945908)) ;
#9564 = DIRECTION('',(0.,-1.,0.)) ;
#9565 = DIRECTION('center_axis',(0.,-1.,0.)) ;
#9566 = DIRECTION('ref_axis',(0.,0.,-1.)) ;
#9567 = DIRECTION('',(0.946101641249514,1.10210091516262E-14,0.323869857234315)) ;
#9568 = DIRECTION('center_axis',(0.,-1.,0.)) ;
#9569 = DIRECTION('ref_axis',(0.,0.,-1.)) ;
#9570 = DIRECTION('',(-0.946101641249307,0.,-0.32386985723492)) ;
#9571 = DIRECTION('',(-0.946101641249533,0.,-0.323869857234259)) ;
#9572 = DIRECTION('center_axis',(0.,-1.,0.)) ;
#9573 = DIRECTION('ref_axis',(0.94610389636497,0.,0.323863269425573)) ;
#9574 = DIRECTION('',(0.,1.,0.)) ;
#9575 = DIRECTION('center_axis',(-0.946101641249535,-2.18705461187032E-30,
-0.323869857234255)) ;
#9576 = DIRECTION('ref_axis',(1.6950188065742E-15,1.,0.)) ;
#9577 = DIRECTION('',(0.946101641249535,2.18705461187032E-30,0.323869857234254)) ;
#9578 = DIRECTION('',(-0.668994874693665,0.707106793246477,-0.229010568704352)) ;
#9579 = DIRECTION('center_axis',(-0.946101641249535,-2.18705461187032E-30,
-0.323869857234255)) ;
#9580 = DIRECTION('ref_axis',(1.6950188065742E-15,1.,0.)) ;
#9581 = DIRECTION('',(0.946101641249535,2.18705461187032E-30,0.323869857234254)) ;
#9582 = DIRECTION('',(0.668994876573621,0.707106791113638,0.229010569798033)) ;
#9583 = DIRECTION('center_axis',(-0.946101641249535,-1.74964368949631E-30,
-0.323869857234254)) ;
#9584 = DIRECTION('ref_axis',(-1.69501880657431E-15,-1.,0.)) ;
#9585 = DIRECTION('',(0.946101641249535,1.74964368949631E-30,0.323869857234254)) ;
#9586 = DIRECTION('center_axis',(-0.946101641249535,-1.74964368949631E-30,
-0.323869857234254)) ;
#9587 = DIRECTION('ref_axis',(-1.69501880657431E-15,-1.,0.)) ;
#9588 = DIRECTION('',(0.946101641249535,1.74964368949631E-30,0.323869857234254)) ;
#9589 = DIRECTION('',(-0.668994882500867,-0.707106785016779,-0.229010571308153)) ;
#9590 = DIRECTION('',(0.668994877081364,-0.707106791113096,0.229010568316467)) ;
#9591 = DIRECTION('center_axis',(0.946101641249535,-1.74964368949631E-30,
0.323869857234254)) ;
#9592 = DIRECTION('ref_axis',(-1.69501880657431E-15,1.,0.)) ;
#9593 = DIRECTION('center_axis',(0.946101641249537,1.59018832135268E-14,0.323869857234249)) ;
#9594 = DIRECTION('ref_axis',(0.188203553203261,0.813826036051114,-0.549787782336964)) ;
#9595 = DIRECTION('',(-0.946101641249535,1.74964368949631E-30,-0.323869857234254)) ;
#9596 = DIRECTION('center_axis',(-0.946101641249539,-4.86663357488556E-15,
-0.323869857234242)) ;
#9597 = DIRECTION('ref_axis',(-0.188203553203284,0.813826036051079,0.54978778233701)) ;
#9598 = DIRECTION('center_axis',(-0.946101641249539,-4.86663357488556E-15,
-0.323869857234242)) ;
#9599 = DIRECTION('ref_axis',(-0.188203553203284,0.813826036051079,0.54978778233701)) ;
#9600 = DIRECTION('center_axis',(0.946101641249535,0.,0.323869857234254)) ;
#9601 = DIRECTION('ref_axis',(0.323869857234254,0.,-0.946101641249535)) ;
#9602 = DIRECTION('center_axis',(-0.946101641249535,-1.97215226305253E-31,
-0.323869857234254)) ;
#9603 = DIRECTION('ref_axis',(-0.323869857234254,0.,0.946101641249535)) ;
#9604 = DIRECTION('',(-0.668994894197647,-0.707106772753729,-0.229010575003176)) ;
#9605 = DIRECTION('center_axis',(0.946101641249535,-1.74835062554578E-30,
0.323869857234255)) ;
#9606 = DIRECTION('ref_axis',(0.,1.,0.)) ;
#9607 = DIRECTION('center_axis',(-0.946101641249527,2.48640733553338E-14,
-0.323869857234278)) ;
#9608 = DIRECTION('ref_axis',(0.188203553203274,-0.813826036051078,-0.549787782337014)) ;
#9609 = DIRECTION('',(-0.946101641249535,1.74835062554578E-30,-0.323869857234255)) ;
#9610 = DIRECTION('center_axis',(-0.946101641249534,-2.31955132725112E-15,
-0.323869857234258)) ;
#9611 = DIRECTION('ref_axis',(0.188203553203289,-0.813826036051069,-0.549787782337023)) ;
#9612 = DIRECTION('center_axis',(-0.946101641249535,1.97215226305253E-31,
-0.323869857234254)) ;
#9613 = DIRECTION('ref_axis',(-0.323869857234254,0.,0.946101641249535)) ;
#9614 = DIRECTION('center_axis',(0.946101641249535,0.,0.323869857234254)) ;
#9615 = DIRECTION('ref_axis',(0.323869857234254,0.,-0.946101641249535)) ;
#9616 = DIRECTION('center_axis',(0.,-1.,0.)) ;
#9617 = DIRECTION('ref_axis',(-0.946101641249535,0.,-0.323869857234253)) ;
#9618 = DIRECTION('',(0.,1.,0.)) ;
#9619 = DIRECTION('center_axis',(3.75494695140922E-9,-1.,-3.24758869446514E-8)) ;
#9620 = DIRECTION('ref_axis',(0.389434122263594,3.1374361622722E-8,-0.921054322185605)) ;
#9621 = DIRECTION('center_axis',(0.,-1.,0.)) ;
#9622 = DIRECTION('ref_axis',(-0.946101641249535,0.,-0.323869857234253)) ;
#9623 = DIRECTION('',(0.,1.,0.)) ;
#9624 = DIRECTION('center_axis',(0.,-1.,0.)) ;
#9625 = DIRECTION('ref_axis',(-0.946101641249535,0.,-0.323869857234253)) ;
#9626 = DIRECTION('',(0.,1.,0.)) ;
#9627 = DIRECTION('center_axis',(0.,-1.,0.)) ;
#9628 = DIRECTION('ref_axis',(-0.946101641249535,0.,-0.323869857234253)) ;
#9629 = DIRECTION('',(0.,1.,0.)) ;
#9630 = DIRECTION('center_axis',(0.,-1.,0.)) ;
#9631 = DIRECTION('ref_axis',(-0.946101641249535,0.,-0.323869857234253)) ;
#9632 = DIRECTION('center_axis',(0.,-1.,0.)) ;
#9633 = DIRECTION('ref_axis',(-0.946101641249535,0.,-0.323869857234253)) ;
#9634 = DIRECTION('center_axis',(-2.38472166595684E-16,-1.,-1.12237188351893E-14)) ;
#9635 = DIRECTION('ref_axis',(-0.958165701602871,-2.98389028785182E-15,0.286214060227441)) ;
#9636 = DIRECTION('',(0.85700945699712,-0.447213595499954,-0.255997637913916)) ;
#9637 = DIRECTION('center_axis',(-1.89537453127107E-15,-1.,-3.74799467464299E-17)) ;
#9638 = DIRECTION('ref_axis',(-0.95816570160281,0.,0.286214060227646)) ;
#9639 = DIRECTION('center_axis',(-1.05069562641528E-15,1.,-5.42645984197838E-15)) ;
#9640 = DIRECTION('ref_axis',(-0.958165701602825,5.46388591979422E-16,0.286214060227598)) ;
#9641 = DIRECTION('',(-0.857009456997078,-0.447213595499957,0.255997637914053)) ;
#9642 = DIRECTION('center_axis',(-1.00269417211326E-16,-1.,-1.95454945674237E-15)) ;
#9643 = DIRECTION('ref_axis',(-0.95816570160282,-4.63344819438314E-16,0.286214060227614)) ;
#9644 = DIRECTION('center_axis',(1.81627551085956E-15,1.,1.3519073427862E-15)) ;
#9645 = DIRECTION('ref_axis',(-0.58175859519622,2.21012228981213E-15,-0.813361504446406)) ;
#9646 = DIRECTION('',(0.857009456997073,-0.447213595499959,-0.255997637914066)) ;
#9647 = DIRECTION('center_axis',(0.,1.,0.)) ;
#9648 = DIRECTION('ref_axis',(0.,0.,1.)) ;
#9649 = DIRECTION('',(0.946101641249534,0.,0.323869857234258)) ;
#9650 = DIRECTION('',(0.192571296739865,0.,0.981282984501376)) ;
#9651 = DIRECTION('',(-0.753530344509659,0.,0.657413127267136)) ;
#9652 = DIRECTION('',(-0.946101641249533,0.,-0.323869857234258)) ;
#9653 = DIRECTION('',(-0.192571296739865,0.,-0.981282984501376)) ;
#9654 = DIRECTION('',(0.753530344509681,0.,-0.65741312726711)) ;
#9655 = DIRECTION('center_axis',(-0.323869857234258,0.,0.946101641249534)) ;
#9656 = DIRECTION('ref_axis',(0.946101641249534,0.,0.323869857234258)) ;
#9657 = DIRECTION('',(0.,-1.,0.)) ;
#9658 = DIRECTION('',(0.946101641249534,0.,0.323869857234258)) ;
#9659 = DIRECTION('',(0.,-1.,0.)) ;
#9660 = DIRECTION('center_axis',(-0.981282984501376,0.,0.192571296739865)) ;
#9661 = DIRECTION('ref_axis',(0.192571296739865,0.,0.981282984501376)) ;
#9662 = DIRECTION('',(0.192571296739865,0.,0.981282984501376)) ;
#9663 = DIRECTION('',(0.,-1.,0.)) ;
#9664 = DIRECTION('center_axis',(-0.657413127267136,0.,-0.753530344509659)) ;
#9665 = DIRECTION('ref_axis',(-0.753530344509659,0.,0.657413127267136)) ;
#9666 = DIRECTION('',(-0.753530344509659,0.,0.657413127267136)) ;
#9667 = DIRECTION('',(0.,-1.,0.)) ;
#9668 = DIRECTION('center_axis',(0.323869857234259,0.,-0.946101641249534)) ;
#9669 = DIRECTION('ref_axis',(-0.946101641249533,0.,-0.323869857234259)) ;
#9670 = DIRECTION('',(-0.946101641249533,0.,-0.323869857234258)) ;
#9671 = DIRECTION('',(0.,-1.,0.)) ;
#9672 = DIRECTION('center_axis',(0.981282984501376,0.,-0.192571296739865)) ;
#9673 = DIRECTION('ref_axis',(-0.192571296739865,0.,-0.981282984501376)) ;
#9674 = DIRECTION('',(-0.192571296739865,0.,-0.981282984501376)) ;
#9675 = DIRECTION('',(0.,-1.,0.)) ;
#9676 = DIRECTION('center_axis',(0.65741312726711,0.,0.753530344509681)) ;
#9677 = DIRECTION('ref_axis',(0.753530344509681,0.,-0.65741312726711)) ;
#9678 = DIRECTION('',(0.753530344509681,0.,-0.65741312726711)) ;
#9679 = DIRECTION('center_axis',(0.,1.,0.)) ;
#9680 = DIRECTION('ref_axis',(0.,0.,1.)) ;
#9681 = DIRECTION('center_axis',(0.,1.,0.)) ;
#9682 = DIRECTION('ref_axis',(0.946101641249538,0.,0.323869857234247)) ;
#9683 = DIRECTION('',(0.,-1.,0.)) ;
#9684 = DIRECTION('center_axis',(1.69348985501441E-8,1.,-2.79641211295213E-8)) ;
#9685 = DIRECTION('ref_axis',(0.2567101959962,-3.13743616227142E-8,-0.96648842479959)) ;
#9686 = DIRECTION('center_axis',(0.,1.,0.)) ;
#9687 = DIRECTION('ref_axis',(0.946101641249538,0.,0.323869857234247)) ;
#9688 = DIRECTION('',(0.,-1.,0.)) ;
#9689 = DIRECTION('center_axis',(0.,1.,0.)) ;
#9690 = DIRECTION('ref_axis',(0.946101641249538,0.,0.323869857234247)) ;
#9691 = DIRECTION('',(0.,-1.,0.)) ;
#9692 = DIRECTION('center_axis',(0.,1.,0.)) ;
#9693 = DIRECTION('ref_axis',(0.946101641249538,0.,0.323869857234247)) ;
#9694 = DIRECTION('',(0.,-1.,0.)) ;
#9695 = DIRECTION('center_axis',(0.,1.,0.)) ;
#9696 = DIRECTION('ref_axis',(0.946101641249538,0.,0.323869857234247)) ;
#9697 = DIRECTION('center_axis',(0.,1.,0.)) ;
#9698 = DIRECTION('ref_axis',(0.946101641249538,0.,0.323869857234247)) ;
#9699 = DIRECTION('center_axis',(-3.54843881531938E-15,1.,8.31280498735044E-15)) ;
#9700 = DIRECTION('ref_axis',(0.581758595196255,-4.69698079034066E-15,0.813361504446381)) ;
#9701 = DIRECTION('center_axis',(4.35227724980002E-15,1.,-4.32131170149782E-15)) ;
#9702 = DIRECTION('ref_axis',(0.581758595196233,0.,0.813361504446397)) ;
#9703 = DIRECTION('',(0.520340706141445,-0.447213595499963,0.727492645689438)) ;
#9704 = DIRECTION('center_axis',(-1.26502582361951E-15,-1.,3.83372877494251E-15)) ;
#9705 = DIRECTION('ref_axis',(0.581758595196241,2.38226775799081E-15,0.813361504446391)) ;
#9706 = DIRECTION('',(-0.520340706141432,-0.447213595499961,-0.727492645689449)) ;
#9707 = DIRECTION('center_axis',(-1.40046452293039E-15,1.,-4.36789479033898E-15)) ;
#9708 = DIRECTION('ref_axis',(0.58175859519628,4.36740975141576E-15,0.813361504446363)) ;
#9709 = DIRECTION('',(0.520340706141466,-0.447213595499955,0.727492645689427)) ;
#9710 = DIRECTION('center_axis',(-2.26373725714479E-15,-1.,-4.47641088586434E-17)) ;
#9711 = DIRECTION('ref_axis',(0.958165701602815,-2.21012228981212E-15,-0.286214060227631)) ;
#9712 = DIRECTION('center_axis',(0.,-1.,0.)) ;
#9713 = DIRECTION('ref_axis',(0.,0.,-1.)) ;
#9714 = DIRECTION('',(-0.946101641249534,0.,-0.323869857234258)) ;
#9715 = DIRECTION('',(-0.753530344509683,0.,0.657413127267107)) ;
#9716 = DIRECTION('',(0.19257129673986,0.,0.981282984501377)) ;
#9717 = DIRECTION('',(0.946101641249533,0.,0.323869857234258)) ;
#9718 = DIRECTION('',(0.753530344509662,0.,-0.657413127267132)) ;
#9719 = DIRECTION('',(-0.192571296739863,0.,-0.981282984501376)) ;
#9720 = DIRECTION('center_axis',(-0.323869857234258,0.,0.946101641249534)) ;
#9721 = DIRECTION('ref_axis',(0.946101641249534,0.,0.323869857234258)) ;
#9722 = DIRECTION('',(0.,1.,0.)) ;
#9723 = DIRECTION('',(-0.946101641249534,0.,-0.323869857234258)) ;
#9724 = DIRECTION('',(0.,1.,0.)) ;
#9725 = DIRECTION('center_axis',(0.657413127267108,0.,0.753530344509683)) ;
#9726 = DIRECTION('ref_axis',(0.753530344509683,0.,-0.657413127267108)) ;
#9727 = DIRECTION('',(-0.753530344509683,0.,0.657413127267107)) ;
#9728 = DIRECTION('',(0.,1.,0.)) ;
#9729 = DIRECTION('center_axis',(0.981282984501377,0.,-0.19257129673986)) ;
#9730 = DIRECTION('ref_axis',(-0.19257129673986,0.,-0.981282984501377)) ;
#9731 = DIRECTION('',(0.19257129673986,0.,0.981282984501377)) ;
#9732 = DIRECTION('',(0.,1.,0.)) ;
#9733 = DIRECTION('center_axis',(0.323869857234256,0.,-0.946101641249534)) ;
#9734 = DIRECTION('ref_axis',(-0.946101641249534,0.,-0.323869857234256)) ;
#9735 = DIRECTION('',(0.946101641249534,0.,0.323869857234256)) ;
#9736 = DIRECTION('',(7.60950359874019E-15,1.,0.)) ;
#9737 = DIRECTION('center_axis',(-0.657413127267136,0.,-0.753530344509659)) ;
#9738 = DIRECTION('ref_axis',(-0.753530344509659,0.,0.657413127267136)) ;
#9739 = DIRECTION('',(0.753530344509659,0.,-0.657413127267136)) ;
#9740 = DIRECTION('',(0.,1.,0.)) ;
#9741 = DIRECTION('center_axis',(-0.981282984501376,0.,0.192571296739863)) ;
#9742 = DIRECTION('ref_axis',(0.192571296739863,0.,0.981282984501376)) ;
#9743 = DIRECTION('',(-0.192571296739863,0.,-0.981282984501376)) ;
#9744 = DIRECTION('center_axis',(0.,-1.,0.)) ;
#9745 = DIRECTION('ref_axis',(0.,0.,-1.)) ;
#9746 = DIRECTION('center_axis',(0.,1.,0.)) ;
#9747 = DIRECTION('ref_axis',(0.455018599800652,0.,-0.89048193346943)) ;
#9748 = DIRECTION('center_axis',(-2.55214171167663E-16,-1.,4.99460041171382E-16)) ;
#9749 = DIRECTION('ref_axis',(0.7484309423753,-5.40804574512742E-16,-0.66321272944299)) ;
#9750 = DIRECTION('',(0.,1.,0.)) ;
#9751 = DIRECTION('center_axis',(0.,-1.,0.)) ;
#9752 = DIRECTION('ref_axis',(0.7484309423753,0.,-0.66321272944299)) ;
#9753 = DIRECTION('',(0.,1.,0.)) ;
#9754 = DIRECTION('center_axis',(0.,-1.,0.)) ;
#9755 = DIRECTION('ref_axis',(0.946102418141935,0.,0.323867587736074)) ;
#9756 = DIRECTION('center_axis',(0.,1.,0.)) ;
#9757 = DIRECTION('ref_axis',(-0.184992222823419,0.,-0.982739984683055)) ;
#9758 = DIRECTION('',(0.,1.,0.)) ;
#9759 = DIRECTION('center_axis',(0.,1.,0.)) ;
#9760 = DIRECTION('ref_axis',(-0.184992222823419,0.,-0.982739984683055)) ;
#9761 = DIRECTION('center_axis',(0.,1.,0.)) ;
#9762 = DIRECTION('ref_axis',(-0.186143933560967,0.,0.982522486255887)) ;
#9763 = DIRECTION('center_axis',(0.,-1.,0.)) ;
#9764 = DIRECTION('ref_axis',(-0.531640234764764,0.,0.846970283291726)) ;
#9765 = DIRECTION('',(0.,1.,0.)) ;
#9766 = DIRECTION('center_axis',(-1.04405775373722E-16,-1.,5.5108442180881E-16)) ;
#9767 = DIRECTION('ref_axis',(-0.531640234764764,5.40804574512721E-16,0.846970283291726)) ;
#9768 = DIRECTION('center_axis',(0.,-1.,0.)) ;
#9769 = DIRECTION('ref_axis',(-0.946102418141937,0.,-0.323867587736067)) ;
#9770 = DIRECTION('center_axis',(0.,1.,0.)) ;
#9771 = DIRECTION('ref_axis',(-0.0989310419315636,0.,0.995094291483141)) ;
#9772 = DIRECTION('center_axis',(0.,1.,0.)) ;
#9773 = DIRECTION('ref_axis',(-0.0989310419315636,0.,0.995094291483141)) ;
#9774 = DIRECTION('center_axis',(0.,1.,0.)) ;
#9775 = DIRECTION('ref_axis',(-0.99990130540252,0.,0.014049179845692)) ;
#9776 = DIRECTION('center_axis',(-8.38487460979998E-16,-1.,-1.63767295998206E-15)) ;
#9777 = DIRECTION('ref_axis',(0.80558161685206,0.,-0.592484817181015)) ;
#9778 = DIRECTION('',(0.,-1.,0.)) ;
#9779 = DIRECTION('center_axis',(-2.99404737873291E-16,-1.,-1.81877242912888E-15)) ;
#9780 = DIRECTION('ref_axis',(0.80558161685206,1.11022302462515E-15,-0.592484817181015)) ;
#9781 = DIRECTION('center_axis',(0.,-1.,0.)) ;
#9782 = DIRECTION('ref_axis',(0.,0.,-1.)) ;
#9783 = DIRECTION('center_axis',(2.21922717480124E-16,-1.,-1.77769816013821E-16)) ;
#9784 = DIRECTION('ref_axis',(0.552511269382308,0.,-0.833505427220214)) ;
#9785 = DIRECTION('center_axis',(-9.60395777197369E-15,-1.,-3.28760405712621E-15)) ;
#9786 = DIRECTION('ref_axis',(-0.910070227772796,1.00819783257895E-14,-0.414454075286481)) ;
#9787 = DIRECTION('center_axis',(0.,-1.,0.)) ;
#9788 = DIRECTION('ref_axis',(-0.973142732923728,0.,-0.230202565923443)) ;
#9789 = DIRECTION('center_axis',(-1.22695023382735E-14,1.,-4.20006761299971E-15)) ;
#9790 = DIRECTION('ref_axis',(-0.973142645740024,-1.28801978463218E-14,-0.230202934477618)) ;
#9791 = DIRECTION('center_axis',(0.,-1.,0.)) ;
#9792 = DIRECTION('ref_axis',(0.91007020491951,0.,0.414454125468382)) ;
#9793 = DIRECTION('center_axis',(-7.59289697485827E-17,-1.,-2.8895302269988E-17)) ;
#9794 = DIRECTION('ref_axis',(0.998564477438101,0.,0.0535629013289298)) ;
#9795 = DIRECTION('center_axis',(-1.15689962621907E-15,-1.,-9.23506116525419E-16)) ;
#9796 = DIRECTION('ref_axis',(-0.623865270298613,0.,0.781531908827297)) ;
#9797 = DIRECTION('center_axis',(-1.66226250514315E-14,1.,1.46874856665111E-14)) ;
#9798 = DIRECTION('ref_axis',(-0.62386527029487,-2.17997072578483E-14,0.781531908830284)) ;
#9799 = DIRECTION('center_axis',(7.74016996102823E-16,-1.,1.26181600964286E-15)) ;
#9800 = DIRECTION('ref_axis',(0.852406595651028,0.,-0.522879523112757)) ;
#9801 = DIRECTION('center_axis',(1.14665281872477E-14,-1.,-1.01316426725251E-14)) ;
#9802 = DIRECTION('ref_axis',(-0.852406991796352,-1.50377410845894E-14,0.522878877309739)) ;
#9803 = DIRECTION('center_axis',(0.,1.,0.)) ;
#9804 = DIRECTION('ref_axis',(0.,0.,1.)) ;
#9805 = DIRECTION('center_axis',(0.,1.,0.)) ;
#9806 = DIRECTION('ref_axis',(-0.323867587734822,0.,0.946102418142364)) ;
#9807 = DIRECTION('center_axis',(0.,-1.,0.)) ;
#9808 = DIRECTION('ref_axis',(0.323867121549058,0.,-0.946102577725866)) ;
#9809 = DIRECTION('center_axis',(0.,-1.,0.)) ;
#9810 = DIRECTION('ref_axis',(-0.662139670450416,0.,-0.749380448647957)) ;
#9811 = DIRECTION('center_axis',(-3.40221204910911E-14,1.,3.00614012171144E-14)) ;
#9812 = DIRECTION('ref_axis',(0.662139806159003,-2.24593216937398E-20,0.749380328738163)) ;
#9813 = DIRECTION('center_axis',(0.,1.,0.)) ;
#9814 = DIRECTION('ref_axis',(-0.934005212398469,0.,0.357259378060941)) ;
#9815 = DIRECTION('center_axis',(0.,-1.,0.)) ;
#9816 = DIRECTION('ref_axis',(0.552511269382305,0.,-0.833505427220215)) ;
#9817 = DIRECTION('',(0.,-1.,0.)) ;
#9818 = DIRECTION('center_axis',(0.,1.,0.)) ;
#9819 = DIRECTION('ref_axis',(0.414453894976047,0.,-0.910070309887749)) ;
#9820 = DIRECTION('',(0.,1.,0.)) ;
#9821 = DIRECTION('',(0.,1.,-6.23283101543947E-15)) ;
#9822 = DIRECTION('center_axis',(0.,-1.,0.)) ;
#9823 = DIRECTION('ref_axis',(-0.946102418141937,0.,-0.323867587736067)) ;
#9824 = DIRECTION('',(0.,1.,6.23283101543947E-15)) ;
#9825 = DIRECTION('center_axis',(-2.45390046765453E-14,1.,-8.40013522599877E-15)) ;
#9826 = DIRECTION('ref_axis',(-0.973142645740026,-2.58220234335363E-14,-0.23020293447761)) ;
#9827 = DIRECTION('center_axis',(0.,1.,0.)) ;
#9828 = DIRECTION('ref_axis',(-0.23020275012694,0.,0.973142689349303)) ;
#9829 = DIRECTION('',(0.,1.,0.)) ;
#9830 = DIRECTION('center_axis',(0.,1.,0.)) ;
#9831 = DIRECTION('ref_axis',(-0.946102433711068,0.,-0.323867542254538)) ;
#9832 = DIRECTION('center_axis',(0.,1.,0.)) ;
#9833 = DIRECTION('ref_axis',(-0.781531908823211,0.,-0.623865270303732)) ;
#9834 = DIRECTION('center_axis',(0.,-1.,0.)) ;
#9835 = DIRECTION('ref_axis',(0.998564477438101,0.,0.0535629013289298)) ;
#9836 = DIRECTION('',(0.,-1.,0.)) ;
#9837 = DIRECTION('center_axis',(0.,1.,0.)) ;
#9838 = DIRECTION('ref_axis',(-0.749379940776913,0.,0.662140245236)) ;
#9839 = DIRECTION('',(0.,1.,0.)) ;
#9840 = DIRECTION('',(1.55820775385987E-15,1.,1.2465662030879E-14)) ;
#9841 = DIRECTION('center_axis',(0.,1.,0.)) ;
#9842 = DIRECTION('ref_axis',(-0.522879200211183,0.,-0.852406793723815)) ;
#9843 = DIRECTION('',(0.,1.,0.)) ;
#9844 = DIRECTION('center_axis',(-1.40492466406194E-15,-1.,-8.74807498650115E-16)) ;
#9845 = DIRECTION('ref_axis',(0.852406595651023,-7.40148683083545E-16,-0.522879523112765)) ;
#9846 = DIRECTION('center_axis',(0.,-1.,0.)) ;
#9847 = DIRECTION('ref_axis',(-0.749379997167278,0.,0.662140181415967)) ;
#9848 = DIRECTION('',(3.11641550771974E-15,1.,0.)) ;
#9849 = DIRECTION('center_axis',(1.21477315178064E-14,1.,-1.13769124036181E-14)) ;
#9850 = DIRECTION('ref_axis',(-0.623865270294834,1.64745879276906E-14,0.781531908830314)) ;
#9851 = DIRECTION('center_axis',(0.,1.,0.)) ;
#9852 = DIRECTION('ref_axis',(0.781531908809468,0.,0.623865270320947)) ;
#9853 = DIRECTION('',(0.660441423512288,0.70710677669281,-0.252620530567424)) ;
#9854 = DIRECTION('',(0.643516813504555,0.707106780936073,0.293063322664521)) ;
#9855 = DIRECTION('',(0.643516895788544,-0.707106780933182,0.293063141989894)) ;
#9856 = DIRECTION('',(-0.68811576949862,-0.70710677538888,-0.162778057386315)) ;
#9857 = DIRECTION('',(-0.688115800926617,0.7071067782106,-0.162777912272352)) ;
#9858 = DIRECTION('',(0.552626512834363,0.707106780687659,0.441139363487398)) ;
#9859 = DIRECTION('',(-0.602742728927109,0.707106778605105,0.369731262373379)) ;
#9860 = DIRECTION('',(0.441139312684097,-0.707106778989338,-0.552626555561643)) ;
#9861 = DIRECTION('',(0.602742658952527,0.707106777346419,-0.369731378854432)) ;
#9862 = DIRECTION('',(-0.441139363669859,-0.707106780410578,0.552626513043248)) ;
#9863 = DIRECTION('center_axis',(0.,-1.,0.)) ;
#9864 = DIRECTION('ref_axis',(-0.186143933560965,0.,0.982522486255888)) ;
#9865 = DIRECTION('center_axis',(0.,1.,0.)) ;
#9866 = DIRECTION('ref_axis',(0.184992222813461,0.,0.982739984684929)) ;
#9867 = DIRECTION('',(0.,-1.,0.)) ;
#9868 = DIRECTION('center_axis',(1.04405775373719E-16,1.,-5.51084421808798E-16)) ;
#9869 = DIRECTION('ref_axis',(0.184992222813461,5.40804574512736E-16,0.982739984684929)) ;
#9870 = DIRECTION('',(0.,-1.,0.)) ;
#9871 = DIRECTION('center_axis',(0.,1.,0.)) ;
#9872 = DIRECTION('ref_axis',(0.946102418141937,0.,0.323867587736069)) ;
#9873 = DIRECTION('center_axis',(0.,-1.,0.)) ;
#9874 = DIRECTION('ref_axis',(-0.748430942382017,0.,0.66321272943541)) ;
#9875 = DIRECTION('',(0.,-1.,0.)) ;
#9876 = DIRECTION('center_axis',(0.,-1.,0.)) ;
#9877 = DIRECTION('ref_axis',(-0.748430942382017,0.,0.66321272943541)) ;
#9878 = DIRECTION('center_axis',(0.,-1.,0.)) ;
#9879 = DIRECTION('ref_axis',(0.455018599800648,0.,-0.890481933469432)) ;
#9880 = DIRECTION('center_axis',(2.55214171167679E-16,1.,-4.99460041171418E-16)) ;
#9881 = DIRECTION('ref_axis',(0.0989310425378922,-5.40804574512704E-16,-0.995094291422861)) ;
#9882 = DIRECTION('',(0.,-1.,0.)) ;
#9883 = DIRECTION('center_axis',(2.55214171167679E-16,1.,-4.99460041171418E-16)) ;
#9884 = DIRECTION('ref_axis',(0.0989310425378922,-5.40804574512704E-16,-0.995094291422861)) ;
#9885 = DIRECTION('center_axis',(0.,1.,0.)) ;
#9886 = DIRECTION('ref_axis',(-0.946102418141937,0.,-0.323867587736068)) ;
#9887 = DIRECTION('center_axis',(0.,-1.,0.)) ;
#9888 = DIRECTION('ref_axis',(0.53164023528083,0.,-0.846970282967793)) ;
#9889 = DIRECTION('center_axis',(0.,-1.,0.)) ;
#9890 = DIRECTION('ref_axis',(0.53164023528083,0.,-0.846970282967793)) ;
#9891 = DIRECTION('center_axis',(0.,1.,0.)) ;
#9892 = DIRECTION('ref_axis',(0.,0.,1.)) ;
#9893 = DIRECTION('center_axis',(0.,1.,0.)) ;
#9894 = DIRECTION('ref_axis',(-0.0741867580339807,0.,0.997244365706023)) ;
#9895 = DIRECTION('center_axis',(-9.60395745588678E-15,1.,-3.2876049804992E-15)) ;
#9896 = DIRECTION('ref_axis',(-0.973142633081286,-1.00819783257896E-14,-0.230202987990212)) ;
#9897 = DIRECTION('center_axis',(0.,1.,0.)) ;
#9898 = DIRECTION('ref_axis',(-0.910070048017682,0.,-0.414454469997724)) ;
#9899 = DIRECTION('center_axis',(0.,-1.,0.)) ;
#9900 = DIRECTION('ref_axis',(-0.910070204982189,0.,-0.414454125330749)) ;
#9901 = DIRECTION('center_axis',(0.,1.,0.)) ;
#9902 = DIRECTION('ref_axis',(0.973142645774834,0.,0.230202934330464)) ;
#9903 = DIRECTION('center_axis',(-7.09105905758385E-17,1.,5.21847544066181E-16)) ;
#9904 = DIRECTION('ref_axis',(0.821909814783993,-3.1720657846433E-16,0.569617640493816)) ;
#9905 = DIRECTION('center_axis',(-1.48015126885593E-15,1.,2.07969639555734E-17)) ;
#9906 = DIRECTION('ref_axis',(-0.0140491798391936,0.,-0.999901305402611)) ;
#9907 = DIRECTION('center_axis',(0.,-1.,0.)) ;
#9908 = DIRECTION('ref_axis',(-0.0140491798343224,0.,-0.99990130540268)) ;
#9909 = DIRECTION('center_axis',(1.38491428068804E-15,1.,-5.22775657039832E-16)) ;
#9910 = DIRECTION('ref_axis',(0.353155349954092,0.,0.935564695143421)) ;
#9911 = DIRECTION('center_axis',(1.42608153219998E-15,1.,7.51659194327274E-15)) ;
#9912 = DIRECTION('ref_axis',(-0.353156058759361,7.57626650063376E-15,-0.935564427584522)) ;
#9913 = DIRECTION('center_axis',(5.68566921680937E-16,1.,1.17837026301599E-17)) ;
#9914 = DIRECTION('ref_axis',(0.945793391259251,0.,0.324768934860349)) ;
#9915 = DIRECTION('center_axis',(0.,-1.,0.)) ;
#9916 = DIRECTION('ref_axis',(0.,0.,-1.)) ;
#9917 = DIRECTION('center_axis',(0.,-1.,0.)) ;
#9918 = DIRECTION('ref_axis',(0.323867587734909,0.,-0.946102418142334)) ;
#9919 = DIRECTION('center_axis',(2.86285518001772E-14,1.,9.80006109242406E-15)) ;
#9920 = DIRECTION('ref_axis',(-0.323868053924072,1.34246448737236E-20,0.946102258557411)) ;
#9921 = DIRECTION('center_axis',(0.,1.,0.)) ;
#9922 = DIRECTION('ref_axis',(0.982473666441365,0.,-0.186401434407735)) ;
#9923 = DIRECTION('center_axis',(5.20045044510935E-15,-1.,2.21184655932972E-14)) ;
#9924 = DIRECTION('ref_axis',(0.98247394286439,9.86425565709368E-16,-0.186399977447689)) ;
#9925 = DIRECTION('center_axis',(0.,-1.,0.)) ;
#9926 = DIRECTION('ref_axis',(-0.51913214316201,0.,-0.854693990815437)) ;
#9927 = DIRECTION('center_axis',(1.328521953279E-16,1.,5.52953428666426E-16)) ;
#9928 = DIRECTION('ref_axis',(-0.0741867580339955,-5.55111512312574E-16,0.997244365706022)) ;
#9929 = DIRECTION('',(0.,1.,0.)) ;
#9930 = DIRECTION('center_axis',(0.,-1.,0.)) ;
#9931 = DIRECTION('ref_axis',(-0.230203180796986,0.,0.973142587471615)) ;
#9932 = DIRECTION('',(0.,-1.,0.)) ;
#9933 = DIRECTION('',(1.55820775385987E-15,-1.,0.)) ;
#9934 = DIRECTION('center_axis',(0.,1.,0.)) ;
#9935 = DIRECTION('ref_axis',(-0.946102418141937,0.,-0.323867587736068)) ;
#9936 = DIRECTION('',(0.,-1.,0.)) ;
#9937 = DIRECTION('center_axis',(-2.45390046765461E-14,-1.,-8.40013522599915E-15)) ;
#9938 = DIRECTION('ref_axis',(-0.910070204982191,2.58220234335356E-14,-0.414454125330746)) ;
#9939 = DIRECTION('center_axis',(0.,-1.,0.)) ;
#9940 = DIRECTION('ref_axis',(0.414454297733063,0.,-0.910070126468611)) ;
#9941 = DIRECTION('',(0.,-1.,0.)) ;
#9942 = DIRECTION('center_axis',(0.,-1.,0.)) ;
#9943 = DIRECTION('ref_axis',(-0.946102402572802,0.,-0.323867633217603)) ;
#9944 = DIRECTION('center_axis',(0.,-1.,0.)) ;
#9945 = DIRECTION('ref_axis',(-0.99990130540252,0.,0.0140491798457023)) ;
#9946 = DIRECTION('center_axis',(1.48618877891001E-16,1.,-4.98150096463128E-16)) ;
#9947 = DIRECTION('ref_axis',(0.821909814783993,1.58603289232165E-16,0.569617640493816)) ;
#9948 = DIRECTION('',(0.,1.,0.)) ;
#9949 = DIRECTION('center_axis',(0.,-1.,0.)) ;
#9950 = DIRECTION('ref_axis',(-0.186399383787626,0.,-0.982474055496426)) ;
#9951 = DIRECTION('',(1.55820775385987E-15,-1.,0.)) ;
#9952 = DIRECTION('',(0.,-1.,0.)) ;
#9953 = DIRECTION('center_axis',(0.,-1.,0.)) ;
#9954 = DIRECTION('ref_axis',(-0.935564561363999,0.,0.353155704356858)) ;
#9955 = DIRECTION('',(0.,-1.,-6.23283101543948E-15)) ;
#9956 = DIRECTION('center_axis',(0.,1.,0.)) ;
#9957 = DIRECTION('ref_axis',(-0.186399467458827,0.,-0.982474039621946)) ;
#9958 = DIRECTION('',(1.55820775385987E-15,-1.,0.)) ;
#9959 = DIRECTION('center_axis',(2.06734131486432E-15,-1.,1.08965395694644E-14)) ;
#9960 = DIRECTION('ref_axis',(-0.0140491798343041,-1.09830586184606E-14,-0.99990130540268)) ;
#9961 = DIRECTION('center_axis',(0.,-1.,0.)) ;
#9962 = DIRECTION('ref_axis',(0.99990130540221,0.,-0.0140491798677303)) ;
#9963 = DIRECTION('center_axis',(0.,-1.,0.)) ;
#9964 = DIRECTION('ref_axis',(-0.958437301458723,0.,0.285303240732594)) ;
#9965 = DIRECTION('',(0.,1.,0.)) ;
#9966 = DIRECTION('',(0.367081861009792,-0.707106776692743,0.604359920637352)) ;
#9967 = DIRECTION('',(0.688115764120616,-0.707106780936084,0.162778056023868)) ;
#9968 = DIRECTION('',(0.688115718421299,0.707106780933206,0.162778249222119)) ;
#9969 = DIRECTION('',(0.643516818589292,-0.707106775388879,0.293063324883645)) ;
#9970 = DIRECTION('',(-0.643516754494961,-0.707106778210615,-0.293063458815452)) ;
#9971 = DIRECTION('',(0.707036994066234,-0.707106780687713,-0.00993427034270016)) ;
#9972 = DIRECTION('',(-0.249719016897138,-0.707106780355147,-0.661543962088465)) ;
#9973 = DIRECTION('',(-0.00993427042518335,-0.707106777296336,-0.707036997456787)) ;
#9974 = DIRECTION('',(0.249718850397837,-0.707106779276632,0.661544026091243)) ;
#9975 = DIRECTION('',(0.00993427042313984,-0.707106778684187,0.707036996068828)) ;
#9976 = DIRECTION('',(0.677717522537246,-0.7071067736206,-0.201739858099097)) ;
#9977 = DIRECTION('center_axis',(0.,-1.,0.)) ;
#9978 = DIRECTION('ref_axis',(0.587391769794684,0.,-0.809302729995068)) ;
#9979 = DIRECTION('center_axis',(-6.57177564856263E-16,1.,-6.46151479728032E-16)) ;
#9980 = DIRECTION('ref_axis',(-0.948327476740895,-5.55111512312572E-16,0.317293234813235)) ;
#9981 = DIRECTION('',(0.,1.,0.)) ;
#9982 = DIRECTION('center_axis',(1.11571400579693E-15,1.,3.09771438098241E-16)) ;
#9983 = DIRECTION('ref_axis',(-0.948327476740895,1.11022302462514E-15,0.317293234813235)) ;
#9984 = DIRECTION('center_axis',(0.,-1.,0.)) ;
#9985 = DIRECTION('ref_axis',(0.,0.,-1.)) ;
#9986 = DIRECTION('center_axis',(0.,1.,0.)) ;
#9987 = DIRECTION('ref_axis',(0.,0.,1.)) ;
#9988 = DIRECTION('',(0.415348703634992,-0.707106781186545,-0.572263448412299)) ;
#9989 = DIRECTION('',(0.415348703634974,0.707106781186551,-0.572263448412304)) ;
#9990 = DIRECTION('center_axis',(0.,1.,0.)) ;
#9991 = DIRECTION('ref_axis',(-0.323408449520454,0.,0.946259464829164)) ;
#9992 = DIRECTION('center_axis',(0.,-1.,0.)) ;
#9993 = DIRECTION('ref_axis',(-0.931688169129028,0.,-0.36325907491073)) ;
#9994 = DIRECTION('',(0.,-1.,0.)) ;
#9995 = DIRECTION('center_axis',(0.,-1.,0.)) ;
#9996 = DIRECTION('ref_axis',(-0.931688169129028,0.,-0.36325907491073)) ;
#9997 = DIRECTION('',(0.,-1.,0.)) ;
#9998 = DIRECTION('center_axis',(-0.931688169129027,0.,-0.363259074910734)) ;
#9999 = DIRECTION('ref_axis',(-0.363259074910734,0.,0.931688169129026)) ;
#10000 = DIRECTION('',(0.363259074910734,0.,-0.931688169129027)) ;
#10001 = DIRECTION('',(0.,-1.,0.)) ;
#10002 = DIRECTION('',(0.363259074910734,0.,-0.931688169129027)) ;
#10003 = DIRECTION('center_axis',(0.,1.,0.)) ;
#10004 = DIRECTION('ref_axis',(0.162186831709887,0.,-0.986760067909068)) ;
#10005 = DIRECTION('center_axis',(0.,-1.,0.)) ;
#10006 = DIRECTION('ref_axis',(0.998944452320448,0.,-0.0459345314355166)) ;
#10007 = DIRECTION('',(0.,-1.,0.)) ;
#10008 = DIRECTION('center_axis',(0.,-1.,0.)) ;
#10009 = DIRECTION('ref_axis',(0.998944452320448,0.,-0.0459345314355166)) ;
#10010 = DIRECTION('center_axis',(0.,-1.,0.)) ;
#10011 = DIRECTION('ref_axis',(-0.488673380771942,0.,0.872466805629257)) ;
#10012 = DIRECTION('center_axis',(0.,1.,0.)) ;
#10013 = DIRECTION('ref_axis',(0.48267674456582,0.,0.875798584296265)) ;
#10014 = DIRECTION('',(0.,-1.,0.)) ;
#10015 = DIRECTION('center_axis',(0.,1.,0.)) ;
#10016 = DIRECTION('ref_axis',(0.48267674456582,0.,0.875798584296265)) ;
#10017 = DIRECTION('center_axis',(-0.482676744565949,0.,-0.875798584296194)) ;
#10018 = DIRECTION('ref_axis',(-0.875798584296194,0.,0.482676744565949)) ;
#10019 = DIRECTION('',(0.875798584296194,0.,-0.482676744565949)) ;
#10020 = DIRECTION('',(0.,-1.,0.)) ;
#10021 = DIRECTION('',(0.875798584296194,0.,-0.482676744565949)) ;
#10022 = DIRECTION('center_axis',(-0.983502142252922,0.,0.180896479191588)) ;
#10023 = DIRECTION('ref_axis',(0.180896479191588,0.,0.983502142252922)) ;
#10024 = DIRECTION('',(-0.180896479191588,0.,-0.983502142252922)) ;
#10025 = DIRECTION('',(0.,-1.,0.)) ;
#10026 = DIRECTION('',(-0.180896479191588,0.,-0.983502142252922)) ;
#10027 = DIRECTION('center_axis',(0.,1.,0.)) ;
#10028 = DIRECTION('ref_axis',(0.928762380268974,0.,-0.370675654713267)) ;
#10029 = DIRECTION('center_axis',(0.,-1.,0.)) ;
#10030 = DIRECTION('ref_axis',(0.545993817711977,0.,0.837789204406634)) ;
#10031 = DIRECTION('',(0.,-1.,0.)) ;
#10032 = DIRECTION('center_axis',(0.,-1.,0.)) ;
#10033 = DIRECTION('ref_axis',(0.545993817711977,0.,0.837789204406634)) ;
#10034 = DIRECTION('center_axis',(0.515454087003814,0.,0.856917197978349)) ;
#10035 = DIRECTION('ref_axis',(0.856917197978349,0.,-0.515454087003814)) ;
#10036 = DIRECTION('',(-0.856917197978349,0.,0.515454087003814)) ;
#10037 = DIRECTION('',(0.,-1.,0.)) ;
#10038 = DIRECTION('',(-0.856917197978349,0.,0.515454087003814)) ;
#10039 = DIRECTION('center_axis',(0.,-1.,0.)) ;
#10040 = DIRECTION('ref_axis',(-0.98759867396716,0.,-0.156999551522628)) ;
#10041 = DIRECTION('center_axis',(0.,1.,0.)) ;
#10042 = DIRECTION('ref_axis',(-0.755777768077742,0.,0.654828195238588)) ;
#10043 = DIRECTION('',(0.,-1.,0.)) ;
#10044 = DIRECTION('center_axis',(0.,1.,0.)) ;
#10045 = DIRECTION('ref_axis',(-0.755777768077742,0.,0.654828195238588)) ;
#10046 = DIRECTION('center_axis',(0.,1.,0.)) ;
#10047 = DIRECTION('ref_axis',(0.915970102946441,0.,-0.401246520867516)) ;
#10048 = DIRECTION('center_axis',(7.3591138693603E-18,-1.,-3.22370656776922E-18)) ;
#10049 = DIRECTION('ref_axis',(0.993756958760637,7.58941520739936E-18,-0.111566603044145)) ;
#10050 = DIRECTION('',(0.,-1.,0.)) ;
#10051 = DIRECTION('center_axis',(3.76786630111247E-15,-1.,-1.65053776269784E-15)) ;
#10052 = DIRECTION('ref_axis',(0.993756958760637,3.88578058618847E-15,-0.111566603044145)) ;
#10053 = DIRECTION('center_axis',(-0.226066317498263,0.,0.974111913536004)) ;
#10054 = DIRECTION('ref_axis',(0.974111913536004,0.,0.226066317498263)) ;
#10055 = DIRECTION('',(-0.974111913536004,0.,-0.226066317498263)) ;
#10056 = DIRECTION('',(0.,-1.,0.)) ;
#10057 = DIRECTION('',(-0.974111913536004,0.,-0.226066317498263)) ;
#10058 = DIRECTION('center_axis',(0.,-1.,0.)) ;
#10059 = DIRECTION('ref_axis',(-0.503747852925287,0.,-0.863850739811667)) ;
#10060 = DIRECTION('center_axis',(0.,1.,0.)) ;
#10061 = DIRECTION('ref_axis',(-0.959127119717865,0.,-0.28297556117395)) ;
#10062 = DIRECTION('center_axis',(4.10636256070708E-16,1.,7.04178551908964E-16)) ;
#10063 = DIRECTION('ref_axis',(-0.959127119717865,6.66133814775114E-16,-0.28297556117395)) ;
#10064 = DIRECTION('center_axis',(0.,1.,0.)) ;
#10065 = DIRECTION('ref_axis',(0.,0.,1.)) ;
#10066 = DIRECTION('center_axis',(-1.1978755459731E-19,1.,3.59810729949512E-18)) ;
#10067 = DIRECTION('ref_axis',(0.875530529285933,-2.16840434497102E-18,0.48316280101876)) ;
#10068 = DIRECTION('center_axis',(-6.93236427336665E-16,1.,-9.96444582969986E-17)) ;
#10069 = DIRECTION('ref_axis',(-0.948327476740892,-6.2558465352413E-16,0.317293234813244)) ;
#10070 = DIRECTION('center_axis',(0.,-1.,0.)) ;
#10071 = DIRECTION('ref_axis',(0.,0.,-1.)) ;
#10072 = DIRECTION('center_axis',(2.78998493207323E-16,1.,5.4878418411934E-17)) ;
#10073 = DIRECTION('ref_axis',(0.875530529285933,0.,0.48316280101876)) ;
#10074 = DIRECTION('center_axis',(1.14634110235167E-16,1.,-8.40950104074492E-17)) ;
#10075 = DIRECTION('ref_axis',(-0.948327476740892,0.,0.317293234813244)) ;
#10076 = DIRECTION('center_axis',(0.,-1.,0.)) ;
#10077 = DIRECTION('ref_axis',(0.993299589837987,0.,-0.115567836475751)) ;
#10078 = DIRECTION('',(0.,1.,0.)) ;
#10079 = DIRECTION('center_axis',(0.,1.,0.)) ;
#10080 = DIRECTION('ref_axis',(-0.587391769794674,0.,0.809302729995075)) ;
#10081 = DIRECTION('',(0.,-1.,0.)) ;
#10082 = DIRECTION('center_axis',(-4.35747896024226E-15,-1.,5.94017881872706E-16)) ;
#10083 = DIRECTION('ref_axis',(0.,-5.94017881872706E-16,-1.)) ;
#10084 = DIRECTION('',(0.323867587736079,-1.97204328484321E-15,-0.946102418141933)) ;
#10085 = DIRECTION('center_axis',(0.,1.,0.)) ;
#10086 = DIRECTION('ref_axis',(0.946102418142542,0.,0.3238675877343)) ;
#10087 = DIRECTION('center_axis',(1.67995222306785E-15,1.,-3.91636034436018E-16)) ;
#10088 = DIRECTION('ref_axis',(0.946102418142689,-1.46256864286623E-15,0.323867587733871)) ;
#10089 = DIRECTION('center_axis',(0.946102418141937,-3.68441630821444E-14,
0.323867587736069)) ;
#10090 = DIRECTION('ref_axis',(-0.166270483818289,0.858155219939116,0.485719821195387)) ;
#10091 = DIRECTION('center_axis',(1.78081198063816E-15,1.,9.26117405585395E-16)) ;
#10092 = DIRECTION('ref_axis',(0.946102418142689,-1.98476993124453E-15,0.323867587733871)) ;
#10093 = DIRECTION('',(-2.3431716883402E-14,-1.,4.6863433766804E-14)) ;
#10094 = DIRECTION('center_axis',(1.67995222306785E-15,1.,-3.91636034436018E-16)) ;
#10095 = DIRECTION('ref_axis',(0.946102418142689,-1.46256864286623E-15,0.323867587733871)) ;
#10096 = DIRECTION('center_axis',(0.,1.,0.)) ;
#10097 = DIRECTION('ref_axis',(0.94610241814253,0.,0.323867587734335)) ;
#10098 = DIRECTION('',(-6.71796199601783E-16,-1.,1.34359239920357E-15)) ;
#10099 = DIRECTION('',(0.229008967494671,-0.707106781186611,-0.668995435565098)) ;
#10100 = DIRECTION('center_axis',(1.60765258969569E-16,-1.,-4.67018853280937E-16)) ;
#10101 = DIRECTION('ref_axis',(0.,4.67018853280937E-16,-1.)) ;
#10102 = DIRECTION('center_axis',(0.,-1.,0.)) ;
#10103 = DIRECTION('ref_axis',(0.946102418141985,0.,0.323867587735927)) ;
#10104 = DIRECTION('',(0.323867587736072,4.92709653940649E-16,-0.946102418141936)) ;
#10105 = DIRECTION('center_axis',(0.946102418141932,5.1997810801415E-14,0.323867587736083)) ;
#10106 = DIRECTION('ref_axis',(-0.166270483818375,0.858155219939103,0.485719821195381)) ;
#10107 = DIRECTION('center_axis',(1.08752723635674E-15,-1.,1.33899319096163E-15)) ;
#10108 = DIRECTION('ref_axis',(0.946102418141425,1.46256864286554E-15,0.323867587737563)) ;
#10109 = DIRECTION('',(0.,-1.,-4.68634337668034E-14)) ;
#10110 = DIRECTION('center_axis',(1.97477928217485E-15,-1.,3.59487894101525E-16)) ;
#10111 = DIRECTION('ref_axis',(0.946102418141425,1.98476993124473E-15,0.323867587737563)) ;
#10112 = DIRECTION('center_axis',(1.08752723635674E-15,-1.,1.33899319096163E-15)) ;
#10113 = DIRECTION('ref_axis',(0.946102418141397,1.46256864286562E-15,0.323867587737645)) ;
#10114 = DIRECTION('',(0.,-1.,-1.34359239920357E-15)) ;
#10115 = DIRECTION('center_axis',(0.,-1.,0.)) ;
#10116 = DIRECTION('ref_axis',(0.946102418141491,0.,0.323867587737372)) ;
#10117 = DIRECTION('',(0.229008967494697,-0.707106781186544,-0.66899543556516)) ;
#10118 = DIRECTION('center_axis',(-0.958097822844588,-0.0208105263954551,
0.285684238017439)) ;
#10119 = DIRECTION('ref_axis',(0.285746119898407,0.,0.958305355804195)) ;
#10120 = DIRECTION('center_axis',(0.958097822844581,0.0208105263955041,-0.285684238017459)) ;
#10121 = DIRECTION('ref_axis',(0.286206169394248,-0.0291560893922151,0.957724360686322)) ;
#10122 = DIRECTION('center_axis',(0.0789989380213253,0.96979445877955,-0.230776678873718)) ;
#10123 = DIRECTION('ref_axis',(0.946102418132454,7.31486930126385E-12,0.323867587763771)) ;
#10124 = DIRECTION('center_axis',(0.0789989380213253,0.96979445877955,-0.230776678873718)) ;
#10125 = DIRECTION('ref_axis',(0.946102418132454,7.31486930126385E-12,0.323867587763771)) ;
#10126 = DIRECTION('center_axis',(0.0789989380213253,0.96979445877955,-0.230776678873718)) ;
#10127 = DIRECTION('ref_axis',(0.946102418132454,7.31486930126385E-12,0.323867587763771)) ;
#10128 = DIRECTION('center_axis',(-0.0396714859666553,0.0207623501566727,
-0.998997046050272)) ;
#10129 = DIRECTION('ref_axis',(0.999186758728018,0.00803913676004757,-0.0395119407616252)) ;
#10130 = DIRECTION('',(0.00302837173055173,2.34500326237813E-6,0.999995414469068)) ;
#10131 = DIRECTION('center_axis',(-0.03967148596651,0.020762350156785,-0.998997046050275)) ;
#10132 = DIRECTION('ref_axis',(0.999186758728035,0.0080391367584932,-0.0395119407615118)) ;
#10133 = DIRECTION('center_axis',(-0.03967148596651,0.020762350156785,-0.998997046050275)) ;
#10134 = DIRECTION('ref_axis',(0.999186758728035,0.0080391367584932,-0.0395119407615118)) ;
#10135 = DIRECTION('center_axis',(-0.03967148596651,0.020762350156785,-0.998997046050275)) ;
#10136 = DIRECTION('ref_axis',(0.999186758728035,0.0080391367584932,-0.0395119407615118)) ;
#10137 = DIRECTION('center_axis',(0.958097822844586,-0.0208105263955017,-0.285684238017442)) ;
#10138 = DIRECTION('ref_axis',(-0.285746119898411,0.,-0.958305355804194)) ;
#10139 = DIRECTION('center_axis',(-0.958097822844564,0.0208105263953766,0.285684238017527)) ;
#10140 = DIRECTION('ref_axis',(0.286206169391818,0.0291560891774949,0.957724360693585)) ;
#10141 = DIRECTION('center_axis',(-0.0789989380212596,0.969794458779555,0.230776678873719)) ;
#10142 = DIRECTION('ref_axis',(0.946102418124642,-1.34456916771157E-11,0.32386758778659)) ;
#10143 = DIRECTION('center_axis',(-0.0789989380212596,0.969794458779555,0.230776678873719)) ;
#10144 = DIRECTION('ref_axis',(0.946102418124642,-1.34456916771157E-11,0.32386758778659)) ;
#10145 = DIRECTION('center_axis',(-0.0789989380212596,0.969794458779555,0.230776678873719)) ;
#10146 = DIRECTION('ref_axis',(0.946102418124642,-1.34456916771157E-11,0.32386758778659)) ;
#10147 = DIRECTION('center_axis',(0.0396714859665023,0.0207623501562736,0.998997046050286)) ;
#10148 = DIRECTION('ref_axis',(0.999186758727716,-0.00803913680279955,-0.0395119407605742)) ;
#10149 = DIRECTION('',(-0.00302837173057115,2.34500326237817E-6,-0.999995414469068)) ;
#10150 = DIRECTION('center_axis',(0.0396714859664518,0.0207623501564799,0.998997046050284)) ;
#10151 = DIRECTION('ref_axis',(0.999186758728069,-0.00803913675410597,-0.0395119407615483)) ;
#10152 = DIRECTION('center_axis',(0.0396714859664518,0.0207623501564799,0.998997046050284)) ;
#10153 = DIRECTION('ref_axis',(0.999186758728069,-0.00803913675410597,-0.0395119407615483)) ;
#10154 = DIRECTION('center_axis',(0.0396714859664518,0.0207623501564799,0.998997046050284)) ;
#10155 = DIRECTION('ref_axis',(0.999186758728069,-0.00803913675410597,-0.0395119407615483)) ;
#10156 = DIRECTION('center_axis',(0.94610241814194,0.,0.323867587736059)) ;
#10157 = DIRECTION('ref_axis',(0.323867587736059,0.,-0.94610241814194)) ;
#10158 = DIRECTION('center_axis',(-0.94610241814194,0.,-0.32386758773606)) ;
#10159 = DIRECTION('ref_axis',(-0.32386758773606,0.,0.94610241814194)) ;
#10160 = DIRECTION('center_axis',(-7.50393630258175E-16,1.,-7.64952095823687E-16)) ;
#10161 = DIRECTION('ref_axis',(0.,7.64952095823687E-16,1.)) ;
#10162 = DIRECTION('center_axis',(-4.70706556975765E-19,1.,-2.40039210366457E-19)) ;
#10163 = DIRECTION('ref_axis',(0.950103467612796,5.22096546399878E-19,0.311934930442457)) ;
#10164 = DIRECTION('',(0.311934930442522,-4.9210731940036E-16,-0.950103467612775)) ;
#10165 = DIRECTION('center_axis',(-0.950103467612774,8.85448435361195E-14,
-0.311934930442524)) ;
#10166 = DIRECTION('ref_axis',(-0.160144373097325,-0.858155219939114,0.487773921255037)) ;
#10167 = DIRECTION('center_axis',(-1.02409251240679E-16,1.,-1.31144614757413E-15)) ;
#10168 = DIRECTION('ref_axis',(0.950103467612728,5.06385247542231E-16,0.311934930442666)) ;
#10169 = DIRECTION('',(2.34317168834017E-14,1.,0.)) ;
#10170 = DIRECTION('center_axis',(0.,1.,0.)) ;
#10171 = DIRECTION('ref_axis',(0.950103467612728,0.,0.311934930442666)) ;
#10172 = DIRECTION('center_axis',(-1.73521265163545E-15,1.,-8.84880545094921E-16)) ;
#10173 = DIRECTION('ref_axis',(0.950103467612728,1.92465670864857E-15,0.311934930442666)) ;
#10174 = DIRECTION('',(6.71796199601783E-16,1.,0.)) ;
#10175 = DIRECTION('center_axis',(0.,1.,0.)) ;
#10176 = DIRECTION('ref_axis',(0.950103467612751,0.,0.311934930442595)) ;
#10177 = DIRECTION('',(0.220571304604853,0.707106781186509,-0.671824604777889)) ;
#10178 = DIRECTION('center_axis',(0.,1.,0.)) ;
#10179 = DIRECTION('ref_axis',(0.,0.,1.)) ;
#10180 = DIRECTION('',(0.311934930442493,-6.02334540269699E-19,-0.950103467612784)) ;
#10181 = DIRECTION('center_axis',(-5.21384921350609E-19,-1.,-8.56810894045757E-20)) ;
#10182 = DIRECTION('ref_axis',(0.950103467612636,-5.22096546399847E-19,0.311934930442945)) ;
#10183 = DIRECTION('center_axis',(-8.59827508034601E-16,-1.,9.95527653635857E-16)) ;
#10184 = DIRECTION('ref_axis',(0.950103467612776,-5.06385247542023E-16,0.311934930442517)) ;
#10185 = DIRECTION('center_axis',(-0.950103467612784,4.27867700308741E-14,
-0.311934930442494)) ;
#10186 = DIRECTION('ref_axis',(-0.160144373097263,-0.858155219939135,0.487773921255021)) ;
#10187 = DIRECTION('center_axis',(0.,-1.,0.)) ;
#10188 = DIRECTION('ref_axis',(0.950103467612776,0.,0.311934930442517)) ;
#10189 = DIRECTION('',(0.,1.,4.6863433766804E-14)) ;
#10190 = DIRECTION('center_axis',(-1.92203337406689E-15,-1.,-3.15854767981034E-16)) ;
#10191 = DIRECTION('ref_axis',(0.950103467612776,-1.92465670864854E-15,0.311934930442517)) ;
#10192 = DIRECTION('center_axis',(0.,-1.,0.)) ;
#10193 = DIRECTION('ref_axis',(0.95010346761278,0.,0.311934930442505)) ;
#10194 = DIRECTION('',(0.,1.,1.34359239920357E-15)) ;
#10195 = DIRECTION('',(0.220571304604875,0.707106781186631,-0.671824604777754)) ;
#10196 = DIRECTION('center_axis',(-0.94996636698286,0.0212343718222728,0.311629592713367)) ;
#10197 = DIRECTION('ref_axis',(0.311699873146498,0.,0.950180608663667)) ;
#10198 = DIRECTION('center_axis',(-0.94996636698287,0.0212343718222707,0.311629592713338)) ;
#10199 = DIRECTION('ref_axis',(0.312152280469402,0.0288488649901466,0.949593964169177)) ;
#10200 = DIRECTION('center_axis',(-0.0760882816615384,0.969794458779537,0.231752629142151)) ;
#10201 = DIRECTION('ref_axis',(0.950103467612754,-2.02102068934678E-14,0.311934930442585)) ;
#10202 = DIRECTION('center_axis',(-0.0760882816615384,0.969794458779537,0.231752629142151)) ;
#10203 = DIRECTION('ref_axis',(0.950103467612754,-2.02102068934678E-14,0.311934930442585)) ;
#10204 = DIRECTION('center_axis',(-0.0760882816615384,0.969794458779537,0.231752629142151)) ;
#10205 = DIRECTION('ref_axis',(0.950103467612754,-2.02102068934678E-14,0.311934930442585)) ;
#10206 = DIRECTION('center_axis',(0.0420144257474089,0.020843567561995,0.998899561377621)) ;
#10207 = DIRECTION('ref_axis',(0.999092865779137,-0.00782614817447476,-0.0418592517131076)) ;
#10208 = DIRECTION('',(0.0252238094988886,-2.33710244054272E-6,0.999681829098089)) ;
#10209 = DIRECTION('center_axis',(0.0420144257475537,0.0208435675618864,0.998899561377617)) ;
#10210 = DIRECTION('ref_axis',(0.999092865779119,-0.00782614817623618,-0.041859251713216)) ;
#10211 = DIRECTION('center_axis',(0.0420144257475537,0.0208435675618864,0.998899561377617)) ;
#10212 = DIRECTION('ref_axis',(0.999092865779119,-0.00782614817623618,-0.041859251713216)) ;
#10213 = DIRECTION('center_axis',(0.0420144257475537,0.0208435675618864,0.998899561377617)) ;
#10214 = DIRECTION('ref_axis',(0.999092865779119,-0.00782614817623618,-0.041859251713216)) ;
#10215 = DIRECTION('center_axis',(0.949966366982867,0.0212343718222273,-0.311629592713352)) ;
#10216 = DIRECTION('ref_axis',(-0.311699873146483,0.,-0.950180608663672)) ;
#10217 = DIRECTION('center_axis',(0.949966366982847,0.0212343718222471,-0.31162959271341)) ;
#10218 = DIRECTION('ref_axis',(0.312152280468722,-0.0288488649229102,0.949593964171443)) ;
#10219 = DIRECTION('center_axis',(0.0760882816615399,0.969794458779565,-0.231752629142034)) ;
#10220 = DIRECTION('ref_axis',(0.950103467611678,8.48549543021553E-13,0.311934930445863)) ;
#10221 = DIRECTION('center_axis',(0.0760882816615399,0.969794458779565,-0.231752629142034)) ;
#10222 = DIRECTION('ref_axis',(0.950103467611678,8.48549543021553E-13,0.311934930445863)) ;
#10223 = DIRECTION('center_axis',(0.0760882816615399,0.969794458779565,-0.231752629142034)) ;
#10224 = DIRECTION('ref_axis',(0.950103467611678,8.48549543021553E-13,0.311934930445863)) ;
#10225 = DIRECTION('center_axis',(-0.0420144257478324,0.0208435675616726,
-0.99889956137761)) ;
#10226 = DIRECTION('ref_axis',(0.999092865779128,0.00782614817325717,-0.0418592517135592)) ;
#10227 = DIRECTION('',(-0.0252238094988909,-2.33710244054257E-6,-0.999681829098089)) ;
#10228 = DIRECTION('center_axis',(-0.0420144257474992,0.0208435675615805,
-0.998899561377626)) ;
#10229 = DIRECTION('ref_axis',(0.999092865779118,0.00782614817675116,-0.0418592517131527)) ;
#10230 = DIRECTION('center_axis',(-0.0420144257474992,0.0208435675615805,
-0.998899561377626)) ;
#10231 = DIRECTION('ref_axis',(0.999092865779118,0.00782614817675116,-0.0418592517131527)) ;
#10232 = DIRECTION('center_axis',(-0.0420144257474992,0.0208435675615805,
-0.998899561377626)) ;
#10233 = DIRECTION('ref_axis',(0.999092865779118,0.00782614817675116,-0.0418592517131527)) ;
#10234 = DIRECTION('center_axis',(0.950103467612781,0.,0.311934930442502)) ;
#10235 = DIRECTION('ref_axis',(0.311934930442502,0.,-0.950103467612781)) ;
#10236 = DIRECTION('center_axis',(-0.950103467612781,0.,-0.311934930442503)) ;
#10237 = DIRECTION('ref_axis',(-0.311934930442503,0.,0.950103467612781)) ;
#10238 = DIRECTION('center_axis',(0.148915206578323,0.,-0.988849969029547)) ;
#10239 = DIRECTION('ref_axis',(-0.988849969029547,0.,-0.148915206578323)) ;
#10240 = DIRECTION('',(-0.988849969029547,0.,-0.148915206578323)) ;
#10241 = DIRECTION('',(0.,1.,0.)) ;
#10242 = DIRECTION('',(-0.988849969029547,0.,-0.148915206578323)) ;
#10243 = DIRECTION('',(0.,1.,0.)) ;
#10244 = DIRECTION('center_axis',(-1.08830637864895E-26,-1.,6.02632521955549E-27)) ;
#10245 = DIRECTION('ref_axis',(0.895004054636058,-1.24231708851682E-26,-0.446058003162163)) ;
#10246 = DIRECTION('',(0.,1.,0.)) ;
#10247 = DIRECTION('center_axis',(-7.47878448692068E-16,-1.,4.14125915728814E-16)) ;
#10248 = DIRECTION('ref_axis',(0.895004054636058,-8.5371380263067E-16,-0.446058003162163)) ;
#10249 = DIRECTION('center_axis',(0.,1.,0.)) ;
#10250 = DIRECTION('ref_axis',(0.97735290249656,0.,-0.211615935084173)) ;
#10251 = DIRECTION('center_axis',(0.,-1.,0.)) ;
#10252 = DIRECTION('ref_axis',(0.999355666138518,0.,0.0358922353279835)) ;
#10253 = DIRECTION('',(0.,1.,0.)) ;
#10254 = DIRECTION('center_axis',(0.,-1.,0.)) ;
#10255 = DIRECTION('ref_axis',(0.999355666138518,0.,0.0358922353279835)) ;
#10256 = DIRECTION('center_axis',(0.,-1.,0.)) ;
#10257 = DIRECTION('ref_axis',(-0.989177166167747,0.,0.146726050626141)) ;
#10258 = DIRECTION('center_axis',(0.,1.,0.)) ;
#10259 = DIRECTION('ref_axis',(-0.945907682666056,0.,0.324435904106393)) ;
#10260 = DIRECTION('',(0.,1.,0.)) ;
#10261 = DIRECTION('center_axis',(0.,1.,0.)) ;
#10262 = DIRECTION('ref_axis',(-0.945907682666056,0.,0.324435904106393)) ;
#10263 = DIRECTION('center_axis',(0.,1.,0.)) ;
#10264 = DIRECTION('ref_axis',(0.961183535222693,0.,0.275909788910806)) ;
#10265 = DIRECTION('center_axis',(-1.72231588589536E-26,-1.,-4.94394457563211E-27)) ;
#10266 = DIRECTION('ref_axis',(0.629810177126175,-1.61558713389262E-26,0.776749084832609)) ;
#10267 = DIRECTION('',(0.,1.,0.)) ;
#10268 = DIRECTION('center_axis',(0.,-1.,0.)) ;
#10269 = DIRECTION('ref_axis',(0.629810177126175,0.,0.776749084832609)) ;
#10270 = DIRECTION('center_axis',(0.,-1.,0.)) ;
#10271 = DIRECTION('ref_axis',(-0.641485626683685,0.,0.767135053793163)) ;
#10272 = DIRECTION('center_axis',(0.,1.,0.)) ;
#10273 = DIRECTION('ref_axis',(0.875957545458479,0.,0.482388203166658)) ;
#10274 = DIRECTION('',(0.,1.,0.)) ;
#10275 = DIRECTION('center_axis',(0.,1.,0.)) ;
#10276 = DIRECTION('ref_axis',(0.875957545458479,0.,0.482388203166658)) ;
#10277 = DIRECTION('center_axis',(0.,1.,0.)) ;
#10278 = DIRECTION('ref_axis',(-0.360497640279418,0.,-0.932760125301769)) ;
#10279 = DIRECTION('center_axis',(0.,-1.,0.)) ;
#10280 = DIRECTION('ref_axis',(0.323867587736058,0.,-0.94610241814194)) ;
#10281 = DIRECTION('',(0.,1.,0.)) ;
#10282 = DIRECTION('center_axis',(3.41689582144301E-16,-1.,8.84095710607688E-16)) ;
#10283 = DIRECTION('ref_axis',(0.323867587736058,-6.66133814775089E-16,-0.94610241814194)) ;
#10284 = DIRECTION('center_axis',(-0.323867587736067,0.,0.946102418141937)) ;
#10285 = DIRECTION('ref_axis',(0.946102418141937,0.,0.323867587736067)) ;
#10286 = DIRECTION('',(0.946102418141937,0.,0.323867587736067)) ;
#10287 = DIRECTION('',(0.,1.,0.)) ;
#10288 = DIRECTION('',(0.946102418141937,0.,0.323867587736067)) ;
#10289 = DIRECTION('center_axis',(0.,-1.,0.)) ;
#10290 = DIRECTION('ref_axis',(0.281795707735394,0.,0.959474428581559)) ;
#10291 = DIRECTION('center_axis',(0.,1.,0.)) ;
#10292 = DIRECTION('ref_axis',(0.78403805150818,0.,0.620712762706919)) ;
#10293 = DIRECTION('',(0.,1.,0.)) ;
#10294 = DIRECTION('center_axis',(1.42075501258625E-16,1.,4.83746936676411E-16)) ;
#10295 = DIRECTION('ref_axis',(0.78403805150818,-3.70074341541716E-16,0.620712762706919)) ;
#10296 = DIRECTION('center_axis',(0.323867587736072,0.,-0.946102418141936)) ;
#10297 = DIRECTION('ref_axis',(-0.946102418141936,0.,-0.323867587736072)) ;
#10298 = DIRECTION('',(-0.946102418141936,0.,-0.323867587736072)) ;
#10299 = DIRECTION('',(0.,1.,0.)) ;
#10300 = DIRECTION('',(-0.946102418141936,0.,-0.323867587736072)) ;
#10301 = DIRECTION('center_axis',(0.,1.,0.)) ;
#10302 = DIRECTION('ref_axis',(-0.884669187906721,0.,0.466219291716315)) ;
#10303 = DIRECTION('center_axis',(0.,-1.,0.)) ;
#10304 = DIRECTION('ref_axis',(-0.963515178899987,0.,-0.267653694219464)) ;
#10305 = DIRECTION('',(0.,1.,0.)) ;
#10306 = DIRECTION('center_axis',(0.,-1.,0.)) ;
#10307 = DIRECTION('ref_axis',(-0.963515178899987,0.,-0.267653694219464)) ;
#10308 = DIRECTION('center_axis',(0.,-1.,0.)) ;
#10309 = DIRECTION('ref_axis',(0.915016641398165,0.,-0.403416095321471)) ;
#10310 = DIRECTION('center_axis',(5.44264897655763E-27,1.,-2.39957624702134E-27)) ;
#10311 = DIRECTION('ref_axis',(0.452302175480044,-4.03896783473152E-27,-0.89186475547362)) ;
#10312 = DIRECTION('',(0.,1.,0.)) ;
#10313 = DIRECTION('center_axis',(0.,1.,0.)) ;
#10314 = DIRECTION('ref_axis',(0.452302175480044,0.,-0.89186475547362)) ;
#10315 = DIRECTION('center_axis',(0.,1.,0.)) ;
#10316 = DIRECTION('ref_axis',(-0.65655456191829,0.,0.754278534245992)) ;
#10317 = DIRECTION('center_axis',(0.,-1.,0.)) ;
#10318 = DIRECTION('ref_axis',(-0.820987567029615,0.,0.570946069942506)) ;
#10319 = DIRECTION('',(0.,1.,0.)) ;
#10320 = DIRECTION('center_axis',(0.,-1.,0.)) ;
#10321 = DIRECTION('ref_axis',(-0.820987567029615,0.,0.570946069942506)) ;
#10322 = DIRECTION('center_axis',(2.10056525288621E-26,-1.,-1.32433786101226E-26)) ;
#10323 = DIRECTION('ref_axis',(-0.869115672797272,-2.48102628179586E-26,0.494608883157335)) ;
#10324 = DIRECTION('',(0.,1.,0.)) ;
#10325 = DIRECTION('center_axis',(0.,-1.,0.)) ;
#10326 = DIRECTION('ref_axis',(-0.869115672797272,0.,0.494608883157335)) ;
#10327 = DIRECTION('center_axis',(-0.554110366789135,0.,-0.832443212127296)) ;
#10328 = DIRECTION('ref_axis',(-0.832443212127296,0.,0.554110366789135)) ;
#10329 = DIRECTION('',(-0.832443212127296,0.,0.554110366789135)) ;
#10330 = DIRECTION('',(-0.832443212127296,0.,0.554110366789135)) ;
#10331 = DIRECTION('center_axis',(0.,1.,0.)) ;
#10332 = DIRECTION('ref_axis',(-0.519132143162002,0.,-0.854693990815442)) ;
#10333 = DIRECTION('center_axis',(4.61307474394722E-16,-1.,-2.01875545076625E-16)) ;
#10334 = DIRECTION('ref_axis',(0.919153266546442,2.77555756156287E-16,0.393900079457984)) ;
#10335 = DIRECTION('',(0.,-1.,0.)) ;
#10336 = DIRECTION('center_axis',(1.56231020031328E-27,-1.,1.35626158679747E-27)) ;
#10337 = DIRECTION('ref_axis',(0.919153266546442,0.,0.393900079457984)) ;
#10338 = DIRECTION('center_axis',(0.,1.,0.)) ;
#10339 = DIRECTION('ref_axis',(-0.99990130540252,0.,0.0140491798457102)) ;
#10340 = DIRECTION('center_axis',(0.,-1.,0.)) ;
#10341 = DIRECTION('ref_axis',(0.805581616852069,0.,-0.592484817181003)) ;
#10342 = DIRECTION('',(0.,-1.,0.)) ;
#10343 = DIRECTION('center_axis',(-3.92234304386299E-27,-1.,1.31767206146335E-27)) ;
#10344 = DIRECTION('ref_axis',(0.805581616852069,0.,-0.592484817181003)) ;
#10345 = DIRECTION('center_axis',(0.,-1.,0.)) ;
#10346 = DIRECTION('ref_axis',(0.,0.,-1.)) ;
#10347 = DIRECTION('center_axis',(0.,1.,0.)) ;
#10348 = DIRECTION('ref_axis',(0.,0.,1.)) ;
#10349 = DIRECTION('center_axis',(0.,1.,0.)) ;
#10350 = DIRECTION('ref_axis',(-0.623533159707219,0.,-0.78179690377075)) ;
#10351 = DIRECTION('center_axis',(1.79188741038833E-16,-1.,-1.92949962064913E-16)) ;
#10352 = DIRECTION('ref_axis',(0.961756409181177,1.58603289232165E-16,0.273906205477219)) ;
#10353 = DIRECTION('',(0.,-1.,0.)) ;
#10354 = DIRECTION('center_axis',(-2.4680833998183E-16,-1.,1.47919563675122E-16)) ;
#10355 = DIRECTION('ref_axis',(0.961756409181177,-1.58603289232165E-16,0.273906205477219)) ;
#10356 = DIRECTION('center_axis',(0.,1.,0.)) ;
#10357 = DIRECTION('ref_axis',(0.,0.,1.)) ;
#10358 = DIRECTION('center_axis',(0.,-1.,0.)) ;
#10359 = DIRECTION('ref_axis',(0.961756409181177,0.,0.273906205477219)) ;
#10360 = DIRECTION('center_axis',(4.42840651093008E-17,1.,1.84317809555473E-16)) ;
#10361 = DIRECTION('ref_axis',(-0.0741867580339816,0.,0.997244365706023)) ;
#10362 = DIRECTION('center_axis',(0.,-1.,0.)) ;
#10363 = DIRECTION('ref_axis',(0.,0.,-1.)) ;
#10364 = DIRECTION('center_axis',(-4.42840651093008E-17,1.,-1.84317809555473E-16)) ;
#10365 = DIRECTION('ref_axis',(-0.0741867580339816,0.,0.997244365706023)) ;
#10366 = DIRECTION('center_axis',(0.,1.,0.)) ;
#10367 = DIRECTION('ref_axis',(0.69769452851967,0.,-0.716395383062813)) ;
#10368 = DIRECTION('center_axis',(-1.84442498271352E-17,-1.,3.70289586508121E-17)) ;
#10369 = DIRECTION('ref_axis',(-0.15149846795078,0.,0.988457492363008)) ;
#10370 = DIRECTION('',(0.,-1.,0.)) ;
#10371 = DIRECTION('center_axis',(-1.08888592718918E-16,-1.,-7.82420061571595E-17)) ;
#10372 = DIRECTION('ref_axis',(-0.15149846795078,-8.07612056149597E-17,0.988457492363008)) ;
#10373 = DIRECTION('center_axis',(0.,1.,0.)) ;
#10374 = DIRECTION('ref_axis',(0.,0.,1.)) ;
#10375 = DIRECTION('center_axis',(0.,-1.,0.)) ;
#10376 = DIRECTION('ref_axis',(0.961756409181177,0.,0.273906205477219)) ;
#10377 = DIRECTION('center_axis',(0.,-1.,0.)) ;
#10378 = DIRECTION('ref_axis',(0.,0.,-1.)) ;
#10379 = DIRECTION('center_axis',(0.,1.,0.)) ;
#10380 = DIRECTION('ref_axis',(-0.623533159707219,0.,-0.78179690377075)) ;
#10381 = DIRECTION('',(0.,-1.,0.)) ;
#10382 = DIRECTION('center_axis',(0.,-1.,0.)) ;
#10383 = DIRECTION('ref_axis',(0.519132143162,0.,0.854693990815443)) ;
#10384 = DIRECTION('',(0.,1.,0.)) ;
#10385 = DIRECTION('center_axis',(0.664443266232236,-6.36113025469821E-15,
0.747338708992541)) ;
#10386 = DIRECTION('ref_axis',(0.747338708992541,0.,-0.664443266232236)) ;
#10387 = DIRECTION('',(-0.747338708992541,-7.25975707680218E-15,0.664443266232236)) ;
#10388 = DIRECTION('',(0.,-1.,-1.03620815631681E-14)) ;
#10389 = DIRECTION('',(-0.747338708992547,-6.45311740160199E-15,0.664443266232229)) ;
#10390 = DIRECTION('',(0.,-1.,-8.88178419700125E-15)) ;
#10391 = DIRECTION('center_axis',(4.66744588567091E-17,1.,1.02423325316423E-14)) ;
#10392 = DIRECTION('ref_axis',(0.780900470920595,6.36148092073446E-15,-0.624655468651314)) ;
#10393 = DIRECTION('',(0.,-1.,-4.44089209850063E-15)) ;
#10394 = DIRECTION('center_axis',(-6.66122276787905E-17,1.,1.00236394903081E-14)) ;
#10395 = DIRECTION('ref_axis',(0.780900470920575,6.31333874337391E-15,-0.624655468651339)) ;
#10396 = DIRECTION('center_axis',(0.810464275400705,6.12393213561332E-15,
-0.585788066026622)) ;
#10397 = DIRECTION('ref_axis',(-0.585788066026622,0.,-0.810464275400705)) ;
#10398 = DIRECTION('',(0.585788066026618,-8.18378228936874E-15,0.810464275400708)) ;
#10399 = DIRECTION('',(0.,-1.,-1.03620815631681E-14)) ;
#10400 = DIRECTION('',(0.585788066026622,-8.1837822893688E-15,0.810464275400705)) ;
#10401 = DIRECTION('center_axis',(0.582685209706625,-6.37206611617975E-15,
0.812697942897081)) ;
#10402 = DIRECTION('ref_axis',(0.812697942897081,0.,-0.582685209706625)) ;
#10403 = DIRECTION('',(-0.812697942896989,-6.4531174016024E-15,0.582685209706753)) ;
#10404 = DIRECTION('',(0.,-1.,-1.03620815631681E-14)) ;
#10405 = DIRECTION('',(-0.812697942896989,-6.4531174016024E-15,0.582685209706753)) ;
#10406 = DIRECTION('center_axis',(2.78074422198555E-16,1.,1.1053880869225E-14)) ;
#10407 = DIRECTION('ref_axis',(0.841916892643634,5.73063831119028E-15,-0.539607214445181)) ;
#10408 = DIRECTION('',(0.,-1.,-8.88178419700125E-15)) ;
#10409 = DIRECTION('center_axis',(-1.12606857017318E-16,1.,1.07950474400035E-14)) ;
#10410 = DIRECTION('ref_axis',(0.841916892643638,5.91989109405419E-15,-0.539607214445176)) ;
#10411 = DIRECTION('center_axis',(0.867255993642043,5.43853653899861E-15,
-0.497862472468003)) ;
#10412 = DIRECTION('ref_axis',(-0.497862472468003,0.,-0.867255993642043)) ;
#10413 = DIRECTION('',(0.497862472467983,-8.87732316134922E-15,0.867255993642054)) ;
#10414 = DIRECTION('',(0.,-1.,-8.88178419700125E-15)) ;
#10415 = DIRECTION('',(0.497862472467983,-8.59990681255706E-15,0.867255993642054)) ;
#10416 = DIRECTION('center_axis',(0.494543132089066,-9.82182503760574E-15,
0.869153088071104)) ;
#10417 = DIRECTION('ref_axis',(0.869153088071104,0.,-0.494543132089066)) ;
#10418 = DIRECTION('',(-0.8691530880711,-6.45311740160154E-15,0.494543132089074)) ;
#10419 = DIRECTION('',(0.,-1.,-5.9211894646675E-15)) ;
#10420 = DIRECTION('',(-0.869153088071089,-4.03319837600091E-15,0.494543132089093)) ;
#10421 = DIRECTION('center_axis',(-9.65634952856587E-17,1.,9.46520975680336E-15)) ;
#10422 = DIRECTION('ref_axis',(0.893709096708599,4.3328367904494E-15,-0.448646910677318)) ;
#10423 = DIRECTION('',(0.,-1.,-7.40148683083438E-15)) ;
#10424 = DIRECTION('center_axis',(1.19841912038013E-16,1.,1.09286484407924E-14)) ;
#10425 = DIRECTION('ref_axis',(0.89370909670859,4.79600055388485E-15,-0.448646910677334)) ;
#10426 = DIRECTION('center_axis',(0.914545873732089,4.76517226719697E-15,
-0.404482193476561)) ;
#10427 = DIRECTION('ref_axis',(-0.404482193476561,0.,-0.914545873732089)) ;
#10428 = DIRECTION('',(0.404482193476528,-9.1547395101418E-15,0.914545873732104)) ;
#10429 = DIRECTION('',(0.,-1.,-8.88178419700125E-15)) ;
#10430 = DIRECTION('',(0.404482193476528,-9.43215585893399E-15,0.914545873732103)) ;
#10431 = DIRECTION('center_axis',(0.400982736425919,-9.74791193386703E-15,
0.916085610130615)) ;
#10432 = DIRECTION('ref_axis',(0.916085610130615,0.,-0.400982736425919)) ;
#10433 = DIRECTION('',(-0.916085610130582,-3.22655870080085E-15,0.400982736425995)) ;
#10434 = DIRECTION('',(0.,-1.,-5.9211894646675E-15)) ;
#10435 = DIRECTION('',(-0.916085610130573,-3.22655870080082E-15,0.400982736426017)) ;
#10436 = DIRECTION('center_axis',(-7.13111576133292E-17,1.,1.0031952483866E-14)) ;
#10437 = DIRECTION('ref_axis',(0.935709636889367,3.60570982618191E-15,-0.352771137470696)) ;
#10438 = DIRECTION('',(0.,-1.,-8.88178419700125E-15)) ;
#10439 = DIRECTION('center_axis',(-1.00429960718429E-16,1.,1.04064782229712E-14)) ;
#10440 = DIRECTION('ref_axis',(0.935709636889337,3.76507844185907E-15,-0.352771137470776)) ;
#10441 = DIRECTION('center_axis',(0.951815797848528,3.05707044117608E-15,
-0.306670322929968)) ;
#10442 = DIRECTION('ref_axis',(-0.306670322929968,0.,-0.951815797848528)) ;
#10443 = DIRECTION('',(0.306670322929944,-9.43215585893339E-15,0.951815797848535)) ;
#10444 = DIRECTION('',(0.,-1.,-8.88178419700125E-15)) ;
#10445 = DIRECTION('',(0.306670322929944,-1.01256967309138E-14,0.951815797848535)) ;
#10446 = DIRECTION('center_axis',(0.303029089991586,-9.4998790733618E-15,
0.952981306542196)) ;
#10447 = DIRECTION('ref_axis',(0.952981306542196,0.,-0.303029089991586)) ;
#10448 = DIRECTION('',(-0.952981306542202,-3.22655870080064E-15,0.303029089991566)) ;
#10449 = DIRECTION('',(0.,-1.,-1.77635683940025E-14)) ;
#10450 = DIRECTION('',(-0.952981306542225,-1.61327935040036E-15,0.303029089991496)) ;
#10451 = DIRECTION('center_axis',(1.2480662469827E-16,1.,9.71479571659155E-15)) ;
#10452 = DIRECTION('ref_axis',(0.96745834647859,2.33739275392867E-15,-0.253030329859707)) ;
#10453 = DIRECTION('',(0.,-1.,-8.88178419700125E-15)) ;
#10454 = DIRECTION('center_axis',(-3.27466891807325E-16,1.,1.11937858983162E-14)) ;
#10455 = DIRECTION('ref_axis',(0.967458346478616,3.14917791590319E-15,-0.253030329859608)) ;
#10456 = DIRECTION('center_axis',(0.978657428903444,3.17959536473004E-15,
-0.205498508150548)) ;
#10457 = DIRECTION('ref_axis',(-0.205498508150548,0.,-0.978657428903444)) ;
#10458 = DIRECTION('',(0.205498508150497,-9.98698855651799E-15,0.978657428903455)) ;
#10459 = DIRECTION('',(0.,-1.,-8.88178419700125E-15)) ;
#10460 = DIRECTION('',(0.205498508150497,-9.98698855651799E-15,0.978657428903455)) ;
#10461 = DIRECTION('center_axis',(0.201755393434541,-1.06080915271686E-14,
0.979435940335086)) ;
#10462 = DIRECTION('ref_axis',(0.979435940335086,0.,-0.201755393434541)) ;
#10463 = DIRECTION('',(-0.979435940335062,-1.61327935040034E-15,0.201755393434655)) ;
#10464 = DIRECTION('',(0.,-1.,-1.1842378929335E-14)) ;
#10465 = DIRECTION('',(-0.979435940335067,-8.06639675200175E-16,0.20175539343463)) ;
#10466 = DIRECTION('center_axis',(1.82586758620613E-16,1.,9.77984243998921E-15)) ;
#10467 = DIRECTION('ref_axis',(0.9886073799701,1.29152855830694E-15,-0.150517269004768)) ;
#10468 = DIRECTION('',(0.,-1.,-8.88178419700125E-15)) ;
#10469 = DIRECTION('center_axis',(-2.54053681858878E-16,1.,1.14670287668068E-14)) ;
#10470 = DIRECTION('ref_axis',(0.988607379970118,1.97714519837175E-15,-0.150517269004648)) ;
#10471 = DIRECTION('center_axis',(0.994776684370062,1.35439464247368E-15,
-0.102075208712529)) ;
#10472 = DIRECTION('ref_axis',(-0.102075208712529,0.,-0.994776684370062)) ;
#10473 = DIRECTION('',(0.10207520871253,-1.05418212541018E-14,0.994776684370062)) ;
#10474 = DIRECTION('',(0.,-1.,-5.9211894646675E-15)) ;
#10475 = DIRECTION('',(0.102075208712529,-1.01256967309135E-14,0.994776684370062)) ;
#10476 = DIRECTION('center_axis',(0.0982712225671941,-1.39810986889151E-14,
0.995159669005506)) ;
#10477 = DIRECTION('ref_axis',(0.995159669005506,0.,-0.0982712225671941)) ;
#10478 = DIRECTION('',(-0.995159669005508,-8.06639675199961E-16,0.0982712225671731)) ;
#10479 = DIRECTION('',(0.,-1.,-1.1842378929335E-14)) ;
#10480 = DIRECTION('',(-0.995159669005514,-2.41991902559989E-15,0.098271222567122)) ;
#10481 = DIRECTION('center_axis',(-1.35982084744398E-16,1.,9.88995300307463E-15)) ;
#10482 = DIRECTION('ref_axis',(0.998925024127247,5.94285761224491E-16,-0.0463551094527745)) ;
#10483 = DIRECTION('',(0.,-1.,-1.1842378929335E-14)) ;
#10484 = DIRECTION('center_axis',(6.87947995565783E-17,1.,1.09363115505266E-14)) ;
#10485 = DIRECTION('ref_axis',(0.998925024127252,4.38233072126194E-16,-0.0463551094526625)) ;
#10486 = DIRECTION('center_axis',(0.999996958312326,-2.13640474537978E-17,
0.00246644807282737)) ;
#10487 = DIRECTION('ref_axis',(0.00246644807282737,0.,-0.999996958312326)) ;
#10488 = DIRECTION('',(-0.00246644807286617,-9.98698855651738E-15,0.999996958312326)) ;
#10489 = DIRECTION('',(0.,-1.,-1.1842378929335E-14)) ;
#10490 = DIRECTION('',(-0.00246644807286617,-1.05418212541017E-14,0.999996958312326)) ;
#10491 = DIRECTION('center_axis',(-0.00628962837959365,-1.10239774849311E-14,
0.999980220091801)) ;
#10492 = DIRECTION('ref_axis',(0.999980220091801,0.,0.00628962837959364)) ;
#10493 = DIRECTION('',(-0.999980220091801,0.,-0.00628962837952103)) ;
#10494 = DIRECTION('',(0.,-1.,-1.1842378929335E-14)) ;
#10495 = DIRECTION('',(-0.999980220091801,0.,-0.00628962837952103)) ;
#10496 = DIRECTION('center_axis',(3.10052989716172E-17,1.,1.02021323753836E-14)) ;
#10497 = DIRECTION('ref_axis',(0.998298236681544,-6.25889133664531E-16,0.0583149263784192)) ;
#10498 = DIRECTION('',(0.,-1.,-8.88178419700125E-15)) ;
#10499 = DIRECTION('center_axis',(2.09939991149458E-16,1.,9.87182977187906E-15)) ;
#10500 = DIRECTION('ref_axis',(0.998298236681544,-7.85257749340864E-16,0.0583149263784198)) ;
#10501 = DIRECTION('center_axis',(0.994261056316501,-1.10487221809803E-15,
0.106981081936929)) ;
#10502 = DIRECTION('ref_axis',(0.106981081936929,0.,-0.994261056316501)) ;
#10503 = DIRECTION('',(-0.106981081936948,-9.84828038212133E-15,0.994261056316499)) ;
#10504 = DIRECTION('',(0.,-1.,-8.88178419700125E-15)) ;
#10505 = DIRECTION('',(-0.106981081936948,-1.02644049053096E-14,0.994261056316499)) ;
#10506 = DIRECTION('center_axis',(-0.110781568841626,-8.68506275659569E-15,
0.993844778627421)) ;
#10507 = DIRECTION('ref_axis',(0.993844778627421,0.,0.110781568841626)) ;
#10508 = DIRECTION('',(-0.993844778627431,0.,-0.110781568841543)) ;
#10509 = DIRECTION('',(0.,-1.,-8.88178419700125E-15)) ;
#10510 = DIRECTION('',(-0.993844778627431,1.6132793504004E-15,-0.110781568841543)) ;
#10511 = DIRECTION('center_axis',(-4.24008527350335E-16,1.,1.08192196707972E-14)) ;
#10512 = DIRECTION('ref_axis',(0.986733884847439,-1.33807401433826E-15,0.162346051673214)) ;
#10513 = DIRECTION('',(0.,-1.,-1.1842378929335E-14)) ;
#10514 = DIRECTION('center_axis',(-3.80940090177415E-17,1.,1.00483850234157E-14)) ;
#10515 = DIRECTION('ref_axis',(0.986733884847427,-1.59372698473701E-15,0.162346051673284)) ;
#10516 = DIRECTION('center_axis',(0.977631822125172,-2.02289727404569E-15,
0.210323608680092)) ;
#10517 = DIRECTION('ref_axis',(0.210323608680092,0.,-0.977631822125172)) ;
#10518 = DIRECTION('',(-0.210323608680131,-9.84828038212189E-15,0.977631822125163)) ;
#10519 = DIRECTION('',(0.,-1.,-8.88178419700125E-15)) ;
#10520 = DIRECTION('',(-0.21032360868013,-9.98698855651793E-15,0.977631822125164)) ;
#10521 = DIRECTION('center_axis',(-0.214059763252521,-1.01780060649862E-14,
0.976820565793061)) ;
#10522 = DIRECTION('ref_axis',(0.97682056579306,0.,0.214059763252521)) ;
#10523 = DIRECTION('',(-0.976820565793055,1.61327935040072E-15,-0.214059763252546)) ;
#10524 = DIRECTION('',(0.,-1.,-8.88178419700125E-15)) ;
#10525 = DIRECTION('',(-0.976820565793055,2.41991902560109E-15,-0.214059763252546)) ;
#10526 = DIRECTION('center_axis',(-4.16654738518614E-16,1.,1.06536625491829E-14)) ;
#10527 = DIRECTION('ref_axis',(0.964358670083603,-2.41713830372618E-15,0.264598479652823)) ;
#10528 = DIRECTION('',(0.,-1.,-5.9211894646675E-15)) ;
#10529 = DIRECTION('center_axis',(3.60484251114169E-16,1.,1.01050337219711E-14)) ;
#10530 = DIRECTION('ref_axis',(0.964358670083581,-3.02141267266539E-15,0.264598479652902)) ;
#10531 = DIRECTION('center_axis',(0.950291449108004,-4.53195111194576E-15,
0.311361785953592)) ;
#10532 = DIRECTION('ref_axis',(0.311361785953592,0.,-0.950291449108004)) ;
#10533 = DIRECTION('',(-0.311361785953556,-9.70957220772521E-15,0.950291449108015)) ;
#10534 = DIRECTION('',(0.,-1.,-1.1842378929335E-14)) ;
#10535 = DIRECTION('',(-0.311361785953559,-9.70957220772529E-15,0.950291449108014)) ;
#10536 = DIRECTION('center_axis',(-0.314992674102648,-1.6116694398679E-14,
0.949094102426974)) ;
#10537 = DIRECTION('ref_axis',(0.949094102426974,0.,0.314992674102648)) ;
#10538 = DIRECTION('',(-0.949094102426984,8.06639675200338E-16,-0.314992674102618)) ;
#10539 = DIRECTION('',(0.,-1.,-1.1842378929335E-14)) ;
#10540 = DIRECTION('',(-0.949094102426984,1.61327935040068E-15,-0.314992674102618)) ;
#10541 = DIRECTION('center_axis',(-1.06044466970472E-16,1.,1.06621542785655E-14)) ;
#10542 = DIRECTION('ref_axis',(0.931417739925256,-3.78173973070147E-15,0.363951911318692)) ;
#10543 = DIRECTION('',(0.,-1.,-1.03620815631681E-14)) ;
#10544 = DIRECTION('center_axis',(2.78715990627001E-16,1.,9.72764976003551E-15)) ;
#10545 = DIRECTION('ref_axis',(0.93141773992525,-3.79999774087469E-15,0.363951911318705)) ;
#10546 = DIRECTION('center_axis',(0.912539484113185,-3.16975044997102E-15,
0.408988618343399)) ;
#10547 = DIRECTION('ref_axis',(0.408988618343399,0.,-0.912539484113185)) ;
#10548 = DIRECTION('',(-0.408988618343402,-9.29344768453725E-15,0.912539484113183)) ;
#10549 = DIRECTION('',(0.,-1.,-5.9211894646675E-15)) ;
#10550 = DIRECTION('',(-0.408988618343399,-9.2934476845372E-15,0.912539484113185)) ;
#10551 = DIRECTION('center_axis',(-0.412474459298762,-8.54656819163357E-15,
0.910969165464009)) ;
#10552 = DIRECTION('ref_axis',(0.910969165464009,0.,0.412474459298762)) ;
#10553 = DIRECTION('',(-0.910969165464023,3.22655870080118E-15,-0.412474459298732)) ;
#10554 = DIRECTION('',(0.,-1.,-5.9211894646675E-15)) ;
#10555 = DIRECTION('',(-0.910969165464023,4.83983805120177E-15,-0.412474459298732)) ;
#10556 = DIRECTION('center_axis',(-4.7928013500189E-17,1.,9.98863037990808E-15)) ;
#10557 = DIRECTION('ref_axis',(0.888272002096688,-4.54538271531492E-15,0.459317809682079)) ;
#10558 = DIRECTION('',(0.,-1.,-1.1842378929335E-14)) ;
#10559 = DIRECTION('center_axis',(2.30672676937894E-16,1.,1.00715009843182E-14)) ;
#10560 = DIRECTION('ref_axis',(0.888272002096683,-4.83091985290065E-15,0.459317809682087)) ;
#10561 = DIRECTION('center_axis',(0.864789545569235,-4.95945989665175E-15,
0.502134485844337)) ;
#10562 = DIRECTION('ref_axis',(0.502134485844337,0.,-0.864789545569235)) ;
#10563 = DIRECTION('',(-0.502134485844335,-8.32249046376412E-15,0.864789545569236)) ;
#10564 = DIRECTION('',(0.,-1.,-4.44089209850063E-15)) ;
#10565 = DIRECTION('',(-0.50213448584433,-8.32249046376404E-15,0.864789545569239)) ;
#10566 = DIRECTION('center_axis',(-0.505437088002973,-8.877387526951E-15,
0.862863459691668)) ;
#10567 = DIRECTION('ref_axis',(0.862863459691668,0.,0.505437088002973)) ;
#10568 = DIRECTION('',(-0.862863459691667,4.83983805120085E-15,-0.505437088002975)) ;
#10569 = DIRECTION('',(0.,-1.,-4.44089209850063E-15)) ;
#10570 = DIRECTION('',(-0.862863459691667,1.61327935040028E-15,-0.505437088002975)) ;
#10571 = DIRECTION('center_axis',(-3.12375763769512E-16,1.,1.04175774898207E-14)) ;
#10572 = DIRECTION('ref_axis',(0.835394170330091,-5.46507838902905E-15,0.549651326004494)) ;
#10573 = DIRECTION('',(0.,-1.,-5.9211894646675E-15)) ;
#10574 = DIRECTION('center_axis',(3.27850817823959E-16,1.,1.00244112908562E-14)) ;
#10575 = DIRECTION('ref_axis',(0.835394170330105,-5.78381562038142E-15,0.549651326004473)) ;
#10576 = DIRECTION('center_axis',(0.807564791795142,-6.61148326513208E-15,
0.589778862840022)) ;
#10577 = DIRECTION('ref_axis',(0.589778862840022,0.,-0.807564791795142)) ;
#10578 = DIRECTION('',(-0.589778862840036,-8.32249046376468E-15,0.807564791795131)) ;
#10579 = DIRECTION('',(0.,-1.,-1.03620815631681E-14)) ;
#10580 = DIRECTION('',(-0.589778862840039,-8.4611986381608E-15,0.807564791795129)) ;
#10581 = DIRECTION('center_axis',(-0.592862042201395,-1.10336639724356E-14,
0.805304041289246)) ;
#10582 = DIRECTION('ref_axis',(0.805304041289246,0.,0.592862042201395)) ;
#10583 = DIRECTION('',(-0.805304041289226,7.25975707680362E-15,-0.592862042201421)) ;
#10584 = DIRECTION('',(0.,-1.,-1.1842378929335E-14)) ;
#10585 = DIRECTION('',(-0.80530404128922,7.25975707680356E-15,-0.59286204220143)) ;
#10586 = DIRECTION('center_axis',(8.05508786178003E-16,1.,9.79559856706725E-15)) ;
#10587 = DIRECTION('ref_axis',(0.773363585216148,-6.83299574258059E-15,0.633962747376868)) ;
#10588 = DIRECTION('',(0.,-1.,-1.1842378929335E-14)) ;
#10589 = DIRECTION('center_axis',(-6.98671796633277E-16,1.,1.0449544858123E-14)) ;
#10590 = DIRECTION('ref_axis',(0.773363585216172,-6.08429484155941E-15,0.633962747376838)) ;
#10591 = DIRECTION('center_axis',(0.741492189168412,-6.18313970631509E-15,
0.670961499195174)) ;
#10592 = DIRECTION('ref_axis',(0.670961499195174,0.,-0.741492189168412)) ;
#10593 = DIRECTION('',(-0.670961499195179,-7.21282506859625E-15,0.741492189168408)) ;
#10594 = DIRECTION('',(0.,-1.,-4.44089209850062E-15)) ;
#10595 = DIRECTION('',(-0.670961499195173,-7.62894959178444E-15,0.741492189168413)) ;
#10596 = DIRECTION('center_axis',(-0.673791475801331,-6.49989590464668E-15,
0.738921543289586)) ;
#10597 = DIRECTION('ref_axis',(0.738921543289586,0.,0.673791475801331)) ;
#10598 = DIRECTION('',(-0.738921543289622,6.45311740160379E-15,-0.673791475801293)) ;
#10599 = DIRECTION('',(0.,-1.,-8.88178419700125E-15)) ;
#10600 = DIRECTION('',(-0.738921543289602,7.25975707680407E-15,-0.673791475801314)) ;
#10601 = DIRECTION('center_axis',(5.76177143425464E-16,1.,9.72978509576633E-15)) ;
#10602 = DIRECTION('ref_axis',(0.702859866825769,-7.3260436732026E-15,0.711328340223882)) ;
#10603 = DIRECTION('',(0.,-1.,-1.1842378929335E-14)) ;
#10604 = DIRECTION('center_axis',(-4.52089530171145E-16,1.,1.04074137845229E-14)) ;
#10605 = DIRECTION('ref_axis',(0.702859866825789,-7.08533278639819E-15,0.711328340223862)) ;
#10606 = DIRECTION('center_axis',(0.667295642949931,-5.98026974983842E-15,
0.744792940957444)) ;
#10607 = DIRECTION('ref_axis',(0.744792940957444,0.,-0.667295642949931)) ;
#10608 = DIRECTION('',(-0.744792940957427,-6.65799237101186E-15,0.66729564294995)) ;
#10609 = DIRECTION('',(0.,-1.,-1.1842378929335E-14)) ;
#10610 = DIRECTION('',(-0.744792940957427,-6.65799237101186E-15,0.66729564294995)) ;
#10611 = DIRECTION('center_axis',(-0.747338708992256,-6.73908241214502E-15,
0.664443266232556)) ;
#10612 = DIRECTION('ref_axis',(0.664443266232556,0.,0.747338708992256)) ;
#10613 = DIRECTION('',(-0.66444326623258,8.06639675199954E-15,-0.747338708992235)) ;
#10614 = DIRECTION('',(0.,-1.,-1.03620815631681E-14)) ;
#10615 = DIRECTION('',(-0.664443266232586,7.25975707679966E-15,-0.74733870899223)) ;
#10616 = DIRECTION('center_axis',(-2.40293164046626E-18,1.,1.01147575739767E-14)) ;
#10617 = DIRECTION('ref_axis',(0.624655468651339,-7.89711794837585E-15,0.780900470920575)) ;
#10618 = DIRECTION('',(0.,-1.,-1.1842378929335E-14)) ;
#10619 = DIRECTION('center_axis',(-2.40293164048761E-18,1.,1.01147575739767E-14)) ;
#10620 = DIRECTION('ref_axis',(0.624655468651347,-7.89711794837578E-15,0.780900470920569)) ;
#10621 = DIRECTION('center_axis',(0.585788066026616,-8.98424710862706E-15,
0.81046427540071)) ;
#10622 = DIRECTION('ref_axis',(0.81046427540071,0.,-0.585788066026616)) ;
#10623 = DIRECTION('',(-0.81046427540072,-5.40961880144683E-15,0.585788066026602)) ;
#10624 = DIRECTION('',(0.,-1.,-1.03620815631681E-14)) ;
#10625 = DIRECTION('',(-0.810464275400719,-6.10315967342718E-15,0.585788066026603)) ;
#10626 = DIRECTION('center_axis',(-0.812697942896984,-6.2108132023361E-15,
0.582685209706759)) ;
#10627 = DIRECTION('ref_axis',(0.582685209706759,0.,0.812697942896984)) ;
#10628 = DIRECTION('',(-0.582685209706789,7.25975707680523E-15,-0.812697942896963)) ;
#10629 = DIRECTION('',(0.,-1.,-1.1842378929335E-14)) ;
#10630 = DIRECTION('',(-0.582685209706783,8.87303642720631E-15,-0.812697942896967)) ;
#10631 = DIRECTION('center_axis',(-2.58097566505664E-16,1.,1.01309728578212E-14)) ;
#10632 = DIRECTION('ref_axis',(0.53960721444501,-8.39016587899778E-15,0.841916892643744)) ;
#10633 = DIRECTION('',(0.,-1.,-1.03620815631681E-14)) ;
#10634 = DIRECTION('center_axis',(-1.15038675022374E-16,1.,1.01713935082179E-14)) ;
#10635 = DIRECTION('ref_axis',(0.539607214444995,-8.50139231731336E-15,0.841916892643753)) ;
#10636 = DIRECTION('center_axis',(0.497862472467958,-8.95314996644656E-15,
0.867255993642069)) ;
#10637 = DIRECTION('ref_axis',(0.867255993642069,0.,-0.497862472467958)) ;
#10638 = DIRECTION('',(-0.867255993642076,-4.99349427825883E-15,0.497862472467946)) ;
#10639 = DIRECTION('',(0.,-1.,-1.1842378929335E-14)) ;
#10640 = DIRECTION('',(-0.867255993642077,-4.99349427825884E-15,0.497862472467944)) ;
#10641 = DIRECTION('center_axis',(-0.869153088071225,-5.21179790260549E-15,
0.494543132088854)) ;
#10642 = DIRECTION('ref_axis',(0.494543132088854,0.,0.869153088071225)) ;
#10643 = DIRECTION('',(-0.494543132088752,8.87303642720399E-15,-0.869153088071283)) ;
#10644 = DIRECTION('',(0.,-1.,-1.03620815631681E-14)) ;
#10645 = DIRECTION('',(-0.494543132088758,9.67967610240446E-15,-0.86915308807128)) ;
#10646 = DIRECTION('center_axis',(8.69948525886045E-17,1.,1.01282337442175E-14)) ;
#10647 = DIRECTION('ref_axis',(0.448646910677143,-9.09072460265772E-15,0.893709096708686)) ;
#10648 = DIRECTION('',(0.,-1.,-1.03620815631681E-14)) ;
#10649 = DIRECTION('center_axis',(-1.11840364983332E-16,1.,1.03692241613454E-14)) ;
#10650 = DIRECTION('ref_axis',(0.4486469106771,-9.21689312456731E-15,0.893709096708708)) ;
#10651 = DIRECTION('center_axis',(0.404482193476513,-9.52526104942849E-15,
0.91454587373211)) ;
#10652 = DIRECTION('ref_axis',(0.91454587373211,0.,-0.404482193476513)) ;
#10653 = DIRECTION('',(-0.914545873732115,-4.57736975507068E-15,0.404482193476501)) ;
#10654 = DIRECTION('',(0.,-1.,-1.03620815631681E-14)) ;
#10655 = DIRECTION('',(-0.914545873732115,-4.57736975507068E-15,0.404482193476501)) ;
#10656 = DIRECTION('center_axis',(-0.916085610130591,-4.35036638410241E-15,
0.400982736425975)) ;
#10657 = DIRECTION('ref_axis',(0.400982736425975,0.,0.916085610130591)) ;
#10658 = DIRECTION('',(-0.400982736425998,1.04863157776022E-14,-0.916085610130581)) ;
#10659 = DIRECTION('',(0.,-1.,-1.33226762955019E-14)) ;
#10660 = DIRECTION('',(-0.400982736425988,1.04863157776019E-14,-0.916085610130585)) ;
#10661 = DIRECTION('center_axis',(-1.19510675862447E-15,1.,1.03007299649568E-14)) ;
#10662 = DIRECTION('ref_axis',(0.352771137470432,-9.21689312456767E-15,0.935709636889467)) ;
#10663 = DIRECTION('',(0.,-1.,-9.62193288008469E-15)) ;
#10664 = DIRECTION('center_axis',(2.62874961807059E-16,1.,1.00597569142651E-14)) ;
#10665 = DIRECTION('ref_axis',(0.352771137470435,-9.5057461887325E-15,0.935709636889465)) ;
#10666 = DIRECTION('center_axis',(0.306670322929972,-9.16808398683043E-15,
0.951815797848526)) ;
#10667 = DIRECTION('ref_axis',(0.951815797848526,0.,-0.306670322929972)) ;
#10668 = DIRECTION('',(-0.951815797848531,-3.32899618550598E-15,0.306670322929957)) ;
#10669 = DIRECTION('',(0.,-1.,-1.03620815631681E-14)) ;
#10670 = DIRECTION('',(-0.951815797848531,-3.32899618550598E-15,0.306670322929957)) ;
#10671 = DIRECTION('center_axis',(-0.952981306542044,-2.78616357327354E-15,
0.303029089992064)) ;
#10672 = DIRECTION('ref_axis',(0.303029089992064,0.,0.952981306542044)) ;
#10673 = DIRECTION('',(-0.303029089992085,8.87303642720486E-15,-0.952981306542038)) ;
#10674 = DIRECTION('',(0.,-1.,-9.62193288008469E-15)) ;
#10675 = DIRECTION('',(-0.303029089992087,8.87303642720491E-15,-0.952981306542037)) ;
#10676 = DIRECTION('center_axis',(4.41761309766277E-16,1.,1.03191000423786E-14)) ;
#10677 = DIRECTION('ref_axis',(0.253030329859623,-1.00950784740764E-14,0.967458346478612)) ;
#10678 = DIRECTION('',(0.,-1.,-1.11022302462516E-14)) ;
#10679 = DIRECTION('center_axis',(-1.64998512723164E-15,1.,1.01729446383235E-14)) ;
#10680 = DIRECTION('ref_axis',(0.253030329859623,-9.42440391760401E-15,0.967458346478612)) ;
#10681 = DIRECTION('center_axis',(0.205498508150586,-1.03749921183994E-14,
0.978657428903436)) ;
#10682 = DIRECTION('ref_axis',(0.978657428903436,0.,-0.205498508150586)) ;
#10683 = DIRECTION('',(-0.978657428903435,-2.35803896473325E-15,0.205498508150591)) ;
#10684 = DIRECTION('',(0.,-1.,-1.11022302462516E-14)) ;
#10685 = DIRECTION('',(-0.978657428903435,-2.21933079033718E-15,0.205498508150591)) ;
#10686 = DIRECTION('center_axis',(-0.979435940335074,-1.96062109375471E-15,
0.201755393434598)) ;
#10687 = DIRECTION('ref_axis',(0.201755393434598,0.,0.979435940335074)) ;
#10688 = DIRECTION('',(-0.201755393434827,1.04863157776031E-14,-0.979435940335027)) ;
#10689 = DIRECTION('',(0.,-1.,-9.25185853854297E-15)) ;
#10690 = DIRECTION('',(-0.20175539343483,9.67967610240306E-15,-0.979435940335026)) ;
#10691 = DIRECTION('center_axis',(1.16349434456036E-16,1.,1.01634702626516E-14)) ;
#10692 = DIRECTION('ref_axis',(0.15051726900468,-1.00651943068888E-14,0.988607379970114)) ;
#10693 = DIRECTION('',(0.,-1.,-9.99200722162641E-15)) ;
#10694 = DIRECTION('center_axis',(-1.54373974013215E-17,1.,1.02473462852837E-14)) ;
#10695 = DIRECTION('ref_axis',(0.150517269004685,-1.01282785678434E-14,0.988607379970113)) ;
#10696 = DIRECTION('center_axis',(0.102075208712476,-1.03071176810047E-14,
0.994776684370067)) ;
#10697 = DIRECTION('ref_axis',(0.994776684370067,0.,-0.102075208712476)) ;
#10698 = DIRECTION('',(-0.994776684370067,-1.24837356956462E-15,0.10207520871248)) ;
#10699 = DIRECTION('',(0.,-1.,-9.99200722162641E-15)) ;
#10700 = DIRECTION('',(-0.994776684370067,-1.10966539516855E-15,0.10207520871248)) ;
#10701 = DIRECTION('center_axis',(-0.995159669005516,-1.00726298496902E-15,
0.0982712225670959)) ;
#10702 = DIRECTION('ref_axis',(0.0982712225670959,0.,0.995159669005516)) ;
#10703 = DIRECTION('',(-0.0982712225669734,1.20995951280066E-14,-0.995159669005528)) ;
#10704 = DIRECTION('',(0.,-1.,-9.80697005085555E-15)) ;
#10705 = DIRECTION('',(-0.0982712225669735,1.04863157776057E-14,-0.995159669005528)) ;
#10706 = DIRECTION('center_axis',(-1.01419216451375E-15,1.,9.837244959081E-15)) ;
#10707 = DIRECTION('ref_axis',(0.0463551094529302,-9.77965716930322E-15,0.99892502412724)) ;
#10708 = DIRECTION('',(0.,-1.,-1.02001740387436E-14)) ;
#10709 = DIRECTION('center_axis',(7.57942546382629E-16,1.,1.03782113655385E-14)) ;
#10710 = DIRECTION('ref_axis',(0.0463551094529352,-1.04021895484147E-14,0.99892502412724)) ;
#10711 = DIRECTION('center_axis',(-0.00246644807291988,-1.01845851894549E-14,
0.999996958312326)) ;
#10712 = DIRECTION('ref_axis',(0.999996958312326,0.,0.00246644807291987)) ;
#10713 = DIRECTION('',(-0.999996958312326,0.,-0.00246644807291069)) ;
#10714 = DIRECTION('',(0.,-1.,-1.01886092155704E-14)) ;
#10715 = DIRECTION('',(-0.999996958312326,0.,-0.00246644807291067)) ;
#10716 = DIRECTION('center_axis',(-0.9999802200918,6.40022194237738E-17,-0.0062896283798014)) ;
#10717 = DIRECTION('ref_axis',(-0.0062896283798014,0.,0.9999802200918)) ;
#10718 = DIRECTION('',(0.00628962837972571,1.20995951280024E-14,-0.9999802200918)) ;
#10719 = DIRECTION('',(0.,-1.,-1.01307850997045E-14)) ;
#10720 = DIRECTION('',(0.00628962837972571,8.87303642720178E-15,-0.9999802200918)) ;
#10721 = DIRECTION('center_axis',(1.24526289911119E-15,1.,1.07188166549086E-14)) ;
#10722 = DIRECTION('ref_axis',(-0.0583149263784924,-1.06279583516244E-14,
0.998298236681539)) ;
#10723 = DIRECTION('',(0.,-1.,-1.01770443923973E-14)) ;
#10724 = DIRECTION('center_axis',(-1.3595468835695E-15,1.,9.57556002417888E-15)) ;
#10725 = DIRECTION('ref_axis',(-0.0583149263784947,-9.63854656379947E-15,
0.998298236681539)) ;
#10726 = DIRECTION('center_axis',(-0.106981081936937,-9.97833486220179E-15,
0.9942610563165)) ;
#10727 = DIRECTION('ref_axis',(0.9942610563165,0.,0.106981081936937)) ;
#10728 = DIRECTION('',(-0.9942610563165,8.3224904637647E-16,-0.106981081936942)) ;
#10729 = DIRECTION('',(0.,-1.,-1.01770443923973E-14)) ;
#10730 = DIRECTION('',(-0.9942610563165,1.10966539516863E-15,-0.106981081936942)) ;
#10731 = DIRECTION('center_axis',(-0.993844778627483,1.14948413007461E-15,
-0.110781568841076)) ;
#10732 = DIRECTION('ref_axis',(-0.110781568841076,0.,0.993844778627483)) ;
#10733 = DIRECTION('',(0.110781568841025,1.20995951280029E-14,-0.993844778627488)) ;
#10734 = DIRECTION('',(0.,-1.,-9.99200722162641E-15)) ;
#10735 = DIRECTION('',(0.110781568841026,1.12929554528027E-14,-0.993844778627488)) ;
#10736 = DIRECTION('center_axis',(-2.06325056525915E-16,1.,9.99663592581918E-15)) ;
#10737 = DIRECTION('ref_axis',(-0.162346051673367,-9.89751546077705E-15,0.986733884847414)) ;
#10738 = DIRECTION('',(0.,-1.,-9.99200722162641E-15)) ;
#10739 = DIRECTION('center_axis',(2.54720187971674E-16,1.,1.01700699513823E-14)) ;
#10740 = DIRECTION('ref_axis',(-0.162346051673361,-9.99379981549869E-15,0.986733884847414)) ;
#10741 = DIRECTION('center_axis',(-0.21032360868011,-1.0737514915797E-14,
0.977631822125168)) ;
#10742 = DIRECTION('ref_axis',(0.977631822125168,0.,0.21032360868011)) ;
#10743 = DIRECTION('',(-0.977631822125166,2.21933079033706E-15,-0.210323608680118)) ;
#10744 = DIRECTION('',(0.,-1.,-1.11022302462516E-14)) ;
#10745 = DIRECTION('',(-0.977631822125166,2.21933079033706E-15,-0.210323608680119)) ;
#10746 = DIRECTION('center_axis',(-0.976820565792972,2.30207841056971E-15,
-0.214059763252926)) ;
#10747 = DIRECTION('ref_axis',(-0.214059763252926,0.,0.976820565792972)) ;
#10748 = DIRECTION('',(0.214059763252875,1.04863157776044E-14,-0.976820565792983)) ;
#10749 = DIRECTION('',(0.,-1.,-9.99200722162641E-15)) ;
#10750 = DIRECTION('',(0.214059763252877,1.04863157776045E-14,-0.976820565792982)) ;
#10751 = DIRECTION('center_axis',(3.14375358646724E-16,1.,1.04029311063133E-14)) ;
#10752 = DIRECTION('ref_axis',(-0.264598479652911,-9.94897356471713E-15,0.964358670083578)) ;
#10753 = DIRECTION('',(0.,-1.,-1.03620815631681E-14)) ;
#10754 = DIRECTION('center_axis',(-2.57388810828378E-16,1.,9.91553448107732E-15)) ;
#10755 = DIRECTION('ref_axis',(-0.264598479652907,-9.63023633336446E-15,0.96435867008358)) ;
#10756 = DIRECTION('center_axis',(-0.311361785953514,-1.0310618920799E-14,
0.950291449108029)) ;
#10757 = DIRECTION('ref_axis',(0.950291449108029,0.,0.311361785953514)) ;
#10758 = DIRECTION('',(-0.950291449108031,3.19028801110968E-15,-0.311361785953507)) ;
#10759 = DIRECTION('',(0.,-1.,-1.11022302462516E-14)) ;
#10760 = DIRECTION('',(-0.950291449108031,3.19028801110968E-15,-0.311361785953508)) ;
#10761 = DIRECTION('center_axis',(-0.949094102427042,3.05407571808092E-15,
-0.314992674102442)) ;
#10762 = DIRECTION('ref_axis',(-0.314992674102442,0.,0.949094102427042)) ;
#10763 = DIRECTION('',(0.314992674102518,8.87303642720378E-15,-0.949094102427017)) ;
#10764 = DIRECTION('',(0.,-1.,-8.88178419700125E-15)) ;
#10765 = DIRECTION('',(0.314992674102523,1.04863157776047E-14,-0.949094102427015)) ;
#10766 = DIRECTION('center_axis',(2.13050222577358E-16,1.,1.04778275683277E-14)) ;
#10767 = DIRECTION('ref_axis',(-0.363951911318568,-9.68169443730498E-15,0.931417739925304)) ;
#10768 = DIRECTION('',(0.,-1.,-1.1842378929335E-14)) ;
#10769 = DIRECTION('center_axis',(-4.07408769772116E-16,1.,9.65434384961991E-15)) ;
#10770 = DIRECTION('ref_axis',(-0.363951911318561,-9.14050432932127E-15,0.931417739925307)) ;
#10771 = DIRECTION('center_axis',(-0.408988618343441,-9.7764772913756E-15,
0.912539484113166)) ;
#10772 = DIRECTION('ref_axis',(0.912539484113166,0.,0.408988618343441)) ;
#10773 = DIRECTION('',(-0.912539484113162,4.29995340627867E-15,-0.408988618343449)) ;
#10774 = DIRECTION('',(0.,-1.,-1.33226762955019E-14)) ;
#10775 = DIRECTION('',(-0.912539484113162,4.16124523188258E-15,-0.408988618343451)) ;
#10776 = DIRECTION('center_axis',(-0.910969165464027,4.61117069050101E-15,
-0.412474459298723)) ;
#10777 = DIRECTION('ref_axis',(-0.412474459298723,0.,0.910969165464027)) ;
#10778 = DIRECTION('',(0.412474459298713,8.06639675200559E-15,-0.910969165464032)) ;
#10779 = DIRECTION('',(0.,-1.,-1.1842378929335E-14)) ;
#10780 = DIRECTION('',(0.412474459298718,8.87303642720626E-15,-0.91096916546403)) ;
#10781 = DIRECTION('center_axis',(5.92970049971339E-16,1.,1.08173517202205E-14)) ;
#10782 = DIRECTION('ref_axis',(-0.459317809681956,-9.33638896534518E-15,0.888272002096751)) ;
#10783 = DIRECTION('',(0.,-1.,-1.1842378929335E-14)) ;
#10784 = DIRECTION('center_axis',(-6.34736289703598E-16,1.,9.60689667364641E-15)) ;
#10785 = DIRECTION('ref_axis',(-0.459317809681976,-8.82508302454874E-15,0.888272002096741)) ;
#10786 = DIRECTION('center_axis',(-0.502134485844411,-9.34725315396912E-15,
0.864789545569192)) ;
#10787 = DIRECTION('ref_axis',(0.864789545569192,0.,0.502134485844411)) ;
#10788 = DIRECTION('',(-0.864789545569198,4.85478610386242E-15,-0.502134485844401)) ;
#10789 = DIRECTION('',(0.,-1.,-1.03620815631681E-14)) ;
#10790 = DIRECTION('',(-0.864789545569198,5.13220245265457E-15,-0.502134485844399)) ;
#10791 = DIRECTION('center_axis',(-0.862863459691754,4.75053847963801E-15,
-0.505437088002826)) ;
#10792 = DIRECTION('ref_axis',(-0.505437088002826,0.,0.862863459691754)) ;
#10793 = DIRECTION('',(0.505437088002901,9.67967610240523E-15,-0.86286345969171)) ;
#10794 = DIRECTION('',(0.,-1.,-1.03620815631681E-14)) ;
#10795 = DIRECTION('',(0.505437088002901,9.67967610240523E-15,-0.86286345969171)) ;
#10796 = DIRECTION('center_axis',(-2.06384456131493E-16,1.,1.00148389344165E-14)) ;
#10797 = DIRECTION('ref_axis',(-0.549651326004506,-8.47977755258572E-15,0.835394170330083)) ;
#10798 = DIRECTION('',(0.,-1.,-1.1842378929335E-14)) ;
#10799 = DIRECTION('center_axis',(4.94903174920278E-16,1.,1.07067666570303E-14)) ;
#10800 = DIRECTION('ref_axis',(-0.5496513260045,-8.67234626202893E-15,0.835394170330087)) ;
#10801 = DIRECTION('center_axis',(-0.589778862840025,-8.99774787762385E-15,
0.80756479179514)) ;
#10802 = DIRECTION('ref_axis',(0.80756479179514,0.,0.589778862840025)) ;
#10803 = DIRECTION('',(-0.807564791795133,6.10315967342726E-15,-0.589778862840033)) ;
#10804 = DIRECTION('',(0.,-1.,-1.1842378929335E-14)) ;
#10805 = DIRECTION('',(-0.807564791795133,6.10315967342726E-15,-0.589778862840033)) ;
#10806 = DIRECTION('center_axis',(-0.805304041289175,6.46502283087815E-15,
-0.592862042201491)) ;
#10807 = DIRECTION('ref_axis',(-0.592862042201491,0.,0.805304041289175)) ;
#10808 = DIRECTION('',(0.592862042201495,7.25975707680057E-15,-0.805304041289172)) ;
#10809 = DIRECTION('',(0.,-1.,-1.03620815631681E-14)) ;
#10810 = DIRECTION('',(0.592862042201501,8.06639675200072E-15,-0.805304041289168)) ;
#10811 = DIRECTION('center_axis',(-5.37378105936948E-17,1.,1.01243572961915E-14)) ;
#10812 = DIRECTION('ref_axis',(-0.633962747376891,-7.86387702663371E-15,0.773363585216129)) ;
#10813 = DIRECTION('',(0.,-1.,-1.1842378929335E-14)) ;
#10814 = DIRECTION('center_axis',(-5.95031163058821E-17,1.,9.97580953733601E-15)) ;
#10815 = DIRECTION('ref_axis',(-0.633962747376891,-7.75265058831819E-15,0.773363585216129)) ;
#10816 = DIRECTION('center_axis',(-0.670961499195151,-8.51234557961098E-15,
0.741492189168433)) ;
#10817 = DIRECTION('ref_axis',(0.741492189168433,0.,0.670961499195151)) ;
#10818 = DIRECTION('',(-0.741492189168433,6.79670054540769E-15,-0.670961499195151)) ;
#10819 = DIRECTION('',(0.,-1.,-8.88178419700125E-15)) ;
#10820 = DIRECTION('',(-0.741492189168435,6.79670054540771E-15,-0.670961499195149)) ;
#10821 = DIRECTION('center_axis',(-0.738921543289562,8.37973499779816E-15,
-0.673791475801358)) ;
#10822 = DIRECTION('ref_axis',(-0.673791475801358,0.,0.738921543289562)) ;
#10823 = DIRECTION('',(0.673791475801357,8.87303642720419E-15,-0.738921543289563)) ;
#10824 = DIRECTION('',(0.,-1.,-1.1842378929335E-14)) ;
#10825 = DIRECTION('',(0.673791475801344,8.87303642720402E-15,-0.738921543289574)) ;
#10826 = DIRECTION('center_axis',(3.31674154241743E-16,1.,1.07847814889023E-14)) ;
#10827 = DIRECTION('ref_axis',(0.711328340223895,7.34426085540283E-15,-0.702859866825755)) ;
#10828 = DIRECTION('',(0.,-1.,-8.88178419700125E-15)) ;
#10829 = DIRECTION('center_axis',(1.96148416490426E-16,1.,1.05791281541831E-14)) ;
#10830 = DIRECTION('ref_axis',(0.711328340223907,7.2961186780419E-15,-0.702859866825744)) ;
#10831 = DIRECTION('center_axis',(-0.744792940957456,-6.11851680912663E-15,
0.667295642949918)) ;
#10832 = DIRECTION('ref_axis',(0.667295642949918,0.,0.744792940957456)) ;
#10833 = DIRECTION('',(-0.667295642949917,7.49024141738854E-15,-0.744792940957456)) ;
#10834 = DIRECTION('',(0.,-1.,-1.03620815631681E-14)) ;
#10835 = DIRECTION('',(-0.667295642949916,7.62894959178462E-15,-0.744792940957457)) ;
#10836 = DIRECTION('center_axis',(-0.664443266232475,7.93440611492218E-15,
-0.747338708992329)) ;
#10837 = DIRECTION('ref_axis',(-0.747338708992329,0.,0.664443266232475)) ;
#10838 = DIRECTION('',(0.747338708992195,6.45311740160396E-15,-0.664443266232626)) ;
#10839 = DIRECTION('',(0.,-1.,-8.88178419700125E-15)) ;
#10840 = DIRECTION('',(0.747338708992201,6.45311740160402E-15,-0.664443266232618)) ;
#10841 = DIRECTION('center_axis',(-2.4269460922747E-16,1.,9.29325279088581E-15)) ;
#10842 = DIRECTION('ref_axis',(0.780900470920493,5.99460151202269E-15,-0.624655468651442)) ;
#10843 = DIRECTION('',(0.,-1.,-1.03620815631681E-14)) ;
#10844 = DIRECTION('center_axis',(2.14289630963276E-17,1.,1.03888328400212E-14)) ;
#10845 = DIRECTION('ref_axis',(0.780900470920472,6.47270735905191E-15,-0.624655468651468)) ;
#10846 = DIRECTION('center_axis',(-0.810464275400682,-6.27451715502398E-15,
0.585788066026653)) ;
#10847 = DIRECTION('ref_axis',(0.585788066026653,0.,0.810464275400682)) ;
#10848 = DIRECTION('',(-0.585788066026645,8.3224904637648E-15,-0.810464275400688)) ;
#10849 = DIRECTION('',(0.,-1.,-5.9211894646675E-15)) ;
#10850 = DIRECTION('',(-0.585788066026648,8.46119863816093E-15,-0.810464275400686)) ;
#10851 = DIRECTION('center_axis',(-0.582685209706604,6.72659363941242E-15,
-0.812697942897096)) ;
#10852 = DIRECTION('ref_axis',(-0.812697942897096,0.,0.582685209706604)) ;
#10853 = DIRECTION('',(0.812697942897149,4.83983805120176E-15,-0.582685209706529)) ;
#10854 = DIRECTION('',(0.,-1.,-5.9211894646675E-15)) ;
#10855 = DIRECTION('',(0.812697942897149,4.83983805120176E-15,-0.582685209706529)) ;
#10856 = DIRECTION('center_axis',(-1.70957791178252E-16,1.,9.90719736310644E-15)) ;
#10857 = DIRECTION('ref_axis',(0.841916892643665,5.48992742438604E-15,-0.539607214445132)) ;
#10858 = DIRECTION('',(0.,-1.,-8.88178419700125E-15)) ;
#10859 = DIRECTION('center_axis',(1.88267979523057E-16,1.,1.08245441680019E-14)) ;
#10860 = DIRECTION('ref_axis',(0.841916892643639,5.68249613382989E-15,-0.539607214445174)) ;
#10861 = DIRECTION('center_axis',(-0.867255993642078,-4.40191700704748E-15,
0.497862472467942)) ;
#10862 = DIRECTION('ref_axis',(0.497862472467942,0.,0.867255993642078)) ;
#10863 = DIRECTION('',(-0.497862472467943,8.59990681255647E-15,-0.867255993642077)) ;
#10864 = DIRECTION('',(0.,-1.,-7.40148683083438E-15)) ;
#10865 = DIRECTION('',(-0.497862472467944,9.01603133574471E-15,-0.867255993642077)) ;
#10866 = DIRECTION('center_axis',(-0.494543132088875,7.68473217341133E-15,
-0.869153088071213)) ;
#10867 = DIRECTION('ref_axis',(-0.869153088071213,0.,0.494543132088875)) ;
#10868 = DIRECTION('',(0.869153088071255,5.64647772640236E-15,-0.494543132088801)) ;
#10869 = DIRECTION('',(0.,-1.,-7.40148683083438E-15)) ;
#10870 = DIRECTION('',(0.869153088071255,4.83983805120202E-15,-0.494543132088801)) ;
#10871 = DIRECTION('center_axis',(-3.1221234649742E-17,1.,9.70267745702815E-15)) ;
#10872 = DIRECTION('ref_axis',(0.893709096708702,4.38097896780909E-15,-0.448646910677112)) ;
#10873 = DIRECTION('',(0.,-1.,-7.40148683083438E-15)) ;
#10874 = DIRECTION('center_axis',(3.41210259861974E-17,1.,9.94014515725119E-15)) ;
#10875 = DIRECTION('ref_axis',(0.893709096708695,4.42912114517003E-15,-0.448646910677125)) ;
#10876 = DIRECTION('center_axis',(-0.914545873732137,-4.20941261989503E-15,
0.404482193476453)) ;
#10877 = DIRECTION('ref_axis',(0.404482193476453,0.,0.914545873732137)) ;
#10878 = DIRECTION('',(-0.404482193476438,9.57086403332927E-15,-0.914545873732144)) ;
#10879 = DIRECTION('',(0.,-1.,-8.88178419700125E-15)) ;
#10880 = DIRECTION('',(-0.404482193476437,9.2934476845371E-15,-0.914545873732144)) ;
#10881 = DIRECTION('center_axis',(-0.400982736425726,9.53362691950711E-15,
-0.9160856101307)) ;
#10882 = DIRECTION('ref_axis',(-0.9160856101307,0.,0.400982736425726)) ;
#10883 = DIRECTION('',(0.916085610130674,3.22655870080186E-15,-0.400982736425785)) ;
#10884 = DIRECTION('',(0.,-1.,-8.88178419700125E-15)) ;
#10885 = DIRECTION('',(0.916085610130674,4.03319837600232E-15,-0.400982736425785)) ;
#10886 = DIRECTION('center_axis',(-2.01056104879991E-17,1.,1.08924721297816E-14)) ;
#10887 = DIRECTION('ref_axis',(0.935709636889487,3.86136279657659E-15,-0.352771137470377)) ;
#10888 = DIRECTION('',(0.,-1.,-8.88178419700125E-15)) ;
#10889 = DIRECTION('center_axis',(-7.13111576134709E-17,1.,1.00319524838657E-14)) ;
#10890 = DIRECTION('ref_axis',(0.935709636889487,3.60570982617873E-15,-0.352771137470377)) ;
#10891 = DIRECTION('center_axis',(-0.951815797848514,-3.21985774616526E-15,
0.30667032293001)) ;
#10892 = DIRECTION('ref_axis',(0.30667032293001,0.,0.951815797848514)) ;
#10893 = DIRECTION('',(-0.306670322930025,9.84828038212145E-15,-0.951815797848509)) ;
#10894 = DIRECTION('',(0.,-1.,-8.88178419700125E-15)) ;
#10895 = DIRECTION('',(-0.306670322930025,9.70957220772538E-15,-0.951815797848509)) ;
#10896 = DIRECTION('center_axis',(-0.303029089991788,9.05281451950862E-15,
-0.952981306542132)) ;
#10897 = DIRECTION('ref_axis',(-0.952981306542132,0.,0.303029089991788)) ;
#10898 = DIRECTION('',(0.952981306542113,3.22655870080145E-15,-0.303029089991849)) ;
#10899 = DIRECTION('',(0.,-1.,-8.88178419700125E-15)) ;
#10900 = DIRECTION('',(0.952981306542113,2.41991902560109E-15,-0.303029089991849)) ;
#10901 = DIRECTION('center_axis',(1.68432817896581E-16,1.,1.04523873599391E-14)) ;
#10902 = DIRECTION('ref_axis',(0.967458346478576,2.48181928601245E-15,-0.253030329859762)) ;
#10903 = DIRECTION('',(0.,-1.,-8.88178419700125E-15)) ;
#10904 = DIRECTION('center_axis',(-4.04932785370262E-17,1.,9.96192856271833E-15)) ;
#10905 = DIRECTION('ref_axis',(0.967458346478598,2.55984563056011E-15,-0.253030329859679)) ;
#10906 = DIRECTION('center_axis',(-0.978657428903448,-2.07313293814295E-15,
0.205498508150528)) ;
#10907 = DIRECTION('ref_axis',(0.205498508150528,0.,0.978657428903448)) ;
#10908 = DIRECTION('',(-0.20549850815054,1.01256967309133E-14,-0.978657428903445)) ;
#10909 = DIRECTION('',(0.,-1.,-5.9211894646675E-15)) ;
#10910 = DIRECTION('',(-0.205498508150541,9.84828038212124E-15,-0.978657428903445)) ;
#10911 = DIRECTION('center_axis',(-0.201755393434603,8.89276926769736E-15,
-0.979435940335073)) ;
#10912 = DIRECTION('ref_axis',(-0.979435940335073,0.,0.201755393434603)) ;
#10913 = DIRECTION('',(0.979435940335075,2.41991902560011E-15,-0.201755393434595)) ;
#10914 = DIRECTION('',(0.,-1.,-8.88178419700125E-15)) ;
#10915 = DIRECTION('',(0.979435940335069,2.4199190256001E-15,-0.20175539343462)) ;
#10916 = DIRECTION('center_axis',(-8.02786814923323E-17,1.,9.6305190171109E-15)) ;
#10917 = DIRECTION('ref_axis',(0.988607379970119,1.52892351853044E-15,-0.150517269004647)) ;
#10918 = DIRECTION('',(0.,-1.,-2.96059473233375E-15)) ;
#10919 = DIRECTION('center_axis',(4.25238749047059E-17,1.,1.08782409716021E-14)) ;
#10920 = DIRECTION('ref_axis',(0.988607379970123,1.59532370606395E-15,-0.150517269004616)) ;
#10921 = DIRECTION('center_axis',(-0.994776684370068,-8.31135026344039E-16,
0.102075208712465)) ;
#10922 = DIRECTION('ref_axis',(0.102075208712465,0.,0.994776684370068)) ;
#10923 = DIRECTION('',(-0.102075208712471,1.01256967309134E-14,-0.994776684370068)) ;
#10924 = DIRECTION('',(0.,-1.,-1.1842378929335E-14)) ;
#10925 = DIRECTION('',(-0.10207520871247,1.04031130797054E-14,-0.994776684370068)) ;
#10926 = DIRECTION('center_axis',(-0.0982712225670478,1.21544506469537E-14,
-0.995159669005521)) ;
#10927 = DIRECTION('ref_axis',(-0.995159669005521,0.,0.0982712225670478)) ;
#10928 = DIRECTION('',(0.995159669005524,0.,-0.0982712225670169)) ;
#10929 = DIRECTION('',(0.,-1.,-5.9211894646675E-15)) ;
#10930 = DIRECTION('',(0.995159669005529,0.,-0.0982712225669658)) ;
#10931 = DIRECTION('center_axis',(-3.35936425939149E-17,1.,1.04131322768018E-14)) ;
#10932 = DIRECTION('ref_axis',(0.998925024127235,5.1625941667882E-16,-0.0463551094530441)) ;
#10933 = DIRECTION('',(0.,-1.,-5.9211894646675E-15)) ;
#10934 = DIRECTION('center_axis',(1.13981116732401E-16,1.,9.43907375433126E-15)) ;
#10935 = DIRECTION('ref_axis',(0.998925024127238,3.23690707234739E-16,-0.0463551094529721)) ;
#10936 = DIRECTION('center_axis',(-0.999996958312326,3.165819530985E-17,-0.0024664480727807)) ;
#10937 = DIRECTION('ref_axis',(-0.0024664480727807,0.,0.999996958312326)) ;
#10938 = DIRECTION('',(0.00246644807278117,9.98698855651831E-15,-0.999996958312326)) ;
#10939 = DIRECTION('',(0.,-1.,-8.88178419700125E-15)) ;
#10940 = DIRECTION('',(0.00246644807278116,9.84828038212218E-15,-0.999996958312326)) ;
#10941 = DIRECTION('center_axis',(0.00628962837951835,1.23218756090995E-14,
-0.999980220091801)) ;
#10942 = DIRECTION('ref_axis',(-0.999980220091801,0.,-0.00628962837951835)) ;
#10943 = DIRECTION('',(0.999980220091801,0.,0.00628962837952207)) ;
#10944 = DIRECTION('',(0.,-1.,-5.9211894646675E-15)) ;
#10945 = DIRECTION('',(0.999980220091801,0.,0.00628962837954788)) ;
#10946 = DIRECTION('center_axis',(2.0993999114902E-16,1.,9.8718297718797E-15)) ;
#10947 = DIRECTION('ref_axis',(0.998298236681533,-7.85257749342236E-16,0.0583149263785996)) ;
#10948 = DIRECTION('',(0.,-1.,-8.88178419700125E-15)) ;
#10949 = DIRECTION('center_axis',(-2.64718292924584E-16,1.,1.06244133911044E-14)) ;
#10950 = DIRECTION('ref_axis',(0.99829823668153,-3.55294079674656E-16,0.0583149263786514)) ;
#10951 = DIRECTION('center_axis',(-0.994261056316499,1.10829147690483E-15,
-0.106981081936945)) ;
#10952 = DIRECTION('ref_axis',(-0.106981081936945,0.,0.994261056316499)) ;
#10953 = DIRECTION('',(0.106981081937005,1.04031130797057E-14,-0.994261056316493)) ;
#10954 = DIRECTION('',(0.,-1.,-8.88178419700125E-15)) ;
#10955 = DIRECTION('',(0.106981081937005,1.01256967309136E-14,-0.994261056316493)) ;
#10956 = DIRECTION('center_axis',(0.1107815688414,9.26633671878109E-15,-0.993844778627446)) ;
#10957 = DIRECTION('ref_axis',(-0.993844778627446,0.,-0.1107815688414)) ;
#10958 = DIRECTION('',(0.993844778627456,-2.41991902560067E-15,0.110781568841314)) ;
#10959 = DIRECTION('',(0.,-1.,-8.88178419700125E-15)) ;
#10960 = DIRECTION('',(0.993844778627456,0.,0.110781568841314)) ;
#10961 = DIRECTION('center_axis',(9.52458188624454E-19,1.,1.01996408650293E-14)) ;
#10962 = DIRECTION('ref_axis',(0.986733884847386,-1.65681124569414E-15,0.162346051673533)) ;
#10963 = DIRECTION('',(0.,-1.,-8.88178419700125E-15)) ;
#10964 = DIRECTION('center_axis',(-8.57645545929274E-17,1.,1.04301634872781E-14)) ;
#10965 = DIRECTION('ref_axis',(0.98673388484739,-1.60866906833312E-15,0.162346051673509)) ;
#10966 = DIRECTION('center_axis',(-0.977631822125173,2.52799211926821E-15,
-0.210323608680085)) ;
#10967 = DIRECTION('ref_axis',(-0.210323608680085,0.,0.977631822125173)) ;
#10968 = DIRECTION('',(0.210323608680057,1.01256967309132E-14,-0.977631822125179)) ;
#10969 = DIRECTION('',(0.,-1.,-1.1842378929335E-14)) ;
#10970 = DIRECTION('',(0.210323608680056,1.01256967309132E-14,-0.97763182212518)) ;
#10971 = DIRECTION('center_axis',(0.214059763252555,1.1740929645326E-14,-0.976820565793053)) ;
#10972 = DIRECTION('ref_axis',(-0.976820565793053,0.,-0.214059763252555)) ;
#10973 = DIRECTION('',(0.976820565793052,-3.22655870080087E-15,0.21405976325256)) ;
#10974 = DIRECTION('',(0.,-1.,-8.88178419700125E-15)) ;
#10975 = DIRECTION('',(0.976820565793047,-4.03319837600107E-15,0.214059763252584)) ;
#10976 = DIRECTION('center_axis',(1.81080030082074E-16,1.,9.86170298058838E-15)) ;
#10977 = DIRECTION('ref_axis',(0.964358670083573,-2.78401771244109E-15,0.26459847965293)) ;
#10978 = DIRECTION('',(0.,-1.,-5.9211894646675E-15)) ;
#10979 = DIRECTION('center_axis',(-6.26182825359398E-17,1.,1.01475850653259E-14)) ;
#10980 = DIRECTION('ref_axis',(0.964358670083549,-2.62464909676563E-15,0.264598479653017)) ;
#10981 = DIRECTION('center_axis',(-0.950291449108025,2.79072426922236E-15,
-0.311361785953526)) ;
#10982 = DIRECTION('ref_axis',(-0.311361785953526,0.,0.950291449108025)) ;
#10983 = DIRECTION('',(0.311361785953537,9.70957220772551E-15,-0.950291449108022)) ;
#10984 = DIRECTION('',(0.,-1.,-1.1842378929335E-14)) ;
#10985 = DIRECTION('',(0.311361785953534,9.70957220772542E-15,-0.950291449108023)) ;
#10986 = DIRECTION('center_axis',(0.314992674102732,1.05082710782995E-14,
-0.949094102426946)) ;
#10987 = DIRECTION('ref_axis',(-0.949094102426946,0.,-0.314992674102732)) ;
#10988 = DIRECTION('',(0.949094102426945,-3.22655870080122E-15,0.314992674102735)) ;
#10989 = DIRECTION('',(0.,-1.,-1.1842378929335E-14)) ;
#10990 = DIRECTION('',(0.949094102426945,-4.83983805120183E-15,0.314992674102735)) ;
#10991 = DIRECTION('center_axis',(-3.91781290604668E-16,1.,1.06088593500335E-14)) ;
#10992 = DIRECTION('ref_axis',(0.931417739925253,-3.49620259311591E-15,0.363951911318697)) ;
#10993 = DIRECTION('',(0.,-1.,-8.88178419700125E-15)) ;
#10994 = DIRECTION('center_axis',(-1.26280518287485E-16,1.,1.01939480117985E-14)) ;
#10995 = DIRECTION('ref_axis',(0.931417739925251,-3.59248694783763E-15,0.363951911318703)) ;
#10996 = DIRECTION('center_axis',(-0.912539484113164,4.35097671557943E-15,
-0.408988618343445)) ;
#10997 = DIRECTION('ref_axis',(-0.408988618343445,0.,0.912539484113164)) ;
#10998 = DIRECTION('',(0.408988618343461,9.29344768453666E-15,-0.912539484113157)) ;
#10999 = DIRECTION('',(0.,-1.,-1.1842378929335E-14)) ;
#11000 = DIRECTION('',(0.40898861834346,9.43215585893269E-15,-0.912539484113158)) ;
#11001 = DIRECTION('center_axis',(0.412474459298714,9.2066751427435E-15,-0.910969165464031)) ;
#11002 = DIRECTION('ref_axis',(-0.910969165464031,0.,-0.412474459298714)) ;
#11003 = DIRECTION('',(0.910969165464035,-3.22655870080239E-15,0.412474459298706)) ;
#11004 = DIRECTION('',(0.,-1.,-8.88178419700125E-15)) ;
#11005 = DIRECTION('',(0.910969165464025,-4.83983805120353E-15,0.412474459298727)) ;
#11006 = DIRECTION('center_axis',(-2.11241429924909E-16,1.,1.03369922670322E-14)) ;
#11007 = DIRECTION('ref_axis',(0.888272002096608,-4.56032479891027E-15,0.459317809682233)) ;
#11008 = DIRECTION('',(0.,-1.,-1.03620815631681E-14)) ;
#11009 = DIRECTION('center_axis',(-3.55344389385075E-16,1.,1.03735164026929E-14)) ;
#11010 = DIRECTION('ref_axis',(0.888272002096621,-4.4490983605945E-15,0.459317809682208)) ;
#11011 = DIRECTION('center_axis',(-0.864789545569218,5.11990655170529E-15,
-0.502134485844365)) ;
#11012 = DIRECTION('ref_axis',(-0.502134485844365,0.,0.864789545569218)) ;
#11013 = DIRECTION('',(0.502134485844339,8.8773231613489E-15,-0.864789545569234)) ;
#11014 = DIRECTION('',(0.,-1.,-5.9211894646675E-15)) ;
#11015 = DIRECTION('',(0.502134485844341,8.59990681255679E-15,-0.864789545569232)) ;
#11016 = DIRECTION('center_axis',(0.505437088002809,8.79800213895728E-15,
-0.862863459691764)) ;
#11017 = DIRECTION('ref_axis',(-0.862863459691764,0.,-0.505437088002809)) ;
#11018 = DIRECTION('',(0.86286345969171,-7.25975707680022E-15,0.505437088002902)) ;
#11019 = DIRECTION('',(0.,-1.,-4.44089209850063E-15)) ;
#11020 = DIRECTION('',(0.862863459691704,-4.0331983760001E-15,0.505437088002912)) ;
#11021 = DIRECTION('center_axis',(-2.86525193258626E-16,1.,1.02635167737766E-14)) ;
#11022 = DIRECTION('ref_axis',(0.835394170330141,-5.40199412807391E-15,0.549651326004418)) ;
#11023 = DIRECTION('',(0.,-1.,-5.9211894646675E-15)) ;
#11024 = DIRECTION('center_axis',(1.54868887170924E-16,1.,1.01997331986189E-14)) ;
#11025 = DIRECTION('ref_axis',(0.835394170330114,-5.73567344302071E-15,0.54965132600446)) ;
#11026 = DIRECTION('center_axis',(-0.807564791795179,4.15110561799591E-15,
-0.589778862839971)) ;
#11027 = DIRECTION('ref_axis',(-0.589778862839971,0.,0.807564791795179)) ;
#11028 = DIRECTION('',(0.589778862839977,8.32249046376459E-15,-0.807564791795174)) ;
#11029 = DIRECTION('',(0.,-1.,-7.40148683083438E-15)) ;
#11030 = DIRECTION('',(0.589778862839976,8.32249046376458E-15,-0.807564791795175)) ;
#11031 = DIRECTION('center_axis',(0.592862042201329,8.7200926955354E-15,-0.805304041289295)) ;
#11032 = DIRECTION('ref_axis',(-0.805304041289295,0.,-0.592862042201329)) ;
#11033 = DIRECTION('',(0.805304041289269,-5.64647772640202E-15,0.592862042201364)) ;
#11034 = DIRECTION('',(0.,-1.,-8.88178419700125E-15)) ;
#11035 = DIRECTION('',(0.805304041289275,-7.25975707680266E-15,0.592862042201356)) ;
#11036 = DIRECTION('center_axis',(-2.53028520067911E-16,1.,1.0432248940987E-14)) ;
#11037 = DIRECTION('ref_axis',(0.773363585216212,-6.41797415650504E-15,0.633962747376789)) ;
#11038 = DIRECTION('',(0.,-1.,-7.40148683083438E-15)) ;
#11039 = DIRECTION('center_axis',(5.08413268466143E-16,1.,9.80712917849221E-15)) ;
#11040 = DIRECTION('ref_axis',(0.773363585216203,-6.61054286594857E-15,0.6339627473768)) ;
#11041 = DIRECTION('center_axis',(-0.741492189168386,5.86396883463657E-15,
-0.670961499195203)) ;
#11042 = DIRECTION('ref_axis',(-0.670961499195203,0.,0.741492189168386)) ;
#11043 = DIRECTION('',(0.670961499195207,7.76765776618055E-15,-0.741492189168383)) ;
#11044 = DIRECTION('',(0.,-1.,-8.88178419700125E-15)) ;
#11045 = DIRECTION('',(0.670961499195206,7.49024141738837E-15,-0.741492189168384)) ;
#11046 = DIRECTION('center_axis',(0.673791475801613,8.07239481379984E-15,
-0.738921543289329)) ;
#11047 = DIRECTION('ref_axis',(-0.738921543289329,0.,-0.673791475801613)) ;
#11048 = DIRECTION('',(0.738921543289407,-8.06639675200647E-15,0.673791475801528)) ;
#11049 = DIRECTION('',(0.,-1.,-7.40148683083438E-15)) ;
#11050 = DIRECTION('',(0.7389215432894,-6.45311740160512E-15,0.673791475801535)) ;
#11051 = DIRECTION('center_axis',(1.6487047398713E-16,1.,1.00008365712691E-14)) ;
#11052 = DIRECTION('ref_axis',(0.702859866825732,-7.22975931848158E-15,0.711328340223918)) ;
#11053 = DIRECTION('',(0.,-1.,-8.88178419700125E-15)) ;
#11054 = DIRECTION('center_axis',(-6.00426167406994E-16,1.,1.03976200383323E-14)) ;
#11055 = DIRECTION('ref_axis',(0.702859866825719,-6.97410634808367E-15,0.711328340223931)) ;
#11056 = DIRECTION('center_axis',(-0.667295642949829,9.23495925018412E-15,
-0.744792940957535)) ;
#11057 = DIRECTION('ref_axis',(-0.744792940957535,0.,0.667295642949829)) ;
#11058 = DIRECTION('',(0.744792940957537,6.6579923710114E-15,-0.667295642949826)) ;
#11059 = DIRECTION('',(0.,-1.,-8.88178419700125E-15)) ;
#11060 = DIRECTION('',(0.744792940957537,6.93540871980354E-15,-0.667295642949826)) ;
#11061 = DIRECTION('center_axis',(0.747338708992277,7.68942937953467E-15,
-0.664443266232533)) ;
#11062 = DIRECTION('ref_axis',(-0.664443266232533,0.,-0.747338708992277)) ;
#11063 = DIRECTION('',(0.664443266232557,-8.0663967520038E-15,0.747338708992256)) ;
#11064 = DIRECTION('',(0.,-1.,-1.03620815631681E-14)) ;
#11065 = DIRECTION('',(0.664443266232563,-9.67967610240466E-15,0.74733870899225)) ;
#11066 = DIRECTION('center_axis',(-5.86289322685982E-16,1.,1.03160854512866E-14)) ;
#11067 = DIRECTION('ref_axis',(0.62465546865154,-7.68960715533712E-15,0.780900470920414)) ;
#11068 = DIRECTION('',(0.,-1.,-1.03620815631681E-14)) ;
#11069 = DIRECTION('center_axis',(-1.24448328915284E-15,1.,1.03536356505393E-14)) ;
#11070 = DIRECTION('ref_axis',(0.62465546865156,-7.30778566302953E-15,0.780900470920398)) ;
#11071 = DIRECTION('center_axis',(-0.58578806602664,9.01205074559401E-15,
-0.810464275400692)) ;
#11072 = DIRECTION('ref_axis',(-0.810464275400692,0.,0.58578806602664)) ;
#11073 = DIRECTION('',(0.81046427540069,5.96445149903181E-15,-0.585788066026643)) ;
#11074 = DIRECTION('',(0.,-1.,-1.1842378929335E-14)) ;
#11075 = DIRECTION('',(0.810464275400689,5.9644514990318E-15,-0.585788066026645)) ;
#11076 = DIRECTION('center_axis',(0.812697942896958,6.80319698211002E-15,
-0.582685209706796)) ;
#11077 = DIRECTION('ref_axis',(-0.582685209706796,0.,-0.812697942896958)) ;
#11078 = DIRECTION('',(0.582685209706823,-7.25975707680421E-15,0.812697942896939)) ;
#11079 = DIRECTION('',(0.,-1.,-1.33226762955019E-14)) ;
#11080 = DIRECTION('',(0.582685209706829,-7.25975707680429E-15,0.812697942896934)) ;
#11081 = DIRECTION('center_axis',(-5.73712077470761E-16,1.,1.03510063935686E-14)) ;
#11082 = DIRECTION('ref_axis',(0.539607214445007,-8.40510796259135E-15,0.841916892643745)) ;
#11083 = DIRECTION('',(0.,-1.,-1.1842378929335E-14)) ;
#11084 = DIRECTION('center_axis',(5.43474700650759E-16,1.,1.02028490167325E-14)) ;
#11085 = DIRECTION('ref_axis',(0.539607214445004,-8.88321380962026E-15,0.841916892643748)) ;
#11086 = DIRECTION('center_axis',(-0.497862472467949,9.24279903998311E-15,
-0.867255993642074)) ;
#11087 = DIRECTION('ref_axis',(-0.867255993642074,0.,0.497862472467949)) ;
#11088 = DIRECTION('',(0.867255993642073,5.13220245265459E-15,-0.49786247246795)) ;
#11089 = DIRECTION('',(0.,-1.,-1.1842378929335E-14)) ;
#11090 = DIRECTION('',(0.867255993642073,5.13220245265459E-15,-0.49786247246795)) ;
#11091 = DIRECTION('center_axis',(0.869153088071339,5.40930396016028E-15,
-0.494543132088654)) ;
#11092 = DIRECTION('ref_axis',(-0.494543132088654,0.,-0.869153088071339)) ;
#11093 = DIRECTION('',(0.494543132088806,-9.67967610240516E-15,0.869153088071252)) ;
#11094 = DIRECTION('',(0.,-1.,-1.03620815631681E-14)) ;
#11095 = DIRECTION('',(0.494543132088801,-9.67967610240505E-15,0.869153088071255)) ;
#11096 = DIRECTION('center_axis',(2.25044944025704E-16,1.,1.01833866921453E-14)) ;
#11097 = DIRECTION('ref_axis',(0.448646910677237,-9.20195104097265E-15,0.893709096708639)) ;
#11098 = DIRECTION('',(0.,-1.,-1.25825276124184E-14)) ;
#11099 = DIRECTION('center_axis',(8.69948525886785E-17,1.,1.01282337442173E-14)) ;
#11100 = DIRECTION('ref_axis',(0.44864691067723,-9.0907246026572E-15,0.893709096708643)) ;
#11101 = DIRECTION('center_axis',(-0.404482193476504,8.53954795220647E-15,
-0.914545873732114)) ;
#11102 = DIRECTION('ref_axis',(-0.914545873732114,0.,0.404482193476504)) ;
#11103 = DIRECTION('',(0.914545873732116,4.02253705748631E-15,-0.4044821934765)) ;
#11104 = DIRECTION('',(0.,-1.,-1.11022302462516E-14)) ;
#11105 = DIRECTION('',(0.914545873732117,4.02253705748631E-15,-0.404482193476498)) ;
#11106 = DIRECTION('center_axis',(0.916085610130586,4.65184225264105E-15,
-0.400982736425987)) ;
#11107 = DIRECTION('ref_axis',(-0.400982736425986,0.,-0.916085610130586)) ;
#11108 = DIRECTION('',(0.400982736425754,-8.06639675200351E-15,0.916085610130688)) ;
#11109 = DIRECTION('',(0.,-1.,-1.25825276124184E-14)) ;
#11110 = DIRECTION('',(0.400982736425759,-8.87303642720397E-15,0.916085610130686)) ;
#11111 = DIRECTION('center_axis',(5.25932533206529E-16,1.,1.01983188707056E-14)) ;
#11112 = DIRECTION('ref_axis',(0.352771137470506,-9.72819906536265E-15,0.935709636889439)) ;
#11113 = DIRECTION('',(0.,-1.,-1.11022302462516E-14)) ;
#11114 = DIRECTION('center_axis',(-2.23118945004188E-16,1.,1.01400812644954E-14)) ;
#11115 = DIRECTION('ref_axis',(0.35277113747051,-9.40946183401001E-15,0.935709636889437)) ;
#11116 = DIRECTION('center_axis',(-0.306670322929993,8.8306883875111E-15,
-0.95181579784852)) ;
#11117 = DIRECTION('ref_axis',(-0.95181579784852,0.,0.306670322929993)) ;
#11118 = DIRECTION('',(0.951815797848522,2.91287166231757E-15,-0.306670322929987)) ;
#11119 = DIRECTION('',(0.,-1.,-1.03620815631681E-14)) ;
#11120 = DIRECTION('',(0.951815797848522,3.19028801110972E-15,-0.306670322929986)) ;
#11121 = DIRECTION('center_axis',(0.952981306542014,2.98443212964133E-15,
-0.30302908999216)) ;
#11122 = DIRECTION('ref_axis',(-0.30302908999216,0.,-0.952981306542014)) ;
#11123 = DIRECTION('',(0.303029089992011,-9.67967610240377E-15,0.952981306542061)) ;
#11124 = DIRECTION('',(0.,-1.,-9.62193288008469E-15)) ;
#11125 = DIRECTION('',(0.303029089992009,-1.0486315777604E-14,0.952981306542062)) ;
#11126 = DIRECTION('center_axis',(1.94628463640725E-16,1.,1.01538001391442E-14)) ;
#11127 = DIRECTION('ref_axis',(0.253030329859795,-9.87262559744541E-15,0.967458346478567)) ;
#11128 = DIRECTION('',(0.,-1.,-9.25185853854297E-15)) ;
#11129 = DIRECTION('center_axis',(1.05705549506074E-15,1.,1.03726658651972E-14)) ;
#11130 = DIRECTION('ref_axis',(0.253030329859796,-1.03025892671137E-14,0.967458346478567)) ;
#11131 = DIRECTION('center_axis',(-0.205498508150555,1.04287811652079E-14,
-0.978657428903442)) ;
#11132 = DIRECTION('ref_axis',(-0.978657428903442,0.,0.205498508150555)) ;
#11133 = DIRECTION('',(0.978657428903442,1.94191444154532E-15,-0.205498508150555)) ;
#11134 = DIRECTION('',(0.,-1.,-9.99200722162641E-15)) ;
#11135 = DIRECTION('',(0.978657428903442,2.3580389647336E-15,-0.205498508150556)) ;
#11136 = DIRECTION('center_axis',(0.979435940334998,2.23710833589319E-15,
-0.201755393434965)) ;
#11137 = DIRECTION('ref_axis',(-0.201755393434965,0.,-0.979435940334998)) ;
#11138 = DIRECTION('',(0.201755393435196,-8.87303642720528E-15,0.979435940334951)) ;
#11139 = DIRECTION('',(0.,-1.,-1.03620815631681E-14)) ;
#11140 = DIRECTION('',(0.201755393435197,-1.12929554528067E-14,0.979435940334951)) ;
#11141 = DIRECTION('center_axis',(-4.89974951768729E-16,1.,1.0045882123369E-14)) ;
#11142 = DIRECTION('ref_axis',(0.150517269004771,-9.85768351385133E-15,0.9886073799701)) ;
#11143 = DIRECTION('',(0.,-1.,-1.01770443923973E-14)) ;
#11144 = DIRECTION('center_axis',(-1.29687638237839E-16,1.,1.01522328904347E-14)) ;
#11145 = DIRECTION('ref_axis',(0.150517269004776,-1.00170521295277E-14,0.988607379970099)) ;
#11146 = DIRECTION('center_axis',(-0.102075208712513,1.01166708051081E-14,
-0.994776684370064)) ;
#11147 = DIRECTION('ref_axis',(-0.994776684370063,0.,0.102075208712513)) ;
#11148 = DIRECTION('',(0.994776684370064,8.32249046376464E-16,-0.102075208712511)) ;
#11149 = DIRECTION('',(0.,-1.,-1.03620815631681E-14)) ;
#11150 = DIRECTION('',(0.994776684370064,8.32249046376464E-16,-0.102075208712511)) ;
#11151 = DIRECTION('center_axis',(0.995159669005514,1.02795200060226E-15,
-0.0982712225671202)) ;
#11152 = DIRECTION('ref_axis',(-0.0982712225671202,0.,-0.995159669005514)) ;
#11153 = DIRECTION('',(0.0982712225673851,-8.87303642720472E-15,0.995159669005488)) ;
#11154 = DIRECTION('',(0.,-1.,-9.80697005085555E-15)) ;
#11155 = DIRECTION('',(0.0982712225673846,-8.87303642720467E-15,0.995159669005488)) ;
#11156 = DIRECTION('center_axis',(-7.6283654532969E-17,1.,1.01609955402209E-14)) ;
#11157 = DIRECTION('ref_axis',(0.0463551094530843,-1.01465365780165E-14,0.998925024127233)) ;
#11158 = DIRECTION('',(0.,-1.,-1.01886092155704E-14)) ;
#11159 = DIRECTION('center_axis',(-7.6283654532977E-17,1.,1.01609955402209E-14)) ;
#11160 = DIRECTION('ref_axis',(0.0463551094530828,-1.01465365780165E-14,0.998925024127233)) ;
#11161 = DIRECTION('center_axis',(0.00246644807280478,1.01799886558946E-14,
-0.999996958312326)) ;
#11162 = DIRECTION('ref_axis',(-0.999996958312326,0.,-0.00246644807280478)) ;
#11163 = DIRECTION('',(0.999996958312326,0.,0.00246644807279149)) ;
#11164 = DIRECTION('',(0.,-1.,-1.01886092155704E-14)) ;
#11165 = DIRECTION('',(0.999996958312326,0.,0.00246644807279149)) ;
#11166 = DIRECTION('center_axis',(0.9999802200918,-6.40285403098758E-17,0.00628962837969165)) ;
#11167 = DIRECTION('ref_axis',(0.00628962837969165,0.,-0.9999802200918)) ;
#11168 = DIRECTION('',(-0.00628962837970035,-1.04863157776029E-14,0.9999802200918)) ;
#11169 = DIRECTION('',(0.,-1.,-1.022330368509E-14)) ;
#11170 = DIRECTION('',(-0.00628962837970035,-1.04863157776029E-14,0.9999802200918)) ;
#11171 = DIRECTION('center_axis',(-1.30314881765276E-16,1.,1.01745098931728E-14)) ;
#11172 = DIRECTION('ref_axis',(-0.0583149263785945,-1.01647945881894E-14,
0.998298236681534)) ;
#11173 = DIRECTION('',(0.,-1.,-9.43689570931383E-15)) ;
#11174 = DIRECTION('center_axis',(-2.2229329398051E-16,1.,1.0057720993455E-14)) ;
#11175 = DIRECTION('ref_axis',(-0.0583149263785934,-1.00535681498739E-14,
0.998298236681534)) ;
#11176 = DIRECTION('center_axis',(0.10698108193693,9.92439105702673E-15,-0.994261056316501)) ;
#11177 = DIRECTION('ref_axis',(-0.994261056316501,0.,-0.10698108193693)) ;
#11178 = DIRECTION('',(0.994261056316502,-1.10966539516868E-15,0.106981081936923)) ;
#11179 = DIRECTION('',(0.,-1.,-1.03620815631681E-14)) ;
#11180 = DIRECTION('',(0.994261056316502,-1.10966539516868E-15,0.106981081936921)) ;
#11181 = DIRECTION('center_axis',(0.993844778627463,-1.14674067685148E-15,
0.110781568841248)) ;
#11182 = DIRECTION('ref_axis',(0.110781568841248,0.,-0.993844778627463)) ;
#11183 = DIRECTION('',(-0.110781568840856,-9.67967610240325E-15,0.993844778627507)) ;
#11184 = DIRECTION('',(0.,-1.,-1.03620815631681E-14)) ;
#11185 = DIRECTION('',(-0.110781568840856,-9.67967610240325E-15,0.993844778627507)) ;
#11186 = DIRECTION('center_axis',(1.82731126992894E-16,1.,1.03348798985764E-14)) ;
#11187 = DIRECTION('ref_axis',(-0.162346051673409,-1.01681105147685E-14,0.986733884847406)) ;
#11188 = DIRECTION('',(0.,-1.,-1.1842378929335E-14)) ;
#11189 = DIRECTION('center_axis',(-1.27058275890956E-16,1.,1.01223994058069E-14)) ;
#11190 = DIRECTION('ref_axis',(-0.162346051673407,-1.00087418990923E-14,0.986733884847407)) ;
#11191 = DIRECTION('center_axis',(0.210323608680103,1.03556219669971E-14,
-0.977631822125169)) ;
#11192 = DIRECTION('ref_axis',(-0.977631822125169,0.,-0.210323608680103)) ;
#11193 = DIRECTION('',(0.977631822125166,-2.08062261594135E-15,0.210323608680121)) ;
#11194 = DIRECTION('',(0.,-1.,-1.14723045877933E-14)) ;
#11195 = DIRECTION('',(0.977631822125165,-1.80320626714917E-15,0.210323608680122)) ;
#11196 = DIRECTION('center_axis',(0.97682056579313,-2.26744049898666E-15,
0.214059763252206)) ;
#11197 = DIRECTION('ref_axis',(0.214059763252206,0.,-0.976820565793129)) ;
#11198 = DIRECTION('',(-0.214059763252224,-1.04863157776028E-14,0.976820565793125)) ;
#11199 = DIRECTION('',(0.,-1.,-1.03620815631681E-14)) ;
#11200 = DIRECTION('',(-0.214059763252222,-1.04863157776027E-14,0.976820565793126)) ;
#11201 = DIRECTION('center_axis',(6.00257443383549E-16,1.,1.06466294189312E-14)) ;
#11202 = DIRECTION('ref_axis',(-0.264598479653095,-1.01083421803929E-14,0.964358670083528)) ;
#11203 = DIRECTION('',(0.,-1.,-9.62193288008469E-15)) ;
#11204 = DIRECTION('center_axis',(-6.32092923448246E-16,1.,9.8282183636024E-15)) ;
#11205 = DIRECTION('ref_axis',(-0.264598479653085,-9.64517841695802E-15,0.964358670083531)) ;
#11206 = DIRECTION('center_axis',(0.311361785953555,1.015548158715E-14,-0.950291449108016)) ;
#11207 = DIRECTION('ref_axis',(-0.950291449108016,0.,-0.311361785953555)) ;
#11208 = DIRECTION('',(0.950291449108017,-2.91287166231775E-15,0.311361785953551)) ;
#11209 = DIRECTION('',(0.,-1.,-9.62193288008469E-15)) ;
#11210 = DIRECTION('',(0.950291449108017,-3.05157983671383E-15,0.311361785953551)) ;
#11211 = DIRECTION('center_axis',(0.949094102427118,-3.3188211289215E-15,
0.314992674102214)) ;
#11212 = DIRECTION('ref_axis',(0.314992674102214,0.,-0.949094102427118)) ;
#11213 = DIRECTION('',(-0.314992674102324,-1.04863157776006E-14,0.949094102427081)) ;
#11214 = DIRECTION('',(0.,-1.,-1.03620815631681E-14)) ;
#11215 = DIRECTION('',(-0.314992674102326,-9.67967610240063E-15,0.94909410242708)) ;
#11216 = DIRECTION('center_axis',(2.13050222576724E-16,1.,1.04778275683273E-14)) ;
#11217 = DIRECTION('ref_axis',(-0.363951911318812,-9.6816944373038E-15,0.931417739925209)) ;
#11218 = DIRECTION('',(0.,-1.,-1.1842378929335E-14)) ;
#11219 = DIRECTION('center_axis',(-4.57923600694674E-17,1.,1.0205581445571E-14)) ;
#11220 = DIRECTION('ref_axis',(-0.363951911318796,-9.52232582162755E-15,0.931417739925215)) ;
#11221 = DIRECTION('center_axis',(0.4089886183435,9.42299093837688E-15,-0.91253948411314)) ;
#11222 = DIRECTION('ref_axis',(-0.91253948411314,0.,-0.4089886183435)) ;
#11223 = DIRECTION('',(0.912539484113151,-3.88382888309014E-15,0.408988618343474)) ;
#11224 = DIRECTION('',(0.,-1.,-1.03620815631681E-14)) ;
#11225 = DIRECTION('',(0.91253948411315,-4.16124523188229E-15,0.408988618343476)) ;
#11226 = DIRECTION('center_axis',(0.910969165464123,-4.00871546860473E-15,
0.412474459298511)) ;
#11227 = DIRECTION('ref_axis',(0.412474459298511,0.,-0.910969165464123)) ;
#11228 = DIRECTION('',(-0.4124744592984,-1.04863157776079E-14,0.910969165464173)) ;
#11229 = DIRECTION('',(0.,-1.,-1.1842378929335E-14)) ;
#11230 = DIRECTION('',(-0.412474459298405,-8.87303642720676E-15,0.910969165464171)) ;
#11231 = DIRECTION('center_axis',(-2.133261312597E-16,1.,1.00584160089897E-14)) ;
#11232 = DIRECTION('ref_axis',(-0.459317809682225,-9.03259381758412E-15,0.888272002096612)) ;
#11233 = DIRECTION('',(0.,-1.,-1.1842378929335E-14)) ;
#11234 = DIRECTION('center_axis',(9.85116202033927E-17,1.,1.00776264659541E-14)) ;
#11235 = DIRECTION('ref_axis',(-0.459317809682244,-8.90642529567464E-15,0.888272002096602)) ;
#11236 = DIRECTION('center_axis',(0.502134485844415,9.27426518722038E-15,
-0.864789545569189)) ;
#11237 = DIRECTION('ref_axis',(-0.864789545569189,0.,-0.502134485844415)) ;
#11238 = DIRECTION('',(0.86478954556918,-5.40961880144727E-15,0.502134485844432)) ;
#11239 = DIRECTION('',(0.,-1.,-1.03620815631681E-14)) ;
#11240 = DIRECTION('',(0.864789545569179,-4.99349427825901E-15,0.502134485844433)) ;
#11241 = DIRECTION('center_axis',(0.862863459691766,-5.88507142137273E-15,
0.505437088002807)) ;
#11242 = DIRECTION('ref_axis',(0.505437088002807,0.,-0.862863459691766)) ;
#11243 = DIRECTION('',(-0.505437088002738,-7.25975707680418E-15,0.862863459691806)) ;
#11244 = DIRECTION('',(0.,-1.,-1.03620815631681E-14)) ;
#11245 = DIRECTION('',(-0.505437088002738,-1.0486315777606E-14,0.862863459691806)) ;
#11246 = DIRECTION('center_axis',(6.91486274403049E-16,1.,1.10268799478273E-14)) ;
#11247 = DIRECTION('ref_axis',(-0.549651326004292,-8.83171487770677E-15,0.835394170330224)) ;
#11248 = DIRECTION('',(0.,-1.,-1.1842378929335E-14)) ;
#11249 = DIRECTION('center_axis',(-2.27645647850203E-16,1.,9.86770757427363E-15)) ;
#11250 = DIRECTION('ref_axis',(-0.549651326004315,-8.36855111427142E-15,0.835394170330209)) ;
#11251 = DIRECTION('center_axis',(0.589778862839997,7.48932209630947E-15,
-0.80756479179516)) ;
#11252 = DIRECTION('ref_axis',(-0.80756479179516,0.,-0.589778862839997)) ;
#11253 = DIRECTION('',(0.807564791795158,-6.24186784782375E-15,0.589778862839999)) ;
#11254 = DIRECTION('',(0.,-1.,-1.1842378929335E-14)) ;
#11255 = DIRECTION('',(0.807564791795158,-6.10315967342767E-15,0.589778862839999)) ;
#11256 = DIRECTION('center_axis',(0.8053040412894,-5.68145037082667E-15,0.592862042201185)) ;
#11257 = DIRECTION('ref_axis',(0.592862042201185,0.,-0.8053040412894)) ;
#11258 = DIRECTION('',(-0.592862042201501,-8.06639675200317E-15,0.805304041289168)) ;
#11259 = DIRECTION('',(0.,-1.,-1.1842378929335E-14)) ;
#11260 = DIRECTION('',(-0.592862042201501,-8.87303642720349E-15,0.805304041289168)) ;
#11261 = DIRECTION('center_axis',(9.67768243175678E-17,1.,1.01661699844692E-14)) ;
#11262 = DIRECTION('ref_axis',(-0.633962747376858,-7.80079276567923E-15,0.773363585216156)) ;
#11263 = DIRECTION('',(0.,-1.,-8.88178419700125E-15)) ;
#11264 = DIRECTION('center_axis',(-5.9503116306081E-17,1.,9.97580953733579E-15)) ;
#11265 = DIRECTION('ref_axis',(-0.633962747376867,-7.75265058831834E-15,0.773363585216148)) ;
#11266 = DIRECTION('center_axis',(0.670961499195176,6.24391619839882E-15,
-0.741492189168411)) ;
#11267 = DIRECTION('ref_axis',(-0.741492189168411,0.,-0.670961499195176)) ;
#11268 = DIRECTION('',(0.74149218916841,-7.07411689419958E-15,0.670961499195176)) ;
#11269 = DIRECTION('',(0.,-1.,-1.1842378929335E-14)) ;
#11270 = DIRECTION('',(0.741492189168413,-6.79670054540746E-15,0.670961499195174)) ;
#11271 = DIRECTION('center_axis',(0.738921543289395,-5.46368409941558E-15,
0.673791475801542)) ;
#11272 = DIRECTION('ref_axis',(0.673791475801541,0.,-0.738921543289395)) ;
#11273 = DIRECTION('',(-0.67379147580165,-7.25975707680296E-15,0.738921543289296)) ;
#11274 = DIRECTION('',(0.,-1.,-1.1842378929335E-14)) ;
#11275 = DIRECTION('',(-0.67379147580165,-8.06639675200329E-15,0.738921543289296)) ;
#11276 = DIRECTION('center_axis',(7.04164249301842E-17,1.,1.02251381822285E-14)) ;
#11277 = DIRECTION('ref_axis',(0.711328340223902,7.13675006236594E-15,-0.702859866825748)) ;
#11278 = DIRECTION('',(0.,-1.,-8.88178419700125E-15)) ;
#11279 = DIRECTION('center_axis',(-1.81047558190989E-16,1.,9.51715823831775E-15)) ;
#11280 = DIRECTION('ref_axis',(0.71132834022391,6.8180128310131E-15,-0.70285986682574)) ;
#11281 = DIRECTION('center_axis',(0.744792940957504,5.45910190214161E-15,
-0.667295642949863)) ;
#11282 = DIRECTION('ref_axis',(-0.667295642949863,0.,-0.744792940957504)) ;
#11283 = DIRECTION('',(0.667295642949854,-7.62894959178434E-15,0.744792940957512)) ;
#11284 = DIRECTION('',(0.667295642949854,-7.62894959178434E-15,0.744792940957512)) ;
#11285 = DIRECTION('center_axis',(1.01038501025472E-18,1.,1.01832385299507E-14)) ;
#11286 = DIRECTION('ref_axis',(0.,-1.01832385299507E-14,1.)) ;
#11287 = DIRECTION('',(0.685780405335872,-7.40870801634297E-15,0.727808515790635)) ;
#11288 = DIRECTION('center_axis',(2.99231463188634E-15,1.,9.17249458945792E-15)) ;
#11289 = DIRECTION('ref_axis',(-0.727808515790229,-4.21884749357582E-15,0.685780405336303)) ;
#11290 = DIRECTION('center_axis',(-9.73559573494954E-19,1.,1.01191400279987E-14)) ;
#11291 = DIRECTION('ref_axis',(-0.579268556534064,8.25126782750514E-15,-0.815136761170138)) ;
#11292 = DIRECTION('center_axis',(-3.90366527253116E-16,1.,1.16402614894552E-14)) ;
#11293 = DIRECTION('ref_axis',(0.45164185742236,1.06581410364017E-14,-0.89219932337123)) ;
#11294 = DIRECTION('',(0.569953339326871,8.37382706828044E-15,-0.821677060036453)) ;
#11295 = DIRECTION('center_axis',(-1.93203794446472E-16,1.,7.89444606623193E-15)) ;
#11296 = DIRECTION('ref_axis',(0.821677060036449,-4.44089209850189E-15,0.569953339326876)) ;
#11297 = DIRECTION('center_axis',(1.1550026710782E-15,-1.,-7.82090740015345E-15)) ;
#11298 = DIRECTION('ref_axis',(0.0537080995988211,7.86672314592065E-15,-0.998556678430165)) ;
#11299 = DIRECTION('center_axis',(-1.25123697270413E-16,1.,1.09805252983441E-14)) ;
#11300 = DIRECTION('ref_axis',(0.201569759100209,-1.0658141036402E-14,0.979474161076383)) ;
#11301 = DIRECTION('center_axis',(-4.61040819041639E-17,1.,1.0045818217579E-14)) ;
#11302 = DIRECTION('ref_axis',(0.85487989018869,-5.20417042793038E-15,0.51882595670511)) ;
#11303 = DIRECTION('',(0.904104831215912,4.36195963669746E-15,-0.427310723212099)) ;
#11304 = DIRECTION('center_axis',(-3.71070252500866E-16,1.,1.14893261314214E-14)) ;
#11305 = DIRECTION('ref_axis',(0.427310723212573,-1.0214051826551E-14,0.904104831215688)) ;
#11306 = DIRECTION('center_axis',(-6.5542035569204E-17,1.,1.0154433419378E-14)) ;
#11307 = DIRECTION('ref_axis',(-0.954244956658656,-3.10213905535359E-15,0.299026023435283)) ;
#11308 = DIRECTION('center_axis',(-5.51213759928002E-17,1.,9.72049936282107E-15)) ;
#11309 = DIRECTION('ref_axis',(-0.708966971011695,6.88338275267498E-15,-0.705241684824786)) ;
#11310 = DIRECTION('',(-0.605336054385156,8.09943047508256E-15,-0.795970012790313)) ;
#11311 = DIRECTION('center_axis',(-4.37006372857839E-15,1.,1.28163190547884E-14)) ;
#11312 = DIRECTION('ref_axis',(0.795970012790317,1.13242748511803E-14,-0.605336054385151)) ;
#11313 = DIRECTION('center_axis',(4.49394212051378E-16,-1.,-9.96715601710005E-15)) ;
#11314 = DIRECTION('ref_axis',(-0.933087120399413,3.17206578464678E-15,-0.359650421582863)) ;
#11315 = DIRECTION('center_axis',(2.35873547596961E-15,1.,1.17632702241326E-14)) ;
#11316 = DIRECTION('ref_axis',(0.99382376454844,-3.55271367880014E-15,0.110969928443552)) ;
#11317 = DIRECTION('',(-0.12701289025145,1.01053641908739E-14,-0.991901066493011)) ;
#11318 = DIRECTION('center_axis',(1.15531629141496E-15,1.,9.89396570300712E-15)) ;
#11319 = DIRECTION('ref_axis',(0.991901066492928,0.,-0.127012890252103)) ;
#11320 = DIRECTION('center_axis',(1.00617405775911E-16,1.,1.02022269426731E-14)) ;
#11321 = DIRECTION('ref_axis',(-0.0104872602741568,-1.01997769393712E-14,
0.999945007173866)) ;
#11322 = DIRECTION('center_axis',(-4.95744530348576E-16,1.,9.94939236716821E-15)) ;
#11323 = DIRECTION('ref_axis',(-0.889807542408672,-4.8849813083509E-15,0.456335991866343)) ;
#11324 = DIRECTION('',(-0.944071595552654,-3.36845473029134E-15,0.329740538106351)) ;
#11325 = DIRECTION('center_axis',(4.63955102136965E-17,1.,2.22312900262673E-14)) ;
#11326 = DIRECTION('ref_axis',(-0.329740538106308,2.10942374678848E-14,-0.944071595552669)) ;
#11327 = DIRECTION('center_axis',(2.20937231112283E-15,-1.,-1.67700671001831E-14)) ;
#11328 = DIRECTION('ref_axis',(-0.630387654470438,-1.44011786622908E-14,0.776280493823759)) ;
#11329 = DIRECTION('center_axis',(2.8694095257642E-15,1.,9.77672005189204E-15)) ;
#11330 = DIRECTION('ref_axis',(0.412647106218261,7.77156117237546E-15,-0.910890973569118)) ;
#11331 = DIRECTION('',(-0.982603114400669,1.89239029791646E-15,-0.185717849357851)) ;
#11332 = DIRECTION('center_axis',(2.32293377607812E-15,1.,9.72874974239161E-15)) ;
#11333 = DIRECTION('ref_axis',(0.185717849357345,9.10382880192643E-15,-0.982603114400765)) ;
#11334 = DIRECTION('center_axis',(1.82671911090264E-17,1.,1.01683562978219E-14)) ;
#11335 = DIRECTION('ref_axis',(0.94776347336036,-3.26392862059879E-15,0.318973977878926)) ;
#11336 = DIRECTION('center_axis',(-4.9958972588217E-16,1.,1.09497348570251E-14)) ;
#11337 = DIRECTION('ref_axis',(0.159035666357331,-1.06581410364028E-14,0.987272838087973)) ;
#11338 = DIRECTION('',(0.0218677205202773,-1.01810598027907E-14,0.999760872808717)) ;
#11339 = DIRECTION('center_axis',(-2.90264567693173E-16,1.,9.90066071632332E-15)) ;
#11340 = DIRECTION('ref_axis',(-0.999760872808717,-4.4408920985022E-16,0.0218677205202719)) ;
#11341 = DIRECTION('center_axis',(1.25843900772593E-14,-1.,4.50134704742774E-15)) ;
#11342 = DIRECTION('ref_axis',(0.543486123848407,1.06264203785598E-14,0.839418151569427)) ;
#11343 = DIRECTION('center_axis',(-2.52101501674842E-16,1.,9.31589964004196E-15)) ;
#11344 = DIRECTION('ref_axis',(-0.738793827546322,5.99520433297592E-15,-0.673931510154746)) ;
#11345 = DIRECTION('',(-0.480269231899665,-8.93208220616572E-15,0.877121123272325)) ;
#11346 = DIRECTION('center_axis',(-5.02745638862898E-16,1.,8.71829150130473E-15)) ;
#11347 = DIRECTION('ref_axis',(-0.877121123272599,3.77475828372576E-15,-0.480269231899166)) ;
#11348 = DIRECTION('center_axis',(-2.09226926848338E-18,1.,1.02438071869812E-14)) ;
#11349 = DIRECTION('ref_axis',(0.596237300106514,8.22313051181033E-15,-0.802808247317935)) ;
#11350 = DIRECTION('center_axis',(-6.55287701147568E-16,1.,1.11149082005131E-14)) ;
#11351 = DIRECTION('ref_axis',(0.988096989640894,-1.11022302462509E-15,0.153832178241753)) ;
#11352 = DIRECTION('',(0.957586590090667,-2.94266691326012E-15,0.288145661911694)) ;
#11353 = DIRECTION('center_axis',(3.1901714689479E-15,1.,8.32778241288616E-15)) ;
#11354 = DIRECTION('ref_axis',(-0.288145661911686,-7.10542735760418E-15,0.95758659009067)) ;
#11355 = DIRECTION('center_axis',(2.16932355798421E-14,-1.,-1.82594434819788E-14)) ;
#11356 = DIRECTION('ref_axis',(0.966280551422668,2.56620121977777E-14,-0.25749154538024)) ;
#11357 = DIRECTION('center_axis',(-1.0463360744244E-14,1.,5.55222444913644E-15)) ;
#11358 = DIRECTION('ref_axis',(-0.869246802320409,-1.17683640610269E-14,0.494378394204019)) ;
#11359 = DIRECTION('center_axis',(-1.01038501025472E-18,-1.,-1.01832385299507E-14)) ;
#11360 = DIRECTION('ref_axis',(0.,1.01832385299507E-14,-1.)) ;
#11361 = DIRECTION('center_axis',(1.27732005678872E-17,1.,1.01872910948437E-14)) ;
#11362 = DIRECTION('ref_axis',(-0.567531504838376,-8.38184392457865E-15,0.823351681249202)) ;
#11363 = DIRECTION('center_axis',(-9.9248854779219E-16,1.,1.0123642478546E-14)) ;
#11364 = DIRECTION('ref_axis',(0.053708099598814,1.0162335480767E-14,-0.998556678430165)) ;
#11365 = DIRECTION('',(0.,-1.,-1.03620815631681E-14)) ;
#11366 = DIRECTION('center_axis',(-1.27095136349964E-15,-1.,-2.69759843588644E-14)) ;
#11367 = DIRECTION('ref_axis',(0.0537080995988265,2.68673971959465E-14,-0.998556678430164)) ;
#11368 = DIRECTION('',(0.,-1.,-1.03620815631681E-14)) ;
#11369 = DIRECTION('center_axis',(1.36053615763085E-16,-1.,-1.01410167552715E-14)) ;
#11370 = DIRECTION('ref_axis',(0.201569759100217,-9.90543958427637E-15,0.979474161076381)) ;
#11371 = DIRECTION('center_axis',(-7.84926116427115E-17,1.,1.00769224206684E-14)) ;
#11372 = DIRECTION('ref_axis',(0.201569759100214,-9.76996261670192E-15,0.979474161076382)) ;
#11373 = DIRECTION('',(0.,-1.,-9.99200722162641E-15)) ;
#11374 = DIRECTION('center_axis',(0.727808515790636,7.02309814391564E-15,
-0.685780405335871)) ;
#11375 = DIRECTION('ref_axis',(-0.685780405335871,0.,-0.727808515790636)) ;
#11376 = DIRECTION('',(0.,-1.,-1.1842378929335E-14)) ;
#11377 = DIRECTION('',(0.685780405335872,-7.39924606485339E-15,0.727808515790635)) ;
#11378 = DIRECTION('center_axis',(1.88696881337211E-17,-1.,-1.02210045222401E-14)) ;
#11379 = DIRECTION('ref_axis',(-0.727808515790264,-7.02309814391841E-15,0.685780405336265)) ;
#11380 = DIRECTION('center_axis',(2.99231463188634E-15,1.,9.17249458945792E-15)) ;
#11381 = DIRECTION('ref_axis',(-0.727808515790229,-4.21884749357582E-15,0.685780405336303)) ;
#11382 = DIRECTION('',(0.,-1.,-8.88178419700125E-15)) ;
#11383 = DIRECTION('center_axis',(-8.16917681390859E-16,-1.,-9.66049649164156E-15)) ;
#11384 = DIRECTION('ref_axis',(-0.579268556534065,8.34784054759856E-15,-0.815136761170137)) ;
#11385 = DIRECTION('center_axis',(1.12759823687013E-17,1.,1.01917284713483E-14)) ;
#11386 = DIRECTION('ref_axis',(-0.579268556534064,8.31457678781848E-15,-0.815136761170138)) ;
#11387 = DIRECTION('',(0.,-1.,-8.88178419700125E-15)) ;
#11388 = DIRECTION('center_axis',(5.64135403633836E-16,-1.,-9.18738132441649E-15)) ;
#11389 = DIRECTION('ref_axis',(0.45164185742237,8.45176256273169E-15,-0.892199323371225)) ;
#11390 = DIRECTION('center_axis',(-5.55151177432328E-15,1.,1.23389758122368E-14)) ;
#11391 = DIRECTION('ref_axis',(0.451641857422362,1.35447209004271E-14,-0.892199323371229)) ;
#11392 = DIRECTION('',(0.,-1.,-8.88178419700125E-15)) ;
#11393 = DIRECTION('center_axis',(-0.821677060036453,5.25321865069352E-15,
-0.569953339326871)) ;
#11394 = DIRECTION('ref_axis',(-0.569953339326871,0.,0.821677060036453)) ;
#11395 = DIRECTION('',(0.569953339326872,8.37382706828045E-15,-0.821677060036452)) ;
#11396 = DIRECTION('',(0.,-1.,-9.99200722162641E-15)) ;
#11397 = DIRECTION('center_axis',(1.15120034560029E-17,-1.,-1.01296141149143E-14)) ;
#11398 = DIRECTION('ref_axis',(0.821677060036409,-5.76394824173468E-15,0.569953339326935)) ;
#11399 = DIRECTION('center_axis',(2.83896812655439E-15,1.,1.61596563378519E-14)) ;
#11400 = DIRECTION('ref_axis',(0.821677060036451,-1.15463194561049E-14,0.569953339326874)) ;
#11401 = DIRECTION('center_axis',(4.35568030595358E-19,-1.,-1.01768969648663E-14)) ;
#11402 = DIRECTION('ref_axis',(0.997217727878536,7.59060640552051E-16,-0.0745439682655105)) ;
#11403 = DIRECTION('center_axis',(8.35722644427098E-17,1.,1.0193865474578E-14)) ;
#11404 = DIRECTION('ref_axis',(0.85487989018869,-5.34294830600853E-15,0.51882595670511)) ;
#11405 = DIRECTION('',(-4.35568030595358E-19,1.,1.01768969648663E-14)) ;
#11406 = DIRECTION('center_axis',(3.00697478893843E-18,1.,1.01692228197527E-14)) ;
#11407 = DIRECTION('ref_axis',(-0.933087120399434,3.66017104374068E-15,-0.35965042158281)) ;
#11408 = DIRECTION('',(0.,-1.,-1.01770443923973E-14)) ;
#11409 = DIRECTION('center_axis',(-5.14081247751989E-15,-1.,-1.14600397072667E-14)) ;
#11410 = DIRECTION('ref_axis',(-0.933087120399412,8.91350485485745E-15,-0.359650421582866)) ;
#11411 = DIRECTION('',(0.,-1.,-1.01770443923973E-14)) ;
#11412 = DIRECTION('center_axis',(-2.48643695099992E-19,-1.,-1.01827982029087E-14)) ;
#11413 = DIRECTION('ref_axis',(0.993823764548442,-1.13023149594521E-15,0.110969928443534)) ;
#11414 = DIRECTION('center_axis',(8.86561589770877E-17,1.,1.04217772078769E-14)) ;
#11415 = DIRECTION('ref_axis',(0.99382376454844,-1.33226762955005E-15,0.110969928443552)) ;
#11416 = DIRECTION('',(0.,-1.,-1.01822847028976E-14)) ;
#11417 = DIRECTION('center_axis',(-0.427310723212094,9.20507379483528E-15,
-0.904104831215914)) ;
#11418 = DIRECTION('ref_axis',(-0.904104831215914,0.,0.427310723212094)) ;
#11419 = DIRECTION('',(0.,-1.,-1.03620815631681E-14)) ;
#11420 = DIRECTION('',(0.904104831215912,4.34303573371829E-15,-0.427310723212099)) ;
#11421 = DIRECTION('center_axis',(1.05573181252421E-16,-1.,-1.01629152374729E-14)) ;
#11422 = DIRECTION('ref_axis',(0.42731072321255,-9.14322821300122E-15,0.904104831215699)) ;
#11423 = DIRECTION('center_axis',(1.37735827364208E-16,1.,9.59365051910165E-15)) ;
#11424 = DIRECTION('ref_axis',(0.427310723212573,-8.65973959207583E-15,0.904104831215688)) ;
#11425 = DIRECTION('',(0.,-1.,-1.03620815631681E-14)) ;
#11426 = DIRECTION('center_axis',(2.24889090216542E-18,-1.,-1.02338540319814E-14)) ;
#11427 = DIRECTION('ref_axis',(-0.954244956658656,-3.06233466840199E-15,0.299026023435285)) ;
#11428 = DIRECTION('center_axis',(8.21270872692169E-19,1.,1.01916550133699E-14)) ;
#11429 = DIRECTION('ref_axis',(-0.954244956658657,-3.04586442396396E-15,0.299026023435282)) ;
#11430 = DIRECTION('',(0.,-1.,-1.1842378929335E-14)) ;
#11431 = DIRECTION('center_axis',(-2.23460467479023E-16,-1.,-1.00163897919004E-14)) ;
#11432 = DIRECTION('ref_axis',(-0.708966971011677,7.22240170347135E-15,-0.705241684824804)) ;
#11433 = DIRECTION('center_axis',(2.75045346022906E-17,1.,1.06984003662012E-14)) ;
#11434 = DIRECTION('ref_axis',(-0.708966971011695,7.54951656744997E-15,-0.705241684824786)) ;
#11435 = DIRECTION('',(0.,-1.,-1.1842378929335E-14)) ;
#11436 = DIRECTION('center_axis',(-0.79597001279031,-6.19926508094888E-15,
0.60533605438516)) ;
#11437 = DIRECTION('ref_axis',(0.60533605438516,0.,0.79597001279031)) ;
#11438 = DIRECTION('',(-0.605336054385156,8.09943047508256E-15,-0.795970012790313)) ;
#11439 = DIRECTION('',(0.,-1.,-9.99200722162641E-15)) ;
#11440 = DIRECTION('center_axis',(-8.09828272505317E-18,-1.,-1.02516792551804E-14)) ;
#11441 = DIRECTION('ref_axis',(0.795970012790343,6.19926508094789E-15,-0.605336054385117)) ;
#11442 = DIRECTION('center_axis',(9.43700811201809E-15,1.,1.03942385143954E-14)) ;
#11443 = DIRECTION('ref_axis',(0.795970012790318,-1.11022302462551E-15,-0.60533605438515)) ;
#11444 = DIRECTION('center_axis',(4.4990462626596E-16,1.,1.05423745132031E-14)) ;
#11445 = DIRECTION('ref_axis',(-0.630387654470441,-7.90022537109696E-15,0.776280493823757)) ;
#11446 = DIRECTION('',(0.,-1.,-1.03620815631681E-14)) ;
#11447 = DIRECTION('center_axis',(-4.63754202816028E-15,-1.,-2.86699818779913E-15)) ;
#11448 = DIRECTION('ref_axis',(-0.630387654470438,6.97854472622012E-16,0.77628049382376)) ;
#11449 = DIRECTION('',(0.,-1.,-9.99200722162641E-15)) ;
#11450 = DIRECTION('center_axis',(9.31785348230183E-17,-1.,-1.00708065010557E-14)) ;
#11451 = DIRECTION('ref_axis',(0.412647106218168,9.21185659112935E-15,-0.91089097356916)) ;
#11452 = DIRECTION('center_axis',(-3.52226263200537E-15,1.,9.96767797577172E-15)) ;
#11453 = DIRECTION('ref_axis',(0.412647106218264,1.04360964314755E-14,-0.910890973569116)) ;
#11454 = DIRECTION('',(0.,-1.,-9.99200722162641E-15)) ;
#11455 = DIRECTION('center_axis',(-0.991901066493012,-1.3007429008436E-15,
0.127012890251444)) ;
#11456 = DIRECTION('ref_axis',(0.127012890251444,0.,0.991901066493012)) ;
#11457 = DIRECTION('',(0.,-1.,-7.40148683083438E-15)) ;
#11458 = DIRECTION('',(-0.12701289025145,1.01148261423635E-14,-0.991901066493011)) ;
#11459 = DIRECTION('center_axis',(3.94655273193483E-17,-1.,-9.93282650058954E-15)) ;
#11460 = DIRECTION('ref_axis',(0.991901066492934,1.30074290085124E-15,-0.127012890252055)) ;
#11461 = DIRECTION('center_axis',(-9.73674917507053E-16,1.,8.39436511489026E-15)) ;
#11462 = DIRECTION('ref_axis',(0.991901066492929,1.99840144432547E-15,-0.127012890252095)) ;
#11463 = DIRECTION('',(0.,-1.,-1.03620815631681E-14)) ;
#11464 = DIRECTION('center_axis',(9.70577347955382E-16,-1.,-9.71879985172455E-15)) ;
#11465 = DIRECTION('ref_axis',(-0.0104872602741544,-9.72844408471828E-15,
0.999945007173866)) ;
#11466 = DIRECTION('center_axis',(-8.65191641729209E-18,1.,1.02495761242682E-14)) ;
#11467 = DIRECTION('ref_axis',(-0.0104872602741568,-1.02490172418371E-14,
0.999945007173866)) ;
#11468 = DIRECTION('',(0.,-1.,-1.11022302462516E-14)) ;
#11469 = DIRECTION('center_axis',(-8.59442262184789E-18,-1.,-1.02577888676658E-14)) ;
#11470 = DIRECTION('ref_axis',(-0.889807542408722,-4.67335087520974E-15,0.456335991866246)) ;
#11471 = DIRECTION('center_axis',(1.04858035239816E-16,1.,1.01895922080626E-14)) ;
#11472 = DIRECTION('ref_axis',(-0.889807542408673,-4.66293670342585E-15,0.456335991866342)) ;
#11473 = DIRECTION('',(0.,-1.,-1.1842378929335E-14)) ;
#11474 = DIRECTION('center_axis',(0.329740538106355,-9.42655948374898E-15,
0.944071595552653)) ;
#11475 = DIRECTION('ref_axis',(0.944071595552653,0.,-0.329740538106355)) ;
#11476 = DIRECTION('',(-0.944071595552654,-3.35899277880175E-15,0.329740538106351)) ;
#11477 = DIRECTION('',(0.,-1.,-9.99200722162641E-15)) ;
#11478 = DIRECTION('center_axis',(2.37459557569859E-17,-1.,-1.01213116247813E-14)) ;
#11479 = DIRECTION('ref_axis',(-0.329740538106337,9.5474128104636E-15,-0.944071595552659)) ;
#11480 = DIRECTION('center_axis',(-3.88792192335817E-16,1.,1.14881096764339E-14)) ;
#11481 = DIRECTION('ref_axis',(-0.32974053810631,1.0658141036405E-14,-0.944071595552669)) ;
#11482 = DIRECTION('center_axis',(2.42728163606961E-16,1.,1.00838748912754E-14)) ;
#11483 = DIRECTION('ref_axis',(0.543486123848403,-8.59650701067922E-15,0.83941815156943)) ;
#11484 = DIRECTION('',(0.,-1.,-9.99200722162641E-15)) ;
#11485 = DIRECTION('center_axis',(1.29625497688541E-14,-1.,4.18092764719124E-15)) ;
#11486 = DIRECTION('ref_axis',(0.543486123848413,1.05629790628669E-14,0.839418151569423)) ;
#11487 = DIRECTION('',(0.,-1.,-9.99200722162641E-15)) ;
#11488 = DIRECTION('center_axis',(-3.28765762400409E-17,-1.,-1.01409834277618E-14)) ;
#11489 = DIRECTION('ref_axis',(-0.738793827546362,6.85861728752183E-15,-0.673931510154701)) ;
#11490 = DIRECTION('center_axis',(2.41297603013022E-16,1.,1.00743387886781E-14)) ;
#11491 = DIRECTION('ref_axis',(-0.73879382754632,6.88338275267602E-15,-0.673931510154747)) ;
#11492 = DIRECTION('',(0.,-1.,-9.99200722162641E-15)) ;
#11493 = DIRECTION('center_axis',(-0.185717849357856,-1.00628686023381E-14,
0.982603114400668)) ;
#11494 = DIRECTION('ref_axis',(0.982603114400668,0.,0.185717849357856)) ;
#11495 = DIRECTION('',(0.,-1.,-9.62193288008469E-15)) ;
#11496 = DIRECTION('',(-0.982603114400669,1.89239029791646E-15,-0.185717849357851)) ;
#11497 = DIRECTION('center_axis',(8.26778425727097E-18,-1.,-1.01114550972676E-14)) ;
#11498 = DIRECTION('ref_axis',(0.185717849357425,9.93708274481032E-15,-0.98260311440075)) ;
#11499 = DIRECTION('center_axis',(4.37018402263533E-15,1.,6.82416255865663E-15)) ;
#11500 = DIRECTION('ref_axis',(0.185717849357345,5.99520433297595E-15,-0.982603114400765)) ;
#11501 = DIRECTION('',(0.,-1.,-9.62193288008469E-15)) ;
#11502 = DIRECTION('center_axis',(3.62128080408835E-17,-1.,-1.0348629313777E-14)) ;
#11503 = DIRECTION('ref_axis',(0.947763473360361,-3.26662228108087E-15,0.318973977878924)) ;
#11504 = DIRECTION('center_axis',(-2.1280459065345E-16,1.,9.97985065191849E-15)) ;
#11505 = DIRECTION('ref_axis',(0.94776347336036,-2.98255546365061E-15,0.318973977878926)) ;
#11506 = DIRECTION('',(0.,-1.,-1.03620815631681E-14)) ;
#11507 = DIRECTION('center_axis',(-2.80344073704828E-16,-1.,-9.93984541648658E-15)) ;
#11508 = DIRECTION('ref_axis',(0.159035666357184,-9.85792410106006E-15,0.987272838087996)) ;
#11509 = DIRECTION('center_axis',(7.4253034470058E-16,1.,9.45879140455388E-15)) ;
#11510 = DIRECTION('ref_axis',(0.159035666357338,-9.54791801177758E-15,0.987272838087971)) ;
#11511 = DIRECTION('',(0.,-1.,-7.40148683083438E-15)) ;
#11512 = DIRECTION('center_axis',(0.999760872808717,2.18349295995649E-16,
-0.0218677205202793)) ;
#11513 = DIRECTION('ref_axis',(-0.0218677205202793,0.,-0.999760872808717)) ;
#11514 = DIRECTION('',(0.0218677205202773,-1.01905217542803E-14,0.999760872808717)) ;
#11515 = DIRECTION('',(0.,-1.,-1.07321559047098E-14)) ;
#11516 = DIRECTION('center_axis',(5.0107008882313E-19,-1.,-1.0282128875273E-14)) ;
#11517 = DIRECTION('ref_axis',(-0.999760872808717,-2.25347670868714E-16,0.0218677205202789)) ;
#11518 = DIRECTION('center_axis',(1.9244387534717E-15,1.,1.1331727736871E-14)) ;
#11519 = DIRECTION('ref_axis',(-0.999760872808717,1.77635683940087E-15,0.0218677205202701)) ;
#11520 = DIRECTION('center_axis',(-1.47015018359715E-17,1.,1.01378559388477E-14)) ;
#11521 = DIRECTION('ref_axis',(0.966280551422667,2.62461796783717E-15,-0.257491545380244)) ;
#11522 = DIRECTION('',(0.,-1.,-1.02695629777827E-14)) ;
#11523 = DIRECTION('center_axis',(1.41800139605514E-14,-1.,-1.62531235822279E-14)) ;
#11524 = DIRECTION('ref_axis',(0.966280551422669,1.78904510253976E-14,-0.257491545380237)) ;
#11525 = DIRECTION('',(0.,-1.,-9.99200722162641E-15)) ;
#11526 = DIRECTION('center_axis',(-1.37590905074469E-17,-1.,-1.02012162869233E-14)) ;
#11527 = DIRECTION('ref_axis',(-0.869246802320393,-5.03130088143227E-15,0.494378394204046)) ;
#11528 = DIRECTION('center_axis',(-5.18014709467136E-15,1.,9.15466687533215E-15)) ;
#11529 = DIRECTION('ref_axis',(-0.869246802320409,-9.10382880192644E-15,0.494378394204018)) ;
#11530 = DIRECTION('',(0.,-1.,-9.99200722162641E-15)) ;
#11531 = DIRECTION('center_axis',(0.877121123272322,-4.85697127072896E-15,
0.480269231899671)) ;
#11532 = DIRECTION('ref_axis',(0.480269231899671,0.,-0.877121123272322)) ;
#11533 = DIRECTION('',(0.,-1.,-1.03620815631681E-14)) ;
#11534 = DIRECTION('',(-0.480269231899665,-8.93208220616572E-15,0.877121123272325)) ;
#11535 = DIRECTION('center_axis',(-3.92906616480111E-17,-1.,-1.0169273661626E-14)) ;
#11536 = DIRECTION('ref_axis',(-0.877121123272574,4.91845191972174E-15,-0.48026923189921)) ;
#11537 = DIRECTION('center_axis',(-6.63014437645751E-16,1.,1.07398920018271E-14)) ;
#11538 = DIRECTION('ref_axis',(-0.877121123272594,4.6629367034259E-15,-0.480269231899175)) ;
#11539 = DIRECTION('',(0.,-1.,-1.1842378929335E-14)) ;
#11540 = DIRECTION('center_axis',(5.50013901675183E-17,-1.,-9.94415591679671E-15)) ;
#11541 = DIRECTION('ref_axis',(0.596237300106512,8.01604426299543E-15,-0.802808247317936)) ;
#11542 = DIRECTION('center_axis',(1.63311325766893E-16,1.,1.01319355034507E-14)) ;
#11543 = DIRECTION('ref_axis',(0.596237300106513,8.03320363087032E-15,-0.802808247317936)) ;
#11544 = DIRECTION('',(0.,-1.,-1.03620815631681E-14)) ;
#11545 = DIRECTION('center_axis',(-1.52159333529704E-17,-1.,-1.01432954457967E-14)) ;
#11546 = DIRECTION('ref_axis',(0.988096989640907,-1.5754000509151E-15,0.153832178241672)) ;
#11547 = DIRECTION('center_axis',(-8.46415552567221E-16,1.,9.70638848492343E-15)) ;
#11548 = DIRECTION('ref_axis',(0.988096989640894,-6.66133814775051E-16,0.153832178241752)) ;
#11549 = DIRECTION('',(0.,-1.,-9.99200722162641E-15)) ;
#11550 = DIRECTION('center_axis',(0.288145661911693,9.745381900288E-15,-0.957586590090668)) ;
#11551 = DIRECTION('ref_axis',(-0.957586590090668,0.,-0.288145661911693)) ;
#11552 = DIRECTION('',(0.957586590090667,-2.91428105879137E-15,0.288145661911694)) ;
#11553 = DIRECTION('',(0.,-1.,-1.01770443923973E-14)) ;
#11554 = DIRECTION('center_axis',(-4.04272951601914E-17,-1.,-1.02051907145046E-14)) ;
#11555 = DIRECTION('ref_axis',(-0.288145661911697,-9.76070482780411E-15,0.957586590090666)) ;
#11556 = DIRECTION('center_axis',(-3.73351796497035E-15,1.,1.37656397128939E-14)) ;
#11557 = DIRECTION('ref_axis',(-0.288145661911685,-1.42108547152084E-14,0.95758659009067)) ;
#11558 = DIRECTION('center_axis',(3.25068633533587E-16,-1.,-1.13443493764018E-14)) ;
#11559 = DIRECTION('ref_axis',(0.016584812332587,-1.13401417803123E-14,0.99986246254167)) ;
#11560 = DIRECTION('',(-3.25068633533587E-16,1.,1.13443493764018E-14)) ;
#11561 = DIRECTION('center_axis',(-8.63182864965974E-18,-1.,-1.0183797638573E-14)) ;
#11562 = DIRECTION('ref_axis',(0.594525808996939,-8.1952846003432E-15,0.804076527723907)) ;
#11563 = DIRECTION('center_axis',(5.42235451464647E-16,1.,1.13299633222955E-14)) ;
#11564 = DIRECTION('ref_axis',(0.0165848123325861,-1.13397508997188E-14,0.99986246254167)) ;
#11565 = DIRECTION('center_axis',(-8.64209275723101E-18,1.,1.01866654475327E-14)) ;
#11566 = DIRECTION('ref_axis',(-0.567531504838378,-8.39360559958068E-15,0.823351681249201)) ;
#11567 = DIRECTION('',(-5.42235451464647E-16,-1.,-1.13299633222955E-14)) ;
#11568 = DIRECTION('center_axis',(-1.30163597487239E-17,-1.,-1.01751445312373E-14)) ;
#11569 = DIRECTION('ref_axis',(0.594525808996942,-8.19172107843299E-15,0.804076527723905)) ;
#11570 = DIRECTION('center_axis',(1.40039764464111E-20,-1.,-1.01816657134689E-14)) ;
#11571 = DIRECTION('ref_axis',(0.,1.01816657134689E-14,-1.)) ;
#11572 = DIRECTION('center_axis',(-1.01038501025472E-18,-1.,-1.01832385299507E-14)) ;
#11573 = DIRECTION('ref_axis',(0.,1.01832385299507E-14,-1.)) ;
#11574 = DIRECTION('',(0.,0.,1.)) ;
#11575 = DIRECTION('',(1.,0.,0.)) ;
#11576 = CARTESIAN_POINT('',(0.,0.,0.)) ;
#11578 = CARTESIAN_POINT('Origin',(-5.63784594171726E-6,12.,130.056019952763)) ;
#11579 = CARTESIAN_POINT('',(-2.69639531535793,12.3,129.132990859662)) ;
#11580 = CARTESIAN_POINT('',(-2.69662395993644,11.7,129.132912589967)) ;
#11581 = CARTESIAN_POINT('Ctrl Pts',(-2.69639531535755,12.3,129.132990859662)) ;
#11582 = CARTESIAN_POINT('Ctrl Pts',(-2.69077162240415,12.3,129.116167020409)) ;
#11583 = CARTESIAN_POINT('Ctrl Pts',(-2.68469199795713,12.2984224191665,129.099524200288)) ;
#11584 = CARTESIAN_POINT('Ctrl Pts',(-2.67835058694966,12.2953054979811,129.083291730847)) ;
#11585 = CARTESIAN_POINT('Ctrl Pts',(-2.67199862621724,12.29218339141,129.067032256677)) ;
#11586 = CARTESIAN_POINT('Ctrl Pts',(-2.66538421612455,12.2875170237535,129.051185110066)) ;
#11587 = CARTESIAN_POINT('Ctrl Pts',(-2.65869785319305,12.2813953186066,129.035967275889)) ;
#11588 = CARTESIAN_POINT('Ctrl Pts',(-2.65198326201708,12.275247769067,129.020685195612)) ;
#11589 = CARTESIAN_POINT('Ctrl Pts',(-2.64519630460819,12.2676328803879,129.006038323483)) ;
#11590 = CARTESIAN_POINT('Ctrl Pts',(-2.63852218903446,12.2586877093307,128.992223877476)) ;
#11591 = CARTESIAN_POINT('Ctrl Pts',(-2.63285454385406,12.2510914885176,128.980492678418)) ;
#11592 = CARTESIAN_POINT('Ctrl Pts',(-2.62726819434588,12.2425369009626,128.969361542656)) ;
#11593 = CARTESIAN_POINT('Ctrl Pts',(-2.62187074130637,12.2331313228689,128.958934247103)) ;
#11594 = CARTESIAN_POINT('Ctrl Pts',(-2.61410225905873,12.2195939996322,128.943926379541)) ;
#11595 = CARTESIAN_POINT('Ctrl Pts',(-2.60671352792775,12.2042653708087,128.930342789742)) ;
#11596 = CARTESIAN_POINT('Ctrl Pts',(-2.5999983071543,12.1874446308271,128.918413851356)) ;
#11597 = CARTESIAN_POINT('Ctrl Pts',(-2.59798504529316,12.1824016761092,128.914837486928)) ;
#11598 = CARTESIAN_POINT('Ctrl Pts',(-2.59603224850718,12.177224876733,128.911409636886)) ;
#11599 = CARTESIAN_POINT('Ctrl Pts',(-2.59414765019636,12.1719230232504,128.908135975523)) ;
#11600 = CARTESIAN_POINT('Ctrl Pts',(-2.58907722564732,12.1576586317889,128.899328341107)) ;
#11601 = CARTESIAN_POINT('Ctrl Pts',(-2.58450466969039,12.1425004895536,128.891649109489)) ;
#11602 = CARTESIAN_POINT('Ctrl Pts',(-2.58058794256455,12.1266788388559,128.885199808432)) ;
#11603 = CARTESIAN_POINT('Ctrl Pts',(-2.57667746312546,12.110882425739,128.878760794845)) ;
#11604 = CARTESIAN_POINT('Ctrl Pts',(-2.57342083523148,12.0944252333348,128.873548122155)) ;
#11605 = CARTESIAN_POINT('Ctrl Pts',(-2.5709605467127,12.0775615159586,128.869619839075)) ;
#11606 = CARTESIAN_POINT('Ctrl Pts',(-2.57022851236607,12.0725438847999,128.868451017566)) ;
#11607 = CARTESIAN_POINT('Ctrl Pts',(-2.56956687301894,12.0674903983032,128.867395596478)) ;
#11608 = CARTESIAN_POINT('Ctrl Pts',(-2.56897911005068,12.0624080546532,128.866454310522)) ;
#11609 = CARTESIAN_POINT('Ctrl Pts',(-2.56704834434127,12.045712863951,128.863362243235)) ;
#11610 = CARTESIAN_POINT('Ctrl Pts',(-2.56591702181591,12.0287200061612,128.861508378651)) ;
#11611 = CARTESIAN_POINT('Ctrl Pts',(-2.56555956232846,12.011690688947,128.860928790889)) ;
#11612 = CARTESIAN_POINT('Ctrl Pts',(-2.56547769957746,12.0077907595744,128.860796057949)) ;
#11613 = CARTESIAN_POINT('Ctrl Pts',(-2.56543635359737,12.0038889319103,128.860729952645)) ;
#11614 = CARTESIAN_POINT('Ctrl Pts',(-2.56543509258672,11.9999883515565,128.860730544395)) ;
#11615 = CARTESIAN_POINT('Ctrl Pts',(-2.56542845485952,11.9794564170477,128.860733659257)) ;
#11616 = CARTESIAN_POINT('Ctrl Pts',(-2.56653357884379,11.9589330509582,128.862588005132)) ;
#11617 = CARTESIAN_POINT('Ctrl Pts',(-2.56882120220927,11.9387964657361,128.866240323405)) ;
#11618 = CARTESIAN_POINT('Ctrl Pts',(-2.57070901888315,11.9221791405632,128.869254328)) ;
#11619 = CARTESIAN_POINT('Ctrl Pts',(-2.57340054229553,11.9058576648792,128.873488140823)) ;
#11620 = CARTESIAN_POINT('Ctrl Pts',(-2.57675906187904,11.8900798109946,128.878905495549)) ;
#11621 = CARTESIAN_POINT('Ctrl Pts',(-2.58012267828092,11.8742780129722,128.884331071539)) ;
#11622 = CARTESIAN_POINT('Ctrl Pts',(-2.58415521179501,11.8590221908532,128.890943477565)) ;
#11623 = CARTESIAN_POINT('Ctrl Pts',(-2.58870394705331,11.8445394749185,128.898661349037)) ;
#11624 = CARTESIAN_POINT('Ctrl Pts',(-2.59046092141454,11.8389454451205,128.901642419935)) ;
#11625 = CARTESIAN_POINT('Ctrl Pts',(-2.59229475598414,11.8334664720546,128.904787970042)) ;
#11626 = CARTESIAN_POINT('Ctrl Pts',(-2.59419609809682,11.8281144498417,128.908091697553)) ;
#11627 = CARTESIAN_POINT('Ctrl Pts',(-2.59928180221649,11.8137988770498,128.916928497888)) ;
#11628 = CARTESIAN_POINT('Ctrl Pts',(-2.60486398800593,11.8003383447438,128.926936410632)) ;
#11629 = CARTESIAN_POINT('Ctrl Pts',(-2.61079581228568,11.7879509898805,128.937988632388)) ;
#11630 = CARTESIAN_POINT('Ctrl Pts',(-2.61671887218773,11.7755819375581,128.949024524286)) ;
#11631 = CARTESIAN_POINT('Ctrl Pts',(-2.62299039132912,11.7642834255358,128.961101212608)) ;
#11632 = CARTESIAN_POINT('Ctrl Pts',(-2.62945152491257,11.7542383902569,128.974055496983)) ;
#11633 = CARTESIAN_POINT('Ctrl Pts',(-2.63590617735524,11.7442034311181,128.98699678696)) ;
#11634 = CARTESIAN_POINT('Ctrl Pts',(-2.64254988476032,11.7354198617474,129.000813389561)) ;
#11635 = CARTESIAN_POINT('Ctrl Pts',(-2.64921409275335,11.728028674419,129.015312836051)) ;
#11636 = CARTESIAN_POINT('Ctrl Pts',(-2.65587755978878,11.7206383088771,129.029810670425)) ;
#11637 = CARTESIAN_POINT('Ctrl Pts',(-2.66256131921654,11.714640322129,129.044990601979)) ;
#11638 = CARTESIAN_POINT('Ctrl Pts',(-2.66908955986842,11.7101287337753,129.060638863111)) ;
#11639 = CARTESIAN_POINT('Ctrl Pts',(-2.67159074995444,11.7084001914828,129.066634241911)) ;
#11640 = CARTESIAN_POINT('Ctrl Pts',(-2.67406905115582,11.7068893270032,129.072698192146)) ;
#11641 = CARTESIAN_POINT('Ctrl Pts',(-2.67651439134326,11.7055994810325,129.078818152777)) ;
#11642 = CARTESIAN_POINT('Ctrl Pts',(-2.68218483507541,11.7026084865535,129.093009590261)) ;
#11643 = CARTESIAN_POINT('Ctrl Pts',(-2.68767315026768,11.7008127780343,129.107487919033)) ;
#11644 = CARTESIAN_POINT('Ctrl Pts',(-2.69284221889314,11.7002201050426,129.122062838334)) ;
#11645 = CARTESIAN_POINT('Ctrl Pts',(-2.69412086000923,11.7000734991237,129.125668147614)) ;
#11646 = CARTESIAN_POINT('Ctrl Pts',(-2.69537996760857,11.7000002555525,129.129279369597)) ;
#11647 = CARTESIAN_POINT('Ctrl Pts',(-2.69661747639193,11.7000000006677,129.13289365344)) ;
#11648 = CARTESIAN_POINT('Ctrl Pts',(-2.69661963763213,11.7000000002226,129.132899965585)) ;
#11649 = CARTESIAN_POINT('Ctrl Pts',(-2.69662179881363,11.7,129.132906277761)) ;
#11650 = CARTESIAN_POINT('Ctrl Pts',(-2.69662395993644,11.7,129.132912589967)) ;
#11651 = CARTESIAN_POINT('',(2.69661214327121,11.7,130.979127130373)) ;
#11652 = CARTESIAN_POINT('',(-5.63784594223766E-6,11.7,130.056019952763)) ;
#11653 = CARTESIAN_POINT('',(2.69638403966492,12.3,130.979049045863)) ;
#11654 = CARTESIAN_POINT('Ctrl Pts',(2.69661214327121,11.7,130.979127130373)) ;
#11655 = CARTESIAN_POINT('Ctrl Pts',(2.7020891025457,11.7,130.963130731944)) ;
#11656 = CARTESIAN_POINT('Ctrl Pts',(2.70718927973337,11.7014342946098,130.946939435389)) ;
#11657 = CARTESIAN_POINT('Ctrl Pts',(2.7119095593469,11.7043050991552,130.930837632166)) ;
#11658 = CARTESIAN_POINT('Ctrl Pts',(2.71648101121153,11.7070853888554,130.9152435097)) ;
#11659 = CARTESIAN_POINT('Ctrl Pts',(2.72069587103395,11.71121272146,130.899734122869)) ;
#11660 = CARTESIAN_POINT('Ctrl Pts',(2.72455232691621,11.7166364757703,130.884564828158)) ;
#11661 = CARTESIAN_POINT('Ctrl Pts',(2.72859710841077,11.7223250929191,130.868654758289)) ;
#11662 = CARTESIAN_POINT('Ctrl Pts',(2.7322472787346,11.7294400178026,130.853119824288)) ;
#11663 = CARTESIAN_POINT('Ctrl Pts',(2.73550668072301,11.7378640130638,130.838237316637)) ;
#11664 = CARTESIAN_POINT('Ctrl Pts',(2.73876608271141,11.7462880083249,130.823354808985)) ;
#11665 = CARTESIAN_POINT('Ctrl Pts',(2.74163442922915,11.7560205212514,130.809125566473)) ;
#11666 = CARTESIAN_POINT('Ctrl Pts',(2.7441261790723,11.7668904353912,130.795795867812)) ;
#11667 = CARTESIAN_POINT('Ctrl Pts',(2.74674638783286,11.7783207337953,130.781778973899)) ;
#11668 = CARTESIAN_POINT('Ctrl Pts',(2.74895573258088,11.7910207154901,130.768740512001)) ;
#11669 = CARTESIAN_POINT('Ctrl Pts',(2.75079104972321,11.8047759870922,130.756908352675)) ;
#11670 = CARTESIAN_POINT('Ctrl Pts',(2.75178960579543,11.8122599306932,130.750470732566)) ;
#11671 = CARTESIAN_POINT('Ctrl Pts',(2.75267765917822,11.8200556433546,130.744389568471)) ;
#11672 = CARTESIAN_POINT('Ctrl Pts',(2.75346280589737,11.828124644252,130.73869670229)) ;
#11673 = CARTESIAN_POINT('Ctrl Pts',(2.75480500156664,11.8419184713109,130.728964839254)) ;
#11674 = CARTESIAN_POINT('Ctrl Pts',(2.75585627744475,11.8565598978607,130.720339061431)) ;
#11675 = CARTESIAN_POINT('Ctrl Pts',(2.75668210855654,11.871835167371,130.712992921434)) ;
#11676 = CARTESIAN_POINT('Ctrl Pts',(2.75750686491625,11.8870905573592,130.70565634184)) ;
#11677 = CARTESIAN_POINT('Ctrl Pts',(2.75810663489716,11.9029774700657,130.699596445547)) ;
#11678 = CARTESIAN_POINT('Ctrl Pts',(2.75856124093594,11.9192571844188,130.694943450429)) ;
#11679 = CARTESIAN_POINT('Ctrl Pts',(2.7587415994758,11.9257159316846,130.693097440184)) ;
#11680 = CARTESIAN_POINT('Ctrl Pts',(2.75889928098971,11.932236276286,130.691472373768)) ;
#11681 = CARTESIAN_POINT('Ctrl Pts',(2.75903996599774,11.9388025611289,130.69007434979)) ;
#11682 = CARTESIAN_POINT('Ctrl Pts',(2.75947141313785,11.9589397801284,130.685786945926)) ;
#11683 = CARTESIAN_POINT('Ctrl Pts',(2.75973882505761,11.9794562190332,130.683647098857)) ;
#11684 = CARTESIAN_POINT('Ctrl Pts',(2.75974727407528,11.9999849854668,130.683648905163)) ;
#11685 = CARTESIAN_POINT('Ctrl Pts',(2.75975416941714,12.0167387511568,130.683650379311)) ;
#11686 = CARTESIAN_POINT('Ctrl Pts',(2.75958781337012,12.0335208417918,130.685080532272)) ;
#11687 = CARTESIAN_POINT('Ctrl Pts',(2.75928684742077,12.0500768654106,130.687940087924)) ;
#11688 = CARTESIAN_POINT('Ctrl Pts',(2.75921183402169,12.054203324266,130.688652809711)) ;
#11689 = CARTESIAN_POINT('Ctrl Pts',(2.75912854044863,12.0583157490574,130.689454088763)) ;
#11690 = CARTESIAN_POINT('Ctrl Pts',(2.75903772786621,12.0624102439617,130.690343460518)) ;
#11691 = CARTESIAN_POINT('Ctrl Pts',(2.75865720954827,12.0795667906892,130.694070061338)) ;
#11692 = CARTESIAN_POINT('Ctrl Pts',(2.75814458404643,12.0963905502863,130.69934360946)) ;
#11693 = CARTESIAN_POINT('Ctrl Pts',(2.75741685280201,12.11261990984,130.70604220651)) ;
#11694 = CARTESIAN_POINT('Ctrl Pts',(2.75668771854481,12.1288805584159,130.712753717967)) ;
#11695 = CARTESIAN_POINT('Ctrl Pts',(2.75574274873753,12.1445438866639,130.720895485112)) ;
#11696 = CARTESIAN_POINT('Ctrl Pts',(2.75451370053682,12.159369543475,130.730300393157)) ;
#11697 = CARTESIAN_POINT('Ctrl Pts',(2.75416100014212,12.1636240674278,130.732999322929)) ;
#11698 = CARTESIAN_POINT('Ctrl Pts',(2.753784995479,12.1678097828153,130.735802011507)) ;
#11699 = CARTESIAN_POINT('Ctrl Pts',(2.75338428427923,12.1719214624448,130.738703894657)) ;
#11700 = CARTESIAN_POINT('Ctrl Pts',(2.75177907201284,12.1883924734382,130.750328572059)) ;
#11701 = CARTESIAN_POINT('Ctrl Pts',(2.7497776751587,12.2036674747774,130.763544211412)) ;
#11702 = CARTESIAN_POINT('Ctrl Pts',(2.74730616641282,12.2174775160371,130.778059876953)) ;
#11703 = CARTESIAN_POINT('Ctrl Pts',(2.74483523432164,12.2312843351252,130.792572155686)) ;
#11704 = CARTESIAN_POINT('Ctrl Pts',(2.74189444507797,12.2436268239637,130.808383750645)) ;
#11705 = CARTESIAN_POINT('Ctrl Pts',(2.73842112100024,12.2542750535698,130.825171217944)) ;
#11706 = CARTESIAN_POINT('Ctrl Pts',(2.73499271641421,12.2647855727144,130.841741577803)) ;
#11707 = CARTESIAN_POINT('Ctrl Pts',(2.73104549225507,12.273645282714,130.859262643965)) ;
#11708 = CARTESIAN_POINT('Ctrl Pts',(2.72652958071105,12.2806718149886,130.87739295159)) ;
#11709 = CARTESIAN_POINT('Ctrl Pts',(2.72376917651805,12.284966865714,130.888475315958)) ;
#11710 = CARTESIAN_POINT('Ctrl Pts',(2.72079648829852,12.2885777183418,130.899784731069)) ;
#11711 = CARTESIAN_POINT('Ctrl Pts',(2.71760202350623,12.2914703716165,130.911237667668)) ;
#11712 = CARTESIAN_POINT('Ctrl Pts',(2.71343032445383,12.2952479305221,130.926194227802)) ;
#11713 = CARTESIAN_POINT('Ctrl Pts',(2.70888518495084,12.2977936154712,130.941381586919)) ;
#11714 = CARTESIAN_POINT('Ctrl Pts',(2.70396510786262,12.2990595555217,130.956556330231)) ;
#11715 = CARTESIAN_POINT('Ctrl Pts',(2.70152986494422,12.2996861456112,130.964067226)) ;
#11716 = CARTESIAN_POINT('Ctrl Pts',(2.69900283215451,12.3,130.971574842711)) ;
#11717 = CARTESIAN_POINT('Ctrl Pts',(2.69638403966492,12.3,130.979049045863)) ;
#11718 = CARTESIAN_POINT('Ctrl Pts',(2.69638403966492,12.3,130.979049045863)) ;
#11719 = CARTESIAN_POINT('Ctrl Pts',(2.69076103324602,12.3,130.995871488196)) ;
#11720 = CARTESIAN_POINT('Ctrl Pts',(2.68468187264347,12.2984226929191,131.012512912544)) ;
#11721 = CARTESIAN_POINT('Ctrl Pts',(2.67834076653583,12.2953062802814,131.028744053711)) ;
#11722 = CARTESIAN_POINT('Ctrl Pts',(2.67198914216565,12.2921846983174,131.045002118163)) ;
#11723 = CARTESIAN_POINT('Ctrl Pts',(2.6653749116115,12.2875191057773,131.060847926535)) ;
#11724 = CARTESIAN_POINT('Ctrl Pts',(2.65868863600529,12.2813983887177,131.076064554073)) ;
#11725 = CARTESIAN_POINT('Ctrl Pts',(2.65197416245748,12.2752518588391,131.091345354493)) ;
#11726 = CARTESIAN_POINT('Ctrl Pts',(2.64518723041611,12.2676382176756,131.105991084888)) ;
#11727 = CARTESIAN_POINT('Ctrl Pts',(2.6385131129551,12.2586944855711,131.119804584815)) ;
#11728 = CARTESIAN_POINT('Ctrl Pts',(2.63284426241128,12.2510978735995,131.131537471902)) ;
#11729 = CARTESIAN_POINT('Ctrl Pts',(2.62725672268844,12.2425426252491,131.142670181118)) ;
#11730 = CARTESIAN_POINT('Ctrl Pts',(2.62185820287899,12.2331361662797,131.153098904998)) ;
#11731 = CARTESIAN_POINT('Ctrl Pts',(2.6140905139445,12.2196016327727,131.168104329808)) ;
#11732 = CARTESIAN_POINT('Ctrl Pts',(2.60670260441095,12.2042764153757,131.181686029092)) ;
#11733 = CARTESIAN_POINT('Ctrl Pts',(2.59998827003384,12.1874596072397,131.193613809643)) ;
#11734 = CARTESIAN_POINT('Ctrl Pts',(2.59797355128117,12.1824135167698,131.197192887152)) ;
#11735 = CARTESIAN_POINT('Ctrl Pts',(2.59601940693364,12.1772333991662,131.200623262055)) ;
#11736 = CARTESIAN_POINT('Ctrl Pts',(2.59413359107694,12.171928064592,131.203899250854)) ;
#11737 = CARTESIAN_POINT('Ctrl Pts',(2.58906520381469,12.1576692544956,131.212703917461)) ;
#11738 = CARTESIAN_POINT('Ctrl Pts',(2.58449456346057,12.1425172907174,131.220381171779)) ;
#11739 = CARTESIAN_POINT('Ctrl Pts',(2.58057886543894,12.1267022432644,131.226829324827)) ;
#11740 = CARTESIAN_POINT('Ctrl Pts',(2.57666933487568,12.1109121054562,131.233267321649)) ;
#11741 = CARTESIAN_POINT('Ctrl Pts',(2.5734127985507,12.0944615861081,131.238479754618)) ;
#11742 = CARTESIAN_POINT('Ctrl Pts',(2.57095099057126,12.077604774293,131.242408414304)) ;
#11743 = CARTESIAN_POINT('Ctrl Pts',(2.57015954596351,12.072185491828,131.243671435852)) ;
#11744 = CARTESIAN_POINT('Ctrl Pts',(2.56945012023564,12.0667243718766,131.244802124643)) ;
#11745 = CARTESIAN_POINT('Ctrl Pts',(2.56882707329253,12.0612302416503,131.245799567725)) ;
#11746 = CARTESIAN_POINT('Ctrl Pts',(2.56693331953243,12.0445308101071,131.248831300097)) ;
#11747 = CARTESIAN_POINT('Ctrl Pts',(2.56583978787764,12.0275399677871,131.250625591239)) ;
#11748 = CARTESIAN_POINT('Ctrl Pts',(2.56551894829632,12.0105187380547,131.251146954998)) ;
#11749 = CARTESIAN_POINT('Ctrl Pts',(2.56545279235428,12.0070090230656,131.251254458289)) ;
#11750 = CARTESIAN_POINT('Ctrl Pts',(2.5654194316577,12.003498026412,131.251308007848)) ;
#11751 = CARTESIAN_POINT('Ctrl Pts',(2.56541853562656,11.9999880414362,131.251307553233)) ;
#11752 = CARTESIAN_POINT('Ctrl Pts',(2.56541319175008,11.9790546995262,131.251304841935)) ;
#11753 = CARTESIAN_POINT('Ctrl Pts',(2.56656382462477,11.9581302988702,131.249377613881)) ;
#11754 = CARTESIAN_POINT('Ctrl Pts',(2.56894086365112,11.9376174897209,131.245582103419)) ;
#11755 = CARTESIAN_POINT('Ctrl Pts',(2.57086617671789,11.9210028784109,131.242507881327)) ;
#11756 = CARTESIAN_POINT('Ctrl Pts',(2.57359436233372,11.9046908810092,131.238212953675)) ;
#11757 = CARTESIAN_POINT('Ctrl Pts',(2.57698748511119,11.888929144442,131.232734634183)) ;
#11758 = CARTESIAN_POINT('Ctrl Pts',(2.58038579213371,11.8731433260157,131.227247944539)) ;
#11759 = CARTESIAN_POINT('Ctrl Pts',(2.58445096343336,11.8579101506032,131.220574554715)) ;
#11760 = CARTESIAN_POINT('Ctrl Pts',(2.58902909197395,11.8434563529271,131.212796756995)) ;
#11761 = CARTESIAN_POINT('Ctrl Pts',(2.59068159970462,11.8382391528888,131.209989306145)) ;
#11762 = CARTESIAN_POINT('Ctrl Pts',(2.59240080428413,11.8331232393153,131.207038360296)) ;
#11763 = CARTESIAN_POINT('Ctrl Pts',(2.59417902645037,11.8281183129569,131.203949078297)) ;
#11764 = CARTESIAN_POINT('Ctrl Pts',(2.59926557248941,11.8138018856694,131.195112288715)) ;
#11765 = CARTESIAN_POINT('Ctrl Pts',(2.60484849396956,11.8003405866959,131.185104224137)) ;
#11766 = CARTESIAN_POINT('Ctrl Pts',(2.61078097101818,11.7879525676142,131.174051718868)) ;
#11767 = CARTESIAN_POINT('Ctrl Pts',(2.61670468421967,11.775582848933,131.163015541089)) ;
#11768 = CARTESIAN_POINT('Ctrl Pts',(2.62297677417685,11.7642837731286,131.150938435019)) ;
#11769 = CARTESIAN_POINT('Ctrl Pts',(2.62943841959953,11.7542382898846,131.137983630684)) ;
#11770 = CARTESIAN_POINT('Ctrl Pts',(2.6358935823194,11.7442028848604,131.12504182337)) ;
#11771 = CARTESIAN_POINT('Ctrl Pts',(2.64253774111245,11.7354189847105,131.111224601619)) ;
#11772 = CARTESIAN_POINT('Ctrl Pts',(2.64920236517453,11.728027594741,131.096724463487)) ;
#11773 = CARTESIAN_POINT('Ctrl Pts',(2.65586623767915,11.7206370382851,131.08222596051)) ;
#11774 = CARTESIAN_POINT('Ctrl Pts',(2.66255036723862,11.7146389842908,131.067045289927)) ;
#11775 = CARTESIAN_POINT('Ctrl Pts',(2.66907896661331,11.7101274655826,131.051396249006)) ;
#11776 = CARTESIAN_POINT('Ctrl Pts',(2.67157789020874,11.7084006111834,131.045406333657)) ;
#11777 = CARTESIAN_POINT('Ctrl Pts',(2.67405396720279,11.7068910362849,131.039347972696)) ;
#11778 = CARTESIAN_POINT('Ctrl Pts',(2.67649715581827,11.7056020732647,131.033233692652)) ;
#11779 = CARTESIAN_POINT('Ctrl Pts',(2.68216787636944,11.7026103480075,131.019042249027)) ;
#11780 = CARTESIAN_POINT('Ctrl Pts',(2.68765653077774,11.7008139298584,131.004563843729)) ;
#11781 = CARTESIAN_POINT('Ctrl Pts',(2.69282602724084,11.7002205914637,130.989988791192)) ;
#11782 = CARTESIAN_POINT('Ctrl Pts',(2.69410636351323,11.7000736385305,130.986378967959)) ;
#11783 = CARTESIAN_POINT('Ctrl Pts',(2.69536712310768,11.7000002331711,130.982763213871)) ;
#11784 = CARTESIAN_POINT('Ctrl Pts',(2.69660623340049,11.7000000005547,130.97914439066)) ;
#11785 = CARTESIAN_POINT('Ctrl Pts',(2.69660820340615,11.7000000001849,130.979138637256)) ;
#11786 = CARTESIAN_POINT('Ctrl Pts',(2.69661017336306,11.7,130.979132883827)) ;
#11787 = CARTESIAN_POINT('Ctrl Pts',(2.69661214327121,11.7,130.979127130373)) ;
#11788 = CARTESIAN_POINT('Ctrl Pts',(-2.69662395993644,11.7,129.132912589967)) ;
#11789 = CARTESIAN_POINT('Ctrl Pts',(-2.70210316791571,11.7,129.148916257214)) ;
#11790 = CARTESIAN_POINT('Ctrl Pts',(-2.70720519533175,11.7014355895077,129.16511505006)) ;
#11791 = CARTESIAN_POINT('Ctrl Pts',(-2.71192694782818,11.7043089893165,129.18122418407)) ;
#11792 = CARTESIAN_POINT('Ctrl Pts',(-2.71649777889907,11.7070905466165,129.196818421657)) ;
#11793 = CARTESIAN_POINT('Ctrl Pts',(-2.72071198318379,11.7112191551628,129.212327843349)) ;
#11794 = CARTESIAN_POINT('Ctrl Pts',(-2.72456777165,11.7166441842152,129.227497082678)) ;
#11795 = CARTESIAN_POINT('Ctrl Pts',(-2.7286145279346,11.7223379017531,129.243417617512)) ;
#11796 = CARTESIAN_POINT('Ctrl Pts',(-2.73226613681452,11.7294598193962,129.258962417819)) ;
#11797 = CARTESIAN_POINT('Ctrl Pts',(-2.73552647831201,11.7378924370324,129.273853640129)) ;
#11798 = CARTESIAN_POINT('Ctrl Pts',(-2.73878681980949,11.7463250546687,129.288744862438)) ;
#11799 = CARTESIAN_POINT('Ctrl Pts',(-2.74165560587231,11.7560678176211,129.302981665281)) ;
#11800 = CARTESIAN_POINT('Ctrl Pts',(-2.74414736354406,11.7669492094914,129.316317307692)) ;
#11801 = CARTESIAN_POINT('Ctrl Pts',(-2.74676548257675,11.7783824156497,129.3303292237)) ;
#11802 = CARTESIAN_POINT('Ctrl Pts',(-2.74897292156973,11.7910846326551,129.343362497685)) ;
#11803 = CARTESIAN_POINT('Ctrl Pts',(-2.75080654868513,11.804841448991,129.355189389573)) ;
#11804 = CARTESIAN_POINT('Ctrl Pts',(-2.75180139444525,11.8123052949875,129.361606143095)) ;
#11805 = CARTESIAN_POINT('Ctrl Pts',(-2.75268641904973,11.8200789640212,129.367668410619)) ;
#11806 = CARTESIAN_POINT('Ctrl Pts',(-2.7534691588745,11.8281243002186,129.373344634198)) ;
#11807 = CARTESIAN_POINT('Ctrl Pts',(-2.75481124983114,11.8419188876561,129.38307712524)) ;
#11808 = CARTESIAN_POINT('Ctrl Pts',(-2.75586245147619,11.8565611448242,129.391703367661)) ;
#11809 = CARTESIAN_POINT('Ctrl Pts',(-2.75668826024365,11.8718372879133,129.399049797183)) ;
#11810 = CARTESIAN_POINT('Ctrl Pts',(-2.75751299426833,11.8870935499778,129.406386665748)) ;
#11811 = CARTESIAN_POINT('Ctrl Pts',(-2.75811279370541,11.9029813776506,129.412446676533)) ;
#11812 = CARTESIAN_POINT('Ctrl Pts',(-2.75856750267306,11.9192620246435,129.417099601109)) ;
#11813 = CARTESIAN_POINT('Ctrl Pts',(-2.75874784386331,11.9257190586269,129.418944987974)) ;
#11814 = CARTESIAN_POINT('Ctrl Pts',(-2.75890553423442,11.9322376529964,129.420569544473)) ;
#11815 = CARTESIAN_POINT('Ctrl Pts',(-2.75904625010287,11.9388021643198,129.421967177062)) ;
#11816 = CARTESIAN_POINT('Ctrl Pts',(-2.75947790845114,11.9589393822915,129.426254538405)) ;
#11817 = CARTESIAN_POINT('Ctrl Pts',(-2.75974565709021,11.9794557280933,129.428394318667)) ;
#11818 = CARTESIAN_POINT('Ctrl Pts',(-2.75975338546674,11.9999848592252,129.428392768201)) ;
#11819 = CARTESIAN_POINT('Ctrl Pts',(-2.75975968681783,12.0167233375462,129.428391504025)) ;
#11820 = CARTESIAN_POINT('Ctrl Pts',(-2.75959234533244,12.0334902652325,129.426964401046)) ;
#11821 = CARTESIAN_POINT('Ctrl Pts',(-2.75929232930461,12.0500316612174,129.424109886153)) ;
#11822 = CARTESIAN_POINT('Ctrl Pts',(-2.75922438665313,12.0537776820901,129.423463442988)) ;
#11823 = CARTESIAN_POINT('Ctrl Pts',(-2.75914970817866,12.0575121447524,129.422743994089)) ;
#11824 = CARTESIAN_POINT('Ctrl Pts',(-2.75906888965378,12.061232130531,129.421951871596)) ;
#11825 = CARTESIAN_POINT('Ctrl Pts',(-2.75869605947647,12.078393084155,129.418297670164)) ;
#11826 = CARTESIAN_POINT('Ctrl Pts',(-2.75819241407854,12.0952281482433,129.413096445186)) ;
#11827 = CARTESIAN_POINT('Ctrl Pts',(-2.75747522563908,12.1114755686859,129.406468571523)) ;
#11828 = CARTESIAN_POINT('Ctrl Pts',(-2.75675666310361,12.127754118347,129.399827999197)) ;
#11829 = CARTESIAN_POINT('Ctrl Pts',(-2.75582383790127,12.1434421409862,129.391755596649)) ;
#11830 = CARTESIAN_POINT('Ctrl Pts',(-2.75460882273409,12.1582989041564,129.382417059579)) ;
#11831 = CARTESIAN_POINT('Ctrl Pts',(-2.75423056993796,12.1629240416545,129.379509830226)) ;
#11832 = CARTESIAN_POINT('Ctrl Pts',(-2.75382507299212,12.1674688166651,129.376480197129)) ;
#11833 = CARTESIAN_POINT('Ctrl Pts',(-2.75339055690962,12.1719265521261,129.373333961513)) ;
#11834 = CARTESIAN_POINT('Ctrl Pts',(-2.75178527076731,12.1883953118562,129.361710436775)) ;
#11835 = CARTESIAN_POINT('Ctrl Pts',(-2.749784179485,12.2036683820203,129.348496221254)) ;
#11836 = CARTESIAN_POINT('Ctrl Pts',(-2.74731325680201,12.2174768642847,129.333982186267)) ;
#11837 = CARTESIAN_POINT('Ctrl Pts',(-2.74484292966562,12.2312820184018,129.319471649481)) ;
#11838 = CARTESIAN_POINT('Ctrl Pts',(-2.74190303311995,12.2436232361933,129.303662023544)) ;
#11839 = CARTESIAN_POINT('Ctrl Pts',(-2.73843079462914,12.254270639284,129.286876688016)) ;
#11840 = CARTESIAN_POINT('Ctrl Pts',(-2.73500340435313,12.2647805181169,129.270308155665)) ;
#11841 = CARTESIAN_POINT('Ctrl Pts',(-2.73105736529469,12.2736399653289,129.252789044357)) ;
#11842 = CARTESIAN_POINT('Ctrl Pts',(-2.72654271562355,12.280666652311,129.234660773318)) ;
#11843 = CARTESIAN_POINT('Ctrl Pts',(-2.72378204235909,12.2849634169113,129.223575476156)) ;
#11844 = CARTESIAN_POINT('Ctrl Pts',(-2.72080895358385,12.2885756232418,129.212262987302)) ;
#11845 = CARTESIAN_POINT('Ctrl Pts',(-2.71761392427958,12.2914692428885,129.200806919405)) ;
#11846 = CARTESIAN_POINT('Ctrl Pts',(-2.71344268022509,12.2952469840602,129.185850544814)) ;
#11847 = CARTESIAN_POINT('Ctrl Pts',(-2.70889793126579,12.2977928925214,129.170663409752)) ;
#11848 = CARTESIAN_POINT('Ctrl Pts',(-2.70397812212487,12.2990591076826,129.155488943472)) ;
#11849 = CARTESIAN_POINT('Ctrl Pts',(-2.70154237978428,12.299685996611,129.147976235365)) ;
#11850 = CARTESIAN_POINT('Ctrl Pts',(-2.69901476984933,12.3,129.140466820952)) ;
#11851 = CARTESIAN_POINT('Ctrl Pts',(-2.69639531535756,12.3,129.132990859662)) ;
#11852 = CARTESIAN_POINT('Origin',(-5.63784594070025E-6,-12.,130.056019952763)) ;
#11853 = CARTESIAN_POINT('',(-2.69639531535792,-12.3,129.132990859662)) ;
#11854 = CARTESIAN_POINT('',(-2.69662341896302,-11.7,129.132912775153)) ;
#11855 = CARTESIAN_POINT('Ctrl Pts',(-2.69639531535756,-12.3,129.132990859662)) ;
#11856 = CARTESIAN_POINT('Ctrl Pts',(-2.70226117920183,-12.3,129.149730166849)) ;
#11857 = CARTESIAN_POINT('Ctrl Pts',(-2.70765564961494,-12.2984226929367,
129.16660597449)) ;
#11858 = CARTESIAN_POINT('Ctrl Pts',(-2.71259169348251,-12.2953062803316,
129.183318096982)) ;
#11859 = CARTESIAN_POINT('Ctrl Pts',(-2.7175359249746,-12.2921846984012,129.200057940576)) ;
#11860 = CARTESIAN_POINT('Ctrl Pts',(-2.72201999879468,-12.2875191059108,
129.216632944885)) ;
#11861 = CARTESIAN_POINT('Ctrl Pts',(-2.72606156203862,-12.2813983889147,
129.23275491124)) ;
#11862 = CARTESIAN_POINT('Ctrl Pts',(-2.73012016971229,-12.275251859102,129.248944868544)) ;
#11863 = CARTESIAN_POINT('Ctrl Pts',(-2.73373233104272,-12.2676382180192,
129.264677387526)) ;
#11864 = CARTESIAN_POINT('Ctrl Pts',(-2.73692362652984,-12.2586944860079,
129.279683128273)) ;
#11865 = CARTESIAN_POINT('Ctrl Pts',(-2.73963424355121,-12.2510978744367,
129.292428678302)) ;
#11866 = CARTESIAN_POINT('Ctrl Pts',(-2.74204130819701,-12.2425426265771,
129.304650128334)) ;
#11867 = CARTESIAN_POINT('Ctrl Pts',(-2.74416631789832,-12.2331361681733,
129.316199440896)) ;
#11868 = CARTESIAN_POINT('Ctrl Pts',(-2.74722389952739,-12.2196016349464,
129.332817231345)) ;
#11869 = CARTESIAN_POINT('Ctrl Pts',(-2.7497090908537,-12.2042764178469,129.348077230942)) ;
#11870 = CARTESIAN_POINT('Ctrl Pts',(-2.75171298541311,-12.1874596100186,
129.361617491048)) ;
#11871 = CARTESIAN_POINT('Ctrl Pts',(-2.75231427877979,-12.1824135186719,
129.365680413693)) ;
#11872 = CARTESIAN_POINT('Ctrl Pts',(-2.75287230997023,-12.1772334001408,
129.369588707344)) ;
#11873 = CARTESIAN_POINT('Ctrl Pts',(-2.75338972338882,-12.1719280645935,
129.373333128882)) ;
#11874 = CARTESIAN_POINT('Ctrl Pts',(-2.75478034225058,-12.1576692544915,
129.383396770507)) ;
#11875 = CARTESIAN_POINT('Ctrl Pts',(-2.75587337962017,-12.1425172907069,
129.392264479144)) ;
#11876 = CARTESIAN_POINT('Ctrl Pts',(-2.75673073612266,-12.126702243247,129.399759564773)) ;
#11877 = CARTESIAN_POINT('Ctrl Pts',(-2.7575867422374,-12.1109121054322,129.407242845194)) ;
#11878 = CARTESIAN_POINT('Ctrl Pts',(-2.75820769589563,-12.094461586077,129.413357491779)) ;
#11879 = CARTESIAN_POINT('Ctrl Pts',(-2.75866992540113,-12.0776047742543,
129.417970647894)) ;
#11880 = CARTESIAN_POINT('Ctrl Pts',(-2.75881852718141,-12.0721854918048,
129.419453727627)) ;
#11881 = CARTESIAN_POINT('Ctrl Pts',(-2.75895084447806,-12.066724371869,129.420781972381)) ;
#11882 = CARTESIAN_POINT('Ctrl Pts',(-2.75906976307799,-12.0612302416584,
129.421951988857)) ;
#11883 = CARTESIAN_POINT('Ctrl Pts',(-2.75943121665534,-12.0445308101116,
129.425508258785)) ;
#11884 = CARTESIAN_POINT('Ctrl Pts',(-2.75966668090157,-12.0275399677879,
129.427596283874)) ;
#11885 = CARTESIAN_POINT('Ctrl Pts',(-2.75973265423389,-12.0105187380521,
129.428204893541)) ;
#11886 = CARTESIAN_POINT('Ctrl Pts',(-2.75974625769244,-12.0070090230641,
129.428330386616)) ;
#11887 = CARTESIAN_POINT('Ctrl Pts',(-2.75975271216325,-12.0034980264116,
129.428393146724)) ;
#11888 = CARTESIAN_POINT('Ctrl Pts',(-2.759751725504,-11.9999880414369,129.428393336592)) ;
#11889 = CARTESIAN_POINT('Ctrl Pts',(-2.75974584112683,-11.9790546995273,
129.428394468955)) ;
#11890 = CARTESIAN_POINT('Ctrl Pts',(-2.75947403180639,-11.9581302988716,
129.426166401703)) ;
#11891 = CARTESIAN_POINT('Ctrl Pts',(-2.75902641398435,-11.9376174897222,
129.421710411074)) ;
#11892 = CARTESIAN_POINT('Ctrl Pts',(-2.75866386022208,-11.9210028784051,
129.418101224648)) ;
#11893 = CARTESIAN_POINT('Ctrl Pts',(-2.75818766763213,-11.9046908809968,
129.413035393923)) ;
#11894 = CARTESIAN_POINT('Ctrl Pts',(-2.75751170425596,-11.8889291444235,
129.406626935435)) ;
#11895 = CARTESIAN_POINT('Ctrl Pts',(-2.75683470809671,-11.873143325991,129.400208685665)) ;
#11896 = CARTESIAN_POINT('Ctrl Pts',(-2.75595743654763,-11.8579101505729,
129.392444012836)) ;
#11897 = CARTESIAN_POINT('Ctrl Pts',(-2.75480870069275,-11.8434563528919,
129.383492264161)) ;
#11898 = CARTESIAN_POINT('Ctrl Pts',(-2.75439405639888,-11.8382391528647,
129.380261067456)) ;
#11899 = CARTESIAN_POINT('Ctrl Pts',(-2.75394417936731,-11.833123239302,129.376875604947)) ;
#11900 = CARTESIAN_POINT('Ctrl Pts',(-2.75345616280295,-11.8281183129539,
129.373344659306)) ;
#11901 = CARTESIAN_POINT('Ctrl Pts',(-2.75206020747337,-11.8138018857667,
129.363244505446)) ;
#11902 = CARTESIAN_POINT('Ctrl Pts',(-2.75033870662451,-11.8003405868789,
129.351914598047)) ;
#11903 = CARTESIAN_POINT('Ctrl Pts',(-2.74825336831493,-11.7879525678663,
129.339545138952)) ;
#11904 = CARTESIAN_POINT('Ctrl Pts',(-2.74617111060459,-11.7755828492521,
129.327193952837)) ;
#11905 = CARTESIAN_POINT('Ctrl Pts',(-2.74372623641133,-11.7642837734984,
129.313806712992)) ;
#11906 = CARTESIAN_POINT('Ctrl Pts',(-2.74089327437816,-11.7542382902871,
129.299609736567)) ;
#11907 = CARTESIAN_POINT('Ctrl Pts',(-2.7380631545389,-11.7442028852945,129.285427003382)) ;
#11908 = CARTESIAN_POINT('Ctrl Pts',(-2.73484590441089,-11.7354189851583,
129.270436681145)) ;
#11909 = CARTESIAN_POINT('Ctrl Pts',(-2.73122631627443,-11.7280275951829,
129.25489416535)) ;
#11910 = CARTESIAN_POINT('Ctrl Pts',(-2.72760713631055,-11.7206370387174,
129.239353402248)) ;
#11911 = CARTESIAN_POINT('Ctrl Pts',(-2.72358591267336,-11.7146389846951,
129.223261164881)) ;
#11912 = CARTESIAN_POINT('Ctrl Pts',(-2.71915475623112,-11.7101274659389,
129.206894126674)) ;
#11913 = CARTESIAN_POINT('Ctrl Pts',(-2.71745866047623,-11.7084006102274,
129.200629381932)) ;
#11914 = CARTESIAN_POINT('Ctrl Pts',(-2.71570256550788,-11.7068910343395,
129.194324551297)) ;
#11915 = CARTESIAN_POINT('Ctrl Pts',(-2.71388621274829,-11.7056020706594,
129.187995687355)) ;
#11916 = CARTESIAN_POINT('Ctrl Pts',(-2.70967040184253,-11.702610346111,129.173306198496)) ;
#11917 = CARTESIAN_POINT('Ctrl Pts',(-2.70513486121312,-11.7008139286664,
129.158501522976)) ;
#11918 = CARTESIAN_POINT('Ctrl Pts',(-2.70028788857756,-11.7002205909573,
129.143816064066)) ;
#11919 = CARTESIAN_POINT('Ctrl Pts',(-2.69908743359452,-11.7000736383617,
129.14017890049)) ;
#11920 = CARTESIAN_POINT('Ctrl Pts',(-2.69786787424697,-11.7000002331707,
129.136549047369)) ;
#11921 = CARTESIAN_POINT('Ctrl Pts',(-2.6966293264623,-11.7000000005548,129.132930036242)) ;
#11922 = CARTESIAN_POINT('Ctrl Pts',(-2.69662735734983,-11.7000000001849,
129.132924282535)) ;
#11923 = CARTESIAN_POINT('Ctrl Pts',(-2.6966253881834,-11.7,129.132918528839)) ;
#11924 = CARTESIAN_POINT('Ctrl Pts',(-2.69662341896302,-11.7,129.132912775153)) ;
#11925 = CARTESIAN_POINT('',(2.69661245380302,-11.7,130.979127236674)) ;
#11926 = CARTESIAN_POINT('',(-5.63784594017984E-6,-11.7,130.056019952763)) ;
#11927 = CARTESIAN_POINT('',(2.69638403966492,-12.3,130.979049045863)) ;
#11928 = CARTESIAN_POINT('Ctrl Pts',(2.69661245380302,-11.7,130.979127236674)) ;
#11929 = CARTESIAN_POINT('Ctrl Pts',(2.69113431078088,-11.7,130.995132749034)) ;
#11930 = CARTESIAN_POINT('Ctrl Pts',(2.68523850579487,-11.7014358277356,131.011061288262)) ;
#11931 = CARTESIAN_POINT('Ctrl Pts',(2.67909713495093,-11.7043096952124,131.026685859201)) ;
#11932 = CARTESIAN_POINT('Ctrl Pts',(2.67315243899305,-11.7070915282602,131.041810059655)) ;
#11933 = CARTESIAN_POINT('Ctrl Pts',(2.66697792645336,-11.7112204554927,131.056648651996)) ;
#11934 = CARTESIAN_POINT('Ctrl Pts',(2.66072866461214,-11.7166458361922,131.070998734394)) ;
#11935 = CARTESIAN_POINT('Ctrl Pts',(2.65416927601188,-11.7223404576078,131.086060956027)) ;
#11936 = CARTESIAN_POINT('Ctrl Pts',(2.64752788465194,-11.7294635845994,131.100583957441)) ;
#11937 = CARTESIAN_POINT('Ctrl Pts',(2.64097785752022,-11.7378976704316,131.114350489788)) ;
#11938 = CARTESIAN_POINT('Ctrl Pts',(2.63442783038849,-11.7463317562638,131.128117022136)) ;
#11939 = CARTESIAN_POINT('Ctrl Pts',(2.62796945565154,-11.7560762459643,131.141126243614)) ;
#11940 = CARTESIAN_POINT('Ctrl Pts',(2.62176544834925,-11.7669595581195,131.153192022274)) ;
#11941 = CARTESIAN_POINT('Ctrl Pts',(2.6152474940389,-11.7783936083899,131.165868376475)) ;
#11942 = CARTESIAN_POINT('Ctrl Pts',(2.60900474534324,-11.7910966245474,131.177519621961)) ;
#11943 = CARTESIAN_POINT('Ctrl Pts',(2.60320587339938,-11.8048541799202,131.187988390373)) ;
#11944 = CARTESIAN_POINT('Ctrl Pts',(2.6000608605201,-11.8123155774565,131.193666117318)) ;
#11945 = CARTESIAN_POINT('Ctrl Pts',(2.59704619393286,-11.8200865437393,131.19899666061)) ;
#11946 = CARTESIAN_POINT('Ctrl Pts',(2.59418713529822,-11.8281289649774,131.203959724246)) ;
#11947 = CARTESIAN_POINT('Ctrl Pts',(2.5892779034638,-11.8419384440448,131.212481700571)) ;
#11948 = CARTESIAN_POINT('Ctrl Pts',(2.584817673955,-11.8565971445557,131.219948801914)) ;
#11949 = CARTESIAN_POINT('Ctrl Pts',(2.58096540364702,-11.8718908385621,131.2262640739)) ;
#11950 = CARTESIAN_POINT('Ctrl Pts',(2.57711829862176,-11.8871640261537,131.232570878109)) ;
#11951 = CARTESIAN_POINT('Ctrl Pts',(2.57387765122074,-11.903069835983,131.237728566734)) ;
#11952 = CARTESIAN_POINT('Ctrl Pts',(2.57138717998916,-11.9193690965159,131.24168322434)) ;
#11953 = CARTESIAN_POINT('Ctrl Pts',(2.57046502112798,-11.9254043027614,131.243147534591)) ;
#11954 = CARTESIAN_POINT('Ctrl Pts',(2.56964556070338,-11.9314932494922,131.244447352992)) ;
#11955 = CARTESIAN_POINT('Ctrl Pts',(2.56893554017386,-11.9376231925806,131.245581562453)) ;
#11956 = CARTESIAN_POINT('Ctrl Pts',(2.5665594885193,-11.9581367704451,131.249377143222)) ;
#11957 = CARTESIAN_POINT('Ctrl Pts',(2.56541360463764,-11.979054438517,131.251304739745)) ;
#11958 = CARTESIAN_POINT('Ctrl Pts',(2.56541995514723,-11.9999847393984,131.251308039005)) ;
#11959 = CARTESIAN_POINT('Ctrl Pts',(2.56542503678568,-12.0167330365428,131.251310679052)) ;
#11960 = CARTESIAN_POINT('Ctrl Pts',(2.56616861398396,-12.0335095446092,131.250079103225)) ;
#11961 = CARTESIAN_POINT('Ctrl Pts',(2.56768297526068,-12.0500600292145,131.247636932901)) ;
#11962 = CARTESIAN_POINT('Ctrl Pts',(2.56802487089586,-12.0537966134323,131.247085566865)) ;
#11963 = CARTESIAN_POINT('Ctrl Pts',(2.56840598653394,-12.0575216852744,131.246472693794)) ;
#11964 = CARTESIAN_POINT('Ctrl Pts',(2.5688265749632,-12.061232350046,131.245798932508)) ;
#11965 = CARTESIAN_POINT('Ctrl Pts',(2.57077173436107,-12.078393626845,131.242682886019)) ;
#11966 = CARTESIAN_POINT('Ctrl Pts',(2.57356133844419,-12.0952290052352,131.238264044836)) ;
#11967 = CARTESIAN_POINT('Ctrl Pts',(2.57705639028525,-12.1114767204747,131.232586883274)) ;
#11968 = CARTESIAN_POINT('Ctrl Pts',(2.58055813602547,-12.1277555541559,131.226898848526)) ;
#11969 = CARTESIAN_POINT('Ctrl Pts',(2.58476793490904,-12.1434438420947,131.219947959217)) ;
#11970 = CARTESIAN_POINT('Ctrl Pts',(2.58953071272326,-12.1583008404025,131.211823573806)) ;
#11971 = CARTESIAN_POINT('Ctrl Pts',(2.5910131951914,-12.1629252928501,131.209294743068)) ;
#11972 = CARTESIAN_POINT('Ctrl Pts',(2.59254914837815,-12.1674694062319,131.206652524045)) ;
#11973 = CARTESIAN_POINT('Ctrl Pts',(2.5941336213501,-12.1719265063663,131.203900413003)) ;
#11974 = CARTESIAN_POINT('Ctrl Pts',(2.59998807347437,-12.188394997664,131.193731667545)) ;
#11975 = CARTESIAN_POINT('Ctrl Pts',(2.60650465511311,-12.2036678470003,131.182063449917)) ;
#11976 = CARTESIAN_POINT('Ctrl Pts',(2.61344658327035,-12.2174761624351,131.169080221189)) ;
#11977 = CARTESIAN_POINT('Ctrl Pts',(2.62038683170025,-12.2312811366937,131.156100133992)) ;
#11978 = CARTESIAN_POINT('Ctrl Pts',(2.62775218527328,-12.2436222312856,131.141805775879)) ;
#11979 = CARTESIAN_POINT('Ctrl Pts',(2.63529483228866,-12.2542695739186,131.126414193534)) ;
#11980 = CARTESIAN_POINT('Ctrl Pts',(2.6427400745756,-12.2647794182018,131.111221376012)) ;
#11981 = CARTESIAN_POINT('Ctrl Pts',(2.65035803048437,-12.2736388840425,131.094959578602)) ;
#11982 = CARTESIAN_POINT('Ctrl Pts',(2.65789995579973,-12.2806656473848,131.077867956574)) ;
#11983 = CARTESIAN_POINT('Ctrl Pts',(2.66251197593969,-12.2849626369064,131.06741612873)) ;
#11984 = CARTESIAN_POINT('Ctrl Pts',(2.66709536320241,-12.2885750329263,131.056654571847)) ;
#11985 = CARTESIAN_POINT('Ctrl Pts',(2.6715913359282,-12.2914688040928,131.045643523228)) ;
#11986 = CARTESIAN_POINT('Ctrl Pts',(2.67746084722523,-12.2952466345178,131.03126855296)) ;
#11987 = CARTESIAN_POINT('Ctrl Pts',(2.68317659539627,-12.2977926378117,131.016482324032)) ;
#11988 = CARTESIAN_POINT('Ctrl Pts',(2.68858815040895,-12.299058953697,131.001476237306)) ;
#11989 = CARTESIAN_POINT('Ctrl Pts',(2.6912675760568,-12.2996859452462,130.99404626689)) ;
#11990 = CARTESIAN_POINT('Ctrl Pts',(2.69387236298024,-12.3,130.986562585859)) ;
#11991 = CARTESIAN_POINT('Ctrl Pts',(2.69638403966493,-12.3,130.979049045863)) ;
#11992 = CARTESIAN_POINT('Ctrl Pts',(2.69638403966492,-12.3,130.979049045863)) ;
#11993 = CARTESIAN_POINT('Ctrl Pts',(2.70225022747721,-12.3,130.962308165737)) ;
#11994 = CARTESIAN_POINT('Ctrl Pts',(2.70764519706473,-12.2984224104787,130.945430926132)) ;
#11995 = CARTESIAN_POINT('Ctrl Pts',(2.71258182346257,-12.2953054737208,130.928717527059)) ;
#11996 = CARTESIAN_POINT('Ctrl Pts',(2.71752666370191,-12.2921833508252,130.911976319276)) ;
#11997 = CARTESIAN_POINT('Ctrl Pts',(2.72201142529684,-12.2875169592251,130.895400108087)) ;
#11998 = CARTESIAN_POINT('Ctrl Pts',(2.72605366680566,-12.2813952242403,130.879277100824)) ;
#11999 = CARTESIAN_POINT('Ctrl Pts',(2.73011297470477,-12.2752476432197,130.863086022039)) ;
#12000 = CARTESIAN_POINT('Ctrl Pts',(2.73372582255887,-12.267632716394,130.847352552993)) ;
#12001 = CARTESIAN_POINT('Ctrl Pts',(2.736917703741,-12.2586875021641,130.832346039818)) ;
#12002 = CARTESIAN_POINT('Ctrl Pts',(2.7396281801801,-12.2510914197822,130.819602833517)) ;
#12003 = CARTESIAN_POINT('Ctrl Pts',(2.74203517470168,-12.242537011286,130.807383607764)) ;
#12004 = CARTESIAN_POINT('Ctrl Pts',(2.74416011607381,-12.2331316461142,130.795836299742)) ;
#12005 = CARTESIAN_POINT('Ctrl Pts',(2.7472186064759,-12.2195942283374,130.779215920836)) ;
#12006 = CARTESIAN_POINT('Ctrl Pts',(2.74970433309686,-12.2042654698107,130.763953772354)) ;
#12007 = CARTESIAN_POINT('Ctrl Pts',(2.75170825078127,-12.1874445705517,130.750411931767)) ;
#12008 = CARTESIAN_POINT('Ctrl Pts',(2.75230902884218,-12.1824016352464,130.746352064042)) ;
#12009 = CARTESIAN_POINT('Ctrl Pts',(2.75286657377173,-12.1772248561933,130.742446608027)) ;
#12010 = CARTESIAN_POINT('Ctrl Pts',(2.75338351917669,-12.1719230237542,130.738704786761)) ;
#12011 = CARTESIAN_POINT('Ctrl Pts',(2.75477436360932,-12.1576584146486,130.72863739623)) ;
#12012 = CARTESIAN_POINT('Ctrl Pts',(2.75586710296249,-12.1425000310335,130.719766833699)) ;
#12013 = CARTESIAN_POINT('Ctrl Pts',(2.75672435039289,-12.1266781224806,130.712270137096)) ;
#12014 = CARTESIAN_POINT('Ctrl Pts',(2.75758023008551,-12.1108814577735,130.704785401468)) ;
#12015 = CARTESIAN_POINT('Ctrl Pts',(2.75820125540657,-12.0944239978118,130.698670482248)) ;
#12016 = CARTESIAN_POINT('Ctrl Pts',(2.75866445797828,-12.0775600039634,130.694058577431)) ;
#12017 = CARTESIAN_POINT('Ctrl Pts',(2.75880226333131,-12.072542871573,130.692686509981)) ;
#12018 = CARTESIAN_POINT('Ctrl Pts',(2.75892620482364,-12.0674898913635,130.691447167072)) ;
#12019 = CARTESIAN_POINT('Ctrl Pts',(2.7590385826833,-12.0624080592774,130.690343262022)) ;
#12020 = CARTESIAN_POINT('Ctrl Pts',(2.7594077366967,-12.0457145689792,130.686717005206)) ;
#12021 = CARTESIAN_POINT('Ctrl Pts',(2.75964985448609,-12.0287234593521,130.684558819819)) ;
#12022 = CARTESIAN_POINT('Ctrl Pts',(2.75972259697515,-12.0116958892487,130.683881526958)) ;
#12023 = CARTESIAN_POINT('Ctrl Pts',(2.75973926506155,-12.0077942216904,130.68372633326)) ;
#12024 = CARTESIAN_POINT('Ctrl Pts',(2.75974711015346,-12.0038906537072,130.683648688519)) ;
#12025 = CARTESIAN_POINT('Ctrl Pts',(2.75974574765666,-11.99998833549,130.683648382481)) ;
#12026 = CARTESIAN_POINT('Ctrl Pts',(2.75973857892329,-11.9794564129564,130.683646772273)) ;
#12027 = CARTESIAN_POINT('Ctrl Pts',(2.7594754211691,-11.9589331107215,130.685789331442)) ;
#12028 = CARTESIAN_POINT('Ctrl Pts',(2.75904489406721,-11.9387965376136,130.690077363479)) ;
#12029 = CARTESIAN_POINT('Ctrl Pts',(2.75868965035837,-11.9221811122835,130.69361557605)) ;
#12030 = CARTESIAN_POINT('Ctrl Pts',(2.7582220316112,-11.9058614188827,130.69860992392)) ;
#12031 = CARTESIAN_POINT('Ctrl Pts',(2.75755623473998,-11.8900851853341,130.704948007217)) ;
#12032 = CARTESIAN_POINT('Ctrl Pts',(2.75688942885809,-11.8742850430101,130.711295695837)) ;
#12033 = CARTESIAN_POINT('Ctrl Pts',(2.75602394875841,-11.8590307121269,130.718990888978)) ;
#12034 = CARTESIAN_POINT('Ctrl Pts',(2.75488898277129,-11.84454928171,130.727875740134)) ;
#12035 = CARTESIAN_POINT('Ctrl Pts',(2.75445028470273,-11.8389517786781,130.731309999033)) ;
#12036 = CARTESIAN_POINT('Ctrl Pts',(2.75397147789854,-11.8334694651347,130.734921549577)) ;
#12037 = CARTESIAN_POINT('Ctrl Pts',(2.75344902648665,-11.8281142579715,130.738699659381)) ;
#12038 = CARTESIAN_POINT('Ctrl Pts',(2.75205230124255,-11.8137976098355,130.748800084451)) ;
#12039 = CARTESIAN_POINT('Ctrl Pts',(2.75033014856981,-11.8003361745224,130.76013034769)) ;
#12040 = CARTESIAN_POINT('Ctrl Pts',(2.74824424245493,-11.7879481058189,130.77250021509)) ;
#12041 = CARTESIAN_POINT('Ctrl Pts',(2.74616141622784,-11.7755783283804,130.7848518181)) ;
#12042 = CARTESIAN_POINT('Ctrl Pts',(2.74371605674675,-11.7642792817948,130.7982395287)) ;
#12043 = CARTESIAN_POINT('Ctrl Pts',(2.74088265796537,-11.7542339159119,130.812436999292)) ;
#12044 = CARTESIAN_POINT('Ctrl Pts',(2.73805210114096,-11.7441986257365,130.82662022953)) ;
#12045 = CARTESIAN_POINT('Ctrl Pts',(2.73483446227555,-11.7354149289329,130.841611072598)) ;
#12046 = CARTESIAN_POINT('Ctrl Pts',(2.73121449845122,-11.7280238296724,130.857154104223)) ;
#12047 = CARTESIAN_POINT('Ctrl Pts',(2.72759494388778,-11.7206335660247,130.872695378606)) ;
#12048 = CARTESIAN_POINT('Ctrl Pts',(2.72357335891403,-11.7146358913333,130.888788121982)) ;
#12049 = CARTESIAN_POINT('Ctrl Pts',(2.71914181881838,-11.7101248366017,130.905155633563)) ;
#12050 = CARTESIAN_POINT('Ctrl Pts',(2.71744585098747,-11.7083984382067,130.911419544645)) ;
#12051 = CARTESIAN_POINT('Ctrl Pts',(2.71568990011048,-11.7068892616191,130.917723523857)) ;
#12052 = CARTESIAN_POINT('Ctrl Pts',(2.71387370572788,-11.7056006375845,130.924051524917)) ;
#12053 = CARTESIAN_POINT('Ctrl Pts',(2.70965766191582,-11.7026092752947,130.938741103285)) ;
#12054 = CARTESIAN_POINT('Ctrl Pts',(2.70512187378689,-11.7008132376122,130.953545840774)) ;
#12055 = CARTESIAN_POINT('Ctrl Pts',(2.70027461522219,-11.7002202946038,130.968231324017)) ;
#12056 = CARTESIAN_POINT('Ctrl Pts',(2.69907513223611,-11.7000735673267,130.971865334264)) ;
#12057 = CARTESIAN_POINT('Ctrl Pts',(2.69785657570499,-11.700000260626,130.975492044451)) ;
#12058 = CARTESIAN_POINT('Ctrl Pts',(2.69661906089626,-11.7000000006939,130.979107932074)) ;
#12059 = CARTESIAN_POINT('Ctrl Pts',(2.69661685859934,-11.7000000002313,130.979114366953)) ;
#12060 = CARTESIAN_POINT('Ctrl Pts',(2.69661465623493,-11.7,130.97912080182)) ;
#12061 = CARTESIAN_POINT('Ctrl Pts',(2.69661245380302,-11.7,130.979127236674)) ;
#12062 = CARTESIAN_POINT('Ctrl Pts',(-2.69662341896302,-11.7,129.132912775153)) ;
#12063 = CARTESIAN_POINT('Ctrl Pts',(-2.69114835812364,-11.7,129.116915692321)) ;
#12064 = CARTESIAN_POINT('Ctrl Pts',(-2.68525611727231,-11.7014343001684,
129.100995500579)) ;
#12065 = CARTESIAN_POINT('Ctrl Pts',(-2.67911851841346,-11.704305115768,129.085378841304)) ;
#12066 = CARTESIAN_POINT('Ctrl Pts',(-2.67317444510001,-11.7070854112526,
129.070254593244)) ;
#12067 = CARTESIAN_POINT('Ctrl Pts',(-2.66700051540259,-11.7112127500097,
129.055415834658)) ;
#12068 = CARTESIAN_POINT('Ctrl Pts',(-2.66075178708574,-11.7166365107268,
129.041065462901)) ;
#12069 = CARTESIAN_POINT('Ctrl Pts',(-2.6541978921369,-11.7223251494649,129.026014267809)) ;
#12070 = CARTESIAN_POINT('Ctrl Pts',(-2.64756206239371,-11.7294401036985,
129.01150134337)) ;
#12071 = CARTESIAN_POINT('Ctrl Pts',(-2.6410172671884,-11.7378641349517,128.997743455817)) ;
#12072 = CARTESIAN_POINT('Ctrl Pts',(-2.6344724719831,-11.746288166205,128.983985568265)) ;
#12073 = CARTESIAN_POINT('Ctrl Pts',(-2.6280189984544,-11.7560207217575,128.970983556401)) ;
#12074 = CARTESIAN_POINT('Ctrl Pts',(-2.62181919984631,-11.7668906835074,
128.958923174318)) ;
#12075 = CARTESIAN_POINT('Ctrl Pts',(-2.61529979661753,-11.7783210005563,
128.946241069807)) ;
#12076 = CARTESIAN_POINT('Ctrl Pts',(-2.60905533324604,-11.7910209995357,
128.93458392869)) ;
#12077 = CARTESIAN_POINT('Ctrl Pts',(-2.60325456376142,-11.8047762867985,
128.924109243443)) ;
#12078 = CARTESIAN_POINT('Ctrl Pts',(-2.6000985336779,-11.8122601388157,128.918410271636)) ;
#12079 = CARTESIAN_POINT('Ctrl Pts',(-2.59707362546236,-11.8200557510676,
128.913060687359)) ;
#12080 = CARTESIAN_POINT('Ctrl Pts',(-2.59420535418644,-11.8281246442548,
128.908080996712)) ;
#12081 = CARTESIAN_POINT('Ctrl Pts',(-2.5893020251905,-11.8419184713108,128.899568182132)) ;
#12082 = CARTESIAN_POINT('Ctrl Pts',(-2.58484664609052,-11.8565598978575,
128.892107698161)) ;
#12083 = CARTESIAN_POINT('Ctrl Pts',(-2.58099731417302,-11.8718351673646,
128.885796564058)) ;
#12084 = CARTESIAN_POINT('Ctrl Pts',(-2.57715299184827,-11.8870905573495,
128.879493643383)) ;
#12085 = CARTESIAN_POINT('Ctrl Pts',(-2.57391326831685,-11.9029774700525,
128.874337456948)) ;
#12086 = CARTESIAN_POINT('Ctrl Pts',(-2.57142102170537,-11.9192571844022,
128.87038198769)) ;
#12087 = CARTESIAN_POINT('Ctrl Pts',(-2.57043225798016,-11.9257159316753,
128.868812710998)) ;
#12088 = CARTESIAN_POINT('Ctrl Pts',(-2.5695609749712,-11.9322362762841,128.867431924904)) ;
#12089 = CARTESIAN_POINT('Ctrl Pts',(-2.56881539891482,-11.9388025611347,
128.866240967448)) ;
#12090 = CARTESIAN_POINT('Ctrl Pts',(-2.56652889617113,-11.958939780132,128.862588586892)) ;
#12091 = CARTESIAN_POINT('Ctrl Pts',(-2.56542885216133,-11.979456219035,128.860733766742)) ;
#12092 = CARTESIAN_POINT('Ctrl Pts',(-2.56543663567068,-11.9999849854663,
128.860730016324)) ;
#12093 = CARTESIAN_POINT('Ctrl Pts',(-2.56544298788344,-12.0167387511885,
128.860726955564)) ;
#12094 = CARTESIAN_POINT('Ctrl Pts',(-2.5661879677875,-12.0335208418553,128.861959033802)) ;
#12095 = CARTESIAN_POINT('Ctrl Pts',(-2.5677025541412,-12.0500768655049,128.864403142488)) ;
#12096 = CARTESIAN_POINT('Ctrl Pts',(-2.5680800528906,-12.0542033243281,128.865012317376)) ;
#12097 = CARTESIAN_POINT('Ctrl Pts',(-2.56850527884464,-12.0583157490876,
128.865696546005)) ;
#12098 = CARTESIAN_POINT('Ctrl Pts',(-2.56897854879208,-12.0624102439602,
128.866454994808)) ;
#12099 = CARTESIAN_POINT('Ctrl Pts',(-2.57096162074754,-12.0795667906575,
128.869633008879)) ;
#12100 = CARTESIAN_POINT('Ctrl Pts',(-2.5737883114194,-12.0963905502262,128.87411440536)) ;
#12101 = CARTESIAN_POINT('Ctrl Pts',(-2.57731833127862,-12.1126199097541,
128.879853721937)) ;
#12102 = CARTESIAN_POINT('Ctrl Pts',(-2.58085515675867,-12.1288805583034,
128.885604103498)) ;
#12103 = CARTESIAN_POINT('Ctrl Pts',(-2.58509792556663,-12.1445438865275,
128.89261696687)) ;
#12104 = CARTESIAN_POINT('Ctrl Pts',(-2.58989029851729,-12.1593695433182,
128.900802076266)) ;
#12105 = CARTESIAN_POINT('Ctrl Pts',(-2.59126556748867,-12.1636240673243,
128.903150960023)) ;
#12106 = CARTESIAN_POINT('Ctrl Pts',(-2.59268600730169,-12.1678097827635,
128.905596117215)) ;
#12107 = CARTESIAN_POINT('Ctrl Pts',(-2.59414771277222,-12.1719214624428,
128.908134800458)) ;
#12108 = CARTESIAN_POINT('Ctrl Pts',(-2.60000316994638,-12.1883924716587,
128.918304531167)) ;
#12109 = CARTESIAN_POINT('Ctrl Pts',(-2.60652054073974,-12.2036674715057,
128.929974259017)) ;
#12110 = CARTESIAN_POINT('Ctrl Pts',(-2.61346311317316,-12.2174775116136,
128.942959386473)) ;
#12111 = CARTESIAN_POINT('Ctrl Pts',(-2.6204040657376,-12.2312843295072,128.955941484188)) ;
#12112 = CARTESIAN_POINT('Ctrl Pts',(-2.62776998615462,-12.2436268175001,
128.970238264367)) ;
#12113 = CARTESIAN_POINT('Ctrl Pts',(-2.63531313020966,-12.2542750466656,
128.985632546937)) ;
#12114 = CARTESIAN_POINT('Ctrl Pts',(-2.64275872104803,-12.2647855654813,
129.000827739874)) ;
#12115 = CARTESIAN_POINT('Ctrl Pts',(-2.65037695111223,-12.2736452755129,
129.017092143517)) ;
#12116 = CARTESIAN_POINT('Ctrl Pts',(-2.65791915501401,-12.2806718082327,
129.034186487092)) ;
#12117 = CARTESIAN_POINT('Ctrl Pts',(-2.66252943392023,-12.2849668758288,
129.044635646598)) ;
#12118 = CARTESIAN_POINT('Ctrl Pts',(-2.66711110523052,-12.2885777401896,
129.055394321234)) ;
#12119 = CARTESIAN_POINT('Ctrl Pts',(-2.67160547807788,-12.29147039969,129.066402321398)) ;
#12120 = CARTESIAN_POINT('Ctrl Pts',(-2.67747472379133,-12.2952479521871,
129.080777777099)) ;
#12121 = CARTESIAN_POINT('Ctrl Pts',(-2.68319031030512,-12.2977936307649,
129.095564468109)) ;
#12122 = CARTESIAN_POINT('Ctrl Pts',(-2.68860188327558,-12.2990595646063,
129.110570961495)) ;
#12123 = CARTESIAN_POINT('Ctrl Pts',(-2.69128038443391,-12.2996861486475,
129.11799854496)) ;
#12124 = CARTESIAN_POINT('Ctrl Pts',(-2.69388434284319,-12.3,129.125479787993)) ;
#12125 = CARTESIAN_POINT('Ctrl Pts',(-2.69639531535756,-12.3,129.132990859662)) ;
#12126 = CARTESIAN_POINT('Ctrl Pts',(-2.69634333633521,12.2999450599054,129.133008652785)) ;
#12127 = CARTESIAN_POINT('Ctrl Pts',(-2.66564577776436,12.301084845338,129.041173414331)) ;
#12128 = CARTESIAN_POINT('Ctrl Pts',(-2.60382900342522,12.229363413126,128.921431450579)) ;
#12129 = CARTESIAN_POINT('Ctrl Pts',(-2.56885602948563,12.0820021895678,128.86657194469)) ;
#12130 = CARTESIAN_POINT('Ctrl Pts',(-2.56422288068699,12.0003596690755,128.858780178468)) ;
#12131 = CARTESIAN_POINT('Ctrl Pts',(-2.56880156245784,11.9185468804347,128.866672863108)) ;
#12132 = CARTESIAN_POINT('Ctrl Pts',(-2.60359744333516,11.7703554429164,128.920157345138)) ;
#12133 = CARTESIAN_POINT('Ctrl Pts',(-2.70921355792956,11.6499856574159,129.128497465002)) ;
#12134 = CARTESIAN_POINT('Ctrl Pts',(-2.75358463094391,11.7702822363656,129.358212195121)) ;
#12135 = CARTESIAN_POINT('Ctrl Pts',(-2.75873449232472,11.918576320469,129.421574629153)) ;
#12136 = CARTESIAN_POINT('Ctrl Pts',(-2.75999748629359,11.9999479462354,129.430655077509)) ;
#12137 = CARTESIAN_POINT('Ctrl Pts',(-2.75887443013528,12.0816127336495,129.421791811517)) ;
#12138 = CARTESIAN_POINT('Ctrl Pts',(-2.75297468183829,12.2291419145039,129.357308950944)) ;
#12139 = CARTESIAN_POINT('Ctrl Pts',(-2.7283570304801,12.301091767988,129.224375795964)) ;
#12140 = CARTESIAN_POINT('Ctrl Pts',(-2.69634333633521,12.2999450599054,129.133008652785)) ;
#12141 = CARTESIAN_POINT('Ctrl Pts',(-2.83831085827015,12.4500000000046,129.084411247894)) ;
#12142 = CARTESIAN_POINT('Ctrl Pts',(-2.78948214878003,12.4517099925444,128.939496819705)) ;
#12143 = CARTESIAN_POINT('Ctrl Pts',(-2.70167351947378,12.3441081369419,128.747029727252)) ;
#12144 = CARTESIAN_POINT('Ctrl Pts',(-2.65407477200972,12.1230258146196,128.657777998572)) ;
#12145 = CARTESIAN_POINT('Ctrl Pts',(-2.64768441549552,12.0005396024158,128.645155374403)) ;
#12146 = CARTESIAN_POINT('Ctrl Pts',(-2.65403071331193,11.8777979413041,128.657923013224)) ;
#12147 = CARTESIAN_POINT('Ctrl Pts',(-2.70121137800042,11.6554700696645,128.745050570368)) ;
#12148 = CARTESIAN_POINT('Ctrl Pts',(-2.85184170514048,11.4748823176714,129.079612830176)) ;
#12149 = CARTESIAN_POINT('Ctrl Pts',(-2.93806835347429,11.6553602398041,129.43686799927)) ;
#12150 = CARTESIAN_POINT('Ctrl Pts',(-2.95399843334428,11.8778421094138,129.534266097453)) ;
#12151 = CARTESIAN_POINT('Ctrl Pts',(-2.95686297599919,11.9999219050466,129.548308897304)) ;
#12152 = CARTESIAN_POINT('Ctrl Pts',(-2.9541885151246,12.1224415237254,129.534619673828)) ;
#12153 = CARTESIAN_POINT('Ctrl Pts',(-2.93724684308448,12.3437758281832,129.435392991623)) ;
#12154 = CARTESIAN_POINT('Ctrl Pts',(-2.88852216719596,12.4517203783323,129.228824659478)) ;
#12155 = CARTESIAN_POINT('Ctrl Pts',(-2.83831085827015,12.4500000000046,129.084411247894)) ;
#12156 = CARTESIAN_POINT('',(-2.83831085827015,12.4500000000046,129.084411247894)) ;
#12157 = CARTESIAN_POINT('',(-2.69639531535756,12.3,129.132990859662)) ;
#12158 = CARTESIAN_POINT('Ctrl Pts',(-2.83831085827015,12.4500000000046,129.084411247894)) ;
#12159 = CARTESIAN_POINT('Ctrl Pts',(-2.78948214878003,12.4517099925444,128.939496819705)) ;
#12160 = CARTESIAN_POINT('Ctrl Pts',(-2.70167351947378,12.3441081369419,128.747029727252)) ;
#12161 = CARTESIAN_POINT('Ctrl Pts',(-2.65407477200972,12.1230258146196,128.657777998572)) ;
#12162 = CARTESIAN_POINT('Ctrl Pts',(-2.64768441549552,12.0005396024158,128.645155374403)) ;
#12163 = CARTESIAN_POINT('Ctrl Pts',(-2.65403071331193,11.8777979413041,128.657923013224)) ;
#12164 = CARTESIAN_POINT('Ctrl Pts',(-2.70121137800042,11.6554700696645,128.745050570368)) ;
#12165 = CARTESIAN_POINT('Ctrl Pts',(-2.85184170514048,11.4748823176714,129.079612830176)) ;
#12166 = CARTESIAN_POINT('Ctrl Pts',(-2.93806835347429,11.6553602398041,129.43686799927)) ;
#12167 = CARTESIAN_POINT('Ctrl Pts',(-2.95399843334428,11.8778421094138,129.534266097453)) ;
#12168 = CARTESIAN_POINT('Ctrl Pts',(-2.95686297599919,11.9999219050466,129.548308897304)) ;
#12169 = CARTESIAN_POINT('Ctrl Pts',(-2.9541885151246,12.1224415237254,129.534619673828)) ;
#12170 = CARTESIAN_POINT('Ctrl Pts',(-2.93724684308448,12.3437758281832,129.435392991623)) ;
#12171 = CARTESIAN_POINT('Ctrl Pts',(-2.88852216719596,12.4517203783323,129.228824659478)) ;
#12172 = CARTESIAN_POINT('Ctrl Pts',(-2.83831085827015,12.4500000000046,129.084411247894)) ;
#12173 = CARTESIAN_POINT('Ctrl Pts',(2.6963321026674,12.2999451040947,130.979031266417)) ;
#12174 = CARTESIAN_POINT('Ctrl Pts',(2.66563648729354,12.3010858736612,131.070864278016)) ;
#12175 = CARTESIAN_POINT('Ctrl Pts',(2.60362757434741,12.229152508386,131.190957001293)) ;
#12176 = CARTESIAN_POINT('Ctrl Pts',(2.56876939441479,12.0816041171335,131.24557404925)) ;
#12177 = CARTESIAN_POINT('Ctrl Pts',(2.56420616301492,11.9995576103439,131.253256926599)) ;
#12178 = CARTESIAN_POINT('Ctrl Pts',(2.56885622936123,11.9181473996368,131.245258218949)) ;
#12179 = CARTESIAN_POINT('Ctrl Pts',(2.60376633380277,11.7701460020227,131.191527526079)) ;
#12180 = CARTESIAN_POINT('Ctrl Pts',(2.70920033301593,11.6499866682161,130.983540223053)) ;
#12181 = CARTESIAN_POINT('Ctrl Pts',(2.75357841904063,11.7702819290618,130.753829963316)) ;
#12182 = CARTESIAN_POINT('Ctrl Pts',(2.758728952533,11.9185765432388,130.690466270959)) ;
#12183 = CARTESIAN_POINT('Ctrl Pts',(2.75999631694092,12.0003485349743,130.681342359721)) ;
#12184 = CARTESIAN_POINT('Ctrl Pts',(2.75885870872237,12.0820111503522,130.690378302155)) ;
#12185 = CARTESIAN_POINT('Ctrl Pts',(2.75289914346115,12.2293524229409,130.755122466735)) ;
#12186 = CARTESIAN_POINT('Ctrl Pts',(2.72834618207466,12.3010911231439,130.887661418871)) ;
#12187 = CARTESIAN_POINT('Ctrl Pts',(2.6963321026674,12.2999451040947,130.979031266417)) ;
#12188 = CARTESIAN_POINT('Ctrl Pts',(2.83829898912097,12.45,131.027630391263)) ;
#12189 = CARTESIAN_POINT('Ctrl Pts',(2.78947280025513,12.4517114687695,131.172541087384)) ;
#12190 = CARTESIAN_POINT('Ctrl Pts',(2.70139471334048,12.3437916712311,131.365573723284)) ;
#12191 = CARTESIAN_POINT('Ctrl Pts',(2.65396227551661,12.1224285785616,131.454437395721)) ;
#12192 = CARTESIAN_POINT('Ctrl Pts',(2.64766695170644,11.999336294049,131.466882783976)) ;
#12193 = CARTESIAN_POINT('Ctrl Pts',(2.65410944362262,11.8771986284416,131.453942044738)) ;
#12194 = CARTESIAN_POINT('Ctrl Pts',(2.70145638019102,11.6551559015813,131.366420835457)) ;
#12195 = CARTESIAN_POINT('Ctrl Pts',(2.85182798968834,11.4748839115138,131.032425729989)) ;
#12196 = CARTESIAN_POINT('Ctrl Pts',(2.93806166665439,11.6553598295364,130.675176301307)) ;
#12197 = CARTESIAN_POINT('Ctrl Pts',(2.95399268904346,11.8778424616273,130.577776192786)) ;
#12198 = CARTESIAN_POINT('Ctrl Pts',(2.95686908638074,12.0005228981401,130.563666450679)) ;
#12199 = CARTESIAN_POINT('Ctrl Pts',(2.95415063990756,12.123039240118,130.577621186444)) ;
#12200 = CARTESIAN_POINT('Ctrl Pts',(2.93710053667241,12.3440915979847,130.677255743497)) ;
#12201 = CARTESIAN_POINT('Ctrl Pts',(2.88851115280989,12.4517193443413,130.883212820616)) ;
#12202 = CARTESIAN_POINT('Ctrl Pts',(2.83829898912097,12.45,131.027630391263)) ;
#12203 = CARTESIAN_POINT('',(2.83829898912097,12.45,131.027630391263)) ;
#12204 = CARTESIAN_POINT('',(2.69638403966492,12.3,130.979049045863)) ;
#12205 = CARTESIAN_POINT('Ctrl Pts',(2.83829898912097,12.45,131.027630391263)) ;
#12206 = CARTESIAN_POINT('Ctrl Pts',(2.78947280025513,12.4517114687695,131.172541087384)) ;
#12207 = CARTESIAN_POINT('Ctrl Pts',(2.70139471334048,12.3437916712311,131.365573723284)) ;
#12208 = CARTESIAN_POINT('Ctrl Pts',(2.65396227551661,12.1224285785616,131.454437395721)) ;
#12209 = CARTESIAN_POINT('Ctrl Pts',(2.64766695170644,11.999336294049,131.466882783976)) ;
#12210 = CARTESIAN_POINT('Ctrl Pts',(2.65410944362262,11.8771986284416,131.453942044738)) ;
#12211 = CARTESIAN_POINT('Ctrl Pts',(2.70145638019102,11.6551559015813,131.366420835457)) ;
#12212 = CARTESIAN_POINT('Ctrl Pts',(2.85182798968834,11.4748839115138,131.032425729989)) ;
#12213 = CARTESIAN_POINT('Ctrl Pts',(2.93806166665439,11.6553598295364,130.675176301307)) ;
#12214 = CARTESIAN_POINT('Ctrl Pts',(2.95399268904346,11.8778424616273,130.577776192786)) ;
#12215 = CARTESIAN_POINT('Ctrl Pts',(2.95686908638074,12.0005228981401,130.563666450679)) ;
#12216 = CARTESIAN_POINT('Ctrl Pts',(2.95415063990756,12.123039240118,130.577621186444)) ;
#12217 = CARTESIAN_POINT('Ctrl Pts',(2.93710053667241,12.3440915979847,130.677255743497)) ;
#12218 = CARTESIAN_POINT('Ctrl Pts',(2.88851115280989,12.4517193443413,130.883212820616)) ;
#12219 = CARTESIAN_POINT('Ctrl Pts',(2.83829898912097,12.45,131.027630391263)) ;
#12220 = CARTESIAN_POINT('Ctrl Pts',(-2.69634337775187,-12.2999451036814,
129.133008638608)) ;
#12221 = CARTESIAN_POINT('Ctrl Pts',(-2.72836499658603,-12.3010858731961,
129.224387732003)) ;
#12222 = CARTESIAN_POINT('Ctrl Pts',(-2.75296065854718,-12.2291525080769,
129.357287772783)) ;
#12223 = CARTESIAN_POINT('Ctrl Pts',(-2.75888597978306,-12.0816041170245,
129.421809127302)) ;
#12224 = CARTESIAN_POINT('Ctrl Pts',(-2.75998831777564,-11.9995576103479,
129.430676738931)) ;
#12225 = CARTESIAN_POINT('Ctrl Pts',(-2.75876104868106,-11.9181473997497,
129.421506338094)) ;
#12226 = CARTESIAN_POINT('Ctrl Pts',(-2.75341994188481,-11.7701460023394,
129.357653575336)) ;
#12227 = CARTESIAN_POINT('Ctrl Pts',(-2.70927528047414,-11.6499866686978,
129.128685684283)) ;
#12228 = CARTESIAN_POINT('Ctrl Pts',(-2.60357079350359,-11.7702819293804,
128.91996870082)) ;
#12229 = CARTESIAN_POINT('Ctrl Pts',(-2.56880981077416,-11.9185765433525,
128.866741268284)) ;
#12230 = CARTESIAN_POINT('Ctrl Pts',(-2.5642199185338,-12.000348534976,128.858754726001)) ;
#12231 = CARTESIAN_POINT('Ctrl Pts',(-2.5688584365676,-12.082011150236,128.866592235696)) ;
#12232 = CARTESIAN_POINT('Ctrl Pts',(-2.60382610039754,-12.2293524226308,
128.921406337355)) ;
#12233 = CARTESIAN_POINT('Ctrl Pts',(-2.66564747078675,-12.3010911227233,
129.041187553936)) ;
#12234 = CARTESIAN_POINT('Ctrl Pts',(-2.69634337775187,-12.2999451036814,
129.133008638608)) ;
#12235 = CARTESIAN_POINT('Ctrl Pts',(-2.83831085827053,-12.4500000000046,
129.084411247895)) ;
#12236 = CARTESIAN_POINT('Ctrl Pts',(-2.88853286687405,-12.4517114685942,
129.22884412645)) ;
#12237 = CARTESIAN_POINT('Ctrl Pts',(-2.93722782612733,-12.3437916712762,
129.435358408931)) ;
#12238 = CARTESIAN_POINT('Ctrl Pts',(-2.95420403662341,-12.122428578556,129.534647868183)) ;
#12239 = CARTESIAN_POINT('Ctrl Pts',(-2.95685624455285,-11.9993362940612,
129.548340369185)) ;
#12240 = CARTESIAN_POINT('Ctrl Pts',(-2.9540167665531,-11.877198628427,129.534166244923)) ;
#12241 = CARTESIAN_POINT('Ctrl Pts',(-2.93779569001346,-11.6551559016217,
129.435990019905)) ;
#12242 = CARTESIAN_POINT('Ctrl Pts',(-2.85194041548293,-11.4748839115136,
129.079909659282)) ;
#12243 = CARTESIAN_POINT('Ctrl Pts',(-2.70115138870184,-11.6553598294949,
128.744758841329)) ;
#12244 = CARTESIAN_POINT('Ctrl Pts',(-2.65405087213571,-11.8778424616459,
128.658028685406)) ;
#12245 = CARTESIAN_POINT('Ctrl Pts',(-2.64767700965671,-12.000522898136,128.645116196827)) ;
#12246 = CARTESIAN_POINT('Ctrl Pts',(-2.65408069536962,-12.1230392401235,
128.657809400166)) ;
#12247 = CARTESIAN_POINT('Ctrl Pts',(-2.70166622738757,-12.3440915979617,
128.746991058121)) ;
#12248 = CARTESIAN_POINT('Ctrl Pts',(-2.78948627088357,-12.4517193444251,
128.939518681633)) ;
#12249 = CARTESIAN_POINT('Ctrl Pts',(-2.83831085827053,-12.4500000000046,
129.084411247895)) ;
#12250 = CARTESIAN_POINT('',(-2.83831085827053,-12.4500000000046,129.084411247895)) ;
#12251 = CARTESIAN_POINT('',(-2.69639531535755,-12.3,129.132990859662)) ;
#12252 = CARTESIAN_POINT('Ctrl Pts',(-2.83831085827053,-12.4500000000046,
129.084411247895)) ;
#12253 = CARTESIAN_POINT('Ctrl Pts',(-2.88853286687405,-12.4517114685942,
129.22884412645)) ;
#12254 = CARTESIAN_POINT('Ctrl Pts',(-2.93722782612733,-12.3437916712762,
129.435358408931)) ;
#12255 = CARTESIAN_POINT('Ctrl Pts',(-2.95420403662341,-12.122428578556,129.534647868183)) ;
#12256 = CARTESIAN_POINT('Ctrl Pts',(-2.95685624455285,-11.9993362940612,
129.548340369185)) ;
#12257 = CARTESIAN_POINT('Ctrl Pts',(-2.9540167665531,-11.877198628427,129.534166244923)) ;
#12258 = CARTESIAN_POINT('Ctrl Pts',(-2.93779569001346,-11.6551559016217,
129.435990019905)) ;
#12259 = CARTESIAN_POINT('Ctrl Pts',(-2.85194041548293,-11.4748839115136,
129.079909659282)) ;
#12260 = CARTESIAN_POINT('Ctrl Pts',(-2.70115138870184,-11.6553598294949,
128.744758841329)) ;
#12261 = CARTESIAN_POINT('Ctrl Pts',(-2.65405087213571,-11.8778424616459,
128.658028685406)) ;
#12262 = CARTESIAN_POINT('Ctrl Pts',(-2.64767700965671,-12.000522898136,128.645116196827)) ;
#12263 = CARTESIAN_POINT('Ctrl Pts',(-2.65408069536962,-12.1230392401235,
128.657809400166)) ;
#12264 = CARTESIAN_POINT('Ctrl Pts',(-2.70166622738757,-12.3440915979617,
128.746991058121)) ;
#12265 = CARTESIAN_POINT('Ctrl Pts',(-2.78948627088357,-12.4517193444251,
128.939518681633)) ;
#12266 = CARTESIAN_POINT('Ctrl Pts',(-2.83831085827053,-12.4500000000046,
129.084411247895)) ;
#12267 = CARTESIAN_POINT('Ctrl Pts',(2.69633205354012,-12.2999450521686,130.979031249599)) ;
#12268 = CARTESIAN_POINT('Ctrl Pts',(2.72835348567343,-12.3010848681391,130.887649149123)) ;
#12269 = CARTESIAN_POINT('Ctrl Pts',(2.75288606391975,-12.2293633531313,130.755144199488)) ;
#12270 = CARTESIAN_POINT('Ctrl Pts',(2.75886920933641,-12.082002231396,130.690360713879)) ;
#12271 = CARTESIAN_POINT('Ctrl Pts',(2.75998307604284,-12.000359613974,130.681364400907)) ;
#12272 = CARTESIAN_POINT('Ctrl Pts',(2.75876427003582,-11.918547034261,130.690406873977)) ;
#12273 = CARTESIAN_POINT('Ctrl Pts',(2.75348410569851,-11.7703549557434,130.753996321671)) ;
#12274 = CARTESIAN_POINT('Ctrl Pts',(2.70926597240985,-11.64998584046,130.983353308347)) ;
#12275 = CARTESIAN_POINT('Ctrl Pts',(2.60373618782364,-11.7700747434147,131.191714976771)) ;
#12276 = CARTESIAN_POINT('Ctrl Pts',(2.56886561000273,-11.9181762331761,131.245190263093)) ;
#12277 = CARTESIAN_POINT('Ctrl Pts',(2.56420273427314,-11.9995468614726,131.253281856879)) ;
#12278 = CARTESIAN_POINT('Ctrl Pts',(2.5687721064189,-12.0816128339373,131.245553724604)) ;
#12279 = CARTESIAN_POINT('Ctrl Pts',(2.60362416609314,-12.2291417112777,131.190981884302)) ;
#12280 = CARTESIAN_POINT('Ctrl Pts',(2.66563834676689,-12.3010918886182,131.070850177172)) ;
#12281 = CARTESIAN_POINT('Ctrl Pts',(2.69633205354012,-12.2999450521686,130.979031249599)) ;
#12282 = CARTESIAN_POINT('Ctrl Pts',(2.83829898912097,-12.45,131.027630391263)) ;
#12283 = CARTESIAN_POINT('Ctrl Pts',(2.88852128598129,-12.4517100383197,130.883192931152)) ;
#12284 = CARTESIAN_POINT('Ctrl Pts',(2.93708261399409,-12.3441080558366,130.677290924386)) ;
#12285 = CARTESIAN_POINT('Ctrl Pts',(2.95416519277115,-12.1230258805381,130.577592616342)) ;
#12286 = CARTESIAN_POINT('Ctrl Pts',(2.95685094224693,-12.0005395197688,130.56370210597)) ;
#12287 = CARTESIAN_POINT('Ctrl Pts',(2.95404148282776,-11.8777981689198,130.577679899858)) ;
#12288 = CARTESIAN_POINT('Ctrl Pts',(2.93793040819287,-11.6554693299226,130.675445005759)) ;
#12289 = CARTESIAN_POINT('Ctrl Pts',(2.85193092472614,-11.4748825787485,131.032130289841)) ;
#12290 = CARTESIAN_POINT('Ctrl Pts',(2.70139276112938,-11.6550489344215,131.366711469615)) ;
#12291 = CARTESIAN_POINT('Ctrl Pts',(2.65413082319135,-11.8772418654012,131.453837068699)) ;
#12292 = CARTESIAN_POINT('Ctrl Pts',(2.64765915018694,-11.9993201676784,131.466921440071)) ;
#12293 = CARTESIAN_POINT('Ctrl Pts',(2.65396858084,-12.1224416773533,131.454406087865)) ;
#12294 = CARTESIAN_POINT('Ctrl Pts',(2.70138694980991,-12.3437755321235,131.365612282658)) ;
#12295 = CARTESIAN_POINT('Ctrl Pts',(2.78947717755393,-12.4517205710547,131.17251934375)) ;
#12296 = CARTESIAN_POINT('Ctrl Pts',(2.83829898912097,-12.45,131.027630391263)) ;
#12297 = CARTESIAN_POINT('',(2.83829898912098,-12.45,131.027630391263)) ;
#12298 = CARTESIAN_POINT('',(2.69638403966492,-12.3,130.979049045863)) ;
#12299 = CARTESIAN_POINT('Ctrl Pts',(2.83829898912097,-12.45,131.027630391263)) ;
#12300 = CARTESIAN_POINT('Ctrl Pts',(2.88852128598129,-12.4517100383197,130.883192931152)) ;
#12301 = CARTESIAN_POINT('Ctrl Pts',(2.93708261399409,-12.3441080558366,130.677290924386)) ;
#12302 = CARTESIAN_POINT('Ctrl Pts',(2.95416519277115,-12.1230258805381,130.577592616342)) ;
#12303 = CARTESIAN_POINT('Ctrl Pts',(2.95685094224693,-12.0005395197688,130.56370210597)) ;
#12304 = CARTESIAN_POINT('Ctrl Pts',(2.95404148282776,-11.8777981689198,130.577679899858)) ;
#12305 = CARTESIAN_POINT('Ctrl Pts',(2.93793040819287,-11.6554693299226,130.675445005759)) ;
#12306 = CARTESIAN_POINT('Ctrl Pts',(2.85193092472614,-11.4748825787485,131.032130289841)) ;
#12307 = CARTESIAN_POINT('Ctrl Pts',(2.70139276112938,-11.6550489344215,131.366711469615)) ;
#12308 = CARTESIAN_POINT('Ctrl Pts',(2.65413082319135,-11.8772418654012,131.453837068699)) ;
#12309 = CARTESIAN_POINT('Ctrl Pts',(2.64765915018694,-11.9993201676784,131.466921440071)) ;
#12310 = CARTESIAN_POINT('Ctrl Pts',(2.65396858084,-12.1224416773533,131.454406087865)) ;
#12311 = CARTESIAN_POINT('Ctrl Pts',(2.70138694980991,-12.3437755321235,131.365612282658)) ;
#12312 = CARTESIAN_POINT('Ctrl Pts',(2.78947717755393,-12.4517205710547,131.17251934375)) ;
#12313 = CARTESIAN_POINT('Ctrl Pts',(2.83829898912097,-12.45,131.027630391263)) ;
#12314 = CARTESIAN_POINT('Origin',(5.27355936696949E-15,100.00000000005,130.056003483261)) ;
#12315 = CARTESIAN_POINT('',(0.643026455659758,99.8500000000496,132.986279404965)) ;
#12316 = CARTESIAN_POINT('Origin',(-1.36002320516582E-14,99.8500000000496,
130.056003483261)) ;
#12317 = CARTESIAN_POINT('',(0.643026455659758,-99.8499999999504,132.986279404965)) ;
#12318 = CARTESIAN_POINT('',(0.643026455659782,100.00000000005,132.986279404965)) ;
#12319 = CARTESIAN_POINT('Origin',(-1.12410081243297E-14,-99.8499999999504,
130.056003483261)) ;
#12320 = CARTESIAN_POINT('Origin',(0.643026455659758,100.00000000005,132.986279404965)) ;
#12321 = CARTESIAN_POINT('',(0.610875132876776,100.00000000005,132.83976560888)) ;
#12322 = CARTESIAN_POINT('Ctrl Pts',(0.610875132876776,100.00000000005,132.83976560888)) ;
#12323 = CARTESIAN_POINT('Ctrl Pts',(0.246570545573965,100.00000000005,132.91992659085)) ;
#12324 = CARTESIAN_POINT('Ctrl Pts',(-0.513976097476131,100.00000000005,132.934697342956)) ;
#12325 = CARTESIAN_POINT('Ctrl Pts',(-1.57650948054571,100.00000000005,132.518992741361)) ;
#12326 = CARTESIAN_POINT('Ctrl Pts',(-2.39903957015677,100.00000000005,131.728143423236)) ;
#12327 = CARTESIAN_POINT('Ctrl Pts',(-2.85632478451787,100.00000000005,130.68282018298)) ;
#12328 = CARTESIAN_POINT('Ctrl Pts',(-2.87877507902931,100.00000000005,129.542025478823)) ;
#12329 = CARTESIAN_POINT('Ctrl Pts',(-2.46294820116718,100.00000000005,128.479497242434)) ;
#12330 = CARTESIAN_POINT('Ctrl Pts',(-1.67216208711123,100.000000000049,127.656961864287)) ;
#12331 = CARTESIAN_POINT('Ctrl Pts',(-0.626804505408765,100.00000000005,127.199679863034)) ;
#12332 = CARTESIAN_POINT('Ctrl Pts',(0.513970981949363,100.000000000049,127.177227729026)) ;
#12333 = CARTESIAN_POINT('Ctrl Pts',(1.57651021040797,100.00000000005,127.593055664409)) ;
#12334 = CARTESIAN_POINT('Ctrl Pts',(2.39903942226395,100.00000000005,128.383841184256)) ;
#12335 = CARTESIAN_POINT('Ctrl Pts',(2.85632483652517,100.00000000005,129.429199095725)) ;
#12336 = CARTESIAN_POINT('Ctrl Pts',(2.8787739006122,100.00000000005,130.569976264547)) ;
#12337 = CARTESIAN_POINT('Ctrl Pts',(2.462957930535,100.00000000005,131.632548023818)) ;
#12338 = CARTESIAN_POINT('Ctrl Pts',(1.67212837843037,100.000000000049,132.454981361557)) ;
#12339 = CARTESIAN_POINT('Ctrl Pts',(0.975293053555267,100.00000000005,132.760016407974)) ;
#12340 = CARTESIAN_POINT('Ctrl Pts',(0.610875132876776,100.00000000005,132.83976560888)) ;
#12341 = CARTESIAN_POINT('Origin',(0.643026455659758,-99.9999999999504,132.986279404965)) ;
#12342 = CARTESIAN_POINT('',(0.610875132876776,-99.9999999999504,132.83976560888)) ;
#12343 = CARTESIAN_POINT('Ctrl Pts',(0.610875132876776,-99.9999999999504,
132.83976560888)) ;
#12344 = CARTESIAN_POINT('Ctrl Pts',(0.246570545573981,-99.9999999999506,
132.919926590851)) ;
#12345 = CARTESIAN_POINT('Ctrl Pts',(-0.513976097476131,-99.9999999999504,
132.934697342956)) ;
#12346 = CARTESIAN_POINT('Ctrl Pts',(-1.57650948054572,-99.9999999999505,
132.518992741361)) ;
#12347 = CARTESIAN_POINT('Ctrl Pts',(-2.39903957015677,-99.9999999999504,
131.728143423236)) ;
#12348 = CARTESIAN_POINT('Ctrl Pts',(-2.85632478451788,-99.9999999999505,
130.68282018298)) ;
#12349 = CARTESIAN_POINT('Ctrl Pts',(-2.87877507896514,-99.9999999999504,
129.542025478827)) ;
#12350 = CARTESIAN_POINT('Ctrl Pts',(-2.46294820107204,-99.9999999999504,
128.479497242403)) ;
#12351 = CARTESIAN_POINT('Ctrl Pts',(-1.67216208741986,-99.9999999999505,
127.656961864367)) ;
#12352 = CARTESIAN_POINT('Ctrl Pts',(-0.626804504682387,-99.9999999999505,
127.199679862876)) ;
#12353 = CARTESIAN_POINT('Ctrl Pts',(0.513970981616631,-99.9999999999502,
127.177227729086)) ;
#12354 = CARTESIAN_POINT('Ctrl Pts',(1.5765102105793,-99.9999999999503,127.593055664377)) ;
#12355 = CARTESIAN_POINT('Ctrl Pts',(2.39903942217006,-99.9999999999505,128.383841184273)) ;
#12356 = CARTESIAN_POINT('Ctrl Pts',(2.85632483657695,-99.9999999999504,129.429199095716)) ;
#12357 = CARTESIAN_POINT('Ctrl Pts',(2.87877390058261,-99.9999999999505,130.569976264552)) ;
#12358 = CARTESIAN_POINT('Ctrl Pts',(2.46295793055283,-99.9999999999503,131.632548023814)) ;
#12359 = CARTESIAN_POINT('Ctrl Pts',(1.67212837841725,-99.9999999999505,132.45498136156)) ;
#12360 = CARTESIAN_POINT('Ctrl Pts',(0.975293053561667,-99.9999999999504,
132.760016407972)) ;
#12361 = CARTESIAN_POINT('Ctrl Pts',(0.610875132876776,-99.9999999999504,
132.83976560888)) ;
#12362 = CARTESIAN_POINT('Ctrl Pts',(0.643026455659758,99.8500000000496,132.986279404965)) ;
#12363 = CARTESIAN_POINT('Ctrl Pts',(0.259547942953796,99.8500000000496,133.070659386104)) ;
#12364 = CARTESIAN_POINT('Ctrl Pts',(-0.541027471492163,99.8500000000496,
133.086207545669)) ;
#12365 = CARTESIAN_POINT('Ctrl Pts',(-1.65948366334539,99.8500000000496,132.648623755083)) ;
#12366 = CARTESIAN_POINT('Ctrl Pts',(-2.52530481091486,99.8500000000496,131.816150788913)) ;
#12367 = CARTESIAN_POINT('Ctrl Pts',(-3.00665766787806,99.8500000000497,130.715810534794)) ;
#12368 = CARTESIAN_POINT('Ctrl Pts',(-3.03028955669294,99.8500000000495,129.514974005128)) ;
#12369 = CARTESIAN_POINT('Ctrl Pts',(-2.59257705385615,99.8500000000497,128.396523229773)) ;
#12370 = CARTESIAN_POINT('Ctrl Pts',(-1.76017061831144,99.8500000000494,127.530696516006)) ;
#12371 = CARTESIAN_POINT('Ctrl Pts',(-0.659794215338994,99.8500000000498,
127.049347040875)) ;
#12372 = CARTESIAN_POINT('Ctrl Pts',(0.541022085740472,99.8500000000495,127.025713215585)) ;
#12373 = CARTESIAN_POINT('Ctrl Pts',(1.6594844324448,99.8500000000496,127.463426831923)) ;
#12374 = CARTESIAN_POINT('Ctrl Pts',(2.52530465476544,99.8500000000496,128.295832642362)) ;
#12375 = CARTESIAN_POINT('Ctrl Pts',(3.00665772253955,99.8500000000496,129.396209390568)) ;
#12376 = CARTESIAN_POINT('Ctrl Pts',(3.03028831652775,99.8500000000497,130.597027463672)) ;
#12377 = CARTESIAN_POINT('Ctrl Pts',(2.59258729503993,99.8500000000496,131.715524052452)) ;
#12378 = CARTESIAN_POINT('Ctrl Pts',(1.76013513546983,99.8500000000496,132.581243354859)) ;
#12379 = CARTESIAN_POINT('Ctrl Pts',(1.02662426675004,99.8500000000496,132.902332877864)) ;
#12380 = CARTESIAN_POINT('Ctrl Pts',(0.643026455659758,99.8500000000496,132.986279404965)) ;
#12381 = CARTESIAN_POINT('Ctrl Pts',(0.610875132876776,100.00000000005,132.83976560888)) ;
#12382 = CARTESIAN_POINT('Ctrl Pts',(0.246570545573965,100.00000000005,132.91992659085)) ;
#12383 = CARTESIAN_POINT('Ctrl Pts',(-0.513976097476131,100.00000000005,132.934697342956)) ;
#12384 = CARTESIAN_POINT('Ctrl Pts',(-1.57650948054571,100.00000000005,132.518992741361)) ;
#12385 = CARTESIAN_POINT('Ctrl Pts',(-2.39903957015677,100.00000000005,131.728143423236)) ;
#12386 = CARTESIAN_POINT('Ctrl Pts',(-2.85632478451787,100.00000000005,130.68282018298)) ;
#12387 = CARTESIAN_POINT('Ctrl Pts',(-2.87877507902931,100.00000000005,129.542025478823)) ;
#12388 = CARTESIAN_POINT('Ctrl Pts',(-2.46294820116718,100.00000000005,128.479497242434)) ;
#12389 = CARTESIAN_POINT('Ctrl Pts',(-1.67216208711123,100.000000000049,127.656961864287)) ;
#12390 = CARTESIAN_POINT('Ctrl Pts',(-0.626804505408765,100.00000000005,127.199679863034)) ;
#12391 = CARTESIAN_POINT('Ctrl Pts',(0.513970981949363,100.000000000049,127.177227729026)) ;
#12392 = CARTESIAN_POINT('Ctrl Pts',(1.57651021040797,100.00000000005,127.593055664409)) ;
#12393 = CARTESIAN_POINT('Ctrl Pts',(2.39903942226395,100.00000000005,128.383841184256)) ;
#12394 = CARTESIAN_POINT('Ctrl Pts',(2.85632483652517,100.00000000005,129.429199095725)) ;
#12395 = CARTESIAN_POINT('Ctrl Pts',(2.8787739006122,100.00000000005,130.569976264547)) ;
#12396 = CARTESIAN_POINT('Ctrl Pts',(2.462957930535,100.00000000005,131.632548023818)) ;
#12397 = CARTESIAN_POINT('Ctrl Pts',(1.67212837843037,100.000000000049,132.454981361557)) ;
#12398 = CARTESIAN_POINT('Ctrl Pts',(0.975293053555267,100.00000000005,132.760016407974)) ;
#12399 = CARTESIAN_POINT('Ctrl Pts',(0.610875132876776,100.00000000005,132.83976560888)) ;
#12400 = CARTESIAN_POINT('',(0.643026455659758,99.8500000000496,132.986279404965)) ;
#12401 = CARTESIAN_POINT('Ctrl Pts',(0.643026455659758,-99.8499999999504,
132.986279404965)) ;
#12402 = CARTESIAN_POINT('Ctrl Pts',(0.610875132876776,-99.9999999999504,
132.83976560888)) ;
#12403 = CARTESIAN_POINT('Ctrl Pts',(0.259547942953806,-99.8499999999506,
133.070659386104)) ;
#12404 = CARTESIAN_POINT('Ctrl Pts',(0.246570545573981,-99.9999999999506,
132.919926590851)) ;
#12405 = CARTESIAN_POINT('Ctrl Pts',(-0.541027471492161,-99.8499999999503,
133.086207545669)) ;
#12406 = CARTESIAN_POINT('Ctrl Pts',(-0.513976097476131,-99.9999999999504,
132.934697342956)) ;
#12407 = CARTESIAN_POINT('Ctrl Pts',(-1.6594836633454,-99.8499999999505,132.648623755083)) ;
#12408 = CARTESIAN_POINT('Ctrl Pts',(-1.57650948054572,-99.9999999999505,
132.518992741361)) ;
#12409 = CARTESIAN_POINT('Ctrl Pts',(-2.52530481091486,-99.8499999999504,
131.816150788913)) ;
#12410 = CARTESIAN_POINT('Ctrl Pts',(-2.39903957015677,-99.9999999999504,
131.728143423236)) ;
#12411 = CARTESIAN_POINT('Ctrl Pts',(-3.00665766787808,-99.8499999999505,
130.715810534794)) ;
#12412 = CARTESIAN_POINT('Ctrl Pts',(-2.85632478451788,-99.9999999999505,
130.68282018298)) ;
#12413 = CARTESIAN_POINT('Ctrl Pts',(-3.03028955675574,-99.8499999999505,
129.514974005143)) ;
#12414 = CARTESIAN_POINT('Ctrl Pts',(-2.87877507896514,-99.9999999999504,
129.542025478827)) ;
#12415 = CARTESIAN_POINT('Ctrl Pts',(-2.59257705395858,-99.8499999999503,
128.396523229796)) ;
#12416 = CARTESIAN_POINT('Ctrl Pts',(-2.46294820107204,-99.9999999999504,
128.479497242403)) ;
#12417 = CARTESIAN_POINT('Ctrl Pts',(-1.76017061799586,-99.8499999999505,
127.53069651594)) ;
#12418 = CARTESIAN_POINT('Ctrl Pts',(-1.67216208741986,-99.9999999999505,
127.656961864367)) ;
#12419 = CARTESIAN_POINT('Ctrl Pts',(-0.659794216106477,-99.8499999999505,
127.049347041044)) ;
#12420 = CARTESIAN_POINT('Ctrl Pts',(-0.626804504682387,-99.9999999999505,
127.199679862876)) ;
#12421 = CARTESIAN_POINT('Ctrl Pts',(0.541022086074333,-99.8499999999503,
127.025713215508)) ;
#12422 = CARTESIAN_POINT('Ctrl Pts',(0.513970981616631,-99.9999999999502,
127.177227729086)) ;
#12423 = CARTESIAN_POINT('Ctrl Pts',(1.65948443226611,-99.8499999999503,127.463426831961)) ;
#12424 = CARTESIAN_POINT('Ctrl Pts',(1.5765102105793,-99.9999999999503,127.593055664377)) ;
#12425 = CARTESIAN_POINT('Ctrl Pts',(2.52530465486198,-99.8499999999505,128.295832642341)) ;
#12426 = CARTESIAN_POINT('Ctrl Pts',(2.39903942217006,-99.9999999999505,128.383841184273)) ;
#12427 = CARTESIAN_POINT('Ctrl Pts',(3.00665772248627,-99.8499999999503,129.39620939058)) ;
#12428 = CARTESIAN_POINT('Ctrl Pts',(2.85632483657695,-99.9999999999504,129.429199095716)) ;
#12429 = CARTESIAN_POINT('Ctrl Pts',(3.03028831655821,-99.8499999999504,130.597027463665)) ;
#12430 = CARTESIAN_POINT('Ctrl Pts',(2.87877390058261,-99.9999999999505,130.569976264552)) ;
#12431 = CARTESIAN_POINT('Ctrl Pts',(2.59258729502161,-99.8499999999503,131.715524052456)) ;
#12432 = CARTESIAN_POINT('Ctrl Pts',(2.46295793055283,-99.9999999999503,131.632548023814)) ;
#12433 = CARTESIAN_POINT('Ctrl Pts',(1.76013513548333,-99.8499999999505,132.581243354857)) ;
#12434 = CARTESIAN_POINT('Ctrl Pts',(1.67212837841725,-99.9999999999505,132.45498136156)) ;
#12435 = CARTESIAN_POINT('Ctrl Pts',(1.02662426674344,-99.8499999999505,132.902332877865)) ;
#12436 = CARTESIAN_POINT('Ctrl Pts',(0.975293053561667,-99.9999999999504,
132.760016407972)) ;
#12437 = CARTESIAN_POINT('Ctrl Pts',(0.643026455659758,-99.8499999999504,
132.986279404965)) ;
#12438 = CARTESIAN_POINT('Ctrl Pts',(0.610875132876776,-99.9999999999504,
132.83976560888)) ;
#12439 = CARTESIAN_POINT('',(0.643026455659758,-99.8499999999504,132.986279404965)) ;
#12440 = CARTESIAN_POINT('Origin',(-19.4092722359532,-13.9601742359176,123.411814366564)) ;
#12441 = CARTESIAN_POINT('',(-18.2266423654683,-13.7497401139871,123.816643453356)) ;
#12442 = CARTESIAN_POINT('',(-18.2266423654683,-13.8098218143905,123.816643453356)) ;
#12443 = CARTESIAN_POINT('',(-18.2266423654683,-13.9601742359176,123.816643453356)) ;
#12444 = CARTESIAN_POINT('',(-20.5919020986874,-13.9898268235108,123.006985257131)) ;
#12445 = CARTESIAN_POINT('Ctrl Pts',(-18.2266423654683,-13.8098218143905,
123.816643453356)) ;
#12446 = CARTESIAN_POINT('Ctrl Pts',(-18.237831871297,-13.8114016285963,123.849331430235)) ;
#12447 = CARTESIAN_POINT('Ctrl Pts',(-18.2503723181934,-13.8129755447532,
123.881541832065)) ;
#12448 = CARTESIAN_POINT('Ctrl Pts',(-18.2642254820877,-13.8145603623162,
123.913180431967)) ;
#12449 = CARTESIAN_POINT('Ctrl Pts',(-18.293387889375,-13.8178965745782,123.979783104353)) ;
#12450 = CARTESIAN_POINT('Ctrl Pts',(-18.3283004942603,-13.8212461938646,
124.043704483388)) ;
#12451 = CARTESIAN_POINT('Ctrl Pts',(-18.368570392836,-13.8245506968226,124.104230190913)) ;
#12452 = CARTESIAN_POINT('Ctrl Pts',(-18.4086263458682,-13.8278376436479,
124.16443433802)) ;
#12453 = CARTESIAN_POINT('Ctrl Pts',(-18.4538295093184,-13.8311300264904,
124.221047239389)) ;
#12454 = CARTESIAN_POINT('Ctrl Pts',(-18.5036720507278,-13.8344876377522,
124.27343394886)) ;
#12455 = CARTESIAN_POINT('Ctrl Pts',(-18.5538218980809,-13.8378659504845,
124.326143650433)) ;
#12456 = CARTESIAN_POINT('Ctrl Pts',(-18.6084761746544,-13.8412029173428,
124.374373283239)) ;
#12457 = CARTESIAN_POINT('Ctrl Pts',(-18.6670195804605,-13.8444858761846,
124.417578253115)) ;
#12458 = CARTESIAN_POINT('Ctrl Pts',(-18.7250431716585,-13.8477396852026,
124.460399600375)) ;
#12459 = CARTESIAN_POINT('Ctrl Pts',(-18.7866588014402,-13.8510396003789,
124.498116602261)) ;
#12460 = CARTESIAN_POINT('Ctrl Pts',(-18.8511838442244,-13.8543957488816,
124.530312174829)) ;
#12461 = CARTESIAN_POINT('Ctrl Pts',(-18.8538780263867,-13.8545358816896,
124.531656470525)) ;
#12462 = CARTESIAN_POINT('Ctrl Pts',(-18.8565786729133,-13.8546760972818,
124.532991824414)) ;
#12463 = CARTESIAN_POINT('Ctrl Pts',(-18.8592826188426,-13.8548162117366,
124.534316669968)) ;
#12464 = CARTESIAN_POINT('Ctrl Pts',(-18.9219079625751,-13.858061363866,124.565001051386)) ;
#12465 = CARTESIAN_POINT('Ctrl Pts',(-18.9869884803353,-13.8612363658325,
124.590389744184)) ;
#12466 = CARTESIAN_POINT('Ctrl Pts',(-19.053848666975,-13.8643940206219,124.610219175755)) ;
#12467 = CARTESIAN_POINT('Ctrl Pts',(-19.1231784430325,-13.8676683085116,
124.630781039537)) ;
#12468 = CARTESIAN_POINT('Ctrl Pts',(-19.1941569425128,-13.8709919984484,
124.645286729952)) ;
#12469 = CARTESIAN_POINT('Ctrl Pts',(-19.2659898090002,-13.8743315341806,
124.653575271973)) ;
#12470 = CARTESIAN_POINT('Ctrl Pts',(-19.3380668459781,-13.8776824214866,
124.66189198797)) ;
#12471 = CARTESIAN_POINT('Ctrl Pts',(-19.4107314337425,-13.8809853979147,
124.663917527542)) ;
#12472 = CARTESIAN_POINT('Ctrl Pts',(-19.4831611255667,-13.8843026555778,
124.659628628411)) ;
#12473 = CARTESIAN_POINT('Ctrl Pts',(-19.5555009961429,-13.8876157994552,
124.655345048013)) ;
#12474 = CARTESIAN_POINT('Ctrl Pts',(-19.6273312746973,-13.8909438819607,
124.64477956539)) ;
#12475 = CARTESIAN_POINT('Ctrl Pts',(-19.6978504764238,-13.8942620357105,
124.628047320896)) ;
#12476 = CARTESIAN_POINT('Ctrl Pts',(-19.7371131245775,-13.8961094687501,
124.618731386905)) ;
#12477 = CARTESIAN_POINT('Ctrl Pts',(-19.7759127401105,-13.8979557647332,
124.607516713119)) ;
#12478 = CARTESIAN_POINT('Ctrl Pts',(-19.8141025333163,-13.8998064971626,
124.594443822655)) ;
#12479 = CARTESIAN_POINT('Ctrl Pts',(-19.8442734021559,-13.901268620958,124.58411592008)) ;
#12480 = CARTESIAN_POINT('Ctrl Pts',(-19.8740391175611,-13.9027321500355,
124.572636509389)) ;
#12481 = CARTESIAN_POINT('Ctrl Pts',(-19.9033228985707,-13.9041954603202,
124.560036445625)) ;
#12482 = CARTESIAN_POINT('Ctrl Pts',(-19.9702090673073,-13.9075377615958,
124.531257033883)) ;
#12483 = CARTESIAN_POINT('Ctrl Pts',(-20.0344429672726,-13.9108526467104,
124.496693112604)) ;
#12484 = CARTESIAN_POINT('Ctrl Pts',(-20.0953021057173,-13.9142011387571,
124.456736860277)) ;
#12485 = CARTESIAN_POINT('Ctrl Pts',(-20.1561612240545,-13.9175496296976,
124.416780621151)) ;
#12486 = CARTESIAN_POINT('Ctrl Pts',(-20.2134131689817,-13.9209012130819,
124.371584177511)) ;
#12487 = CARTESIAN_POINT('Ctrl Pts',(-20.2664070546696,-13.9242062414883,
124.321660453889)) ;
#12488 = CARTESIAN_POINT('Ctrl Pts',(-20.3188879116673,-13.9274792742338,
124.272220037014)) ;
#12489 = CARTESIAN_POINT('Ctrl Pts',(-20.3669908018908,-13.930769637394,124.218333654268)) ;
#12490 = CARTESIAN_POINT('Ctrl Pts',(-20.4101800759874,-13.9341146887793,
124.16060238452)) ;
#12491 = CARTESIAN_POINT('Ctrl Pts',(-20.4537632768795,-13.937490250179,124.1023445513)) ;
#12492 = CARTESIAN_POINT('Ctrl Pts',(-20.4921765254999,-13.9408084513923,
124.040394209155)) ;
#12493 = CARTESIAN_POINT('Ctrl Pts',(-20.5249854989838,-13.944113296651,123.975448924388)) ;
#12494 = CARTESIAN_POINT('Ctrl Pts',(-20.5272755731685,-13.9443439756393,
123.970915728001)) ;
#12495 = CARTESIAN_POINT('Ctrl Pts',(-20.5295394125655,-13.9445749823401,
123.966365762471)) ;
#12496 = CARTESIAN_POINT('Ctrl Pts',(-20.5317741930428,-13.9448060533355,
123.961804690484)) ;
#12497 = CARTESIAN_POINT('Ctrl Pts',(-20.5613319019382,-13.9478622502575,
123.901478927213)) ;
#12498 = CARTESIAN_POINT('Ctrl Pts',(-20.5859770073022,-13.9509585031166,
123.838871618375)) ;
#12499 = CARTESIAN_POINT('Ctrl Pts',(-20.6054716276694,-13.9540439669129,
123.774591178576)) ;
#12500 = CARTESIAN_POINT('Ctrl Pts',(-20.6264743153418,-13.9573681164073,
123.705338124395)) ;
#12501 = CARTESIAN_POINT('Ctrl Pts',(-20.6414226330833,-13.9606555846865,
123.634394702244)) ;
#12502 = CARTESIAN_POINT('Ctrl Pts',(-20.650149436559,-13.9639885363328,123.562558431431)) ;
#12503 = CARTESIAN_POINT('Ctrl Pts',(-20.6589235477942,-13.9673395558174,
123.490332738187)) ;
#12504 = CARTESIAN_POINT('Ctrl Pts',(-20.6613751505953,-13.9706784023529,
123.41747960217)) ;
#12505 = CARTESIAN_POINT('Ctrl Pts',(-20.65747594891,-13.9739866550751,123.344825628431)) ;
#12506 = CARTESIAN_POINT('Ctrl Pts',(-20.6536031184412,-13.9772725333073,
123.272663030576)) ;
#12507 = CARTESIAN_POINT('Ctrl Pts',(-20.6434804026981,-13.9805825593519,
123.200973456345)) ;
#12508 = CARTESIAN_POINT('Ctrl Pts',(-20.6272177792161,-13.9839176336044,
123.13055176023)) ;
#12509 = CARTESIAN_POINT('Ctrl Pts',(-20.6175741403921,-13.9858953127641,
123.088792114042)) ;
#12510 = CARTESIAN_POINT('Ctrl Pts',(-20.6057862739718,-13.9878667772688,
123.047545187057)) ;
#12511 = CARTESIAN_POINT('Ctrl Pts',(-20.5919020986876,-13.9898268235108,
123.006985257131)) ;
#12512 = CARTESIAN_POINT('',(-20.5016202458523,-13.9999999999504,122.804133672988)) ;
#12513 = CARTESIAN_POINT('Ctrl Pts',(-20.5919020986876,-13.9898268235109,
123.006985257131)) ;
#12514 = CARTESIAN_POINT('Ctrl Pts',(-20.5829797836085,-13.9910863977926,
122.98092044111)) ;
#12515 = CARTESIAN_POINT('Ctrl Pts',(-20.5732018900406,-13.9923407865095,
122.95516708369)) ;
#12516 = CARTESIAN_POINT('Ctrl Pts',(-20.5589092931437,-13.9940330998902,
122.920973150037)) ;
#12517 = CARTESIAN_POINT('Ctrl Pts',(-20.5551412455448,-13.9944678789148,
122.912239873399)) ;
#12518 = CARTESIAN_POINT('Ctrl Pts',(-20.5468065244909,-13.9954058172095,
122.893512858021)) ;
#12519 = CARTESIAN_POINT('Ctrl Pts',(-20.5422069987443,-13.9959090495036,
122.883534578517)) ;
#12520 = CARTESIAN_POINT('Ctrl Pts',(-20.526250497057,-13.9976076684926,122.850085445758)) ;
#12521 = CARTESIAN_POINT('Ctrl Pts',(-20.5142956053927,-13.9988037114221,
122.826918507055)) ;
#12522 = CARTESIAN_POINT('Ctrl Pts',(-20.5016202458523,-13.9999999999504,
122.804133672988)) ;
#12523 = CARTESIAN_POINT('',(-19.4275508050227,-13.9999999999504,122.161948016114)) ;
#12524 = CARTESIAN_POINT('Origin',(-19.4092722359532,-13.9999999999504,123.411814366564)) ;
#12525 = CARTESIAN_POINT('',(-20.5919020529002,-13.9297284766184,123.006985123376)) ;
#12526 = CARTESIAN_POINT('Ctrl Pts',(-19.4275508050227,-13.9999999999504,
122.161948016114)) ;
#12527 = CARTESIAN_POINT('Ctrl Pts',(-19.4313400989441,-13.9998265546944,
122.162003432335)) ;
#12528 = CARTESIAN_POINT('Ctrl Pts',(-19.4351191276508,-13.999653443417,122.16207587392)) ;
#12529 = CARTESIAN_POINT('Ctrl Pts',(-19.4429233390417,-13.9992956353971,
122.162260951395)) ;
#12530 = CARTESIAN_POINT('Ctrl Pts',(-19.4469384386358,-13.9991113818313,
122.162375536062)) ;
#12531 = CARTESIAN_POINT('Ctrl Pts',(-19.4568925373842,-13.9986541355976,
122.16270763557)) ;
#12532 = CARTESIAN_POINT('Ctrl Pts',(-19.4628306599564,-13.9983809660134,
122.162948155404)) ;
#12533 = CARTESIAN_POINT('Ctrl Pts',(-19.4831706784865,-13.9974438136556,
122.163917350673)) ;
#12534 = CARTESIAN_POINT('Ctrl Pts',(-19.4975614785456,-13.9967782187756,
122.164852880824)) ;
#12535 = CARTESIAN_POINT('Ctrl Pts',(-19.5339902925882,-13.9950870857167,
122.167854864106)) ;
#12536 = CARTESIAN_POINT('Ctrl Pts',(-19.5559955461641,-13.9940591023316,
122.170258045284)) ;
#12537 = CARTESIAN_POINT('Ctrl Pts',(-19.5928424694167,-13.9923365170248,
122.175275398734)) ;
#12538 = CARTESIAN_POINT('Ctrl Pts',(-19.6077218672209,-13.991640719076,122.177575977864)) ;
#12539 = CARTESIAN_POINT('Ctrl Pts',(-19.6261327352259,-13.9907806249149,
122.180764124246)) ;
#12540 = CARTESIAN_POINT('Ctrl Pts',(-19.6297065625804,-13.9906137014449,
122.181399037088)) ;
#12541 = CARTESIAN_POINT('Ctrl Pts',(-19.6362191814793,-13.990309578876,122.182585330092)) ;
#12542 = CARTESIAN_POINT('Ctrl Pts',(-19.6391588541742,-13.9901723273278,
122.183131704924)) ;
#12543 = CARTESIAN_POINT('Ctrl Pts',(-19.6449603074068,-13.9899015045205,
122.184231526615)) ;
#12544 = CARTESIAN_POINT('Ctrl Pts',(-19.647822168119,-13.9897679284137,122.18478444603)) ;
#12545 = CARTESIAN_POINT('Ctrl Pts',(-19.654434616522,-13.9894593362366,122.186085997644)) ;
#12546 = CARTESIAN_POINT('Ctrl Pts',(-19.6581837571266,-13.9892844006816,
122.186841843616)) ;
#12547 = CARTESIAN_POINT('Ctrl Pts',(-19.6690890614828,-13.9887756119914,
122.189092541385)) ;
#12548 = CARTESIAN_POINT('Ctrl Pts',(-19.6762356664328,-13.988442258957,122.190632982731)) ;
#12549 = CARTESIAN_POINT('Ctrl Pts',(-19.7082799404323,-13.9869472701456,
122.197834825916)) ;
#12550 = CARTESIAN_POINT('Ctrl Pts',(-19.7330141597435,-13.9857932844965,
122.204195592942)) ;
#12551 = CARTESIAN_POINT('Ctrl Pts',(-19.77189986965,-13.9839594567732,122.215476254775)) ;
#12552 = CARTESIAN_POINT('Ctrl Pts',(-19.7861875528098,-13.9832812405568,
122.219900561472)) ;
#12553 = CARTESIAN_POINT('Ctrl Pts',(-19.8073400288787,-13.9822683001325,
122.226868991719)) ;
#12554 = CARTESIAN_POINT('Ctrl Pts',(-19.8142674640842,-13.9819351401419,
122.229218757883)) ;
#12555 = CARTESIAN_POINT('Ctrl Pts',(-19.8256238694404,-13.9813864381683,
122.233182306854)) ;
#12556 = CARTESIAN_POINT('Ctrl Pts',(-19.8300650540129,-13.9811712130438,
122.234760578939)) ;
#12557 = CARTESIAN_POINT('Ctrl Pts',(-19.8380556278999,-13.9807827776198,
122.23765120823)) ;
#12558 = CARTESIAN_POINT('Ctrl Pts',(-19.8416081886326,-13.9806096508407,
122.238954637732)) ;
#12559 = CARTESIAN_POINT('Ctrl Pts',(-19.8481787379539,-13.9802886327113,
122.241399272334)) ;
#12560 = CARTESIAN_POINT('Ctrl Pts',(-19.851198333927,-13.9801407832986,122.242536070278)) ;
#12561 = CARTESIAN_POINT('Ctrl Pts',(-19.8578651656588,-13.9798136344481,
122.245075469938)) ;
#12562 = CARTESIAN_POINT('Ctrl Pts',(-19.861510291863,-13.9796342864989,122.246483507899)) ;
#12563 = CARTESIAN_POINT('Ctrl Pts',(-19.871770979672,-13.9791280781222,122.250502395653)) ;
#12564 = CARTESIAN_POINT('Ctrl Pts',(-19.8783709302037,-13.9788008679235,
122.253152640202)) ;
#12565 = CARTESIAN_POINT('Ctrl Pts',(-19.9053759425105,-13.9774554241485,
122.26426520365)) ;
#12566 = CARTESIAN_POINT('Ctrl Pts',(-19.9255774279037,-13.976433158422,122.273211317236)) ;
#12567 = CARTESIAN_POINT('Ctrl Pts',(-19.9625548125104,-13.9745363265479,
122.290773079595)) ;
#12568 = CARTESIAN_POINT('Ctrl Pts',(-19.9793935891346,-13.9736625907819,
122.299242200312)) ;
#12569 = CARTESIAN_POINT('Ctrl Pts',(-20.0030028643973,-13.9724270345094,
122.311793356447)) ;
#12570 = CARTESIAN_POINT('Ctrl Pts',(-20.0099360213834,-13.9720628560408,
122.315563802345)) ;
#12571 = CARTESIAN_POINT('Ctrl Pts',(-20.0173571119298,-13.9716716660796,
122.319691139405)) ;
#12572 = CARTESIAN_POINT('Ctrl Pts',(-20.0178809821164,-13.9716440436766,
122.319982990487)) ;
#12573 = CARTESIAN_POINT('Ctrl Pts',(-20.0186824307534,-13.9716017737803,
122.320430238153)) ;
#12574 = CARTESIAN_POINT('Ctrl Pts',(-20.0189601601499,-13.9715871237066,
122.320585363851)) ;
#12575 = CARTESIAN_POINT('Ctrl Pts',(-20.0197876471307,-13.9715434679437,
122.321047971057)) ;
#12576 = CARTESIAN_POINT('Ctrl Pts',(-20.020337231717,-13.9715144652276,122.321355762212)) ;
#12577 = CARTESIAN_POINT('Ctrl Pts',(-20.0213193983153,-13.9714626194997,
122.321906793688)) ;
#12578 = CARTESIAN_POINT('Ctrl Pts',(-20.0217520684562,-13.9714397749691,
122.322149876391)) ;
#12579 = CARTESIAN_POINT('Ctrl Pts',(-20.0225225239134,-13.9713990865927,
122.322583337473)) ;
#12580 = CARTESIAN_POINT('Ctrl Pts',(-20.0228603655731,-13.9713812417699,
122.322773615441)) ;
#12581 = CARTESIAN_POINT('Ctrl Pts',(-20.0234603996002,-13.9713495423621,
122.3231119323)) ;
#12582 = CARTESIAN_POINT('Ctrl Pts',(-20.023722627053,-13.971335687167,122.323259908756)) ;
#12583 = CARTESIAN_POINT('Ctrl Pts',(-20.0241874961885,-13.9713111217335,
122.323522458574)) ;
#12584 = CARTESIAN_POINT('Ctrl Pts',(-20.0243901593995,-13.9713004111175,
122.323636993834)) ;
#12585 = CARTESIAN_POINT('Ctrl Pts',(-20.0287511708992,-13.9710699102416,
122.326103230215)) ;
#12586 = CARTESIAN_POINT('Ctrl Pts',(-20.0328960444638,-13.9708503582615,
122.328478699236)) ;
#12587 = CARTESIAN_POINT('Ctrl Pts',(-20.0401386450013,-13.9704658746123,
122.332684846911)) ;
#12588 = CARTESIAN_POINT('Ctrl Pts',(-20.0432422701575,-13.9703008392668,
122.334505245617)) ;
#12589 = CARTESIAN_POINT('Ctrl Pts',(-20.0494089887849,-13.9699723614362,
122.338158146935)) ;
#12590 = CARTESIAN_POINT('Ctrl Pts',(-20.0524721788521,-13.9698089183065,
122.339990419353)) ;
#12591 = CARTESIAN_POINT('Ctrl Pts',(-20.0597411972348,-13.9694203765605,
122.344380826212)) ;
#12592 = CARTESIAN_POINT('Ctrl Pts',(-20.0639398478046,-13.9691954007169,
122.346950736389)) ;
#12593 = CARTESIAN_POINT('Ctrl Pts',(-20.0823086507002,-13.9682085640206,
122.358343617163)) ;
#12594 = CARTESIAN_POINT('Ctrl Pts',(-20.0963164762467,-13.9674493441243,
122.367425142087)) ;
#12595 = CARTESIAN_POINT('Ctrl Pts',(-20.1213689212244,-13.9660749163178,
122.384389298333)) ;
#12596 = CARTESIAN_POINT('Ctrl Pts',(-20.132474838872,-13.9654594559669,122.392176223856)) ;
#12597 = CARTESIAN_POINT('Ctrl Pts',(-20.1571536534888,-13.9640732867552,
122.410085864093)) ;
#12598 = CARTESIAN_POINT('Ctrl Pts',(-20.1706519807994,-13.9633021838136,
122.420306676723)) ;
#12599 = CARTESIAN_POINT('Ctrl Pts',(-20.1902573263851,-13.9621613987188,
122.435788183106)) ;
#12600 = CARTESIAN_POINT('Ctrl Pts',(-20.1965276577979,-13.9617933117389,
122.440838711654)) ;
#12601 = CARTESIAN_POINT('Ctrl Pts',(-20.2068064265991,-13.9611844404265,
122.449282916893)) ;
#12602 = CARTESIAN_POINT('Ctrl Pts',(-20.2108430570657,-13.9609439064896,
122.452641913128)) ;
#12603 = CARTESIAN_POINT('Ctrl Pts',(-20.2197349388992,-13.9604108763614,
122.46013643701)) ;
#12604 = CARTESIAN_POINT('Ctrl Pts',(-20.2245799470123,-13.9601183077058,
122.464283886588)) ;
#12605 = CARTESIAN_POINT('Ctrl Pts',(-20.2352820252772,-13.9594672759103,
122.473587996888)) ;
#12606 = CARTESIAN_POINT('Ctrl Pts',(-20.2411229747021,-13.9591087169046,
122.478762791973)) ;
#12607 = CARTESIAN_POINT('Ctrl Pts',(-20.2569437608605,-13.9581286420425,
122.493045878624)) ;
#12608 = CARTESIAN_POINT('Ctrl Pts',(-20.2668249758572,-13.9575066710911,
122.502261814118)) ;
#12609 = CARTESIAN_POINT('Ctrl Pts',(-20.2945935725675,-13.9557310272155,
122.529015648875)) ;
#12610 = CARTESIAN_POINT('Ctrl Pts',(-20.3121059166192,-13.9545778178095,
122.546933565339)) ;
#12611 = CARTESIAN_POINT('Ctrl Pts',(-20.3370085670051,-13.9528889187766,
122.573994098076)) ;
#12612 = CARTESIAN_POINT('Ctrl Pts',(-20.3448272295371,-13.9523509602435,
122.582733937836)) ;
#12613 = CARTESIAN_POINT('Ctrl Pts',(-20.3600652353632,-13.9512864797164,
122.600257326914)) ;
#12614 = CARTESIAN_POINT('Ctrl Pts',(-20.3674886746231,-13.9507599910363,
122.609035808208)) ;
#12615 = CARTESIAN_POINT('Ctrl Pts',(-20.3879539588389,-13.949284985644,122.633925116559)) ;
#12616 = CARTESIAN_POINT('Ctrl Pts',(-20.4007177078815,-13.9483373362306,
122.650259722292)) ;
#12617 = CARTESIAN_POINT('Ctrl Pts',(-20.4189775564808,-13.9469350335655,
122.674865618212)) ;
#12618 = CARTESIAN_POINT('Ctrl Pts',(-20.4247907882943,-13.9464811282198,
122.682897113889)) ;
#12619 = CARTESIAN_POINT('Ctrl Pts',(-20.4346542250202,-13.9456972002265,
122.696871376891)) ;
#12620 = CARTESIAN_POINT('Ctrl Pts',(-20.4387498237064,-13.9453674144131,
122.702781505505)) ;
#12621 = CARTESIAN_POINT('Ctrl Pts',(-20.4465129998918,-13.9447336976661,
122.714193186951)) ;
#12622 = CARTESIAN_POINT('Ctrl Pts',(-20.4501883632713,-13.9444298562635,
122.71968914071)) ;
#12623 = CARTESIAN_POINT('Ctrl Pts',(-20.463156107996,-13.9433443836467,122.739417396655)) ;
#12624 = CARTESIAN_POINT('Ctrl Pts',(-20.4722016005217,-13.9425621315287,
122.753809756139)) ;
#12625 = CARTESIAN_POINT('Ctrl Pts',(-20.4874546139563,-13.9411997355344,
122.779214648094)) ;
#12626 = CARTESIAN_POINT('Ctrl Pts',(-20.4937938393718,-13.9406193020215,
122.79014521236)) ;
#12627 = CARTESIAN_POINT('Ctrl Pts',(-20.5037522393955,-13.9396841060832,
122.807932272416)) ;
#12628 = CARTESIAN_POINT('Ctrl Pts',(-20.5074752388329,-13.9393288726186,
122.814729593285)) ;
#12629 = CARTESIAN_POINT('Ctrl Pts',(-20.5145480006963,-13.9386429369001,
122.827932758823)) ;
#12630 = CARTESIAN_POINT('Ctrl Pts',(-20.5179058835757,-13.9383122056115,
122.834333904803)) ;
#12631 = CARTESIAN_POINT('Ctrl Pts',(-20.5293114355171,-13.9371708050483,
122.856542520223)) ;
#12632 = CARTESIAN_POINT('Ctrl Pts',(-20.5370780527677,-13.9363616963756,
122.872491944226)) ;
#12633 = CARTESIAN_POINT('Ctrl Pts',(-20.5573951475415,-13.9341494952713,
122.916574527132)) ;
#12634 = CARTESIAN_POINT('Ctrl Pts',(-20.5692492643665,-13.932747799697,122.945014618369)) ;
#12635 = CARTESIAN_POINT('Ctrl Pts',(-20.5822750711628,-13.9310479712546,
122.979836339052)) ;
#12636 = CARTESIAN_POINT('Ctrl Pts',(-20.5844636170084,-13.9307561760045,
122.985826238473)) ;
#12637 = CARTESIAN_POINT('Ctrl Pts',(-20.58840503499,-13.9302189335495,122.996875207426)) ;
#12638 = CARTESIAN_POINT('Ctrl Pts',(-20.5901681493033,-13.929974026106,123.001919861591)) ;
#12639 = CARTESIAN_POINT('Ctrl Pts',(-20.5919020529013,-13.9297284766178,
123.006985123375)) ;
#12640 = CARTESIAN_POINT('Ctrl Pts',(-20.5919020529002,-13.9297284766184,
123.006985123376)) ;
#12641 = CARTESIAN_POINT('Ctrl Pts',(-20.6024246541309,-13.9282383012773,
123.037724867468)) ;
#12642 = CARTESIAN_POINT('Ctrl Pts',(-20.6117446103661,-13.9267411197154,
123.068862757242)) ;
#12643 = CARTESIAN_POINT('Ctrl Pts',(-20.6198408276881,-13.9252413439706,
123.100328115213)) ;
#12644 = CARTESIAN_POINT('Ctrl Pts',(-20.6379709053181,-13.9218828557287,
123.170789339262)) ;
#12645 = CARTESIAN_POINT('Ctrl Pts',(-20.6499146685378,-13.9185651787582,
123.242698766736)) ;
#12646 = CARTESIAN_POINT('Ctrl Pts',(-20.6555359566546,-13.9152437317152,
123.31523932559)) ;
#12647 = CARTESIAN_POINT('Ctrl Pts',(-20.6611343658999,-13.9119358030968,
123.387484641415)) ;
#12648 = CARTESIAN_POINT('Ctrl Pts',(-20.6604401452033,-13.9086000938307,
123.460079826942)) ;
#12649 = CARTESIAN_POINT('Ctrl Pts',(-20.6534612032785,-13.9052867540257,
123.53220462224)) ;
#12650 = CARTESIAN_POINT('Ctrl Pts',(-20.6464800094602,-13.901972345106,123.604352690028)) ;
#12651 = CARTESIAN_POINT('Ctrl Pts',(-20.6332366280487,-13.8986781273188,
123.675755651677)) ;
#12652 = CARTESIAN_POINT('Ctrl Pts',(-20.6138811082396,-13.8953268861809,
123.745606914241)) ;
#12653 = CARTESIAN_POINT('Ctrl Pts',(-20.5944401554272,-13.8919608530561,
123.815766492118)) ;
#12654 = CARTESIAN_POINT('Ctrl Pts',(-20.5689075331187,-13.888617535704,123.884092649026)) ;
#12655 = CARTESIAN_POINT('Ctrl Pts',(-20.5375717903147,-13.8853232938337,
123.949810756611)) ;
#12656 = CARTESIAN_POINT('Ctrl Pts',(-20.5356609335309,-13.8851224106293,
123.953818253497)) ;
#12657 = CARTESIAN_POINT('Ctrl Pts',(-20.5337286362003,-13.8849215188531,
123.957815753525)) ;
#12658 = CARTESIAN_POINT('Ctrl Pts',(-20.5317752294988,-13.8847205822267,
123.961802575126)) ;
#12659 = CARTESIAN_POINT('Ctrl Pts',(-20.5020529870819,-13.8816632121898,
124.022464432178)) ;
#12660 = CARTESIAN_POINT('Ctrl Pts',(-20.4674642360604,-13.8785603363961,
124.080613672752)) ;
#12661 = CARTESIAN_POINT('Ctrl Pts',(-20.4283471324293,-13.8754303943831,
124.135683384722)) ;
#12662 = CARTESIAN_POINT('Ctrl Pts',(-20.3862144846183,-13.8720591646073,
124.194998430164)) ;
#12663 = CARTESIAN_POINT('Ctrl Pts',(-20.3389839905469,-13.8687568953655,
124.250521590318)) ;
#12664 = CARTESIAN_POINT('Ctrl Pts',(-20.2871913450968,-13.8654334148974,
124.301622232272)) ;
#12665 = CARTESIAN_POINT('Ctrl Pts',(-20.2355216253904,-13.862117822447,124.352601590899)) ;
#12666 = CARTESIAN_POINT('Ctrl Pts',(-20.1795096491898,-13.8587707311508,
124.398983559086)) ;
#12667 = CARTESIAN_POINT('Ctrl Pts',(-20.1197902982936,-13.8554599676142,
124.440242333494)) ;
#12668 = CARTESIAN_POINT('Ctrl Pts',(-20.060515588533,-13.8521738544067,124.481193915208)) ;
#12669 = CARTESIAN_POINT('Ctrl Pts',(-19.9978127986901,-13.8488823096299,
124.51694345188)) ;
#12670 = CARTESIAN_POINT('Ctrl Pts',(-19.9323811071369,-13.8455608652241,
124.547092794512)) ;
#12671 = CARTESIAN_POINT('Ctrl Pts',(-19.893785334744,-13.8436016661073,124.564876793954)) ;
#12672 = CARTESIAN_POINT('Ctrl Pts',(-19.8543076305284,-13.8416507393192,
124.580681111942)) ;
#12673 = CARTESIAN_POINT('Ctrl Pts',(-19.814101322745,-13.8397085566956,124.594444237049)) ;
#12674 = CARTESIAN_POINT('Ctrl Pts',(-19.785503854565,-13.8383271439561,124.604233510275)) ;
#12675 = CARTESIAN_POINT('Ctrl Pts',(-19.7565607840212,-13.8369502231916,
124.612982255014)) ;
#12676 = CARTESIAN_POINT('Ctrl Pts',(-19.7273292786425,-13.8355640133331,
124.620673215922)) ;
#12677 = CARTESIAN_POINT('Ctrl Pts',(-19.6569681088544,-13.8322273618005,
124.639185605185)) ;
#12678 = CARTESIAN_POINT('Ctrl Pts',(-19.5851249922426,-13.8288723975086,
124.651519743502)) ;
#12679 = CARTESIAN_POINT('Ctrl Pts',(-19.5126168537562,-13.825567149945,124.657534997383)) ;
#12680 = CARTESIAN_POINT('Ctrl Pts',(-19.440714796089,-13.8222895302752,124.663499970977)) ;
#12681 = CARTESIAN_POINT('Ctrl Pts',(-19.3684348667034,-13.8190014895072,
124.663228499334)) ;
#12682 = CARTESIAN_POINT('Ctrl Pts',(-19.2965827995173,-13.8156538984272,
124.65672444002)) ;
#12683 = CARTESIAN_POINT('Ctrl Pts',(-19.2241237717474,-13.812278029026,124.650165438548)) ;
#12684 = CARTESIAN_POINT('Ctrl Pts',(-19.1523768839061,-13.8089523611346,
124.637293312943)) ;
#12685 = CARTESIAN_POINT('Ctrl Pts',(-19.0821535042039,-13.8056569319892,
124.618252651523)) ;
#12686 = CARTESIAN_POINT('Ctrl Pts',(-19.012336785255,-13.8023805865408,124.599322253804)) ;
#12687 = CARTESIAN_POINT('Ctrl Pts',(-18.9442978433093,-13.7990669066114,
124.574368048075)) ;
#12688 = CARTESIAN_POINT('Ctrl Pts',(-18.878800215249,-13.7957175977018,124.54367099853)) ;
#12689 = CARTESIAN_POINT('Ctrl Pts',(-18.8722681340602,-13.795383570984,124.540609580494)) ;
#12690 = CARTESIAN_POINT('Ctrl Pts',(-18.8657617689437,-13.7950494529779,
124.537491232689)) ;
#12691 = CARTESIAN_POINT('Ctrl Pts',(-18.8592840273916,-13.7947155573251,
124.53431736011)) ;
#12692 = CARTESIAN_POINT('Ctrl Pts',(-18.8006996277619,-13.7916958202453,
124.505613001024)) ;
#12693 = CARTESIAN_POINT('Ctrl Pts',(-18.7444522920878,-13.7887201278197,
124.472366521467)) ;
#12694 = CARTESIAN_POINT('Ctrl Pts',(-18.691055332827,-13.7857602612236,124.434880581498)) ;
#12695 = CARTESIAN_POINT('Ctrl Pts',(-18.6320350318466,-13.7824886850931,
124.393446921416)) ;
#12696 = CARTESIAN_POINT('Ctrl Pts',(-18.5767130247363,-13.7791846808591,
124.346985418166)) ;
#12697 = CARTESIAN_POINT('Ctrl Pts',(-18.525705839709,-13.7758516214606,124.296014809622)) ;
#12698 = CARTESIAN_POINT('Ctrl Pts',(-18.4742416165445,-13.7724886969507,
124.244587490677)) ;
#12699 = CARTESIAN_POINT('Ctrl Pts',(-18.42736553566,-13.7691782751684,124.188765347694)) ;
#12700 = CARTESIAN_POINT('Ctrl Pts',(-18.385610641675,-13.7658541875205,124.12918243142)) ;
#12701 = CARTESIAN_POINT('Ctrl Pts',(-18.3439058817256,-13.7625340910197,
124.069671054834)) ;
#12702 = CARTESIAN_POINT('Ctrl Pts',(-18.3074701725757,-13.7591911677825,
124.006636261331)) ;
#12703 = CARTESIAN_POINT('Ctrl Pts',(-18.2767175507807,-13.7558684310501,
123.940794408881)) ;
#12704 = CARTESIAN_POINT('Ctrl Pts',(-18.2578201439997,-13.7538266178976,
123.900334760359)) ;
#12705 = CARTESIAN_POINT('Ctrl Pts',(-18.2411044753891,-13.7517886023727,
123.858891710066)) ;
#12706 = CARTESIAN_POINT('Ctrl Pts',(-18.2266423654683,-13.7497401139871,
123.816643453356)) ;
#12707 = CARTESIAN_POINT('Origin',(-19.4092722359532,-13.9601742359176,123.411814366564)) ;
#12708 = CARTESIAN_POINT('',(-18.2266423654683,-13.389762567023,123.816643453356)) ;
#12709 = CARTESIAN_POINT('',(-18.2266423654683,-13.4498216097391,123.816643453356)) ;
#12710 = CARTESIAN_POINT('',(-18.2266423654683,-13.9601742359176,123.816643453356)) ;
#12711 = CARTESIAN_POINT('',(-20.5919018244023,-13.6298117104086,123.006984455878)) ;
#12712 = CARTESIAN_POINT('Ctrl Pts',(-18.2266423654683,-13.4498216097391,
123.816643453356)) ;
#12713 = CARTESIAN_POINT('Ctrl Pts',(-18.2411051331282,-13.451866762096,123.858893631524)) ;
#12714 = CARTESIAN_POINT('Ctrl Pts',(-18.2578210120249,-13.4539192653427,
123.900335766088)) ;
#12715 = CARTESIAN_POINT('Ctrl Pts',(-18.2767132755134,-13.4559701748973,
123.940785255369)) ;
#12716 = CARTESIAN_POINT('Ctrl Pts',(-18.3074696069924,-13.4593090259637,
124.006636438382)) ;
#12717 = CARTESIAN_POINT('Ctrl Pts',(-18.3439059816794,-13.4626146525442,
124.069671167035)) ;
#12718 = CARTESIAN_POINT('Ctrl Pts',(-18.3856104692784,-13.4659567452903,
124.129182185416)) ;
#12719 = CARTESIAN_POINT('Ctrl Pts',(-18.4273644851252,-13.4693028071056,
124.18876387908)) ;
#12720 = CARTESIAN_POINT('Ctrl Pts',(-18.4742402852349,-13.4726487236205,
124.2445862188)) ;
#12721 = CARTESIAN_POINT('Ctrl Pts',(-18.5257063424073,-13.4759548813671,
124.29601531196)) ;
#12722 = CARTESIAN_POINT('Ctrl Pts',(-18.5767150680731,-13.4792316603312,
124.346987402078)) ;
#12723 = CARTESIAN_POINT('Ctrl Pts',(-18.6320372107052,-13.4825256909799,
124.393448715711)) ;
#12724 = CARTESIAN_POINT('Ctrl Pts',(-18.6910584062643,-13.4858646864138,
124.434882739118)) ;
#12725 = CARTESIAN_POINT('Ctrl Pts',(-18.7444501579562,-13.4888852083368,
124.472364783803)) ;
#12726 = CARTESIAN_POINT('Ctrl Pts',(-18.8006970773752,-13.4918805679309,
124.505611928027)) ;
#12727 = CARTESIAN_POINT('Ctrl Pts',(-18.859286755982,-13.4948413716543,124.534318697022)) ;
#12728 = CARTESIAN_POINT('Ctrl Pts',(-18.8657621299384,-13.4951686018384,
124.537491390041)) ;
#12729 = CARTESIAN_POINT('Ctrl Pts',(-18.8722685020963,-13.4954958458738,
124.540609730944)) ;
#12730 = CARTESIAN_POINT('Ctrl Pts',(-18.8787970831716,-13.4958229221628,
124.543669530601)) ;
#12731 = CARTESIAN_POINT('Ctrl Pts',(-18.9443008042512,-13.4991046021717,
124.574369656864)) ;
#12732 = CARTESIAN_POINT('Ctrl Pts',(-19.0123400187616,-13.5024091769527,
124.599323127993)) ;
#12733 = CARTESIAN_POINT('Ctrl Pts',(-19.0821534630279,-13.5057638741365,
124.618252640358)) ;
#12734 = CARTESIAN_POINT('Ctrl Pts',(-19.1523733052118,-13.5091380996785,
124.637292345173)) ;
#12735 = CARTESIAN_POINT('Ctrl Pts',(-19.2241200758587,-13.5124685609189,
124.650165107281)) ;
#12736 = CARTESIAN_POINT('Ctrl Pts',(-19.2965828555023,-13.5157624361232,
124.656724445088)) ;
#12737 = CARTESIAN_POINT('Ctrl Pts',(-19.3684380285421,-13.5190286919022,
124.663228782286)) ;
#12738 = CARTESIAN_POINT('Ctrl Pts',(-19.4407179870657,-13.5223421499354,
124.663499697653)) ;
#12739 = CARTESIAN_POINT('Ctrl Pts',(-19.5126167057451,-13.525677463468,124.657535009662)) ;
#12740 = CARTESIAN_POINT('Ctrl Pts',(-19.585123561392,-13.5290409878991,124.651519870879)) ;
#12741 = CARTESIAN_POINT('Ctrl Pts',(-19.6569671415057,-13.5323424562459,
124.639186510576)) ;
#12742 = CARTESIAN_POINT('Ctrl Pts',(-19.7273397362501,-13.5356766263208,
124.620670464423)) ;
#12743 = CARTESIAN_POINT('Ctrl Pts',(-19.7565608213304,-13.5370610866747,
124.612981974864)) ;
#12744 = CARTESIAN_POINT('Ctrl Pts',(-19.7855040203861,-13.538454324686,124.604233408267)) ;
#12745 = CARTESIAN_POINT('Ctrl Pts',(-19.8140996478306,-13.5398436253275,
124.594444810392)) ;
#12746 = CARTESIAN_POINT('Ctrl Pts',(-19.8543069293484,-13.5417970709064,
124.58068141558)) ;
#12747 = CARTESIAN_POINT('Ctrl Pts',(-19.8937845784459,-13.5437386231534,
124.564876738282)) ;
#12748 = CARTESIAN_POINT('Ctrl Pts',(-19.9323712999088,-13.5456743108948,
124.547097313395)) ;
#12749 = CARTESIAN_POINT('Ctrl Pts',(-19.9978143159808,-13.5489572341173,
124.516943438059)) ;
#12750 = CARTESIAN_POINT('Ctrl Pts',(-20.0605169122456,-13.5522582528221,
124.481192993183)) ;
#12751 = CARTESIAN_POINT('Ctrl Pts',(-20.119790210187,-13.5555757593791,124.440242394365)) ;
#12752 = CARTESIAN_POINT('Ctrl Pts',(-20.1795094803893,-13.5589182268535,
124.398983683265)) ;
#12753 = CARTESIAN_POINT('Ctrl Pts',(-20.2355214723119,-13.5622118339914,
124.352601702896)) ;
#12754 = CARTESIAN_POINT('Ctrl Pts',(-20.2871910044519,-13.5655509085027,
124.301622568366)) ;
#12755 = CARTESIAN_POINT('Ctrl Pts',(-20.3389824289868,-13.5688978601473,
124.250523170142)) ;
#12756 = CARTESIAN_POINT('Ctrl Pts',(-20.386213329745,-13.572251750231,124.195000415073)) ;
#12757 = CARTESIAN_POINT('Ctrl Pts',(-20.4283492010573,-13.5755496368404,
124.135680472464)) ;
#12758 = CARTESIAN_POINT('Ctrl Pts',(-20.4674660268464,-13.5786112290647,
124.080610818304)) ;
#12759 = CARTESIAN_POINT('Ctrl Pts',(-20.5020545595273,-13.5816906805821,
124.022461487235)) ;
#12760 = CARTESIAN_POINT('Ctrl Pts',(-20.5317761765119,-13.5848255321454,
123.961800642308)) ;
#12761 = CARTESIAN_POINT('Ctrl Pts',(-20.5337286702634,-13.5850314690597,
123.957815666633)) ;
#12762 = CARTESIAN_POINT('Ctrl Pts',(-20.5356609628748,-13.5852375713387,
123.953818171768)) ;
#12763 = CARTESIAN_POINT('Ctrl Pts',(-20.5375707370962,-13.5854435438225,
123.949812965442)) ;
#12764 = CARTESIAN_POINT('Ctrl Pts',(-20.568906233374,-13.5888231318001,123.884095706035)) ;
#12765 = CARTESIAN_POINT('Ctrl Pts',(-20.5944392442653,-13.5921401332644,
123.815769648868)) ;
#12766 = CARTESIAN_POINT('Ctrl Pts',(-20.6138809472479,-13.5954485434704,
123.745607495236)) ;
#12767 = CARTESIAN_POINT('Ctrl Pts',(-20.633237100436,-13.5987423955991,123.675754077821)) ;
#12768 = CARTESIAN_POINT('Ctrl Pts',(-20.6464801951646,-13.6020801028086,
123.604351035323)) ;
#12769 = CARTESIAN_POINT('Ctrl Pts',(-20.653461245587,-13.6054094130713,123.532204184997)) ;
#12770 = CARTESIAN_POINT('Ctrl Pts',(-20.6604401449323,-13.6087376974708,
123.460079565342)) ;
#12771 = CARTESIAN_POINT('Ctrl Pts',(-20.6611343238489,-13.6120319361397,
123.387484385675)) ;
#12772 = CARTESIAN_POINT('Ctrl Pts',(-20.655535986198,-13.6153669540374,123.315239706836)) ;
#12773 = CARTESIAN_POINT('Ctrl Pts',(-20.6499148235769,-13.6187155691292,
123.242700479376)) ;
#12774 = CARTESIAN_POINT('Ctrl Pts',(-20.6379719182571,-13.6220539984323,
123.170790628025)) ;
#12775 = CARTESIAN_POINT('Ctrl Pts',(-20.6198380029924,-13.6253653991054,
123.100317137446)) ;
#12776 = CARTESIAN_POINT('Ctrl Pts',(-20.6117442443413,-13.6268433853789,
123.068862516879)) ;
#12777 = CARTESIAN_POINT('Ctrl Pts',(-20.6024245338594,-13.6283234680977,
123.037724446227)) ;
#12778 = CARTESIAN_POINT('Ctrl Pts',(-20.5919018244078,-13.6298117104086,
123.006984455876)) ;
#12779 = CARTESIAN_POINT('Ctrl Pts',(-20.5919018244078,-13.6298117104086,
123.006984455876)) ;
#12780 = CARTESIAN_POINT('Ctrl Pts',(-20.5790310378141,-13.6316320449137,
122.969385027943)) ;
#12781 = CARTESIAN_POINT('Ctrl Pts',(-20.5643742233044,-13.6334632796243,
122.932421164832)) ;
#12782 = CARTESIAN_POINT('Ctrl Pts',(-20.5479870005735,-13.6352947183417,
122.896228597839)) ;
#12783 = CARTESIAN_POINT('Ctrl Pts',(-20.5180638601431,-13.6386389334554,
122.830140812104)) ;
#12784 = CARTESIAN_POINT('Ctrl Pts',(-20.4824491042485,-13.6419425094988,
122.766792714165)) ;
#12785 = CARTESIAN_POINT('Ctrl Pts',(-20.4415430467989,-13.6452625229901,
122.706890985514)) ;
#12786 = CARTESIAN_POINT('Ctrl Pts',(-20.4006930189139,-13.6485779890153,
122.647071305047)) ;
#12787 = CARTESIAN_POINT('Ctrl Pts',(-20.3547207077085,-13.6519098165663,
122.590915838348)) ;
#12788 = CARTESIAN_POINT('Ctrl Pts',(-20.3041444000383,-13.6552161178838,
122.539057922863)) ;
#12789 = CARTESIAN_POINT('Ctrl Pts',(-20.2536686246012,-13.6585158471545,
122.487303087107)) ;
#12790 = CARTESIAN_POINT('Ctrl Pts',(-20.1987988823212,-13.6618078080636,
122.440025296584)) ;
#12791 = CARTESIAN_POINT('Ctrl Pts',(-20.1401511310019,-13.6651498353065,
122.397755176552)) ;
#12792 = CARTESIAN_POINT('Ctrl Pts',(-20.0830181192173,-13.668405545501,122.356576798667)) ;
#12793 = CARTESIAN_POINT('Ctrl Pts',(-20.0225069177832,-13.6716387672799,
122.320299907186)) ;
#12794 = CARTESIAN_POINT('Ctrl Pts',(-19.9592592694379,-13.6748309727741,
122.289310797272)) ;
#12795 = CARTESIAN_POINT('Ctrl Pts',(-19.9571731087758,-13.6749362644917,
122.288288652358)) ;
#12796 = CARTESIAN_POINT('Ctrl Pts',(-19.9550828947529,-13.6750416109726,
122.287271738945)) ;
#12797 = CARTESIAN_POINT('Ctrl Pts',(-19.9529911303783,-13.6751468959294,
122.286261274116)) ;
#12798 = CARTESIAN_POINT('Ctrl Pts',(-19.8877979152717,-13.6784282716526,
122.254768505734)) ;
#12799 = CARTESIAN_POINT('Ctrl Pts',(-19.8199962513967,-13.6817361681552,
122.229001185791)) ;
#12800 = CARTESIAN_POINT('Ctrl Pts',(-19.7503470286679,-13.6850947732519,
122.209247118611)) ;
#12801 = CARTESIAN_POINT('Ctrl Pts',(-19.6803520183055,-13.6884700528219,
122.189394978374)) ;
#12802 = CARTESIAN_POINT('Ctrl Pts',(-19.6087586922491,-13.691794810947,122.175691770181)) ;
#12803 = CARTESIAN_POINT('Ctrl Pts',(-19.5363764920953,-13.6950917400237,
122.168293354218)) ;
#12804 = CARTESIAN_POINT('Ctrl Pts',(-19.4647038593956,-13.6983563490884,
122.160967465412)) ;
#12805 = CARTESIAN_POINT('Ctrl Pts',(-19.3925347024683,-13.7016707095442,
122.159851859288)) ;
#12806 = CARTESIAN_POINT('Ctrl Pts',(-19.320672411073,-13.7049909610782,122.164958291828)) ;
#12807 = CARTESIAN_POINT('Ctrl Pts',(-19.2484184491182,-13.7083293089566,
122.170092555923)) ;
#12808 = CARTESIAN_POINT('Ctrl Pts',(-19.1767469037732,-13.7116146814287,
122.181497090581)) ;
#12809 = CARTESIAN_POINT('Ctrl Pts',(-19.1064574395215,-13.7149444349367,
122.199047612758)) ;
#12810 = CARTESIAN_POINT('Ctrl Pts',(-19.0720477046613,-13.7165744933897,
122.207639352946)) ;
#12811 = CARTESIAN_POINT('Ctrl Pts',(-19.0380083961707,-13.7182141781467,
122.217694693546)) ;
#12812 = CARTESIAN_POINT('Ctrl Pts',(-19.0044432721584,-13.7198430895508,
122.229184453976)) ;
#12813 = CARTESIAN_POINT('Ctrl Pts',(-18.9692063464723,-13.7215531332878,
122.241246492963)) ;
#12814 = CARTESIAN_POINT('Ctrl Pts',(-18.9345261004571,-13.7232493727939,
122.254877696253)) ;
#12815 = CARTESIAN_POINT('Ctrl Pts',(-18.9005158290295,-13.7249402776874,
122.270032023694)) ;
#12816 = CARTESIAN_POINT('Ctrl Pts',(-18.8344701658612,-13.7282239014385,
122.299460709902)) ;
#12817 = CARTESIAN_POINT('Ctrl Pts',(-18.7711147119131,-13.7315221600936,
122.334558126477)) ;
#12818 = CARTESIAN_POINT('Ctrl Pts',(-18.7111486940344,-13.734874028962,122.374932733833)) ;
#12819 = CARTESIAN_POINT('Ctrl Pts',(-18.650836934586,-13.7382452234492,122.415540126034)) ;
#12820 = CARTESIAN_POINT('Ctrl Pts',(-18.5941839619728,-13.741568557929,122.461331315927)) ;
#12821 = CARTESIAN_POINT('Ctrl Pts',(-18.5418304272057,-13.7448644969519,
122.511789528844)) ;
#12822 = CARTESIAN_POINT('Ctrl Pts',(-18.4897993844536,-13.748140133353,122.561936924721)) ;
#12823 = CARTESIAN_POINT('Ctrl Pts',(-18.4422167280386,-13.7514622574866,
122.616499809659)) ;
#12824 = CARTESIAN_POINT('Ctrl Pts',(-18.3996148755258,-13.7547935670707,
122.674866597309)) ;
#12825 = CARTESIAN_POINT('Ctrl Pts',(-18.3567697587302,-13.758143899035,122.733566669873)) ;
#12826 = CARTESIAN_POINT('Ctrl Pts',(-18.3191252112809,-13.7614413358972,
122.795891495704)) ;
#12827 = CARTESIAN_POINT('Ctrl Pts',(-18.287109025779,-13.7647793411791,122.8611332158)) ;
#12828 = CARTESIAN_POINT('Ctrl Pts',(-18.2869957400592,-13.7647911523404,
122.861364066387)) ;
#12829 = CARTESIAN_POINT('Ctrl Pts',(-18.2868824555566,-13.7648029714618,
122.861595094763)) ;
#12830 = CARTESIAN_POINT('Ctrl Pts',(-18.2867693133322,-13.7648147838155,
122.861826013248)) ;
#12831 = CARTESIAN_POINT('Ctrl Pts',(-18.2548919329702,-13.7681428684017,
122.92688639572)) ;
#12832 = CARTESIAN_POINT('Ctrl Pts',(-18.2287311833278,-13.7714802152786,
122.994594787555)) ;
#12833 = CARTESIAN_POINT('Ctrl Pts',(-18.2085821491953,-13.7747699914811,
123.064189114839)) ;
#12834 = CARTESIAN_POINT('Ctrl Pts',(-18.1884929782487,-13.7780499936923,
123.133576675976)) ;
#12835 = CARTESIAN_POINT('Ctrl Pts',(-18.1744570679719,-13.7813420328621,
123.204572243812)) ;
#12836 = CARTESIAN_POINT('Ctrl Pts',(-18.1666307377936,-13.7846958763151,
123.276381330981)) ;
#12837 = CARTESIAN_POINT('Ctrl Pts',(-18.1587479612325,-13.7880739089254,
123.3487083318)) ;
#12838 = CARTESIAN_POINT('Ctrl Pts',(-18.1571945924796,-13.7914005465369,
123.421583595596)) ;
#12839 = CARTESIAN_POINT('Ctrl Pts',(-18.1619891169103,-13.7946933269657,
123.494184391611)) ;
#12840 = CARTESIAN_POINT('Ctrl Pts',(-18.1667385232767,-13.7979551212391,
123.56610199007)) ;
#12841 = CARTESIAN_POINT('Ctrl Pts',(-18.177698121041,-13.801270000348,123.637471180153)) ;
#12842 = CARTESIAN_POINT('Ctrl Pts',(-18.1947494013785,-13.8045976378414,
123.707507255171)) ;
#12843 = CARTESIAN_POINT('Ctrl Pts',(-18.2037176269291,-13.8063478292054,
123.744343158692)) ;
#12844 = CARTESIAN_POINT('Ctrl Pts',(-18.2143600602923,-13.8080877109819,
123.780763074565)) ;
#12845 = CARTESIAN_POINT('Ctrl Pts',(-18.2266423654683,-13.8098218143905,
123.816643453356)) ;
#12846 = CARTESIAN_POINT('',(-20.5919017786445,-13.5697518725948,123.006984322209)) ;
#12847 = CARTESIAN_POINT('Ctrl Pts',(-18.2266423654683,-13.7497401139871,
123.816643453356)) ;
#12848 = CARTESIAN_POINT('Ctrl Pts',(-18.217683602435,-13.7484711482467,123.790472160059)) ;
#12849 = CARTESIAN_POINT('Ctrl Pts',(-18.209596088243,-13.747199545287,123.764010798093)) ;
#12850 = CARTESIAN_POINT('Ctrl Pts',(-18.2023931563355,-13.7459265169278,
123.73730305647)) ;
#12851 = CARTESIAN_POINT('Ctrl Pts',(-18.1834359019463,-13.7425760587033,
123.66701147818)) ;
#12852 = CARTESIAN_POINT('Ctrl Pts',(-18.1706557494658,-13.7392571781483,
123.595198077764)) ;
#12853 = CARTESIAN_POINT('Ctrl Pts',(-18.1641985295719,-13.7359220780221,
123.522681249598)) ;
#12854 = CARTESIAN_POINT('Ctrl Pts',(-18.1577686536347,-13.7326011008212,
123.450471503589)) ;
#12855 = CARTESIAN_POINT('Ctrl Pts',(-18.1576327530631,-13.7292616282286,
123.377839031082)) ;
#12856 = CARTESIAN_POINT('Ctrl Pts',(-18.1637925927213,-13.7259597703705,
123.305604864303)) ;
#12857 = CARTESIAN_POINT('Ctrl Pts',(-18.1699125413955,-13.7226792952701,
123.233838484373)) ;
#12858 = CARTESIAN_POINT('Ctrl Pts',(-18.1822235644136,-13.7194010053182,
123.162738000472)) ;
#12859 = CARTESIAN_POINT('Ctrl Pts',(-18.2005879905351,-13.7160618772626,
123.093094434721)) ;
#12860 = CARTESIAN_POINT('Ctrl Pts',(-18.219138810058,-13.7126888580616,123.022744007727)) ;
#12861 = CARTESIAN_POINT('Ctrl Pts',(-18.2437955606779,-13.7093580573816,
122.954148592409)) ;
#12862 = CARTESIAN_POINT('Ctrl Pts',(-18.274280345546,-13.7060635466254,122.888084084085)) ;
#12863 = CARTESIAN_POINT('Ctrl Pts',(-18.2783413762808,-13.7056246683622,
122.879283300352)) ;
#12864 = CARTESIAN_POINT('Ctrl Pts',(-18.2825046241964,-13.7051855312,122.870530065893)) ;
#12865 = CARTESIAN_POINT('Ctrl Pts',(-18.2867692424076,-13.7047457607437,
122.861826158003)) ;
#12866 = CARTESIAN_POINT('Ctrl Pts',(-18.3143524068913,-13.7019013652481,
122.805530069791)) ;
#12867 = CARTESIAN_POINT('Ctrl Pts',(-18.3461303693126,-13.6990184536646,
122.751390936298)) ;
#12868 = CARTESIAN_POINT('Ctrl Pts',(-18.3818346967705,-13.6961143986274,
122.699864857713)) ;
#12869 = CARTESIAN_POINT('Ctrl Pts',(-18.4232731976758,-13.6927439475965,
122.640063606545)) ;
#12870 = CARTESIAN_POINT('Ctrl Pts',(-18.4698531456278,-13.689426373171,122.583994631975)) ;
#12871 = CARTESIAN_POINT('Ctrl Pts',(-18.5210469159295,-13.6861158596704,
122.532294167282)) ;
#12872 = CARTESIAN_POINT('Ctrl Pts',(-18.571913546219,-13.6828265011154,122.480924080496)) ;
#12873 = CARTESIAN_POINT('Ctrl Pts',(-18.6271400827939,-13.6794977337672,
122.434064187781)) ;
#12874 = CARTESIAN_POINT('Ctrl Pts',(-18.6861055940097,-13.6761809275718,
122.392240922395)) ;
#12875 = CARTESIAN_POINT('Ctrl Pts',(-18.7451892734769,-13.67285747442,122.350333842215)) ;
#12876 = CARTESIAN_POINT('Ctrl Pts',(-18.8078034512258,-13.6695704256265,
122.313642136408)) ;
#12877 = CARTESIAN_POINT('Ctrl Pts',(-18.8732410608961,-13.6662262115031,
122.28257985618)) ;
#12878 = CARTESIAN_POINT('Ctrl Pts',(-18.9159303161709,-13.6640445607501,
122.26231588846)) ;
#12879 = CARTESIAN_POINT('Ctrl Pts',(-18.9597342782377,-13.6618533221964,
122.24448890521)) ;
#12880 = CARTESIAN_POINT('Ctrl Pts',(-19.0044431491614,-13.6596962188292,
122.229184496079)) ;
#12881 = CARTESIAN_POINT('Ctrl Pts',(-19.0285400460438,-13.6585335972659,
122.220935825043)) ;
#12882 = CARTESIAN_POINT('Ctrl Pts',(-19.0528835163119,-13.657379728912,122.213425529107)) ;
#12883 = CARTESIAN_POINT('Ctrl Pts',(-19.0774397388877,-13.6562275396947,
122.206664087982)) ;
#12884 = CARTESIAN_POINT('Ctrl Pts',(-19.1469020155668,-13.6529683378388,
122.187537974723)) ;
#12885 = CARTESIAN_POINT('Ctrl Pts',(-19.2178827654257,-13.6496744544506,
122.174454152537)) ;
#12886 = CARTESIAN_POINT('Ctrl Pts',(-19.2895950549861,-13.6463266758792,
122.167556606921)) ;
#12887 = CARTESIAN_POINT('Ctrl Pts',(-19.3620164691775,-13.6429457929088,
122.160590855151)) ;
#12888 = CARTESIAN_POINT('Ctrl Pts',(-19.4349066876325,-13.6396283033778,
122.159961021446)) ;
#12889 = CARTESIAN_POINT('Ctrl Pts',(-19.5074413065022,-13.636328050303,122.165675195499)) ;
#12890 = CARTESIAN_POINT('Ctrl Pts',(-19.5797278270375,-13.6330390854559,
122.171369824718)) ;
#12891 = CARTESIAN_POINT('Ctrl Pts',(-19.6513798255484,-13.629714992131,122.183343256875)) ;
#12892 = CARTESIAN_POINT('Ctrl Pts',(-19.7215877702431,-13.6263635044537,
122.201459456996)) ;
#12893 = CARTESIAN_POINT('Ctrl Pts',(-19.7917261706841,-13.6230153365818,
122.219557712172)) ;
#12894 = CARTESIAN_POINT('Ctrl Pts',(-19.8601587554996,-13.61969725647,122.243718185573)) ;
#12895 = CARTESIAN_POINT('Ctrl Pts',(-19.9261151842666,-13.6164089669526,
122.273669662735)) ;
#12896 = CARTESIAN_POINT('Ctrl Pts',(-19.9372394666596,-13.615854360497,122.278721311168)) ;
#12897 = CARTESIAN_POINT('Ctrl Pts',(-19.9482890748614,-13.6152998312536,
122.283935775826)) ;
#12898 = CARTESIAN_POINT('Ctrl Pts',(-19.9592604445148,-13.6147444918876,
122.289311373019)) ;
#12899 = CARTESIAN_POINT('Ctrl Pts',(-20.0129695493756,-13.6120258905479,
122.315627003833)) ;
#12900 = CARTESIAN_POINT('Ctrl Pts',(-20.0647188293458,-13.6092767926613,
122.34576245919)) ;
#12901 = CARTESIAN_POINT('Ctrl Pts',(-20.1141113952294,-13.6065083972215,
122.379486046878)) ;
#12902 = CARTESIAN_POINT('Ctrl Pts',(-20.1741978731161,-13.6031406205451,
122.420511079079)) ;
#12903 = CARTESIAN_POINT('Ctrl Pts',(-20.2305877405618,-13.599821667702,122.466703443609)) ;
#12904 = CARTESIAN_POINT('Ctrl Pts',(-20.2826406945403,-13.596510155924,122.517539500753)) ;
#12905 = CARTESIAN_POINT('Ctrl Pts',(-20.3346590645714,-13.5932008443122,
122.568341782456)) ;
#12906 = CARTESIAN_POINT('Ctrl Pts',(-20.3821449392596,-13.5898716234696,
122.623585216385)) ;
#12907 = CARTESIAN_POINT('Ctrl Pts',(-20.4245584780755,-13.5865186222975,
122.682640966999)) ;
#12908 = CARTESIAN_POINT('Ctrl Pts',(-20.4669279463567,-13.5831691051203,
122.741635354696)) ;
#12909 = CARTESIAN_POINT('Ctrl Pts',(-20.5040750609174,-13.5798384928574,
122.804210376071)) ;
#12910 = CARTESIAN_POINT('Ctrl Pts',(-20.535578672954,-13.5765375789663,122.869657737861)) ;
#12911 = CARTESIAN_POINT('Ctrl Pts',(-20.5570569928827,-13.5742871041785,
122.914277998338)) ;
#12912 = CARTESIAN_POINT('Ctrl Pts',(-20.5758642994148,-13.5720326291569,
122.960134052569)) ;
#12913 = CARTESIAN_POINT('Ctrl Pts',(-20.5919017786445,-13.5697518725948,
123.006984322209)) ;
#12914 = CARTESIAN_POINT('Ctrl Pts',(-20.5919017786508,-13.5697518725948,
123.006984322206)) ;
#12915 = CARTESIAN_POINT('Ctrl Pts',(-20.5992029839164,-13.5687135376991,
123.028313324747)) ;
#12916 = CARTESIAN_POINT('Ctrl Pts',(-20.6059253602587,-13.5676717649293,
123.049835019345)) ;
#12917 = CARTESIAN_POINT('Ctrl Pts',(-20.6120597630125,-13.5666314897859,
123.071517195218)) ;
#12918 = CARTESIAN_POINT('Ctrl Pts',(-20.6318565136898,-13.563274346723,123.141489227888)) ;
#12919 = CARTESIAN_POINT('Ctrl Pts',(-20.6455076403348,-13.5599739327008,
123.213046366258)) ;
#12920 = CARTESIAN_POINT('Ctrl Pts',(-20.6528618564878,-13.5566399755896,
123.285383137137)) ;
#12921 = CARTESIAN_POINT('Ctrl Pts',(-20.660220857568,-13.5533038492817,123.357766973017)) ;
#12922 = CARTESIAN_POINT('Ctrl Pts',(-20.6612462363588,-13.5499476510624,
123.430654522817)) ;
#12923 = CARTESIAN_POINT('Ctrl Pts',(-20.6559258644321,-13.5466424204047,
123.50321858242)) ;
#12924 = CARTESIAN_POINT('Ctrl Pts',(-20.6506501065631,-13.5433649058076,
123.575174155024)) ;
#12925 = CARTESIAN_POINT('Ctrl Pts',(-20.639154812979,-13.5400766780383,123.64653531386)) ;
#12926 = CARTESIAN_POINT('Ctrl Pts',(-20.6215689686222,-13.5367288178819,
123.716505410141)) ;
#12927 = CARTESIAN_POINT('Ctrl Pts',(-20.6038344301335,-13.5333526504602,
123.787067126734)) ;
#12928 = CARTESIAN_POINT('Ctrl Pts',(-20.5799743244755,-13.530026994319,123.855944559216)) ;
#12929 = CARTESIAN_POINT('Ctrl Pts',(-20.5502534132391,-13.5267312778305,
123.922365003774)) ;
#12930 = CARTESIAN_POINT('Ctrl Pts',(-20.5443254392809,-13.5260739318507,
123.935612870318)) ;
#12931 = CARTESIAN_POINT('Ctrl Pts',(-20.5381641641557,-13.5254154865591,
123.948762911758)) ;
#12932 = CARTESIAN_POINT('Ctrl Pts',(-20.5317771332164,-13.5247555390931,
123.961798689701)) ;
#12933 = CARTESIAN_POINT('Ctrl Pts',(-20.5063461686967,-13.5221278548448,
124.013702682259)) ;
#12934 = CARTESIAN_POINT('Ctrl Pts',(-20.4773484677845,-13.519468252138,124.06377475595)) ;
#12935 = CARTESIAN_POINT('Ctrl Pts',(-20.4449958583186,-13.5167925737403,
124.111654761333)) ;
#12936 = CARTESIAN_POINT('Ctrl Pts',(-20.4044204134483,-13.5134368369663,
124.171704091229)) ;
#12937 = CARTESIAN_POINT('Ctrl Pts',(-20.3587041928444,-13.5101223925437,
124.228105177321)) ;
#12938 = CARTESIAN_POINT('Ctrl Pts',(-20.3083577719846,-13.506835085905,124.280229704392)) ;
#12939 = CARTESIAN_POINT('Ctrl Pts',(-20.2582587553424,-13.5035639332156,
124.332098089565)) ;
#12940 = CARTESIAN_POINT('Ctrl Pts',(-20.2037672884561,-13.5002613201806,
124.379531995468)) ;
#12941 = CARTESIAN_POINT('Ctrl Pts',(-20.1454918425646,-13.4969268449828,
124.422002809834)) ;
#12942 = CARTESIAN_POINT('Ctrl Pts',(-20.0866940195142,-13.4935624797746,
124.464854329711)) ;
#12943 = CARTESIAN_POINT('Ctrl Pts',(-20.0242676357262,-13.4902466827157,
124.502491060534)) ;
#12944 = CARTESIAN_POINT('Ctrl Pts',(-19.958913061696,-13.4869295538181,124.534487499205)) ;
#12945 = CARTESIAN_POINT('Ctrl Pts',(-19.9119493347376,-13.4845458685422,
124.557480105792)) ;
#12946 = CARTESIAN_POINT('Ctrl Pts',(-19.8635811255283,-13.482150708584,124.577506858947)) ;
#12947 = CARTESIAN_POINT('Ctrl Pts',(-19.8140974496505,-13.4797495433924,
124.594445562851)) ;
#12948 = CARTESIAN_POINT('Ctrl Pts',(-19.7947726882597,-13.4788118211322,
124.601060601152)) ;
#12949 = CARTESIAN_POINT('Ctrl Pts',(-19.7752847959478,-13.4778732271369,
124.607202084085)) ;
#12950 = CARTESIAN_POINT('Ctrl Pts',(-19.7556641998379,-13.4769335316329,
124.612860830042)) ;
#12951 = CARTESIAN_POINT('Ctrl Pts',(-19.6860443921091,-13.4735992078467,
124.632939771746)) ;
#12952 = CARTESIAN_POINT('Ctrl Pts',(-19.6148188662507,-13.4702746386561,
124.646925572577)) ;
#12953 = CARTESIAN_POINT('Ctrl Pts',(-19.5427825802482,-13.4669784003535,
124.65466391017)) ;
#12954 = CARTESIAN_POINT('Ctrl Pts',(-19.4711211737222,-13.463699315796,124.662361977171)) ;
#12955 = CARTESIAN_POINT('Ctrl Pts',(-19.398930139708,-13.4604087499291,124.66384764412)) ;
#12956 = CARTESIAN_POINT('Ctrl Pts',(-19.3270149562398,-13.4570754198169,
124.659104926141)) ;
#12957 = CARTESIAN_POINT('Ctrl Pts',(-19.2544168698574,-13.4537104365719,
124.654317171554)) ;
#12958 = CARTESIAN_POINT('Ctrl Pts',(-19.1823760896568,-13.4503926760514,
124.643200486903)) ;
#12959 = CARTESIAN_POINT('Ctrl Pts',(-19.11171025158,-13.4470784684345,124.625880619094)) ;
#12960 = CARTESIAN_POINT('Ctrl Pts',(-19.0412853620556,-13.4437755612359,
124.608619806653)) ;
#12961 = CARTESIAN_POINT('Ctrl Pts',(-18.972496652837,-13.4404418428525,124.585264697601)) ;
#12962 = CARTESIAN_POINT('Ctrl Pts',(-18.9061147649918,-13.4371150407692,
124.556075070902)) ;
#12963 = CARTESIAN_POINT('Ctrl Pts',(-18.8903614558579,-13.4363255461744,
124.549147982387)) ;
#12964 = CARTESIAN_POINT('Ctrl Pts',(-18.8747453259081,-13.4355365787144,
124.541892804038)) ;
#12965 = CARTESIAN_POINT('Ctrl Pts',(-18.8592878554704,-13.4347481692111,
124.53431923573)) ;
#12966 = CARTESIAN_POINT('Ctrl Pts',(-18.809762050661,-13.4322221016165,124.510053488806)) ;
#12967 = CARTESIAN_POINT('Ctrl Pts',(-18.7619006318004,-13.4297044741409,
124.482538510267)) ;
#12968 = CARTESIAN_POINT('Ctrl Pts',(-18.7160195400566,-13.4271691247233,
124.451958923685)) ;
#12969 = CARTESIAN_POINT('Ctrl Pts',(-18.6556158482899,-13.4238312689983,
124.411700075169)) ;
#12970 = CARTESIAN_POINT('Ctrl Pts',(-18.5988404405405,-13.4204997684909,
124.366261186538)) ;
#12971 = CARTESIAN_POINT('Ctrl Pts',(-18.5463281077966,-13.4171952325858,
124.316152484613)) ;
#12972 = CARTESIAN_POINT('Ctrl Pts',(-18.4940118329209,-13.4139030343589,
124.266230866459)) ;
#12973 = CARTESIAN_POINT('Ctrl Pts',(-18.4461272458628,-13.410599070874,124.211864739455)) ;
#12974 = CARTESIAN_POINT('Ctrl Pts',(-18.4032120923609,-13.4072587644132,
124.153665421393)) ;
#12975 = CARTESIAN_POINT('Ctrl Pts',(-18.3600613169715,-13.4039001182927,
124.095146565079)) ;
#12976 = CARTESIAN_POINT('Ctrl Pts',(-18.3220981235732,-13.4005793799823,
124.032974773141)) ;
#12977 = CARTESIAN_POINT('Ctrl Pts',(-18.2897515266574,-13.3972674064958,
123.967847982035)) ;
#12978 = CARTESIAN_POINT('Ctrl Pts',(-18.2654336498414,-13.3947774950077,
123.918886253923)) ;
#12979 = CARTESIAN_POINT('Ctrl Pts',(-18.2443509121134,-13.392276521157,123.868375546994)) ;
#12980 = CARTESIAN_POINT('Ctrl Pts',(-18.2266423654683,-13.389762567023,123.816643453356)) ;
#12981 = CARTESIAN_POINT('Origin',(-19.4092722359532,-13.9601742359176,123.411814366564)) ;
#12982 = CARTESIAN_POINT('',(-18.2266423654684,-13.0298305431221,123.816643453356)) ;
#12983 = CARTESIAN_POINT('',(-18.2266423654688,-13.0898424649011,123.816643453357)) ;
#12984 = CARTESIAN_POINT('',(-18.2266423654683,-13.9601742359176,123.816643453356)) ;
#12985 = CARTESIAN_POINT('',(-20.5919015501437,-13.2698313022293,123.006983654703)) ;
#12986 = CARTESIAN_POINT('Ctrl Pts',(-18.2266423654692,-13.0898424649011,
123.816643453359)) ;
#12987 = CARTESIAN_POINT('Ctrl Pts',(-18.2310349193409,-13.0904621593805,
123.829475449838)) ;
#12988 = CARTESIAN_POINT('Ctrl Pts',(-18.2356360431616,-13.0910823834473,
123.842235141906)) ;
#12989 = CARTESIAN_POINT('Ctrl Pts',(-18.2440506239372,-13.0921691632372,
123.864431331654)) ;
#12990 = CARTESIAN_POINT('Ctrl Pts',(-18.2477733535108,-13.0926353551193,
123.873900795199)) ;
#12991 = CARTESIAN_POINT('Ctrl Pts',(-18.2516463086842,-13.0931062465292,
123.883409766478)) ;
#12992 = CARTESIAN_POINT('Ctrl Pts',(-18.2516813587955,-13.0931105069494,
123.883495794889)) ;
#12993 = CARTESIAN_POINT('Ctrl Pts',(-18.2517618579049,-13.0931202892023,
123.883693312144)) ;
#12994 = CARTESIAN_POINT('Ctrl Pts',(-18.2518073133862,-13.0931258110546,
123.883804798245)) ;
#12995 = CARTESIAN_POINT('Ctrl Pts',(-18.2518971976611,-13.0931367262883,
123.884025161276)) ;
#12996 = CARTESIAN_POINT('Ctrl Pts',(-18.2519416257492,-13.0931421196713,
123.884134038596)) ;
#12997 = CARTESIAN_POINT('Ctrl Pts',(-18.2520295016494,-13.0931527838599,
123.88434930409)) ;
#12998 = CARTESIAN_POINT('Ctrl Pts',(-18.2520729487653,-13.0931580546624,
123.884455692533)) ;
#12999 = CARTESIAN_POINT('Ctrl Pts',(-18.2521589063775,-13.0931684792276,
123.884666093028)) ;
#13000 = CARTESIAN_POINT('Ctrl Pts',(-18.2522014162068,-13.0931736329853,
123.884770105289)) ;
#13001 = CARTESIAN_POINT('Ctrl Pts',(-18.2522855402971,-13.0931838286635,
123.884975859327)) ;
#13002 = CARTESIAN_POINT('Ctrl Pts',(-18.2523271539625,-13.0931888705825,
123.885077601367)) ;
#13003 = CARTESIAN_POINT('Ctrl Pts',(-18.2524095244819,-13.0931988474895,
123.885278914824)) ;
#13004 = CARTESIAN_POINT('Ctrl Pts',(-18.2524502807722,-13.0932037824754,
123.88537848647)) ;
#13005 = CARTESIAN_POINT('Ctrl Pts',(-18.2525309731381,-13.0932135501443,
123.885575553321)) ;
#13006 = CARTESIAN_POINT('Ctrl Pts',(-18.2525709086823,-13.0932183828248,
123.885673048732)) ;
#13007 = CARTESIAN_POINT('Ctrl Pts',(-18.2526499940244,-13.0932279502384,
123.885866051727)) ;
#13008 = CARTESIAN_POINT('Ctrl Pts',(-18.2526891433718,-13.0932326849749,
123.885961559622)) ;
#13009 = CARTESIAN_POINT('Ctrl Pts',(-18.2527666891164,-13.0932420606393,
123.886150671782)) ;
#13010 = CARTESIAN_POINT('Ctrl Pts',(-18.2528050850144,-13.0932467015614,
123.886244276152)) ;
#13011 = CARTESIAN_POINT('Ctrl Pts',(-18.2528811547807,-13.0932558934961,
123.886429660569)) ;
#13012 = CARTESIAN_POINT('Ctrl Pts',(-18.2529188281946,-13.0932604445051,
123.886521440752)) ;
#13013 = CARTESIAN_POINT('Ctrl Pts',(-18.2529934823241,-13.0932694603092,
123.886703251942)) ;
#13014 = CARTESIAN_POINT('Ctrl Pts',(-18.2530304626129,-13.0932739251008,
123.886793283077)) ;
#13015 = CARTESIAN_POINT('Ctrl Pts',(-18.2531037582241,-13.0932827719612,
123.886971667157)) ;
#13016 = CARTESIAN_POINT('Ctrl Pts',(-18.2531400731929,-13.0932871540326,
123.887060020339)) ;
#13017 = CARTESIAN_POINT('Ctrl Pts',(-18.2532120645626,-13.0932958387727,
123.887235116003)) ;
#13018 = CARTESIAN_POINT('Ctrl Pts',(-18.2532477406168,-13.0933001414421,
123.887321858677)) ;
#13019 = CARTESIAN_POINT('Ctrl Pts',(-18.2533184792844,-13.0933086705353,
123.887493797491)) ;
#13020 = CARTESIAN_POINT('Ctrl Pts',(-18.2533535415375,-13.0933128969558,
123.887578993732)) ;
#13021 = CARTESIAN_POINT('Ctrl Pts',(-18.2534230763846,-13.0933212765373,
123.887747900365)) ;
#13022 = CARTESIAN_POINT('Ctrl Pts',(-18.253457548674,-13.0933254296994,123.887831610938)) ;
#13023 = CARTESIAN_POINT('Ctrl Pts',(-18.2535259262764,-13.0933336656095,
123.887997604052)) ;
#13024 = CARTESIAN_POINT('Ctrl Pts',(-18.2535598312941,-13.0933377483577,
123.888079886745)) ;
#13025 = CARTESIAN_POINT('Ctrl Pts',(-18.2536270959504,-13.093345846147,123.888243079094)) ;
#13026 = CARTESIAN_POINT('Ctrl Pts',(-18.2536604552935,-13.0933498611864,
123.888323988855)) ;
#13027 = CARTESIAN_POINT('Ctrl Pts',(-18.2537266492693,-13.0933578261462,
123.88848448791)) ;
#13028 = CARTESIAN_POINT('Ctrl Pts',(-18.2537594835681,-13.0933617760584,
123.888564077171)) ;
#13029 = CARTESIAN_POINT('Ctrl Pts',(-18.2538246470169,-13.0933696132122,
123.888721984952)) ;
#13030 = CARTESIAN_POINT('Ctrl Pts',(-18.253856975902,-13.0933735004522,123.888800303564)) ;
#13031 = CARTESIAN_POINT('Ctrl Pts',(-18.2539211471992,-13.0933812145971,
123.888955717474)) ;
#13032 = CARTESIAN_POINT('Ctrl Pts',(-18.2539529893937,-13.0933850415045,
123.889032812941)) ;
#13033 = CARTESIAN_POINT('Ctrl Pts',(-18.2540162052135,-13.0933926372212,
123.889185825978)) ;
#13034 = CARTESIAN_POINT('Ctrl Pts',(-18.254047578617,-13.093396406031,123.889261743671)) ;
#13035 = CARTESIAN_POINT('Ctrl Pts',(-18.2541098739552,-13.0934038876874,
123.8894124445)) ;
#13036 = CARTESIAN_POINT('Ctrl Pts',(-18.2541407956692,-13.0934076005332,
123.889487227727)) ;
#13037 = CARTESIAN_POINT('Ctrl Pts',(-18.2542022040059,-13.0934149723049,
123.889635701095)) ;
#13038 = CARTESIAN_POINT('Ctrl Pts',(-18.2542326903996,-13.0934186312276,
123.889709391274)) ;
#13039 = CARTESIAN_POINT('Ctrl Pts',(-18.2542932437135,-13.0934258971,123.889855718061)) ;
#13040 = CARTESIAN_POINT('Ctrl Pts',(-18.2543233104349,-13.0934295040491,
123.889928354751)) ;
#13041 = CARTESIAN_POINT('Ctrl Pts',(-18.2543830393939,-13.0934366678415,
123.890072612448)) ;
#13042 = CARTESIAN_POINT('Ctrl Pts',(-18.2544127014494,-13.093440224685,123.89014423355)) ;
#13043 = CARTESIAN_POINT('Ctrl Pts',(-18.254471635314,-13.0934472900391,123.890286496041)) ;
#13044 = CARTESIAN_POINT('Ctrl Pts',(-18.2545009070083,-13.0934507985568,
123.890357137662)) ;
#13045 = CARTESIAN_POINT('Ctrl Pts',(-18.2545590740688,-13.09345776899,123.890497476293)) ;
#13046 = CARTESIAN_POINT('Ctrl Pts',(-18.2545879692201,-13.0934612308995,
123.890567173269)) ;
#13047 = CARTESIAN_POINT('Ctrl Pts',(-18.2546453963592,-13.0934681097528,
123.890705655805)) ;
#13048 = CARTESIAN_POINT('Ctrl Pts',(-18.2546739281699,-13.0934715266943,
123.890774441398)) ;
#13049 = CARTESIAN_POINT('Ctrl Pts',(-18.2547306413153,-13.0934783171873,
123.890911133128)) ;
#13050 = CARTESIAN_POINT('Ctrl Pts',(-18.2547588224857,-13.0934816907372,
123.890979039307)) ;
#13051 = CARTESIAN_POINT('Ctrl Pts',(-18.2548148464286,-13.0934883959466,
123.891114002616)) ;
#13052 = CARTESIAN_POINT('Ctrl Pts',(-18.2548426890988,-13.093491727611,123.891181059918)) ;
#13053 = CARTESIAN_POINT('Ctrl Pts',(-18.2548980478379,-13.0934983505123,
123.891314355129)) ;
#13054 = CARTESIAN_POINT('Ctrl Pts',(-18.2549255637414,-13.0935016417458,
123.891380593038)) ;
#13055 = CARTESIAN_POINT('Ctrl Pts',(-18.2549802802188,-13.0935081851821,
123.891512277781)) ;
#13056 = CARTESIAN_POINT('Ctrl Pts',(-18.2550074806312,-13.0935114373813,
123.891577724607)) ;
#13057 = CARTESIAN_POINT('Ctrl Pts',(-18.2550615769081,-13.0935179040846,
123.891707854257)) ;
#13058 = CARTESIAN_POINT('Ctrl Pts',(-18.2550884726559,-13.0935211185898,
123.891772537162)) ;
#13059 = CARTESIAN_POINT('Ctrl Pts',(-18.2551419700071,-13.0935275111928,
123.89190116507)) ;
#13060 = CARTESIAN_POINT('Ctrl Pts',(-18.2551685715089,-13.0935306892928,
123.891965110173)) ;
#13061 = CARTESIAN_POINT('Ctrl Pts',(-18.2588710159056,-13.09397293733,123.900863018245)) ;
#13062 = CARTESIAN_POINT('Ctrl Pts',(-18.2626481557355,-13.0944123725398,
123.909654470195)) ;
#13063 = CARTESIAN_POINT('Ctrl Pts',(-18.2713158519632,-13.0953955404166,
123.929206832528)) ;
#13064 = CARTESIAN_POINT('Ctrl Pts',(-18.2762588528341,-13.0959394388412,
123.939943487203)) ;
#13065 = CARTESIAN_POINT('Ctrl Pts',(-18.2894723128965,-13.0973517592336,
123.967604727234)) ;
#13066 = CARTESIAN_POINT('Ctrl Pts',(-18.2979743756871,-13.0982214800677,
123.984415321352)) ;
#13067 = CARTESIAN_POINT('Ctrl Pts',(-18.3107049403825,-13.099467662679,124.008234247871)) ;
#13068 = CARTESIAN_POINT('Ctrl Pts',(-18.314627450329,-13.0998445454559,124.015403275877)) ;
#13069 = CARTESIAN_POINT('Ctrl Pts',(-18.3236841768078,-13.100698657994,124.031577227637)) ;
#13070 = CARTESIAN_POINT('Ctrl Pts',(-18.3288606811316,-13.1011756304112,
124.040557805285)) ;
#13071 = CARTESIAN_POINT('Ctrl Pts',(-18.3370102802456,-13.1019095112886,
124.054298431914)) ;
#13072 = CARTESIAN_POINT('Ctrl Pts',(-18.3399047205286,-13.1021669917538,
124.059104558902)) ;
#13073 = CARTESIAN_POINT('Ctrl Pts',(-18.345200664374,-13.102632451578,124.06776582654)) ;
#13074 = CARTESIAN_POINT('Ctrl Pts',(-18.3475910075618,-13.1028405148632,
124.071627670998)) ;
#13075 = CARTESIAN_POINT('Ctrl Pts',(-18.3527709573131,-13.1032871125696,
124.07989538022)) ;
#13076 = CARTESIAN_POINT('Ctrl Pts',(-18.3555671953804,-13.1035255895825,
124.084296991062)) ;
#13077 = CARTESIAN_POINT('Ctrl Pts',(-18.3620621274432,-13.1040736458535,
124.094380813642)) ;
#13078 = CARTESIAN_POINT('Ctrl Pts',(-18.3657796736979,-13.1043830718856,
124.1000506915)) ;
#13079 = CARTESIAN_POINT('Ctrl Pts',(-18.3764534158412,-13.1052598094217,
124.116044622508)) ;
#13080 = CARTESIAN_POINT('Ctrl Pts',(-18.3835179685778,-13.105826351122,124.126295404085)) ;
#13081 = CARTESIAN_POINT('Ctrl Pts',(-18.4082567007505,-13.1077673156245,
124.161068350903)) ;
#13082 = CARTESIAN_POINT('Ctrl Pts',(-18.426666418208,-13.1091407114837,124.18505393761)) ;
#13083 = CARTESIAN_POINT('Ctrl Pts',(-18.450842503503,-13.1108736009269,124.214292990531)) ;
#13084 = CARTESIAN_POINT('Ctrl Pts',(-18.4558124867118,-13.1112262783963,
124.220191753671)) ;
#13085 = CARTESIAN_POINT('Ctrl Pts',(-18.4645840571794,-13.1118427289033,
124.230409101703)) ;
#13086 = CARTESIAN_POINT('Ctrl Pts',(-18.4683614606816,-13.1121063083581,
124.23474814777)) ;
#13087 = CARTESIAN_POINT('Ctrl Pts',(-18.4721925190756,-13.1123717686401,
124.239087964348)) ;
#13088 = CARTESIAN_POINT('Ctrl Pts',(-18.4722163631817,-13.112373420765,124.239114972558)) ;
#13089 = CARTESIAN_POINT('Ctrl Pts',(-18.4722637217479,-13.1123767020309,
124.239168610915)) ;
#13090 = CARTESIAN_POINT('Ctrl Pts',(-18.4722872362699,-13.1123783311782,
124.239195241196)) ;
#13091 = CARTESIAN_POINT('Ctrl Pts',(-18.472333945564,-13.1123815671806,124.239248135096)) ;
#13092 = CARTESIAN_POINT('Ctrl Pts',(-18.4723571399538,-13.112383174011,124.239274398343)) ;
#13093 = CARTESIAN_POINT('Ctrl Pts',(-18.4724032156809,-13.1123863658493,
124.239326565945)) ;
#13094 = CARTESIAN_POINT('Ctrl Pts',(-18.4724260977675,-13.1123879509109,
124.239352471208)) ;
#13095 = CARTESIAN_POINT('Ctrl Pts',(-18.4724715588855,-13.1123910999094,
124.239403934336)) ;
#13096 = CARTESIAN_POINT('Ctrl Pts',(-18.4724941374926,-13.1123926638187,
124.239429491778)) ;
#13097 = CARTESIAN_POINT('Ctrl Pts',(-18.4725389991235,-13.1123957710355,
124.239480267896)) ;
#13098 = CARTESIAN_POINT('Ctrl Pts',(-18.4725612821389,-13.1123973143441,
124.239505486616)) ;
#13099 = CARTESIAN_POINT('Ctrl Pts',(-18.4757623563816,-13.1126190098441,
124.243127995727)) ;
#13100 = CARTESIAN_POINT('Ctrl Pts',(-18.4789618382074,-13.1128393168581,
124.246706939893)) ;
#13101 = CARTESIAN_POINT('Ctrl Pts',(-18.4821934827412,-13.1130605712647,
124.250280219011)) ;
#13102 = CARTESIAN_POINT('Ctrl Pts',(-18.4822051132287,-13.1130613675291,
124.250293078482)) ;
#13103 = CARTESIAN_POINT('Ctrl Pts',(-18.4867060902776,-13.1133695140606,
124.255269461835)) ;
#13104 = CARTESIAN_POINT('Ctrl Pts',(-18.4912352182578,-13.1136771503203,
124.260196842037)) ;
#13105 = CARTESIAN_POINT('Ctrl Pts',(-18.5029961979599,-13.1144697875344,
124.272787515896)) ;
#13106 = CARTESIAN_POINT('Ctrl Pts',(-18.5102857583995,-13.114955144885,124.280396160682)) ;
#13107 = CARTESIAN_POINT('Ctrl Pts',(-18.5391706341844,-13.1168551330375,
124.309792211026)) ;
#13108 = CARTESIAN_POINT('Ctrl Pts',(-18.5614688750062,-13.1182719238249,
124.330873928998)) ;
#13109 = CARTESIAN_POINT('Ctrl Pts',(-18.5912077229221,-13.1200931114176,
124.356986128304)) ;
#13110 = CARTESIAN_POINT('Ctrl Pts',(-18.5979579289442,-13.1205022267812,
124.36278665988)) ;
#13111 = CARTESIAN_POINT('Ctrl Pts',(-18.610123962439,-13.1212321034245,124.373017248742)) ;
#13112 = CARTESIAN_POINT('Ctrl Pts',(-18.6155161200615,-13.1215530319699,
124.377474851738)) ;
#13113 = CARTESIAN_POINT('Ctrl Pts',(-18.6265375378131,-13.1222039352963,
124.386431376386)) ;
#13114 = CARTESIAN_POINT('Ctrl Pts',(-18.6321688506471,-13.1225338803142,
124.390927359243)) ;
#13115 = CARTESIAN_POINT('Ctrl Pts',(-18.659317713252,-13.1241124725078,124.412220967454)) ;
#13116 = CARTESIAN_POINT('Ctrl Pts',(-18.6813427454416,-13.125356647541,124.428359403571)) ;
#13117 = CARTESIAN_POINT('Ctrl Pts',(-18.7141400913974,-13.1271703067843,
124.450778179022)) ;
#13118 = CARTESIAN_POINT('Ctrl Pts',(-18.7245057083716,-13.1277383650305,
124.457639066536)) ;
#13119 = CARTESIAN_POINT('Ctrl Pts',(-18.7452014217814,-13.1288631932976,
124.470897717983)) ;
#13120 = CARTESIAN_POINT('Ctrl Pts',(-18.7555259128987,-13.1294197552475,
124.477301736512)) ;
#13121 = CARTESIAN_POINT('Ctrl Pts',(-18.8034374491011,-13.1319815211123,
124.506061454043)) ;
#13122 = CARTESIAN_POINT('Ctrl Pts',(-18.84208816418,-13.133989051426,124.526585513917)) ;
#13123 = CARTESIAN_POINT('Ctrl Pts',(-18.8978516103161,-13.1368079660639,
124.55254439048)) ;
#13124 = CARTESIAN_POINT('Ctrl Pts',(-18.9141267182019,-13.1376217468465,
124.559702410876)) ;
#13125 = CARTESIAN_POINT('Ctrl Pts',(-18.9565876111898,-13.1397245216049,
124.577306185277)) ;
#13126 = CARTESIAN_POINT('Ctrl Pts',(-18.9829839269009,-13.1410125449557,
124.587217626758)) ;
#13127 = CARTESIAN_POINT('Ctrl Pts',(-19.0168268126724,-13.1426477650394,
124.598635026514)) ;
#13128 = CARTESIAN_POINT('Ctrl Pts',(-19.0239825691278,-13.142992615301,124.600977333331)) ;
#13129 = CARTESIAN_POINT('Ctrl Pts',(-19.0395993618215,-13.1437435089535,
124.605933447781)) ;
#13130 = CARTESIAN_POINT('Ctrl Pts',(-19.0480678925587,-13.1441496124396,
124.60852228238)) ;
#13131 = CARTESIAN_POINT('Ctrl Pts',(-19.0566656126265,-13.144560997464,124.611051032389)) ;
#13132 = CARTESIAN_POINT('Ctrl Pts',(-19.0567680294082,-13.144565897787,124.611081140822)) ;
#13133 = CARTESIAN_POINT('Ctrl Pts',(-19.0569720854165,-13.1445756609693,
124.611141100707)) ;
#13134 = CARTESIAN_POINT('Ctrl Pts',(-19.0570737239492,-13.1445805237974,
124.611170952171)) ;
#13135 = CARTESIAN_POINT('Ctrl Pts',(-19.0572762544782,-13.1445902134805,
124.611230407876)) ;
#13136 = CARTESIAN_POINT('Ctrl Pts',(-19.0573771462216,-13.1445950403253,
124.61126001225)) ;
#13137 = CARTESIAN_POINT('Ctrl Pts',(-19.0575782135723,-13.1446046595024,
124.61131898331)) ;
#13138 = CARTESIAN_POINT('Ctrl Pts',(-19.0576783891745,-13.1446094518364,
124.611348350193)) ;
#13139 = CARTESIAN_POINT('Ctrl Pts',(-19.057878054072,-13.1446190034247,124.611406855605)) ;
#13140 = CARTESIAN_POINT('Ctrl Pts',(-19.0579775434136,-13.144623762683,124.611435994335)) ;
#13141 = CARTESIAN_POINT('Ctrl Pts',(-19.0581758649481,-13.1446332495206,
124.611494052542)) ;
#13142 = CARTESIAN_POINT('Ctrl Pts',(-19.0582746971249,-13.1446379771008,
124.611522972192)) ;
#13143 = CARTESIAN_POINT('Ctrl Pts',(-19.0584717333316,-13.1446474019748,
124.611580601255)) ;
#13144 = CARTESIAN_POINT('Ctrl Pts',(-19.0585699370761,-13.1446520992564,
124.611609310755)) ;
#13145 = CARTESIAN_POINT('Ctrl Pts',(-19.0587657431968,-13.1446614648194,
124.611666527853)) ;
#13146 = CARTESIAN_POINT('Ctrl Pts',(-19.0588633458189,-13.144666133114,124.611695035685)) ;
#13147 = CARTESIAN_POINT('Ctrl Pts',(-19.059057978144,-13.1446754420682,124.611751858236)) ;
#13148 = CARTESIAN_POINT('Ctrl Pts',(-19.0591550073154,-13.1446800827039,
124.611780172953)) ;
#13149 = CARTESIAN_POINT('Ctrl Pts',(-19.0593485180305,-13.1446893375547,
124.611836617113)) ;
#13150 = CARTESIAN_POINT('Ctrl Pts',(-19.0594449998465,-13.1446939517842,
124.611864746779)) ;
#13151 = CARTESIAN_POINT('Ctrl Pts',(-19.0596374421591,-13.1447031550851,
124.611920828939)) ;
#13152 = CARTESIAN_POINT('Ctrl Pts',(-19.0597334025954,-13.144707744155,124.611948781553)) ;
#13153 = CARTESIAN_POINT('Ctrl Pts',(-19.0599248278039,-13.1447168983678,
124.612004517491)) ;
#13154 = CARTESIAN_POINT('Ctrl Pts',(-19.060020292348,-13.144721463501,124.612032300878)) ;
#13155 = CARTESIAN_POINT('Ctrl Pts',(-19.0602107502955,-13.1447305710172,
124.612087705889)) ;
#13156 = CARTESIAN_POINT('Ctrl Pts',(-19.0603057437097,-13.1447351134018,
124.612115327638)) ;
#13157 = CARTESIAN_POINT('Ctrl Pts',(-19.0604952835146,-13.1447441765778,
124.61217041675)) ;
#13158 = CARTESIAN_POINT('Ctrl Pts',(-19.0605898300139,-13.1447486973754,
124.612197884261)) ;
#13159 = CARTESIAN_POINT('Ctrl Pts',(-19.0607785001241,-13.144757718535,124.612252672255)) ;
#13160 = CARTESIAN_POINT('Ctrl Pts',(-19.0608726236526,-13.1447622188941,
124.612279992824)) ;
#13161 = CARTESIAN_POINT('Ctrl Pts',(-19.0610604710687,-13.1447712002914,
124.612334494007)) ;
#13162 = CARTESIAN_POINT('Ctrl Pts',(-19.0611541950045,-13.1447756813329,
124.612361674739)) ;
#13163 = CARTESIAN_POINT('Ctrl Pts',(-19.0613412658663,-13.1447846251805,
124.612415903118)) ;
#13164 = CARTESIAN_POINT('Ctrl Pts',(-19.0614346129884,-13.1447890879967,
124.61244295092)) ;
#13165 = CARTESIAN_POINT('Ctrl Pts',(-19.0616209532137,-13.1447979964959,
124.612496920388)) ;
#13166 = CARTESIAN_POINT('Ctrl Pts',(-19.0617139461724,-13.1448024421727,
124.612523842105)) ;
#13167 = CARTESIAN_POINT('Ctrl Pts',(-19.0701246441923,-13.1452045196795,
124.614957703267)) ;
#13168 = CARTESIAN_POINT('Ctrl Pts',(-19.0784671134198,-13.1456025103169,
124.617278156111)) ;
#13169 = CARTESIAN_POINT('Ctrl Pts',(-19.0966574785671,-13.1464688668204,
124.622134743199)) ;
#13170 = CARTESIAN_POINT('Ctrl Pts',(-19.1065135525949,-13.1469373914084,
124.624637758299)) ;
#13171 = CARTESIAN_POINT('Ctrl Pts',(-19.1380898301671,-13.1484361587805,
124.63224786319)) ;
#13172 = CARTESIAN_POINT('Ctrl Pts',(-19.1599168044813,-13.1494678486818,
124.636893830941)) ;
#13173 = CARTESIAN_POINT('Ctrl Pts',(-19.1903972640696,-13.1508961541302,
124.642533339211)) ;
#13174 = CARTESIAN_POINT('Ctrl Pts',(-19.1989543551023,-13.1512958441314,
124.644024508106)) ;
#13175 = CARTESIAN_POINT('Ctrl Pts',(-19.2123542771536,-13.1519196102268,
124.646215942286)) ;
#13176 = CARTESIAN_POINT('Ctrl Pts',(-19.2171868347842,-13.1521441370725,
124.646977162109)) ;
#13177 = CARTESIAN_POINT('Ctrl Pts',(-19.2242912449845,-13.1524735931526,
124.64805353947)) ;
#13178 = CARTESIAN_POINT('Ctrl Pts',(-19.2265596862365,-13.1525786955101,
124.648390843715)) ;
#13179 = CARTESIAN_POINT('Ctrl Pts',(-19.2330304688316,-13.1528782405571,
124.649334817798)) ;
#13180 = CARTESIAN_POINT('Ctrl Pts',(-19.2372349950484,-13.1530725610995,
124.649926322557)) ;
#13181 = CARTESIAN_POINT('Ctrl Pts',(-19.2462901288882,-13.1534904117656,
124.651153208099)) ;
#13182 = CARTESIAN_POINT('Ctrl Pts',(-19.2511416191126,-13.153713883491,124.651781559505)) ;
#13183 = CARTESIAN_POINT('Ctrl Pts',(-19.2634422001535,-13.1542795397735,
124.653301330934)) ;
#13184 = CARTESIAN_POINT('Ctrl Pts',(-19.2708958641679,-13.1546214308535,
124.65415420025)) ;
#13185 = CARTESIAN_POINT('Ctrl Pts',(-19.2948238210377,-13.1557166956165,
124.656674090119)) ;
#13186 = CARTESIAN_POINT('Ctrl Pts',(-19.31132372631,-13.1564683854513,124.658080895838)) ;
#13187 = CARTESIAN_POINT('Ctrl Pts',(-19.3329598836559,-13.1574531361168,
124.659493283953)) ;
#13188 = CARTESIAN_POINT('Ctrl Pts',(-19.3380750562304,-13.157685892142,124.659795623455)) ;
#13189 = CARTESIAN_POINT('Ctrl Pts',(-19.3615756453435,-13.1587553070828,
124.661039703747)) ;
#13190 = CARTESIAN_POINT('Ctrl Pts',(-19.3799784943124,-13.1595930499558,
124.661606660638)) ;
#13191 = CARTESIAN_POINT('Ctrl Pts',(-19.4044460601184,-13.1607103448831,
124.661819735427)) ;
#13192 = CARTESIAN_POINT('Ctrl Pts',(-19.4105053340604,-13.1609873078717,
124.661828443805)) ;
#13193 = CARTESIAN_POINT('Ctrl Pts',(-19.4214952121225,-13.1614902158258,
124.661764330555)) ;
#13194 = CARTESIAN_POINT('Ctrl Pts',(-19.4264257824356,-13.1617160523299,
124.661706389616)) ;
#13195 = CARTESIAN_POINT('Ctrl Pts',(-19.4330679733629,-13.1620205884781,
124.661589024318)) ;
#13196 = CARTESIAN_POINT('Ctrl Pts',(-19.4347800097721,-13.1620991101471,
124.661555254008)) ;
#13197 = CARTESIAN_POINT('Ctrl Pts',(-19.436523232661,-13.162179090023,124.661517284954)) ;
#13198 = CARTESIAN_POINT('Ctrl Pts',(-19.4365544949973,-13.1621805243627,
124.661516602857)) ;
#13199 = CARTESIAN_POINT('Ctrl Pts',(-19.4366168350662,-13.1621833845904,
124.66151524035)) ;
#13200 = CARTESIAN_POINT('Ctrl Pts',(-19.4366479118928,-13.1621848104368,
124.661514559974)) ;
#13201 = CARTESIAN_POINT('Ctrl Pts',(-19.4367098839824,-13.1621876538171,
124.661513200884)) ;
#13202 = CARTESIAN_POINT('Ctrl Pts',(-19.4367407796487,-13.1621890713695,
124.661512522175)) ;
#13203 = CARTESIAN_POINT('Ctrl Pts',(-19.4368023945972,-13.1621918983992,
124.661511166346)) ;
#13204 = CARTESIAN_POINT('Ctrl Pts',(-19.4368331139683,-13.1621933078805,
124.661510489237)) ;
#13205 = CARTESIAN_POINT('Ctrl Pts',(-19.4368943808986,-13.1621961189775,
124.661509136545)) ;
#13206 = CARTESIAN_POINT('Ctrl Pts',(-19.4369249284788,-13.1621975205941,
124.661508460975)) ;
#13207 = CARTESIAN_POINT('Ctrl Pts',(-19.4369858576715,-13.1622003162296,
124.66150711127)) ;
#13208 = CARTESIAN_POINT('Ctrl Pts',(-19.4370162387357,-13.1622017102231,
124.66150643716)) ;
#13209 = CARTESIAN_POINT('Ctrl Pts',(-19.4370768368356,-13.1622044907013,
124.661505090367)) ;
#13210 = CARTESIAN_POINT('Ctrl Pts',(-19.4371070548759,-13.162205877232,124.661504417675)) ;
#13211 = CARTESIAN_POINT('Ctrl Pts',(-19.4371673331625,-13.1622086430699,
124.661503073616)) ;
#13212 = CARTESIAN_POINT('Ctrl Pts',(-19.437197393112,-13.1622100223635,124.661502402267)) ;
#13213 = CARTESIAN_POINT('Ctrl Pts',(-19.4372573587044,-13.1622127738874,
124.66150106085)) ;
#13214 = CARTESIAN_POINT('Ctrl Pts',(-19.4372872644325,-13.1622141461214,
124.661500390792)) ;
#13215 = CARTESIAN_POINT('Ctrl Pts',(-19.4373469272122,-13.162216883784,124.661499051864)) ;
#13216 = CARTESIAN_POINT('Ctrl Pts',(-19.4373766835954,-13.1622182491819,
124.66149838302)) ;
#13217 = CARTESIAN_POINT('Ctrl Pts',(-19.4374360496195,-13.1622209732608,
124.661497046509)) ;
#13218 = CARTESIAN_POINT('Ctrl Pts',(-19.4374656599422,-13.162222331973,124.661496378836)) ;
#13219 = CARTESIAN_POINT('Ctrl Pts',(-19.4431424395461,-13.1624828207325,
124.661368173396)) ;
#13220 = CARTESIAN_POINT('Ctrl Pts',(-19.4487886668811,-13.1627422070177,
124.661202360058)) ;
#13221 = CARTESIAN_POINT('Ctrl Pts',(-19.4610445885615,-13.1633059021537,
124.660759275812)) ;
#13222 = CARTESIAN_POINT('Ctrl Pts',(-19.4676535954587,-13.163610293137,124.660467792989)) ;
#13223 = CARTESIAN_POINT('Ctrl Pts',(-19.4860926208311,-13.1644606623515,
124.659507846472)) ;
#13224 = CARTESIAN_POINT('Ctrl Pts',(-19.4979158879045,-13.1650072329207,
124.658723622613)) ;
#13225 = CARTESIAN_POINT('Ctrl Pts',(-19.5399823241736,-13.1669554952568,
124.655332061422)) ;
#13226 = CARTESIAN_POINT('Ctrl Pts',(-19.570139811574,-13.168357632994,124.651791395006)) ;
#13227 = CARTESIAN_POINT('Ctrl Pts',(-19.6089550128361,-13.1701642708499,
124.645794258631)) ;
#13228 = CARTESIAN_POINT('Ctrl Pts',(-19.6177566470167,-13.1705741618161,
124.644337728013)) ;
#13229 = CARTESIAN_POINT('Ctrl Pts',(-19.6272606473483,-13.1710170818383,
124.642660248542)) ;
#13230 = CARTESIAN_POINT('Ctrl Pts',(-19.627979228012,-13.1710505722539,124.642532768275)) ;
#13231 = CARTESIAN_POINT('Ctrl Pts',(-19.6295028986685,-13.1711215893653,
124.642261083915)) ;
#13232 = CARTESIAN_POINT('Ctrl Pts',(-19.630307959614,-13.1711591152381,124.642116718796)) ;
#13233 = CARTESIAN_POINT('Ctrl Pts',(-19.6321185686697,-13.1712435182342,
124.641790202252)) ;
#13234 = CARTESIAN_POINT('Ctrl Pts',(-19.6331240363326,-13.1712903931164,
124.641607607661)) ;
#13235 = CARTESIAN_POINT('Ctrl Pts',(-19.6355950408535,-13.1714056020495,
124.641155738341)) ;
#13236 = CARTESIAN_POINT('Ctrl Pts',(-19.6370603226104,-13.1714739291314,
124.640885075661)) ;
#13237 = CARTESIAN_POINT('Ctrl Pts',(-19.6437717659995,-13.1717869335608,
124.63963294272)) ;
#13238 = CARTESIAN_POINT('Ctrl Pts',(-19.6490120984118,-13.1720314554083,
124.638620497968)) ;
#13239 = CARTESIAN_POINT('Ctrl Pts',(-19.662602030648,-13.1726659916714,124.635904490251)) ;
#13240 = CARTESIAN_POINT('Ctrl Pts',(-19.6709409870404,-13.1730557513577,
124.634149051108)) ;
#13241 = CARTESIAN_POINT('Ctrl Pts',(-19.6908393878121,-13.1739871506946,
124.629747266883)) ;
#13242 = CARTESIAN_POINT('Ctrl Pts',(-19.7023804036596,-13.1745284529203,
124.627021432699)) ;
#13243 = CARTESIAN_POINT('Ctrl Pts',(-19.7460984587356,-13.1765853735677,
124.616036769641)) ;
#13244 = CARTESIAN_POINT('Ctrl Pts',(-19.7779804360324,-13.1781007308305,
124.606660698948)) ;
#13245 = CARTESIAN_POINT('Ctrl Pts',(-19.8283478969974,-13.1805330323252,
124.589640101509)) ;
#13246 = CARTESIAN_POINT('Ctrl Pts',(-19.8470892114594,-13.1814462454693,
124.582802908141)) ;
#13247 = CARTESIAN_POINT('Ctrl Pts',(-19.8797664604814,-13.1830549926636,
124.569987420011)) ;
#13248 = CARTESIAN_POINT('Ctrl Pts',(-19.8937722886083,-13.1837499850763,
124.564198562149)) ;
#13249 = CARTESIAN_POINT('Ctrl Pts',(-19.9190991042095,-13.1850180725259,
124.553187179286)) ;
#13250 = CARTESIAN_POINT('Ctrl Pts',(-19.9304538572855,-13.185590834726,124.548047198927)) ;
#13251 = CARTESIAN_POINT('Ctrl Pts',(-19.9605375507083,-13.1871210210911,
124.533883301463)) ;
#13252 = CARTESIAN_POINT('Ctrl Pts',(-19.9791213745648,-13.1880805375218,
124.524560560187)) ;
#13253 = CARTESIAN_POINT('Ctrl Pts',(-20.011706357743,-13.1897841325236,124.507183557057)) ;
#13254 = CARTESIAN_POINT('Ctrl Pts',(-20.0258003924317,-13.1905280291399,
124.499313134937)) ;
#13255 = CARTESIAN_POINT('Ctrl Pts',(-20.0451481404434,-13.1915580342455,
124.488011880329)) ;
#13256 = CARTESIAN_POINT('Ctrl Pts',(-20.0505343489378,-13.1918457553199,
124.484811177997)) ;
#13257 = CARTESIAN_POINT('Ctrl Pts',(-20.0595177192731,-13.1923272742818,
124.479381094275)) ;
#13258 = CARTESIAN_POINT('Ctrl Pts',(-20.06312802651,-13.1925212411184,124.477173701232)) ;
#13259 = CARTESIAN_POINT('Ctrl Pts',(-20.0707778154162,-13.1929332048542,
124.472442978393)) ;
#13260 = CARTESIAN_POINT('Ctrl Pts',(-20.0748142264151,-13.1931511586604,
124.469914807443)) ;
#13261 = CARTESIAN_POINT('Ctrl Pts',(-20.0835648084347,-13.1936249669841,
124.464364073129)) ;
#13262 = CARTESIAN_POINT('Ctrl Pts',(-20.088273318736,-13.1938807445917,124.461332774182)) ;
#13263 = CARTESIAN_POINT('Ctrl Pts',(-20.1002424181368,-13.1945331689814,
124.453512907989)) ;
#13264 = CARTESIAN_POINT('Ctrl Pts',(-20.1074736957034,-13.1949294546799,
124.448680011807)) ;
#13265 = CARTESIAN_POINT('Ctrl Pts',(-20.1314072437273,-13.1962489094192,
124.432320534887)) ;
#13266 = CARTESIAN_POINT('Ctrl Pts',(-20.1478791658137,-13.1971697804674,
124.420462775931)) ;
#13267 = CARTESIAN_POINT('Ctrl Pts',(-20.1789628313203,-13.1989415873577,
124.396916469971)) ;
#13268 = CARTESIAN_POINT('Ctrl Pts',(-20.1936151270096,-13.1997923122615,
124.38529060656)) ;
#13269 = CARTESIAN_POINT('Ctrl Pts',(-20.2124628006012,-13.2009109731273,
124.369634058183)) ;
#13270 = CARTESIAN_POINT('Ctrl Pts',(-20.2168987312121,-13.2011760663774,
124.365896694586)) ;
#13271 = CARTESIAN_POINT('Ctrl Pts',(-20.2248042548,-13.2016518552551,124.359141485154)) ;
#13272 = CARTESIAN_POINT('Ctrl Pts',(-20.2282835151841,-13.2018624337127,
124.35613511065)) ;
#13273 = CARTESIAN_POINT('Ctrl Pts',(-20.2350006148788,-13.2022713162564,
124.350265922449)) ;
#13274 = CARTESIAN_POINT('Ctrl Pts',(-20.2382403519709,-13.2024695946763,
124.34740537817)) ;
#13275 = CARTESIAN_POINT('Ctrl Pts',(-20.2415009548241,-13.2026702463444,
124.344496178256)) ;
#13276 = CARTESIAN_POINT('Ctrl Pts',(-20.2415367247745,-13.2026724476971,
124.344464259622)) ;
#13277 = CARTESIAN_POINT('Ctrl Pts',(-20.2416084121409,-13.2026768597465,
124.344400283358)) ;
#13278 = CARTESIAN_POINT('Ctrl Pts',(-20.2416443297749,-13.2026790704577,
124.344368225502)) ;
#13279 = CARTESIAN_POINT('Ctrl Pts',(-20.241716322823,-13.2026835018622,124.344303961493)) ;
#13280 = CARTESIAN_POINT('Ctrl Pts',(-20.2417523976714,-13.2026857225219,
124.344271755811)) ;
#13281 = CARTESIAN_POINT('Ctrl Pts',(-20.2418247136814,-13.2026901743526,
124.344207188429)) ;
#13282 = CARTESIAN_POINT('Ctrl Pts',(-20.2418609547872,-13.2026924055213,
124.344174826744)) ;
#13283 = CARTESIAN_POINT('Ctrl Pts',(-20.241933612165,-13.202696878919,124.344109939344)) ;
#13284 = CARTESIAN_POINT('Ctrl Pts',(-20.2419700285834,-13.2026991211583,
124.344077413461)) ;
#13285 = CARTESIAN_POINT('Ctrl Pts',(-20.2420430462514,-13.2027036172961,
124.344012188917)) ;
#13286 = CARTESIAN_POINT('Ctrl Pts',(-20.242079647378,-13.2027058711886,124.343979490328)) ;
#13287 = CARTESIAN_POINT('Ctrl Pts',(-20.2421530437522,-13.2027103912095,
124.343913911951)) ;
#13288 = CARTESIAN_POINT('Ctrl Pts',(-20.2421898389658,-13.2027126573372,
124.343881032153)) ;
#13289 = CARTESIAN_POINT('Ctrl Pts',(-20.2422636327911,-13.2027172024045,
124.343815082944)) ;
#13290 = CARTESIAN_POINT('Ctrl Pts',(-20.2423006314859,-13.2027194813508,
124.343782013414)) ;
#13291 = CARTESIAN_POINT('Ctrl Pts',(-20.2423748418137,-13.2027240526477,
124.343715676079)) ;
#13292 = CARTESIAN_POINT('Ctrl Pts',(-20.2424120535201,-13.2027263450045,
124.343682408162)) ;
#13293 = CARTESIAN_POINT('Ctrl Pts',(-20.242486699591,-13.2027309437264,124.343615665223)) ;
#13294 = CARTESIAN_POINT('Ctrl Pts',(-20.2425241339824,-13.2027332500949,
124.343582190128)) ;
#13295 = CARTESIAN_POINT('Ctrl Pts',(-20.2425992350049,-13.2027378774359,
124.343515024115)) ;
#13296 = CARTESIAN_POINT('Ctrl Pts',(-20.2426369017402,-13.2027401984166,
124.343481333054)) ;
#13297 = CARTESIAN_POINT('Ctrl Pts',(-20.2427124776084,-13.2027448556137,
124.343413725867)) ;
#13298 = CARTESIAN_POINT('Ctrl Pts',(-20.2427503866397,-13.2027471918257,
124.343379809779)) ;
#13299 = CARTESIAN_POINT('Ctrl Pts',(-20.2428264570372,-13.2027518801036,
124.343311743486)) ;
#13300 = CARTESIAN_POINT('Ctrl Pts',(-20.2428646183768,-13.2027542321699,
124.343277593248)) ;
#13301 = CARTESIAN_POINT('Ctrl Pts',(-20.2465276130872,-13.2029800148025,
124.339999207004)) ;
#13302 = CARTESIAN_POINT('Ctrl Pts',(-20.2501334717912,-13.203203658973,124.336733847621)) ;
#13303 = CARTESIAN_POINT('Ctrl Pts',(-20.2589724710791,-13.2037553160657,
124.328635099664)) ;
#13304 = CARTESIAN_POINT('Ctrl Pts',(-20.2641835221125,-13.2040835582772,
124.323777873765)) ;
#13305 = CARTESIAN_POINT('Ctrl Pts',(-20.279355708365,-13.2050481212444,124.309391534564)) ;
#13306 = CARTESIAN_POINT('Ctrl Pts',(-20.2892010393449,-13.2056854730979,
124.299741908408)) ;
#13307 = CARTESIAN_POINT('Ctrl Pts',(-20.3188834461116,-13.2076412136095,
124.269670930688)) ;
#13308 = CARTESIAN_POINT('Ctrl Pts',(-20.3381843649342,-13.208960842666,124.24873295245)) ;
#13309 = CARTESIAN_POINT('Ctrl Pts',(-20.3615161931857,-13.2106091507762,
124.221619749046)) ;
#13310 = CARTESIAN_POINT('Ctrl Pts',(-20.3662301694618,-13.2109451172313,
124.216043703116)) ;
#13311 = CARTESIAN_POINT('Ctrl Pts',(-20.3734020262741,-13.211460815155,124.207407946915)) ;
#13312 = CARTESIAN_POINT('Ctrl Pts',(-20.375894791969,-13.211640925463,124.204377444177)) ;
#13313 = CARTESIAN_POINT('Ctrl Pts',(-20.3801244114799,-13.2119480236235,
124.199185778373)) ;
#13314 = CARTESIAN_POINT('Ctrl Pts',(-20.3818684178132,-13.2120750897628,
124.197030485814)) ;
#13315 = CARTESIAN_POINT('Ctrl Pts',(-20.3836409275724,-13.2122046863192,
124.19482500258)) ;
#13316 = CARTESIAN_POINT('Ctrl Pts',(-20.3836766105861,-13.2122072954613,
124.194780597009)) ;
#13317 = CARTESIAN_POINT('Ctrl Pts',(-20.3837438250645,-13.2122122105394,
124.194696940534)) ;
#13318 = CARTESIAN_POINT('Ctrl Pts',(-20.383775357339,-13.2122145164933,124.194657689982)) ;
#13319 = CARTESIAN_POINT('Ctrl Pts',(-20.3838346878026,-13.2122188556048,
124.194583827831)) ;
#13320 = CARTESIAN_POINT('Ctrl Pts',(-20.3838624865803,-13.2122208887727,
124.19454921658)) ;
#13321 = CARTESIAN_POINT('Ctrl Pts',(-20.3839147403571,-13.212224710764,124.194484150196)) ;
#13322 = CARTESIAN_POINT('Ctrl Pts',(-20.3839391955521,-13.2122264995759,
124.194453695673)) ;
#13323 = CARTESIAN_POINT('Ctrl Pts',(-20.3839851232315,-13.2122298591915,
124.194396495561)) ;
#13324 = CARTESIAN_POINT('Ctrl Pts',(-20.384006596013,-13.2122314299965,124.194369750273)) ;
#13325 = CARTESIAN_POINT('Ctrl Pts',(-20.3840575440562,-13.212235157177,124.194306286905)) ;
#13326 = CARTESIAN_POINT('Ctrl Pts',(-20.3840870182223,-13.2122373135327,
124.194269568197)) ;
#13327 = CARTESIAN_POINT('Ctrl Pts',(-20.3841450951676,-13.2122415627468,
124.194197207973)) ;
#13328 = CARTESIAN_POINT('Ctrl Pts',(-20.3841736982301,-13.2122436556185,
124.194161566351)) ;
#13329 = CARTESIAN_POINT('Ctrl Pts',(-20.3842300466298,-13.212247778842,124.19409134401)) ;
#13330 = CARTESIAN_POINT('Ctrl Pts',(-20.3842577921076,-13.2122498091969,
124.194056763352)) ;
#13331 = CARTESIAN_POINT('Ctrl Pts',(-20.3843124396511,-13.2122538084129,
124.193988645799)) ;
#13332 = CARTESIAN_POINT('Ctrl Pts',(-20.3843393416097,-13.2122557772594,
124.193955109264)) ;
#13333 = CARTESIAN_POINT('Ctrl Pts',(-20.3843923164775,-13.2122596544895,
124.193889062722)) ;
#13334 = CARTESIAN_POINT('Ctrl Pts',(-20.384418389635,-13.2122615628848,124.193856552621)) ;
#13335 = CARTESIAN_POINT('Ctrl Pts',(-20.3844697217364,-13.212265320279,124.193792541086)) ;
#13336 = CARTESIAN_POINT('Ctrl Pts',(-20.3844949808291,-13.2122671692827,
124.193761039671)) ;
#13337 = CARTESIAN_POINT('Ctrl Pts',(-20.3845447001952,-13.2122708090022,
124.193699026918)) ;
#13338 = CARTESIAN_POINT('Ctrl Pts',(-20.3845691604211,-13.2122725997086,
124.193668515833)) ;
#13339 = CARTESIAN_POINT('Ctrl Pts',(-20.387271314347,-13.2124704312913,124.190297591266)) ;
#13340 = CARTESIAN_POINT('Ctrl Pts',(-20.3899318356961,-13.2126662822313,
124.186943438435)) ;
#13341 = CARTESIAN_POINT('Ctrl Pts',(-20.3956417030208,-13.2130889627621,
124.179668483476)) ;
#13342 = CARTESIAN_POINT('Ctrl Pts',(-20.3986850183309,-13.2133157255107,
124.175743039087)) ;
#13343 = CARTESIAN_POINT('Ctrl Pts',(-20.4066368105968,-13.2139122399235,
124.165359128652)) ;
#13344 = CARTESIAN_POINT('Ctrl Pts',(-20.4115059607716,-13.2142815979078,
124.158870833534)) ;
#13345 = CARTESIAN_POINT('Ctrl Pts',(-20.4279107743671,-13.2155408918573,
124.136561825865)) ;
#13346 = CARTESIAN_POINT('Ctrl Pts',(-20.4391377325234,-13.2164282997163,
124.120517698698)) ;
#13347 = CARTESIAN_POINT('Ctrl Pts',(-20.4604098068225,-13.2181707260936,
124.088544831266)) ;
#13348 = CARTESIAN_POINT('Ctrl Pts',(-20.4704810381876,-13.2190255576639,
124.072639749763)) ;
#13349 = CARTESIAN_POINT('Ctrl Pts',(-20.4846951720288,-13.2202814601768,
124.049028487326)) ;
#13350 = CARTESIAN_POINT('Ctrl Pts',(-20.4891225103211,-13.2206801676099,
124.041496596796)) ;
#13351 = CARTESIAN_POINT('Ctrl Pts',(-20.4959629754166,-13.2213085324731,
124.029575095466)) ;
#13352 = CARTESIAN_POINT('Ctrl Pts',(-20.4984293048242,-13.221537713073,124.0252163233)) ;
#13353 = CARTESIAN_POINT('Ctrl Pts',(-20.5028175879064,-13.2219503033097,
124.017350948677)) ;
#13354 = CARTESIAN_POINT('Ctrl Pts',(-20.5047490376571,-13.2221336247457,
124.013849719241)) ;
#13355 = CARTESIAN_POINT('Ctrl Pts',(-20.5067105899526,-13.2223215959497,
124.010253226312)) ;
#13356 = CARTESIAN_POINT('Ctrl Pts',(-20.5067575187116,-13.2223260940893,
124.010167158665)) ;
#13357 = CARTESIAN_POINT('Ctrl Pts',(-20.5068505934254,-13.2223350174414,
124.00999641125)) ;
#13358 = CARTESIAN_POINT('Ctrl Pts',(-20.5068967396566,-13.2223394426462,
124.009911731753)) ;
#13359 = CARTESIAN_POINT('Ctrl Pts',(-20.5069883325988,-13.2223482280149,
124.009743610095)) ;
#13360 = CARTESIAN_POINT('Ctrl Pts',(-20.5070337796333,-13.2223525881798,
124.009660168022)) ;
#13361 = CARTESIAN_POINT('Ctrl Pts',(-20.5071240516448,-13.2223612508123,
124.009494380994)) ;
#13362 = CARTESIAN_POINT('Ctrl Pts',(-20.5071688768753,-13.2223655532779,
124.00941203617)) ;
#13363 = CARTESIAN_POINT('Ctrl Pts',(-20.5072579776126,-13.2223741073777,
124.009248312512)) ;
#13364 = CARTESIAN_POINT('Ctrl Pts',(-20.5073022532778,-13.2223783590042,
124.009166933908)) ;
#13365 = CARTESIAN_POINT('Ctrl Pts',(-20.5073903223693,-13.222386817839,124.009005020179)) ;
#13366 = CARTESIAN_POINT('Ctrl Pts',(-20.5074341160333,-13.2223910250504,
124.008924485067)) ;
#13367 = CARTESIAN_POINT('Ctrl Pts',(-20.5075212847402,-13.2223994011089,
124.008764142647)) ;
#13368 = CARTESIAN_POINT('Ctrl Pts',(-20.5075646599821,-13.2224035699582,
124.008684335357)) ;
#13369 = CARTESIAN_POINT('Ctrl Pts',(-20.5076510520888,-13.2224118750332,
124.008525338863)) ;
#13370 = CARTESIAN_POINT('Ctrl Pts',(-20.5076940690545,-13.2224160112544,
124.008446149797)) ;
#13371 = CARTESIAN_POINT('Ctrl Pts',(-20.5077798015358,-13.2224242565055,
124.0082882859)) ;
#13372 = CARTESIAN_POINT('Ctrl Pts',(-20.5078225172013,-13.2224283655379,
124.008209611062)) ;
#13373 = CARTESIAN_POINT('Ctrl Pts',(-20.5079077016156,-13.2224365616231,
124.008052675961)) ;
#13374 = CARTESIAN_POINT('Ctrl Pts',(-20.5079501703968,-13.2224406486693,
124.007974415855)) ;
#13375 = CARTESIAN_POINT('Ctrl Pts',(-20.5080349130489,-13.2224488057597,
124.007818215007)) ;
#13376 = CARTESIAN_POINT('Ctrl Pts',(-20.5080771869836,-13.2224528758026,
124.007740274315)) ;
#13377 = CARTESIAN_POINT('Ctrl Pts',(-20.5081615899908,-13.2224610036838,
124.007584620499)) ;
#13378 = CARTESIAN_POINT('Ctrl Pts',(-20.5082037191219,-13.2224650615225,
124.007506907386)) ;
#13379 = CARTESIAN_POINT('Ctrl Pts',(-20.5082878809129,-13.2224731696416,
124.007351619802)) ;
#13380 = CARTESIAN_POINT('Ctrl Pts',(-20.5083299136024,-13.2224772199216,
124.007274045351)) ;
#13381 = CARTESIAN_POINT('Ctrl Pts',(-20.5084139292939,-13.2224853174226,
124.007118948949)) ;
#13382 = CARTESIAN_POINT('Ctrl Pts',(-20.5084559123575,-13.2224893646482,
124.007041426915)) ;
#13383 = CARTESIAN_POINT('Ctrl Pts',(-20.5085398747323,-13.2224974604656,
124.006886350601)) ;
#13384 = CARTESIAN_POINT('Ctrl Pts',(-20.5085818539358,-13.2225015090477,
124.006808796508)) ;
#13385 = CARTESIAN_POINT('Ctrl Pts',(-20.5086658531473,-13.2225096118778,
124.006653573701)) ;
#13386 = CARTESIAN_POINT('Ctrl Pts',(-20.5087078731521,-13.2225136661279,
124.00657590494)) ;
#13387 = CARTESIAN_POINT('Ctrl Pts',(-20.5087919977242,-13.2225217845244,
124.006420371736)) ;
#13388 = CARTESIAN_POINT('Ctrl Pts',(-20.5088341023445,-13.2225258486801,
124.0063425071)) ;
#13389 = CARTESIAN_POINT('Ctrl Pts',(-20.5089184396558,-13.2225339911008,
124.006186501382)) ;
#13390 = CARTESIAN_POINT('Ctrl Pts',(-20.5089606722452,-13.2225380693621,
124.006108360351)) ;
#13391 = CARTESIAN_POINT('Ctrl Pts',(-20.5090453082258,-13.2225462441396,
124.00595172235)) ;
#13392 = CARTESIAN_POINT('Ctrl Pts',(-20.5090877115827,-13.2225503406603,
124.005873225265)) ;
#13393 = CARTESIAN_POINT('Ctrl Pts',(-20.5091727318396,-13.2225585561104,
124.005715795483)) ;
#13394 = CARTESIAN_POINT('Ctrl Pts',(-20.5092153485984,-13.2225626750358,
124.005636862826)) ;
#13395 = CARTESIAN_POINT('Ctrl Pts',(-20.509300838192,-13.2225709394361,124.005478482443)) ;
#13396 = CARTESIAN_POINT('Ctrl Pts',(-20.5093437108805,-13.2225750849084,
124.005399034726)) ;
#13397 = CARTESIAN_POINT('Ctrl Pts',(-20.5094297547471,-13.2225834065394,
124.00523954482)) ;
#13398 = CARTESIAN_POINT('Ctrl Pts',(-20.5094729258629,-13.2225875827056,
124.005159502441)) ;
#13399 = CARTESIAN_POINT('Ctrl Pts',(-20.5095596094434,-13.2225959699116,
124.00499874281)) ;
#13400 = CARTESIAN_POINT('Ctrl Pts',(-20.5096031217613,-13.2226001809528,
124.004918025482)) ;
#13401 = CARTESIAN_POINT('Ctrl Pts',(-20.5096905308847,-13.2226086421313,
124.004755834856)) ;
#13402 = CARTESIAN_POINT('Ctrl Pts',(-20.5097344275118,-13.2226128922687,
124.004674361496)) ;
#13403 = CARTESIAN_POINT('Ctrl Pts',(-20.5098226488504,-13.2226214359145,
124.004510576681)) ;
#13404 = CARTESIAN_POINT('Ctrl Pts',(-20.5098669733686,-13.2226257294237,
124.004428265143)) ;
#13405 = CARTESIAN_POINT('Ctrl Pts',(-20.5099560947392,-13.222634364159,124.004262720447)) ;
#13406 = CARTESIAN_POINT('Ctrl Pts',(-20.5100008913645,-13.2226387053849,
124.004179487218)) ;
#13407 = CARTESIAN_POINT('Ctrl Pts',(-20.5100910019517,-13.2226474399816,
124.004012014019)) ;
#13408 = CARTESIAN_POINT('Ctrl Pts',(-20.5101363156724,-13.222651833353,124.003927773953)) ;
#13409 = CARTESIAN_POINT('Ctrl Pts',(-20.5102275062613,-13.2226606767558,
124.003758200254)) ;
#13410 = CARTESIAN_POINT('Ctrl Pts',(-20.5102733829157,-13.222665126793,124.003672866418)) ;
#13411 = CARTESIAN_POINT('Ctrl Pts',(-20.510365746308,-13.2226740881611,124.003501016047)) ;
#13412 = CARTESIAN_POINT('Ctrl Pts',(-20.5104122327811,-13.2226785994953,
124.003414499346)) ;
#13413 = CARTESIAN_POINT('Ctrl Pts',(-20.5127192806822,-13.2229025432853,
123.999119602498)) ;
#13414 = CARTESIAN_POINT('Ctrl Pts',(-20.51495570431,-13.2231221882135,123.994898312744)) ;
#13415 = CARTESIAN_POINT('Ctrl Pts',(-20.5203926287287,-13.2236625351034,
123.984492257007)) ;
#13416 = CARTESIAN_POINT('Ctrl Pts',(-20.5235657444156,-13.2239834654429,
123.978293377557)) ;
#13417 = CARTESIAN_POINT('Ctrl Pts',(-20.5324914662498,-13.2249024247406,
123.960491214424)) ;
#13418 = CARTESIAN_POINT('Ctrl Pts',(-20.5381157482922,-13.2255014262097,
123.948824649928)) ;
#13419 = CARTESIAN_POINT('Ctrl Pts',(-20.5497460249898,-13.2267836645162,
123.923709293786)) ;
#13420 = CARTESIAN_POINT('Ctrl Pts',(-20.5556976834382,-13.2274672902103,
123.910237450697)) ;
#13421 = CARTESIAN_POINT('Ctrl Pts',(-20.5687669555109,-13.2290298513582,
123.879181200905)) ;
#13422 = CARTESIAN_POINT('Ctrl Pts',(-20.5757252103543,-13.2299077599351,
123.861533427979)) ;
#13423 = CARTESIAN_POINT('Ctrl Pts',(-20.5840096247004,-13.2310117694385,
123.839034620967)) ;
#13424 = CARTESIAN_POINT('Ctrl Pts',(-20.5857117523212,-13.2312420594871,
123.834324890587)) ;
#13425 = CARTESIAN_POINT('Ctrl Pts',(-20.5883811745478,-13.231608824275,123.826797480329)) ;
#13426 = CARTESIAN_POINT('Ctrl Pts',(-20.5893667745698,-13.2317455053305,
123.823986361942)) ;
#13427 = CARTESIAN_POINT('Ctrl Pts',(-20.5913247343314,-13.2320195997308,
123.818337293829)) ;
#13428 = CARTESIAN_POINT('Ctrl Pts',(-20.592296945304,-13.2321570105281,123.815499313575)) ;
#13429 = CARTESIAN_POINT('Ctrl Pts',(-20.5932702436132,-13.232295919675,123.812624445251)) ;
#13430 = CARTESIAN_POINT('Ctrl Pts',(-20.5932815534663,-13.2322975340031,
123.812591034251)) ;
#13431 = CARTESIAN_POINT('Ctrl Pts',(-20.5933039539709,-13.2323007317392,
123.812524850581)) ;
#13432 = CARTESIAN_POINT('Ctrl Pts',(-20.5933150446569,-13.2323023151451,
123.812492077986)) ;
#13433 = CARTESIAN_POINT('Ctrl Pts',(-20.593337007394,-13.2323054510967,123.812427169979)) ;
#13434 = CARTESIAN_POINT('Ctrl Pts',(-20.5933478795744,-13.2323070036539,
123.812395034357)) ;
#13435 = CARTESIAN_POINT('Ctrl Pts',(-20.5933694060848,-13.2323100779995,
123.812331398497)) ;
#13436 = CARTESIAN_POINT('Ctrl Pts',(-20.5933800603911,-13.2323115997778,
123.812299898496)) ;
#13437 = CARTESIAN_POINT('Ctrl Pts',(-20.5934011519478,-13.232314612659,123.812237532032)) ;
#13438 = CARTESIAN_POINT('Ctrl Pts',(-20.5934115892942,-13.232316103769,123.812206665449)) ;
#13439 = CARTESIAN_POINT('Ctrl Pts',(-20.5934322479728,-13.2323190554426,
123.812145563235)) ;
#13440 = CARTESIAN_POINT('Ctrl Pts',(-20.5934424691705,-13.2323205159807,
123.812115328163)) ;
#13441 = CARTESIAN_POINT('Ctrl Pts',(-20.5934626964174,-13.2323234066149,
123.812055486888)) ;
#13442 = CARTESIAN_POINT('Ctrl Pts',(-20.5934727027086,-13.2323248367394,
123.812025880128)) ;
#13443 = CARTESIAN_POINT('Ctrl Pts',(-20.5934925013243,-13.2323276666968,
123.811967292451)) ;
#13444 = CARTESIAN_POINT('Ctrl Pts',(-20.5935022936413,-13.2323290665225,
123.811938311711)) ;
#13445 = CARTESIAN_POINT('Ctrl Pts',(-20.5935216656142,-13.2323318360507,
123.811880972668)) ;
#13446 = CARTESIAN_POINT('Ctrl Pts',(-20.593531245312,-13.2323332057531,123.811852614391)) ;
#13447 = CARTESIAN_POINT('Ctrl Pts',(-20.5935501933926,-13.2323359152095,
123.811796516736)) ;
#13448 = CARTESIAN_POINT('Ctrl Pts',(-20.5935595618137,-13.232337254963,123.81176877739)) ;
#13449 = CARTESIAN_POINT('Ctrl Pts',(-20.5949634967169,-13.2325380472751,
123.807611326579)) ;
#13450 = CARTESIAN_POINT('Ctrl Pts',(-20.5963364569888,-13.2327372525458,
123.80347433993)) ;
#13451 = CARTESIAN_POINT('Ctrl Pts',(-20.5992447333403,-13.233165478885,123.794555374446)) ;
#13452 = CARTESIAN_POINT('Ctrl Pts',(-20.6007729250949,-13.2333944186272,
123.789771152056)) ;
#13453 = CARTESIAN_POINT('Ctrl Pts',(-20.6050610497314,-13.2340483877114,
123.776062058956)) ;
#13454 = CARTESIAN_POINT('Ctrl Pts',(-20.6077498272948,-13.2344726890735,
123.767115271395)) ;
#13455 = CARTESIAN_POINT('Ctrl Pts',(-20.6198084755657,-13.2364464684551,
123.725295478689)) ;
#13456 = CARTESIAN_POINT('Ctrl Pts',(-20.6279276550355,-13.2379883912266,
123.692077419293)) ;
#13457 = CARTESIAN_POINT('Ctrl Pts',(-20.6362462453926,-13.2399072669868,
123.650766479905)) ;
#13458 = CARTESIAN_POINT('Ctrl Pts',(-20.6377426628943,-13.2402702657409,
123.642950130762)) ;
#13459 = CARTESIAN_POINT('Ctrl Pts',(-20.639956169466,-13.2408365305729,123.63075888611)) ;
#13460 = CARTESIAN_POINT('Ctrl Pts',(-20.6407248013252,-13.2410393107784,
123.62639354988)) ;
#13461 = CARTESIAN_POINT('Ctrl Pts',(-20.6420475115065,-13.2413995259455,
123.618640151511)) ;
#13462 = CARTESIAN_POINT('Ctrl Pts',(-20.6426108818422,-13.2415568735001,
123.615253718243)) ;
#13463 = CARTESIAN_POINT('Ctrl Pts',(-20.6432139852792,-13.2417297357313,
123.611533849585)) ;
#13464 = CARTESIAN_POINT('Ctrl Pts',(-20.643267543516,-13.2417451260631,123.611202664968)) ;
#13465 = CARTESIAN_POINT('Ctrl Pts',(-20.6433625295904,-13.2417724912093,
123.610613801525)) ;
#13466 = CARTESIAN_POINT('Ctrl Pts',(-20.6434040100676,-13.241784465553,123.610356131217)) ;
#13467 = CARTESIAN_POINT('Ctrl Pts',(-20.6434793526173,-13.2418062587071,
123.60988717903)) ;
#13468 = CARTESIAN_POINT('Ctrl Pts',(-20.6435132411385,-13.2418160772806,
123.609675901436)) ;
#13469 = CARTESIAN_POINT('Ctrl Pts',(-20.6435758635897,-13.2418342509642,
123.609284840375)) ;
#13470 = CARTESIAN_POINT('Ctrl Pts',(-20.6436046125028,-13.2418426059436,
123.609105059261)) ;
#13471 = CARTESIAN_POINT('Ctrl Pts',(-20.6436584482548,-13.2418582736923,
123.608767925417)) ;
#13472 = CARTESIAN_POINT('Ctrl Pts',(-20.6436835442932,-13.241865586382,123.608610574118)) ;
#13473 = CARTESIAN_POINT('Ctrl Pts',(-20.6437310470047,-13.2418794452309,
123.608312367153)) ;
#13474 = CARTESIAN_POINT('Ctrl Pts',(-20.6437534596543,-13.241885991336,123.608171512468)) ;
#13475 = CARTESIAN_POINT('Ctrl Pts',(-20.6437962658573,-13.2418985076946,
123.607902195314)) ;
#13476 = CARTESIAN_POINT('Ctrl Pts',(-20.6438166634713,-13.2419044779131,
123.607773733471)) ;
#13477 = CARTESIAN_POINT('Ctrl Pts',(-20.6438559229165,-13.2419159804863,
123.607526232546)) ;
#13478 = CARTESIAN_POINT('Ctrl Pts',(-20.6438747875813,-13.2419215128154,
123.607407193926)) ;
#13479 = CARTESIAN_POINT('Ctrl Pts',(-20.6439113434672,-13.2419322434317,
123.607176305273)) ;
#13480 = CARTESIAN_POINT('Ctrl Pts',(-20.6439290367006,-13.2419374416993,
123.607064455597)) ;
#13481 = CARTESIAN_POINT('Ctrl Pts',(-20.64396353105,-13.2419475851048,123.606846203688)) ;
#13482 = CARTESIAN_POINT('Ctrl Pts',(-20.6439803336231,-13.2419525302333,
123.60673980161)) ;
#13483 = CARTESIAN_POINT('Ctrl Pts',(-20.6440132725188,-13.2419622325864,
123.606531041336)) ;
#13484 = CARTESIAN_POINT('Ctrl Pts',(-20.6440294098682,-13.241966989802,123.606428683301)) ;
#13485 = CARTESIAN_POINT('Ctrl Pts',(-20.6440612056593,-13.2419763706723,
123.606226841756)) ;
#13486 = CARTESIAN_POINT('Ctrl Pts',(-20.6440768647887,-13.2419809943155,
123.606127358472)) ;
#13487 = CARTESIAN_POINT('Ctrl Pts',(-20.6441078645935,-13.241990154814,123.60593025999)) ;
#13488 = CARTESIAN_POINT('Ctrl Pts',(-20.6441232057302,-13.2419946916694,
123.605832644777)) ;
#13489 = CARTESIAN_POINT('Ctrl Pts',(-20.644153711724,-13.242003720262,123.605638385829)) ;
#13490 = CARTESIAN_POINT('Ctrl Pts',(-20.644168876814,-13.242008211998,123.605541742112)) ;
#13491 = CARTESIAN_POINT('Ctrl Pts',(-20.6441991609771,-13.242017188754,123.605348599886)) ;
#13492 = CARTESIAN_POINT('Ctrl Pts',(-20.6442142800696,-13.242021673769,123.605252101481)) ;
#13493 = CARTESIAN_POINT('Ctrl Pts',(-20.6442445955782,-13.2420306736674,
123.605058462736)) ;
#13494 = CARTESIAN_POINT('Ctrl Pts',(-20.6442597918502,-13.242035188554,123.604961322332)) ;
#13495 = CARTESIAN_POINT('Ctrl Pts',(-20.6442903824531,-13.2420442842324,
123.604765624249)) ;
#13496 = CARTESIAN_POINT('Ctrl Pts',(-20.6443057764614,-13.2420488650311,
123.604667066432)) ;
#13497 = CARTESIAN_POINT('Ctrl Pts',(-20.6443368845317,-13.2420581291745,
123.60446774522)) ;
#13498 = CARTESIAN_POINT('Ctrl Pts',(-20.6443525980408,-13.2420628125177,
123.604366981871)) ;
#13499 = CARTESIAN_POINT('Ctrl Pts',(-20.6443844718098,-13.2420723200347,
123.604162425944)) ;
#13500 = CARTESIAN_POINT('Ctrl Pts',(-20.6444006313255,-13.2420771442172,
123.604058633201)) ;
#13501 = CARTESIAN_POINT('Ctrl Pts',(-20.644433532294,-13.2420869745007,123.603847134545)) ;
#13502 = CARTESIAN_POINT('Ctrl Pts',(-20.6444502727458,-13.2420919806114,
123.603739428455)) ;
#13503 = CARTESIAN_POINT('Ctrl Pts',(-20.6444844831264,-13.2421022198438,
123.603519133043)) ;
#13504 = CARTESIAN_POINT('Ctrl Pts',(-20.6445019517491,-13.2421074529765,
123.603406543524)) ;
#13505 = CARTESIAN_POINT('Ctrl Pts',(-20.6449826564407,-13.2422515899396,
123.600305486515)) ;
#13506 = CARTESIAN_POINT('Ctrl Pts',(-20.6454350606017,-13.2423905868134,
123.597315354453)) ;
#13507 = CARTESIAN_POINT('Ctrl Pts',(-20.646710448646,-13.2427923297152,123.588673872152)) ;
#13508 = CARTESIAN_POINT('Ctrl Pts',(-20.6475055582442,-13.2430553012139,
123.583018496788)) ;
#13509 = CARTESIAN_POINT('Ctrl Pts',(-20.6496686256223,-13.243808176189,123.566829290923)) ;
#13510 = CARTESIAN_POINT('Ctrl Pts',(-20.6509411030967,-13.2442987359153,
123.556283232296)) ;
#13511 = CARTESIAN_POINT('Ctrl Pts',(-20.6547674229386,-13.2459499561538,
123.520770943318)) ;
#13512 = CARTESIAN_POINT('Ctrl Pts',(-20.6567038410745,-13.2471120323295,
123.495744117968)) ;
#13513 = CARTESIAN_POINT('Ctrl Pts',(-20.6583711143033,-13.2487443418533,
123.460376708612)) ;
#13514 = CARTESIAN_POINT('Ctrl Pts',(-20.658729187192,-13.2492189084885,123.450071881699)) ;
#13515 = CARTESIAN_POINT('Ctrl Pts',(-20.659081761401,-13.2499434469168,123.434307408055)) ;
#13516 = CARTESIAN_POINT('Ctrl Pts',(-20.6591680572249,-13.2501939920321,
123.428850299373)) ;
#13517 = CARTESIAN_POINT('Ctrl Pts',(-20.6592697800476,-13.2506976969608,
123.417868832571)) ;
#13518 = CARTESIAN_POINT('Ctrl Pts',(-20.6592843302475,-13.2509508458169,
123.412344587542)) ;
#13519 = CARTESIAN_POINT('Ctrl Pts',(-20.6592320658466,-13.2515498551347,
123.399262759844)) ;
#13520 = CARTESIAN_POINT('Ctrl Pts',(-20.659133329772,-13.2518955266524,123.391705517948)) ;
#13521 = CARTESIAN_POINT('Ctrl Pts',(-20.6587447242202,-13.2526979643449,
123.374151119848)) ;
#13522 = CARTESIAN_POINT('Ctrl Pts',(-20.6584033994821,-13.2531544857217,
123.364155621625)) ;
#13523 = CARTESIAN_POINT('Ctrl Pts',(-20.657046757164,-13.2544968066178,123.334770965737)) ;
#13524 = CARTESIAN_POINT('Ctrl Pts',(-20.6556996299527,-13.2553818816995,
123.31540022368)) ;
#13525 = CARTESIAN_POINT('Ctrl Pts',(-20.6535233190389,-13.2564573036706,
123.291998019709)) ;
#13526 = CARTESIAN_POINT('Ctrl Pts',(-20.653124782946,-13.2566445191073,123.287929113048)) ;
#13527 = CARTESIAN_POINT('Ctrl Pts',(-20.6523541012807,-13.256989643681,123.280439657227)) ;
#13528 = CARTESIAN_POINT('Ctrl Pts',(-20.6519877812442,-13.2571474886067,
123.277018552164)) ;
#13529 = CARTESIAN_POINT('Ctrl Pts',(-20.6510804613769,-13.2575241778776,
123.268863197068)) ;
#13530 = CARTESIAN_POINT('Ctrl Pts',(-20.6505265065881,-13.2577431117644,
123.264130443661)) ;
#13531 = CARTESIAN_POINT('Ctrl Pts',(-20.6493650304723,-13.2581810325394,
123.254675812322)) ;
#13532 = CARTESIAN_POINT('Ctrl Pts',(-20.648757567283,-13.2584000157855,123.249954002097)) ;
#13533 = CARTESIAN_POINT('Ctrl Pts',(-20.6455744831582,-13.2594990464321,
123.226281291259)) ;
#13534 = CARTESIAN_POINT('Ctrl Pts',(-20.6425911423181,-13.260379790579,123.207387737494)) ;
#13535 = CARTESIAN_POINT('Ctrl Pts',(-20.6377892840867,-13.2616155057429,
123.180933216226)) ;
#13536 = CARTESIAN_POINT('Ctrl Pts',(-20.6363319886945,-13.2619719370507,
123.173309425696)) ;
#13537 = CARTESIAN_POINT('Ctrl Pts',(-20.63359074007,-13.2626106272623,123.159659339202)) ;
#13538 = CARTESIAN_POINT('Ctrl Pts',(-20.6323330578236,-13.262893015385,123.153628031461)) ;
#13539 = CARTESIAN_POINT('Ctrl Pts',(-20.6298130798562,-13.2634389804049,
123.141975078206)) ;
#13540 = CARTESIAN_POINT('Ctrl Pts',(-20.6285564052381,-13.2637025829745,
123.13635237654)) ;
#13541 = CARTESIAN_POINT('Ctrl Pts',(-20.6257019214129,-13.26428290333,123.123983012898)) ;
#13542 = CARTESIAN_POINT('Ctrl Pts',(-20.624086762122,-13.2645995092757,123.117240546905)) ;
#13543 = CARTESIAN_POINT('Ctrl Pts',(-20.6137387177837,-13.2665581274631,
123.075575905445)) ;
#13544 = CARTESIAN_POINT('Ctrl Pts',(-20.6035597890057,-13.2681895061261,
123.041040791705)) ;
#13545 = CARTESIAN_POINT('Ctrl Pts',(-20.591901550154,-13.2698313022358,123.0069836547)) ;
#13546 = CARTESIAN_POINT('Ctrl Pts',(-20.5919015501539,-13.2698313022293,
123.006983654699)) ;
#13547 = CARTESIAN_POINT('Ctrl Pts',(-20.5758636698524,-13.2720898707903,
122.960132299735)) ;
#13548 = CARTESIAN_POINT('Ctrl Pts',(-20.5570558803912,-13.2743709415705,
122.91427657311)) ;
#13549 = CARTESIAN_POINT('Ctrl Pts',(-20.5355828802695,-13.2766593340433,
122.86966647846)) ;
#13550 = CARTESIAN_POINT('Ctrl Pts',(-20.5040766219917,-13.2800169777764,
122.804212319476)) ;
#13551 = CARTESIAN_POINT('Ctrl Pts',(-20.4669292256426,-13.2833316962248,
122.741637162349)) ;
#13552 = CARTESIAN_POINT('Ctrl Pts',(-20.4245586326818,-13.2866403923901,
122.68264118227)) ;
#13553 = CARTESIAN_POINT('Ctrl Pts',(-20.3821437711191,-13.289952545466,122.623583563461)) ;
#13554 = CARTESIAN_POINT('Ctrl Pts',(-20.3346576217278,-13.2932753101363,
122.568340364587)) ;
#13555 = CARTESIAN_POINT('Ctrl Pts',(-20.2826406174913,-13.2966313478395,
122.517539425506)) ;
#13556 = CARTESIAN_POINT('Ctrl Pts',(-20.2305895807283,-13.2999895812562,
122.466705249518)) ;
#13557 = CARTESIAN_POINT('Ctrl Pts',(-20.1742002693491,-13.3033270706483,
122.420512234535)) ;
#13558 = CARTESIAN_POINT('Ctrl Pts',(-20.1141057638357,-13.3066289349038,
122.379482201974)) ;
#13559 = CARTESIAN_POINT('Ctrl Pts',(-20.0647167286884,-13.3093425921404,
122.345761419966)) ;
#13560 = CARTESIAN_POINT('Ctrl Pts',(-20.0129675752083,-13.3120689961557,
122.315625819962)) ;
#13561 = CARTESIAN_POINT('Ctrl Pts',(-19.9592567940543,-13.3148330239689,
122.289309584425)) ;
#13562 = CARTESIAN_POINT('Ctrl Pts',(-19.9482890254929,-13.3153974398404,
122.283935795875)) ;
#13563 = CARTESIAN_POINT('Ctrl Pts',(-19.9372394078935,-13.315962787667,122.278721351692)) ;
#13564 = CARTESIAN_POINT('Ctrl Pts',(-19.9261208864848,-13.3165278298207,
122.273672252187)) ;
#13565 = CARTESIAN_POINT('Ctrl Pts',(-19.8601614086344,-13.319879883934,122.243718991793)) ;
#13566 = CARTESIAN_POINT('Ctrl Pts',(-19.7917288273833,-13.3231893604028,
122.219558406364)) ;
#13567 = CARTESIAN_POINT('Ctrl Pts',(-19.7215879104552,-13.3264812840528,
122.201459493175)) ;
#13568 = CARTESIAN_POINT('Ctrl Pts',(-19.6513770194176,-13.3297764917976,
122.183342524116)) ;
#13569 = CARTESIAN_POINT('Ctrl Pts',(-19.5797249492104,-13.3330861811419,
122.171369594936)) ;
#13570 = CARTESIAN_POINT('Ctrl Pts',(-19.5074412538907,-13.3364442850282,
122.165675191354)) ;
#13571 = CARTESIAN_POINT('Ctrl Pts',(-19.4349103776582,-13.3398138722674,
122.159961315223)) ;
#13572 = CARTESIAN_POINT('Ctrl Pts',(-19.3620201718235,-13.343152644204,122.160590466159)) ;
#13573 = CARTESIAN_POINT('Ctrl Pts',(-19.2895944956645,-13.3464412063207,
122.167556660719)) ;
#13574 = CARTESIAN_POINT('Ctrl Pts',(-19.217878727295,-13.3496975343459,122.174454573476)) ;
#13575 = CARTESIAN_POINT('Ctrl Pts',(-19.1468977227055,-13.3529957519314,
122.187538562837)) ;
#13576 = CARTESIAN_POINT('Ctrl Pts',(-19.0774301610563,-13.3563408421583,
122.206666725234)) ;
#13577 = CARTESIAN_POINT('Ctrl Pts',(-19.0528841036413,-13.3575228150794,
122.213425577298)) ;
#13578 = CARTESIAN_POINT('Ctrl Pts',(-19.0285405414498,-13.3587029390482,
122.220935718747)) ;
#13579 = CARTESIAN_POINT('Ctrl Pts',(-19.0044459295036,-13.3598747971121,
122.229183544337)) ;
#13580 = CARTESIAN_POINT('Ctrl Pts',(-18.9597352574063,-13.3620493314751,
122.244488452601)) ;
#13581 = CARTESIAN_POINT('Ctrl Pts',(-18.9159313512225,-13.3641865237851,
122.262315850384)) ;
#13582 = CARTESIAN_POINT('Ctrl Pts',(-18.8732508465882,-13.3663367400634,
122.282575211106)) ;
#13583 = CARTESIAN_POINT('Ctrl Pts',(-18.8078025555862,-13.3696339827251,
122.313641866655)) ;
#13584 = CARTESIAN_POINT('Ctrl Pts',(-18.7451885059782,-13.3729744547292,
122.350334337807)) ;
#13585 = CARTESIAN_POINT('Ctrl Pts',(-18.6861050339502,-13.3762902569431,
122.392241319636)) ;
#13586 = CARTESIAN_POINT('Ctrl Pts',(-18.6271390302697,-13.3795994667584,
122.434064983005)) ;
#13587 = CARTESIAN_POINT('Ctrl Pts',(-18.5719126530199,-13.3828853672828,
122.480925013947)) ;
#13588 = CARTESIAN_POINT('Ctrl Pts',(-18.5210471848208,-13.3862235309958,
122.53229389573)) ;
#13589 = CARTESIAN_POINT('Ctrl Pts',(-18.4698550783826,-13.3895831310969,
122.583992648478)) ;
#13590 = CARTESIAN_POINT('Ctrl Pts',(-18.4232745350601,-13.3929217653088,
122.640061106466)) ;
#13591 = CARTESIAN_POINT('Ctrl Pts',(-18.3818315198481,-13.3962207864909,
122.699869442455)) ;
#13592 = CARTESIAN_POINT('Ctrl Pts',(-18.3461290173133,-13.3990628410931,
122.751393378547)) ;
#13593 = CARTESIAN_POINT('Ctrl Pts',(-18.3143510291542,-13.4019183731984,
122.805532452684)) ;
#13594 = CARTESIAN_POINT('Ctrl Pts',(-18.2867675863735,-13.4048208345985,
122.861829537912)) ;
#13595 = CARTESIAN_POINT('Ctrl Pts',(-18.2825046326577,-13.4052694029193,
122.870530114942)) ;
#13596 = CARTESIAN_POINT('Ctrl Pts',(-18.2783413961633,-13.4057187472834,
122.879283352965)) ;
#13597 = CARTESIAN_POINT('Ctrl Pts',(-18.2742825127642,-13.4061681389656,
122.888079387466)) ;
#13598 = CARTESIAN_POINT('Ctrl Pts',(-18.2437967985826,-13.4095434579958,
122.954145191128)) ;
#13599 = CARTESIAN_POINT('Ctrl Pts',(-18.2191397332698,-13.4128687018052,
123.02274052249)) ;
#13600 = CARTESIAN_POINT('Ctrl Pts',(-18.2005880082575,-13.4161655690401,
123.093094367513)) ;
#13601 = CARTESIAN_POINT('Ctrl Pts',(-18.1822228833748,-13.4194292751619,
123.162740567474)) ;
#13602 = CARTESIAN_POINT('Ctrl Pts',(-18.1699123138942,-13.4227413347909,
123.233841164989)) ;
#13603 = CARTESIAN_POINT('Ctrl Pts',(-18.1637925943239,-13.4260626235858,
123.305604845509)) ;
#13604 = CARTESIAN_POINT('Ctrl Pts',(-18.1576328251841,-13.4294056480477,
123.377838172471)) ;
#13605 = CARTESIAN_POINT('Ctrl Pts',(-18.1577686102074,-13.4326992417446,
123.450470650516)) ;
#13606 = CARTESIAN_POINT('Ctrl Pts',(-18.1641984800143,-13.4360244491812,
123.522680693047)) ;
#13607 = CARTESIAN_POINT('Ctrl Pts',(-18.1706556540056,-13.4393637769779,
123.59519737263)) ;
#13608 = CARTESIAN_POINT('Ctrl Pts',(-18.1834351267467,-13.4427053334337,
123.667011175704)) ;
#13609 = CARTESIAN_POINT('Ctrl Pts',(-18.2023961502137,-13.4460291065788,
123.737314157264)) ;
#13610 = CARTESIAN_POINT('Ctrl Pts',(-18.2095965795631,-13.4472913060453,
123.764011642907)) ;
#13611 = CARTESIAN_POINT('Ctrl Pts',(-18.2176842050297,-13.4485548533778,
123.790473920422)) ;
#13612 = CARTESIAN_POINT('Ctrl Pts',(-18.2266423654683,-13.4498216097391,
123.816643453356)) ;
#13613 = CARTESIAN_POINT('',(-20.5919015043581,-13.2097350150005,123.006983520952)) ;
#13614 = CARTESIAN_POINT('Ctrl Pts',(-18.2266423654683,-13.389762567023,123.816643453356)) ;
#13615 = CARTESIAN_POINT('Ctrl Pts',(-18.2208517141787,-13.3889405101913,
123.799727185706)) ;
#13616 = CARTESIAN_POINT('Ctrl Pts',(-18.2154234961749,-13.3881173609619,
123.782684538791)) ;
#13617 = CARTESIAN_POINT('Ctrl Pts',(-18.2103653496133,-13.3872939371745,
123.765540642041)) ;
#13618 = CARTESIAN_POINT('Ctrl Pts',(-18.1898368125956,-13.3839520637243,
123.695961970329)) ;
#13619 = CARTESIAN_POINT('Ctrl Pts',(-18.1754061855548,-13.3806318060667,
123.624737071429)) ;
#13620 = CARTESIAN_POINT('Ctrl Pts',(-18.1672328931745,-13.3773259277796,
123.552662764019)) ;
#13621 = CARTESIAN_POINT('Ctrl Pts',(-18.1590901255551,-13.3740323959423,
123.480857632224)) ;
#13622 = CARTESIAN_POINT('Ctrl Pts',(-18.1571895862557,-13.3707236336382,
123.408482713554)) ;
#13623 = CARTESIAN_POINT('Ctrl Pts',(-18.1615522218905,-13.367395382414,123.336350689321)) ;
#13624 = CARTESIAN_POINT('Ctrl Pts',(-18.1659397697021,-13.3640481257101,
123.263806765977)) ;
#13625 = CARTESIAN_POINT('Ctrl Pts',(-18.1766465054669,-13.3607406977954,
123.191783782171)) ;
#13626 = CARTESIAN_POINT('Ctrl Pts',(-18.1935445680407,-13.3574142163685,
123.121114800779)) ;
#13627 = CARTESIAN_POINT('Ctrl Pts',(-18.2149719826111,-13.3531961057843,
123.031503725253)) ;
#13628 = CARTESIAN_POINT('Ctrl Pts',(-18.2462351295285,-13.3489456270476,
122.944550720865)) ;
#13629 = CARTESIAN_POINT('Ctrl Pts',(-18.2867794094466,-13.3447298622308,
122.861805407985)) ;
#13630 = CARTESIAN_POINT('Ctrl Pts',(-18.3100370599979,-13.3423115485966,
122.814339734021)) ;
#13631 = CARTESIAN_POINT('Ctrl Pts',(-18.3362958328213,-13.3399055899912,
122.768378902966)) ;
#13632 = CARTESIAN_POINT('Ctrl Pts',(-18.3653355906569,-13.3374879499868,
122.724285253956)) ;
#13633 = CARTESIAN_POINT('Ctrl Pts',(-18.415126928534,-13.333342683659,122.648682633973)) ;
#13634 = CARTESIAN_POINT('Ctrl Pts',(-18.4728742233197,-13.3292130717818,
122.578872618133)) ;
#13635 = CARTESIAN_POINT('Ctrl Pts',(-18.53750654097,-13.3250805809609,122.515977007929)) ;
#13636 = CARTESIAN_POINT('Ctrl Pts',(-18.576278451038,-13.3226015647614,122.478246921323)) ;
#13637 = CARTESIAN_POINT('Ctrl Pts',(-18.6175297786796,-13.320121512542,122.443004244074)) ;
#13638 = CARTESIAN_POINT('Ctrl Pts',(-18.6610320384471,-13.3176364234057,
122.410496930927)) ;
#13639 = CARTESIAN_POINT('Ctrl Pts',(-18.7189857342124,-13.314325788498,122.367190699334)) ;
#13640 = CARTESIAN_POINT('Ctrl Pts',(-18.7806663699553,-13.3110019360265,
122.328946485067)) ;
#13641 = CARTESIAN_POINT('Ctrl Pts',(-18.8453187237122,-13.307674266914,122.29626228974)) ;
#13642 = CARTESIAN_POINT('Ctrl Pts',(-18.8967457914757,-13.3050273058213,
122.270263973667)) ;
#13643 = CARTESIAN_POINT('Ctrl Pts',(-18.9499160737166,-13.3023886041235,
122.247849585121)) ;
#13644 = CARTESIAN_POINT('Ctrl Pts',(-19.0044473239371,-13.2997505571177,
122.229183067009)) ;
#13645 = CARTESIAN_POINT('Ctrl Pts',(-19.0187299939376,-13.2990596073471,
122.224293985663)) ;
#13646 = CARTESIAN_POINT('Ctrl Pts',(-19.0331042467207,-13.298368351145,122.219662764486)) ;
#13647 = CARTESIAN_POINT('Ctrl Pts',(-19.0475514893392,-13.2976762861676,
122.215295206022)) ;
#13648 = CARTESIAN_POINT('Ctrl Pts',(-19.1172019067191,-13.2943398284228,
122.194239127852)) ;
#13649 = CARTESIAN_POINT('Ctrl Pts',(-19.1885509316519,-13.2910006049844,
122.179306471)) ;
#13650 = CARTESIAN_POINT('Ctrl Pts',(-19.2607930012224,-13.2876772541355,
122.170664127097)) ;
#13651 = CARTESIAN_POINT('Ctrl Pts',(-19.3286989617926,-13.2845533772443,
122.162540513421)) ;
#13652 = CARTESIAN_POINT('Ctrl Pts',(-19.397150832558,-13.2814420977885,122.160008543899)) ;
#13653 = CARTESIAN_POINT('Ctrl Pts',(-19.4653809380022,-13.2783029805218,
122.163074276061)) ;
#13654 = CARTESIAN_POINT('Ctrl Pts',(-19.4694620308998,-13.2781152184027,
122.163257648748)) ;
#13655 = CARTESIAN_POINT('Ctrl Pts',(-19.4735423315437,-13.277927356689,122.163461032831)) ;
#13656 = CARTESIAN_POINT('Ctrl Pts',(-19.4776216758803,-13.2777393867278,
122.163684423755)) ;
#13657 = CARTESIAN_POINT('Ctrl Pts',(-19.5670120361899,-13.2736204153501,
122.16857957197)) ;
#13658 = CARTESIAN_POINT('Ctrl Pts',(-19.6554229814129,-13.2695312352565,
122.183050310254)) ;
#13659 = CARTESIAN_POINT('Ctrl Pts',(-19.7413880498576,-13.2654431054393,
122.206742133779)) ;
#13660 = CARTESIAN_POINT('Ctrl Pts',(-19.7949433711462,-13.262896244141,122.22150188729)) ;
#13661 = CARTESIAN_POINT('Ctrl Pts',(-19.8475511865818,-13.2603497904714,
122.239841482505)) ;
#13662 = CARTESIAN_POINT('Ctrl Pts',(-19.8988539340659,-13.2577967950862,
122.261679695776)) ;
#13663 = CARTESIAN_POINT('Ctrl Pts',(-19.9192020596477,-13.2567842046645,
122.27034135091)) ;
#13664 = CARTESIAN_POINT('Ctrl Pts',(-19.9393590955496,-13.2557662128757,
122.27956102932)) ;
#13665 = CARTESIAN_POINT('Ctrl Pts',(-19.9592313584971,-13.2547486978814,
122.289297122329)) ;
#13666 = CARTESIAN_POINT('Ctrl Pts',(-20.0695534587163,-13.2490999002847,
122.343347646492)) ;
#13667 = CARTESIAN_POINT('Ctrl Pts',(-20.1712738397568,-13.243529037934,122.413352172863)) ;
#13668 = CARTESIAN_POINT('Ctrl Pts',(-20.2611234786059,-13.2378957449231,
122.497019602441)) ;
#13669 = CARTESIAN_POINT('Ctrl Pts',(-20.3284914887736,-13.2336719801345,
122.559752278039)) ;
#13670 = CARTESIAN_POINT('Ctrl Pts',(-20.3885923439257,-13.2294726355754,
122.629608515275)) ;
#13671 = CARTESIAN_POINT('Ctrl Pts',(-20.4404392406267,-13.2252696171872,
122.705277312654)) ;
#13672 = CARTESIAN_POINT('Ctrl Pts',(-20.4703608779298,-13.2228439909726,
122.748946933294)) ;
#13673 = CARTESIAN_POINT('Ctrl Pts',(-20.4975339476738,-13.2204171411448,
122.794554140896)) ;
#13674 = CARTESIAN_POINT('Ctrl Pts',(-20.5217638682247,-13.2179836675985,
122.84184737787)) ;
#13675 = CARTESIAN_POINT('Ctrl Pts',(-20.5490412263194,-13.2152441320232,
122.895088764183)) ;
#13676 = CARTESIAN_POINT('Ctrl Pts',(-20.5724985243224,-13.2124837581967,
122.950301743001)) ;
#13677 = CARTESIAN_POINT('Ctrl Pts',(-20.591901504369,-13.2097350150005,123.006983520948)) ;
#13678 = CARTESIAN_POINT('Ctrl Pts',(-20.5919015043689,-13.2097350149936,
123.006983520948)) ;
#13679 = CARTESIAN_POINT('Ctrl Pts',(-20.5946210858209,-13.2093497426924,
123.014928213547)) ;
#13680 = CARTESIAN_POINT('Ctrl Pts',(-20.5972574366855,-13.2089651469592,
123.022890624025)) ;
#13681 = CARTESIAN_POINT('Ctrl Pts',(-20.602492077826,-13.2081779162429,123.039250951045)) ;
#13682 = CARTESIAN_POINT('Ctrl Pts',(-20.6050795424771,-13.2077757810124,
123.047641364186)) ;
#13683 = CARTESIAN_POINT('Ctrl Pts',(-20.613334929197,-13.2064479730121,123.075448288885)) ;
#13684 = CARTESIAN_POINT('Ctrl Pts',(-20.6186199971734,-13.2055234737724,
123.09497512782)) ;
#13685 = CARTESIAN_POINT('Ctrl Pts',(-20.6305962877421,-13.2032221981241,
123.143903285706)) ;
#13686 = CARTESIAN_POINT('Ctrl Pts',(-20.6367020130782,-13.2018468734285,
123.173434582012)) ;
#13687 = CARTESIAN_POINT('Ctrl Pts',(-20.6428457861355,-13.2001628545531,
123.209723679776)) ;
#13688 = CARTESIAN_POINT('Ctrl Pts',(-20.6439049388441,-13.1998579709665,
123.216298540924)) ;
#13689 = CARTESIAN_POINT('Ctrl Pts',(-20.6458110168909,-13.1992801267645,
123.228764478808)) ;
#13690 = CARTESIAN_POINT('Ctrl Pts',(-20.6466685086863,-13.1990072266369,
123.234653755426)) ;
#13691 = CARTESIAN_POINT('Ctrl Pts',(-20.6483603441677,-13.1984404431535,
123.246885355422)) ;
#13692 = CARTESIAN_POINT('Ctrl Pts',(-20.6491881240791,-13.1981465201376,
123.253228400078)) ;
#13693 = CARTESIAN_POINT('Ctrl Pts',(-20.653781363816,-13.1964113876931,123.290662238473)) ;
#13694 = CARTESIAN_POINT('Ctrl Pts',(-20.6564259793383,-13.1949632529976,
123.321879200189)) ;
#13695 = CARTESIAN_POINT('Ctrl Pts',(-20.6592114629349,-13.1922203625568,
123.381178413588)) ;
#13696 = CARTESIAN_POINT('Ctrl Pts',(-20.6595841871457,-13.1909260926596,
123.409230991839)) ;
#13697 = CARTESIAN_POINT('Ctrl Pts',(-20.6588665845069,-13.1893054903826,
123.444458217046)) ;
#13698 = CARTESIAN_POINT('Ctrl Pts',(-20.6586582324099,-13.188975205851,123.451642612342)) ;
#13699 = CARTESIAN_POINT('Ctrl Pts',(-20.6581484001321,-13.1883528058748,
123.465189374786)) ;
#13700 = CARTESIAN_POINT('Ctrl Pts',(-20.6578602299974,-13.1880606346941,
123.471552012739)) ;
#13701 = CARTESIAN_POINT('Ctrl Pts',(-20.6571614943111,-13.1874549642785,
123.484747572547)) ;
#13702 = CARTESIAN_POINT('Ctrl Pts',(-20.6567434041897,-13.1871415129795,
123.491579888144)) ;
#13703 = CARTESIAN_POINT('Ctrl Pts',(-20.6556804399702,-13.1864394819941,
123.506887092897)) ;
#13704 = CARTESIAN_POINT('Ctrl Pts',(-20.6550052056448,-13.18605107047,123.515359541256)) ;
#13705 = CARTESIAN_POINT('Ctrl Pts',(-20.6503822642157,-13.183695725344,123.566742675482)) ;
#13706 = CARTESIAN_POINT('Ctrl Pts',(-20.6443042032766,-13.1817414224927,
123.6094325397)) ;
#13707 = CARTESIAN_POINT('Ctrl Pts',(-20.63357903935,-13.1792008227938,123.664275109249)) ;
#13708 = CARTESIAN_POINT('Ctrl Pts',(-20.6309318665241,-13.1786189595901,
123.67678855567)) ;
#13709 = CARTESIAN_POINT('Ctrl Pts',(-20.6253580497198,-13.1774742231183,
123.701274453927)) ;
#13710 = CARTESIAN_POINT('Ctrl Pts',(-20.6224454427361,-13.1769115250492,
123.713248633236)) ;
#13711 = CARTESIAN_POINT('Ctrl Pts',(-20.616980561564,-13.1759148896647,123.734351818554)) ;
#13712 = CARTESIAN_POINT('Ctrl Pts',(-20.6145005965985,-13.1754812589473,
123.743498562509)) ;
#13713 = CARTESIAN_POINT('Ctrl Pts',(-20.5961905856121,-13.1724064222122,
123.808112170504)) ;
#13714 = CARTESIAN_POINT('Ctrl Pts',(-20.5766418625237,-13.1697622421254,
123.862453108665)) ;
#13715 = CARTESIAN_POINT('Ctrl Pts',(-20.5419059478119,-13.1658113150005,
123.941396178308)) ;
#13716 = CARTESIAN_POINT('Ctrl Pts',(-20.5295081099116,-13.16450380464,123.967140942648)) ;
#13717 = CARTESIAN_POINT('Ctrl Pts',(-20.5100001568819,-13.1625794616165,
124.004333106074)) ;
#13718 = CARTESIAN_POINT('Ctrl Pts',(-20.5035698017111,-13.161963806948,124.016126578198)) ;
#13719 = CARTESIAN_POINT('Ctrl Pts',(-20.491053121771,-13.1607984553304,124.038227435898)) ;
#13720 = CARTESIAN_POINT('Ctrl Pts',(-20.4850063703509,-13.1602489441725,
124.048555514217)) ;
#13721 = CARTESIAN_POINT('Ctrl Pts',(-20.4713014719199,-13.1590313997102,
124.071211423003)) ;
#13722 = CARTESIAN_POINT('Ctrl Pts',(-20.463575087642,-13.1583630165779,124.083495891202)) ;
#13723 = CARTESIAN_POINT('Ctrl Pts',(-20.4350794840134,-13.1559581988703,
124.127098600494)) ;
#13724 = CARTESIAN_POINT('Ctrl Pts',(-20.413114441118,-13.1542165471007,124.157611174154)) ;
#13725 = CARTESIAN_POINT('Ctrl Pts',(-20.3815599326205,-13.1518662655605,
124.197520101744)) ;
#13726 = CARTESIAN_POINT('Ctrl Pts',(-20.3731455648034,-13.1512526701005,
124.207820067248)) ;
#13727 = CARTESIAN_POINT('Ctrl Pts',(-20.3594754546815,-13.1502763347377,
124.224018899634)) ;
#13728 = CARTESIAN_POINT('Ctrl Pts',(-20.3543254046035,-13.149912962448,124.230005584681)) ;
#13729 = CARTESIAN_POINT('Ctrl Pts',(-20.3451672504657,-13.1492744825268,
124.240449658568)) ;
#13730 = CARTESIAN_POINT('Ctrl Pts',(-20.3411831712019,-13.1489992156631,
124.244927764828)) ;
#13731 = CARTESIAN_POINT('Ctrl Pts',(-20.3331605812835,-13.1484498174186,
124.253815600412)) ;
#13732 = CARTESIAN_POINT('Ctrl Pts',(-20.3291223287344,-13.1481756919887,
124.258225353916)) ;
#13733 = CARTESIAN_POINT('Ctrl Pts',(-20.3209595124054,-13.1476263432251,
124.267011696828)) ;
#13734 = CARTESIAN_POINT('Ctrl Pts',(-20.3168346933931,-13.1473511297979,
124.271387836283)) ;
#13735 = CARTESIAN_POINT('Ctrl Pts',(-20.3049913677881,-13.1465675658135,
124.283772475927)) ;
#13736 = CARTESIAN_POINT('Ctrl Pts',(-20.2971973189354,-13.1460598190212,
124.291707971596)) ;
#13737 = CARTESIAN_POINT('Ctrl Pts',(-20.2580438929012,-13.1435464495336,
124.330521878437)) ;
#13738 = CARTESIAN_POINT('Ctrl Pts',(-20.2251749613224,-13.1415542245009,
124.359833128599)) ;
#13739 = CARTESIAN_POINT('Ctrl Pts',(-20.1803738382925,-13.1389463361932,
124.395725837094)) ;
#13740 = CARTESIAN_POINT('Ctrl Pts',(-20.1697850111937,-13.1383370517942,
124.403933200245)) ;
#13741 = CARTESIAN_POINT('Ctrl Pts',(-20.1493832669874,-13.1371747867644,
124.419227945175)) ;
#13742 = CARTESIAN_POINT('Ctrl Pts',(-20.1395953499515,-13.1366222814638,
124.426346083255)) ;
#13743 = CARTESIAN_POINT('Ctrl Pts',(-20.1265156477306,-13.1358907642432,
124.435570746782)) ;
#13744 = CARTESIAN_POINT('Ctrl Pts',(-20.1233151274146,-13.1357122956839,
124.437805588207)) ;
#13745 = CARTESIAN_POINT('Ctrl Pts',(-20.1013867319363,-13.1344931300381,
124.452965320774)) ;
#13746 = CARTESIAN_POINT('Ctrl Pts',(-20.0823194569265,-13.1334510254705,
124.465391710472)) ;
#13747 = CARTESIAN_POINT('Ctrl Pts',(-20.0256225069944,-13.1304035066777,
124.500174317462)) ;
#13748 = CARTESIAN_POINT('Ctrl Pts',(-19.9871453231867,-13.128399731876,124.521083377027)) ;
#13749 = CARTESIAN_POINT('Ctrl Pts',(-19.9288247336841,-13.1254399836714,
124.548916102886)) ;
#13750 = CARTESIAN_POINT('Ctrl Pts',(-19.9097764052515,-13.1244847172175,
124.557428058674)) ;
#13751 = CARTESIAN_POINT('Ctrl Pts',(-19.8767869505092,-13.1228462004059,
124.571189861526)) ;
#13752 = CARTESIAN_POINT('Ctrl Pts',(-19.8629486302767,-13.1221635391203,
124.576674561629)) ;
#13753 = CARTESIAN_POINT('Ctrl Pts',(-19.8388027008165,-13.1209788264789,
124.585749039904)) ;
#13754 = CARTESIAN_POINT('Ctrl Pts',(-19.828539909192,-13.1204772644073,124.589453383613)) ;
#13755 = CARTESIAN_POINT('Ctrl Pts',(-19.8038969018518,-13.1192766497714,
124.597985279752)) ;
#13756 = CARTESIAN_POINT('Ctrl Pts',(-19.789474816449,-13.1185769195871,124.602686339933)) ;
#13757 = CARTESIAN_POINT('Ctrl Pts',(-19.7552307062143,-13.1169201861169,
124.613163141805)) ;
#13758 = CARTESIAN_POINT('Ctrl Pts',(-19.7353441433544,-13.1159624063868,
124.618712560235)) ;
#13759 = CARTESIAN_POINT('Ctrl Pts',(-19.6919784186862,-13.1138875783725,
124.629663804484)) ;
#13760 = CARTESIAN_POINT('Ctrl Pts',(-19.6684618344387,-13.1127710659302,
124.634884602325)) ;
#13761 = CARTESIAN_POINT('Ctrl Pts',(-19.6344197839601,-13.1111691733207,
124.641416128066)) ;
#13762 = CARTESIAN_POINT('Ctrl Pts',(-19.6240056038621,-13.1106810061279,
124.643277517649)) ;
#13763 = CARTESIAN_POINT('Ctrl Pts',(-19.6072053451249,-13.10989650755,124.646060732617)) ;
#13764 = CARTESIAN_POINT('Ctrl Pts',(-19.6008335936111,-13.1095996685999,
124.647065699069)) ;
#13765 = CARTESIAN_POINT('Ctrl Pts',(-19.5895980975686,-13.1090774373909,
124.64874876092)) ;
#13766 = CARTESIAN_POINT('Ctrl Pts',(-19.5847376076761,-13.1088519115615,
124.649447598103)) ;
#13767 = CARTESIAN_POINT('Ctrl Pts',(-19.5750788573241,-13.1084045034829,
124.650778282738)) ;
#13768 = CARTESIAN_POINT('Ctrl Pts',(-19.5702807933502,-13.1081826194189,
124.651410940409)) ;
#13769 = CARTESIAN_POINT('Ctrl Pts',(-19.5600063967649,-13.1077082457941,
124.652705030246)) ;
#13770 = CARTESIAN_POINT('Ctrl Pts',(-19.5545291121831,-13.1074558186349,
124.653358109896)) ;
#13771 = CARTESIAN_POINT('Ctrl Pts',(-19.5398903818906,-13.1067823384053,
124.655005348596)) ;
#13772 = CARTESIAN_POINT('Ctrl Pts',(-19.5307219475339,-13.1063617454783,
124.655934492005)) ;
#13773 = CARTESIAN_POINT('Ctrl Pts',(-19.4825436801578,-13.1041571812783,
124.66027930177)) ;
#13774 = CARTESIAN_POINT('Ctrl Pts',(-19.443399469158,-13.1023862276664,124.661961864056)) ;
#13775 = CARTESIAN_POINT('Ctrl Pts',(-19.3809520941096,-13.0995603406129,
124.661710497427)) ;
#13776 = CARTESIAN_POINT('Ctrl Pts',(-19.3576708227804,-13.0985059328195,
124.6609659417)) ;
#13777 = CARTESIAN_POINT('Ctrl Pts',(-19.317738254551,-13.0966872479062,124.658570534926)) ;
#13778 = CARTESIAN_POINT('Ctrl Pts',(-19.3010744125512,-13.0959257543479,
124.657235034425)) ;
#13779 = CARTESIAN_POINT('Ctrl Pts',(-19.2699653508192,-13.0944991984778,
124.654112756357)) ;
#13780 = CARTESIAN_POINT('Ctrl Pts',(-19.2555147613564,-13.0938345314503,
124.65240710177)) ;
#13781 = CARTESIAN_POINT('Ctrl Pts',(-19.2389782275323,-13.0930714487792,
124.650161863816)) ;
#13782 = CARTESIAN_POINT('Ctrl Pts',(-19.2368599137098,-13.092973651853,124.649868712862)) ;
#13783 = CARTESIAN_POINT('Ctrl Pts',(-19.2141324810124,-13.0919238780786,
124.646664028981)) ;
#13784 = CARTESIAN_POINT('Ctrl Pts',(-19.1935984356369,-13.0909709543967,
124.643243626117)) ;
#13785 = CARTESIAN_POINT('Ctrl Pts',(-19.144258780188,-13.0886686890323,124.633752998499)) ;
#13786 = CARTESIAN_POINT('Ctrl Pts',(-19.1155635138413,-13.0873193296974,
124.627174943626)) ;
#13787 = CARTESIAN_POINT('Ctrl Pts',(-19.0594368525581,-13.0846530206157,
124.612204517602)) ;
#13788 = CARTESIAN_POINT('Ctrl Pts',(-19.0320086602249,-13.0833369254941,
124.603868684193)) ;
#13789 = CARTESIAN_POINT('Ctrl Pts',(-18.953680150316,-13.0795281393135,124.577089007611)) ;
#13790 = CARTESIAN_POINT('Ctrl Pts',(-18.9036603400733,-13.0770249750502,
124.556273038884)) ;
#13791 = CARTESIAN_POINT('Ctrl Pts',(-18.8412132313845,-13.0738048888424,
124.525389976062)) ;
#13792 = CARTESIAN_POINT('Ctrl Pts',(-18.8274081499145,-13.0730872103483,
124.518239176167)) ;
#13793 = CARTESIAN_POINT('Ctrl Pts',(-18.8060922881046,-13.071970005057,124.506688611288)) ;
#13794 = CARTESIAN_POINT('Ctrl Pts',(-18.7984880245361,-13.0715696063642,
124.502464772995)) ;
#13795 = CARTESIAN_POINT('Ctrl Pts',(-18.7854343560365,-13.0708790061069,
124.495034687726)) ;
#13796 = CARTESIAN_POINT('Ctrl Pts',(-18.7799640546951,-13.0705885959289,
124.491865836585)) ;
#13797 = CARTESIAN_POINT('Ctrl Pts',(-18.7693926914893,-13.0700253691977,
124.485634446979)) ;
#13798 = CARTESIAN_POINT('Ctrl Pts',(-18.7642889911474,-13.0697525308087,
124.482576716805)) ;
#13799 = CARTESIAN_POINT('Ctrl Pts',(-18.7541541620249,-13.0692088333995,
124.47640598287)) ;
#13800 = CARTESIAN_POINT('Ctrl Pts',(-18.7491229150831,-13.068937978748,124.473293464187)) ;
#13801 = CARTESIAN_POINT('Ctrl Pts',(-18.7370780491303,-13.0682871807584,
124.465723296967)) ;
#13802 = CARTESIAN_POINT('Ctrl Pts',(-18.7300864096677,-13.067907463319,124.46123119146)) ;
#13803 = CARTESIAN_POINT('Ctrl Pts',(-18.694373230457,-13.0659571651033,124.437779178113)) ;
#13804 = CARTESIAN_POINT('Ctrl Pts',(-18.6663987396338,-13.064394117346,124.417708678766)) ;
#13805 = CARTESIAN_POINT('Ctrl Pts',(-18.6266587834868,-13.0621010006204,
124.386633943294)) ;
#13806 = CARTESIAN_POINT('Ctrl Pts',(-18.6142207163909,-13.0613720753055,
124.37651644575)) ;
#13807 = CARTESIAN_POINT('Ctrl Pts',(-18.5967015051739,-13.0603263955924,
124.361696791309)) ;
#13808 = CARTESIAN_POINT('Ctrl Pts',(-18.5914594271576,-13.0600109980012,
124.357187320837)) ;
#13809 = CARTESIAN_POINT('Ctrl Pts',(-18.5830978895291,-13.0595035800914,
124.349872757504)) ;
#13810 = CARTESIAN_POINT('Ctrl Pts',(-18.5799546578483,-13.0593118338709,
124.347095046369)) ;
#13811 = CARTESIAN_POINT('Ctrl Pts',(-18.5768123715238,-13.0591190969748,
124.344289875357)) ;
#13812 = CARTESIAN_POINT('Ctrl Pts',(-18.5767992702655,-13.0591182933709,
124.344278179151)) ;
#13813 = CARTESIAN_POINT('Ctrl Pts',(-18.5767732091918,-13.0591166948023,
124.344254912025)) ;
#13814 = CARTESIAN_POINT('Ctrl Pts',(-18.5767602506733,-13.0591158999176,
124.344243342274)) ;
#13815 = CARTESIAN_POINT('Ctrl Pts',(-18.5767344749876,-13.0591143187829,
124.344220328009)) ;
#13816 = CARTESIAN_POINT('Ctrl Pts',(-18.5767216563103,-13.0591135324407,
124.344208882157)) ;
#13817 = CARTESIAN_POINT('Ctrl Pts',(-18.5766961578895,-13.0591119682439,
124.344186113563)) ;
#13818 = CARTESIAN_POINT('Ctrl Pts',(-18.5766834791831,-13.0591111904534,
124.344174791756)) ;
#13819 = CARTESIAN_POINT('Ctrl Pts',(-18.576658259452,-13.0591096432842,124.344152270166)) ;
#13820 = CARTESIAN_POINT('Ctrl Pts',(-18.576645717573,-13.0591088738536,124.344141069629)) ;
#13821 = CARTESIAN_POINT('Ctrl Pts',(-18.5766207697322,-13.0591073432972,
124.344118789032)) ;
#13822 = CARTESIAN_POINT('Ctrl Pts',(-18.5766083640755,-13.0591065821904,
124.344107709253)) ;
#13823 = CARTESIAN_POINT('Ctrl Pts',(-18.5765836873645,-13.0591050682022,
124.344085669027)) ;
#13824 = CARTESIAN_POINT('Ctrl Pts',(-18.5765714155829,-13.0591043152765,
124.34407470794)) ;
#13825 = CARTESIAN_POINT('Ctrl Pts',(-18.5765470045118,-13.0591028175217,
124.344052903239)) ;
#13826 = CARTESIAN_POINT('Ctrl Pts',(-18.5765348657958,-13.0591020727283,
124.344042060148)) ;
#13827 = CARTESIAN_POINT('Ctrl Pts',(-18.5765107189499,-13.0591005911224,
124.344020489765)) ;
#13828 = CARTESIAN_POINT('Ctrl Pts',(-18.5764987112384,-13.0590998543358,
124.344009762857)) ;
#13829 = CARTESIAN_POINT('Ctrl Pts',(-18.5764748252108,-13.0590983886716,
124.343988423804)) ;
#13830 = CARTESIAN_POINT('Ctrl Pts',(-18.5764629468541,-13.0590976597918,
124.343977811631)) ;
#13831 = CARTESIAN_POINT('Ctrl Pts',(-18.5764393187023,-13.0590962098908,
124.343956701333)) ;
#13832 = CARTESIAN_POINT('Ctrl Pts',(-18.5764275680372,-13.0590954888165,
124.343946202437)) ;
#13833 = CARTESIAN_POINT('Ctrl Pts',(-18.5764041926353,-13.0590940543661,
124.343925316365)) ;
#13834 = CARTESIAN_POINT('Ctrl Pts',(-18.576392569134,-13.059093341066,124.343914930301)) ;
#13835 = CARTESIAN_POINT('Ctrl Pts',(-18.5763694473039,-13.0590919221184,
124.343894269241)) ;
#13836 = CARTESIAN_POINT('Ctrl Pts',(-18.5763579480308,-13.0590912164133,
124.34388399341)) ;
#13837 = CARTESIAN_POINT('Ctrl Pts',(-18.5763350733448,-13.059089812576,124.343863551669)) ;
#13838 = CARTESIAN_POINT('Ctrl Pts',(-18.576323697843,-13.0590891144387,124.343853385688)) ;
#13839 = CARTESIAN_POINT('Ctrl Pts',(-18.5763010687545,-13.0590877256186,
124.343833161932)) ;
#13840 = CARTESIAN_POINT('Ctrl Pts',(-18.576289815373,-13.0590870349487,124.343823104349)) ;
#13841 = CARTESIAN_POINT('Ctrl Pts',(-18.5762674290795,-13.0590856609755,
124.343803096123)) ;
#13842 = CARTESIAN_POINT('Ctrl Pts',(-18.5762562962323,-13.0590849776765,
124.343793145545)) ;
#13843 = CARTESIAN_POINT('Ctrl Pts',(-18.5762341500843,-13.0590836183894,
124.343773350525)) ;
#13844 = CARTESIAN_POINT('Ctrl Pts',(-18.5762231361601,-13.0590829423633,
124.343763505535)) ;
#13845 = CARTESIAN_POINT('Ctrl Pts',(-18.5762012266255,-13.0590815975472,
124.343743920612)) ;
#13846 = CARTESIAN_POINT('Ctrl Pts',(-18.5761903304785,-13.0590809287245,
124.343734180207)) ;
#13847 = CARTESIAN_POINT('Ctrl Pts',(-18.5761686531521,-13.0590795981106,
124.343714801487)) ;
#13848 = CARTESIAN_POINT('Ctrl Pts',(-18.5761578743407,-13.059078936465,124.343705165295)) ;
#13849 = CARTESIAN_POINT('Ctrl Pts',(-18.5761364315411,-13.0590776201972,
124.343685994895)) ;
#13850 = CARTESIAN_POINT('Ctrl Pts',(-18.5761257665994,-13.0590769655168,
124.34367645984)) ;
#13851 = CARTESIAN_POINT('Ctrl Pts',(-18.5761045512553,-13.0590756631627,
124.343657491479)) ;
#13852 = CARTESIAN_POINT('Ctrl Pts',(-18.5760939999669,-13.0590750154349,
124.343648057388)) ;
#13853 = CARTESIAN_POINT('Ctrl Pts',(-18.5760730092267,-13.059073726821,124.34362928856)) ;
#13854 = CARTESIAN_POINT('Ctrl Pts',(-18.5760625709037,-13.0590730860044,
124.343619954839)) ;
#13855 = CARTESIAN_POINT('Ctrl Pts',(-18.5760418048441,-13.0590718111368,
124.343601385653)) ;
#13856 = CARTESIAN_POINT('Ctrl Pts',(-18.5760314771134,-13.0590711770864,
124.343592150199)) ;
#13857 = CARTESIAN_POINT('Ctrl Pts',(-18.576010931704,-13.0590699157193,124.343573777091)) ;
#13858 = CARTESIAN_POINT('Ctrl Pts',(-18.5760007134305,-13.0590692883663,
124.34356463891)) ;
#13859 = CARTESIAN_POINT('Ctrl Pts',(-18.5759803855166,-13.0590680403073,
124.343546459097)) ;
#13860 = CARTESIAN_POINT('Ctrl Pts',(-18.5759702757845,-13.059067419596,124.343537417389)) ;
#13861 = CARTESIAN_POINT('Ctrl Pts',(-18.5759501627788,-13.0590661846879,
124.343519428596)) ;
#13862 = CARTESIAN_POINT('Ctrl Pts',(-18.5759401605112,-13.0590655705529,
124.343510482417)) ;
#13863 = CARTESIAN_POINT('Ctrl Pts',(-18.5759202621729,-13.0590643487821,
124.343492684466)) ;
#13864 = CARTESIAN_POINT('Ctrl Pts',(-18.5759103650519,-13.0590637410819,
124.343483831761)) ;
#13865 = CARTESIAN_POINT('Ctrl Pts',(-18.5758906753213,-13.0590625320777,
124.343466219268)) ;
#13866 = CARTESIAN_POINT('Ctrl Pts',(-18.5758808833601,-13.0590619308138,
124.343457460067)) ;
#13867 = CARTESIAN_POINT('Ctrl Pts',(-18.5758614032091,-13.0590607346372,
124.343440033938)) ;
#13868 = CARTESIAN_POINT('Ctrl Pts',(-18.5758517140855,-13.0590601396675,
124.343431366181)) ;
#13869 = CARTESIAN_POINT('Ctrl Pts',(-18.5758324379853,-13.0590589559804,
124.343414121504)) ;
#13870 = CARTESIAN_POINT('Ctrl Pts',(-18.5758228514831,-13.0590583672923,
124.343405545015)) ;
#13871 = CARTESIAN_POINT('Ctrl Pts',(-18.5758037792065,-13.059057196082,124.343388481622)) ;
#13872 = CARTESIAN_POINT('Ctrl Pts',(-18.5757942935344,-13.0590566135662,
124.343379994815)) ;
#13873 = CARTESIAN_POINT('Ctrl Pts',(-18.5757754224789,-13.059055454674,124.343363110411)) ;
#13874 = CARTESIAN_POINT('Ctrl Pts',(-18.5757660362585,-13.0590548782464,
124.34335471207)) ;
#13875 = CARTESIAN_POINT('Ctrl Pts',(-18.5757473631504,-13.0590537314726,
124.343338003758)) ;
#13876 = CARTESIAN_POINT('Ctrl Pts',(-18.5757380755909,-13.0590531610852,
124.343329693191)) ;
#13877 = CARTESIAN_POINT('Ctrl Pts',(-18.575719596903,-13.0590520262143,124.343313157847)) ;
#13878 = CARTESIAN_POINT('Ctrl Pts',(-18.5757104076385,-13.0590514618454,
124.343304934742)) ;
#13879 = CARTESIAN_POINT('Ctrl Pts',(-18.5756921253583,-13.0590503390006,
124.343288574176)) ;
#13880 = CARTESIAN_POINT('Ctrl Pts',(-18.5756830314898,-13.0590497804725,
124.343280435955)) ;
#13881 = CARTESIAN_POINT('Ctrl Pts',(-18.575664938979,-13.0590486692473,124.343264244256)) ;
#13882 = CARTESIAN_POINT('Ctrl Pts',(-18.575655940697,-13.0590481165724,124.343256191106)) ;
#13883 = CARTESIAN_POINT('Ctrl Pts',(-18.5756380379289,-13.0590470169662,
124.343240168281)) ;
#13884 = CARTESIAN_POINT('Ctrl Pts',(-18.5756291336696,-13.059046470049,124.343232198814)) ;
#13885 = CARTESIAN_POINT('Ctrl Pts',(-18.5756114182638,-13.0590453819167,
124.343216342762)) ;
#13886 = CARTESIAN_POINT('Ctrl Pts',(-18.5756026067899,-13.0590448406817,
124.343208455888)) ;
#13887 = CARTESIAN_POINT('Ctrl Pts',(-18.5755850758316,-13.0590437638453,
124.343192764027)) ;
#13888 = CARTESIAN_POINT('Ctrl Pts',(-18.575576356355,-13.0590432282446,124.343184959053)) ;
#13889 = CARTESIAN_POINT('Ctrl Pts',(-18.5755590078182,-13.0590421625808,
124.3431694296)) ;
#13890 = CARTESIAN_POINT('Ctrl Pts',(-18.5755503793518,-13.0590416325543,
124.343161705657)) ;
#13891 = CARTESIAN_POINT('Ctrl Pts',(-18.5755332122344,-13.0590405780024,
124.343146337741)) ;
#13892 = CARTESIAN_POINT('Ctrl Pts',(-18.5755246731923,-13.0590400534532,
124.343138693422)) ;
#13893 = CARTESIAN_POINT('Ctrl Pts',(-18.5755076844,-13.0590390098243,124.3431234843)) ;
#13894 = CARTESIAN_POINT('Ctrl Pts',(-18.5754992339722,-13.0590384907031,
124.343115918894)) ;
#13895 = CARTESIAN_POINT('Ctrl Pts',(-18.5754824207663,-13.0590374578298,
124.34310086614)) ;
#13896 = CARTESIAN_POINT('Ctrl Pts',(-18.5754740583669,-13.0590369441011,
124.343093379135)) ;
#13897 = CARTESIAN_POINT('Ctrl Pts',(-18.5754574204807,-13.059035921968,124.343078482537)) ;
#13898 = CARTESIAN_POINT('Ctrl Pts',(-18.5754491444293,-13.059035413529,124.343071072441)) ;
#13899 = CARTESIAN_POINT('Ctrl Pts',(-18.575432677479,-13.0590344018677,124.343056328097)) ;
#13900 = CARTESIAN_POINT('Ctrl Pts',(-18.5754244876065,-13.0590338987086,
124.343048994772)) ;
#13901 = CARTESIAN_POINT('Ctrl Pts',(-18.5754081929116,-13.0590328976011,
124.34303440389)) ;
#13902 = CARTESIAN_POINT('Ctrl Pts',(-18.5754000869874,-13.0590323995852,
124.34302714535)) ;
#13903 = CARTESIAN_POINT('Ctrl Pts',(-18.5753839586784,-13.0590314086717,
124.343012702696)) ;
#13904 = CARTESIAN_POINT('Ctrl Pts',(-18.5753759370461,-13.0590309158206,
124.343005519261)) ;
#13905 = CARTESIAN_POINT('Ctrl Pts',(-18.5753599752291,-13.0590299351086,
124.342991224955)) ;
#13906 = CARTESIAN_POINT('Ctrl Pts',(-18.5753520365623,-13.0590294473412,
124.342984115449)) ;
#13907 = CARTESIAN_POINT('Ctrl Pts',(-18.5753362416015,-13.0590284768539,
124.34296996984)) ;
#13908 = CARTESIAN_POINT('Ctrl Pts',(-18.5753283835982,-13.0590279940291,
124.342962932211)) ;
#13909 = CARTESIAN_POINT('Ctrl Pts',(-18.5753127493683,-13.059027033391,124.342948929836)) ;
#13910 = CARTESIAN_POINT('Ctrl Pts',(-18.5753049725399,-13.0590265555408,
124.342941964555)) ;
#13911 = CARTESIAN_POINT('Ctrl Pts',(-18.5752894984523,-13.0590256047165,
124.342928104908)) ;
#13912 = CARTESIAN_POINT('Ctrl Pts',(-18.5752818019414,-13.0590251317886,
124.342921211217)) ;
#13913 = CARTESIAN_POINT('Ctrl Pts',(-18.5752664864524,-13.059024190684,124.342907492938)) ;
#13914 = CARTESIAN_POINT('Ctrl Pts',(-18.5752588692233,-13.0590237226151,
124.34290066992)) ;
#13915 = CARTESIAN_POINT('Ctrl Pts',(-18.5752437133664,-13.0590227912946,
124.342887093954)) ;
#13916 = CARTESIAN_POINT('Ctrl Pts',(-18.5752361730028,-13.0590223279366,
124.342880339456)) ;
#13917 = CARTESIAN_POINT('Ctrl Pts',(-18.5752211686278,-13.0590214059001,
124.342866898524)) ;
#13918 = CARTESIAN_POINT('Ctrl Pts',(-18.5752137066611,-13.0590209473474,
124.342860213927)) ;
#13919 = CARTESIAN_POINT('Ctrl Pts',(-18.5751988595061,-13.0590200349483,
124.34284691319)) ;
#13920 = CARTESIAN_POINT('Ctrl Pts',(-18.5751914724873,-13.0590195809894,
124.342840295414)) ;
#13921 = CARTESIAN_POINT('Ctrl Pts',(-18.5751743963632,-13.0590185315866,
124.342824997135)) ;
#13922 = CARTESIAN_POINT('Ctrl Pts',(-18.5751647058763,-13.0590179360534,
124.342816315281)) ;
#13923 = CARTESIAN_POINT('Ctrl Pts',(-18.5727867012847,-13.0588717922316,
124.340685757895)) ;
#13924 = CARTESIAN_POINT('Ctrl Pts',(-18.570426495529,-13.058726134459,124.338554856162)) ;
#13925 = CARTESIAN_POINT('Ctrl Pts',(-18.5653873125959,-13.0584138015554,
124.333970228496)) ;
#13926 = CARTESIAN_POINT('Ctrl Pts',(-18.5627108508765,-13.0582470915148,
124.33151378418)) ;
#13927 = CARTESIAN_POINT('Ctrl Pts',(-18.5555039436618,-13.0577960020574,
124.324841202711)) ;
#13928 = CARTESIAN_POINT('Ctrl Pts',(-18.5509940454421,-13.0575113625089,
124.320603037122)) ;
#13929 = CARTESIAN_POINT('Ctrl Pts',(-18.5316298472319,-13.0562792074135,
124.302132867345)) ;
#13930 = CARTESIAN_POINT('Ctrl Pts',(-18.5170967093551,-13.0553288007821,
124.287568908927)) ;
#13931 = CARTESIAN_POINT('Ctrl Pts',(-18.4898906137748,-13.0535026066794,
124.258924699829)) ;
#13932 = CARTESIAN_POINT('Ctrl Pts',(-18.4771651237092,-13.0526271265878,
124.244901887226)) ;
#13933 = CARTESIAN_POINT('Ctrl Pts',(-18.4556659984273,-13.0511114655823,
124.220101459081)) ;
#13934 = CARTESIAN_POINT('Ctrl Pts',(-18.4467444256926,-13.0504708434954,
124.209456577654)) ;
#13935 = CARTESIAN_POINT('Ctrl Pts',(-18.4328952238659,-13.0494576288438,
124.192361448839)) ;
#13936 = CARTESIAN_POINT('Ctrl Pts',(-18.4278498610943,-13.0490843801677,
124.186008102062)) ;
#13937 = CARTESIAN_POINT('Ctrl Pts',(-18.419089738285,-13.0484289370592,124.174753703802)) ;
#13938 = CARTESIAN_POINT('Ctrl Pts',(-18.415348631302,-13.0481465799679,124.169873519523)) ;
#13939 = CARTESIAN_POINT('Ctrl Pts',(-18.4079182472009,-13.0475807947028,
124.160031193206)) ;
#13940 = CARTESIAN_POINT('Ctrl Pts',(-18.4042294733846,-13.047297377047,124.155068882968)) ;
#13941 = CARTESIAN_POINT('Ctrl Pts',(-18.3963653755716,-13.0466875849945,
124.144324133538)) ;
#13942 = CARTESIAN_POINT('Ctrl Pts',(-18.3922024130721,-13.0463613052809,
124.138532910668)) ;
#13943 = CARTESIAN_POINT('Ctrl Pts',(-18.3808185455468,-13.0454591844857,
124.122407038763)) ;
#13944 = CARTESIAN_POINT('Ctrl Pts',(-18.3737040640521,-13.0448841010443,
124.111998272898)) ;
#13945 = CARTESIAN_POINT('Ctrl Pts',(-18.3359168734013,-13.0417647713829,
124.054878062883)) ;
#13946 = CARTESIAN_POINT('Ctrl Pts',(-18.308245391511,-13.0392411246978,124.006257445023)) ;
#13947 = CARTESIAN_POINT('Ctrl Pts',(-18.2700598212074,-13.0352529346555,
123.927283913443)) ;
#13948 = CARTESIAN_POINT('Ctrl Pts',(-18.2572999984862,-13.0338033535924,
123.898100013226)) ;
#13949 = CARTESIAN_POINT('Ctrl Pts',(-18.2389457281613,-13.0315116611717,
123.851330589327)) ;
#13950 = CARTESIAN_POINT('Ctrl Pts',(-18.2326021688887,-13.0306716162552,
123.834053866237)) ;
#13951 = CARTESIAN_POINT('Ctrl Pts',(-18.2266423654684,-13.0298305431221,
123.816643453356)) ;
#13952 = CARTESIAN_POINT('Origin',(-19.4092722359532,-13.9601742359176,123.411814366564)) ;
#13953 = CARTESIAN_POINT('',(-18.2266423654694,-12.6697781342469,123.816643453359)) ;
#13954 = CARTESIAN_POINT('',(-18.2266423654683,-12.7298216458232,123.816643453356)) ;
#13955 = CARTESIAN_POINT('',(-18.2266423654683,-13.9601742359176,123.816643453356)) ;
#13956 = CARTESIAN_POINT('',(-20.591901275917,-12.9098928303878,123.006982853621)) ;
#13957 = CARTESIAN_POINT('Ctrl Pts',(-18.2266423654683,-12.7298216458232,
123.816643453356)) ;
#13958 = CARTESIAN_POINT('Ctrl Pts',(-18.2326017142761,-12.7306672894293,
123.834052538174)) ;
#13959 = CARTESIAN_POINT('Ctrl Pts',(-18.2389447360747,-12.7315136846607,
123.851327882605)) ;
#13960 = CARTESIAN_POINT('Ctrl Pts',(-18.2572979468201,-12.7338268239059,
123.898095094483)) ;
#13961 = CARTESIAN_POINT('Ctrl Pts',(-18.2700571991135,-12.735294271902,123.927278037118)) ;
#13962 = CARTESIAN_POINT('Ctrl Pts',(-18.3082398863143,-12.7393454067758,
124.006246855078)) ;
#13963 = CARTESIAN_POINT('Ctrl Pts',(-18.3359088431132,-12.7419370427707,
124.054864332949)) ;
#13964 = CARTESIAN_POINT('Ctrl Pts',(-18.3736951240226,-12.7450944938988,
124.11198511765)) ;
#13965 = CARTESIAN_POINT('Ctrl Pts',(-18.3808116436384,-12.7456749550272,
124.122397118766)) ;
#13966 = CARTESIAN_POINT('Ctrl Pts',(-18.3921980634869,-12.7465821741772,
124.138526830088)) ;
#13967 = CARTESIAN_POINT('Ctrl Pts',(-18.3963614188763,-12.7469095920066,
124.144318669634)) ;
#13968 = CARTESIAN_POINT('Ctrl Pts',(-18.4042261169505,-12.7475202460246,
124.155064347167)) ;
#13969 = CARTESIAN_POINT('Ctrl Pts',(-18.4079150871526,-12.747803554078,124.16002696724)) ;
#13970 = CARTESIAN_POINT('Ctrl Pts',(-18.4153454927312,-12.7483681106648,
124.169869402047)) ;
#13971 = CARTESIAN_POINT('Ctrl Pts',(-18.4190864161334,-12.7486493541137,
124.174749390141)) ;
#13972 = CARTESIAN_POINT('Ctrl Pts',(-18.4278457554633,-12.7493011211007,
124.18600288753)) ;
#13973 = CARTESIAN_POINT('Ctrl Pts',(-18.4328905146027,-12.7496714656466,
124.192355548919)) ;
#13974 = CARTESIAN_POINT('Ctrl Pts',(-18.4467372532608,-12.7506748463988,
124.209447872826)) ;
#13975 = CARTESIAN_POINT('Ctrl Pts',(-18.4556569326463,-12.7513071671426,
124.220090716886)) ;
#13976 = CARTESIAN_POINT('Ctrl Pts',(-18.4771552127671,-12.7528005044379,
124.244890841725)) ;
#13977 = CARTESIAN_POINT('Ctrl Pts',(-18.4898818553188,-12.7536608358596,
124.258915238493)) ;
#13978 = CARTESIAN_POINT('Ctrl Pts',(-18.5170916260033,-12.7554572386405,
124.287563817407)) ;
#13979 = CARTESIAN_POINT('Ctrl Pts',(-18.5316272030638,-12.7563931326534,
124.302130338426)) ;
#13980 = CARTESIAN_POINT('Ctrl Pts',(-18.5509938955987,-12.7576151635076,
124.320602896252)) ;
#13981 = CARTESIAN_POINT('Ctrl Pts',(-18.5555038384293,-12.7578980523225,
124.324841104505)) ;
#13982 = CARTESIAN_POINT('Ctrl Pts',(-18.5627107845363,-12.7583476484,124.331513723214)) ;
#13983 = CARTESIAN_POINT('Ctrl Pts',(-18.5653872543757,-12.758514085372,124.333970175208)) ;
#13984 = CARTESIAN_POINT('Ctrl Pts',(-18.5704264469513,-12.7588265050528,
124.338554812247)) ;
#13985 = CARTESIAN_POINT('Ctrl Pts',(-18.5727866565771,-12.7589724502519,
124.340685717616)) ;
#13986 = CARTESIAN_POINT('Ctrl Pts',(-18.5751646562309,-12.7591191023728,
124.342816270802)) ;
#13987 = CARTESIAN_POINT('Ctrl Pts',(-18.5751743458909,-12.7591196999312,
124.342824951917)) ;
#13988 = CARTESIAN_POINT('Ctrl Pts',(-18.5751914208737,-12.7591207529287,
124.342840249175)) ;
#13989 = CARTESIAN_POINT('Ctrl Pts',(-18.5751988058895,-12.7591212083516,
124.342846865157)) ;
#13990 = CARTESIAN_POINT('Ctrl Pts',(-18.5752136547505,-12.7591221240511,
124.342860167424)) ;
#13991 = CARTESIAN_POINT('Ctrl Pts',(-18.5752211171675,-12.7591225842395,
124.342866852425)) ;
#13992 = CARTESIAN_POINT('Ctrl Pts',(-18.5752361163824,-12.7591235091955,
124.342880288736)) ;
#13993 = CARTESIAN_POINT('Ctrl Pts',(-18.5752436552404,-12.7591239740899,
124.342887041887)) ;
#13994 = CARTESIAN_POINT('Ctrl Pts',(-18.5752588107679,-12.7591249086693,
124.342900617559)) ;
#13995 = CARTESIAN_POINT('Ctrl Pts',(-18.5752664274573,-12.7591253783553,
124.342907440094)) ;
#13996 = CARTESIAN_POINT('Ctrl Pts',(-18.5752817405074,-12.7591263226322,
124.342921156191)) ;
#13997 = CARTESIAN_POINT('Ctrl Pts',(-18.5752894363132,-12.7591267971888,
124.342928049251)) ;
#13998 = CARTESIAN_POINT('Ctrl Pts',(-18.5753049082886,-12.7591277512493,
124.342941907008)) ;
#13999 = CARTESIAN_POINT('Ctrl Pts',(-18.5753126844561,-12.7591282307529,
124.342948871698)) ;
#14000 = CARTESIAN_POINT('Ctrl Pts',(-18.575328315123,-12.759129194582,124.342962870884)) ;
#14001 = CARTESIAN_POINT('Ctrl Pts',(-18.5753361711164,-12.7591296789994,
124.342969906714)) ;
#14002 = CARTESIAN_POINT('Ctrl Pts',(-18.5753519669284,-12.7591306529945,
124.342984053087)) ;
#14003 = CARTESIAN_POINT('Ctrl Pts',(-18.5753599053588,-12.7591311424864,
124.342991162383)) ;
#14004 = CARTESIAN_POINT('Ctrl Pts',(-18.5753758637796,-12.7591321264906,
124.34300545365)) ;
#14005 = CARTESIAN_POINT('Ctrl Pts',(-18.5753838844763,-12.7591326210463,
124.343012636248)) ;
#14006 = CARTESIAN_POINT('Ctrl Pts',(-18.5754000099134,-12.7591336153308,
124.343027076332)) ;
#14007 = CARTESIAN_POINT('Ctrl Pts',(-18.5754081140767,-12.7591341150239,
124.343034333297)) ;
#14008 = CARTESIAN_POINT('Ctrl Pts',(-18.5754244091464,-12.7591351197494,
124.343048924517)) ;
#14009 = CARTESIAN_POINT('Ctrl Pts',(-18.5754325988824,-12.7591356247096,
124.343056257722)) ;
#14010 = CARTESIAN_POINT('Ctrl Pts',(-18.5754490614152,-12.7591366397418,
124.343070998112)) ;
#14011 = CARTESIAN_POINT('Ctrl Pts',(-18.5754573358176,-12.7591371499128,
124.343078406733)) ;
#14012 = CARTESIAN_POINT('Ctrl Pts',(-18.5754739732433,-12.7591381757093,
124.343093302922)) ;
#14013 = CARTESIAN_POINT('Ctrl Pts',(-18.5754823349523,-12.7591386912537,
124.34310078931)) ;
#14014 = CARTESIAN_POINT('Ctrl Pts',(-18.5754991450576,-12.7591397276773,
124.343115839291)) ;
#14015 = CARTESIAN_POINT('Ctrl Pts',(-18.575507594108,-12.7591402485969,124.343123403465)) ;
#14016 = CARTESIAN_POINT('Ctrl Pts',(-18.5755245814094,-12.7591412959255,
124.343138611256)) ;
#14017 = CARTESIAN_POINT('Ctrl Pts',(-18.5755331193561,-12.7591418223158,
124.343146254595)) ;
#14018 = CARTESIAN_POINT('Ctrl Pts',(-18.5755502845499,-12.7591428805918,
124.343161620792)) ;
#14019 = CARTESIAN_POINT('Ctrl Pts',(-18.5755589120634,-12.7591434124938,
124.343169343884)) ;
#14020 = CARTESIAN_POINT('Ctrl Pts',(-18.5755762580752,-12.7591444818969,
124.34318487108)) ;
#14021 = CARTESIAN_POINT('Ctrl Pts',(-18.5755849763239,-12.7591450193824,
124.343192674957)) ;
#14022 = CARTESIAN_POINT('Ctrl Pts',(-18.5756025056162,-12.7591461000636,
124.343208365329)) ;
#14023 = CARTESIAN_POINT('Ctrl Pts',(-18.5756113162067,-12.7591466432313,
124.343216251415)) ;
#14024 = CARTESIAN_POINT('Ctrl Pts',(-18.5756290289732,-12.759147735202,124.343232105108)) ;
#14025 = CARTESIAN_POINT('Ctrl Pts',(-18.575637932094,-12.7591482840631,124.343240073557)) ;
#14026 = CARTESIAN_POINT('Ctrl Pts',(-18.5756558327912,-12.7591493875973,
124.343256094533)) ;
#14027 = CARTESIAN_POINT('Ctrl Pts',(-18.5756648300303,-12.7591499422495,
124.343264146752)) ;
#14028 = CARTESIAN_POINT('Ctrl Pts',(-18.5756829202618,-12.7591510574454,
124.343280336415)) ;
#14029 = CARTESIAN_POINT('Ctrl Pts',(-18.575692013104,-12.7591516179798,124.343288473719)) ;
#14030 = CARTESIAN_POINT('Ctrl Pts',(-18.5757102936334,-12.7591527448837,
124.343304832723)) ;
#14031 = CARTESIAN_POINT('Ctrl Pts',(-18.5757194824738,-12.7591533113242,
124.343313055449)) ;
#14032 = CARTESIAN_POINT('Ctrl Pts',(-18.575737956618,-12.7591544501399,124.343329586732)) ;
#14033 = CARTESIAN_POINT('Ctrl Pts',(-18.5757472421849,-12.7591550225311,
124.343337895518)) ;
#14034 = CARTESIAN_POINT('Ctrl Pts',(-18.5757659147772,-12.7591561735558,
124.343354603373)) ;
#14035 = CARTESIAN_POINT('Ctrl Pts',(-18.5757752999546,-12.7591567520751,
124.343363000783)) ;
#14036 = CARTESIAN_POINT('Ctrl Pts',(-18.5757941681839,-12.7591579151347,
124.343379882663)) ;
#14037 = CARTESIAN_POINT('Ctrl Pts',(-18.5758036524342,-12.7591584997486,
124.3433883682)) ;
#14038 = CARTESIAN_POINT('Ctrl Pts',(-18.5758227231047,-12.7591596752617,
124.343405430161)) ;
#14039 = CARTESIAN_POINT('Ctrl Pts',(-18.5758323086862,-12.759160266109,124.343414005829)) ;
#14040 = CARTESIAN_POINT('Ctrl Pts',(-18.5758515817138,-12.7591614540696,
124.343431247762)) ;
#14041 = CARTESIAN_POINT('Ctrl Pts',(-18.5758612694762,-12.7591620512023,
124.343439914304)) ;
#14042 = CARTESIAN_POINT('Ctrl Pts',(-18.575880747629,-12.7591632517802,124.34345733865)) ;
#14043 = CARTESIAN_POINT('Ctrl Pts',(-18.5758905384708,-12.7591638552532,
124.343466096853)) ;
#14044 = CARTESIAN_POINT('Ctrl Pts',(-18.5759102256245,-12.7591650686865,
124.343483707046)) ;
#14045 = CARTESIAN_POINT('Ctrl Pts',(-18.5759201215757,-12.7591656786245,
124.343492558707)) ;
#14046 = CARTESIAN_POINT('Ctrl Pts',(-18.5759400175723,-12.7591669049027,
124.343510354569)) ;
#14047 = CARTESIAN_POINT('Ctrl Pts',(-18.5759500188267,-12.7591675213172,
124.343519299845)) ;
#14048 = CARTESIAN_POINT('Ctrl Pts',(-18.5759701283546,-12.7591687607282,
124.343537285533)) ;
#14049 = CARTESIAN_POINT('Ctrl Pts',(-18.5759802362928,-12.7591693837039,
124.343546325639)) ;
#14050 = CARTESIAN_POINT('Ctrl Pts',(-18.5760005631137,-12.7591706364788,
124.34356450448)) ;
#14051 = CARTESIAN_POINT('Ctrl Pts',(-18.5760107804656,-12.7591712661834,
124.34357364184)) ;
#14052 = CARTESIAN_POINT('Ctrl Pts',(-18.5760313226115,-12.7591725321999,
124.343592012036)) ;
#14053 = CARTESIAN_POINT('Ctrl Pts',(-18.5760416490364,-12.759173168612,124.343601246325)) ;
#14054 = CARTESIAN_POINT('Ctrl Pts',(-18.5760624126772,-12.7591744482494,
124.343619813355)) ;
#14055 = CARTESIAN_POINT('Ctrl Pts',(-18.5760728498013,-12.7591750914688,
124.343629146007)) ;
#14056 = CARTESIAN_POINT('Ctrl Pts',(-18.5760938371435,-12.7591763848621,
124.343647911803)) ;
#14057 = CARTESIAN_POINT('Ctrl Pts',(-18.5761043865159,-12.7591770349838,
124.343657344184)) ;
#14058 = CARTESIAN_POINT('Ctrl Pts',(-18.5761256008144,-12.7591783423326,
124.343676311617)) ;
#14059 = CARTESIAN_POINT('Ctrl Pts',(-18.5761362648107,-12.7591789995024,
124.34368584583)) ;
#14060 = CARTESIAN_POINT('Ctrl Pts',(-18.5761577046036,-12.7591803207157,
124.34370501355)) ;
#14061 = CARTESIAN_POINT('Ctrl Pts',(-18.5761684824747,-12.759180984887,124.343714648904)) ;
#14062 = CARTESIAN_POINT('Ctrl Pts',(-18.5761901562053,-12.759182320484,124.343734024417)) ;
#14063 = CARTESIAN_POINT('Ctrl Pts',(-18.5762010508702,-12.7591829918361,
124.3437437635)) ;
#14064 = CARTESIAN_POINT('Ctrl Pts',(-18.5762229576896,-12.7591843417635,
124.343763346004)) ;
#14065 = CARTESIAN_POINT('Ctrl Pts',(-18.5762339699876,-12.7591850203475,
124.343773189545)) ;
#14066 = CARTESIAN_POINT('Ctrl Pts',(-18.5762561140326,-12.7591863848592,
124.343792982692)) ;
#14067 = CARTESIAN_POINT('Ctrl Pts',(-18.5762672456259,-12.7591870707771,
124.343802932153)) ;
#14068 = CARTESIAN_POINT('Ctrl Pts',(-18.5762896288272,-12.7591884499908,
124.343822937624)) ;
#14069 = CARTESIAN_POINT('Ctrl Pts',(-18.5763008807322,-12.7591891433047,
124.343832993891)) ;
#14070 = CARTESIAN_POINT('Ctrl Pts',(-18.5763235068996,-12.7591905374541,
124.343853215044)) ;
#14071 = CARTESIAN_POINT('Ctrl Pts',(-18.576334880719,-12.7591912382621,124.343863379527)) ;
#14072 = CARTESIAN_POINT('Ctrl Pts',(-18.5763577530773,-12.7591926475448,
124.343883819196)) ;
#14073 = CARTESIAN_POINT('Ctrl Pts',(-18.5763692508888,-12.7591933559744,
124.343894093725)) ;
#14074 = CARTESIAN_POINT('Ctrl Pts',(-18.5763923704753,-12.759194780453,124.343914752789)) ;
#14075 = CARTESIAN_POINT('Ctrl Pts',(-18.5764039930901,-12.7591954965536,
124.343925138066)) ;
#14076 = CARTESIAN_POINT('Ctrl Pts',(-18.5764273643471,-12.7591969365007,
124.343946020443)) ;
#14077 = CARTESIAN_POINT('Ctrl Pts',(-18.5764391133914,-12.7591976603718,
124.343956517895)) ;
#14078 = CARTESIAN_POINT('Ctrl Pts',(-18.5764627386005,-12.7591991159267,
124.343977625574)) ;
#14079 = CARTESIAN_POINT('Ctrl Pts',(-18.576474615157,-12.7591998476345,124.343988236143)) ;
#14080 = CARTESIAN_POINT('Ctrl Pts',(-18.5764984992101,-12.7592013190973,
124.344009573442)) ;
#14081 = CARTESIAN_POINT('Ctrl Pts',(-18.576510505759,-12.7592020587938,124.344020299317)) ;
#14082 = CARTESIAN_POINT('Ctrl Pts',(-18.5765346490174,-12.7592035461856,
124.344041866505)) ;
#14083 = CARTESIAN_POINT('Ctrl Pts',(-18.5765467862843,-12.759204293915,124.344052708307)) ;
#14084 = CARTESIAN_POINT('Ctrl Pts',(-18.5765711940765,-12.7592057975626,
124.344074510089)) ;
#14085 = CARTESIAN_POINT('Ctrl Pts',(-18.5765834641956,-12.7592065534556,
124.344085469696)) ;
#14086 = CARTESIAN_POINT('Ctrl Pts',(-18.5766081383778,-12.7592080734721,
124.344107507675)) ;
#14087 = CARTESIAN_POINT('Ctrl Pts',(-18.5766205427388,-12.7592088376137,
124.344118586301)) ;
#14088 = CARTESIAN_POINT('Ctrl Pts',(-18.5766454867075,-12.7592103742069,
124.344140863452)) ;
#14089 = CARTESIAN_POINT('Ctrl Pts',(-18.5766580267301,-12.7592111466838,
124.344152062337)) ;
#14090 = CARTESIAN_POINT('Ctrl Pts',(-18.5766832440137,-12.7592127000697,
124.344174581752)) ;
#14091 = CARTESIAN_POINT('Ctrl Pts',(-18.576695921225,-12.7592134809753,124.344185902229)) ;
#14092 = CARTESIAN_POINT('Ctrl Pts',(-18.5767214162173,-12.759215051423,124.344208667774)) ;
#14093 = CARTESIAN_POINT('Ctrl Pts',(-18.5767342331826,-12.7592158409146,
124.344220112103)) ;
#14094 = CARTESIAN_POINT('Ctrl Pts',(-18.5767600061612,-12.7592174284398,
124.344243123963)) ;
#14095 = CARTESIAN_POINT('Ctrl Pts',(-18.5767729633222,-12.7592182265438,
124.344254692508)) ;
#14096 = CARTESIAN_POINT('Ctrl Pts',(-18.5767990208619,-12.7592198315499,
124.344277956491)) ;
#14097 = CARTESIAN_POINT('Ctrl Pts',(-18.5768121206846,-12.7592206384175,
124.344289651422)) ;
#14098 = CARTESIAN_POINT('Ctrl Pts',(-18.5799543720719,-12.7594141786897,
124.347094792777)) ;
#14099 = CARTESIAN_POINT('Ctrl Pts',(-18.583097558938,-12.7596070945764,124.349872466011)) ;
#14100 = CARTESIAN_POINT('Ctrl Pts',(-18.5914589411826,-12.7601184272586,
124.357186899497)) ;
#14101 = CARTESIAN_POINT('Ctrl Pts',(-18.5967008949658,-12.7604370990635,
124.361696267903)) ;
#14102 = CARTESIAN_POINT('Ctrl Pts',(-18.6142194942362,-12.7614955712047,
124.37651542867)) ;
#14103 = CARTESIAN_POINT('Ctrl Pts',(-18.6266570252239,-12.7622365207948,
124.386632519347)) ;
#14104 = CARTESIAN_POINT('Ctrl Pts',(-18.6663971117434,-12.7645688214455,
124.417707511162)) ;
#14105 = CARTESIAN_POINT('Ctrl Pts',(-18.6943727063018,-12.7661594369059,
124.437778868525)) ;
#14106 = CARTESIAN_POINT('Ctrl Pts',(-18.73008714712,-12.7681254681389,124.461231667369)) ;
#14107 = CARTESIAN_POINT('Ctrl Pts',(-18.7370786758153,-12.7685074288161,
124.465723695912)) ;
#14108 = CARTESIAN_POINT('Ctrl Pts',(-18.7491234197455,-12.7691605635696,
124.473293777753)) ;
#14109 = CARTESIAN_POINT('Ctrl Pts',(-18.7541546411038,-12.769431946238,124.47640627762)) ;
#14110 = CARTESIAN_POINT('Ctrl Pts',(-18.7642894294835,-12.7699757842253,
124.482576980619)) ;
#14111 = CARTESIAN_POINT('Ctrl Pts',(-18.7693931148766,-12.7702482299903,
124.485634699285)) ;
#14112 = CARTESIAN_POINT('Ctrl Pts',(-18.7799644880319,-12.7708096955153,
124.491866089112)) ;
#14113 = CARTESIAN_POINT('Ctrl Pts',(-18.7854348161993,-12.77109867739,124.495034953049)) ;
#14114 = CARTESIAN_POINT('Ctrl Pts',(-18.798488578728,-12.7717846908643,124.502465083759)) ;
#14115 = CARTESIAN_POINT('Ctrl Pts',(-18.8060929249016,-12.7721814802344,
124.506688963167)) ;
#14116 = CARTESIAN_POINT('Ctrl Pts',(-18.827409080212,-12.7732862682195,124.518239668095)) ;
#14117 = CARTESIAN_POINT('Ctrl Pts',(-18.8412144235751,-12.7739932454686,
124.525390589664)) ;
#14118 = CARTESIAN_POINT('Ctrl Pts',(-18.9036640460803,-12.7771582774044,
124.556274788094)) ;
#14119 = CARTESIAN_POINT('Ctrl Pts',(-18.9536853187154,-12.7796106807045,
124.577091089033)) ;
#14120 = CARTESIAN_POINT('Ctrl Pts',(-19.0320157727976,-12.7833898013155,
124.603870949393)) ;
#14121 = CARTESIAN_POINT('Ctrl Pts',(-19.0594444436341,-12.7846998776024,
124.612206737053)) ;
#14122 = CARTESIAN_POINT('Ctrl Pts',(-19.1155718308537,-12.7873582674251,
124.627176961971)) ;
#14123 = CARTESIAN_POINT('Ctrl Pts',(-19.1442673790073,-12.7887058255138,
124.633754866544)) ;
#14124 = CARTESIAN_POINT('Ctrl Pts',(-19.1936065288727,-12.7910093160185,
124.643245031454)) ;
#14125 = CARTESIAN_POINT('Ctrl Pts',(-19.2141398095654,-12.7919640533508,
124.646665172238)) ;
#14126 = CARTESIAN_POINT('Ctrl Pts',(-19.236866182519,-12.7930183171429,124.649869585487)) ;
#14127 = CARTESIAN_POINT('Ctrl Pts',(-19.2389842913548,-12.7931165519873,
124.650162697319)) ;
#14128 = CARTESIAN_POINT('Ctrl Pts',(-19.2555154005346,-12.793883076883,124.652407119127)) ;
#14129 = CARTESIAN_POINT('Ctrl Pts',(-19.2699606813584,-12.7945519057057,
124.654112169403)) ;
#14130 = CARTESIAN_POINT('Ctrl Pts',(-19.3010638516899,-12.7959913443683,
124.657234110347)) ;
#14131 = CARTESIAN_POINT('Ctrl Pts',(-19.3177270702512,-12.7967621004021,
124.658569703818)) ;
#14132 = CARTESIAN_POINT('Ctrl Pts',(-19.3576560865813,-12.7986107176195,
124.660965280775)) ;
#14133 = CARTESIAN_POINT('Ctrl Pts',(-19.3809344503295,-12.7996907717898,
124.661710037211)) ;
#14134 = CARTESIAN_POINT('Ctrl Pts',(-19.4433867258348,-12.8025898172644,
124.661962466935)) ;
#14135 = CARTESIAN_POINT('Ctrl Pts',(-19.4825398110413,-12.8044067169687,
124.660279821104)) ;
#14136 = CARTESIAN_POINT('Ctrl Pts',(-19.5307263214418,-12.8066364472764,
124.655934057454)) ;
#14137 = CARTESIAN_POINT('Ctrl Pts',(-19.5398937974138,-12.8070604300559,
124.655004983066)) ;
#14138 = CARTESIAN_POINT('Ctrl Pts',(-19.5545314138148,-12.8077371332337,
124.65335783964)) ;
#14139 = CARTESIAN_POINT('Ctrl Pts',(-19.5600085032303,-12.8079902825689,
124.652704773599)) ;
#14140 = CARTESIAN_POINT('Ctrl Pts',(-19.5702826133265,-12.808465075288,124.651410703569)) ;
#14141 = CARTESIAN_POINT('Ctrl Pts',(-19.5750805807026,-12.8086867715125,
124.650778051794)) ;
#14142 = CARTESIAN_POINT('Ctrl Pts',(-19.5847393217084,-12.8091330395337,
124.649447355378)) ;
#14143 = CARTESIAN_POINT('Ctrl Pts',(-19.5895998988103,-12.8093576018542,
124.648748498749)) ;
#14144 = CARTESIAN_POINT('Ctrl Pts',(-19.6008357490794,-12.8098767241804,
124.647065366126)) ;
#14145 = CARTESIAN_POINT('Ctrl Pts',(-19.6072077785756,-12.8101711394818,
124.646060344001)) ;
#14146 = CARTESIAN_POINT('Ctrl Pts',(-19.6240090187073,-12.8109476139213,
124.643276928103)) ;
#14147 = CARTESIAN_POINT('Ctrl Pts',(-19.6344239393097,-12.8114291270485,
124.64141537431)) ;
#14148 = CARTESIAN_POINT('Ctrl Pts',(-19.6684697379865,-12.8130047941458,
124.63488298679)) ;
#14149 = CARTESIAN_POINT('Ctrl Pts',(-19.6919893947084,-12.8140957545046,
124.629661323584)) ;
#14150 = CARTESIAN_POINT('Ctrl Pts',(-19.7353618648572,-12.816121610241,124.618707835472)) ;
#14151 = CARTESIAN_POINT('Ctrl Pts',(-19.7552517860486,-12.8170562573009,
124.613157130575)) ;
#14152 = CARTESIAN_POINT('Ctrl Pts',(-19.7894947587977,-12.8186826313674,
124.602679916513)) ;
#14153 = CARTESIAN_POINT('Ctrl Pts',(-19.8039124706347,-12.8193731537586,
124.597980039551)) ;
#14154 = CARTESIAN_POINT('Ctrl Pts',(-19.8285507303693,-12.8205631056495,
124.589449529066)) ;
#14155 = CARTESIAN_POINT('Ctrl Pts',(-19.8388132444028,-12.8210617156686,
124.585745179152)) ;
#14156 = CARTESIAN_POINT('Ctrl Pts',(-19.8629615017187,-12.8222418478977,
124.576669585387)) ;
#14157 = CARTESIAN_POINT('Ctrl Pts',(-19.8768023814789,-12.8229236901255,
124.571183674441)) ;
#14158 = CARTESIAN_POINT('Ctrl Pts',(-19.9098018091956,-12.8245623797158,
124.5574171103)) ;
#14159 = CARTESIAN_POINT('Ctrl Pts',(-19.9288574422983,-12.8255193692947,
124.548901307972)) ;
#14160 = CARTESIAN_POINT('Ctrl Pts',(-19.9871965467417,-12.8284840258764,
124.521057219369)) ;
#14161 = CARTESIAN_POINT('Ctrl Pts',(-20.0256844747708,-12.8304891715993,
124.500139763345)) ;
#14162 = CARTESIAN_POINT('Ctrl Pts',(-20.0823781022484,-12.8335386363419,
124.465353929019)) ;
#14163 = CARTESIAN_POINT('Ctrl Pts',(-20.1014324430568,-12.8345812962938,
124.452934609476)) ;
#14164 = CARTESIAN_POINT('Ctrl Pts',(-20.1233438087625,-12.8358049379282,
124.437785606451)) ;
#14165 = CARTESIAN_POINT('Ctrl Pts',(-20.1265398989144,-12.8359840554574,
124.435553735641)) ;
#14166 = CARTESIAN_POINT('Ctrl Pts',(-20.1396143035031,-12.8367194523825,
124.426332428001)) ;
#14167 = CARTESIAN_POINT('Ctrl Pts',(-20.1494012861676,-12.8372762312192,
124.419214694118)) ;
#14168 = CARTESIAN_POINT('Ctrl Pts',(-20.1698041636898,-12.8384515108891,
124.403918556395)) ;
#14169 = CARTESIAN_POINT('Ctrl Pts',(-20.1803949931304,-12.8390703489683,
124.395709293072)) ;
#14170 = CARTESIAN_POINT('Ctrl Pts',(-20.225115556298,-12.8417202382887,124.359879394597)) ;
#14171 = CARTESIAN_POINT('Ctrl Pts',(-20.2579095152776,-12.843754580663,124.330641028655)) ;
#14172 = CARTESIAN_POINT('Ctrl Pts',(-20.2970342675946,-12.8462923176429,
124.291873131076)) ;
#14173 = CARTESIAN_POINT('Ctrl Pts',(-20.3048656616391,-12.8468063913784,
124.283902247049)) ;
#14174 = CARTESIAN_POINT('Ctrl Pts',(-20.3167518534326,-12.8475962996151,
124.271475353459)) ;
#14175 = CARTESIAN_POINT('Ctrl Pts',(-20.3208830520861,-12.8478726939179,
124.26709326184)) ;
#14176 = CARTESIAN_POINT('Ctrl Pts',(-20.3290565117171,-12.8484233004166,
124.258296917279)) ;
#14177 = CARTESIAN_POINT('Ctrl Pts',(-20.3330990583362,-12.8486975084328,
124.253883143514)) ;
#14178 = CARTESIAN_POINT('Ctrl Pts',(-20.3411230451982,-12.8492456339764,
124.24499498233)) ;
#14179 = CARTESIAN_POINT('Ctrl Pts',(-20.3451043400114,-12.8495195440812,
124.240520673072)) ;
#14180 = CARTESIAN_POINT('Ctrl Pts',(-20.3542499840372,-12.8501533840125,
124.230092541126)) ;
#14181 = CARTESIAN_POINT('Ctrl Pts',(-20.3593904908652,-12.8505131343864,
124.224118138291)) ;
#14182 = CARTESIAN_POINT('Ctrl Pts',(-20.3730234662391,-12.8514769485059,
124.207967141218)) ;
#14183 = CARTESIAN_POINT('Ctrl Pts',(-20.3814111593863,-12.852080304637,124.197703410935)) ;
#14184 = CARTESIAN_POINT('Ctrl Pts',(-20.4127129938379,-12.8543745585008,
124.158132337548)) ;
#14185 = CARTESIAN_POINT('Ctrl Pts',(-20.4344779286586,-12.856059051023,124.127940852657)) ;
#14186 = CARTESIAN_POINT('Ctrl Pts',(-20.462952793321,-12.858423421377,124.084477101685)) ;
#14187 = CARTESIAN_POINT('Ctrl Pts',(-20.4708222736493,-12.859096559288,124.071988120083)) ;
#14188 = CARTESIAN_POINT('Ctrl Pts',(-20.484652665494,-12.8603163932561,124.049152134433)) ;
#14189 = CARTESIAN_POINT('Ctrl Pts',(-20.490690040506,-12.8608625217,124.038853463684)) ;
#14190 = CARTESIAN_POINT('Ctrl Pts',(-20.5031559892708,-12.8620195826105,
124.016873105728)) ;
#14191 = CARTESIAN_POINT('Ctrl Pts',(-20.509547054518,-12.8626305558189,124.005171818958)) ;
#14192 = CARTESIAN_POINT('Ctrl Pts',(-20.5286655508952,-12.8645145864201,
123.968796683161)) ;
#14193 = CARTESIAN_POINT('Ctrl Pts',(-20.5407591637519,-12.8657878954575,
123.943799353735)) ;
#14194 = CARTESIAN_POINT('Ctrl Pts',(-20.5761903754447,-12.8697966497089,
123.86387804393)) ;
#14195 = CARTESIAN_POINT('Ctrl Pts',(-20.596434399967,-12.8725233361498,123.807674804892)) ;
#14196 = CARTESIAN_POINT('Ctrl Pts',(-20.6153990071595,-12.8757375971586,
123.740244066871)) ;
#14197 = CARTESIAN_POINT('Ctrl Pts',(-20.6180860565241,-12.8762144539577,
123.730211921012)) ;
#14198 = CARTESIAN_POINT('Ctrl Pts',(-20.6232668921773,-12.8771798972182,
123.709857514234)) ;
#14199 = CARTESIAN_POINT('Ctrl Pts',(-20.6257547864346,-12.8776684675554,
123.699534623669)) ;
#14200 = CARTESIAN_POINT('Ctrl Pts',(-20.6309517764012,-12.8787478359158,
123.676697396913)) ;
#14201 = CARTESIAN_POINT('Ctrl Pts',(-20.633600725302,-12.879338944442,123.664170597919)) ;
#14202 = CARTESIAN_POINT('Ctrl Pts',(-20.6443107105378,-12.8819184993699,
123.609377697487)) ;
#14203 = CARTESIAN_POINT('Ctrl Pts',(-20.6503789088771,-12.8839083919632,
123.566751697832)) ;
#14204 = CARTESIAN_POINT('Ctrl Pts',(-20.654999940553,-12.8862792553361,123.515423623374)) ;
#14205 = CARTESIAN_POINT('Ctrl Pts',(-20.6556763172627,-12.8866702638371,
123.506941959054)) ;
#14206 = CARTESIAN_POINT('Ctrl Pts',(-20.6567406270531,-12.887375169527,123.491623482111)) ;
#14207 = CARTESIAN_POINT('Ctrl Pts',(-20.6571590758495,-12.8876892041029,
123.484789135382)) ;
#14208 = CARTESIAN_POINT('Ctrl Pts',(-20.6578583610003,-12.8882948369598,
123.4715911087)) ;
#14209 = CARTESIAN_POINT('Ctrl Pts',(-20.6581467493784,-12.8885864637149,
123.465228040448)) ;
#14210 = CARTESIAN_POINT('Ctrl Pts',(-20.6586568763359,-12.8892064974777,
123.451684472268)) ;
#14211 = CARTESIAN_POINT('Ctrl Pts',(-20.658865374892,-12.8895348294125,123.444503698921)) ;
#14212 = CARTESIAN_POINT('Ctrl Pts',(-20.6595849924584,-12.8911453132697,
123.40924555664)) ;
#14213 = CARTESIAN_POINT('Ctrl Pts',(-20.6592117538883,-12.8924228737751,
123.381158170071)) ;
#14214 = CARTESIAN_POINT('Ctrl Pts',(-20.6564231569889,-12.89512259501,123.321848631689)) ;
#14215 = CARTESIAN_POINT('Ctrl Pts',(-20.6537801752152,-12.8965435669904,
123.290656533896)) ;
#14216 = CARTESIAN_POINT('Ctrl Pts',(-20.6491903713324,-12.8982651229884,
123.253245901899)) ;
#14217 = CARTESIAN_POINT('Ctrl Pts',(-20.6483624559018,-12.8985577366996,
123.246901156957)) ;
#14218 = CARTESIAN_POINT('Ctrl Pts',(-20.6466704796217,-12.8991231389022,
123.234667509143)) ;
#14219 = CARTESIAN_POINT('Ctrl Pts',(-20.6458129994407,-12.8993958720515,
123.228777860617)) ;
#14220 = CARTESIAN_POINT('Ctrl Pts',(-20.6439072145186,-12.8999741464242,
123.216312959949)) ;
#14221 = CARTESIAN_POINT('Ctrl Pts',(-20.6428483703075,-12.9002797301754,
123.209739502278)) ;
#14222 = CARTESIAN_POINT('Ctrl Pts',(-20.6367048048506,-12.901970069064,123.173448546114)) ;
#14223 = CARTESIAN_POINT('Ctrl Pts',(-20.6305987330449,-12.9033575521151,
123.143914086722)) ;
#14224 = CARTESIAN_POINT('Ctrl Pts',(-20.6186215546723,-12.9056739694174,
123.094980946943)) ;
#14225 = CARTESIAN_POINT('Ctrl Pts',(-20.613336029205,-12.9066032901679,123.075452097576)) ;
#14226 = CARTESIAN_POINT('Ctrl Pts',(-20.6050799446674,-12.9079343362961,
123.047642673982)) ;
#14227 = CARTESIAN_POINT('Ctrl Pts',(-20.6024923489333,-12.908336974391,123.039251807705)) ;
#14228 = CARTESIAN_POINT('Ctrl Pts',(-20.5972574559531,-12.9091242371297,
123.02289067531)) ;
#14229 = CARTESIAN_POINT('Ctrl Pts',(-20.5946209881441,-12.909508404291,123.014927913574)) ;
#14230 = CARTESIAN_POINT('Ctrl Pts',(-20.5919012759315,-12.9098928303969,
123.006982853616)) ;
#14231 = CARTESIAN_POINT('Ctrl Pts',(-20.5919012759315,-12.9098928303969,
123.006982853616)) ;
#14232 = CARTESIAN_POINT('Ctrl Pts',(-20.5775883978109,-12.9119159282728,
122.965170828688)) ;
#14233 = CARTESIAN_POINT('Ctrl Pts',(-20.5610720915834,-12.913930083847,122.924156496481)) ;
#14234 = CARTESIAN_POINT('Ctrl Pts',(-20.5390005048911,-12.9163204656711,
122.876763499143)) ;
#14235 = CARTESIAN_POINT('Ctrl Pts',(-20.535515506082,-12.9166903884443,122.86946624177)) ;
#14236 = CARTESIAN_POINT('Ctrl Pts',(-20.5292796758374,-12.9173397518683,
122.856728342592)) ;
#14237 = CARTESIAN_POINT('Ctrl Pts',(-20.5265593912635,-12.9176190406129,
122.851273046282)) ;
#14238 = CARTESIAN_POINT('Ctrl Pts',(-20.5205508334242,-12.9182275802382,
122.839440928627)) ;
#14239 = CARTESIAN_POINT('Ctrl Pts',(-20.5172473473947,-12.9185569433274,
122.833072087567)) ;
#14240 = CARTESIAN_POINT('Ctrl Pts',(-20.5020609149817,-12.9200477324229,
122.804400581149)) ;
#14241 = CARTESIAN_POINT('Ctrl Pts',(-20.4895581579928,-12.9212119086459,
122.782432984259)) ;
#14242 = CARTESIAN_POINT('Ctrl Pts',(-20.466223985624,-12.9232759343705,122.744180711674)) ;
#14243 = CARTESIAN_POINT('Ctrl Pts',(-20.4556601246545,-12.924175579931,122.727742669082)) ;
#14244 = CARTESIAN_POINT('Ctrl Pts',(-20.4364479105815,-12.9257529044473,
122.699334242229)) ;
#14245 = CARTESIAN_POINT('Ctrl Pts',(-20.4279646375281,-12.926430934959,122.687256855252)) ;
#14246 = CARTESIAN_POINT('Ctrl Pts',(-20.4133949963966,-12.9275656788204,
122.667276326277)) ;
#14247 = CARTESIAN_POINT('Ctrl Pts',(-20.4074243176364,-12.9280227994365,
122.65929072306)) ;
#14248 = CARTESIAN_POINT('Ctrl Pts',(-20.3941634429978,-12.9290213380387,
122.641990229912)) ;
#14249 = CARTESIAN_POINT('Ctrl Pts',(-20.3868352717985,-12.929562547123,122.632705642966)) ;
#14250 = CARTESIAN_POINT('Ctrl Pts',(-20.3610542716988,-12.9314315605306,
122.600978331977)) ;
#14251 = CARTESIAN_POINT('Ctrl Pts',(-20.3419515233651,-12.9327561986542,
122.579075828085)) ;
#14252 = CARTESIAN_POINT('Ctrl Pts',(-20.3106440615985,-12.9348459453513,
122.545609901931)) ;
#14253 = CARTESIAN_POINT('Ctrl Pts',(-20.2989397911291,-12.935610738074,122.533592878431)) ;
#14254 = CARTESIAN_POINT('Ctrl Pts',(-20.2814419447094,-12.9367329085392,
122.516336350602)) ;
#14255 = CARTESIAN_POINT('Ctrl Pts',(-20.27583545528,-12.9370894005287,122.510909785357)) ;
#14256 = CARTESIAN_POINT('Ctrl Pts',(-20.2659046674212,-12.9377158583434,
122.501476173242)) ;
#14257 = CARTESIAN_POINT('Ctrl Pts',(-20.2616021434998,-12.9379856691212,
122.497446564531)) ;
#14258 = CARTESIAN_POINT('Ctrl Pts',(-20.2519496753662,-12.938587562321,122.488533695003)) ;
#14259 = CARTESIAN_POINT('Ctrl Pts',(-20.2465854743106,-12.9389197320638,
122.483666207131)) ;
#14260 = CARTESIAN_POINT('Ctrl Pts',(-20.2270582676089,-12.9401204287918,
122.466254240205)) ;
#14261 = CARTESIAN_POINT('Ctrl Pts',(-20.2126532360644,-12.9409902152709,
122.453985095874)) ;
#14262 = CARTESIAN_POINT('Ctrl Pts',(-20.1764627723942,-12.9431355769463,
122.424551696291)) ;
#14263 = CARTESIAN_POINT('Ctrl Pts',(-20.1543739584847,-12.9444108212181,
122.407776355452)) ;
#14264 = CARTESIAN_POINT('Ctrl Pts',(-20.1214485345774,-12.9462637013913,
122.38445652436)) ;
#14265 = CARTESIAN_POINT('Ctrl Pts',(-20.1110416642655,-12.9468427140955,
122.377319858696)) ;
#14266 = CARTESIAN_POINT('Ctrl Pts',(-20.0893877105434,-12.948034356684,122.36294748405)) ;
#14267 = CARTESIAN_POINT('Ctrl Pts',(-20.0781289530905,-12.9486468519291,
122.355732225217)) ;
#14268 = CARTESIAN_POINT('Ctrl Pts',(-20.0404641982286,-12.950673807246,122.332438434902)) ;
#14269 = CARTESIAN_POINT('Ctrl Pts',(-20.013577594316,-12.9520852288538,122.317158833203)) ;
#14270 = CARTESIAN_POINT('Ctrl Pts',(-19.9722410487926,-12.9542132268343,
122.295654876225)) ;
#14271 = CARTESIAN_POINT('Ctrl Pts',(-19.9581949553827,-12.9549293486662,
122.288680474729)) ;
#14272 = CARTESIAN_POINT('Ctrl Pts',(-19.9367534984031,-12.9560139352812,
122.278532330691)) ;
#14273 = CARTESIAN_POINT('Ctrl Pts',(-19.929452589261,-12.9563817676605,122.275162680817)) ;
#14274 = CARTESIAN_POINT('Ctrl Pts',(-19.9165600417877,-12.9570290663708,
122.269362508569)) ;
#14275 = CARTESIAN_POINT('Ctrl Pts',(-19.9109821796069,-12.9573083830753,
122.266902012721)) ;
#14276 = CARTESIAN_POINT('Ctrl Pts',(-19.8991668995139,-12.9578986875235,
122.261793003398)) ;
#14277 = CARTESIAN_POINT('Ctrl Pts',(-19.8929255038013,-12.9582097501578,
122.259154211467)) ;
#14278 = CARTESIAN_POINT('Ctrl Pts',(-19.8700549107403,-12.9593467891548,
122.249703246257)) ;
#14279 = CARTESIAN_POINT('Ctrl Pts',(-19.8533008261686,-12.9601742283784,
122.243199144594)) ;
#14280 = CARTESIAN_POINT('Ctrl Pts',(-19.8150409010411,-12.9620496723781,
122.229287870074)) ;
#14281 = CARTESIAN_POINT('Ctrl Pts',(-19.7934612941257,-12.9630975384539,
122.222101840424)) ;
#14282 = CARTESIAN_POINT('Ctrl Pts',(-19.7608071561949,-12.964667639962,122.212209144376)) ;
#14283 = CARTESIAN_POINT('Ctrl Pts',(-19.7498720628182,-12.9651908792965,
122.20905867726)) ;
#14284 = CARTESIAN_POINT('Ctrl Pts',(-19.730578335943,-12.9661096961196,122.203784261632)) ;
#14285 = CARTESIAN_POINT('Ctrl Pts',(-19.7222378945073,-12.9665054658401,
122.201596683093)) ;
#14286 = CARTESIAN_POINT('Ctrl Pts',(-19.7059301429664,-12.9672766282725,
122.19749925101)) ;
#14287 = CARTESIAN_POINT('Ctrl Pts',(-19.697965364666,-12.9676520343278,122.195581086492)) ;
#14288 = CARTESIAN_POINT('Ctrl Pts',(-19.6793714499795,-12.9685257088492,
122.19129604052)) ;
#14289 = CARTESIAN_POINT('Ctrl Pts',(-19.6687290844817,-12.9690237042166,
122.188989475399)) ;
#14290 = CARTESIAN_POINT('Ctrl Pts',(-19.6314713285406,-12.9707606754512,
122.18142273586)) ;
#14291 = CARTESIAN_POINT('Ctrl Pts',(-19.6047159181063,-12.9719964138408,
122.176890166614)) ;
#14292 = CARTESIAN_POINT('Ctrl Pts',(-19.5534875532042,-12.9743496367233,
122.169918365052)) ;
#14293 = CARTESIAN_POINT('Ctrl Pts',(-19.5290485731015,-12.9754668014679,
122.167323562315)) ;
#14294 = CARTESIAN_POINT('Ctrl Pts',(-19.4953567298301,-12.9770065505603,
122.164748027889)) ;
#14295 = CARTESIAN_POINT('Ctrl Pts',(-19.4861569061565,-12.9774269667192,
122.164147047146)) ;
#14296 = CARTESIAN_POINT('Ctrl Pts',(-19.4692081758792,-12.9782020447752,
122.163228039796)) ;
#14297 = CARTESIAN_POINT('Ctrl Pts',(-19.4614613306496,-12.9785565199066,
122.162880248932)) ;
#14298 = CARTESIAN_POINT('Ctrl Pts',(-19.4457005712165,-12.9792781019746,
122.162319573871)) ;
#14299 = CARTESIAN_POINT('Ctrl Pts',(-19.4376868317705,-12.9796452147584,
122.162111653568)) ;
#14300 = CARTESIAN_POINT('Ctrl Pts',(-19.4231292281717,-12.9803124980177,
122.161874048511)) ;
#14301 = CARTESIAN_POINT('Ctrl Pts',(-19.4165860636093,-12.9806125642582,
122.16181863751)) ;
#14302 = CARTESIAN_POINT('Ctrl Pts',(-19.3894599254743,-12.9818571648361,
122.161801916126)) ;
#14303 = CARTESIAN_POINT('Ctrl Pts',(-19.3688799470573,-12.9828028529772,
122.162297614695)) ;
#14304 = CARTESIAN_POINT('Ctrl Pts',(-19.2997663948605,-12.9859843516414,
122.165671636333)) ;
#14305 = CARTESIAN_POINT('Ctrl Pts',(-19.2513906353841,-12.9882209259606,
122.170872526433)) ;
#14306 = CARTESIAN_POINT('Ctrl Pts',(-19.1906592259112,-12.9910469194208,
122.181011263803)) ;
#14307 = CARTESIAN_POINT('Ctrl Pts',(-19.1779114292336,-12.9916411202217,
122.183343730252)) ;
#14308 = CARTESIAN_POINT('Ctrl Pts',(-19.1387932554911,-12.9934685562291,
122.191131690272)) ;
#14309 = CARTESIAN_POINT('Ctrl Pts',(-19.112561093433,-12.9946994898168,122.19724136478)) ;
#14310 = CARTESIAN_POINT('Ctrl Pts',(-19.0766342740806,-12.9964005165196,
122.206842474578)) ;
#14311 = CARTESIAN_POINT('Ctrl Pts',(-19.0667548191317,-12.9968699254867,
122.209613429599)) ;
#14312 = CARTESIAN_POINT('Ctrl Pts',(-19.0475907638457,-12.9977845517515,
122.215243904706)) ;
#14313 = CARTESIAN_POINT('Ctrl Pts',(-19.0383031769058,-12.9982297840111,
122.218090649035)) ;
#14314 = CARTESIAN_POINT('Ctrl Pts',(-19.0092749852391,-12.9996275150051,
122.227359593344)) ;
#14315 = CARTESIAN_POINT('Ctrl Pts',(-18.9896606004508,-13.0005806747561,
122.234165443737)) ;
#14316 = CARTESIAN_POINT('Ctrl Pts',(-18.9553630060942,-13.0022616890983,
122.247031825415)) ;
#14317 = CARTESIAN_POINT('Ctrl Pts',(-18.9406087125977,-13.00298965324,122.252889666438)) ;
#14318 = CARTESIAN_POINT('Ctrl Pts',(-18.8899170461784,-13.0055084196402,
122.274141977281)) ;
#14319 = CARTESIAN_POINT('Ctrl Pts',(-18.8545930053298,-13.0072943080635,
122.290940047591)) ;
#14320 = CARTESIAN_POINT('Ctrl Pts',(-18.789226128513,-13.0106847478791,122.325872663727)) ;
#14321 = CARTESIAN_POINT('Ctrl Pts',(-18.7590453480146,-13.0122863021443,
122.343670393544)) ;
#14322 = CARTESIAN_POINT('Ctrl Pts',(-18.7164615896387,-13.0146092337777,
122.371256628846)) ;
#14323 = CARTESIAN_POINT('Ctrl Pts',(-18.7034336533728,-13.0153289723965,
122.380049426649)) ;
#14324 = CARTESIAN_POINT('Ctrl Pts',(-18.6805344091642,-13.0166118918159,
122.396141300326)) ;
#14325 = CARTESIAN_POINT('Ctrl Pts',(-18.6705982792143,-13.0171747476147,
122.403344544381)) ;
#14326 = CARTESIAN_POINT('Ctrl Pts',(-18.6469979013449,-13.0185277606215,
122.42098969531)) ;
#14327 = CARTESIAN_POINT('Ctrl Pts',(-18.6334399184256,-13.0193183437501,
122.431569548518)) ;
#14328 = CARTESIAN_POINT('Ctrl Pts',(-18.5984805170206,-13.0213918369986,
122.460029577977)) ;
#14329 = CARTESIAN_POINT('Ctrl Pts',(-18.5774515410442,-13.0226746626617,
122.478352085696)) ;
#14330 = CARTESIAN_POINT('Ctrl Pts',(-18.5429132329147,-13.0248445416171,
122.510539905779)) ;
#14331 = CARTESIAN_POINT('Ctrl Pts',(-18.5290810402856,-13.0257320030397,
122.52404354139)) ;
#14332 = CARTESIAN_POINT('Ctrl Pts',(-18.5047329145781,-13.0273293859359,
122.548941977604)) ;
#14333 = CARTESIAN_POINT('Ctrl Pts',(-18.4941052648056,-13.028039496196,122.560221999166)) ;
#14334 = CARTESIAN_POINT('Ctrl Pts',(-18.4589733246402,-13.0304330212014,
122.598927883898)) ;
#14335 = CARTESIAN_POINT('Ctrl Pts',(-18.4354703127565,-13.0321124777807,
122.627236596445)) ;
#14336 = CARTESIAN_POINT('Ctrl Pts',(-18.4047310311276,-13.0344379210765,
122.667774222138)) ;
#14337 = CARTESIAN_POINT('Ctrl Pts',(-18.3964031040837,-13.0350824709017,
122.679151490865)) ;
#14338 = CARTESIAN_POINT('Ctrl Pts',(-18.3833515378214,-13.0361177635829,
122.697629945667)) ;
#14339 = CARTESIAN_POINT('Ctrl Pts',(-18.3785050054822,-13.0365080752328,
122.704642830045)) ;
#14340 = CARTESIAN_POINT('Ctrl Pts',(-18.369132579751,-13.0372749482622,122.718505711784)) ;
#14341 = CARTESIAN_POINT('Ctrl Pts',(-18.3646016899217,-13.0376514897607,
122.725351807494)) ;
#14342 = CARTESIAN_POINT('Ctrl Pts',(-18.3488433516192,-13.0389822660292,
122.749679759746)) ;
#14343 = CARTESIAN_POINT('Ctrl Pts',(-18.3379846614465,-13.0399379662251,
122.76739634588)) ;
#14344 = CARTESIAN_POINT('Ctrl Pts',(-18.3171127031513,-13.041854177952,122.803436863907)) ;
#14345 = CARTESIAN_POINT('Ctrl Pts',(-18.3071067891807,-13.0428143931389,
122.821757622706)) ;
#14346 = CARTESIAN_POINT('Ctrl Pts',(-18.2941348880858,-13.0441183797035,
122.846991420965)) ;
#14347 = CARTESIAN_POINT('Ctrl Pts',(-18.290765598599,-13.044462973073,122.853693262422)) ;
#14348 = CARTESIAN_POINT('Ctrl Pts',(-18.2867069652352,-13.0448854653208,
122.861950653556)) ;
#14349 = CARTESIAN_POINT('Ctrl Pts',(-18.28596021056,-13.0449635157868,122.863477806124)) ;
#14350 = CARTESIAN_POINT('Ctrl Pts',(-18.2802327545433,-13.0455645893776,
122.875251556097)) ;
#14351 = CARTESIAN_POINT('Ctrl Pts',(-18.2753892269254,-13.0460871962536,
122.885564309199)) ;
#14352 = CARTESIAN_POINT('Ctrl Pts',(-18.2655112925735,-13.0471842395133,
122.907365948865)) ;
#14353 = CARTESIAN_POINT('Ctrl Pts',(-18.2605074570837,-13.0477585241867,
122.918867325056)) ;
#14354 = CARTESIAN_POINT('Ctrl Pts',(-18.2451817496326,-13.0495793052044,
122.955594936856)) ;
#14355 = CARTESIAN_POINT('Ctrl Pts',(-18.2355113869129,-13.0508234540972,
122.981084399287)) ;
#14356 = CARTESIAN_POINT('Ctrl Pts',(-18.2203367506623,-13.0529613368954,
123.02540001655)) ;
#14357 = CARTESIAN_POINT('Ctrl Pts',(-18.2144279535755,-13.0538549217811,
123.04407699115)) ;
#14358 = CARTESIAN_POINT('Ctrl Pts',(-18.2065168751264,-13.0551496405923,
123.071290985516)) ;
#14359 = CARTESIAN_POINT('Ctrl Pts',(-18.2041616510312,-13.0555497707345,
123.079722348193)) ;
#14360 = CARTESIAN_POINT('Ctrl Pts',(-18.2003504332994,-13.0562232653936,
123.093940691903)) ;
#14361 = CARTESIAN_POINT('Ctrl Pts',(-18.1988469605123,-13.0564964154554,
123.099714622365)) ;
#14362 = CARTESIAN_POINT('Ctrl Pts',(-18.1964149231448,-13.0569511588676,
123.109336588704)) ;
#14363 = CARTESIAN_POINT('Ctrl Pts',(-18.1954631943831,-13.0571326213352,
123.113178672354)) ;
#14364 = CARTESIAN_POINT('Ctrl Pts',(-18.1928193199878,-13.057646912745,123.124073328738)) ;
#14365 = CARTESIAN_POINT('Ctrl Pts',(-18.1911702881845,-13.0579800440933,
123.131136177628)) ;
#14366 = CARTESIAN_POINT('Ctrl Pts',(-18.1851915367861,-13.0592356437218,
123.157788890227)) ;
#14367 = CARTESIAN_POINT('Ctrl Pts',(-18.1812721773872,-13.0601593967781,
123.177467705277)) ;
#14368 = CARTESIAN_POINT('Ctrl Pts',(-18.1762450257569,-13.0615059729539,
123.206317538316)) ;
#14369 = CARTESIAN_POINT('Ctrl Pts',(-18.1747624931863,-13.0619297561237,
123.215420010491)) ;
#14370 = CARTESIAN_POINT('Ctrl Pts',(-18.1733279372883,-13.0623693498795,
123.22488706714)) ;
#14371 = CARTESIAN_POINT('Ctrl Pts',(-18.1732752009602,-13.0623855546872,
123.225236087655)) ;
#14372 = CARTESIAN_POINT('Ctrl Pts',(-18.1731739898418,-13.0624167411119,
123.225907850948)) ;
#14373 = CARTESIAN_POINT('Ctrl Pts',(-18.1731254935991,-13.0624317228131,
123.226230590453)) ;
#14374 = CARTESIAN_POINT('Ctrl Pts',(-18.1730322579247,-13.0624605999273,
123.22685272611)) ;
#14375 = CARTESIAN_POINT('Ctrl Pts',(-18.1729875008424,-13.0624744954116,
123.227152119618)) ;
#14376 = CARTESIAN_POINT('Ctrl Pts',(-18.1729013020541,-13.0625013214108,
123.227730165044)) ;
#14377 = CARTESIAN_POINT('Ctrl Pts',(-18.1728598457825,-13.0625142519837,
123.228008814765)) ;
#14378 = CARTESIAN_POINT('Ctrl Pts',(-18.1727798609613,-13.0625392560214,
123.228547686934)) ;
#14379 = CARTESIAN_POINT('Ctrl Pts',(-18.1727413203504,-13.0625513295345,
123.228807907568)) ;
#14380 = CARTESIAN_POINT('Ctrl Pts',(-18.172666825022,-13.0625747156766,123.229311987152)) ;
#14381 = CARTESIAN_POINT('Ctrl Pts',(-18.172630860287,-13.0625860283463,123.229555844607)) ;
#14382 = CARTESIAN_POINT('Ctrl Pts',(-18.1725612139819,-13.0626079789659,
123.230029048278)) ;
#14383 = CARTESIAN_POINT('Ctrl Pts',(-18.1725275240742,-13.0626186169493,
123.230258393242)) ;
#14384 = CARTESIAN_POINT('Ctrl Pts',(-18.1714248313732,-13.0629674569973,
123.237779552869)) ;
#14385 = CARTESIAN_POINT('Ctrl Pts',(-18.1704202705523,-13.0633053813651,
123.245080681877)) ;
#14386 = CARTESIAN_POINT('Ctrl Pts',(-18.168431666638,-13.06401971258,123.260545440612)) ;
#14387 = CARTESIAN_POINT('Ctrl Pts',(-18.1674634882772,-13.0643960305851,
123.268710763728)) ;
#14388 = CARTESIAN_POINT('Ctrl Pts',(-18.1635092236459,-13.0660711434776,
123.305129464474)) ;
#14389 = CARTESIAN_POINT('Ctrl Pts',(-18.1614063174537,-13.0673653346237,
123.333470214096)) ;
#14390 = CARTESIAN_POINT('Ctrl Pts',(-18.1597382240551,-13.0692691129838,
123.375175643557)) ;
#14391 = CARTESIAN_POINT('Ctrl Pts',(-18.1594185947804,-13.0698773215834,
123.388500908696)) ;
#14392 = CARTESIAN_POINT('Ctrl Pts',(-18.1592439251985,-13.0708763703781,
123.410365268362)) ;
#14393 = CARTESIAN_POINT('Ctrl Pts',(-18.159263180604,-13.0712667198629,123.418902286574)) ;
#14394 = CARTESIAN_POINT('Ctrl Pts',(-18.1594670905398,-13.0720133768512,
123.435214793494)) ;
#14395 = CARTESIAN_POINT('Ctrl Pts',(-18.1596368666112,-13.0723696050656,
123.44299007411)) ;
#14396 = CARTESIAN_POINT('Ctrl Pts',(-18.1601550285815,-13.0731320120191,
123.459611551135)) ;
#14397 = CARTESIAN_POINT('Ctrl Pts',(-18.1605248558696,-13.073538264051,123.468456653791)) ;
#14398 = CARTESIAN_POINT('Ctrl Pts',(-18.1618961037786,-13.0747406513569,
123.494596480354)) ;
#14399 = CARTESIAN_POINT('Ctrl Pts',(-18.1631631162199,-13.0755378065521,
123.511875105038)) ;
#14400 = CARTESIAN_POINT('Ctrl Pts',(-18.1668635155437,-13.0773543273082,
123.551131676553)) ;
#14401 = CARTESIAN_POINT('Ctrl Pts',(-18.1695217492384,-13.0783739957619,
123.57308269195)) ;
#14402 = CARTESIAN_POINT('Ctrl Pts',(-18.1737028013295,-13.0796881684279,
123.60131243919)) ;
#14403 = CARTESIAN_POINT('Ctrl Pts',(-18.1746939543766,-13.0799841292373,
123.607665877077)) ;
#14404 = CARTESIAN_POINT('Ctrl Pts',(-18.1769725583315,-13.08063206423,123.62156689713)) ;
#14405 = CARTESIAN_POINT('Ctrl Pts',(-18.1782804218478,-13.0809839434711,
123.629110877309)) ;
#14406 = CARTESIAN_POINT('Ctrl Pts',(-18.1796825750349,-13.0813418989933,
123.636779442194)) ;
#14407 = CARTESIAN_POINT('Ctrl Pts',(-18.1797076591581,-13.0813482967574,
123.636916501118)) ;
#14408 = CARTESIAN_POINT('Ctrl Pts',(-18.1797571007982,-13.08136089524,123.637186393973)) ;
#14409 = CARTESIAN_POINT('Ctrl Pts',(-18.17978145692,-13.0813670959634,123.637319228122)) ;
#14410 = CARTESIAN_POINT('Ctrl Pts',(-18.1798294756377,-13.0813793098524,
123.637580875011)) ;
#14411 = CARTESIAN_POINT('Ctrl Pts',(-18.1798531369639,-13.0813853230271,
123.637709688049)) ;
#14412 = CARTESIAN_POINT('Ctrl Pts',(-18.1798997978742,-13.0813971708785,
123.637963487097)) ;
#14413 = CARTESIAN_POINT('Ctrl Pts',(-18.1799227962642,-13.081403005558,123.638088473264)) ;
#14414 = CARTESIAN_POINT('Ctrl Pts',(-18.1799681618166,-13.0814145050659,
123.638334804078)) ;
#14415 = CARTESIAN_POINT('Ctrl Pts',(-18.1799905278861,-13.0814201698995,
123.638456148926)) ;
#14416 = CARTESIAN_POINT('Ctrl Pts',(-18.1800346581077,-13.0814313379743,
123.63869537427)) ;
#14417 = CARTESIAN_POINT('Ctrl Pts',(-18.18005642125,-13.0814368412202,123.638813254951)) ;
#14418 = CARTESIAN_POINT('Ctrl Pts',(-18.1800993737828,-13.0814476940123,
123.639045721263)) ;
#14419 = CARTESIAN_POINT('Ctrl Pts',(-18.1801205622433,-13.0814530435636,
123.639160307084)) ;
#14420 = CARTESIAN_POINT('Ctrl Pts',(-18.1801623924911,-13.0814635965141,
123.639386345569)) ;
#14421 = CARTESIAN_POINT('Ctrl Pts',(-18.1801830334174,-13.0814687999178,
123.639497798402)) ;
#14422 = CARTESIAN_POINT('Ctrl Pts',(-18.1802237946366,-13.0814790677941,
123.639717725786)) ;
#14423 = CARTESIAN_POINT('Ctrl Pts',(-18.1802439141367,-13.0814841322717,
123.639826200512)) ;
#14424 = CARTESIAN_POINT('Ctrl Pts',(-18.1802836575684,-13.0814941292115,
123.640040319999)) ;
#14425 = CARTESIAN_POINT('Ctrl Pts',(-18.1803032807535,-13.081499061675,123.640145964852)) ;
#14426 = CARTESIAN_POINT('Ctrl Pts',(-18.1803420556776,-13.0815088012103,
123.640354566639)) ;
#14427 = CARTESIAN_POINT('Ctrl Pts',(-18.1803612067343,-13.0815136082854,
123.640457523704)) ;
#14428 = CARTESIAN_POINT('Ctrl Pts',(-18.1803990606398,-13.0815231033946,
123.640660886096)) ;
#14429 = CARTESIAN_POINT('Ctrl Pts',(-18.1804177628551,-13.0815277914313,
123.640761291535)) ;
#14430 = CARTESIAN_POINT('Ctrl Pts',(-18.1804547414835,-13.0815370545586,
123.640959681367)) ;
#14431 = CARTESIAN_POINT('Ctrl Pts',(-18.1804730173109,-13.0815416296518,
123.641057665866)) ;
#14432 = CARTESIAN_POINT('Ctrl Pts',(-18.1805091647896,-13.0815506727483,
123.641251339383)) ;
#14433 = CARTESIAN_POINT('Ctrl Pts',(-18.1805270358877,-13.0815551407512,
123.641347028439)) ;
#14434 = CARTESIAN_POINT('Ctrl Pts',(-18.180562394769,-13.0815639752917,123.641536231661)) ;
#14435 = CARTESIAN_POINT('Ctrl Pts',(-18.1805798820687,-13.0815683418361,
123.641629746015)) ;
#14436 = CARTESIAN_POINT('Ctrl Pts',(-18.1806144935397,-13.0815769788782,
123.641814716)) ;
#14437 = CARTESIAN_POINT('Ctrl Pts',(-18.1806316172486,-13.0815812493785,
123.641906171725)) ;
#14438 = CARTESIAN_POINT('Ctrl Pts',(-18.1806655210745,-13.081589699554,123.642087136392)) ;
#14439 = CARTESIAN_POINT('Ctrl Pts',(-18.1806823007714,-13.0815938792336,
123.642176645462)) ;
#14440 = CARTESIAN_POINT('Ctrl Pts',(-18.1819650070658,-13.0819132007008,
123.649014945714)) ;
#14441 = CARTESIAN_POINT('Ctrl Pts',(-18.1832865131806,-13.082228067896,123.655753204651)) ;
#14442 = CARTESIAN_POINT('Ctrl Pts',(-18.1862418262234,-13.0829032804911,
123.670191157947)) ;
#14443 = CARTESIAN_POINT('Ctrl Pts',(-18.1878929743441,-13.0832635260659,
123.677887005614)) ;
#14444 = CARTESIAN_POINT('Ctrl Pts',(-18.1953906008683,-13.0848290950261,
123.711291358972)) ;
#14445 = CARTESIAN_POINT('Ctrl Pts',(-18.2019769201654,-13.0860303966778,
123.736826857018)) ;
#14446 = CARTESIAN_POINT('Ctrl Pts',(-18.214421298012,-13.0880550658993,123.779450919123)) ;
#14447 = CARTESIAN_POINT('Ctrl Pts',(-18.2198510183822,-13.0888780516765,
123.796655324863)) ;
#14448 = CARTESIAN_POINT('Ctrl Pts',(-18.225980363612,-13.0897489060499,123.814705658685)) ;
#14449 = CARTESIAN_POINT('Ctrl Pts',(-18.2263107702426,-13.0897956839766,
123.815674762045)) ;
#14450 = CARTESIAN_POINT('Ctrl Pts',(-18.2266423654692,-13.0898424649011,
123.816643453359)) ;
#14451 = CARTESIAN_POINT('',(-20.5919012301245,-12.8497876110288,123.00698271985)) ;
#14452 = CARTESIAN_POINT('Ctrl Pts',(-18.2266423654684,-13.0298305431221,
123.816643453356)) ;
#14453 = CARTESIAN_POINT('Ctrl Pts',(-18.2266336269289,-13.0298293099018,
123.816617925403)) ;
#14454 = CARTESIAN_POINT('Ctrl Pts',(-18.2266248892215,-13.0298280766837,
123.81659239716)) ;
#14455 = CARTESIAN_POINT('Ctrl Pts',(-18.2220695400772,-13.0291850824373,
123.803282012787)) ;
#14456 = CARTESIAN_POINT('Ctrl Pts',(-18.2177471039428,-13.0285428243449,
123.789921517234)) ;
#14457 = CARTESIAN_POINT('Ctrl Pts',(-18.2110538843167,-13.0274922431459,
123.767977264901)) ;
#14458 = CARTESIAN_POINT('Ctrl Pts',(-18.2085481026181,-13.0270843823758,
123.759435976209)) ;
#14459 = CARTESIAN_POINT('Ctrl Pts',(-18.2034737365447,-13.0262264601579,
123.741429524127)) ;
#14460 = CARTESIAN_POINT('Ctrl Pts',(-18.2009248867699,-13.025776357877,123.731959421547)) ;
#14461 = CARTESIAN_POINT('Ctrl Pts',(-18.1960681444864,-13.0248784475954,
123.71302961412)) ;
#14462 = CARTESIAN_POINT('Ctrl Pts',(-18.1937588160346,-13.0244306771055,
123.703570974076)) ;
#14463 = CARTESIAN_POINT('Ctrl Pts',(-18.1888032044353,-13.0234201674437,
123.682192629131)) ;
#14464 = CARTESIAN_POINT('Ctrl Pts',(-18.1862205901484,-13.0228571695493,
123.670259198915)) ;
#14465 = CARTESIAN_POINT('Ctrl Pts',(-18.1801998711803,-13.0214465253905,
123.640324607423)) ;
#14466 = CARTESIAN_POINT('Ctrl Pts',(-18.1769820460673,-13.0205977435113,
123.622282147979)) ;
#14467 = CARTESIAN_POINT('Ctrl Pts',(-18.1684886776864,-13.018032102044,123.567748056236)) ;
#14468 = CARTESIAN_POINT('Ctrl Pts',(-18.1644296947558,-13.0163037321195,
123.531087755827)) ;
#14469 = CARTESIAN_POINT('Ctrl Pts',(-18.161852745762,-13.0144791238167,123.492122447006)) ;
#14470 = CARTESIAN_POINT('Ctrl Pts',(-18.1617143016538,-13.0143770752841,
123.489942292877)) ;
#14471 = CARTESIAN_POINT('Ctrl Pts',(-18.1613715988705,-13.0141136548413,
123.484312252165)) ;
#14472 = CARTESIAN_POINT('Ctrl Pts',(-18.16117593067,-13.0139523234107,123.480861859157)) ;
#14473 = CARTESIAN_POINT('Ctrl Pts',(-18.1595470511962,-13.0125040126246,
123.449864791374)) ;
#14474 = CARTESIAN_POINT('Ctrl Pts',(-18.1590116944642,-13.0112227479266,
123.422278195262)) ;
#14475 = CARTESIAN_POINT('Ctrl Pts',(-18.159474092363,-13.0096659130224,123.388516362409)) ;
#14476 = CARTESIAN_POINT('Ctrl Pts',(-18.1596045604335,-13.0093814246662,
123.382337290293)) ;
#14477 = CARTESIAN_POINT('Ctrl Pts',(-18.1598838429588,-13.0089314951013,
123.372550118525)) ;
#14478 = CARTESIAN_POINT('Ctrl Pts',(-18.1600024749048,-13.0087657375565,
123.368941275192)) ;
#14479 = CARTESIAN_POINT('Ctrl Pts',(-18.1602544879414,-13.0084549319154,
123.362168704233)) ;
#14480 = CARTESIAN_POINT('Ctrl Pts',(-18.1603842569619,-13.0083098464332,
123.359004872697)) ;
#14481 = CARTESIAN_POINT('Ctrl Pts',(-18.1605262519108,-13.0081646794803,
123.355836983321)) ;
#14482 = CARTESIAN_POINT('Ctrl Pts',(-18.1605264572053,-13.0081644696259,
123.355832403791)) ;
#14483 = CARTESIAN_POINT('Ctrl Pts',(-18.1605268679082,-13.0081640498524,
123.355823243313)) ;
#14484 = CARTESIAN_POINT('Ctrl Pts',(-18.1605270732759,-13.0081638399751,
123.355818663275)) ;
#14485 = CARTESIAN_POINT('Ctrl Pts',(-18.1605274840961,-13.008163420186,123.355809502436)) ;
#14486 = CARTESIAN_POINT('Ctrl Pts',(-18.1605276895816,-13.0081632102403,
123.355804920897)) ;
#14487 = CARTESIAN_POINT('Ctrl Pts',(-18.1605281006209,-13.0081627903314,
123.355795757425)) ;
#14488 = CARTESIAN_POINT('Ctrl Pts',(-18.1605283061963,-13.008162580346,123.355791175009)) ;
#14489 = CARTESIAN_POINT('Ctrl Pts',(-18.1605287174557,-13.0081621603164,
123.355782008884)) ;
#14490 = CARTESIAN_POINT('Ctrl Pts',(-18.1605289231072,-13.0081619503053,
123.355777425898)) ;
#14491 = CARTESIAN_POINT('Ctrl Pts',(-18.1605293344944,-13.0081615302493,
123.355768259179)) ;
#14492 = CARTESIAN_POINT('Ctrl Pts',(-18.1605295402624,-13.0081613201714,
123.355763674725)) ;
#14493 = CARTESIAN_POINT('Ctrl Pts',(-18.160529951926,-13.0081608999375,123.355754504102)) ;
#14494 = CARTESIAN_POINT('Ctrl Pts',(-18.160530157757,-13.0081606898473,123.355749919372)) ;
#14495 = CARTESIAN_POINT('Ctrl Pts',(-18.1605305695104,-13.0081602696258,
123.355740749002)) ;
#14496 = CARTESIAN_POINT('Ctrl Pts',(-18.1605307754719,-13.0081600594547,
123.355736162494)) ;
#14497 = CARTESIAN_POINT('Ctrl Pts',(-18.1605311874696,-13.0081596390882,
123.35572698894)) ;
#14498 = CARTESIAN_POINT('Ctrl Pts',(-18.1605313935188,-13.0081594288795,
123.355722401605)) ;
#14499 = CARTESIAN_POINT('Ctrl Pts',(-18.1605318057245,-13.0081590084051,
123.355713225676)) ;
#14500 = CARTESIAN_POINT('Ctrl Pts',(-18.1605320118591,-13.0081587981614,
123.355708637567)) ;
#14501 = CARTESIAN_POINT('Ctrl Pts',(-18.1605324242075,-13.0081583776457,
123.355699460718)) ;
#14502 = CARTESIAN_POINT('Ctrl Pts',(-18.1605326304599,-13.0081581673341,
123.355694871117)) ;
#14503 = CARTESIAN_POINT('Ctrl Pts',(-18.1605330430493,-13.0081577466768,
123.35568569116)) ;
#14504 = CARTESIAN_POINT('Ctrl Pts',(-18.1605332493872,-13.0081575363302,
123.355681100786)) ;
#14505 = CARTESIAN_POINT('Ctrl Pts',(-18.1605336622005,-13.008157115549,123.355671918105)) ;
#14506 = CARTESIAN_POINT('Ctrl Pts',(-18.1605338686172,-13.0081569051743,
123.355667327108)) ;
#14507 = CARTESIAN_POINT('Ctrl Pts',(-18.1605342815563,-13.0081564843692,
123.355658143886)) ;
#14508 = CARTESIAN_POINT('Ctrl Pts',(-18.1605344880983,-13.0081562739189,
123.35565355123)) ;
#14509 = CARTESIAN_POINT('Ctrl Pts',(-18.1605349012702,-13.008155852981,123.35564436509)) ;
#14510 = CARTESIAN_POINT('Ctrl Pts',(-18.1605351079081,-13.0081556424851,
123.355639771429)) ;
#14511 = CARTESIAN_POINT('Ctrl Pts',(-18.1605355212854,-13.0081552214423,
123.355630582984)) ;
#14512 = CARTESIAN_POINT('Ctrl Pts',(-18.1605357280191,-13.0081550109011,
123.355625988324)) ;
#14513 = CARTESIAN_POINT('Ctrl Pts',(-18.1605361415585,-13.0081545897976,
123.355616798532)) ;
#14514 = CARTESIAN_POINT('Ctrl Pts',(-18.1605363484103,-13.0081543791883,
123.355612202376)) ;
#14515 = CARTESIAN_POINT('Ctrl Pts',(-18.1605367622167,-13.0081539579174,
123.355603008913)) ;
#14516 = CARTESIAN_POINT('Ctrl Pts',(-18.1605369691463,-13.0081537472812,
123.35559841216)) ;
#14517 = CARTESIAN_POINT('Ctrl Pts',(-18.1605373831376,-13.0081533259264,
123.355589216849)) ;
#14518 = CARTESIAN_POINT('Ctrl Pts',(-18.1605375901665,-13.0081531152414,
123.35558461902)) ;
#14519 = CARTESIAN_POINT('Ctrl Pts',(-18.1605380043394,-13.0081526938064,
123.355575421938)) ;
#14520 = CARTESIAN_POINT('Ctrl Pts',(-18.160538211481,-13.0081524830589,123.355570822737)) ;
#14521 = CARTESIAN_POINT('Ctrl Pts',(-18.1605386258578,-13.0081520615208,
123.355561623386)) ;
#14522 = CARTESIAN_POINT('Ctrl Pts',(-18.1605388331084,-13.0081518507147,
123.355557022897)) ;
#14523 = CARTESIAN_POINT('Ctrl Pts',(-18.1605392477027,-13.00815142906,123.355547820981)) ;
#14524 = CARTESIAN_POINT('Ctrl Pts',(-18.1605394550545,-13.0081512182032,
123.355543219377)) ;
#14525 = CARTESIAN_POINT('Ctrl Pts',(-18.1605398698522,-13.0081507964462,
123.355534015209)) ;
#14526 = CARTESIAN_POINT('Ctrl Pts',(-18.1605400773091,-13.0081505855348,
123.355529412403)) ;
#14527 = CARTESIAN_POINT('Ctrl Pts',(-18.1605404923302,-13.0081501636553,
123.355520205542)) ;
#14528 = CARTESIAN_POINT('Ctrl Pts',(-18.1605406998851,-13.0081499526966,
123.355515601694)) ;
#14529 = CARTESIAN_POINT('Ctrl Pts',(-18.1605411150961,-13.0081495307287,
123.355506392886)) ;
#14530 = CARTESIAN_POINT('Ctrl Pts',(-18.1605413227629,-13.0081493197085,
123.355501787686)) ;
#14531 = CARTESIAN_POINT('Ctrl Pts',(-18.1605417382234,-13.0081488975917,
123.355492575609)) ;
#14532 = CARTESIAN_POINT('Ctrl Pts',(-18.1605419459802,-13.0081486865325,
123.355487969547)) ;
#14533 = CARTESIAN_POINT('Ctrl Pts',(-18.1605423616186,-13.0081482643396,
123.35547875579)) ;
#14534 = CARTESIAN_POINT('Ctrl Pts',(-18.160542569491,-13.0081480532153,123.355474148299)) ;
#14535 = CARTESIAN_POINT('Ctrl Pts',(-18.1605429853108,-13.0081476309429,
123.355464932787)) ;
#14536 = CARTESIAN_POINT('Ctrl Pts',(-18.1605431933107,-13.0081474197415,
123.355460323603)) ;
#14537 = CARTESIAN_POINT('Ctrl Pts',(-18.1607071371375,-13.0079809731343,
123.351827848802)) ;
#14538 = CARTESIAN_POINT('Ctrl Pts',(-18.1608866822671,-13.0078149080799,
123.348200706442)) ;
#14539 = CARTESIAN_POINT('Ctrl Pts',(-18.1613048012872,-13.0074598272328,
123.340439072758)) ;
#14540 = CARTESIAN_POINT('Ctrl Pts',(-18.1615481206548,-13.0072708640559,
123.336304878289)) ;
#14541 = CARTESIAN_POINT('Ctrl Pts',(-18.1622337413082,-13.0067804141476,
123.325565819221)) ;
#14542 = CARTESIAN_POINT('Ctrl Pts',(-18.1627079720956,-13.0064792686464,
123.318963110444)) ;
#14543 = CARTESIAN_POINT('Ctrl Pts',(-18.1642847940806,-13.0055791824351,
123.299206637341)) ;
#14544 = CARTESIAN_POINT('Ctrl Pts',(-18.1655433124905,-13.0049818528825,
123.286066203533)) ;
#14545 = CARTESIAN_POINT('Ctrl Pts',(-18.1715514625257,-13.0025412296005,
123.232318819475)) ;
#14546 = CARTESIAN_POINT('Ctrl Pts',(-18.1780836579929,-13.0007151883165,
123.191937003724)) ;
#14547 = CARTESIAN_POINT('Ctrl Pts',(-18.1968525805178,-12.9966613247086,
123.103627966524)) ;
#14548 = CARTESIAN_POINT('Ctrl Pts',(-18.2099775134481,-12.9944296132711,
123.055960035106)) ;
#14549 = CARTESIAN_POINT('Ctrl Pts',(-18.2300830433367,-12.9915874550878,
122.996865630726)) ;
#14550 = CARTESIAN_POINT('Ctrl Pts',(-18.2344701859164,-12.990993435481,122.984602772603)) ;
#14551 = CARTESIAN_POINT('Ctrl Pts',(-18.2416863646024,-12.9900553184883,
122.965384572863)) ;
#14552 = CARTESIAN_POINT('Ctrl Pts',(-18.2443878243063,-12.9897119888688,
122.958382304742)) ;
#14553 = CARTESIAN_POINT('Ctrl Pts',(-18.2494567369432,-12.9890817584299,
122.945587859146)) ;
#14554 = CARTESIAN_POINT('Ctrl Pts',(-18.2518049374338,-12.9887949789871,
122.939788307398)) ;
#14555 = CARTESIAN_POINT('Ctrl Pts',(-18.2565169420212,-12.9882294608902,
122.928397278077)) ;
#14556 = CARTESIAN_POINT('Ctrl Pts',(-18.258878133078,-12.9879507448073,122.922804901488)) ;
#14557 = CARTESIAN_POINT('Ctrl Pts',(-18.2642164911473,-12.9873307249975,
122.910413904723)) ;
#14558 = CARTESIAN_POINT('Ctrl Pts',(-18.2672136599557,-12.9869893135365,
122.903624155769)) ;
#14559 = CARTESIAN_POINT('Ctrl Pts',(-18.2748041407707,-12.9861408104745,
122.886835111482)) ;
#14560 = CARTESIAN_POINT('Ctrl Pts',(-18.279469348912,-12.9856333172014,122.876869030968)) ;
#14561 = CARTESIAN_POINT('Ctrl Pts',(-18.2928029426141,-12.9842201787856,
122.849337739322)) ;
#14562 = CARTESIAN_POINT('Ctrl Pts',(-18.3017534746653,-12.9833129500962,
122.831912803098)) ;
#14563 = CARTESIAN_POINT('Ctrl Pts',(-18.3320185935628,-12.98036955666,122.776251227436)) ;
#14564 = CARTESIAN_POINT('Ctrl Pts',(-18.3549326776928,-12.978319937505,122.738922182948)) ;
#14565 = CARTESIAN_POINT('Ctrl Pts',(-18.3805682746663,-12.9762021091121,
122.701694512618)) ;
#14566 = CARTESIAN_POINT('Ctrl Pts',(-18.3813817150016,-12.9761350814685,
122.700517576275)) ;
#14567 = CARTESIAN_POINT('Ctrl Pts',(-18.3829085278908,-12.9760095963076,
122.698316576487)) ;
#14568 = CARTESIAN_POINT('Ctrl Pts',(-18.3836214170162,-12.975951137194,122.697292179863)) ;
#14569 = CARTESIAN_POINT('Ctrl Pts',(-18.3856052009132,-12.9757888267649,
122.6944506383)) ;
#14570 = CARTESIAN_POINT('Ctrl Pts',(-18.3868793990702,-12.9756849888592,
122.692635804345)) ;
#14571 = CARTESIAN_POINT('Ctrl Pts',(-18.3885619414863,-12.9755484216114,
122.690252876268)) ;
#14572 = CARTESIAN_POINT('Ctrl Pts',(-18.3889659424946,-12.9755156712703,
122.68968172152)) ;
#14573 = CARTESIAN_POINT('Ctrl Pts',(-18.4095513146084,-12.9738490210497,
122.660630998101)) ;
#14574 = CARTESIAN_POINT('Ctrl Pts',(-18.4309165761555,-12.9722230114565,
122.633008445789)) ;
#14575 = CARTESIAN_POINT('Ctrl Pts',(-18.4574777499708,-12.9703218249028,
122.601489062063)) ;
#14576 = CARTESIAN_POINT('Ctrl Pts',(-18.4615817755378,-12.9700311986185,
122.596693127422)) ;
#14577 = CARTESIAN_POINT('Ctrl Pts',(-18.4680875489468,-12.9695753349817,
122.589206080453)) ;
#14578 = CARTESIAN_POINT('Ctrl Pts',(-18.4704649068005,-12.969409749005,122.586493940138)) ;
#14579 = CARTESIAN_POINT('Ctrl Pts',(-18.4747039860114,-12.96911624171,122.581699924995)) ;
#14580 = CARTESIAN_POINT('Ctrl Pts',(-18.4765610072051,-12.9689882528876,
122.57961393174)) ;
#14581 = CARTESIAN_POINT('Ctrl Pts',(-18.4807071325828,-12.9687037920801,
122.57498789679)) ;
#14582 = CARTESIAN_POINT('Ctrl Pts',(-18.4829997009781,-12.9685473722279,
122.572450987117)) ;
#14583 = CARTESIAN_POINT('Ctrl Pts',(-18.4891499840908,-12.9681300395952,
122.565701092549)) ;
#14584 = CARTESIAN_POINT('Ctrl Pts',(-18.4930262244294,-12.9678694026981,
122.561505083046)) ;
#14585 = CARTESIAN_POINT('Ctrl Pts',(-18.5018871512243,-12.9672788868826,
122.552044122779)) ;
#14586 = CARTESIAN_POINT('Ctrl Pts',(-18.5068891610307,-12.966949267643,122.546795666759)) ;
#14587 = CARTESIAN_POINT('Ctrl Pts',(-18.5226418805273,-12.9659224157567,
122.530552162321)) ;
#14588 = CARTESIAN_POINT('Ctrl Pts',(-18.5335500387934,-12.9652274025998,
122.519711738178)) ;
#14589 = CARTESIAN_POINT('Ctrl Pts',(-18.5685045394797,-12.9630457268317,
122.486233354646)) ;
#14590 = CARTESIAN_POINT('Ctrl Pts',(-18.5932493131368,-12.9615673047214,
122.464345570966)) ;
#14591 = CARTESIAN_POINT('Ctrl Pts',(-18.6206388709681,-12.9599777408857,
122.44198816693)) ;
#14592 = CARTESIAN_POINT('Ctrl Pts',(-18.6224501432689,-12.9598728304576,
122.440518100581)) ;
#14593 = CARTESIAN_POINT('Ctrl Pts',(-18.6499022235741,-12.9582857807891,
122.418364599517)) ;
#14594 = CARTESIAN_POINT('Ctrl Pts',(-18.6763462679647,-12.9567933113416,
122.398698032973)) ;
#14595 = CARTESIAN_POINT('Ctrl Pts',(-18.7133702272744,-12.9547495281684,
122.373372087445)) ;
#14596 = CARTESIAN_POINT('Ctrl Pts',(-18.7233003775803,-12.9542057289873,
122.366785859565)) ;
#14597 = CARTESIAN_POINT('Ctrl Pts',(-18.7409818158024,-12.9532450486145,
122.355419170495)) ;
#14598 = CARTESIAN_POINT('Ctrl Pts',(-18.7486940463885,-12.9528285133464,
122.35057954299)) ;
#14599 = CARTESIAN_POINT('Ctrl Pts',(-18.7622664335023,-12.9520997667497,
122.34226779189)) ;
#14600 = CARTESIAN_POINT('Ctrl Pts',(-18.7681033879392,-12.951787726319,122.338758500398)) ;
#14601 = CARTESIAN_POINT('Ctrl Pts',(-18.7829311162439,-12.9509984493496,
122.330007960016)) ;
#14602 = CARTESIAN_POINT('Ctrl Pts',(-18.7919591987644,-12.9505210172755,
122.324830966065)) ;
#14603 = CARTESIAN_POINT('Ctrl Pts',(-18.8137769629896,-12.949374552362,122.312679446884)) ;
#14604 = CARTESIAN_POINT('Ctrl Pts',(-18.8266259755181,-12.9487053124731,
122.305814580976)) ;
#14605 = CARTESIAN_POINT('Ctrl Pts',(-18.8637275526131,-12.9467890850053,
122.286818262751)) ;
#14606 = CARTESIAN_POINT('Ctrl Pts',(-18.8882587671795,-12.9455415981957,
122.275249280256)) ;
#14607 = CARTESIAN_POINT('Ctrl Pts',(-18.9655149318505,-12.9416657207147,
122.241842280331)) ;
#14608 = CARTESIAN_POINT('Ctrl Pts',(-19.0193720611548,-12.9390347776241,
122.222809309062)) ;
#14609 = CARTESIAN_POINT('Ctrl Pts',(-19.0998063954986,-12.9351796273224,
122.200439281251)) ;
#14610 = CARTESIAN_POINT('Ctrl Pts',(-19.1254912117884,-12.9339608305303,
122.194166204317)) ;
#14611 = CARTESIAN_POINT('Ctrl Pts',(-19.1611221700657,-12.9322863484592,
122.186652674809)) ;
#14612 = CARTESIAN_POINT('Ctrl Pts',(-19.1709130152423,-12.9318278759446,
122.184710251597)) ;
#14613 = CARTESIAN_POINT('Ctrl Pts',(-19.1880786543583,-12.9310267643606,
122.181517926934)) ;
#14614 = CARTESIAN_POINT('Ctrl Pts',(-19.1954433497235,-12.9306839207001,
122.180216567884)) ;
#14615 = CARTESIAN_POINT('Ctrl Pts',(-19.2106804647844,-12.9299762523928,
122.177664926839)) ;
#14616 = CARTESIAN_POINT('Ctrl Pts',(-19.2185540627371,-12.929611481886,122.176423695558)) ;
#14617 = CARTESIAN_POINT('Ctrl Pts',(-19.2267892434218,-12.9292308121882,
122.175206068492)) ;
#14618 = CARTESIAN_POINT('Ctrl Pts',(-19.2271395021093,-12.9292146231502,
122.175154432433)) ;
#14619 = CARTESIAN_POINT('Ctrl Pts',(-19.2278650919944,-12.9291810895227,
122.175047779008)) ;
#14620 = CARTESIAN_POINT('Ctrl Pts',(-19.2282404264384,-12.9291637450193,
122.174992783667)) ;
#14621 = CARTESIAN_POINT('Ctrl Pts',(-19.2290188956756,-12.9291277751127,
122.174879081532)) ;
#14622 = CARTESIAN_POINT('Ctrl Pts',(-19.2294220342588,-12.9291091498134,
122.17482040094)) ;
#14623 = CARTESIAN_POINT('Ctrl Pts',(-19.2302591420934,-12.9290704791468,
122.174698969938)) ;
#14624 = CARTESIAN_POINT('Ctrl Pts',(-19.230693115835,-12.9290504339025,122.17463625077)) ;
#14625 = CARTESIAN_POINT('Ctrl Pts',(-19.2315952603674,-12.9290087688394,
122.174506354742)) ;
#14626 = CARTESIAN_POINT('Ctrl Pts',(-19.2320634365575,-12.9289871491633,
122.17443921521)) ;
#14627 = CARTESIAN_POINT('Ctrl Pts',(-19.2326798965397,-12.9289586856092,
122.174351167854)) ;
#14628 = CARTESIAN_POINT('Ctrl Pts',(-19.2328281457554,-12.9289518408366,
122.174330020993)) ;
#14629 = CARTESIAN_POINT('Ctrl Pts',(-19.2432580248853,-12.9284703053083,
122.172844173597)) ;
#14630 = CARTESIAN_POINT('Ctrl Pts',(-19.2535575246023,-12.927996125137,122.171507635619)) ;
#14631 = CARTESIAN_POINT('Ctrl Pts',(-19.2833886519586,-12.9266258326528,
122.168013969547)) ;
#14632 = CARTESIAN_POINT('Ctrl Pts',(-19.3029560120388,-12.9257308843601,
122.166188833968)) ;
#14633 = CARTESIAN_POINT('Ctrl Pts',(-19.3494351787517,-12.9236089078578,
122.162956733505)) ;
#14634 = CARTESIAN_POINT('Ctrl Pts',(-19.3763653699954,-12.9223825329253,
122.161957179838)) ;
#14635 = CARTESIAN_POINT('Ctrl Pts',(-19.4095786774992,-12.920864405504,122.161798668492)) ;
#14636 = CARTESIAN_POINT('Ctrl Pts',(-19.4158508302743,-12.9205774594865,
122.161815942134)) ;
#14637 = CARTESIAN_POINT('Ctrl Pts',(-19.424764287832,-12.9201691529254,122.161907579719)) ;
#14638 = CARTESIAN_POINT('Ctrl Pts',(-19.4274059076983,-12.9200480805764,
122.161943113438)) ;
#14639 = CARTESIAN_POINT('Ctrl Pts',(-19.433577950039,-12.9197650267835,122.162045707723)) ;
#14640 = CARTESIAN_POINT('Ctrl Pts',(-19.4371082377077,-12.919602993327,122.162119353658)) ;
#14641 = CARTESIAN_POINT('Ctrl Pts',(-19.4444216276046,-12.9192670049565,
122.162302924444)) ;
#14642 = CARTESIAN_POINT('Ctrl Pts',(-19.448204628969,-12.9190930270137,122.162415073944)) ;
#14643 = CARTESIAN_POINT('Ctrl Pts',(-19.4647608464062,-12.9183307874337,
122.162981161356)) ;
#14644 = CARTESIAN_POINT('Ctrl Pts',(-19.4775271204573,-12.9177409559588,
122.163613810563)) ;
#14645 = CARTESIAN_POINT('Ctrl Pts',(-19.5167179285795,-12.9159257189815,
122.16615901209)) ;
#14646 = CARTESIAN_POINT('Ctrl Pts',(-19.5430931910481,-12.9146979116109,
122.16871590326)) ;
#14647 = CARTESIAN_POINT('Ctrl Pts',(-19.5943413384001,-12.9123067125982,
122.175334065345)) ;
#14648 = CARTESIAN_POINT('Ctrl Pts',(-19.6192124398147,-12.9111436626271,
122.17931315571)) ;
#14649 = CARTESIAN_POINT('Ctrl Pts',(-19.6510624441114,-12.9096515318053,
122.185400903659)) ;
#14650 = CARTESIAN_POINT('Ctrl Pts',(-19.6581664503071,-12.9093185273144,
122.186822873812)) ;
#14651 = CARTESIAN_POINT('Ctrl Pts',(-19.6703540734346,-12.9087468532339,
122.18937279983)) ;
#14652 = CARTESIAN_POINT('Ctrl Pts',(-19.6754437342661,-12.9085080046585,
122.190470908064)) ;
#14653 = CARTESIAN_POINT('Ctrl Pts',(-19.6856423385317,-12.9080291478141,
122.192738063472)) ;
#14654 = CARTESIAN_POINT('Ctrl Pts',(-19.6907510886693,-12.9077891469546,
122.193907505581)) ;
#14655 = CARTESIAN_POINT('Ctrl Pts',(-19.6959008113091,-12.9075470716328,
122.19512045997)) ;
#14656 = CARTESIAN_POINT('Ctrl Pts',(-19.6959492799863,-12.9075447932305,
122.195131879232)) ;
#14657 = CARTESIAN_POINT('Ctrl Pts',(-19.6960468120107,-12.9075402084448,
122.195154864015)) ;
#14658 = CARTESIAN_POINT('Ctrl Pts',(-19.6960958755598,-12.9075379020515,
122.195166429657)) ;
#14659 = CARTESIAN_POINT('Ctrl Pts',(-19.6961946333434,-12.9075332595898,
122.195189715919)) ;
#14660 = CARTESIAN_POINT('Ctrl Pts',(-19.6962443272368,-12.9075309235369,
122.195201436538)) ;
#14661 = CARTESIAN_POINT('Ctrl Pts',(-19.6963443822194,-12.9075262200386,
122.195225041611)) ;
#14662 = CARTESIAN_POINT('Ctrl Pts',(-19.6963947433603,-12.9075238525903,
122.195236926163)) ;
#14663 = CARTESIAN_POINT('Ctrl Pts',(-19.6964961705905,-12.9075190845251,
122.195260868275)) ;
#14664 = CARTESIAN_POINT('Ctrl Pts',(-19.6965472363417,-12.9075166839237,
122.195272925848)) ;
#14665 = CARTESIAN_POINT('Ctrl Pts',(-19.6966501111315,-12.9075118477487,
122.195297223336)) ;
#14666 = CARTESIAN_POINT('Ctrl Pts',(-19.6967019206264,-12.9075094121531,
122.195309463459)) ;
#14667 = CARTESIAN_POINT('Ctrl Pts',(-19.6968063228351,-12.9075045041113,
122.195334135785)) ;
#14668 = CARTESIAN_POINT('Ctrl Pts',(-19.6968589155912,-12.9075020316625,
122.195346568104)) ;
#14669 = CARTESIAN_POINT('Ctrl Pts',(-19.6969649258501,-12.9074970479603,
122.195371634962)) ;
#14670 = CARTESIAN_POINT('Ctrl Pts',(-19.6970183430982,-12.9074945367184,
122.195384269554)) ;
#14671 = CARTESIAN_POINT('Ctrl Pts',(-19.6971260448847,-12.9074894734284,
122.195409751368)) ;
#14672 = CARTESIAN_POINT('Ctrl Pts',(-19.6971803293735,-12.9074869213822,
122.195422598699)) ;
#14673 = CARTESIAN_POINT('Ctrl Pts',(-19.6972898096683,-12.9074817744119,
122.195448516779)) ;
#14674 = CARTESIAN_POINT('Ctrl Pts',(-19.6973450053305,-12.907479179494,122.195461587624)) ;
#14675 = CARTESIAN_POINT('Ctrl Pts',(-19.704265524275,-12.9071538223972,122.197100928202)) ;
#14676 = CARTESIAN_POINT('Ctrl Pts',(-19.7111169724853,-12.9068314400042,
122.198785293131)) ;
#14677 = CARTESIAN_POINT('Ctrl Pts',(-19.7263062321166,-12.9061159953381,
122.202656089544)) ;
#14678 = CARTESIAN_POINT('Ctrl Pts',(-19.734636437213,-12.9057231274384,122.204870941649)) ;
#14679 = CARTESIAN_POINT('Ctrl Pts',(-19.7584528572146,-12.9045980652846,
122.211467790609)) ;
#14680 = CARTESIAN_POINT('Ctrl Pts',(-19.7738782638569,-12.9038671703928,
122.216062947165)) ;
#14681 = CARTESIAN_POINT('Ctrl Pts',(-19.8516783300404,-12.9001633362013,
122.24088471048)) ;
#14682 = CARTESIAN_POINT('Ctrl Pts',(-19.9124807820148,-12.8971994397584,
122.265698950611)) ;
#14683 = CARTESIAN_POINT('Ctrl Pts',(-19.9933469057756,-12.8930709015398,
122.306382565535)) ;
#14684 = CARTESIAN_POINT('Ctrl Pts',(-20.0152975841486,-12.8919314023757,
122.318262375764)) ;
#14685 = CARTESIAN_POINT('Ctrl Pts',(-20.0508343508998,-12.8900519423772,
122.338893824642)) ;
#14686 = CARTESIAN_POINT('Ctrl Pts',(-20.0646325832518,-12.8893132135106,
122.347265988289)) ;
#14687 = CARTESIAN_POINT('Ctrl Pts',(-20.0889086065258,-12.8879962232401,
122.362646520013)) ;
#14688 = CARTESIAN_POINT('Ctrl Pts',(-20.0994498145624,-12.8874183586131,
122.369550640215)) ;
#14689 = CARTESIAN_POINT('Ctrl Pts',(-20.1199539244083,-12.8862817600257,
122.383427588994)) ;
#14690 = CARTESIAN_POINT('Ctrl Pts',(-20.1299230498108,-12.8857231260621,
122.390388779537)) ;
#14691 = CARTESIAN_POINT('Ctrl Pts',(-20.1510262187234,-12.8845268629432,
122.405587353481)) ;
#14692 = CARTESIAN_POINT('Ctrl Pts',(-20.1621281300676,-12.883889129219,122.413866585721)) ;
#14693 = CARTESIAN_POINT('Ctrl Pts',(-20.1880618963314,-12.8823780137799,
122.433885745853)) ;
#14694 = CARTESIAN_POINT('Ctrl Pts',(-20.2027693373749,-12.8815039618097,
122.445781207129)) ;
#14695 = CARTESIAN_POINT('Ctrl Pts',(-20.2422270825019,-12.8791075192343,
122.479204108083)) ;
#14696 = CARTESIAN_POINT('Ctrl Pts',(-20.2664088268576,-12.8775784849994,
122.50137903495)) ;
#14697 = CARTESIAN_POINT('Ctrl Pts',(-20.3143596103905,-12.8744327100056,
122.548956005798)) ;
#14698 = CARTESIAN_POINT('Ctrl Pts',(-20.3379978085208,-12.8728190552624,
122.574451495325)) ;
#14699 = CARTESIAN_POINT('Ctrl Pts',(-20.3651938259588,-12.8708871736827,
122.606354680304)) ;
#14700 = CARTESIAN_POINT('Ctrl Pts',(-20.369797483671,-12.870557326814,122.611850216361)) ;
#14701 = CARTESIAN_POINT('Ctrl Pts',(-20.3768479368778,-12.8700477093013,
122.620415183956)) ;
#14702 = CARTESIAN_POINT('Ctrl Pts',(-20.379327966626,-12.869867575701,122.623457034667)) ;
#14703 = CARTESIAN_POINT('Ctrl Pts',(-20.3842477556619,-12.8695084663496,
122.629549708395)) ;
#14704 = CARTESIAN_POINT('Ctrl Pts',(-20.3866876218531,-12.8693294911164,
122.632600388911)) ;
#14705 = CARTESIAN_POINT('Ctrl Pts',(-20.391486102151,-12.8689757270967,122.638658155829)) ;
#14706 = CARTESIAN_POINT('Ctrl Pts',(-20.3938453055434,-12.8688009335381,
122.641664721437)) ;
#14707 = CARTESIAN_POINT('Ctrl Pts',(-20.3991777528262,-12.8684038553865,
122.648524933948)) ;
#14708 = CARTESIAN_POINT('Ctrl Pts',(-20.4021423534296,-12.8681816650298,
122.652385225493)) ;
#14709 = CARTESIAN_POINT('Ctrl Pts',(-20.4179046597561,-12.8669924500009,
122.673159842202)) ;
#14710 = CARTESIAN_POINT('Ctrl Pts',(-20.4302929158171,-12.8660298218524,
122.690380615241)) ;
#14711 = CARTESIAN_POINT('Ctrl Pts',(-20.4558607530719,-12.8639748920025,
122.727900792871)) ;
#14712 = CARTESIAN_POINT('Ctrl Pts',(-20.4689011499024,-12.8628838738838,
122.748284510883)) ;
#14713 = CARTESIAN_POINT('Ctrl Pts',(-20.4960531297929,-12.8604999761191,
122.79357028138)) ;
#14714 = CARTESIAN_POINT('Ctrl Pts',(-20.5099175272468,-12.8592058092289,
122.818604125775)) ;
#14715 = CARTESIAN_POINT('Ctrl Pts',(-20.5278103056523,-12.857410504853,122.853702410417)) ;
#14716 = CARTESIAN_POINT('Ctrl Pts',(-20.5325850941712,-12.8569179869799,
122.863376047395)) ;
#14717 = CARTESIAN_POINT('Ctrl Pts',(-20.5411855853415,-12.8560055498111,
122.881384124822)) ;
#14718 = CARTESIAN_POINT('Ctrl Pts',(-20.5450459528377,-12.8555858504352,
122.889701222488)) ;
#14719 = CARTESIAN_POINT('Ctrl Pts',(-20.5527611804059,-12.8547258746532,
122.906814124024)) ;
#14720 = CARTESIAN_POINT('Ctrl Pts',(-20.5566068930768,-12.8542855922374,
122.915613404169)) ;
#14721 = CARTESIAN_POINT('Ctrl Pts',(-20.5718381409455,-12.8524934115106,
122.951587685943)) ;
#14722 = CARTESIAN_POINT('Ctrl Pts',(-20.5823591340654,-12.8511406227468,
122.979107528826)) ;
#14723 = CARTESIAN_POINT('Ctrl Pts',(-20.5919012301394,-12.8497876110192,
123.006982719845)) ;
#14724 = CARTESIAN_POINT('Ctrl Pts',(-20.591897994858,-12.8497880697573,123.006973268786)) ;
#14725 = CARTESIAN_POINT('Ctrl Pts',(-20.6111184683608,-12.8470627224272,
123.063121767626)) ;
#14726 = CARTESIAN_POINT('Ctrl Pts',(-20.6263167775151,-12.8443459906656,
123.12056761031)) ;
#14727 = CARTESIAN_POINT('Ctrl Pts',(-20.6404254348758,-12.8408729354201,
123.194951409159)) ;
#14728 = CARTESIAN_POINT('Ctrl Pts',(-20.6431587032736,-12.8401219927567,
123.211085880344)) ;
#14729 = CARTESIAN_POINT('Ctrl Pts',(-20.6485794869424,-12.8384343525263,
123.24740073539)) ;
#14730 = CARTESIAN_POINT('Ctrl Pts',(-20.6510923700098,-12.8374973655753,
123.267602520437)) ;
#14731 = CARTESIAN_POINT('Ctrl Pts',(-20.6551772941716,-12.8356010116792,
123.308592176691)) ;
#14732 = CARTESIAN_POINT('Ctrl Pts',(-20.6567249160465,-12.8346419398219,
123.329376219405)) ;
#14733 = CARTESIAN_POINT('Ctrl Pts',(-20.6583609785053,-12.8331162334971,
123.362521647017)) ;
#14734 = CARTESIAN_POINT('Ctrl Pts',(-20.6587869472194,-12.8325489975594,
123.374862420184)) ;
#14735 = CARTESIAN_POINT('Ctrl Pts',(-20.6592477243384,-12.8314746058903,
123.398264816964)) ;
#14736 = CARTESIAN_POINT('Ctrl Pts',(-20.6593186805196,-12.830967401308,123.409324560519)) ;
#14737 = CARTESIAN_POINT('Ctrl Pts',(-20.6591661534216,-12.8299478594391,
123.431572739217)) ;
#14738 = CARTESIAN_POINT('Ctrl Pts',(-20.658939214423,-12.8294355778214,123.442760157749)) ;
#14739 = CARTESIAN_POINT('Ctrl Pts',(-20.6575861303244,-12.827598841482,123.482884715425)) ;
#14740 = CARTESIAN_POINT('Ctrl Pts',(-20.6556047333337,-12.8262772621163,
123.511783798392)) ;
#14741 = CARTESIAN_POINT('Ctrl Pts',(-20.6507140711558,-12.8241107008861,
123.559004657467)) ;
#14742 = CARTESIAN_POINT('Ctrl Pts',(-20.6483977097181,-12.8232659356874,
123.577376652466)) ;
#14743 = CARTESIAN_POINT('Ctrl Pts',(-20.6448453939834,-12.8221626324877,
123.601262802907)) ;
#14744 = CARTESIAN_POINT('Ctrl Pts',(-20.6439790072615,-12.8219051452136,
123.606829565049)) ;
#14745 = CARTESIAN_POINT('Ctrl Pts',(-20.6418443054908,-12.8212967745573,
123.619960758218)) ;
#14746 = CARTESIAN_POINT('Ctrl Pts',(-20.6405439435258,-12.8209457839077,
123.627519741223)) ;
#14747 = CARTESIAN_POINT('Ctrl Pts',(-20.6381883339577,-12.8203415746451,
123.64049687)) ;
#14748 = CARTESIAN_POINT('Ctrl Pts',(-20.6371666138787,-12.820088541863,123.645920880265)) ;
#14749 = CARTESIAN_POINT('Ctrl Pts',(-20.6348819041793,-12.8195414167891,
123.657623135203)) ;
#14750 = CARTESIAN_POINT('Ctrl Pts',(-20.6336065260582,-12.8192472270464,
123.663898787321)) ;
#14751 = CARTESIAN_POINT('Ctrl Pts',(-20.6272779984606,-12.8178391551606,
123.693857594239)) ;
#14752 = CARTESIAN_POINT('Ctrl Pts',(-20.6215855761488,-12.8167219894872,
123.717400325192)) ;
#14753 = CARTESIAN_POINT('Ctrl Pts',(-20.609868590585,-12.8146679819657,123.760355363193)) ;
#14754 = CARTESIAN_POINT('Ctrl Pts',(-20.60404755338,-12.81373140255,123.77981487948)) ;
#14755 = CARTESIAN_POINT('Ctrl Pts',(-20.5944667169948,-12.8123076232002,
123.809214252221)) ;
#14756 = CARTESIAN_POINT('Ctrl Pts',(-20.5910500584737,-12.8118194031044,
123.819262284889)) ;
#14757 = CARTESIAN_POINT('Ctrl Pts',(-20.5848732477587,-12.8109694296603,
123.83669600002)) ;
#14758 = CARTESIAN_POINT('Ctrl Pts',(-20.5821704069237,-12.8106074643119,
123.844101334191)) ;
#14759 = CARTESIAN_POINT('Ctrl Pts',(-20.5765619710992,-12.8098759256259,
123.859027595902)) ;
#14760 = CARTESIAN_POINT('Ctrl Pts',(-20.5736532958038,-12.8095063835442,
123.866546976148)) ;
#14761 = CARTESIAN_POINT('Ctrl Pts',(-20.5671289983014,-12.808698354596,123.882940172802)) ;
#14762 = CARTESIAN_POINT('Ctrl Pts',(-20.5634836714251,-12.8082600277093,
123.891801627255)) ;
#14763 = CARTESIAN_POINT('Ctrl Pts',(-20.5442239905619,-12.8060090510775,
123.937131641893)) ;
#14764 = CARTESIAN_POINT('Ctrl Pts',(-20.5269818522385,-12.8042053158095,
123.972883839771)) ;
#14765 = CARTESIAN_POINT('Ctrl Pts',(-20.5037351473603,-12.8019843312899,
124.015746122103)) ;
#14766 = CARTESIAN_POINT('Ctrl Pts',(-20.4993143935588,-12.8015701363743,
124.023689128243)) ;
#14767 = CARTESIAN_POINT('Ctrl Pts',(-20.4895808701211,-12.8006747773791,
124.040737552588)) ;
#14768 = CARTESIAN_POINT('Ctrl Pts',(-20.4842387633027,-12.8001935162605,
124.049825403061)) ;
#14769 = CARTESIAN_POINT('Ctrl Pts',(-20.4759764565303,-12.7994633905796,
124.063482603025)) ;
#14770 = CARTESIAN_POINT('Ctrl Pts',(-20.4731404129509,-12.7992151917061,
124.068102326436)) ;
#14771 = CARTESIAN_POINT('Ctrl Pts',(-20.4667137767816,-12.7986581674899,
124.078419753693)) ;
#14772 = CARTESIAN_POINT('Ctrl Pts',(-20.4631070056883,-12.7983492405114,
124.084107183854)) ;
#14773 = CARTESIAN_POINT('Ctrl Pts',(-20.4490991301561,-12.7971635698918,
124.105806135454)) ;
#14774 = CARTESIAN_POINT('Ctrl Pts',(-20.4383776607561,-12.7962853555577,
124.121607693117)) ;
#14775 = CARTESIAN_POINT('Ctrl Pts',(-20.414170942734,-12.7943657812944,124.155582065262)) ;
#14776 = CARTESIAN_POINT('Ctrl Pts',(-20.400545607209,-12.7933246556129,124.17364696391)) ;
#14777 = CARTESIAN_POINT('Ctrl Pts',(-20.3785548314267,-12.7917035889498,
124.201213523587)) ;
#14778 = CARTESIAN_POINT('Ctrl Pts',(-20.3705226732172,-12.7911229375677,
124.210974786593)) ;
#14779 = CARTESIAN_POINT('Ctrl Pts',(-20.355315148532,-12.7900442150157,124.228895029304)) ;
#14780 = CARTESIAN_POINT('Ctrl Pts',(-20.3481787790495,-12.7895460575861,
124.237085537754)) ;
#14781 = CARTESIAN_POINT('Ctrl Pts',(-20.3332879201031,-12.7885225946496,
124.253732790805)) ;
#14782 = CARTESIAN_POINT('Ctrl Pts',(-20.3255219236296,-12.7879973835778,
124.262177893759)) ;
#14783 = CARTESIAN_POINT('Ctrl Pts',(-20.3003883323565,-12.7863236944491,
124.288765233842)) ;
#14784 = CARTESIAN_POINT('Ctrl Pts',(-20.2825897784024,-12.785177190022,124.30649151298)) ;
#14785 = CARTESIAN_POINT('Ctrl Pts',(-20.2510111217323,-12.7832012383649,
124.336101102422)) ;
#14786 = CARTESIAN_POINT('Ctrl Pts',(-20.2374833845805,-12.7823719214179,
124.348241947181)) ;
#14787 = CARTESIAN_POINT('Ctrl Pts',(-20.2173881470175,-12.7811616242106,
124.365500797064)) ;
#14788 = CARTESIAN_POINT('Ctrl Pts',(-20.2110266432474,-12.7807815260881,
124.37085503483)) ;
#14789 = CARTESIAN_POINT('Ctrl Pts',(-20.2044183990009,-12.7803895702814,
124.376305238775)) ;
#14790 = CARTESIAN_POINT('Ctrl Pts',(-20.2042245444069,-12.7803780746881,
124.376465023782)) ;
#14791 = CARTESIAN_POINT('Ctrl Pts',(-20.2038946797953,-12.7803585179886,
124.376736748338)) ;
#14792 = CARTESIAN_POINT('Ctrl Pts',(-20.2037586943496,-12.780350457055,124.376848717523)) ;
#14793 = CARTESIAN_POINT('Ctrl Pts',(-20.2031109720567,-12.7803120673327,
124.377381816493)) ;
#14794 = CARTESIAN_POINT('Ctrl Pts',(-20.2025989239471,-12.7802817364031,
124.377802568054)) ;
#14795 = CARTESIAN_POINT('Ctrl Pts',(-20.196974407164,-12.7799487620146,124.382416762939)) ;
#14796 = CARTESIAN_POINT('Ctrl Pts',(-20.1918290918141,-12.7796458770426,
124.38656997156)) ;
#14797 = CARTESIAN_POINT('Ctrl Pts',(-20.1796522912951,-12.7789329269418,
124.396240314173)) ;
#14798 = CARTESIAN_POINT('Ctrl Pts',(-20.172594122113,-12.7785226886753,124.401723237862)) ;
#14799 = CARTESIAN_POINT('Ctrl Pts',(-20.141547880952,-12.7767316008984,124.425311071857)) ;
#14800 = CARTESIAN_POINT('Ctrl Pts',(-20.1169701138398,-12.7753483534963,
124.442623224899)) ;
#14801 = CARTESIAN_POINT('Ctrl Pts',(-20.0785151148125,-12.7732373228449,
124.467686109091)) ;
#14802 = CARTESIAN_POINT('Ctrl Pts',(-20.0650744502059,-12.7725088934285,
124.476086242062)) ;
#14803 = CARTESIAN_POINT('Ctrl Pts',(-20.0410946360899,-12.7712253596146,
124.490446335023)) ;
#14804 = CARTESIAN_POINT('Ctrl Pts',(-20.0306218191546,-12.7706700450617,
124.496513018329)) ;
#14805 = CARTESIAN_POINT('Ctrl Pts',(-20.0087759546366,-12.7695220855161,
124.508747652244)) ;
#14806 = CARTESIAN_POINT('Ctrl Pts',(-19.9973919037328,-12.7689295740919,
124.514893058028)) ;
#14807 = CARTESIAN_POINT('Ctrl Pts',(-19.9660925518482,-12.7673150650081,
124.531166976599)) ;
#14808 = CARTESIAN_POINT('Ctrl Pts',(-19.945997817985,-12.7662943500498,124.540940038853)) ;
#14809 = CARTESIAN_POINT('Ctrl Pts',(-19.9047980069988,-12.7642284240287,
124.559629065831)) ;
#14810 = CARTESIAN_POINT('Ctrl Pts',(-19.883688076969,-12.7631836307977,124.568513974081)) ;
#14811 = CARTESIAN_POINT('Ctrl Pts',(-19.8535349855995,-12.7617054793112,
124.580240652778)) ;
#14812 = CARTESIAN_POINT('Ctrl Pts',(-19.8446853390475,-12.7612733408557,
124.583567244159)) ;
#14813 = CARTESIAN_POINT('Ctrl Pts',(-19.8353641904228,-12.76081963052,124.586950894893)) ;
#14814 = CARTESIAN_POINT('Ctrl Pts',(-19.8349294694028,-12.7607984736074,
124.587108429124)) ;
#14815 = CARTESIAN_POINT('Ctrl Pts',(-19.8341348059984,-12.7607598050446,
124.587395900569)) ;
#14816 = CARTESIAN_POINT('Ctrl Pts',(-19.8337748911753,-12.7607422937099,
124.587525913768)) ;
#14817 = CARTESIAN_POINT('Ctrl Pts',(-19.8331134295949,-12.760710114946,124.587764512348)) ;
#14818 = CARTESIAN_POINT('Ctrl Pts',(-19.8328119006692,-12.7606954477249,
124.587873147072)) ;
#14819 = CARTESIAN_POINT('Ctrl Pts',(-19.8322548081753,-12.7606683520074,
124.588073614102)) ;
#14820 = CARTESIAN_POINT('Ctrl Pts',(-19.8319992563856,-12.7606559236504,
124.588165479123)) ;
#14821 = CARTESIAN_POINT('Ctrl Pts',(-19.8315246761774,-12.7606328452277,
124.588335905231)) ;
#14822 = CARTESIAN_POINT('Ctrl Pts',(-19.8313056556935,-12.7606221952567,
124.588414488459)) ;
#14823 = CARTESIAN_POINT('Ctrl Pts',(-19.8308968899834,-12.7606023203299,
124.588561022311)) ;
#14824 = CARTESIAN_POINT('Ctrl Pts',(-19.830707150122,-12.7605930954353,124.588628988251)) ;
#14825 = CARTESIAN_POINT('Ctrl Pts',(-19.8303513303538,-12.7605757970804,
124.588756347906)) ;
#14826 = CARTESIAN_POINT('Ctrl Pts',(-19.830185254445,-12.7605677236746,124.588815752311)) ;
#14827 = CARTESIAN_POINT('Ctrl Pts',(-19.8298723718533,-12.7605525144503,
124.588927593938)) ;
#14828 = CARTESIAN_POINT('Ctrl Pts',(-19.8297255678651,-12.7605453786632,
124.588980038873)) ;
#14829 = CARTESIAN_POINT('Ctrl Pts',(-19.8294477615593,-12.76053187584,124.589079225083)) ;
#14830 = CARTESIAN_POINT('Ctrl Pts',(-19.8293167612351,-12.7605255088285,
124.589125971961)) ;
#14831 = CARTESIAN_POINT('Ctrl Pts',(-19.8290677964725,-12.7605134089227,
124.589214767077)) ;
#14832 = CARTESIAN_POINT('Ctrl Pts',(-19.8289498335817,-12.7605076760504,
124.589256819429)) ;
#14833 = CARTESIAN_POINT('Ctrl Pts',(-19.8284960393133,-12.7604856229994,
124.589418514769)) ;
#14834 = CARTESIAN_POINT('Ctrl Pts',(-19.8281601627657,-12.7604693022374,
124.589538031922)) ;
#14835 = CARTESIAN_POINT('Ctrl Pts',(-19.8215533261999,-12.7601483016356,
124.591885802008)) ;
#14836 = CARTESIAN_POINT('Ctrl Pts',(-19.8152647384488,-12.7598433916911,
124.594064076999)) ;
#14837 = CARTESIAN_POINT('Ctrl Pts',(-19.8000690057879,-12.7591079026105,
124.599192115322)) ;
#14838 = CARTESIAN_POINT('Ctrl Pts',(-19.791145477876,-12.7586771055641,124.602092006426)) ;
#14839 = CARTESIAN_POINT('Ctrl Pts',(-19.7531986697255,-12.7568503150416,
124.613952974159)) ;
#14840 = CARTESIAN_POINT('Ctrl Pts',(-19.7238865152444,-12.7554521746053,
124.621955051919)) ;
#14841 = CARTESIAN_POINT('Ctrl Pts',(-19.6808877986279,-12.7534217475114,
124.632025447434)) ;
#14842 = CARTESIAN_POINT('Ctrl Pts',(-19.667412410108,-12.7527882655239,124.634947126119)) ;
#14843 = CARTESIAN_POINT('Ctrl Pts',(-19.6415240070757,-12.7515764002764,
124.640113254841)) ;
#14844 = CARTESIAN_POINT('Ctrl Pts',(-19.629119919105,-12.7509979946013,124.642393921712)) ;
#14845 = CARTESIAN_POINT('Ctrl Pts',(-19.605274756875,-12.7498899647433,124.64640614307)) ;
#14846 = CARTESIAN_POINT('Ctrl Pts',(-19.5938399686473,-12.7493603118689,
124.648167307998)) ;
#14847 = CARTESIAN_POINT('Ctrl Pts',(-19.558082345876,-12.7477085470678,124.653167494658)) ;
#14848 = CARTESIAN_POINT('Ctrl Pts',(-19.5336875014784,-12.7465882481635,
124.655849287354)) ;
#14849 = CARTESIAN_POINT('Ctrl Pts',(-19.4945147079598,-12.744794221295,124.65899183605)) ;
#14850 = CARTESIAN_POINT('Ctrl Pts',(-19.4797801406896,-12.7441204923527,
124.659911539982)) ;
#14851 = CARTESIAN_POINT('Ctrl Pts',(-19.4580664522149,-12.7431277471803,
124.660881118485)) ;
#14852 = CARTESIAN_POINT('Ctrl Pts',(-19.4510976689019,-12.7428091483195,
124.66113388505)) ;
#14853 = CARTESIAN_POINT('Ctrl Pts',(-19.4395253783455,-12.7422799063551,
124.66145669146)) ;
#14854 = CARTESIAN_POINT('Ctrl Pts',(-19.4349229434507,-12.7420693732442,
124.661559634178)) ;
#14855 = CARTESIAN_POINT('Ctrl Pts',(-19.4300767291584,-12.7418476000308,
124.66164124752)) ;
#14856 = CARTESIAN_POINT('Ctrl Pts',(-19.4298334076449,-12.7418364648781,
124.661645274134)) ;
#14857 = CARTESIAN_POINT('Ctrl Pts',(-19.4293707042464,-12.7418152896658,
124.661652796038)) ;
#14858 = CARTESIAN_POINT('Ctrl Pts',(-19.4291513226569,-12.7418052496651,
124.661656304622)) ;
#14859 = CARTESIAN_POINT('Ctrl Pts',(-19.4287335909311,-12.7417861317869,
124.661662875421)) ;
#14860 = CARTESIAN_POINT('Ctrl Pts',(-19.4285352409226,-12.7417770539518,
124.66166594818)) ;
#14861 = CARTESIAN_POINT('Ctrl Pts',(-19.4281570631425,-12.7417597456665,
124.661671716714)) ;
#14862 = CARTESIAN_POINT('Ctrl Pts',(-19.4279772354914,-12.7417515152514,
124.661674420896)) ;
#14863 = CARTESIAN_POINT('Ctrl Pts',(-19.427633933676,-12.7417358026273,124.661679509234)) ;
#14864 = CARTESIAN_POINT('Ctrl Pts',(-19.4274704595811,-12.7417283204457,
124.66168190013)) ;
#14865 = CARTESIAN_POINT('Ctrl Pts',(-19.4271579868272,-12.7417140183976,
124.661686408894)) ;
#14866 = CARTESIAN_POINT('Ctrl Pts',(-19.4270089881829,-12.7417071985514,
124.661688532191)) ;
#14867 = CARTESIAN_POINT('Ctrl Pts',(-19.4267238362295,-12.7416941466172,
124.661692544734)) ;
#14868 = CARTESIAN_POINT('Ctrl Pts',(-19.4265876831022,-12.7416879145538,
124.661694438374)) ;
#14869 = CARTESIAN_POINT('Ctrl Pts',(-19.4263268050373,-12.741675973364,124.661698024073)) ;
#14870 = CARTESIAN_POINT('Ctrl Pts',(-19.4262020801381,-12.7416702642528,
124.661699719711)) ;
#14871 = CARTESIAN_POINT('Ctrl Pts',(-19.4259628233202,-12.7416593124649,
124.661702936593)) ;
#14872 = CARTESIAN_POINT('Ctrl Pts',(-19.4258482914266,-12.7416540698004,
124.661704460765)) ;
#14873 = CARTESIAN_POINT('Ctrl Pts',(-19.425628341563,-12.7416440015434,124.661707357584)) ;
#14874 = CARTESIAN_POINT('Ctrl Pts',(-19.4255229236269,-12.7416391759616,
124.661708732637)) ;
#14875 = CARTESIAN_POINT('Ctrl Pts',(-19.4253202574757,-12.7416298986742,
124.661711350535)) ;
#14876 = CARTESIAN_POINT('Ctrl Pts',(-19.4252230090526,-12.7416254469667,
124.66171259537)) ;
#14877 = CARTESIAN_POINT('Ctrl Pts',(-19.4250358524253,-12.7416168794777,
124.661714969235)) ;
#14878 = CARTESIAN_POINT('Ctrl Pts',(-19.424945944365,-12.7416127637092,124.661716099912)) ;
#14879 = CARTESIAN_POINT('Ctrl Pts',(-19.4247727398005,-12.7416048347597,
124.661718259428)) ;
#14880 = CARTESIAN_POINT('Ctrl Pts',(-19.424689443183,-12.741601021579,124.661719289643)) ;
#14881 = CARTESIAN_POINT('Ctrl Pts',(-19.4245288178724,-12.741593668356,124.661721260203)) ;
#14882 = CARTESIAN_POINT('Ctrl Pts',(-19.4244514894822,-12.7415901283321,
124.661722201694)) ;
#14883 = CARTESIAN_POINT('Ctrl Pts',(-19.4241944601864,-12.7415783616686,
124.66172530723)) ;
#14884 = CARTESIAN_POINT('Ctrl Pts',(-19.4240147584981,-12.7415701348681,
124.661727439703)) ;
#14885 = CARTESIAN_POINT('Ctrl Pts',(-19.4236605694096,-12.7415539196717,
124.661731566376)) ;
#14886 = CARTESIAN_POINT('Ctrl Pts',(-19.4234860822174,-12.7415459312944,
124.661733562792)) ;
#14887 = CARTESIAN_POINT('Ctrl Pts',(-19.4231419025592,-12.7415301737581,
124.661737428686)) ;
#14888 = CARTESIAN_POINT('Ctrl Pts',(-19.4229722100233,-12.7415224046041,
124.661739300144)) ;
#14889 = CARTESIAN_POINT('Ctrl Pts',(-19.4226372151494,-12.7415070670136,
124.661742926417)) ;
#14890 = CARTESIAN_POINT('Ctrl Pts',(-19.4224719129676,-12.7414994985916,
124.661744682994)) ;
#14891 = CARTESIAN_POINT('Ctrl Pts',(-19.4221453083585,-12.7414845446067,
124.661748088849)) ;
#14892 = CARTESIAN_POINT('Ctrl Pts',(-19.4219840059091,-12.7414771590492,
124.661749739694)) ;
#14893 = CARTESIAN_POINT('Ctrl Pts',(-19.4216650210744,-12.7414625534245,
124.661752942583)) ;
#14894 = CARTESIAN_POINT('Ctrl Pts',(-19.4215073385547,-12.7414553333568,
124.661754496013)) ;
#14895 = CARTESIAN_POINT('Ctrl Pts',(-19.4211952222683,-12.7414410417241,
124.661757511801)) ;
#14896 = CARTESIAN_POINT('Ctrl Pts',(-19.4210407887336,-12.7414339701748,
124.661758975374)) ;
#14897 = CARTESIAN_POINT('Ctrl Pts',(-19.4207348053506,-12.7414199588746,
124.661761818479)) ;
#14898 = CARTESIAN_POINT('Ctrl Pts',(-19.4205832554236,-12.7414130191247,
124.66176319907)) ;
#14899 = CARTESIAN_POINT('Ctrl Pts',(-19.4202826773881,-12.7413992548634,
124.66176588261)) ;
#14900 = CARTESIAN_POINT('Ctrl Pts',(-19.4201336493401,-12.7413924303588,
124.661767186468)) ;
#14901 = CARTESIAN_POINT('Ctrl Pts',(-19.4198377534698,-12.7413788800386,
124.661769722362)) ;
#14902 = CARTESIAN_POINT('Ctrl Pts',(-19.4196908856624,-12.7413721542271,
124.661770955165)) ;
#14903 = CARTESIAN_POINT('Ctrl Pts',(-19.4193989456822,-12.7413587846041,
124.661773354241)) ;
#14904 = CARTESIAN_POINT('Ctrl Pts',(-19.4192538736498,-12.7413521408019,
124.661774521142)) ;
#14905 = CARTESIAN_POINT('Ctrl Pts',(-19.4189651541696,-12.7413389182103,
124.661776793219)) ;
#14906 = CARTESIAN_POINT('Ctrl Pts',(-19.4188215066021,-12.7413323394177,
124.661777898889)) ;
#14907 = CARTESIAN_POINT('Ctrl Pts',(-19.4185352540363,-12.7413192293539,
124.661780052857)) ;
#14908 = CARTESIAN_POINT('Ctrl Pts',(-19.4183926490306,-12.741312698084,124.661781101513)) ;
#14909 = CARTESIAN_POINT('Ctrl Pts',(-19.4181080838835,-12.7412996648531,
124.661783145383)) ;
#14910 = CARTESIAN_POINT('Ctrl Pts',(-19.4179661234659,-12.7412931628804,
124.661784140819)) ;
#14911 = CARTESIAN_POINT('Ctrl Pts',(-19.4176824277518,-12.7412801690196,
124.66178608178)) ;
#14912 = CARTESIAN_POINT('Ctrl Pts',(-19.4175406926215,-12.7412736771395,
124.661787027381)) ;
#14913 = CARTESIAN_POINT('Ctrl Pts',(-19.4172569990523,-12.7412606829228,
124.661788871819)) ;
#14914 = CARTESIAN_POINT('Ctrl Pts',(-19.4171150405906,-12.7412541805848,
124.66178977058)) ;
#14915 = CARTESIAN_POINT('Ctrl Pts',(-19.4168304142005,-12.7412411431805,
124.661791524104)) ;
#14916 = CARTESIAN_POINT('Ctrl Pts',(-19.4166877464522,-12.7412346081213,
124.661792378625)) ;
#14917 = CARTESIAN_POINT('Ctrl Pts',(-19.4164011667507,-12.7412214807738,
124.661794046052)) ;
#14918 = CARTESIAN_POINT('Ctrl Pts',(-19.4162572546592,-12.7412148884771,
124.661794858532)) ;
#14919 = CARTESIAN_POINT('Ctrl Pts',(-19.4159675882246,-12.7412016192506,
124.661796443867)) ;
#14920 = CARTESIAN_POINT('Ctrl Pts',(-19.4158218341684,-12.7411949423307,
124.66179721608)) ;
#14921 = CARTESIAN_POINT('Ctrl Pts',(-19.415527804632,-12.7411814727326,124.661798722435)) ;
#14922 = CARTESIAN_POINT('Ctrl Pts',(-19.4153795288802,-12.7411746800376,
124.661799455689)) ;
#14923 = CARTESIAN_POINT('Ctrl Pts',(-19.4150796704779,-12.7411609428892,
124.661800885195)) ;
#14924 = CARTESIAN_POINT('Ctrl Pts',(-19.4149280877281,-12.7411539984253,
124.661801580257)) ;
#14925 = CARTESIAN_POINT('Ctrl Pts',(-19.4146764267807,-12.7411424688468,
124.661802688435)) ;
#14926 = CARTESIAN_POINT('Ctrl Pts',(-19.4145763486713,-12.7411378838144,
124.661803117106)) ;
#14927 = CARTESIAN_POINT('Ctrl Pts',(-19.4143577102211,-12.7411278668618,
124.661804027355)) ;
#14928 = CARTESIAN_POINT('Ctrl Pts',(-19.4142391500948,-12.741122434927,124.661804504084)) ;
#14929 = CARTESIAN_POINT('Ctrl Pts',(-19.4139767884034,-12.7411104144087,
124.661805521709)) ;
#14930 = CARTESIAN_POINT('Ctrl Pts',(-19.4138329867694,-12.7411038257816,
124.661806054659)) ;
#14931 = CARTESIAN_POINT('Ctrl Pts',(-19.4135090098818,-12.7410889816924,
124.661807199458)) ;
#14932 = CARTESIAN_POINT('Ctrl Pts',(-19.4133288346815,-12.7410807261601,
124.661807797165)) ;
#14933 = CARTESIAN_POINT('Ctrl Pts',(-19.4129116967387,-12.7410616126508,
124.661809090774)) ;
#14934 = CARTESIAN_POINT('Ctrl Pts',(-19.4126747338643,-12.7410507545197,
124.66180975825)) ;
#14935 = CARTESIAN_POINT('Ctrl Pts',(-19.4122186413849,-12.7410298547295,
124.661810913275)) ;
#14936 = CARTESIAN_POINT('Ctrl Pts',(-19.4119995118601,-12.7410198131256,
124.661811410585)) ;
#14937 = CARTESIAN_POINT('Ctrl Pts',(-19.4061760536978,-12.7407529451198,
124.661823095476)) ;
#14938 = CARTESIAN_POINT('Ctrl Pts',(-19.4005717232996,-12.7404959171753,
124.661796650256)) ;
#14939 = CARTESIAN_POINT('Ctrl Pts',(-19.3885371437218,-12.7399433916313,
124.661658922666)) ;
#14940 = CARTESIAN_POINT('Ctrl Pts',(-19.3821072100128,-12.7396477965462,
124.661535703254)) ;
#14941 = CARTESIAN_POINT('Ctrl Pts',(-19.3561057532977,-12.7384508484387,
124.660836662306)) ;
#14942 = CARTESIAN_POINT('Ctrl Pts',(-19.3365481209036,-12.7375470829579,
124.659850651173)) ;
#14943 = CARTESIAN_POINT('Ctrl Pts',(-19.2991144258305,-12.7358134425116,
124.657080477771)) ;
#14944 = CARTESIAN_POINT('Ctrl Pts',(-19.2812376495889,-12.7349838439677,
124.655369583169)) ;
#14945 = CARTESIAN_POINT('Ctrl Pts',(-19.2491038960038,-12.7334905955723,
124.651593950738)) ;
#14946 = CARTESIAN_POINT('Ctrl Pts',(-19.2348339142787,-12.7328267349061,
124.64966677643)) ;
#14947 = CARTESIAN_POINT('Ctrl Pts',(-19.21213017858,-12.7317693899077,124.64620021637)) ;
#14948 = CARTESIAN_POINT('Ctrl Pts',(-19.2036734814637,-12.7313752928506,
124.644819869289)) ;
#14949 = CARTESIAN_POINT('Ctrl Pts',(-19.1886329593461,-12.730673860828,124.642205835725)) ;
#14950 = CARTESIAN_POINT('Ctrl Pts',(-19.1820436026388,-12.7303663803995,
124.641005973387)) ;
#14951 = CARTESIAN_POINT('Ctrl Pts',(-19.1691632151487,-12.7297649357601,
124.638553458616)) ;
#14952 = CARTESIAN_POINT('Ctrl Pts',(-19.1628715512888,-12.7294709590662,
124.637305225249)) ;
#14953 = CARTESIAN_POINT('Ctrl Pts',(-19.148524178448,-12.7288000686123,124.634343824607)) ;
#14954 = CARTESIAN_POINT('Ctrl Pts',(-19.1404752266585,-12.7284233258926,
124.63259935732)) ;
#14955 = CARTESIAN_POINT('Ctrl Pts',(-19.1158282873605,-12.7272682641916,
124.627001995282)) ;
#14956 = CARTESIAN_POINT('Ctrl Pts',(-19.0992913261169,-12.7264913056927,
124.622889163484)) ;
#14957 = CARTESIAN_POINT('Ctrl Pts',(-19.0511034112341,-12.7242180712362,
124.60985287223)) ;
#14958 = CARTESIAN_POINT('Ctrl Pts',(-19.019714466083,-12.7227259025544,124.600017173422)) ;
#14959 = CARTESIAN_POINT('Ctrl Pts',(-18.9795197956115,-12.7207832260973,
124.58565801372)) ;
#14960 = CARTESIAN_POINT('Ctrl Pts',(-18.9703287956385,-12.7203367556637,
124.582252200529)) ;
#14961 = CARTESIAN_POINT('Ctrl Pts',(-18.9518947179989,-12.7194358270147,
124.575173601909)) ;
#14962 = CARTESIAN_POINT('Ctrl Pts',(-18.9426535103517,-12.7189813740649,
124.571497887254)) ;
#14963 = CARTESIAN_POINT('Ctrl Pts',(-18.9252874242451,-12.7181222055062,
124.564349293078)) ;
#14964 = CARTESIAN_POINT('Ctrl Pts',(-18.9171535661215,-12.7177176241507,
124.560899772032)) ;
#14965 = CARTESIAN_POINT('Ctrl Pts',(-18.8835970301816,-12.716039662397,124.54624699214)) ;
#14966 = CARTESIAN_POINT('Ctrl Pts',(-18.8585148236061,-12.7147643904582,
124.534283997291)) ;
#14967 = CARTESIAN_POINT('Ctrl Pts',(-18.8118708653506,-12.7123525971582,
124.5100969806)) ;
#14968 = CARTESIAN_POINT('Ctrl Pts',(-18.7902330855619,-12.7112165713594,
124.498048057546)) ;
#14969 = CARTESIAN_POINT('Ctrl Pts',(-18.7293221041502,-12.7079650224653,
124.461718506287)) ;
#14970 = CARTESIAN_POINT('Ctrl Pts',(-18.6910169953789,-12.7058549056396,
124.435894588803)) ;
#14971 = CARTESIAN_POINT('Ctrl Pts',(-18.6491946069308,-12.7034521432387,
124.404196293759)) ;
#14972 = CARTESIAN_POINT('Ctrl Pts',(-18.6441900359713,-12.70316290484,124.400343131319)) ;
#14973 = CARTESIAN_POINT('Ctrl Pts',(-18.6311498776929,-12.7024045372778,
124.390144793104)) ;
#14974 = CARTESIAN_POINT('Ctrl Pts',(-18.6231626798287,-12.7019352791285,
124.383738536986)) ;
#14975 = CARTESIAN_POINT('Ctrl Pts',(-18.6079519929447,-12.7010317731049,
124.371228396891)) ;
#14976 = CARTESIAN_POINT('Ctrl Pts',(-18.6007172912797,-12.7005976199917,
124.365139239889)) ;
#14977 = CARTESIAN_POINT('Ctrl Pts',(-18.5673897488739,-12.6985755979616,
124.336436483005)) ;
#14978 = CARTESIAN_POINT('Ctrl Pts',(-18.5421720173711,-12.6969815299611,
124.312830112949)) ;
#14979 = CARTESIAN_POINT('Ctrl Pts',(-18.506446813958,-12.694631909931,124.276497027065)) ;
#14980 = CARTESIAN_POINT('Ctrl Pts',(-18.4951615683014,-12.6938750055421,
124.264557901108)) ;
#14981 = CARTESIAN_POINT('Ctrl Pts',(-18.4774842918996,-12.6926653854845,
124.245102101226)) ;
#14982 = CARTESIAN_POINT('Ctrl Pts',(-18.4709402613766,-12.6922120640712,
124.237726182475)) ;
#14983 = CARTESIAN_POINT('Ctrl Pts',(-18.459214622211,-12.6913895174003,124.224190695924)) ;
#14984 = CARTESIAN_POINT('Ctrl Pts',(-18.4540039325131,-12.691020166777,124.218057034019)) ;
#14985 = CARTESIAN_POINT('Ctrl Pts',(-18.4451026932765,-12.6903824405403,
124.207371669837)) ;
#14986 = CARTESIAN_POINT('Ctrl Pts',(-18.441384248471,-12.6901139305891,124.202843552928)) ;
#14987 = CARTESIAN_POINT('Ctrl Pts',(-18.4313015562118,-12.6893799792537,
124.190387867465)) ;
#14988 = CARTESIAN_POINT('Ctrl Pts',(-18.4250019569179,-12.6889148889622,
124.182408530454)) ;
#14989 = CARTESIAN_POINT('Ctrl Pts',(-18.4041484103778,-12.6873524172539,
124.15532158167)) ;
#14990 = CARTESIAN_POINT('Ctrl Pts',(-18.3900479733075,-12.686257440072,124.135871542147)) ;
#14991 = CARTESIAN_POINT('Ctrl Pts',(-18.3619657477377,-12.6839864835463,
124.094687868424)) ;
#14992 = CARTESIAN_POINT('Ctrl Pts',(-18.348079780465,-12.6828111822156,124.072902611342)) ;
#14993 = CARTESIAN_POINT('Ctrl Pts',(-18.3294714797503,-12.6811501530786,
124.041609770132)) ;
#14994 = CARTESIAN_POINT('Ctrl Pts',(-18.3241799145749,-12.6806670205677,
124.032448378074)) ;
#14995 = CARTESIAN_POINT('Ctrl Pts',(-18.3170899769716,-12.6800038847141,
124.019805523438)) ;
#14996 = CARTESIAN_POINT('Ctrl Pts',(-18.3151907173501,-12.679824621286,124.016381124012)) ;
#14997 = CARTESIAN_POINT('Ctrl Pts',(-18.3132919922828,-12.6796437647429,
124.012919437755)) ;
#14998 = CARTESIAN_POINT('Ctrl Pts',(-18.3132764027887,-12.6796422797065,
124.012891012935)) ;
#14999 = CARTESIAN_POINT('Ctrl Pts',(-18.313245064012,-12.6796392941861,124.012833866677)) ;
#15000 = CARTESIAN_POINT('Ctrl Pts',(-18.3132293149034,-12.6796377937163,
124.0128051455)) ;
#15001 = CARTESIAN_POINT('Ctrl Pts',(-18.3131976531155,-12.6796347769618,
124.012747399463)) ;
#15002 = CARTESIAN_POINT('Ctrl Pts',(-18.3131817403595,-12.6796332606672,
124.012718374406)) ;
#15003 = CARTESIAN_POINT('Ctrl Pts',(-18.309928903321,-12.6793232803598,124.00678460178)) ;
#15004 = CARTESIAN_POINT('Ctrl Pts',(-18.3067397500352,-12.6790145106252,
124.000853805789)) ;
#15005 = CARTESIAN_POINT('Ctrl Pts',(-18.2965035192995,-12.6780075326363,
123.981443316685)) ;
#15006 = CARTESIAN_POINT('Ctrl Pts',(-18.2896545366928,-12.6773084808496,
123.967860734372)) ;
#15007 = CARTESIAN_POINT('Ctrl Pts',(-18.2727067620015,-12.6755123331438,
123.932667321939)) ;
#15008 = CARTESIAN_POINT('Ctrl Pts',(-18.2629755326819,-12.6744151479685,
123.910886252887)) ;
#15009 = CARTESIAN_POINT('Ctrl Pts',(-18.2488486181997,-12.6727140219334,
123.87666961053)) ;
#15010 = CARTESIAN_POINT('Ctrl Pts',(-18.2440164172915,-12.6721093732509,
123.864420430033)) ;
#15011 = CARTESIAN_POINT('Ctrl Pts',(-18.2352505607384,-12.6709674769033,
123.841128311431)) ;
#15012 = CARTESIAN_POINT('Ctrl Pts',(-18.2312769522516,-12.6704301796671,
123.830101910755)) ;
#15013 = CARTESIAN_POINT('Ctrl Pts',(-18.2271859813095,-12.6698549070907,
123.818228919656)) ;
#15014 = CARTESIAN_POINT('Ctrl Pts',(-18.2269137742071,-12.6698165194887,
123.817436321487)) ;
#15015 = CARTESIAN_POINT('Ctrl Pts',(-18.2266423654705,-12.6697781342469,
123.816643453362)) ;
#15016 = CARTESIAN_POINT('Origin',(-19.4092722359532,-13.9601742359176,123.411814366564)) ;
#15017 = CARTESIAN_POINT('',(-18.2266423654684,-12.3098085062257,123.816643453356)) ;
#15018 = CARTESIAN_POINT('',(-18.2266423654683,-12.3699164408135,123.816643453356)) ;
#15019 = CARTESIAN_POINT('',(-18.2266423654683,-13.9601742359176,123.816643453356)) ;
#15020 = CARTESIAN_POINT('',(-20.4795958874297,-12.1420202715133,122.766130804778)) ;
#15021 = CARTESIAN_POINT('Ctrl Pts',(-18.2266423654683,-12.3098085062256,
123.816643453356)) ;
#15022 = CARTESIAN_POINT('Ctrl Pts',(-18.2071382676369,-12.307033814287,123.759666004243)) ;
#15023 = CARTESIAN_POINT('Ctrl Pts',(-18.1917772261847,-12.3042925781088,
123.701353432471)) ;
#15024 = CARTESIAN_POINT('Ctrl Pts',(-18.1806792743743,-12.3015413901064,
123.642160486207)) ;
#15025 = CARTESIAN_POINT('Ctrl Pts',(-18.1672798095677,-12.2982196558401,
123.570692001408)) ;
#15026 = CARTESIAN_POINT('Ctrl Pts',(-18.1601420106916,-12.2948828760311,
123.498190812995)) ;
#15027 = CARTESIAN_POINT('Ctrl Pts',(-18.1593469593498,-12.2915492218341,
123.425481955367)) ;
#15028 = CARTESIAN_POINT('Ctrl Pts',(-18.1585560485259,-12.2882329288491,
123.353151755455)) ;
#15029 = CARTESIAN_POINT('Ctrl Pts',(-18.1640449721141,-12.2849230192802,
123.280889352721)) ;
#15030 = CARTESIAN_POINT('Ctrl Pts',(-18.1757519544758,-12.2816088917125,
123.209508372437)) ;
#15031 = CARTESIAN_POINT('Ctrl Pts',(-18.1874753869865,-12.2782901072751,
123.138027090665)) ;
#15032 = CARTESIAN_POINT('Ctrl Pts',(-18.2053899848115,-12.2749858874049,
123.067700353702)) ;
#15033 = CARTESIAN_POINT('Ctrl Pts',(-18.2292933016391,-12.271654511838,122.999322288276)) ;
#15034 = CARTESIAN_POINT('Ctrl Pts',(-18.2457003206291,-12.2693678859867,
122.952388206866)) ;
#15035 = CARTESIAN_POINT('Ctrl Pts',(-18.2648929858744,-12.2670763569669,
122.906474685123)) ;
#15036 = CARTESIAN_POINT('Ctrl Pts',(-18.2867692424075,-12.2648035518453,
122.861826158003)) ;
#15037 = CARTESIAN_POINT('Ctrl Pts',(-18.2967949115885,-12.2637619480304,
122.841364185377)) ;
#15038 = CARTESIAN_POINT('Ctrl Pts',(-18.3073782405547,-12.2627238792631,
122.821180099074)) ;
#15039 = CARTESIAN_POINT('Ctrl Pts',(-18.3185073894126,-12.2616864052147,
122.801296512913)) ;
#15040 = CARTESIAN_POINT('Ctrl Pts',(-18.3538031655938,-12.2583960860471,
122.738236290088)) ;
#15041 = CARTESIAN_POINT('Ctrl Pts',(-18.3944999698131,-12.2550939574768,
122.678357271757)) ;
#15042 = CARTESIAN_POINT('Ctrl Pts',(-18.4401408613266,-12.251755308735,122.622330751288)) ;
#15043 = CARTESIAN_POINT('Ctrl Pts',(-18.4860923063305,-12.2483939428861,
122.565923010581)) ;
#15044 = CARTESIAN_POINT('Ctrl Pts',(-18.5368805148624,-12.2450746925093,
122.51363490565)) ;
#15045 = CARTESIAN_POINT('Ctrl Pts',(-18.5919290849859,-12.2417567353599,
122.466060607046)) ;
#15046 = CARTESIAN_POINT('Ctrl Pts',(-18.6467053236761,-12.2384551925155,
122.418721663818)) ;
#15047 = CARTESIAN_POINT('Ctrl Pts',(-18.7054903794304,-12.2351249633638,
122.376231244306)) ;
#15048 = CARTESIAN_POINT('Ctrl Pts',(-18.7676211251744,-12.2318073394179,
122.339068426412)) ;
#15049 = CARTESIAN_POINT('Ctrl Pts',(-18.8296626744797,-12.2284944783352,
122.301958960381)) ;
#15050 = CARTESIAN_POINT('Ctrl Pts',(-18.8948062425277,-12.2251977295908,
122.270301806749)) ;
#15051 = CARTESIAN_POINT('Ctrl Pts',(-18.9623192834267,-12.2218722717631,
122.244452786631)) ;
#15052 = CARTESIAN_POINT('Ctrl Pts',(-18.9762682192872,-12.2211851956467,
122.239112095131)) ;
#15053 = CARTESIAN_POINT('Ctrl Pts',(-18.9903117626875,-12.2204976817919,
122.234021847498)) ;
#15054 = CARTESIAN_POINT('Ctrl Pts',(-19.0044431491614,-12.2198107912305,
122.229184496079)) ;
#15055 = CARTESIAN_POINT('Ctrl Pts',(-19.0591252903551,-12.2171528321739,
122.210466111033)) ;
#15056 = CARTESIAN_POINT('Ctrl Pts',(-19.1150398834128,-12.2145206077749,
122.19556279089)) ;
#15057 = CARTESIAN_POINT('Ctrl Pts',(-19.171784845047,-12.2118736008468,122.184581813526)) ;
#15058 = CARTESIAN_POINT('Ctrl Pts',(-19.2429017173703,-12.2085561811443,
122.170819661915)) ;
#15059 = CARTESIAN_POINT('Ctrl Pts',(-19.3150804375643,-12.2052211939969,
122.163265203702)) ;
#15060 = CARTESIAN_POINT('Ctrl Pts',(-19.3875063718663,-12.2019188342252,
122.162003882036)) ;
#15061 = CARTESIAN_POINT('Ctrl Pts',(-19.4595412383739,-12.1986343057257,
122.160749370946)) ;
#15062 = CARTESIAN_POINT('Ctrl Pts',(-19.5315476603163,-12.1953483824408,
122.165724878648)) ;
#15063 = CARTESIAN_POINT('Ctrl Pts',(-19.6027233506959,-12.1920179074264,
122.176874422162)) ;
#15064 = CARTESIAN_POINT('Ctrl Pts',(-19.6746028384665,-12.1886545001058,
122.188134214267)) ;
#15065 = CARTESIAN_POINT('Ctrl Pts',(-19.7453616842655,-12.1853369611187,
122.205647863526)) ;
#15066 = CARTESIAN_POINT('Ctrl Pts',(-19.8141965675247,-12.1820193804115,
122.229217103851)) ;
#15067 = CARTESIAN_POINT('Ctrl Pts',(-19.8637631275544,-12.1796304599181,
122.246188820953)) ;
#15068 = CARTESIAN_POINT('Ctrl Pts',(-19.912213297844,-12.1772230759955,122.266259874658)) ;
#15069 = CARTESIAN_POINT('Ctrl Pts',(-19.9592604445148,-12.1748180670287,
122.289311373019)) ;
#15070 = CARTESIAN_POINT('Ctrl Pts',(-19.9773014805228,-12.1738958250558,
122.29815086577)) ;
#15071 = CARTESIAN_POINT('Ctrl Pts',(-19.9951268470279,-12.1729744116093,
122.307424039078)) ;
#15072 = CARTESIAN_POINT('Ctrl Pts',(-20.0127210039351,-12.1720549235839,
122.317122818914)) ;
#15073 = CARTESIAN_POINT('Ctrl Pts',(-20.0761584828758,-12.1687396182497,
122.352092732213)) ;
#15074 = CARTESIAN_POINT('Ctrl Pts',(-20.1364353178746,-12.1654485820723,
122.39251026949)) ;
#15075 = CARTESIAN_POINT('Ctrl Pts',(-20.1928714724686,-12.1621004922349,
122.437918973512)) ;
#15076 = CARTESIAN_POINT('Ctrl Pts',(-20.2495200548409,-12.1587398000631,
122.48349859758)) ;
#15077 = CARTESIAN_POINT('Ctrl Pts',(-20.3020832139595,-12.1553990858244,
122.533933057542)) ;
#15078 = CARTESIAN_POINT('Ctrl Pts',(-20.349966190867,-12.152108722025,122.588652849446)) ;
#15079 = CARTESIAN_POINT('Ctrl Pts',(-20.3974426337882,-12.1488462939305,
122.642908061732)) ;
#15080 = CARTESIAN_POINT('Ctrl Pts',(-20.4401335679279,-12.1455431186542,
122.701165344678)) ;
#15081 = CARTESIAN_POINT('Ctrl Pts',(-20.4775654001596,-12.1422019500507,
122.762776836536)) ;
#15082 = CARTESIAN_POINT('Ctrl Pts',(-20.4782440081759,-12.1421413774401,
122.76389380169)) ;
#15083 = CARTESIAN_POINT('Ctrl Pts',(-20.4789208411427,-12.1420808251965,
122.765011792716)) ;
#15084 = CARTESIAN_POINT('Ctrl Pts',(-20.4795958968043,-12.1420202930341,
122.766130805631)) ;
#15085 = CARTESIAN_POINT('',(-20.5005106396601,-12.2002211326089,122.802143425663)) ;
#15086 = CARTESIAN_POINT('Ctrl Pts',(-20.5005103834412,-12.2002204255305,
122.802142893111)) ;
#15087 = CARTESIAN_POINT('Ctrl Pts',(-20.4926703724558,-12.1825726976742,
122.788110222342)) ;
#15088 = CARTESIAN_POINT('Ctrl Pts',(-20.4855685242308,-12.1630483237294,
122.776031389631)) ;
#15089 = CARTESIAN_POINT('Ctrl Pts',(-20.4795958968858,-12.1420202930341,
122.766130805581)) ;
#15090 = CARTESIAN_POINT('Ctrl Pts',(-20.5005103834412,-12.2002204255305,
122.802142893111)) ;
#15091 = CARTESIAN_POINT('Ctrl Pts',(-20.4980414512689,-12.2004500404988,
122.797723803343)) ;
#15092 = CARTESIAN_POINT('Ctrl Pts',(-20.495545380739,-12.2006795489797,122.793319183576)) ;
#15093 = CARTESIAN_POINT('Ctrl Pts',(-20.4930223283398,-12.2009089649636,
122.788929355244)) ;
#15094 = CARTESIAN_POINT('Ctrl Pts',(-20.4570110484069,-12.2041833968457,
122.726273765135)) ;
#15095 = CARTESIAN_POINT('Ctrl Pts',(-20.4156352266409,-12.207512021703,122.666860836852)) ;
#15096 = CARTESIAN_POINT('Ctrl Pts',(-20.3693591437261,-12.210839025915,122.61135629171)) ;
#15097 = CARTESIAN_POINT('Ctrl Pts',(-20.3230162773553,-12.2141708315023,
122.555771645032)) ;
#15098 = CARTESIAN_POINT('Ctrl Pts',(-20.271932289558,-12.2174515742627,122.504317235034)) ;
#15099 = CARTESIAN_POINT('Ctrl Pts',(-20.2167075184025,-12.2207696513077,
122.457587839616)) ;
#15100 = CARTESIAN_POINT('Ctrl Pts',(-20.1381326067292,-12.2254906778559,
122.391100318877)) ;
#15101 = CARTESIAN_POINT('Ctrl Pts',(-20.0516694314546,-12.2302432845576,
122.334585724807)) ;
#15102 = CARTESIAN_POINT('Ctrl Pts',(-19.9592320193965,-12.2349405707703,
122.289297446126)) ;
#15103 = CARTESIAN_POINT('Ctrl Pts',(-19.9214262417386,-12.2368617037207,
122.27077509077)) ;
#15104 = CARTESIAN_POINT('Ctrl Pts',(-19.8826793167483,-12.2387770175723,
122.254163964086)) ;
#15105 = CARTESIAN_POINT('Ctrl Pts',(-19.8432390345038,-12.2407017030626,
122.239563191333)) ;
#15106 = CARTESIAN_POINT('Ctrl Pts',(-19.7572792109858,-12.244896541833,122.207740907675)) ;
#15107 = CARTESIAN_POINT('Ctrl Pts',(-19.6682620386448,-12.2490797655514,
122.185533907236)) ;
#15108 = CARTESIAN_POINT('Ctrl Pts',(-19.577774796042,-12.2532634090411,122.173223680615)) ;
#15109 = CARTESIAN_POINT('Ctrl Pts',(-19.5248777586114,-12.2557090835903,
122.166027367637)) ;
#15110 = CARTESIAN_POINT('Ctrl Pts',(-19.4714765234977,-12.2581549015896,
122.162213503222)) ;
#15111 = CARTESIAN_POINT('Ctrl Pts',(-19.4178896361136,-12.260603267245,122.161844070721)) ;
#15112 = CARTESIAN_POINT('Ctrl Pts',(-19.3453693064356,-12.2639166950848,
122.16134410948)) ;
#15113 = CARTESIAN_POINT('Ctrl Pts',(-19.2728507009386,-12.2672457315864,
122.167160940948)) ;
#15114 = CARTESIAN_POINT('Ctrl Pts',(-19.2012479947592,-12.2705914932778,
122.17924553881)) ;
#15115 = CARTESIAN_POINT('Ctrl Pts',(-19.1344032274444,-12.2737149319533,
122.190527125432)) ;
#15116 = CARTESIAN_POINT('Ctrl Pts',(-19.0685839173307,-12.2768197584562,
122.207228164016)) ;
#15117 = CARTESIAN_POINT('Ctrl Pts',(-19.004440839025,-12.2799106019281,122.229185286871)) ;
#15118 = CARTESIAN_POINT('Ctrl Pts',(-18.9997562439645,-12.2801363371195,
122.230788892934)) ;
#15119 = CARTESIAN_POINT('Ctrl Pts',(-18.9950786111294,-12.2803622331698,
122.232421236984)) ;
#15120 = CARTESIAN_POINT('Ctrl Pts',(-18.990413797334,-12.2805880872903,122.234080267341)) ;
#15121 = CARTESIAN_POINT('Ctrl Pts',(-18.9223714524588,-12.2838824618636,
122.258279371666)) ;
#15122 = CARTESIAN_POINT('Ctrl Pts',(-18.8565569035649,-12.2872058584351,
122.288328386266)) ;
#15123 = CARTESIAN_POINT('Ctrl Pts',(-18.7937055044243,-12.2905106869698,
122.323890840249)) ;
#15124 = CARTESIAN_POINT('Ctrl Pts',(-18.7346124431284,-12.2936178960031,
122.357326758967)) ;
#15125 = CARTESIAN_POINT('Ctrl Pts',(-18.6783500331761,-12.2966797947069,
122.395522002636)) ;
#15126 = CARTESIAN_POINT('Ctrl Pts',(-18.6255288196949,-12.299797885005,122.438034998562)) ;
#15127 = CARTESIAN_POINT('Ctrl Pts',(-18.6220810332869,-12.3000014113657,
122.440809939156)) ;
#15128 = CARTESIAN_POINT('Ctrl Pts',(-18.618647896259,-12.3002051771326,122.44360326177)) ;
#15129 = CARTESIAN_POINT('Ctrl Pts',(-18.615229573615,-12.3004092105329,122.446414837632)) ;
#15130 = CARTESIAN_POINT('Ctrl Pts',(-18.5444122897155,-12.3046361641429,
122.504662167325)) ;
#15131 = CARTESIAN_POINT('Ctrl Pts',(-18.480371878575,-12.3088502666534,122.570394955275)) ;
#15132 = CARTESIAN_POINT('Ctrl Pts',(-18.4241492754252,-12.3130415268771,
122.642377720234)) ;
#15133 = CARTESIAN_POINT('Ctrl Pts',(-18.3909287184771,-12.3155180397233,
122.684910570167)) ;
#15134 = CARTESIAN_POINT('Ctrl Pts',(-18.3604369532267,-12.3179865775546,
122.729627329799)) ;
#15135 = CARTESIAN_POINT('Ctrl Pts',(-18.3328942108092,-12.3204450792431,
122.776274952316)) ;
#15136 = CARTESIAN_POINT('Ctrl Pts',(-18.3164372882747,-12.3219140459576,
122.804147133617)) ;
#15137 = CARTESIAN_POINT('Ctrl Pts',(-18.3010393318235,-12.323392818313,122.832703539378)) ;
#15138 = CARTESIAN_POINT('Ctrl Pts',(-18.2867844628654,-12.3248738381016,
122.861795094771)) ;
#15139 = CARTESIAN_POINT('Ctrl Pts',(-18.2372995361152,-12.3300151098995,
122.962784692914)) ;
#15140 = CARTESIAN_POINT('Ctrl Pts',(-18.2016881138637,-12.335146203594,123.069957542943)) ;
#15141 = CARTESIAN_POINT('Ctrl Pts',(-18.1808841676186,-12.3403323963515,
123.180378082354)) ;
#15142 = CARTESIAN_POINT('Ctrl Pts',(-18.163574053859,-12.3446476154717,123.272254502149)) ;
#15143 = CARTESIAN_POINT('Ctrl Pts',(-18.1566580150728,-12.3489087243486,
123.365595950155)) ;
#15144 = CARTESIAN_POINT('Ctrl Pts',(-18.1601514393078,-12.3531688566601,
123.458689044843)) ;
#15145 = CARTESIAN_POINT('Ctrl Pts',(-18.1620825709398,-12.3555238172117,
123.510150020602)) ;
#15146 = CARTESIAN_POINT('Ctrl Pts',(-18.1671952521868,-12.3578784793472,
123.561536635825)) ;
#15147 = CARTESIAN_POINT('Ctrl Pts',(-18.1754965725959,-12.3602418184192,
123.612557019189)) ;
#15148 = CARTESIAN_POINT('Ctrl Pts',(-18.1861378683255,-12.3632713352592,
123.67795902283)) ;
#15149 = CARTESIAN_POINT('Ctrl Pts',(-18.2019792791202,-12.3663301102207,
123.74248622446)) ;
#15150 = CARTESIAN_POINT('Ctrl Pts',(-18.2228680686441,-12.3693743269832,
123.805445096903)) ;
#15151 = CARTESIAN_POINT('Ctrl Pts',(-18.2241083997099,-12.3695550859792,
123.809183458347)) ;
#15152 = CARTESIAN_POINT('Ctrl Pts',(-18.2253665112514,-12.3697357936469,
123.812916292051)) ;
#15153 = CARTESIAN_POINT('Ctrl Pts',(-18.2266423654683,-12.3699164408135,
123.816643453356)) ;
#15154 = CARTESIAN_POINT('Origin',(-19.4092722359532,16.5113612779716,123.411814366564)) ;
#15155 = CARTESIAN_POINT('',(-20.591901915765,13.7497304410597,123.00698472277)) ;
#15156 = CARTESIAN_POINT('',(-20.5919019615554,13.8098330347218,123.006984856535)) ;
#15157 = CARTESIAN_POINT('',(-20.5919021064381,16.5113612779716,123.006985279772)) ;
#15158 = CARTESIAN_POINT('',(-18.1736437367582,14.0000000000496,123.600817573026)) ;
#15159 = CARTESIAN_POINT('Ctrl Pts',(-18.1736437367582,14.0000000000496,123.600817573026)) ;
#15160 = CARTESIAN_POINT('Ctrl Pts',(-18.1774626726793,13.9988411071295,123.625784271471)) ;
#15161 = CARTESIAN_POINT('Ctrl Pts',(-18.1820355296742,13.9976824688196,123.650619704676)) ;
#15162 = CARTESIAN_POINT('Ctrl Pts',(-18.1896653961921,13.9960232543353,123.686001901941)) ;
#15163 = CARTESIAN_POINT('Ctrl Pts',(-18.1921114177232,13.9955221581955,123.696663785581)) ;
#15164 = CARTESIAN_POINT('Ctrl Pts',(-18.1974156151627,13.994495191266,123.718466931781)) ;
#15165 = CARTESIAN_POINT('Ctrl Pts',(-18.200288262439,13.9939694764739,123.72960363417)) ;
#15166 = CARTESIAN_POINT('Ctrl Pts',(-18.2090082034946,13.9924563586871,123.761578001962)) ;
#15167 = CARTESIAN_POINT('Ctrl Pts',(-18.21524346533,13.9914701085433,123.782305451609)) ;
#15168 = CARTESIAN_POINT('Ctrl Pts',(-18.2252105208952,13.9900148307282,123.812566509253)) ;
#15169 = CARTESIAN_POINT('Ctrl Pts',(-18.2285262460103,13.9895476550969,123.822232849602)) ;
#15170 = CARTESIAN_POINT('Ctrl Pts',(-18.2341064833042,13.9887874444646,123.837873343762)) ;
#15171 = CARTESIAN_POINT('Ctrl Pts',(-18.2362989265072,13.988494807074,123.843872711341)) ;
#15172 = CARTESIAN_POINT('Ctrl Pts',(-18.2410879283046,13.9878681419586,123.856672099124)) ;
#15173 = CARTESIAN_POINT('Ctrl Pts',(-18.2436980934359,13.9875340483542,123.863466773523)) ;
#15174 = CARTESIAN_POINT('Ctrl Pts',(-18.2515425072828,13.9865512760902,123.883366056176)) ;
#15175 = CARTESIAN_POINT('Ctrl Pts',(-18.2569394701305,13.9859017227269,123.896405240024)) ;
#15176 = CARTESIAN_POINT('Ctrl Pts',(-18.2723161968905,13.9841210133041,123.931845384347)) ;
#15177 = CARTESIAN_POINT('Ctrl Pts',(-18.2827361925457,13.9829884709045,123.954048483007)) ;
#15178 = CARTESIAN_POINT('Ctrl Pts',(-18.2982079472457,13.9814081723277,123.984641950125)) ;
#15179 = CARTESIAN_POINT('Ctrl Pts',(-18.302715314106,13.9809585867847,123.993301317154)) ;
#15180 = CARTESIAN_POINT('Ctrl Pts',(-18.3103412489143,13.9802155212036,124.007542111373)) ;
#15181 = CARTESIAN_POINT('Ctrl Pts',(-18.3134020234888,13.9799217350464,124.013153986035)) ;
#15182 = CARTESIAN_POINT('Ctrl Pts',(-18.3191921184688,13.9793741626028,124.023578985777)) ;
#15183 = CARTESIAN_POINT('Ctrl Pts',(-18.3219106105217,13.9791203147805,124.028397943711)) ;
#15184 = CARTESIAN_POINT('Ctrl Pts',(-18.3275946469856,13.9785961438282,124.03831929092)) ;
#15185 = CARTESIAN_POINT('Ctrl Pts',(-18.3305645128967,13.978325856509,124.043419049256)) ;
#15186 = CARTESIAN_POINT('Ctrl Pts',(-18.3372625960084,13.9777241008422,124.054735729306)) ;
#15187 = CARTESIAN_POINT('Ctrl Pts',(-18.3410090060583,13.9773927667428,124.060941641393)) ;
#15188 = CARTESIAN_POINT('Ctrl Pts',(-18.3609314387805,13.9756575029645,124.093303437313)) ;
#15189 = CARTESIAN_POINT('Ctrl Pts',(-18.3780146280628,13.9742608468966,124.118888288694)) ;
#15190 = CARTESIAN_POINT('Ctrl Pts',(-18.4026702478654,13.9723458718292,124.15301693434)) ;
#15191 = CARTESIAN_POINT('Ctrl Pts',(-18.4094414481529,13.9718292772952,124.16212577085)) ;
#15192 = CARTESIAN_POINT('Ctrl Pts',(-18.4202152258821,13.9710205269863,124.176214142201)) ;
#15193 = CARTESIAN_POINT('Ctrl Pts',(-18.4241335282709,13.970729028581,124.18125735499)) ;
#15194 = CARTESIAN_POINT('Ctrl Pts',(-18.4285455719007,13.970403619078,124.186847108107)) ;
#15195 = CARTESIAN_POINT('Ctrl Pts',(-18.4290013534839,13.9703700361816,124.187423505905)) ;
#15196 = CARTESIAN_POINT('Ctrl Pts',(-18.4296752113697,13.970320433815,124.188274148053)) ;
#15197 = CARTESIAN_POINT('Ctrl Pts',(-18.4298928952509,13.9703044177141,124.18854870329)) ;
#15198 = CARTESIAN_POINT('Ctrl Pts',(-18.4306537361755,13.9702484649923,124.189507490593)) ;
#15199 = CARTESIAN_POINT('Ctrl Pts',(-18.4311974948828,13.9702085232008,124.190191244528)) ;
#15200 = CARTESIAN_POINT('Ctrl Pts',(-18.4344159675732,13.9699723843594,124.194229642365)) ;
#15201 = CARTESIAN_POINT('Ctrl Pts',(-18.4371072173425,13.9697760439941,124.197571061907)) ;
#15202 = CARTESIAN_POINT('Ctrl Pts',(-18.4427506060693,13.9693666130753,124.204504441975)) ;
#15203 = CARTESIAN_POINT('Ctrl Pts',(-18.4457056892622,13.9691534986071,124.208093919632)) ;
#15204 = CARTESIAN_POINT('Ctrl Pts',(-18.4527626088121,13.9686475595177,124.216569003977)) ;
#15205 = CARTESIAN_POINT('Ctrl Pts',(-18.4568819487203,13.9683545842259,124.221439856322)) ;
#15206 = CARTESIAN_POINT('Ctrl Pts',(-18.4736304101306,13.967172829716,124.240939117987)) ;
#15207 = CARTESIAN_POINT('Ctrl Pts',(-18.486560665668,13.9662815712753,124.255305226442)) ;
#15208 = CARTESIAN_POINT('Ctrl Pts',(-18.5068019288656,13.9649205685167,124.276771566171)) ;
#15209 = CARTESIAN_POINT('Ctrl Pts',(-18.5138753587099,13.9644510609814,124.284091871219)) ;
#15210 = CARTESIAN_POINT('Ctrl Pts',(-18.5264829401535,13.9636258235447,124.296824512246)) ;
#15211 = CARTESIAN_POINT('Ctrl Pts',(-18.5319794341126,13.9632698229375,124.302273371309)) ;
#15212 = CARTESIAN_POINT('Ctrl Pts',(-18.5435767368815,13.9625262213588,124.313558552678)) ;
#15213 = CARTESIAN_POINT('Ctrl Pts',(-18.5496867891908,13.9621387063724,124.319384823664)) ;
#15214 = CARTESIAN_POINT('Ctrl Pts',(-18.5627686055446,13.9613175721196,124.331608432353)) ;
#15215 = CARTESIAN_POINT('Ctrl Pts',(-18.5697549345301,13.9608840605959,124.337989415325)) ;
#15216 = CARTESIAN_POINT('Ctrl Pts',(-18.5781440697749,13.9603690900883,124.345478736162)) ;
#15217 = CARTESIAN_POINT('Ctrl Pts',(-18.5794776389229,13.9602873938489,124.346664146161)) ;
#15218 = CARTESIAN_POINT('Ctrl Pts',(-18.5992498898033,13.9590785366069,124.364164064333)) ;
#15219 = CARTESIAN_POINT('Ctrl Pts',(-18.6181641013105,13.9579531970331,124.379933196125)) ;
#15220 = CARTESIAN_POINT('Ctrl Pts',(-18.6452463333279,13.9563775433393,124.401188207421)) ;
#15221 = CARTESIAN_POINT('Ctrl Pts',(-18.6530320199043,13.9559285191457,124.407151953503)) ;
#15222 = CARTESIAN_POINT('Ctrl Pts',(-18.6677935907847,13.955083954693,124.418185953165)) ;
#15223 = CARTESIAN_POINT('Ctrl Pts',(-18.6747533357469,13.9546885262551,124.42327684053)) ;
#15224 = CARTESIAN_POINT('Ctrl Pts',(-18.6915483860493,13.9537403635067,124.435297250517)) ;
#15225 = CARTESIAN_POINT('Ctrl Pts',(-18.7014321324551,13.9531871694207,124.442157573656)) ;
#15226 = CARTESIAN_POINT('Ctrl Pts',(-18.7177546985943,13.9522819741949,124.453141365083)) ;
#15227 = CARTESIAN_POINT('Ctrl Pts',(-18.7241350703599,13.9519301945439,124.457350347097)) ;
#15228 = CARTESIAN_POINT('Ctrl Pts',(-18.7412113938347,13.9509943661721,124.468391759775)) ;
#15229 = CARTESIAN_POINT('Ctrl Pts',(-18.7519734952643,13.9504104232339,124.475120269405)) ;
#15230 = CARTESIAN_POINT('Ctrl Pts',(-18.7691506254861,13.9494879987677,124.48549902805)) ;
#15231 = CARTESIAN_POINT('Ctrl Pts',(-18.7754987105456,13.9491491296948,124.489258354591)) ;
#15232 = CARTESIAN_POINT('Ctrl Pts',(-18.7872212334678,13.9485271211577,124.496060966905)) ;
#15233 = CARTESIAN_POINT('Ctrl Pts',(-18.7925856602834,13.9482439039994,124.49912104257)) ;
#15234 = CARTESIAN_POINT('Ctrl Pts',(-18.8036283754401,13.9476638170881,124.505312221034)) ;
#15235 = CARTESIAN_POINT('Ctrl Pts',(-18.8093087962845,13.9473669804819,124.508439149661)) ;
#15236 = CARTESIAN_POINT('Ctrl Pts',(-18.8218670007401,13.9467141488494,124.515225341474)) ;
#15237 = CARTESIAN_POINT('Ctrl Pts',(-18.8287551906648,13.9463582978248,124.518864794803)) ;
#15238 = CARTESIAN_POINT('Ctrl Pts',(-18.8600968988099,13.9447490311704,124.535051582596)) ;
#15239 = CARTESIAN_POINT('Ctrl Pts',(-18.8849257999716,13.943503381499,124.546854542897)) ;
#15240 = CARTESIAN_POINT('Ctrl Pts',(-18.9202000696658,13.9417573700227,124.562218299917)) ;
#15241 = CARTESIAN_POINT('Ctrl Pts',(-18.9303338072544,13.9412581327668,124.566473958707)) ;
#15242 = CARTESIAN_POINT('Ctrl Pts',(-18.945672474652,13.9405047369784,124.572678753916)) ;
#15243 = CARTESIAN_POINT('Ctrl Pts',(-18.9508364482386,13.9402514834011,124.574727730801)) ;
#15244 = CARTESIAN_POINT('Ctrl Pts',(-18.9595707122399,13.9398236601065,124.578126119822)) ;
#15245 = CARTESIAN_POINT('Ctrl Pts',(-18.9631338388344,13.9396492776055,124.579493730395)) ;
#15246 = CARTESIAN_POINT('Ctrl Pts',(-18.966745181488,13.9394726659897,124.580860904629)) ;
#15247 = CARTESIAN_POINT('Ctrl Pts',(-18.9667871975745,13.9394706112237,124.580876808397)) ;
#15248 = CARTESIAN_POINT('Ctrl Pts',(-18.9668706198766,13.9394665315524,124.580908379947)) ;
#15249 = CARTESIAN_POINT('Ctrl Pts',(-18.9669120265165,13.9394645066259,124.580924047964)) ;
#15250 = CARTESIAN_POINT('Ctrl Pts',(-18.9669942433454,13.9394604859759,124.580955153311)) ;
#15251 = CARTESIAN_POINT('Ctrl Pts',(-18.9670350533953,13.9394584902587,124.58097059066)) ;
#15252 = CARTESIAN_POINT('Ctrl Pts',(-18.9671160898843,13.9394545273977,124.581001239745)) ;
#15253 = CARTESIAN_POINT('Ctrl Pts',(-18.9671563160248,13.9394525602681,124.581016451437)) ;
#15254 = CARTESIAN_POINT('Ctrl Pts',(-18.9672361962167,13.9394486540174,124.581046653771)) ;
#15255 = CARTESIAN_POINT('Ctrl Pts',(-18.9672758504303,13.939446714888,124.581061644542)) ;
#15256 = CARTESIAN_POINT('Ctrl Pts',(-18.9673545995492,13.9394428640114,124.581091410065)) ;
#15257 = CARTESIAN_POINT('Ctrl Pts',(-18.9673936942426,13.9394409522741,124.581106184802)) ;
#15258 = CARTESIAN_POINT('Ctrl Pts',(-18.9674713347892,13.9394371556684,124.581135522408)) ;
#15259 = CARTESIAN_POINT('Ctrl Pts',(-18.967509881168,13.9394352707739,124.581150085538)) ;
#15260 = CARTESIAN_POINT('Ctrl Pts',(-18.9675864383075,13.9394315272059,124.581179005111)) ;
#15261 = CARTESIAN_POINT('Ctrl Pts',(-18.9676244485248,13.9394296685586,124.58119336141)) ;
#15262 = CARTESIAN_POINT('Ctrl Pts',(-18.9676999440553,13.9394259769598,124.581221871547)) ;
#15263 = CARTESIAN_POINT('Ctrl Pts',(-18.9677374293982,13.9394241440066,124.581236025454)) ;
#15264 = CARTESIAN_POINT('Ctrl Pts',(-18.9678118860851,13.9394205032614,124.581264135101)) ;
#15265 = CARTESIAN_POINT('Ctrl Pts',(-18.9678488576418,13.9394186954588,124.581278090977)) ;
#15266 = CARTESIAN_POINT('Ctrl Pts',(-18.9679222976972,13.9394151044788,124.581305808857)) ;
#15267 = CARTESIAN_POINT('Ctrl Pts',(-18.967958766328,13.9394133212946,124.581319570966)) ;
#15268 = CARTESIAN_POINT('Ctrl Pts',(-18.9680312123382,13.939409778973,124.581346905929)) ;
#15269 = CARTESIAN_POINT('Ctrl Pts',(-18.9680671892768,13.9394080198568,124.58136047867)) ;
#15270 = CARTESIAN_POINT('Ctrl Pts',(-18.9681386615179,13.9394045252001,124.581387438681)) ;
#15271 = CARTESIAN_POINT('Ctrl Pts',(-18.9681741570821,13.9394027896464,124.581400826101)) ;
#15272 = CARTESIAN_POINT('Ctrl Pts',(-18.9682446774375,13.9393993415823,124.581427419718)) ;
#15273 = CARTESIAN_POINT('Ctrl Pts',(-18.9682797022772,13.9393976290692,124.581440625982)) ;
#15274 = CARTESIAN_POINT('Ctrl Pts',(-18.9683492904791,13.939394226631,124.581466860938)) ;
#15275 = CARTESIAN_POINT('Ctrl Pts',(-18.96838385427,13.9393925366845,124.581479889839)) ;
#15276 = CARTESIAN_POINT('Ctrl Pts',(-18.9684525326365,13.9393891787789,124.581505774831)) ;
#15277 = CARTESIAN_POINT('Ctrl Pts',(-18.9684866462715,13.9393875108655,124.581518630613)) ;
#15278 = CARTESIAN_POINT('Ctrl Pts',(-18.9685544328501,13.9393841966083,124.581544172715)) ;
#15279 = CARTESIAN_POINT('Ctrl Pts',(-18.9685881058439,13.9393825502617,124.581556859099)) ;
#15280 = CARTESIAN_POINT('Ctrl Pts',(-18.9686550213212,13.9393792786396,124.581582066369)) ;
#15281 = CARTESIAN_POINT('Ctrl Pts',(-18.9686882636257,13.9393776533724,124.581594587232)) ;
#15282 = CARTESIAN_POINT('Ctrl Pts',(-18.9687543270124,13.9393744234541,124.581619467087)) ;
#15283 = CARTESIAN_POINT('Ctrl Pts',(-18.9687871482268,13.9393728187962,124.581631826169)) ;
#15284 = CARTESIAN_POINT('Ctrl Pts',(-18.9688523781887,13.9393696296675,124.581656385882)) ;
#15285 = CARTESIAN_POINT('Ctrl Pts',(-18.9688847873888,13.9393680451743,124.581668586722)) ;
#15286 = CARTESIAN_POINT('Ctrl Pts',(-18.9689492037355,13.9393648958649,124.581692833989)) ;
#15287 = CARTESIAN_POINT('Ctrl Pts',(-18.9689812105766,13.9393633310635,124.581704880338)) ;
#15288 = CARTESIAN_POINT('Ctrl Pts',(-18.9690448309592,13.9393602207091,124.581728822031)) ;
#15289 = CARTESIAN_POINT('Ctrl Pts',(-18.9690764444664,13.9393586751575,124.581740717397)) ;
#15290 = CARTESIAN_POINT('Ctrl Pts',(-18.9691392875197,13.9393556028453,124.581764360749)) ;
#15291 = CARTESIAN_POINT('Ctrl Pts',(-18.969170516958,13.9393540760898,124.581776108728)) ;
#15292 = CARTESIAN_POINT('Ctrl Pts',(-18.9692325994227,13.939351041,124.581799460249)) ;
#15293 = CARTESIAN_POINT('Ctrl Pts',(-18.969263453047,13.9393495326363,124.58181106405)) ;
#15294 = CARTESIAN_POINT('Ctrl Pts',(-18.9693247941971,13.9393465338253,124.581834131196)) ;
#15295 = CARTESIAN_POINT('Ctrl Pts',(-18.9693552812066,13.939345043403,124.58184559438)) ;
#15296 = CARTESIAN_POINT('Ctrl Pts',(-18.9694158972986,13.9393420800745,124.581868383461)) ;
#15297 = CARTESIAN_POINT('Ctrl Pts',(-18.9694460261724,13.9393406071784,124.581879709313)) ;
#15298 = CARTESIAN_POINT('Ctrl Pts',(-18.9695059349098,13.9393376784658,124.581902227177)) ;
#15299 = CARTESIAN_POINT('Ctrl Pts',(-18.9695357145272,13.9393362226611,124.581913419129)) ;
#15300 = CARTESIAN_POINT('Ctrl Pts',(-18.9695949312375,13.9393333278137,124.581935671721)) ;
#15301 = CARTESIAN_POINT('Ctrl Pts',(-18.9696243692418,13.9393318887263,124.581946732735)) ;
#15302 = CARTESIAN_POINT('Ctrl Pts',(-18.9696829119197,13.9393290268632,124.581968726996)) ;
#15303 = CARTESIAN_POINT('Ctrl Pts',(-18.9697120166187,13.9393276040862,124.581979660282)) ;
#15304 = CARTESIAN_POINT('Ctrl Pts',(-18.9697699017845,13.9393247743987,124.582001402589)) ;
#15305 = CARTESIAN_POINT('Ctrl Pts',(-18.9697986816223,13.9393233675188,124.582012211403)) ;
#15306 = CARTESIAN_POINT('Ctrl Pts',(-18.9698559250561,13.9393205692343,124.582033707849)) ;
#15307 = CARTESIAN_POINT('Ctrl Pts',(-18.9698843883754,13.9393191778431,124.582044395405)) ;
#15308 = CARTESIAN_POINT('Ctrl Pts',(-18.9699410043546,13.9393164102626,124.582065651512)) ;
#15309 = CARTESIAN_POINT('Ctrl Pts',(-18.9699691581441,13.9393150340179,124.582076220513)) ;
#15310 = CARTESIAN_POINT('Ctrl Pts',(-18.9700251644834,13.9393122962695,124.582097243123)) ;
#15311 = CARTESIAN_POINT('Ctrl Pts',(-18.9700530168869,13.9393109347728,124.582107696701)) ;
#15312 = CARTESIAN_POINT('Ctrl Pts',(-18.9701084286675,13.9393082261182,124.582128491623)) ;
#15313 = CARTESIAN_POINT('Ctrl Pts',(-18.9701359877231,13.939306878976,124.582138832869)) ;
#15314 = CARTESIAN_POINT('Ctrl Pts',(-18.9701908187779,13.9393041987381,124.582159405438)) ;
#15315 = CARTESIAN_POINT('Ctrl Pts',(-18.9702180913467,13.9393028656145,124.582169636996)) ;
#15316 = CARTESIAN_POINT('Ctrl Pts',(-18.9732080926408,13.9391567107115,124.583291244657)) ;
#15317 = CARTESIAN_POINT('Ctrl Pts',(-18.9761750241519,13.9390117688047,124.584391365336)) ;
#15318 = CARTESIAN_POINT('Ctrl Pts',(-18.9820807847831,13.9387234143468,124.586555713941)) ;
#15319 = CARTESIAN_POINT('Ctrl Pts',(-18.9850194915413,13.9385800058607,124.587620208521)) ;
#15320 = CARTESIAN_POINT('Ctrl Pts',(-18.9928479852357,13.9381981699311,124.590422772352)) ;
#15321 = CARTESIAN_POINT('Ctrl Pts',(-18.9977446446959,13.9379595339167,124.592141428061)) ;
#15322 = CARTESIAN_POINT('Ctrl Pts',(-19.0207307657352,13.9368402336773,124.600048793045)) ;
#15323 = CARTESIAN_POINT('Ctrl Pts',(-19.038949793513,13.9359554506044,124.605852390117)) ;
#15324 = CARTESIAN_POINT('Ctrl Pts',(-19.0774247613116,13.9340960678331,124.61714310735)) ;
#15325 = CARTESIAN_POINT('Ctrl Pts',(-19.0977005875379,13.9331220884634,124.622542757756)) ;
#15326 = CARTESIAN_POINT('Ctrl Pts',(-19.1263403553744,13.9317600742956,124.629402680527)) ;
#15327 = CARTESIAN_POINT('Ctrl Pts',(-19.1345978289103,13.9313689069911,124.631292009863)) ;
#15328 = CARTESIAN_POINT('Ctrl Pts',(-19.147787481875,13.9307466536259,124.634169067745)) ;
#15329 = CARTESIAN_POINT('Ctrl Pts',(-19.1527074981449,13.9305151027838,124.635211206382)) ;
#15330 = CARTESIAN_POINT('Ctrl Pts',(-19.16130417932,13.9301114985128,124.636977981991)) ;
#15331 = CARTESIAN_POINT('Ctrl Pts',(-19.1649780563968,13.9299393258473,124.637715829006)) ;
#15332 = CARTESIAN_POINT('Ctrl Pts',(-19.1721756599988,13.9296026186865,124.639127726821)) ;
#15333 = CARTESIAN_POINT('Ctrl Pts',(-19.1756990796923,13.9294380729136,124.639803149641)) ;
#15334 = CARTESIAN_POINT('Ctrl Pts',(-19.1827392516312,13.9291098407486,124.641121320646)) ;
#15335 = CARTESIAN_POINT('Ctrl Pts',(-19.186255950468,13.9289461549195,124.641764169133)) ;
#15336 = CARTESIAN_POINT('Ctrl Pts',(-19.1947302003395,13.9285523503711,124.643275712488)) ;
#15337 = CARTESIAN_POINT('Ctrl Pts',(-19.1996903387403,13.9283223694788,124.64412956981)) ;
#15338 = CARTESIAN_POINT('Ctrl Pts',(-19.2245417840649,13.927172527981,124.648253209569)) ;
#15339 = CARTESIAN_POINT('Ctrl Pts',(-19.2445050504352,13.9262568255469,124.65107145639)) ;
#15340 = CARTESIAN_POINT('Ctrl Pts',(-19.2654189592725,13.9253013542152,124.653509594785)) ;
#15341 = CARTESIAN_POINT('Ctrl Pts',(-19.2663102099474,13.9252606433657,124.653612524124)) ;
#15342 = CARTESIAN_POINT('Ctrl Pts',(-19.2677614680521,13.9251943624866,124.653778544885)) ;
#15343 = CARTESIAN_POINT('Ctrl Pts',(-19.2683214086561,13.9251687917241,124.653842217278)) ;
#15344 = CARTESIAN_POINT('Ctrl Pts',(-19.2707238703482,13.9250590887249,124.654113762265)) ;
#15345 = CARTESIAN_POINT('Ctrl Pts',(-19.2725668096922,13.9249749603644,124.654317913683)) ;
#15346 = CARTESIAN_POINT('Ctrl Pts',(-19.2750571409665,13.9248613069928,124.654588172138)) ;
#15347 = CARTESIAN_POINT('Ctrl Pts',(-19.275704140049,13.9248317818754,124.654657875337)) ;
#15348 = CARTESIAN_POINT('Ctrl Pts',(-19.2926060973418,13.924060539582,124.656465424471)) ;
#15349 = CARTESIAN_POINT('Ctrl Pts',(-19.3088934680056,13.9233185683605,124.657884727485)) ;
#15350 = CARTESIAN_POINT('Ctrl Pts',(-19.3332750460147,13.9222063384977,124.659528222146)) ;
#15351 = CARTESIAN_POINT('Ctrl Pts',(-19.3413511852334,13.9218377068823,124.659993908311)) ;
#15352 = CARTESIAN_POINT('Ctrl Pts',(-19.3549040558307,13.9212184829742,124.66064346673)) ;
#15353 = CARTESIAN_POINT('Ctrl Pts',(-19.3603785104605,13.9209681926304,124.660869779183)) ;
#15354 = CARTESIAN_POINT('Ctrl Pts',(-19.3659434873133,13.9207135668985,124.661063191894)) ;
#15355 = CARTESIAN_POINT('Ctrl Pts',(-19.3660327097756,13.9207094844702,124.661066283282)) ;
#15356 = CARTESIAN_POINT('Ctrl Pts',(-19.3662045149436,13.9207016233211,124.661072217574)) ;
#15357 = CARTESIAN_POINT('Ctrl Pts',(-19.3662870975194,13.9206978446137,124.661075061847)) ;
#15358 = CARTESIAN_POINT('Ctrl Pts',(-19.366446161289,13.9206905662934,124.661080524459)) ;
#15359 = CARTESIAN_POINT('Ctrl Pts',(-19.3665226419754,13.92068706671,124.661083143948)) ;
#15360 = CARTESIAN_POINT('Ctrl Pts',(-19.3666699907485,13.9206803242905,124.661088177147)) ;
#15361 = CARTESIAN_POINT('Ctrl Pts',(-19.3667408592481,13.9206770814408,124.661090591864)) ;
#15362 = CARTESIAN_POINT('Ctrl Pts',(-19.3668774321641,13.9206708319806,124.661095233707)) ;
#15363 = CARTESIAN_POINT('Ctrl Pts',(-19.3669431362677,13.9206678253889,124.66109746167)) ;
#15364 = CARTESIAN_POINT('Ctrl Pts',(-19.3670697879421,13.9206620298087,124.661101746304)) ;
#15365 = CARTESIAN_POINT('Ctrl Pts',(-19.3671307358306,13.9206592408094,124.661103803709)) ;
#15366 = CARTESIAN_POINT('Ctrl Pts',(-19.3672482479186,13.920653863364,124.661107761932)) ;
#15367 = CARTESIAN_POINT('Ctrl Pts',(-19.3673048124465,13.9206512749061,124.661109663379)) ;
#15368 = CARTESIAN_POINT('Ctrl Pts',(-19.3674138995754,13.9206462829134,124.661113322985)) ;
#15369 = CARTESIAN_POINT('Ctrl Pts',(-19.3674664219875,13.9206438793902,124.661115081667)) ;
#15370 = CARTESIAN_POINT('Ctrl Pts',(-19.3675677362742,13.9206392430257,124.66111846772)) ;
#15371 = CARTESIAN_POINT('Ctrl Pts',(-19.3676165281633,13.9206370101861,124.661120095546)) ;
#15372 = CARTESIAN_POINT('Ctrl Pts',(-19.3677106680637,13.9206327020776,124.66112323078)) ;
#15373 = CARTESIAN_POINT('Ctrl Pts',(-19.367756015428,13.9206306268404,124.661124738557)) ;
#15374 = CARTESIAN_POINT('Ctrl Pts',(-19.3679269435706,13.9206228045837,124.661130412512)) ;
#15375 = CARTESIAN_POINT('Ctrl Pts',(-19.3680525250163,13.9206170574446,124.661134562228)) ;
#15376 = CARTESIAN_POINT('Ctrl Pts',(-19.3683006178882,13.9206057034606,124.661142722768)) ;
#15377 = CARTESIAN_POINT('Ctrl Pts',(-19.3684231293397,13.9206000966194,124.661146734507)) ;
#15378 = CARTESIAN_POINT('Ctrl Pts',(-19.3686652174968,13.9205890170547,124.661154626238)) ;
#15379 = CARTESIAN_POINT('Ctrl Pts',(-19.3687847942475,13.9205835443338,124.661158507085)) ;
#15380 = CARTESIAN_POINT('Ctrl Pts',(-19.3690211441822,13.920572727019,124.661166143822)) ;
#15381 = CARTESIAN_POINT('Ctrl Pts',(-19.3691379173936,13.9205673824282,124.661169900509)) ;
#15382 = CARTESIAN_POINT('Ctrl Pts',(-19.3693687878214,13.9205568155477,124.661177295394)) ;
#15383 = CARTESIAN_POINT('Ctrl Pts',(-19.3694828849103,13.9205515932677,124.66118093433)) ;
#15384 = CARTESIAN_POINT('Ctrl Pts',(-19.3697085263931,13.9205412653768,124.661188099847)) ;
#15385 = CARTESIAN_POINT('Ctrl Pts',(-19.3698200708131,13.9205361597685,124.661191627121)) ;
#15386 = CARTESIAN_POINT('Ctrl Pts',(-19.3700407278998,13.920526059696,124.661198575192)) ;
#15387 = CARTESIAN_POINT('Ctrl Pts',(-19.3701498401933,13.9205210652524,124.661201996623)) ;
#15388 = CARTESIAN_POINT('Ctrl Pts',(-19.3703657490253,13.9205111822102,124.661208738557)) ;
#15389 = CARTESIAN_POINT('Ctrl Pts',(-19.3704725458167,13.9205062936031,124.66121205967)) ;
#15390 = CARTESIAN_POINT('Ctrl Pts',(-19.3706839380596,13.920496617006,124.661218606309)) ;
#15391 = CARTESIAN_POINT('Ctrl Pts',(-19.370788533413,13.9204918290235,124.661221832392)) ;
#15392 = CARTESIAN_POINT('Ctrl Pts',(-19.370995634061,13.9204823485902,124.661228194061)) ;
#15393 = CARTESIAN_POINT('Ctrl Pts',(-19.3710981392099,13.920477656149,124.661231330164)) ;
#15394 = CARTESIAN_POINT('Ctrl Pts',(-19.3713011679266,13.9204683618408,124.661237516735)) ;
#15395 = CARTESIAN_POINT('Ctrl Pts',(-19.3714016914962,13.9204637599763,124.661240567687)) ;
#15396 = CARTESIAN_POINT('Ctrl Pts',(-19.3764233886142,13.9202338685576,124.661392372686)) ;
#15397 = CARTESIAN_POINT('Ctrl Pts',(-19.3813453883059,13.920008379841,124.661512062472)) ;
#15398 = CARTESIAN_POINT('Ctrl Pts',(-19.3913102620274,13.919551522313,124.661695481316)) ;
#15399 = CARTESIAN_POINT('Ctrl Pts',(-19.3963530721949,13.9193201480641,124.661757776703)) ;
#15400 = CARTESIAN_POINT('Ctrl Pts',(-19.4114053570885,13.9186289925624,124.661852621509)) ;
#15401 = CARTESIAN_POINT('Ctrl Pts',(-19.4214149662524,13.9181686774593,124.661795463211)) ;
#15402 = CARTESIAN_POINT('Ctrl Pts',(-19.4506181858273,13.9168239996106,124.661277888179)) ;
#15403 = CARTESIAN_POINT('Ctrl Pts',(-19.4698031946768,13.9159383507741,124.660495502817)) ;
#15404 = CARTESIAN_POINT('Ctrl Pts',(-19.4953775834862,13.914757901529,124.658861755587)) ;
#15405 = CARTESIAN_POINT('Ctrl Pts',(-19.50178942799,13.9144619770801,124.658402466501)) ;
#15406 = CARTESIAN_POINT('Ctrl Pts',(-19.5148496310689,13.9138595559828,124.657365627663)) ;
#15407 = CARTESIAN_POINT('Ctrl Pts',(-19.5214974836442,13.9135530864495,124.656784255579)) ;
#15408 = CARTESIAN_POINT('Ctrl Pts',(-19.5374234120754,13.9128189560705,124.655262892759)) ;
#15409 = CARTESIAN_POINT('Ctrl Pts',(-19.5466962535454,13.9123915595447,124.654272253695)) ;
#15410 = CARTESIAN_POINT('Ctrl Pts',(-19.5668074263285,13.9114639489423,124.651895830038)) ;
#15411 = CARTESIAN_POINT('Ctrl Pts',(-19.5776404313177,13.9109638642758,124.650471511811)) ;
#15412 = CARTESIAN_POINT('Ctrl Pts',(-19.6080326443963,13.909558338681,124.646069482035)) ;
#15413 = CARTESIAN_POINT('Ctrl Pts',(-19.6275418109054,13.9086530916704,124.64276919171)) ;
#15414 = CARTESIAN_POINT('Ctrl Pts',(-19.6671877083547,13.9068032839008,124.635090269406)) ;
#15415 = CARTESIAN_POINT('Ctrl Pts',(-19.6873110655574,13.905858910027,124.63067396429)) ;
#15416 = CARTESIAN_POINT('Ctrl Pts',(-19.7301892752595,13.9038330797831,124.620146678596)) ;
#15417 = CARTESIAN_POINT('Ctrl Pts',(-19.7528995079878,13.9027520150845,124.613885509814)) ;
#15418 = CARTESIAN_POINT('Ctrl Pts',(-19.8012734673872,13.9004308672457,124.599065902957)) ;
#15419 = CARTESIAN_POINT('Ctrl Pts',(-19.8268639143808,13.8991915779605,124.590308478354)) ;
#15420 = CARTESIAN_POINT('Ctrl Pts',(-19.879223751613,13.8966271417408,124.570470385132)) ;
#15421 = CARTESIAN_POINT('Ctrl Pts',(-19.9059327736428,13.8953029119353,124.559275262651)) ;
#15422 = CARTESIAN_POINT('Ctrl Pts',(-19.956855287508,13.8927364115002,124.535819672403)) ;
#15423 = CARTESIAN_POINT('Ctrl Pts',(-19.9811060066009,13.8914945859408,124.5236782338)) ;
#15424 = CARTESIAN_POINT('Ctrl Pts',(-20.0281006258142,13.8890432369325,124.498205310685)) ;
#15425 = CARTESIAN_POINT('Ctrl Pts',(-20.0508560573835,13.8878344303593,124.484923894662)) ;
#15426 = CARTESIAN_POINT('Ctrl Pts',(-20.080460114139,13.8862323867493,124.466366765715)) ;
#15427 = CARTESIAN_POINT('Ctrl Pts',(-20.0876980866373,13.8858383092675,124.461724979836)) ;
#15428 = CARTESIAN_POINT('Ctrl Pts',(-20.1018009566885,13.8850658649542,124.452473932091)) ;
#15429 = CARTESIAN_POINT('Ctrl Pts',(-20.1086691645535,13.884687494958,124.447870493019)) ;
#15430 = CARTESIAN_POINT('Ctrl Pts',(-20.1219453760699,13.883951980122,124.438779888109)) ;
#15431 = CARTESIAN_POINT('Ctrl Pts',(-20.1283579311245,13.8835948071044,124.434300039068)) ;
#15432 = CARTESIAN_POINT('Ctrl Pts',(-20.1562744967525,13.8820301564728,124.414404842634)) ;
#15433 = CARTESIAN_POINT('Ctrl Pts',(-20.1773279440905,13.8808242007162,124.398369213678)) ;
#15434 = CARTESIAN_POINT('Ctrl Pts',(-20.2033402422412,13.8792903909254,124.377218919719)) ;
#15435 = CARTESIAN_POINT('Ctrl Pts',(-20.2087859377444,13.878966786266,124.372713835882)) ;
#15436 = CARTESIAN_POINT('Ctrl Pts',(-20.2186624930317,13.8783751243418,124.364401127657)) ;
#15437 = CARTESIAN_POINT('Ctrl Pts',(-20.2231054293776,13.8781071752414,124.360608158024)) ;
#15438 = CARTESIAN_POINT('Ctrl Pts',(-20.2276995668302,13.877828195985,124.356630094399)) ;
#15439 = CARTESIAN_POINT('Ctrl Pts',(-20.2278774832658,13.8778173889995,124.356475948594)) ;
#15440 = CARTESIAN_POINT('Ctrl Pts',(-20.2282365229829,13.877795574178,124.356164700991)) ;
#15441 = CARTESIAN_POINT('Ctrl Pts',(-20.2284176446522,13.8777845663278,124.356007597301)) ;
#15442 = CARTESIAN_POINT('Ctrl Pts',(-20.2287839208127,13.8777622992213,124.355689707162)) ;
#15443 = CARTESIAN_POINT('Ctrl Pts',(-20.228969073219,13.8777510399482,124.355528918315)) ;
#15444 = CARTESIAN_POINT('Ctrl Pts',(-20.2293442523262,13.8777282183736,124.355202914006)) ;
#15445 = CARTESIAN_POINT('Ctrl Pts',(-20.2295342763912,13.8777166560548,124.355037695632)) ;
#15446 = CARTESIAN_POINT('Ctrl Pts',(-20.2299200672067,13.8776931749944,124.354702061097)) ;
#15447 = CARTESIAN_POINT('Ctrl Pts',(-20.2301158308275,13.877681256228,124.354531641359)) ;
#15448 = CARTESIAN_POINT('Ctrl Pts',(-20.2353433106641,13.8773628912432,124.34997805692)) ;
#15449 = CARTESIAN_POINT('Ctrl Pts',(-20.2403398901878,13.8770561624978,124.345554739535)) ;
#15450 = CARTESIAN_POINT('Ctrl Pts',(-20.2537736939653,13.8762248039489,124.333468956207)) ;
#15451 = CARTESIAN_POINT('Ctrl Pts',(-20.2621419114022,13.875699665424,124.325730779803)) ;
#15452 = CARTESIAN_POINT('Ctrl Pts',(-20.2890188048205,13.8739891719933,124.300186778883)) ;
#15453 = CARTESIAN_POINT('Ctrl Pts',(-20.3070847995225,13.8728014336502,124.281924801571)) ;
#15454 = CARTESIAN_POINT('Ctrl Pts',(-20.3327228911498,13.871065222241,124.254359324485)) ;
#15455 = CARTESIAN_POINT('Ctrl Pts',(-20.3407442207031,13.8705142530263,124.245482803349)) ;
#15456 = CARTESIAN_POINT('Ctrl Pts',(-20.3522514987485,13.8697126148666,124.232375227732)) ;
#15457 = CARTESIAN_POINT('Ctrl Pts',(-20.3558389721217,13.8694610543272,124.228234253128)) ;
#15458 = CARTESIAN_POINT('Ctrl Pts',(-20.3609359035609,13.8691012787815,124.22227217366)) ;
#15459 = CARTESIAN_POINT('Ctrl Pts',(-20.3624675910696,13.8689928512087,124.22047016994)) ;
#15460 = CARTESIAN_POINT('Ctrl Pts',(-20.36628960837,13.8687215102603,124.215947686043)) ;
#15461 = CARTESIAN_POINT('Ctrl Pts',(-20.3685734618813,13.8685586616537,124.21322175648)) ;
#15462 = CARTESIAN_POINT('Ctrl Pts',(-20.3736850283819,13.868192576821,124.207067605549)) ;
#15463 = CARTESIAN_POINT('Ctrl Pts',(-20.3765061568603,13.867989408835,124.203633973995)) ;
#15464 = CARTESIAN_POINT('Ctrl Pts',(-20.3830296711849,13.8675169572769,124.195607235035)) ;
#15465 = CARTESIAN_POINT('Ctrl Pts',(-20.3867179739935,13.8672478203455,124.191002811594)) ;
#15466 = CARTESIAN_POINT('Ctrl Pts',(-20.3964126849496,13.8665348986633,124.178722914163)) ;
#15467 = CARTESIAN_POINT('Ctrl Pts',(-20.4023621678777,13.8660916906057,124.171002995942)) ;
#15468 = CARTESIAN_POINT('Ctrl Pts',(-20.4219847678086,13.8646097237938,124.144915731517)) ;
#15469 = CARTESIAN_POINT('Ctrl Pts',(-20.4352432116931,13.8635757257447,124.12624269323)) ;
#15470 = CARTESIAN_POINT('Ctrl Pts',(-20.4569931975374,13.8618053092372,124.093755122169)) ;
#15471 = CARTESIAN_POINT('Ctrl Pts',(-20.4657424565696,13.8610701433617,124.080120489348)) ;
#15472 = CARTESIAN_POINT('Ctrl Pts',(-20.4766311972598,13.8601215799561,124.062403314976)) ;
#15473 = CARTESIAN_POINT('Ctrl Pts',(-20.4790165525729,13.8599116168089,124.05847365003)) ;
#15474 = CARTESIAN_POINT('Ctrl Pts',(-20.4827617245927,13.8595784489231,124.052226372633)) ;
#15475 = CARTESIAN_POINT('Ctrl Pts',(-20.4841358418109,13.8594554445667,124.049917374306)) ;
#15476 = CARTESIAN_POINT('Ctrl Pts',(-20.4868163538934,13.8592139829952,124.045379948361)) ;
#15477 = CARTESIAN_POINT('Ctrl Pts',(-20.4881233071963,13.8590955343428,124.043151866303)) ;
#15478 = CARTESIAN_POINT('Ctrl Pts',(-20.4894303910201,13.8589763455646,124.040907650835)) ;
#15479 = CARTESIAN_POINT('Ctrl Pts',(-20.4894374392435,13.8589757028383,124.040895548824)) ;
#15480 = CARTESIAN_POINT('Ctrl Pts',(-20.4894515373059,13.8589744171956,124.040871341091)) ;
#15481 = CARTESIAN_POINT('Ctrl Pts',(-20.4894585869626,13.8589737742958,124.040859235683)) ;
#15482 = CARTESIAN_POINT('Ctrl Pts',(-20.489472687908,13.8589724883046,124.040835021129)) ;
#15483 = CARTESIAN_POINT('Ctrl Pts',(-20.4894797397975,13.8589718451583,124.04082291095)) ;
#15484 = CARTESIAN_POINT('Ctrl Pts',(-20.4894938476967,13.8589705584471,124.040798682581)) ;
#15485 = CARTESIAN_POINT('Ctrl Pts',(-20.4895009034205,13.8589699149082,124.04078656488)) ;
#15486 = CARTESIAN_POINT('Ctrl Pts',(-20.4895150206131,13.8589686272635,124.040762318674)) ;
#15487 = CARTESIAN_POINT('Ctrl Pts',(-20.4895220816866,13.8589679831937,124.040750190847)) ;
#15488 = CARTESIAN_POINT('Ctrl Pts',(-20.4895362104088,13.8589666944114,124.040725922959)) ;
#15489 = CARTESIAN_POINT('Ctrl Pts',(-20.4895432780922,13.8589660496956,124.040713782838)) ;
#15490 = CARTESIAN_POINT('Ctrl Pts',(-20.4895574210412,13.8589647595293,124.04068948863)) ;
#15491 = CARTESIAN_POINT('Ctrl Pts',(-20.4895644965789,13.8589641140539,124.040677334074)) ;
#15492 = CARTESIAN_POINT('Ctrl Pts',(-20.4895786563188,13.8589628222694,124.040653009136)) ;
#15493 = CARTESIAN_POINT('Ctrl Pts',(-20.4895857408142,13.8589621759336,124.040640838247)) ;
#15494 = CARTESIAN_POINT('Ctrl Pts',(-20.4895999205315,13.8589608822399,124.040616477096)) ;
#15495 = CARTESIAN_POINT('Ctrl Pts',(-20.4896070154501,13.8589602349097,124.040604287352)) ;
#15496 = CARTESIAN_POINT('Ctrl Pts',(-20.4896212177068,13.8589589390727,124.040579885577)) ;
#15497 = CARTESIAN_POINT('Ctrl Pts',(-20.4896283246326,13.8589582906034,124.040567674252)) ;
#15498 = CARTESIAN_POINT('Ctrl Pts',(-20.4896425511479,13.8589569924657,124.040543228891)) ;
#15499 = CARTESIAN_POINT('Ctrl Pts',(-20.4896496710771,13.8589563427662,124.040530994268)) ;
#15500 = CARTESIAN_POINT('Ctrl Pts',(-20.4896639249594,13.8589550420437,124.040506499968)) ;
#15501 = CARTESIAN_POINT('Ctrl Pts',(-20.4896710591065,13.8589543910029,124.040494239955)) ;
#15502 = CARTESIAN_POINT('Ctrl Pts',(-20.4896853432603,13.85895308743,124.040469691712)) ;
#15503 = CARTESIAN_POINT('Ctrl Pts',(-20.4896924930939,13.8589524349136,124.040457403779)) ;
#15504 = CARTESIAN_POINT('Ctrl Pts',(-20.4897068096879,13.8589511282918,124.040432797854)) ;
#15505 = CARTESIAN_POINT('Ctrl Pts',(-20.4897139764488,13.8589504741863,124.040420479861)) ;
#15506 = CARTESIAN_POINT('Ctrl Pts',(-20.4897283281319,13.8589491642732,124.040395811688)) ;
#15507 = CARTESIAN_POINT('Ctrl Pts',(-20.4897355130865,13.8589485084626,124.040383461451)) ;
#15508 = CARTESIAN_POINT('Ctrl Pts',(-20.4897499024844,13.8589471950179,124.040358726501)) ;
#15509 = CARTESIAN_POINT('Ctrl Pts',(-20.4897571069399,13.8589465373825,124.040346341765)) ;
#15510 = CARTESIAN_POINT('Ctrl Pts',(-20.4897715364221,13.8589452201891,124.040321535949)) ;
#15511 = CARTESIAN_POINT('Ctrl Pts',(-20.489778761504,13.8589445606258,124.040309114772)) ;
#15512 = CARTESIAN_POINT('Ctrl Pts',(-20.489793234226,13.8589432393949,124.040284232648)) ;
#15513 = CARTESIAN_POINT('Ctrl Pts',(-20.4898004814714,13.8589425777631,124.040271772377)) ;
#15514 = CARTESIAN_POINT('Ctrl Pts',(-20.4898149995318,13.8589412523022,124.040246810319)) ;
#15515 = CARTESIAN_POINT('Ctrl Pts',(-20.4898222702575,13.8589405884811,124.040234308681)) ;
#15516 = CARTESIAN_POINT('Ctrl Pts',(-20.4898368358522,13.8589392585889,124.040209262893)) ;
#15517 = CARTESIAN_POINT('Ctrl Pts',(-20.4898441310091,13.8589385924913,124.040196718243)) ;
#15518 = CARTESIAN_POINT('Ctrl Pts',(-20.4898587477926,13.8589372578331,124.040171582421)) ;
#15519 = CARTESIAN_POINT('Ctrl Pts',(-20.4898660690434,13.8589365893067,124.04015899189)) ;
#15520 = CARTESIAN_POINT('Ctrl Pts',(-20.4898807390652,13.8589352496944,124.040133762486)) ;
#15521 = CARTESIAN_POINT('Ctrl Pts',(-20.4898880878917,13.8589345786033,124.040121123514)) ;
#15522 = CARTESIAN_POINT('Ctrl Pts',(-20.4899028125276,13.8589332339102,124.040095798141)) ;
#15523 = CARTESIAN_POINT('Ctrl Pts',(-20.4899101893572,13.8589325602149,124.040083109981)) ;
#15524 = CARTESIAN_POINT('Ctrl Pts',(-20.4899249737321,13.858931209972,124.040057679799)) ;
#15525 = CARTESIAN_POINT('Ctrl Pts',(-20.4899323805983,13.8589305334861,124.040044938941)) ;
#15526 = CARTESIAN_POINT('Ctrl Pts',(-20.4899472258219,13.8589291775908,124.040019402016)) ;
#15527 = CARTESIAN_POINT('Ctrl Pts',(-20.4899546639547,13.8589284982015,124.040006606331)) ;
#15528 = CARTESIAN_POINT('Ctrl Pts',(-20.4899695730428,13.858927136377,124.039980957449)) ;
#15529 = CARTESIAN_POINT('Ctrl Pts',(-20.4899770439415,13.8589264539467,124.039968104345)) ;
#15530 = CARTESIAN_POINT('Ctrl Pts',(-20.4899920187781,13.8589250860198,124.039942340237)) ;
#15531 = CARTESIAN_POINT('Ctrl Pts',(-20.4899995233242,13.8589244004673,124.039929428182)) ;
#15532 = CARTESIAN_POINT('Ctrl Pts',(-20.490014567712,13.8589230260892,124.039903542275)) ;
#15533 = CARTESIAN_POINT('Ctrl Pts',(-20.4900221074345,13.8589223372742,124.039890568624)) ;
#15534 = CARTESIAN_POINT('Ctrl Pts',(-20.4900372239377,13.8589209562093,124.039864556478)) ;
#15535 = CARTESIAN_POINT('Ctrl Pts',(-20.4900448004046,13.8589202639877,124.039851518516)) ;
#15536 = CARTESIAN_POINT('Ctrl Pts',(-20.4900599912619,13.85891887603,124.039825376245)) ;
#15537 = CARTESIAN_POINT('Ctrl Pts',(-20.4900676057556,13.858918180284,124.039812271751)) ;
#15538 = CARTESIAN_POINT('Ctrl Pts',(-20.4900828737317,13.8589167851793,124.039785994564)) ;
#15539 = CARTESIAN_POINT('Ctrl Pts',(-20.4900905274526,13.8589160857985,124.039772821455)) ;
#15540 = CARTESIAN_POINT('Ctrl Pts',(-20.4901058758524,13.8589146832433,124.039746403629)) ;
#15541 = CARTESIAN_POINT('Ctrl Pts',(-20.4901135703395,13.8589139800862,124.039733159238)) ;
#15542 = CARTESIAN_POINT('Ctrl Pts',(-20.4901290017798,13.8589125698397,124.039706596234)) ;
#15543 = CARTESIAN_POINT('Ctrl Pts',(-20.490136738525,13.8589118627691,124.039693277974)) ;
#15544 = CARTESIAN_POINT('Ctrl Pts',(-20.4901522556526,13.8589104445877,124.039666565199)) ;
#15545 = CARTESIAN_POINT('Ctrl Pts',(-20.4901600360511,13.8589097334752,124.03965317065)) ;
#15546 = CARTESIAN_POINT('Ctrl Pts',(-20.4901756416255,13.858908307105,124.039626303313)) ;
#15547 = CARTESIAN_POINT('Ctrl Pts',(-20.4901834669257,13.8589075918356,124.039612830306)) ;
#15548 = CARTESIAN_POINT('Ctrl Pts',(-20.4901991644811,13.8589061569517,124.039585802283)) ;
#15549 = CARTESIAN_POINT('Ctrl Pts',(-20.4902070363817,13.8589054373692,124.039572247872)) ;
#15550 = CARTESIAN_POINT('Ctrl Pts',(-20.4902228285179,13.8589039937319,124.039545054645)) ;
#15551 = CARTESIAN_POINT('Ctrl Pts',(-20.4902307486361,13.8589032696875,124.039531416024)) ;
#15552 = CARTESIAN_POINT('Ctrl Pts',(-20.4902466377406,13.8589018170766,124.039504053438)) ;
#15553 = CARTESIAN_POINT('Ctrl Pts',(-20.490254607265,13.8589010884606,124.039490328539)) ;
#15554 = CARTESIAN_POINT('Ctrl Pts',(-20.4902705968986,13.8588996265486,124.039462790417)) ;
#15555 = CARTESIAN_POINT('Ctrl Pts',(-20.4902786172617,13.858898893229,124.039448976749)) ;
#15556 = CARTESIAN_POINT('Ctrl Pts',(-20.4902947108765,13.858897421698,124.039421257098)) ;
#15557 = CARTESIAN_POINT('Ctrl Pts',(-20.4903027838594,13.8588966835109,124.03940735157)) ;
#15558 = CARTESIAN_POINT('Ctrl Pts',(-20.490318984017,13.8588952021245,124.039379445929)) ;
#15559 = CARTESIAN_POINT('Ctrl Pts',(-20.4903271111362,13.85889445893,124.039365445904)) ;
#15560 = CARTESIAN_POINT('Ctrl Pts',(-20.4903434209091,13.858892967405,124.039337348932)) ;
#15561 = CARTESIAN_POINT('Ctrl Pts',(-20.4903516036067,13.8588922190701,124.0393232519)) ;
#15562 = CARTESIAN_POINT('Ctrl Pts',(-20.490368026599,13.8588907170744,124.039294957334)) ;
#15563 = CARTESIAN_POINT('Ctrl Pts',(-20.4903762666247,13.8588899634379,124.039280760255)) ;
#15564 = CARTESIAN_POINT('Ctrl Pts',(-20.4903928059815,13.8588884506815,124.039252262623)) ;
#15565 = CARTESIAN_POINT('Ctrl Pts',(-20.4904011051923,13.8588876915722,124.039237962269)) ;
#15566 = CARTESIAN_POINT('Ctrl Pts',(-20.4904177630321,13.8588861678587,124.039209257865)) ;
#15567 = CARTESIAN_POINT('Ctrl Pts',(-20.49042612239,13.8588854031874,124.03919485255)) ;
#15568 = CARTESIAN_POINT('Ctrl Pts',(-20.4904429039086,13.8588838680388,124.039165932363)) ;
#15569 = CARTESIAN_POINT('Ctrl Pts',(-20.4904513255905,13.858883097605,124.039151418306)) ;
#15570 = CARTESIAN_POINT('Ctrl Pts',(-20.4904682332062,13.8588815507975,124.039122278108)) ;
#15571 = CARTESIAN_POINT('Ctrl Pts',(-20.4904767189753,13.8588807744384,124.039107652241)) ;
#15572 = CARTESIAN_POINT('Ctrl Pts',(-20.4904937556984,13.8588792156936,124.039078286781)) ;
#15573 = CARTESIAN_POINT('Ctrl Pts',(-20.4905023070026,13.8588784332754,124.039063546575)) ;
#15574 = CARTESIAN_POINT('Ctrl Pts',(-20.4905194768878,13.8588768622195,124.039033948802)) ;
#15575 = CARTESIAN_POINT('Ctrl Pts',(-20.4905280955026,13.8588760735782,124.039019091165)) ;
#15576 = CARTESIAN_POINT('Ctrl Pts',(-20.4905454021255,13.8588744898809,124.038989254846)) ;
#15577 = CARTESIAN_POINT('Ctrl Pts',(-20.4905540899291,13.8588736948431,124.038974276506)) ;
#15578 = CARTESIAN_POINT('Ctrl Pts',(-20.4905715368505,13.8588720981754,124.038944195435)) ;
#15579 = CARTESIAN_POINT('Ctrl Pts',(-20.4905802958176,13.8588712965588,124.038929092952)) ;
#15580 = CARTESIAN_POINT('Ctrl Pts',(-20.4905978858839,13.8588696866569,124.038898762151)) ;
#15581 = CARTESIAN_POINT('Ctrl Pts',(-20.4906067173874,13.8588688783342,124.038883533122)) ;
#15582 = CARTESIAN_POINT('Ctrl Pts',(-20.4906244559245,13.8588672547074,124.038852943332)) ;
#15583 = CARTESIAN_POINT('Ctrl Pts',(-20.4906333625065,13.8588664394441,124.038837583336)) ;
#15584 = CARTESIAN_POINT('Ctrl Pts',(-20.4925060872012,13.8586950124741,124.035607785913)) ;
#15585 = CARTESIAN_POINT('Ctrl Pts',(-20.4943555594237,13.8585242006034,124.032385061572)) ;
#15586 = CARTESIAN_POINT('Ctrl Pts',(-20.4984073425928,13.8581466155113,124.025251295366)) ;
#15587 = CARTESIAN_POINT('Ctrl Pts',(-20.5006030102197,13.8579397538586,124.021336545848)) ;
#15588 = CARTESIAN_POINT('Ctrl Pts',(-20.5067339656082,13.8573557488863,124.010266070541)) ;
#15589 = CARTESIAN_POINT('Ctrl Pts',(-20.5106202659879,13.8569779812798,124.003083514696)) ;
#15590 = CARTESIAN_POINT('Ctrl Pts',(-20.5250084049492,13.855550733782,123.97585763689)) ;
#15591 = CARTESIAN_POINT('Ctrl Pts',(-20.5350356906742,13.8544962881016,123.95556857681)) ;
#15592 = CARTESIAN_POINT('Ctrl Pts',(-20.5462215008487,13.853253601279,123.931297912025)) ;
#15593 = CARTESIAN_POINT('Ctrl Pts',(-20.5479180270713,13.8530631769229,123.927568714486)) ;
#15594 = CARTESIAN_POINT('Ctrl Pts',(-20.5564722995342,13.8520931399368,123.908517307534)) ;
#15595 = CARTESIAN_POINT('Ctrl Pts',(-20.5630392767027,13.8513157188205,123.893066300478)) ;
#15596 = CARTESIAN_POINT('Ctrl Pts',(-20.5710773663457,13.8503216087064,123.873042918714)) ;
#15597 = CARTESIAN_POINT('Ctrl Pts',(-20.5728360442873,13.8501012649038,123.868588055111)) ;
#15598 = CARTESIAN_POINT('Ctrl Pts',(-20.5755554935889,13.8497560278985,123.861581855792)) ;
#15599 = CARTESIAN_POINT('Ctrl Pts',(-20.5765335913721,13.8496309104058,123.859037308292)) ;
#15600 = CARTESIAN_POINT('Ctrl Pts',(-20.5784730666476,13.8493809012957,123.853942004285)) ;
#15601 = CARTESIAN_POINT('Ctrl Pts',(-20.5794344397893,13.8492560103599,123.851391262342)) ;
#15602 = CARTESIAN_POINT('Ctrl Pts',(-20.5813437051298,13.8490060249524,123.846274896412)) ;
#15603 = CARTESIAN_POINT('Ctrl Pts',(-20.5822915354826,13.8488809319206,123.843709265631)) ;
#15604 = CARTESIAN_POINT('Ctrl Pts',(-20.5844466743752,13.8485941973408,123.837816207583)) ;
#15605 = CARTESIAN_POINT('Ctrl Pts',(-20.5856482861597,13.8484326303224,123.834486719443)) ;
#15606 = CARTESIAN_POINT('Ctrl Pts',(-20.5887268310778,13.8480142128925,123.825841703016)) ;
#15607 = CARTESIAN_POINT('Ctrl Pts',(-20.59058198091,13.8477576376177,123.820518494502)) ;
#15608 = CARTESIAN_POINT('Ctrl Pts',(-20.5961275571019,13.8469766745545,123.80425264692)) ;
#15609 = CARTESIAN_POINT('Ctrl Pts',(-20.599702417897,13.8464536308975,123.793271234192)) ;
#15610 = CARTESIAN_POINT('Ctrl Pts',(-20.6078865899836,13.8452052115143,123.76689442607)) ;
#15611 = CARTESIAN_POINT('Ctrl Pts',(-20.6123521773435,13.8444809736554,123.751456638938)) ;
#15612 = CARTESIAN_POINT('Ctrl Pts',(-20.6221057458753,13.8427831404181,123.715127918939)) ;
#15613 = CARTESIAN_POINT('Ctrl Pts',(-20.6271535931931,13.8418083464274,123.69417799717)) ;
#15614 = CARTESIAN_POINT('Ctrl Pts',(-20.632662572683,13.8406070400145,123.668405883066)) ;
#15615 = CARTESIAN_POINT('Ctrl Pts',(-20.6336405850954,13.8403875204966,123.663697807199)) ;
#15616 = CARTESIAN_POINT('Ctrl Pts',(-20.6351215793787,13.8400450546363,123.656355930081)) ;
#15617 = CARTESIAN_POINT('Ctrl Pts',(-20.6356432956637,13.8399223495409,123.653725947344)) ;
#15618 = CARTESIAN_POINT('Ctrl Pts',(-20.6366693634811,13.8396768262338,123.648464885835)) ;
#15619 = CARTESIAN_POINT('Ctrl Pts',(-20.6371737264599,13.8395540088683,123.645833824075)) ;
#15620 = CARTESIAN_POINT('Ctrl Pts',(-20.6382647529297,13.8392835638612,123.640041730175)) ;
#15621 = CARTESIAN_POINT('Ctrl Pts',(-20.6388476866218,13.8391358901061,123.636880017672)) ;
#15622 = CARTESIAN_POINT('Ctrl Pts',(-20.6404368331247,13.8387242872355,123.628070341032)) ;
#15623 = CARTESIAN_POINT('Ctrl Pts',(-20.6414163682009,13.8384600341338,123.622417663562)) ;
#15624 = CARTESIAN_POINT('Ctrl Pts',(-20.6436865203896,13.8378211990229,123.608758865712)) ;
#15625 = CARTESIAN_POINT('Ctrl Pts',(-20.6449382045098,13.8374461951142,123.600746561701)) ;
#15626 = CARTESIAN_POINT('Ctrl Pts',(-20.6496729280767,13.8359307419014,123.568376055449)) ;
#15627 = CARTESIAN_POINT('Ctrl Pts',(-20.6525143594187,13.8347851345806,123.543929710565)) ;
#15628 = CARTESIAN_POINT('Ctrl Pts',(-20.6560731010156,13.8328688437911,123.50274127297)) ;
#15629 = CARTESIAN_POINT('Ctrl Pts',(-20.6571787555777,13.8320952927126,123.486039873176)) ;
#15630 = CARTESIAN_POINT('Ctrl Pts',(-20.6582002209345,13.8310728765529,123.463860245269)) ;
#15631 = CARTESIAN_POINT('Ctrl Pts',(-20.6584158938758,13.8308214518473,123.458397704149)) ;
#15632 = CARTESIAN_POINT('Ctrl Pts',(-20.6587240404368,13.8303911552722,123.449035373961)) ;
#15633 = CARTESIAN_POINT('Ctrl Pts',(-20.6588341060291,13.8302121351201,123.445136252507)) ;
#15634 = CARTESIAN_POINT('Ctrl Pts',(-20.6590191586386,13.8298516231369,123.437276512479)) ;
#15635 = CARTESIAN_POINT('Ctrl Pts',(-20.6590935730801,13.8296701382022,123.433315924923)) ;
#15636 = CARTESIAN_POINT('Ctrl Pts',(-20.6592073956233,13.8292988307163,123.425205395734)) ;
#15637 = CARTESIAN_POINT('Ctrl Pts',(-20.6592449656735,13.8291090253997,123.421055476931)) ;
#15638 = CARTESIAN_POINT('Ctrl Pts',(-20.6592848914349,13.8286610542947,123.411252675077)) ;
#15639 = CARTESIAN_POINT('Ctrl Pts',(-20.6592695695077,13.828403027617,123.40559980729)) ;
#15640 = CARTESIAN_POINT('Ctrl Pts',(-20.6591212732369,13.8276907096031,123.389980040162)) ;
#15641 = CARTESIAN_POINT('Ctrl Pts',(-20.6589074274615,13.8272369760471,123.380014318608)) ;
#15642 = CARTESIAN_POINT('Ctrl Pts',(-20.6576959315526,13.825587946215,123.343772802066)) ;
#15643 = CARTESIAN_POINT('Ctrl Pts',(-20.6559884885777,13.824395522853,123.317527758314)) ;
#15644 = CARTESIAN_POINT('Ctrl Pts',(-20.6523816219189,13.8226905337696,123.280273378837)) ;
#15645 = CARTESIAN_POINT('Ctrl Pts',(-20.6511606008671,13.8221825655415,123.269205585923)) ;
#15646 = CARTESIAN_POINT('Ctrl Pts',(-20.6489900538264,13.8213755280736,123.251682299429)) ;
#15647 = CARTESIAN_POINT('Ctrl Pts',(-20.6481375719521,13.8210770925249,123.245215369656)) ;
#15648 = CARTESIAN_POINT('Ctrl Pts',(-20.6464332518936,13.8205132799827,123.233023662662)) ;
#15649 = CARTESIAN_POINT('Ctrl Pts',(-20.6455921939868,13.8202479758133,123.227297548119)) ;
#15650 = CARTESIAN_POINT('Ctrl Pts',(-20.6433621649221,13.819575707691,123.212815259956)) ;
#15651 = CARTESIAN_POINT('Ctrl Pts',(-20.6419197522443,13.8191684611513,123.204067652846)) ;
#15652 = CARTESIAN_POINT('Ctrl Pts',(-20.6382952721087,13.8182061765109,123.183455224921)) ;
#15653 = CARTESIAN_POINT('Ctrl Pts',(-20.6360342618968,13.8176508528775,123.171605183326)) ;
#15654 = CARTESIAN_POINT('Ctrl Pts',(-20.6304391192508,13.8163731021567,123.144424107673)) ;
#15655 = CARTESIAN_POINT('Ctrl Pts',(-20.6269871583983,13.8156506840672,123.129119341833)) ;
#15656 = CARTESIAN_POINT('Ctrl Pts',(-20.6222365092715,13.814735199601,123.109761915679)) ;
#15657 = CARTESIAN_POINT('Ctrl Pts',(-20.6212039949632,13.8145404259391,123.105645421179)) ;
#15658 = CARTESIAN_POINT('Ctrl Pts',(-20.6190653056221,13.8141453570206,123.097299116212)) ;
#15659 = CARTESIAN_POINT('Ctrl Pts',(-20.6179578661426,13.8139450614029,123.093069701326)) ;
#15660 = CARTESIAN_POINT('Ctrl Pts',(-20.6152923470607,13.8134727285282,123.083103507354)) ;
#15661 = CARTESIAN_POINT('Ctrl Pts',(-20.6137154874376,13.8132008056718,123.077371858019)) ;
#15662 = CARTESIAN_POINT('Ctrl Pts',(-20.6059504255896,13.8118962166956,123.049914365113)) ;
#15663 = CARTESIAN_POINT('Ctrl Pts',(-20.5992179952884,13.8108659483098,123.028357208965)) ;
#15664 = CARTESIAN_POINT('Ctrl Pts',(-20.5919019615583,13.8098330347236,123.006984856534)) ;
#15665 = CARTESIAN_POINT('',(-18.6288026007436,14.0000000000496,122.435409149151)) ;
#15666 = CARTESIAN_POINT('Origin',(-19.4092722359534,14.0000000000496,123.411814366564)) ;
#15667 = CARTESIAN_POINT('Ctrl Pts',(-20.591901915765,13.7497304410597,123.00698472277)) ;
#15668 = CARTESIAN_POINT('Ctrl Pts',(-20.6063625370814,13.7517786882633,123.049228630798)) ;
#15669 = CARTESIAN_POINT('Ctrl Pts',(-20.618549234163,13.75381645875,123.09221653556)) ;
#15670 = CARTESIAN_POINT('Ctrl Pts',(-20.628409768268,13.7558580462895,123.135764230942)) ;
#15671 = CARTESIAN_POINT('Ctrl Pts',(-20.6444583543449,13.7591808473683,123.206640608462)) ;
#15672 = CARTESIAN_POINT('Ctrl Pts',(-20.6542956538904,13.7625238879391,123.278781574249)) ;
#15673 = CARTESIAN_POINT('Ctrl Pts',(-20.6578098406935,13.7658441537945,123.351367285367)) ;
#15674 = CARTESIAN_POINT('Ctrl Pts',(-20.6613282498486,13.7691684090029,123.424040209387)) ;
#15675 = CARTESIAN_POINT('Ctrl Pts',(-20.6584949399899,13.7724790496621,123.496879685578)) ;
#15676 = CARTESIAN_POINT('Ctrl Pts',(-20.6493425744953,13.7758422437701,123.569057985016)) ;
#15677 = CARTESIAN_POINT('Ctrl Pts',(-20.6402714976604,13.779175566962,123.640595217702)) ;
#15678 = CARTESIAN_POINT('Ctrl Pts',(-20.6250273305645,13.7824798826356,123.71121346105)) ;
#15679 = CARTESIAN_POINT('Ctrl Pts',(-20.6037793807761,13.7857518148978,123.780124943446)) ;
#15680 = CARTESIAN_POINT('Ctrl Pts',(-20.5845554178812,13.7887120771833,123.842472219009)) ;
#15681 = CARTESIAN_POINT('Ctrl Pts',(-20.5604806409632,13.791688203282,123.903216027636)) ;
#15682 = CARTESIAN_POINT('Ctrl Pts',(-20.5317752294988,13.79470840778,123.961802575126)) ;
#15683 = CARTESIAN_POINT('Ctrl Pts',(-20.5286018957133,13.7950422861842,123.968279217022)) ;
#15684 = CARTESIAN_POINT('Ctrl Pts',(-20.5253721137233,13.7953763684717,123.974729168241)) ;
#15685 = CARTESIAN_POINT('Ctrl Pts',(-20.522087337898,13.7957103411746,123.981149548122)) ;
#15686 = CARTESIAN_POINT('Ctrl Pts',(-20.4891410878708,13.799060082149,124.04554585766)) ;
#15687 = CARTESIAN_POINT('Ctrl Pts',(-20.4506672093765,13.8023742322835,124.106961354719)) ;
#15688 = CARTESIAN_POINT('Ctrl Pts',(-20.4070969000589,13.8056510812251,124.164706085059)) ;
#15689 = CARTESIAN_POINT('Ctrl Pts',(-20.3632728925256,13.8089470103785,124.222787047464)) ;
#15690 = CARTESIAN_POINT('Ctrl Pts',(-20.3144647152299,13.8122732103732,124.276927063412)) ;
#15691 = CARTESIAN_POINT('Ctrl Pts',(-20.2612249334786,13.8156496387038,124.32651464603)) ;
#15692 = CARTESIAN_POINT('Ctrl Pts',(-20.208431235917,13.8189977766988,124.375686745416)) ;
#15693 = CARTESIAN_POINT('Ctrl Pts',(-20.1514799540918,13.8222863880002,124.420195860513)) ;
#15694 = CARTESIAN_POINT('Ctrl Pts',(-20.0910054456041,13.825564595863,124.459545167359)) ;
#15695 = CARTESIAN_POINT('Ctrl Pts',(-20.030021323317,13.8288704289188,124.499226067637)) ;
#15696 = CARTESIAN_POINT('Ctrl Pts',(-19.9656903848931,13.8322259945227,124.533506066526)) ;
#15697 = CARTESIAN_POINT('Ctrl Pts',(-19.8987443715233,13.8355632563884,124.561995669045)) ;
#15698 = CARTESIAN_POINT('Ctrl Pts',(-19.8709317381632,13.8369497174489,124.573831637007)) ;
#15699 = CARTESIAN_POINT('Ctrl Pts',(-19.8426988053596,13.8383268906909,124.584654958882)) ;
#15700 = CARTESIAN_POINT('Ctrl Pts',(-19.814101322745,13.8397085566956,124.594444237049)) ;
#15701 = CARTESIAN_POINT('Ctrl Pts',(-19.7738950433856,13.8416510930409,124.608207352427)) ;
#15702 = CARTESIAN_POINT('Ctrl Pts',(-19.7330136490518,13.8436023746858,124.619910968345)) ;
#15703 = CARTESIAN_POINT('Ctrl Pts',(-19.6916159984558,13.8455619284086,124.629509730706)) ;
#15704 = CARTESIAN_POINT('Ctrl Pts',(-19.621434395943,13.8488839676667,124.6457825509)) ;
#15705 = CARTESIAN_POINT('Ctrl Pts',(-19.5499773540891,13.8521761049423,124.655957672648)) ;
#15706 = CARTESIAN_POINT('Ctrl Pts',(-19.4780413667292,13.8554628014865,124.659921255708)) ;
#15707 = CARTESIAN_POINT('Ctrl Pts',(-19.405565930974,13.8587741449875,124.6639145617)) ;
#15708 = CARTESIAN_POINT('Ctrl Pts',(-19.3328805747897,13.8621218045964,124.661587512882)) ;
#15709 = CARTESIAN_POINT('Ctrl Pts',(-19.2608092074874,13.8654379472561,124.652966544685)) ;
#15710 = CARTESIAN_POINT('Ctrl Pts',(-19.1885665372109,13.868761971896,124.644325085723)) ;
#15711 = CARTESIAN_POINT('Ctrl Pts',(-19.1172187765043,13.8720647651682,124.629393167417)) ;
#15712 = CARTESIAN_POINT('Ctrl Pts',(-19.0475756931357,13.8754364916762,124.60834084391)) ;
#15713 = CARTESIAN_POINT('Ctrl Pts',(-18.9829156430693,13.8785669677303,124.588794835518)) ;
#15714 = CARTESIAN_POINT('Ctrl Pts',(-18.9199468679241,13.881670349849,124.564040084399)) ;
#15715 = CARTESIAN_POINT('Ctrl Pts',(-18.8592840273916,13.884728198393,124.53431736011)) ;
#15716 = CARTESIAN_POINT('Ctrl Pts',(-18.855298686588,13.8849290885668,124.532364678949)) ;
#15717 = CARTESIAN_POINT('Ctrl Pts',(-18.8513235602125,13.8851299295488,124.530390680638)) ;
#15718 = CARTESIAN_POINT('Ctrl Pts',(-18.8473593255089,13.8853307575762,124.528395703123)) ;
#15719 = CARTESIAN_POINT('Ctrl Pts',(-18.7823244508309,13.8886254226425,124.495667289604)) ;
#15720 = CARTESIAN_POINT('Ctrl Pts',(-18.7202769990253,13.8919691269502,124.457321787188)) ;
#15721 = CARTESIAN_POINT('Ctrl Pts',(-18.6619196785191,13.895335505774,124.413794483619)) ;
#15722 = CARTESIAN_POINT('Ctrl Pts',(-18.6038188900024,13.8986870863883,124.37045852101)) ;
#15723 = CARTESIAN_POINT('Ctrl Pts',(-18.5495970331295,13.9019816026392,124.322150842453)) ;
#15724 = CARTESIAN_POINT('Ctrl Pts',(-18.4998669553414,13.9052962640052,124.269416859373)) ;
#15725 = CARTESIAN_POINT('Ctrl Pts',(-18.4501529716476,13.9086098526508,124.216699942537)) ;
#15726 = CARTESIAN_POINT('Ctrl Pts',(-18.4051169093404,13.9119457639183,124.159759999861)) ;
#15727 = CARTESIAN_POINT('Ctrl Pts',(-18.365267674092,13.9152538452324,124.099240344317)) ;
#15728 = CARTESIAN_POINT('Ctrl Pts',(-18.3252556152,13.9185754433392,124.038473405963)) ;
#15729 = CARTESIAN_POINT('Ctrl Pts',(-18.2906263158313,13.9218932210603,123.974330716603)) ;
#15730 = CARTESIAN_POINT('Ctrl Pts',(-18.2617728896448,13.9252517568863,123.907541358262)) ;
#15731 = CARTESIAN_POINT('Ctrl Pts',(-18.2488857250803,13.9267518215097,123.87771039654)) ;
#15732 = CARTESIAN_POINT('Ctrl Pts',(-18.237166646834,13.928249280156,123.847388105641)) ;
#15733 = CARTESIAN_POINT('Ctrl Pts',(-18.2266423654683,13.9297397117846,123.816643453356)) ;
#15734 = CARTESIAN_POINT('Ctrl Pts',(-18.2137737426247,13.9315621452446,123.779050260911)) ;
#15735 = CARTESIAN_POINT('Ctrl Pts',(-18.2027048827386,13.9333715008147,123.740864689436)) ;
#15736 = CARTESIAN_POINT('Ctrl Pts',(-18.1934735105708,13.9351820521686,123.702216603874)) ;
#15737 = CARTESIAN_POINT('Ctrl Pts',(-18.176621872162,13.9384871682643,123.631665492809)) ;
#15738 = CARTESIAN_POINT('Ctrl Pts',(-18.1659433494583,13.9418197322647,123.559782448994)) ;
#15739 = CARTESIAN_POINT('Ctrl Pts',(-18.161558421319,13.9451493424424,123.487380475678)) ;
#15740 = CARTESIAN_POINT('Ctrl Pts',(-18.1571794512759,13.9484744284551,123.415076879786)) ;
#15741 = CARTESIAN_POINT('Ctrl Pts',(-18.1590936196939,13.9517699060233,123.342529732206)) ;
#15742 = CARTESIAN_POINT('Ctrl Pts',(-18.1672792240671,13.9551028655101,123.270558009178)) ;
#15743 = CARTESIAN_POINT('Ctrl Pts',(-18.1754485141975,13.958429182273,123.198729728726)) ;
#15744 = CARTESIAN_POINT('Ctrl Pts',(-18.1898334630847,13.9617514594568,123.127745020702)) ;
#15745 = CARTESIAN_POINT('Ctrl Pts',(-18.2102729618659,13.9650365151445,123.058401377536)) ;
#15746 = CARTESIAN_POINT('Ctrl Pts',(-18.2301882885713,13.9682373253976,122.990836055931)) ;
#15747 = CARTESIAN_POINT('Ctrl Pts',(-18.2557778940949,13.9714482125329,122.925078207253)) ;
#15748 = CARTESIAN_POINT('Ctrl Pts',(-18.2867692424076,13.9747119452089,122.861826158003)) ;
#15749 = CARTESIAN_POINT('Ctrl Pts',(-18.2877875997057,13.9748191895262,122.859747733233)) ;
#15750 = CARTESIAN_POINT('Ctrl Pts',(-18.2888117423678,13.9749264410021,122.857672111156)) ;
#15751 = CARTESIAN_POINT('Ctrl Pts',(-18.2898416231274,13.9750336881797,122.855599387312)) ;
#15752 = CARTESIAN_POINT('Ctrl Pts',(-18.3220556999662,13.9783883181092,122.790765779584)) ;
#15753 = CARTESIAN_POINT('Ctrl Pts',(-18.3598411869483,13.9817039828769,122.728853071035)) ;
#15754 = CARTESIAN_POINT('Ctrl Pts',(-18.4027743783516,13.9849814727061,122.67055728382)) ;
#15755 = CARTESIAN_POINT('Ctrl Pts',(-18.445920839689,13.9882752434131,122.611971913224)) ;
#15756 = CARTESIAN_POINT('Ctrl Pts',(-18.494096845034,13.9916059899517,122.557269259677)) ;
#15757 = CARTESIAN_POINT('Ctrl Pts',(-18.5467569764074,13.9949784443263,122.507067204576)) ;
#15758 = CARTESIAN_POINT('Ctrl Pts',(-18.5730635066385,13.9966631642585,122.481988613889)) ;
#15759 = CARTESIAN_POINT('Ctrl Pts',(-18.6004389456167,13.9983320474216,122.458081011944)) ;
#15760 = CARTESIAN_POINT('Ctrl Pts',(-18.6288026007436,14.0000000000496,122.435409149151)) ;
#15761 = CARTESIAN_POINT('Origin',(-19.4092722359532,16.5113612779716,123.411814366564)) ;
#15762 = CARTESIAN_POINT('',(-20.5919016415084,13.3897528569022,123.006983921601)) ;
#15763 = CARTESIAN_POINT('',(-20.5919016872816,13.4498327922206,123.006984055316)) ;
#15764 = CARTESIAN_POINT('',(-20.5919021064381,16.5113612779716,123.006985279772)) ;
#15765 = CARTESIAN_POINT('Ctrl Pts',(-20.5919019615583,13.8098330347217,123.006984856534)) ;
#15766 = CARTESIAN_POINT('Ctrl Pts',(-20.5796177619238,13.8080986910531,122.971098985364)) ;
#15767 = CARTESIAN_POINT('Ctrl Pts',(-20.5657063569306,13.8063585292808,122.935791351964)) ;
#15768 = CARTESIAN_POINT('Ctrl Pts',(-20.5502165472103,13.8046080448643,122.901181348942)) ;
#15769 = CARTESIAN_POINT('Ctrl Pts',(-20.520770181677,13.8012803471765,122.835387203082)) ;
#15770 = CARTESIAN_POINT('Ctrl Pts',(-20.4856929834176,13.7979653615935,122.77227295707)) ;
#15771 = CARTESIAN_POINT('Ctrl Pts',(-20.4453721849218,13.7947034100367,122.712531236621)) ;
#15772 = CARTESIAN_POINT('Ctrl Pts',(-20.4046683728878,13.7914104726945,122.652222020274)) ;
#15773 = CARTESIAN_POINT('Ctrl Pts',(-20.3587800304366,13.7880836260627,122.595586200155)) ;
#15774 = CARTESIAN_POINT('Ctrl Pts',(-20.3082259775898,13.7847053333764,122.543262600419)) ;
#15775 = CARTESIAN_POINT('Ctrl Pts',(-20.2580339768125,13.7813512349492,122.491313725686)) ;
#15776 = CARTESIAN_POINT('Ctrl Pts',(-20.2034335311599,13.7780588930693,122.443813244608)) ;
#15777 = CARTESIAN_POINT('Ctrl Pts',(-20.1450350735511,13.7747785422853,122.401293190692)) ;
#15778 = CARTESIAN_POINT('Ctrl Pts',(-20.0864707072361,13.7714888720984,122.358652338258)) ;
#15779 = CARTESIAN_POINT('Ctrl Pts',(-20.0243124708696,13.7681516077852,122.321184637964)) ;
#15780 = CARTESIAN_POINT('Ctrl Pts',(-19.959260294232,13.7648235341903,122.289311299385)) ;
#15781 = CARTESIAN_POINT('Ctrl Pts',(-19.9590204835755,13.7648112654615,122.289193800377)) ;
#15782 = CARTESIAN_POINT('Ctrl Pts',(-19.9587804848829,13.7647989897311,122.289076304615)) ;
#15783 = CARTESIAN_POINT('Ctrl Pts',(-19.9585405969292,13.7647867222929,122.288958958372)) ;
#15784 = CARTESIAN_POINT('Ctrl Pts',(-19.8932580416504,13.7614482898999,122.257024622146)) ;
#15785 = CARTESIAN_POINT('Ctrl Pts',(-19.8253154321585,13.7581503872716,122.230844614302)) ;
#15786 = CARTESIAN_POINT('Ctrl Pts',(-19.7554846306214,13.7547995544403,122.210716128345)) ;
#15787 = CARTESIAN_POINT('Ctrl Pts',(-19.6860504463898,13.7514677533008,122.190701965948)) ;
#15788 = CARTESIAN_POINT('Ctrl Pts',(-19.6150115325245,13.7481451053711,122.176746188182)) ;
#15789 = CARTESIAN_POINT('Ctrl Pts',(-19.5431634314469,13.7448689186883,122.169005794078)) ;
#15790 = CARTESIAN_POINT('Ctrl Pts',(-19.4708701670743,13.7415724330966,122.161217441304)) ;
#15791 = CARTESIAN_POINT('Ctrl Pts',(-19.3980395735329,13.738248527013,122.159751929489)) ;
#15792 = CARTESIAN_POINT('Ctrl Pts',(-19.3254946073445,13.7348767418505,122.164625002826)) ;
#15793 = CARTESIAN_POINT('Ctrl Pts',(-19.253365677566,13.7315242934589,122.169470129691)) ;
#15794 = CARTESIAN_POINT('Ctrl Pts',(-19.1817924542661,13.7282254390405,122.180562543553)) ;
#15795 = CARTESIAN_POINT('Ctrl Pts',(-19.1115674292446,13.7249412096492,122.197783128029)) ;
#15796 = CARTESIAN_POINT('Ctrl Pts',(-19.0754163348061,13.7232505233612,122.206648101385)) ;
#15797 = CARTESIAN_POINT('Ctrl Pts',(-19.0396689861174,13.7215545046655,122.217126244833)) ;
#15798 = CARTESIAN_POINT('Ctrl Pts',(-19.004443029643,13.7198446883909,122.229184536992)) ;
#15799 = CARTESIAN_POINT('Ctrl Pts',(-18.9708669395833,13.7182149542128,122.240678058929)) ;
#15800 = CARTESIAN_POINT('Ctrl Pts',(-18.9377955116159,13.7165744351769,122.253596611336)) ;
#15801 = CARTESIAN_POINT('Ctrl Pts',(-18.9053287039429,13.7149435467734,122.267899633457)) ;
#15802 = CARTESIAN_POINT('Ctrl Pts',(-18.8390299193649,13.7116131941244,122.297107093332)) ;
#15803 = CARTESIAN_POINT('Ctrl Pts',(-18.7754054879488,13.7083272240729,122.332018128119)) ;
#15804 = CARTESIAN_POINT('Ctrl Pts',(-18.7151634716232,13.7049882872184,122.372240885104)) ;
#15805 = CARTESIAN_POINT('Ctrl Pts',(-18.6552481525976,13.701667457687,122.412245510842)) ;
#15806 = CARTESIAN_POINT('Ctrl Pts',(-18.5989034145165,13.6983525297203,122.45735485489)) ;
#15807 = CARTESIAN_POINT('Ctrl Pts',(-18.5467568890626,13.6950873699958,122.507067287843)) ;
#15808 = CARTESIAN_POINT('Ctrl Pts',(-18.49409422378,13.6917898921261,122.557271768281)) ;
#15809 = CARTESIAN_POINT('Ctrl Pts',(-18.445918683257,13.6884646048685,122.611974839834)) ;
#15810 = CARTESIAN_POINT('Ctrl Pts',(-18.4027743696019,13.6850888225092,122.6705572957)) ;
#15811 = CARTESIAN_POINT('Ctrl Pts',(-18.3598432833932,13.6817297239117,122.728850225869)) ;
#15812 = CARTESIAN_POINT('Ctrl Pts',(-18.3220572040567,13.6784213609289,122.790762571335)) ;
#15813 = CARTESIAN_POINT('Ctrl Pts',(-18.2898410039093,13.6751395513273,122.855600633544)) ;
#15814 = CARTESIAN_POINT('Ctrl Pts',(-18.2888117333323,13.6750347012815,122.85767213513)) ;
#15815 = CARTESIAN_POINT('Ctrl Pts',(-18.2877875931879,13.6749297900114,122.859747751965)) ;
#15816 = CARTESIAN_POINT('Ctrl Pts',(-18.2867698102722,13.6748249334085,122.861824999016)) ;
#15817 = CARTESIAN_POINT('Ctrl Pts',(-18.2557765411956,13.6716318665394,122.925080803166)) ;
#15818 = CARTESIAN_POINT('Ctrl Pts',(-18.2301875245126,13.6683978244689,122.990838860913)) ;
#15819 = CARTESIAN_POINT('Ctrl Pts',(-18.2102732637651,13.6651413129147,123.058400353306)) ;
#15820 = CARTESIAN_POINT('Ctrl Pts',(-18.189833938375,13.6617989393195,123.127743189796)) ;
#15821 = CARTESIAN_POINT('Ctrl Pts',(-18.1754487613198,13.6585066721384,123.198727822783)) ;
#15822 = CARTESIAN_POINT('Ctrl Pts',(-18.1672792829945,13.6552066817733,123.270557491061)) ;
#15823 = CARTESIAN_POINT('Ctrl Pts',(-18.1590935425314,13.6519001224578,123.342530143251)) ;
#15824 = CARTESIAN_POINT('Ctrl Pts',(-18.1571794535857,13.6485680833321,123.415077287784)) ;
#15825 = CARTESIAN_POINT('Ctrl Pts',(-18.1615584446444,13.645252454877,123.487380860816)) ;
#15826 = CARTESIAN_POINT('Ctrl Pts',(-18.1659434387934,13.6419322810787,123.559783553686)) ;
#15827 = CARTESIAN_POINT('Ctrl Pts',(-18.1766215634281,13.6386285943287,123.631666966055)) ;
#15828 = CARTESIAN_POINT('Ctrl Pts',(-18.1934760829817,13.6352843211117,123.702227373324)) ;
#15829 = CARTESIAN_POINT('Ctrl Pts',(-18.2027050724799,13.6334531053182,123.740863969023)) ;
#15830 = CARTESIAN_POINT('Ctrl Pts',(-18.2137735295612,13.6316221081851,123.779049754104)) ;
#15831 = CARTESIAN_POINT('Ctrl Pts',(-18.2266427469473,13.6298019695379,123.816644567771)) ;
#15832 = CARTESIAN_POINT('Ctrl Pts',(-18.2371665378509,13.6283135528017,123.84738769272)) ;
#15833 = CARTESIAN_POINT('Ctrl Pts',(-18.2488858666179,13.626833215586,123.877709981225)) ;
#15834 = CARTESIAN_POINT('Ctrl Pts',(-18.2617683941932,13.6253549862017,123.907530952147)) ;
#15835 = CARTESIAN_POINT('Ctrl Pts',(-18.2906263032546,13.6220436322074,123.974332351326)) ;
#15836 = CARTESIAN_POINT('Ctrl Pts',(-18.3252565395882,13.6187053027923,124.038474850358)) ;
#15837 = CARTESIAN_POINT('Ctrl Pts',(-18.3652678845994,13.6153568405027,124.099240664017)) ;
#15838 = CARTESIAN_POINT('Ctrl Pts',(-18.4051167833731,13.6120219729847,124.159759768204)) ;
#15839 = CARTESIAN_POINT('Ctrl Pts',(-18.4501528084057,13.6087279356488,124.216699732329)) ;
#15840 = CARTESIAN_POINT('Ctrl Pts',(-18.4998666540437,13.6053999030847,124.269416539875)) ;
#15841 = CARTESIAN_POINT('Ctrl Pts',(-18.5495958694593,13.6020708416096,124.322149645609)) ;
#15842 = CARTESIAN_POINT('Ctrl Pts',(-18.6038175488692,13.5987334322945,124.37045756425)) ;
#15843 = CARTESIAN_POINT('Ctrl Pts',(-18.6619201611746,13.5954399239144,124.413794843619)) ;
#15844 = CARTESIAN_POINT('Ctrl Pts',(-18.7202796504269,13.5921318546333,124.457323721052)) ;
#15845 = CARTESIAN_POINT('Ctrl Pts',(-18.7823273457249,13.5888152394048,124.495668911736)) ;
#15846 = CARTESIAN_POINT('Ctrl Pts',(-18.8473615900167,13.5854360760084,124.52839684272)) ;
#15847 = CARTESIAN_POINT('Ctrl Pts',(-18.8513236554735,13.5852302080581,124.530390718504)) ;
#15848 = CARTESIAN_POINT('Ctrl Pts',(-18.8552987755696,13.5850242107854,124.532364714391)) ;
#15849 = CARTESIAN_POINT('Ctrl Pts',(-18.8592821745989,13.5848183791732,124.534316452303)) ;
#15850 = CARTESIAN_POINT('Ctrl Pts',(-18.9199438203079,13.5816838490294,124.564038715334)) ;
#15851 = CARTESIAN_POINT('Ctrl Pts',(-18.9829124758655,13.5786047482829,124.588793676453)) ;
#15852 = CARTESIAN_POINT('Ctrl Pts',(-19.0475722740586,13.5755435395108,124.608339810356)) ;
#15853 = CARTESIAN_POINT('Ctrl Pts',(-19.117220902973,13.5722461429869,124.629394027427)) ;
#15854 = CARTESIAN_POINT('Ctrl Pts',(-19.1885687370152,13.5688927764746,124.644325376909)) ;
#15855 = CARTESIAN_POINT('Ctrl Pts',(-19.2608096826416,13.5655463761473,124.652966601522)) ;
#15856 = CARTESIAN_POINT('Ctrl Pts',(-19.3328807626323,13.5622078444659,124.661587507365)) ;
#15857 = CARTESIAN_POINT('Ctrl Pts',(-19.4055661388187,13.5589148053625,124.663914556485)) ;
#15858 = CARTESIAN_POINT('Ctrl Pts',(-19.4780414738124,13.5555729255004,124.659921249808)) ;
#15859 = CARTESIAN_POINT('Ctrl Pts',(-19.5499757422459,13.5522559945321,124.655957755269)) ;
#15860 = CARTESIAN_POINT('Ctrl Pts',(-19.6214331874791,13.5489555682235,124.645783470017)) ;
#15861 = CARTESIAN_POINT('Ctrl Pts',(-19.6916265174306,13.5456732478082,124.629507291651)) ;
#15862 = CARTESIAN_POINT('Ctrl Pts',(-19.7330142124773,13.543737911837,124.61991046091)) ;
#15863 = CARTESIAN_POINT('Ctrl Pts',(-19.7738957834929,13.5417967144381,124.608207162694)) ;
#15864 = CARTESIAN_POINT('Ctrl Pts',(-19.8141029976705,13.5398436253417,124.5944436637)) ;
#15865 = CARTESIAN_POINT('Ctrl Pts',(-19.8426986118306,13.5384545765513,124.584654979883)) ;
#15866 = CARTESIAN_POINT('Ctrl Pts',(-19.8709315370337,13.5370615910196,124.573831438472)) ;
#15867 = CARTESIAN_POINT('Ctrl Pts',(-19.8987344214074,13.5356773831792,124.561999903374)) ;
#15868 = CARTESIAN_POINT('Ctrl Pts',(-19.9656917047657,13.5323438155049,124.533506188929)) ;
#15869 = CARTESIAN_POINT('Ctrl Pts',(-20.03002253282,13.529042948606,124.499225290944)) ;
#15870 = CARTESIAN_POINT('Ctrl Pts',(-20.0910055699437,13.5256800175593,124.459545086455)) ;
#15871 = CARTESIAN_POINT('Ctrl Pts',(-20.1514772664395,13.5223452845715,124.420197599088)) ;
#15872 = CARTESIAN_POINT('Ctrl Pts',(-20.2084289118012,13.5190323972408,124.375688905688)) ;
#15873 = CARTESIAN_POINT('Ctrl Pts',(-20.2612248925498,13.5157666958334,124.326514684151)) ;
#15874 = CARTESIAN_POINT('Ctrl Pts',(-20.3144674343984,13.5124733723383,124.276924535225)) ;
#15875 = CARTESIAN_POINT('Ctrl Pts',(-20.3632751289368,13.509143443657,124.222784087567)) ;
#15876 = CARTESIAN_POINT('Ctrl Pts',(-20.4070969254272,13.5057697249261,124.164706051438)) ;
#15877 = CARTESIAN_POINT('Ctrl Pts',(-20.4506651917908,13.5024155247774,124.106964024625)) ;
#15878 = CARTESIAN_POINT('Ctrl Pts',(-20.4891397541629,13.4991114205771,124.045548950693)) ;
#15879 = CARTESIAN_POINT('Ctrl Pts',(-20.5220890806921,13.4958301620486,123.981146141667)) ;
#15880 = CARTESIAN_POINT('Ctrl Pts',(-20.5253722816855,13.495503204493,123.974728791485)) ;
#15881 = CARTESIAN_POINT('Ctrl Pts',(-20.5286020647114,13.4951760805788,123.968278837046)) ;
#15882 = CARTESIAN_POINT('Ctrl Pts',(-20.5317740529339,13.4948489720632,123.961804976439)) ;
#15883 = CARTESIAN_POINT('Ctrl Pts',(-20.5604819830401,13.4918884918396,123.903213605737)) ;
#15884 = CARTESIAN_POINT('Ctrl Pts',(-20.5845560403659,13.4888934110731,123.842469535021)) ;
#15885 = CARTESIAN_POINT('Ctrl Pts',(-20.6037782743388,13.4858731327153,123.780128531831)) ;
#15886 = CARTESIAN_POINT('Ctrl Pts',(-20.6250267095882,13.4825344890795,123.711216210218)) ;
#15887 = CARTESIAN_POINT('Ctrl Pts',(-20.6402710993088,13.4792407703463,123.640598033625)) ;
#15888 = CARTESIAN_POINT('Ctrl Pts',(-20.6493424851837,13.4759642590232,123.569058689353)) ;
#15889 = CARTESIAN_POINT('Ctrl Pts',(-20.6584952131101,13.4726583676079,123.496877860185)) ;
#15890 = CARTESIAN_POINT('Ctrl Pts',(-20.6613281797614,13.4693126707748,123.424038400504)) ;
#15891 = CARTESIAN_POINT('Ctrl Pts',(-20.6578098261807,13.4659667790302,123.351366985605)) ;
#15892 = CARTESIAN_POINT('Ctrl Pts',(-20.6542956434512,13.462624853691,123.278781719428)) ;
#15893 = CARTESIAN_POINT('Ctrl Pts',(-20.6444589385975,13.4593193451983,123.206640390291)) ;
#15894 = CARTESIAN_POINT('Ctrl Pts',(-20.6284074207966,13.4559805354722,123.135753863861)) ;
#15895 = CARTESIAN_POINT('Ctrl Pts',(-20.6185489584221,13.4539299175512,123.092217036856)) ;
#15896 = CARTESIAN_POINT('Ctrl Pts',(-20.6063626760676,13.4518776618907,123.049228894074)) ;
#15897 = CARTESIAN_POINT('Ctrl Pts',(-20.5919016872896,13.4498327922206,123.006984055313)) ;
#15898 = CARTESIAN_POINT('Ctrl Pts',(-20.5919016415084,13.3897528569022,123.006983921601)) ;
#15899 = CARTESIAN_POINT('Ctrl Pts',(-20.6096080658287,13.392266476473,123.058709815247)) ;
#15900 = CARTESIAN_POINT('Ctrl Pts',(-20.6239017189868,13.3947672797745,123.111540715973)) ;
#15901 = CARTESIAN_POINT('Ctrl Pts',(-20.6346907958086,13.3972573925309,123.165137749842)) ;
#15902 = CARTESIAN_POINT('Ctrl Pts',(-20.6490396665439,13.4005691036854,123.236418817118)) ;
#15903 = CARTESIAN_POINT('Ctrl Pts',(-20.6571413877915,13.403889973363,123.30881366061)) ;
#15904 = CARTESIAN_POINT('Ctrl Pts',(-20.6589046230443,13.4072487960544,123.381501049216)) ;
#15905 = CARTESIAN_POINT('Ctrl Pts',(-20.6606582369518,13.4105892908493,123.453791808687)) ;
#15906 = CARTESIAN_POINT('Ctrl Pts',(-20.6561356733065,13.4138934854337,123.526098736805)) ;
#15907 = CARTESIAN_POINT('Ctrl Pts',(-20.6453871553045,13.4171859802309,123.597609700824)) ;
#15908 = CARTESIAN_POINT('Ctrl Pts',(-20.6345984778003,13.4204907767195,123.669387850024)) ;
#15909 = CARTESIAN_POINT('Ctrl Pts',(-20.6175786325927,13.4238226028832,123.740088534419)) ;
#15910 = CARTESIAN_POINT('Ctrl Pts',(-20.5945206605617,13.4271604423045,123.808911548673)) ;
#15911 = CARTESIAN_POINT('Ctrl Pts',(-20.5770011918516,13.4296965358179,123.861203339258)) ;
#15912 = CARTESIAN_POINT('Ctrl Pts',(-20.5560402721388,13.4322145441203,123.912278635198)) ;
#15913 = CARTESIAN_POINT('Ctrl Pts',(-20.5317752294988,13.4347408220453,123.961802575126)) ;
#15914 = CARTESIAN_POINT('Ctrl Pts',(-20.5242004077163,13.4355294505814,123.977262470437)) ;
#15915 = CARTESIAN_POINT('Ctrl Pts',(-20.5163070208699,13.4363184440496,123.992564200258)) ;
#15916 = CARTESIAN_POINT('Ctrl Pts',(-20.5081001234656,13.4371083476146,124.007697974076)) ;
#15917 = CARTESIAN_POINT('Ctrl Pts',(-20.4735348526787,13.4404352115042,124.071437407417)) ;
#15918 = CARTESIAN_POINT('Ctrl Pts',(-20.433488919695,13.4437694104166,124.132048922023)) ;
#15919 = CARTESIAN_POINT('Ctrl Pts',(-20.3884151303904,13.4470728117549,124.188846664702)) ;
#15920 = CARTESIAN_POINT('Ctrl Pts',(-20.3431867001421,13.4503875465335,124.245839271329)) ;
#15921 = CARTESIAN_POINT('Ctrl Pts',(-20.2930704869686,13.4537058462015,124.298772133185)) ;
#15922 = CARTESIAN_POINT('Ctrl Pts',(-20.238635611067,13.4570713797941,124.347045029072)) ;
#15923 = CARTESIAN_POINT('Ctrl Pts',(-20.1847124380153,13.4604052764426,124.394864146422)) ;
#15924 = CARTESIAN_POINT('Ctrl Pts',(-20.1267546075334,13.4636964169222,124.43793023851)) ;
#15925 = CARTESIAN_POINT('Ctrl Pts',(-20.0654077536679,13.4669761165231,124.47576275933)) ;
#15926 = CARTESIAN_POINT('Ctrl Pts',(-20.003741022508,13.4702729172688,124.51379254804)) ;
#15927 = CARTESIAN_POINT('Ctrl Pts',(-19.9388859742016,13.4735980873333,124.54638833385)) ;
#15928 = CARTESIAN_POINT('Ctrl Pts',(-19.8715743626068,13.4769325967039,124.573182845458)) ;
#15929 = CARTESIAN_POINT('Ctrl Pts',(-19.8525933543406,13.4778728854361,124.580738552924)) ;
#15930 = CARTESIAN_POINT('Ctrl Pts',(-19.8334299159491,13.4788116501096,124.587827816366)) ;
#15931 = CARTESIAN_POINT('Ctrl Pts',(-19.814101322745,13.4797497313322,124.594444237049)) ;
#15932 = CARTESIAN_POINT('Ctrl Pts',(-19.7646216857739,13.4821511434707,124.611381739432)) ;
#15933 = CARTESIAN_POINT('Ctrl Pts',(-19.7141274172429,13.4845467399973,124.625197452426)) ;
#15934 = CARTESIAN_POINT('Ctrl Pts',(-19.6629163446019,13.4869312681577,124.635809736745)) ;
#15935 = CARTESIAN_POINT('Ctrl Pts',(-19.5916722453883,13.4902485890432,124.650573392296)) ;
#15936 = CARTESIAN_POINT('Ctrl Pts',(-19.5192774247709,13.4935649815752,124.65908828476)) ;
#15937 = CARTESIAN_POINT('Ctrl Pts',(-19.4465542531183,13.4969299197589,124.661258263373)) ;
#15938 = CARTESIAN_POINT('Ctrl Pts',(-19.3744768420486,13.5002649782716,124.663408973207)) ;
#15939 = CARTESIAN_POINT('Ctrl Pts',(-19.3023484006358,13.5035681505303,124.659318872779)) ;
#15940 = CARTESIAN_POINT('Ctrl Pts',(-19.2309733580835,13.5068398475563,124.649032823518)) ;
#15941 = CARTESIAN_POINT('Ctrl Pts',(-19.1592461784923,13.5101276858784,124.638696026841)) ;
#15942 = CARTESIAN_POINT('Ctrl Pts',(-19.0885571371086,13.5134426445569,124.622142011887)) ;
#15943 = CARTESIAN_POINT('Ctrl Pts',(-19.0197012273749,13.5167985406652,124.599557785553)) ;
#15944 = CARTESIAN_POINT('Ctrl Pts',(-18.9647857648684,13.5194750079085,124.581545922239)) ;
#15945 = CARTESIAN_POINT('Ctrl Pts',(-18.911185101128,13.5221350524653,124.559747117296)) ;
#15946 = CARTESIAN_POINT('Ctrl Pts',(-18.8592840273916,13.5247629594564,124.53431736011)) ;
#15947 = CARTESIAN_POINT('Ctrl Pts',(-18.8462460429093,13.5254231117058,124.527929192087)) ;
#15948 = CARTESIAN_POINT('Ctrl Pts',(-18.8333202942993,13.5260815641942,124.521314326895)) ;
#15949 = CARTESIAN_POINT('Ctrl Pts',(-18.8205126727063,13.5267392402366,124.514475772782)) ;
#15950 = CARTESIAN_POINT('Ctrl Pts',(-18.7563299793194,13.5300350449625,124.480205801679)) ;
#15951 = CARTESIAN_POINT('Ctrl Pts',(-18.6952661557814,13.5333610765098,124.440400107414)) ;
#15952 = CARTESIAN_POINT('Ctrl Pts',(-18.6380110606181,13.5367375625947,124.395509542671)) ;
#15953 = CARTESIAN_POINT('Ctrl Pts',(-18.5812356069805,13.5400857629362,124.350995038416)) ;
#15954 = CARTESIAN_POINT('Ctrl Pts',(-18.5284206806311,13.5433742750728,124.301649181655)) ;
#15955 = CARTESIAN_POINT('Ctrl Pts',(-18.4801555612243,13.5466520760842,124.248021401225)) ;
#15956 = CARTESIAN_POINT('Ctrl Pts',(-18.4314837544484,13.5499574962186,124.193941747036)) ;
#15957 = CARTESIAN_POINT('Ctrl Pts',(-18.3876273377621,13.5533138836049,124.135717018223)) ;
#15958 = CARTESIAN_POINT('Ctrl Pts',(-18.3490847229093,13.5566501206704,124.074009532102)) ;
#15959 = CARTESIAN_POINT('Ctrl Pts',(-18.3105665437652,13.5599842425884,124.012341168032)) ;
#15960 = CARTESIAN_POINT('Ctrl Pts',(-18.2775029179448,13.563284743103,123.947430551321)) ;
#15961 = CARTESIAN_POINT('Ctrl Pts',(-18.2502692690622,13.5666414760701,123.880015309337)) ;
#15962 = CARTESIAN_POINT('Ctrl Pts',(-18.2418235197772,13.5676824722722,123.85910837049)) ;
#15963 = CARTESIAN_POINT('Ctrl Pts',(-18.2339450036271,13.5687245182647,123.837976698179)) ;
#15964 = CARTESIAN_POINT('Ctrl Pts',(-18.2266423654683,13.56976307206,123.816643453356)) ;
#15965 = CARTESIAN_POINT('Ctrl Pts',(-18.2106069186927,13.5720435731261,123.769798997357)) ;
#15966 = CARTESIAN_POINT('Ctrl Pts',(-18.1973688323647,13.5742977726772,123.722043018589)) ;
#15967 = CARTESIAN_POINT('Ctrl Pts',(-18.1869980402704,13.5765479499922,123.673626877044)) ;
#15968 = CARTESIAN_POINT('Ctrl Pts',(-18.1717848592061,13.5798487928408,123.602603996529)) ;
#15969 = CARTESIAN_POINT('Ctrl Pts',(-18.1627913440007,13.5831792810849,123.530392408845)) ;
#15970 = CARTESIAN_POINT('Ctrl Pts',(-18.160118757509,13.5865286217716,123.457809881199)) ;
#15971 = CARTESIAN_POINT('Ctrl Pts',(-18.1574433894047,13.5898814484327,123.385151810077)) ;
#15972 = CARTESIAN_POINT('Ctrl Pts',(-18.1611123933561,13.5932104436744,123.312397800328)) ;
#15973 = CARTESIAN_POINT('Ctrl Pts',(-18.1710845532211,13.596519480288,123.240375565803)) ;
#15974 = CARTESIAN_POINT('Ctrl Pts',(-18.1810633531557,13.5998307202592,123.168305374501)) ;
#15975 = CARTESIAN_POINT('Ctrl Pts',(-18.1973148957516,13.6031493528183,123.097246856212)) ;
#15976 = CARTESIAN_POINT('Ctrl Pts',(-18.2196541162406,13.6065167629075,123.028006173156)) ;
#15977 = CARTESIAN_POINT('Ctrl Pts',(-18.2380205748496,13.6092853195836,122.971079113412)) ;
#15978 = CARTESIAN_POINT('Ctrl Pts',(-18.2604495238595,13.6120345366518,122.915543605758)) ;
#15979 = CARTESIAN_POINT('Ctrl Pts',(-18.2867692424076,13.6147532278699,122.861826158003)) ;
#15980 = CARTESIAN_POINT('Ctrl Pts',(-18.292140428932,13.6153080437433,122.85086379034)) ;
#15981 = CARTESIAN_POINT('Ctrl Pts',(-18.297671923081,13.6158620502894,122.839980677052)) ;
#15982 = CARTESIAN_POINT('Ctrl Pts',(-18.30336194444,13.6164161328298,122.829180324304)) ;
#15983 = CARTESIAN_POINT('Ctrl Pts',(-18.3371257771952,13.6197039852025,122.765092462256)) ;
#15984 = CARTESIAN_POINT('Ctrl Pts',(-18.3763951344284,13.6230215899451,122.704063178082)) ;
#15985 = CARTESIAN_POINT('Ctrl Pts',(-18.4207275060417,13.6263692488929,122.646778866055)) ;
#15986 = CARTESIAN_POINT('Ctrl Pts',(-18.4651039227243,13.6297202338046,122.589437640955)) ;
#15987 = CARTESIAN_POINT('Ctrl Pts',(-18.5143858945347,13.6330437932077,122.536065466233)) ;
#15988 = CARTESIAN_POINT('Ctrl Pts',(-18.5680171014335,13.6363321986858,122.48726593694)) ;
#15989 = CARTESIAN_POINT('Ctrl Pts',(-18.6218324962497,13.6396318976735,122.438298813364)) ;
#15990 = CARTESIAN_POINT('Ctrl Pts',(-18.6798167018632,13.6429488094819,122.394126811195)) ;
#15991 = CARTESIAN_POINT('Ctrl Pts',(-18.7413133163744,13.6463290970248,122.355248759595)) ;
#15992 = CARTESIAN_POINT('Ctrl Pts',(-18.8022079204943,13.6496762938318,122.316751297906)) ;
#15993 = CARTESIAN_POINT('Ctrl Pts',(-18.8663156296209,13.6529695807162,122.283590577323)) ;
#15994 = CARTESIAN_POINT('Ctrl Pts',(-18.9329263684835,13.6562281778483,122.256135079469)) ;
#15995 = CARTESIAN_POINT('Ctrl Pts',(-18.9564852890182,13.6573806801655,122.246424604804)) ;
#15996 = CARTESIAN_POINT('Ctrl Pts',(-18.9803352804135,13.6585348629319,122.237436922923)) ;
#15997 = CARTESIAN_POINT('Ctrl Pts',(-19.0044431491614,13.6596978079258,122.229184496079)) ;
#15998 = CARTESIAN_POINT('Ctrl Pts',(-19.0491410660855,13.6618540009626,122.213883836641)) ;
#15999 = CARTESIAN_POINT('Ctrl Pts',(-19.0946693789181,13.6640443093058,122.201129870366)) ;
#16000 = CARTESIAN_POINT('Ctrl Pts',(-19.1408100100882,13.666225029951,122.190983488285)) ;
#16001 = CARTESIAN_POINT('Ctrl Pts',(-19.2115557014482,13.6695686467546,122.17542642292)) ;
#16002 = CARTESIAN_POINT('Ctrl Pts',(-19.2835202288677,13.67285510112,122.166048117887)) ;
#16003 = CARTESIAN_POINT('Ctrl Pts',(-19.3558911093926,13.6761779698804,122.162954704551)) ;
#16004 = CARTESIAN_POINT('Ctrl Pts',(-19.4281174154066,13.6794942005824,122.159867470894)) ;
#16005 = CARTESIAN_POINT('Ctrl Pts',(-19.5004757896116,13.6828224045214,122.163051673021)) ;
#16006 = CARTESIAN_POINT('Ctrl Pts',(-19.572152935276,13.6861112181146,122.172471848184)) ;
#16007 = CARTESIAN_POINT('Ctrl Pts',(-19.6442912188223,13.6894211904262,122.181952628435)) ;
#16008 = CARTESIAN_POINT('Ctrl Pts',(-19.7154607876134,13.6927382445772,122.197713058344)) ;
#16009 = CARTESIAN_POINT('Ctrl Pts',(-19.7848547858062,13.6961082030634,122.219573724612)) ;
#16010 = CARTESIAN_POINT('Ctrl Pts',(-19.8446557588647,13.6990122985457,122.238412372747)) ;
#16011 = CARTESIAN_POINT('Ctrl Pts',(-19.9029549380021,13.7018952591033,122.261723593888)) ;
#16012 = CARTESIAN_POINT('Ctrl Pts',(-19.9592604445148,13.7047397236552,122.289311373019)) ;
#16013 = CARTESIAN_POINT('Ctrl Pts',(-19.9679555433876,13.7051789862079,122.293571675111)) ;
#16014 = CARTESIAN_POINT('Ctrl Pts',(-19.9766008662182,13.7056176176954,122.297932873291)) ;
#16015 = CARTESIAN_POINT('Ctrl Pts',(-19.9851946599321,13.7060559914406,122.30239408478)) ;
#16016 = CARTESIAN_POINT('Ctrl Pts',(-20.0497714252281,13.709350084759,122.335917184919)) ;
#16017 = CARTESIAN_POINT('Ctrl Pts',(-20.111293772392,13.712680504547,122.375011977987)) ;
#16018 = CARTESIAN_POINT('Ctrl Pts',(-20.16906659148,13.7160531847087,122.419235635488)) ;
#16019 = CARTESIAN_POINT('Ctrl Pts',(-20.2262590038304,13.7193919816997,122.463015006053)) ;
#16020 = CARTESIAN_POINT('Ctrl Pts',(-20.2795606967903,13.7226699814663,122.511655498151)) ;
#16021 = CARTESIAN_POINT('Ctrl Pts',(-20.3283780924974,13.7259502118371,122.5646163823)) ;
#16022 = CARTESIAN_POINT('Ctrl Pts',(-20.3775137405789,13.7292518268207,122.617922531223)) ;
#16023 = CARTESIAN_POINT('Ctrl Pts',(-20.4219183778006,13.7325911038699,122.675401764479)) ;
#16024 = CARTESIAN_POINT('Ctrl Pts',(-20.4610902269716,13.7359119352449,122.736404184641)) ;
#16025 = CARTESIAN_POINT('Ctrl Pts',(-20.5004286853823,13.7392468910794,122.797666065795)) ;
#16026 = CARTESIAN_POINT('Ctrl Pts',(-20.5343394352926,13.7425656777551,122.862247058436)) ;
#16027 = CARTESIAN_POINT('Ctrl Pts',(-20.5624361654185,13.7459160952872,122.929411058267)) ;
#16028 = CARTESIAN_POINT('Ctrl Pts',(-20.5731138668484,13.7471893665154,122.954935634751)) ;
#16029 = CARTESIAN_POINT('Ctrl Pts',(-20.5829411995565,13.748461219154,122.980807763874)) ;
#16030 = CARTESIAN_POINT('Ctrl Pts',(-20.591901915765,13.7497304410597,123.00698472277)) ;
#16031 = CARTESIAN_POINT('Origin',(-19.4092722359532,16.5113612779716,123.411814366564)) ;
#16032 = CARTESIAN_POINT('',(-20.5919013672866,13.0298207905601,123.006983120533)) ;
#16033 = CARTESIAN_POINT('',(-20.5919014130239,13.0898536069789,123.006983254143)) ;
#16034 = CARTESIAN_POINT('',(-20.5919021064381,16.5113612779716,123.006985279772)) ;
#16035 = CARTESIAN_POINT('Ctrl Pts',(-20.5919016872895,13.4498327922206,123.006984055313)) ;
#16036 = CARTESIAN_POINT('Ctrl Pts',(-20.5829410927979,13.44856571106,122.980807500216)) ;
#16037 = CARTESIAN_POINT('Ctrl Pts',(-20.5731135903211,13.4473019494881,122.954935597809)) ;
#16038 = CARTESIAN_POINT('Ctrl Pts',(-20.5624403655201,13.4460395001892,122.929421098548)) ;
#16039 = CARTESIAN_POINT('Ctrl Pts',(-20.5343398276492,13.4427157152044,122.862246353698)) ;
#16040 = CARTESIAN_POINT('Ctrl Pts',(-20.5004283260913,13.4393740656987,122.797665446055)) ;
#16041 = CARTESIAN_POINT('Ctrl Pts',(-20.4610899251354,13.4360345919639,122.736403714591)) ;
#16042 = CARTESIAN_POINT('Ctrl Pts',(-20.4219178868664,13.4327092409135,122.675401059906)) ;
#16043 = CARTESIAN_POINT('Ctrl Pts',(-20.3775131542739,13.4294154523931,122.617921893582)) ;
#16044 = CARTESIAN_POINT('Ctrl Pts',(-20.3283780800447,13.4260721821416,122.56461636879)) ;
#16045 = CARTESIAN_POINT('Ctrl Pts',(-20.2795625165461,13.4227506521792,122.511657473925)) ;
#16046 = CARTESIAN_POINT('Ctrl Pts',(-20.2262611118225,13.4194383028478,122.463016614552)) ;
#16047 = CARTESIAN_POINT('Ctrl Pts',(-20.1690665354927,13.4161742615484,122.419235592631)) ;
#16048 = CARTESIAN_POINT('Ctrl Pts',(-20.1112909038241,13.4128770599609,122.375009787338)) ;
#16049 = CARTESIAN_POINT('Ctrl Pts',(-20.0497683592175,13.4095514359962,122.335915254354)) ;
#16050 = CARTESIAN_POINT('Ctrl Pts',(-19.9851900730519,13.4061756943286,122.30239170365)) ;
#16051 = CARTESIAN_POINT('Ctrl Pts',(-19.976600882643,13.4057267061365,122.297932926911)) ;
#16052 = CARTESIAN_POINT('Ctrl Pts',(-19.9679555666344,13.4052777640964,122.293571718947)) ;
#16053 = CARTESIAN_POINT('Ctrl Pts',(-19.9592638229184,13.4048295958068,122.289313028327)) ;
#16054 = CARTESIAN_POINT('Ctrl Pts',(-19.9029574856406,13.4019262986443,122.261724632002)) ;
#16055 = CARTESIAN_POINT('Ctrl Pts',(-19.8446583224451,13.3990699102258,122.238413473407)) ;
#16056 = CARTESIAN_POINT('Ctrl Pts',(-19.7848601012782,13.3962269818687,122.219575399118)) ;
#16057 = CARTESIAN_POINT('Ctrl Pts',(-19.7154581960279,13.3929274749498,122.197711901821)) ;
#16058 = CARTESIAN_POINT('Ctrl Pts',(-19.6442884736089,13.3895883209325,122.181952245224)) ;
#16059 = CARTESIAN_POINT('Ctrl Pts',(-19.5721525566041,13.3862281725593,122.172471798418)) ;
#16060 = CARTESIAN_POINT('Ctrl Pts',(-19.5004770657968,13.3828894712046,122.163051863021)) ;
#16061 = CARTESIAN_POINT('Ctrl Pts',(-19.4281187326612,13.3796030075022,122.159867454332)) ;
#16062 = CARTESIAN_POINT('Ctrl Pts',(-19.3558917953174,13.3762932146361,122.162954675232)) ;
#16063 = CARTESIAN_POINT('Ctrl Pts',(-19.2835211381005,13.3729768358199,122.166048039201)) ;
#16064 = CARTESIAN_POINT('Ctrl Pts',(-19.211556242851,13.3696357695286,122.175425660969)) ;
#16065 = CARTESIAN_POINT('Ctrl Pts',(-19.1407994285092,13.3663379214254,122.190985815236)) ;
#16066 = CARTESIAN_POINT('Ctrl Pts',(-19.0946685383492,13.3641878434431,122.201130474433)) ;
#16067 = CARTESIAN_POINT('Ctrl Pts',(-19.0491400157151,13.3620507828497,122.213884078904)) ;
#16068 = CARTESIAN_POINT('Ctrl Pts',(-19.00444037134,13.3598763993695,122.229185446966)) ;
#16069 = CARTESIAN_POINT('Ctrl Pts',(-18.9803348232941,13.3587038015516,122.23743714266)) ;
#16070 = CARTESIAN_POINT('Ctrl Pts',(-18.9564848539747,13.3575229288198,122.246425003157)) ;
#16071 = CARTESIAN_POINT('Ctrl Pts',(-18.9329355549791,13.3563402041787,122.256131293038)) ;
#16072 = CARTESIAN_POINT('Ctrl Pts',(-18.8663193831009,13.352994516989,122.283588410771)) ;
#16073 = CARTESIAN_POINT('Ctrl Pts',(-18.8022113698638,13.3496957028308,122.316749155544)) ;
#16074 = CARTESIAN_POINT('Ctrl Pts',(-18.7413137914152,13.3464387851846,122.355248459275)) ;
#16075 = CARTESIAN_POINT('Ctrl Pts',(-18.6798135387548,13.3431496353819,122.394128772204)) ;
#16076 = CARTESIAN_POINT('Ctrl Pts',(-18.6218297616564,13.3398102854306,122.438301305722)) ;
#16077 = CARTESIAN_POINT('Ctrl Pts',(-18.5680171402105,13.3364401366298,122.487265901657)) ;
#16078 = CARTESIAN_POINT('Ctrl Pts',(-18.5143880295376,13.333081480646,122.536063519463)) ;
#16079 = CARTESIAN_POINT('Ctrl Pts',(-18.4651056924899,13.3297712570681,122.589435340438)) ;
#16080 = CARTESIAN_POINT('Ctrl Pts',(-18.4207274175418,13.3264755396218,122.64677898041)) ;
#16081 = CARTESIAN_POINT('Ctrl Pts',(-18.3763934622691,13.3231831135411,122.704065352463)) ;
#16082 = CARTESIAN_POINT('Ctrl Pts',(-18.3371241763958,13.3198731611861,122.765094722657)) ;
#16083 = CARTESIAN_POINT('Ctrl Pts',(-18.3033590273297,13.3165206640947,122.829185861367)) ;
#16084 = CARTESIAN_POINT('Ctrl Pts',(-18.2976719942798,13.3159560060883,122.839980673004)) ;
#16085 = CARTESIAN_POINT('Ctrl Pts',(-18.2921404801968,13.3153910434634,122.8508637759)) ;
#16086 = CARTESIAN_POINT('Ctrl Pts',(-18.2867710305383,13.3148270119737,122.861822508517)) ;
#16087 = CARTESIAN_POINT('Ctrl Pts',(-18.2604503598235,13.3120621686366,122.915541457575)) ;
#16088 = CARTESIAN_POINT('Ctrl Pts',(-18.2380215987695,13.3093349778737,122.971077001873)) ;
#16089 = CARTESIAN_POINT('Ctrl Pts',(-18.219656208807,13.3066205690874,123.027999687282)) ;
#16090 = CARTESIAN_POINT('Ctrl Pts',(-18.1973137117869,13.3033183429792,123.097249233941)) ;
#16091 = CARTESIAN_POINT('Ctrl Pts',(-18.1810630063032,13.2999805325553,123.168307925099)) ;
#16092 = CARTESIAN_POINT('Ctrl Pts',(-18.1710845679303,13.2966220234551,123.240375459568)) ;
#16093 = CARTESIAN_POINT('Ctrl Pts',(-18.1611126652386,13.2932657141124,123.312395791219)) ;
#16094 = CARTESIAN_POINT('Ctrl Pts',(-18.1574432993759,13.2899427231762,123.385149783515)) ;
#16095 = CARTESIAN_POINT('Ctrl Pts',(-18.1601187672495,13.28663039293,123.457810145731)) ;
#16096 = CARTESIAN_POINT('Ctrl Pts',(-18.1627914406836,13.2833215223053,123.530394616556)) ;
#16097 = CARTESIAN_POINT('Ctrl Pts',(-18.1717848155254,13.2800066790244,123.602606484272)) ;
#16098 = CARTESIAN_POINT('Ctrl Pts',(-18.1870000723738,13.2766489629358,123.673636363758)) ;
#16099 = CARTESIAN_POINT('Ctrl Pts',(-18.1973688869123,13.274360763943,123.72204143864)) ;
#16100 = CARTESIAN_POINT('Ctrl Pts',(-18.2106063125809,13.2720799068548,123.769797668518)) ;
#16101 = CARTESIAN_POINT('Ctrl Pts',(-18.2266435352718,13.2698214087154,123.816646870694)) ;
#16102 = CARTESIAN_POINT('Ctrl Pts',(-18.2339450354743,13.2687931493378,123.837976590046)) ;
#16103 = CARTESIAN_POINT('Ctrl Pts',(-18.24182366522,13.2677686676792,123.859108252036)) ;
#16104 = CARTESIAN_POINT('Ctrl Pts',(-18.2502655468571,13.2667432995336,123.88000609514)) ;
#16105 = CARTESIAN_POINT('Ctrl Pts',(-18.2775027042839,13.2634350188916,123.947431565781)) ;
#16106 = CARTESIAN_POINT('Ctrl Pts',(-18.3105670637979,13.2600836373738,124.01234206466)) ;
#16107 = CARTESIAN_POINT('Ctrl Pts',(-18.3490850319139,13.2567516262153,124.074010026824)) ;
#16108 = CARTESIAN_POINT('Ctrl Pts',(-18.387628084856,13.2534174450847,124.135718150248)) ;
#16109 = CARTESIAN_POINT('Ctrl Pts',(-18.4314846764746,13.2501174792409,124.193942781695)) ;
#16110 = CARTESIAN_POINT('Ctrl Pts',(-18.4801556395518,13.2467541682034,124.248021488256)) ;
#16111 = CARTESIAN_POINT('Ctrl Pts',(-18.5284185147809,13.2434190572728,124.301646765059)) ;
#16112 = CARTESIAN_POINT('Ctrl Pts',(-18.5812330789978,13.2401060534054,124.350993050291)) ;
#16113 = CARTESIAN_POINT('Ctrl Pts',(-18.6380109954579,13.2368404025748,124.395509491583)) ;
#16114 = CARTESIAN_POINT('Ctrl Pts',(-18.6952690635548,13.2335471352395,124.440402393363)) ;
#16115 = CARTESIAN_POINT('Ctrl Pts',(-18.7563330368345,13.2302170351911,124.480207906015)) ;
#16116 = CARTESIAN_POINT('Ctrl Pts',(-18.8205189799835,13.226842865693,124.514479140492)) ;
#16117 = CARTESIAN_POINT('Ctrl Pts',(-18.833320226369,13.2261699212292,124.521314196502)) ;
#16118 = CARTESIAN_POINT('Ctrl Pts',(-18.8462459585297,13.2254975236865,124.527929095792)) ;
#16119 = CARTESIAN_POINT('Ctrl Pts',(-18.8592802116798,13.2248269260802,124.534315490533)) ;
#16120 = CARTESIAN_POINT('Ctrl Pts',(-18.9111830063035,13.2221565859056,124.559746309684)) ;
#16121 = CARTESIAN_POINT('Ctrl Pts',(-18.9647837095672,13.2195252081346,124.5815448943)) ;
#16122 = CARTESIAN_POINT('Ctrl Pts',(-19.019694317989,13.2169040953244,124.599555519304)) ;
#16123 = CARTESIAN_POINT('Ctrl Pts',(-19.0885599989045,13.213616848586,124.622143394219)) ;
#16124 = CARTESIAN_POINT('Ctrl Pts',(-19.1592492674356,13.2103016820336,124.638696482181)) ;
#16125 = CARTESIAN_POINT('Ctrl Pts',(-19.2309735301825,13.2069465475215,124.649032848319)) ;
#16126 = CARTESIAN_POINT('Ctrl Pts',(-19.3023454913827,13.2036078930544,124.659318443384)) ;
#16127 = CARTESIAN_POINT('Ctrl Pts',(-19.3744738881038,13.200313127969,124.663409024748)) ;
#16128 = CARTESIAN_POINT('Ctrl Pts',(-19.4465536192155,13.1970382089384,124.661258282287)) ;
#16129 = CARTESIAN_POINT('Ctrl Pts',(-19.5192796330319,13.1937339262643,124.659088255798)) ;
#16130 = CARTESIAN_POINT('Ctrl Pts',(-19.5916746647344,13.1903937844111,124.6505734399)) ;
#16131 = CARTESIAN_POINT('Ctrl Pts',(-19.6629253872211,13.18704088229,124.635807862841)) ;
#16132 = CARTESIAN_POINT('Ctrl Pts',(-19.7141264295642,13.1846314739713,124.625197262557)) ;
#16133 = CARTESIAN_POINT('Ctrl Pts',(-19.7646209257032,13.1822377967368,124.611382178439)) ;
#16134 = CARTESIAN_POINT('Ctrl Pts',(-19.8141051483714,13.1798450308754,124.594442927482)) ;
#16135 = CARTESIAN_POINT('Ctrl Pts',(-19.8334298206514,13.1789106034232,124.587827779143)) ;
#16136 = CARTESIAN_POINT('Ctrl Pts',(-19.8525932488088,13.1779769401818,124.580738434888)) ;
#16137 = CARTESIAN_POINT('Ctrl Pts',(-19.8715659077101,13.1770448707288,124.573186211035)) ;
#16138 = CARTESIAN_POINT('Ctrl Pts',(-19.9388875606489,13.1737375611655,124.546388270071)) ;
#16139 = CARTESIAN_POINT('Ctrl Pts',(-20.0037424838628,13.1704339176419,124.513791655081)) ;
#16140 = CARTESIAN_POINT('Ctrl Pts',(-20.0654078568684,13.1670897087974,124.475762695686)) ;
#16141 = CARTESIAN_POINT('Ctrl Pts',(-20.1267524640324,13.1637628955821,124.437931552191)) ;
#16142 = CARTESIAN_POINT('Ctrl Pts',(-20.1847105512711,13.160459384278,124.394865788352)) ;
#16143 = CARTESIAN_POINT('Ctrl Pts',(-20.2386353078162,13.1571865872795,124.347045297996)) ;
#16144 = CARTESIAN_POINT('Ctrl Pts',(-20.2930722512412,13.1538827046759,124.298770600159)) ;
#16145 = CARTESIAN_POINT('Ctrl Pts',(-20.3431881478507,13.150544876991,124.24583746345)) ;
#16146 = CARTESIAN_POINT('Ctrl Pts',(-20.3884152391871,13.1471896049157,124.188846527606)) ;
#16147 = CARTESIAN_POINT('Ctrl Pts',(-20.4334882142278,13.1438457662996,124.132049794654)) ;
#16148 = CARTESIAN_POINT('Ctrl Pts',(-20.4735347227404,13.1405458478673,124.071438635973)) ;
#16149 = CARTESIAN_POINT('Ctrl Pts',(-20.5081039974958,13.1372261673073,124.007690830188)) ;
#16150 = CARTESIAN_POINT('Ctrl Pts',(-20.5163069447483,13.1364384399187,123.992564105893)) ;
#16151 = CARTESIAN_POINT('Ctrl Pts',(-20.5242003769134,13.1356495875477,123.977262397619)) ;
#16152 = CARTESIAN_POINT('Ctrl Pts',(-20.5317733220291,13.1348603689426,123.961806468175)) ;
#16153 = CARTESIAN_POINT('Ctrl Pts',(-20.5560402481142,13.1323313780068,123.912279118952)) ;
#16154 = CARTESIAN_POINT('Ctrl Pts',(-20.5770007045201,13.1297993711523,123.861203677247)) ;
#16155 = CARTESIAN_POINT('Ctrl Pts',(-20.5945181062435,13.127280121411,123.808919172674)) ;
#16156 = CARTESIAN_POINT('Ctrl Pts',(-20.6175795522041,13.1239635598178,123.740087259368)) ;
#16157 = CARTESIAN_POINT('Ctrl Pts',(-20.6345986982784,13.120654726801,123.669386379736)) ;
#16158 = CARTESIAN_POINT('Ctrl Pts',(-20.6453871540013,13.117306267284,123.597609709495)) ;
#16159 = CARTESIAN_POINT('Ctrl Pts',(-20.6561353420231,13.113970305827,123.52610094428)) ;
#16160 = CARTESIAN_POINT('Ctrl Pts',(-20.660658278922,13.1106580562661,123.453794034973)) ;
#16161 = CARTESIAN_POINT('Ctrl Pts',(-20.6589046280877,13.1073697954084,123.38150125712)) ;
#16162 = CARTESIAN_POINT('Ctrl Pts',(-20.6571413476508,13.104063478137,123.308811507018)) ;
#16163 = CARTESIAN_POINT('Ctrl Pts',(-20.6490396908371,13.1007322821932,123.23641645862)) ;
#16164 = CARTESIAN_POINT('Ctrl Pts',(-20.6346891360308,13.0973782862631,123.165129504685)) ;
#16165 = CARTESIAN_POINT('Ctrl Pts',(-20.6239016001173,13.0948570352009,123.111541989351)) ;
#16166 = CARTESIAN_POINT('Ctrl Pts',(-20.6096085084526,13.0923516502569,123.058710819136)) ;
#16167 = CARTESIAN_POINT('Ctrl Pts',(-20.5919014130363,13.0898536069789,123.006983254139)) ;
#16168 = CARTESIAN_POINT('Ctrl Pts',(-20.5919013672997,13.0298207905601,123.006983120529)) ;
#16169 = CARTESIAN_POINT('Ctrl Pts',(-20.6128415365065,13.0327758983278,123.068155409876)) ;
#16170 = CARTESIAN_POINT('Ctrl Pts',(-20.6289991091982,13.0357170266271,123.130860810711)) ;
#16171 = CARTESIAN_POINT('Ctrl Pts',(-20.6402267339071,13.0386471338238,123.194441359862)) ;
#16172 = CARTESIAN_POINT('Ctrl Pts',(-20.6564173041211,13.0428724359275,123.286126410971)) ;
#16173 = CARTESIAN_POINT('Ctrl Pts',(-20.6622820922898,13.04712862656,123.379134979086)) ;
#16174 = CARTESIAN_POINT('Ctrl Pts',(-20.657833380239,13.0513934496921,123.47177326128)) ;
#16175 = CARTESIAN_POINT('Ctrl Pts',(-20.6553317958422,13.0537916303073,123.523865300199)) ;
#16176 = CARTESIAN_POINT('Ctrl Pts',(-20.6495684445029,13.056192540518,123.575841899756)) ;
#16177 = CARTESIAN_POINT('Ctrl Pts',(-20.6405410520404,13.0585922231034,123.627399854497)) ;
#16178 = CARTESIAN_POINT('Ctrl Pts',(-20.6202302906749,13.0639912772098,123.743400274284)) ;
#16179 = CARTESIAN_POINT('Ctrl Pts',(-20.5836175232734,13.069281839856,123.856001963048)) ;
#16180 = CARTESIAN_POINT('Ctrl Pts',(-20.5317601409036,13.0747309735579,123.96183336925)) ;
#16181 = CARTESIAN_POINT('Ctrl Pts',(-20.5197068854819,13.0759975203316,123.986431852867)) ;
#16182 = CARTESIAN_POINT('Ctrl Pts',(-20.5068314945853,13.077267794894,124.010657329884)) ;
#16183 = CARTESIAN_POINT('Ctrl Pts',(-20.4931985752011,13.0785324723927,124.034392627637)) ;
#16184 = CARTESIAN_POINT('Ctrl Pts',(-20.4451665262531,13.0829882349343,124.118017781675)) ;
#16185 = CARTESIAN_POINT('Ctrl Pts',(-20.3877135875372,13.0874031785866,124.195641337355)) ;
#16186 = CARTESIAN_POINT('Ctrl Pts',(-20.3220694358251,13.0917957573214,124.265805743559)) ;
#16187 = CARTESIAN_POINT('Ctrl Pts',(-20.2890474332361,13.0940054247871,124.301101640344)) ;
#16188 = CARTESIAN_POINT('Ctrl Pts',(-20.2539515931778,13.0962094327011,124.334510747036)) ;
#16189 = CARTESIAN_POINT('Ctrl Pts',(-20.216938518417,13.0984101302198,124.365845380865)) ;
#16190 = CARTESIAN_POINT('Ctrl Pts',(-20.105950262194,13.1050091923529,124.459806133667)) ;
#16191 = CARTESIAN_POINT('Ctrl Pts',(-19.9794225674485,13.1116356102903,124.533679037231)) ;
#16192 = CARTESIAN_POINT('Ctrl Pts',(-19.8430228892276,13.1183574025859,124.584145536012)) ;
#16193 = CARTESIAN_POINT('Ctrl Pts',(-19.833439869117,13.1188296549518,124.587691156347)) ;
#16194 = CARTESIAN_POINT('Ctrl Pts',(-19.8237911871676,13.1193020977122,124.591127097987)) ;
#16195 = CARTESIAN_POINT('Ctrl Pts',(-19.8141206275482,13.1197729541245,124.594437628596)) ;
#16196 = CARTESIAN_POINT('Ctrl Pts',(-19.6865529013262,13.1259841853512,124.638107992979)) ;
#16197 = CARTESIAN_POINT('Ctrl Pts',(-19.5527786571738,13.1321239816196,124.66084402754)) ;
#16198 = CARTESIAN_POINT('Ctrl Pts',(-19.4179888083276,13.1382623043066,124.661783974771)) ;
#16199 = CARTESIAN_POINT('Ctrl Pts',(-19.3220565319828,13.1426310551683,124.66245295154)) ;
#16200 = CARTESIAN_POINT('Ctrl Pts',(-19.2265435863915,13.1469968366946,124.652077540438)) ;
#16201 = CARTESIAN_POINT('Ctrl Pts',(-19.1332868126833,13.1513888479219,124.630966549935)) ;
#16202 = CARTESIAN_POINT('Ctrl Pts',(-19.0852591382136,13.1536507542383,124.620094291125)) ;
#16203 = CARTESIAN_POINT('Ctrl Pts',(-19.0378287111207,13.1559196174534,124.606373923211)) ;
#16204 = CARTESIAN_POINT('Ctrl Pts',(-18.9912494073237,13.1581994259979,124.589845314723)) ;
#16205 = CARTESIAN_POINT('Ctrl Pts',(-18.94628666701,13.16040011238,124.573890341793)) ;
#16206 = CARTESIAN_POINT('Ctrl Pts',(-18.9022002374828,13.1625869461434,124.555343671711)) ;
#16207 = CARTESIAN_POINT('Ctrl Pts',(-18.8593086838134,13.1647748278629,124.53432944058)) ;
#16208 = CARTESIAN_POINT('Ctrl Pts',(-18.772080200369,13.1692243193834,124.49159283266)) ;
#16209 = CARTESIAN_POINT('Ctrl Pts',(-18.690158054208,13.1736772079637,124.438843783208)) ;
#16210 = CARTESIAN_POINT('Ctrl Pts',(-18.6152211808927,13.1781001339968,124.377206992408)) ;
#16211 = CARTESIAN_POINT('Ctrl Pts',(-18.5450664514027,13.1822408082161,124.31950359228)) ;
#16212 = CARTESIAN_POINT('Ctrl Pts',(-18.4815599704335,13.1863804049238,124.254452152417)) ;
#16213 = CARTESIAN_POINT('Ctrl Pts',(-18.4257140315598,13.1905344974001,124.183250208774)) ;
#16214 = CARTESIAN_POINT('Ctrl Pts',(-18.3920578426148,13.1930380083822,124.140339549256)) ;
#16215 = CARTESIAN_POINT('Ctrl Pts',(-18.3611833015205,13.1955467842376,124.095193139965)) ;
#16216 = CARTESIAN_POINT('Ctrl Pts',(-18.3333180481067,13.1980642337553,124.04807106455)) ;
#16217 = CARTESIAN_POINT('Ctrl Pts',(-18.2923218608707,13.201767980147,123.978743669676)) ;
#16218 = CARTESIAN_POINT('Ctrl Pts',(-18.2580892369449,13.2054233460874,123.905552327292)) ;
#16219 = CARTESIAN_POINT('Ctrl Pts',(-18.2311459975247,13.2091185082985,123.829568560322)) ;
#16220 = CARTESIAN_POINT('Ctrl Pts',(-18.2296197656979,13.2093278251547,123.825264369513)) ;
#16221 = CARTESIAN_POINT('Ctrl Pts',(-18.2281169132799,13.2095372697089,123.820951227691)) ;
#16222 = CARTESIAN_POINT('Ctrl Pts',(-18.2266375321997,13.2097468579884,123.816629333622)) ;
#16223 = CARTESIAN_POINT('Ctrl Pts',(-18.2072420008511,13.2124946801017,123.759966832634)) ;
#16224 = CARTESIAN_POINT('Ctrl Pts',(-18.1919435736847,13.2152547785462,123.701967615488)) ;
#16225 = CARTESIAN_POINT('Ctrl Pts',(-18.1808718008391,13.217994004838,123.643185002314)) ;
#16226 = CARTESIAN_POINT('Ctrl Pts',(-18.1641841076027,13.2221226451832,123.554586163632)) ;
#16227 = CARTESIAN_POINT('Ctrl Pts',(-18.1571640677684,13.2262321383058,123.464633492152)) ;
#16228 = CARTESIAN_POINT('Ctrl Pts',(-18.1598183418223,13.230348860005,123.3748689133)) ;
#16229 = CARTESIAN_POINT('Ctrl Pts',(-18.1614392540987,13.232862859918,123.320051473618)) ;
#16230 = CARTESIAN_POINT('Ctrl Pts',(-18.1666685394986,13.2353795555852,123.265302296028)) ;
#16231 = CARTESIAN_POINT('Ctrl Pts',(-18.1755124084081,13.2379049538576,123.210974410351)) ;
#16232 = CARTESIAN_POINT('Ctrl Pts',(-18.1952399603618,13.2435382265954,123.089788061005)) ;
#16233 = CARTESIAN_POINT('Ctrl Pts',(-18.2327234730855,13.2491089318735,122.972124085933)) ;
#16234 = CARTESIAN_POINT('Ctrl Pts',(-18.2867834910586,13.2547574492201,122.861797078053)) ;
#16235 = CARTESIAN_POINT('Ctrl Pts',(-18.2965161638263,13.2557743776825,122.841934401247)) ;
#16236 = CARTESIAN_POINT('Ctrl Pts',(-18.3067898552594,13.2567917787257,122.822305058631)) ;
#16237 = CARTESIAN_POINT('Ctrl Pts',(-18.3175560614831,13.2578037787098,122.802999292444)) ;
#16238 = CARTESIAN_POINT('Ctrl Pts',(-18.3596833735975,13.2617636544824,122.72745735865)) ;
#16239 = CARTESIAN_POINT('Ctrl Pts',(-18.4094498495815,13.2657077366537,122.656644641517)) ;
#16240 = CARTESIAN_POINT('Ctrl Pts',(-18.4659943370288,13.2696619762082,122.591615119139)) ;
#16241 = CARTESIAN_POINT('Ctrl Pts',(-18.5044087373086,13.272348351979,122.547436274916)) ;
#16242 = CARTESIAN_POINT('Ctrl Pts',(-18.5459532309635,13.2750394157692,122.505925244562)) ;
#16243 = CARTESIAN_POINT('Ctrl Pts',(-18.590360693387,13.2777433045955,122.467418323832)) ;
#16244 = CARTESIAN_POINT('Ctrl Pts',(-18.6419648825726,13.2808853888964,122.422670925223)) ;
#16245 = CARTESIAN_POINT('Ctrl Pts',(-18.6972101956397,13.2839971960161,122.382181921752)) ;
#16246 = CARTESIAN_POINT('Ctrl Pts',(-18.7554884296589,13.287119167613,122.346419259243)) ;
#16247 = CARTESIAN_POINT('Ctrl Pts',(-18.7589739169019,13.2873058855594,122.344280376588)) ;
#16248 = CARTESIAN_POINT('Ctrl Pts',(-18.7624702419052,13.2874926398637,122.34215838877)) ;
#16249 = CARTESIAN_POINT('Ctrl Pts',(-18.7659772702078,13.2876794391776,122.340053391756)) ;
#16250 = CARTESIAN_POINT('Ctrl Pts',(-18.8283598045692,13.291002199536,122.302609996028)) ;
#16251 = CARTESIAN_POINT('Ctrl Pts',(-18.8938915827265,13.2943408185553,122.270684529986)) ;
#16252 = CARTESIAN_POINT('Ctrl Pts',(-18.9618337722691,13.2976766648834,122.244638792243)) ;
#16253 = CARTESIAN_POINT('Ctrl Pts',(-18.9759375383491,13.2983691358886,122.239232092886)) ;
#16254 = CARTESIAN_POINT('Ctrl Pts',(-18.9901453618968,13.2990607962286,122.234078864962)) ;
#16255 = CARTESIAN_POINT('Ctrl Pts',(-19.0044389742765,13.2997521504947,122.229185925203)) ;
#16256 = CARTESIAN_POINT('Ctrl Pts',(-19.058959152331,13.3023891856044,122.210522767159)) ;
#16257 = CARTESIAN_POINT('Ctrl Pts',(-19.1147001378851,13.3050268795537,122.195653767887)) ;
#16258 = CARTESIAN_POINT('Ctrl Pts',(-19.1712596402296,13.3076728273998,122.184683564916)) ;
#16259 = CARTESIAN_POINT('Ctrl Pts',(-19.2423788180773,13.3109999011477,122.170889387391)) ;
#16260 = CARTESIAN_POINT('Ctrl Pts',(-19.3145571156168,13.3143231624351,122.163310005777)) ;
#16261 = CARTESIAN_POINT('Ctrl Pts',(-19.3868925501702,13.317633218063,122.162014722725)) ;
#16262 = CARTESIAN_POINT('Ctrl Pts',(-19.4772904561789,13.3217698089244,122.160396001883)) ;
#16263 = CARTESIAN_POINT('Ctrl Pts',(-19.5674021360052,13.3258924613772,122.168589834439)) ;
#16264 = CARTESIAN_POINT('Ctrl Pts',(-19.6557028168064,13.3300196499126,122.186346305415)) ;
#16265 = CARTESIAN_POINT('Ctrl Pts',(-19.7088544483455,13.3325039660281,122.197034619414)) ;
#16266 = CARTESIAN_POINT('Ctrl Pts',(-19.7613515886273,13.3349899257055,122.211188766597)) ;
#16267 = CARTESIAN_POINT('Ctrl Pts',(-19.8128584910012,13.3374815582495,122.228759788444)) ;
#16268 = CARTESIAN_POINT('Ctrl Pts',(-19.8628380221861,13.3398993046232,122.245809764153)) ;
#16269 = CARTESIAN_POINT('Ctrl Pts',(-19.9117638198388,13.3423053796767,122.266040733864)) ;
#16270 = CARTESIAN_POINT('Ctrl Pts',(-19.9592397024072,13.344723836538,122.28930121033)) ;
#16271 = CARTESIAN_POINT('Ctrl Pts',(-20.0419784854064,13.3489386118432,122.329838498122)) ;
#16272 = CARTESIAN_POINT('Ctrl Pts',(-20.1199625744019,13.3531881524558,122.379386706394)) ;
#16273 = CARTESIAN_POINT('Ctrl Pts',(-20.1918044690641,13.3574053919986,122.437061421343)) ;
#16274 = CARTESIAN_POINT('Ctrl Pts',(-20.2484665510601,13.3607315511136,122.482549773827)) ;
#16275 = CARTESIAN_POINT('Ctrl Pts',(-20.3010658368689,13.3640386988681,122.532902439704)) ;
#16276 = CARTESIAN_POINT('Ctrl Pts',(-20.3489907498894,13.3673857229415,122.587539464216)) ;
#16277 = CARTESIAN_POINT('Ctrl Pts',(-20.3966435956241,13.37071374613,122.641866317127)) ;
#16278 = CARTESIAN_POINT('Ctrl Pts',(-20.439495919874,13.374022327351,122.700223486028)) ;
#16279 = CARTESIAN_POINT('Ctrl Pts',(-20.4770662197135,13.3773157278759,122.761955914037)) ;
#16280 = CARTESIAN_POINT('Ctrl Pts',(-20.5147773812097,13.3806214762888,122.82391979434)) ;
#16281 = CARTESIAN_POINT('Ctrl Pts',(-20.5470231453038,13.3839416549025,122.889047248779)) ;
#16282 = CARTESIAN_POINT('Ctrl Pts',(-20.5734409337567,13.3872834493149,122.956609749793)) ;
#16283 = CARTESIAN_POINT('Ctrl Pts',(-20.5799521068342,13.3881070989495,122.973261830205)) ;
#16284 = CARTESIAN_POINT('Ctrl Pts',(-20.5861082466563,13.3889304241705,122.990059702568)) ;
#16285 = CARTESIAN_POINT('Ctrl Pts',(-20.5919016415172,13.3897528569022,123.006983921598)) ;
#16286 = CARTESIAN_POINT('Origin',(-19.4092722359532,16.5113612779716,123.411814366564)) ;
#16287 = CARTESIAN_POINT('',(-20.5919010929731,12.6697683433189,123.006982319198)) ;
#16288 = CARTESIAN_POINT('',(-20.5919043739536,12.7298332115048,123.006991903941)) ;
#16289 = CARTESIAN_POINT('',(-20.5919021064381,16.5113612779716,123.006985279772)) ;
#16290 = CARTESIAN_POINT('Ctrl Pts',(-20.5919014130362,13.0898536069868,123.006983254138)) ;
#16291 = CARTESIAN_POINT('Ctrl Pts',(-20.5791790206653,13.0880587850324,122.969817453491)) ;
#16292 = CARTESIAN_POINT('Ctrl Pts',(-20.5647155841445,13.0862721300352,122.933281380902)) ;
#16293 = CARTESIAN_POINT('Ctrl Pts',(-20.5452931183874,13.0841163519632,122.890259692648)) ;
#16294 = CARTESIAN_POINT('Ctrl Pts',(-20.5419658468915,13.0837543841713,122.883072551962)) ;
#16295 = CARTESIAN_POINT('Ctrl Pts',(-20.5357135669482,13.0830872032147,122.86989708902)) ;
#16296 = CARTESIAN_POINT('Ctrl Pts',(-20.5328085362647,13.0827821035447,122.863899601794)) ;
#16297 = CARTESIAN_POINT('Ctrl Pts',(-20.5266929064853,13.0821496688658,122.851526947794)) ;
#16298 = CARTESIAN_POINT('Ctrl Pts',(-20.5234753799025,13.0818223066021,122.845155474289)) ;
#16299 = CARTESIAN_POINT('Ctrl Pts',(-20.5150841630547,13.080981988997,122.828886669669)) ;
#16300 = CARTESIAN_POINT('Ctrl Pts',(-20.5098320947547,13.0804686351631,122.819030498871)) ;
#16301 = CARTESIAN_POINT('Ctrl Pts',(-20.4908842883934,13.078659771017,122.784592592427)) ;
#16302 = CARTESIAN_POINT('Ctrl Pts',(-20.4764913302073,13.0773615396779,122.760404213382)) ;
#16303 = CARTESIAN_POINT('Ctrl Pts',(-20.4527297071399,13.0753350760544,122.723375557597)) ;
#16304 = CARTESIAN_POINT('Ctrl Pts',(-20.4439117842298,13.074605487379,122.710193032768)) ;
#16305 = CARTESIAN_POINT('Ctrl Pts',(-20.4304362998422,13.0735228553301,122.690854289597)) ;
#16306 = CARTESIAN_POINT('Ctrl Pts',(-20.4259687220333,13.0731689209277,122.684567686564)) ;
#16307 = CARTESIAN_POINT('Ctrl Pts',(-20.4166292464149,13.0724390993785,122.671679812802)) ;
#16308 = CARTESIAN_POINT('Ctrl Pts',(-20.4117499578622,13.0720632693731,122.665084347226)) ;
#16309 = CARTESIAN_POINT('Ctrl Pts',(-20.4004511138357,13.0712050694164,122.650121750988)) ;
#16310 = CARTESIAN_POINT('Ctrl Pts',(-20.393989886461,13.0707229458926,122.641786861669)) ;
#16311 = CARTESIAN_POINT('Ctrl Pts',(-20.3705899742046,13.0690061987055,122.612377555842)) ;
#16312 = CARTESIAN_POINT('Ctrl Pts',(-20.3530739992861,13.0677746166432,122.591772147451)) ;
#16313 = CARTESIAN_POINT('Ctrl Pts',(-20.3280211934725,13.0660737435465,122.564167488205)) ;
#16314 = CARTESIAN_POINT('Ctrl Pts',(-20.3210458281659,13.0656062078695,122.556668885868)) ;
#16315 = CARTESIAN_POINT('Ctrl Pts',(-20.3083267464374,13.0647637665576,122.543328278811)) ;
#16316 = CARTESIAN_POINT('Ctrl Pts',(-20.3026162469189,13.0643890731206,122.537455415673)) ;
#16317 = CARTESIAN_POINT('Ctrl Pts',(-20.2956550140089,13.0639364010447,122.530435649181)) ;
#16318 = CARTESIAN_POINT('Ctrl Pts',(-20.2944591356239,13.0638587797494,122.52923461077)) ;
#16319 = CARTESIAN_POINT('Ctrl Pts',(-20.2925818801849,13.0637371557354,122.527356908787)) ;
#16320 = CARTESIAN_POINT('Ctrl Pts',(-20.2919021595124,13.0636931635908,122.526678591529)) ;
#16321 = CARTESIAN_POINT('Ctrl Pts',(-20.2855535475068,13.0632827007654,122.520357671943)) ;
#16322 = CARTESIAN_POINT('Ctrl Pts',(-20.2798314133098,13.0629158959593,122.5147688306)) ;
#16323 = CARTESIAN_POINT('Ctrl Pts',(-20.2620038089164,13.0617826277711,122.49768775231)) ;
#16324 = CARTESIAN_POINT('Ctrl Pts',(-20.2497215250182,13.0610151242612,122.486382796024)) ;
#16325 = CARTESIAN_POINT('Ctrl Pts',(-20.2275007691805,13.0596504182977,122.466737519096)) ;
#16326 = CARTESIAN_POINT('Ctrl Pts',(-20.2176518666741,13.059053514139,122.45829952495)) ;
#16327 = CARTESIAN_POINT('Ctrl Pts',(-20.2032180846653,13.0581909897426,122.446317852719)) ;
#16328 = CARTESIAN_POINT('Ctrl Pts',(-20.1987370681398,13.0579248875879,122.442650392889)) ;
#16329 = CARTESIAN_POINT('Ctrl Pts',(-20.1935525025875,13.0576190062421,122.438466934799)) ;
#16330 = CARTESIAN_POINT('Ctrl Pts',(-20.1928737080088,13.0575789976055,122.437920382319)) ;
#16331 = CARTESIAN_POINT('Ctrl Pts',(-20.1915087192564,13.0574986234605,122.4368236703)) ;
#16332 = CARTESIAN_POINT('Ctrl Pts',(-20.1908225152045,13.057458258173,122.436273524459)) ;
#16333 = CARTESIAN_POINT('Ctrl Pts',(-20.1875199419223,13.0572641797235,122.433631495324)) ;
#16334 = CARTESIAN_POINT('Ctrl Pts',(-20.1848957489494,13.057110545949,122.431549408724)) ;
#16335 = CARTESIAN_POINT('Ctrl Pts',(-20.1817827671608,13.0569289610988,122.429099833748)) ;
#16336 = CARTESIAN_POINT('Ctrl Pts',(-20.1813020415568,13.0569009383371,122.428722126184)) ;
#16337 = CARTESIAN_POINT('Ctrl Pts',(-20.1749755695237,13.0565323959611,122.423758900124)) ;
#16338 = CARTESIAN_POINT('Ctrl Pts',(-20.1690893191057,13.0561922396103,122.419225226801)) ;
#16339 = CARTESIAN_POINT('Ctrl Pts',(-20.1464151149356,13.0548917623543,122.402081122969)) ;
#16340 = CARTESIAN_POINT('Ctrl Pts',(-20.1293507949056,13.0539333670138,122.38984190088)) ;
#16341 = CARTESIAN_POINT('Ctrl Pts',(-20.0935184368185,13.0519557092244,122.365484690616)) ;
#16342 = CARTESIAN_POINT('Ctrl Pts',(-20.0747175367803,13.0509367931673,122.353428234847)) ;
#16343 = CARTESIAN_POINT('Ctrl Pts',(-20.0446747203537,13.0493330165717,122.335279780015)) ;
#16344 = CARTESIAN_POINT('Ctrl Pts',(-20.0336451243973,13.0487492306961,122.328845517366)) ;
#16345 = CARTESIAN_POINT('Ctrl Pts',(-20.0148661944338,13.0477629679816,122.318272833221)) ;
#16346 = CARTESIAN_POINT('Ctrl Pts',(-20.0071682925871,13.0473608151302,122.314045068055)) ;
#16347 = CARTESIAN_POINT('Ctrl Pts',(-19.9885573709466,13.0463934044849,122.304077594401)) ;
#16348 = CARTESIAN_POINT('Ctrl Pts',(-19.9776027396486,13.0458279314908,122.298417554343)) ;
#16349 = CARTESIAN_POINT('Ctrl Pts',(-19.9450826159544,13.0441602047694,122.28222006754)) ;
#16350 = CARTESIAN_POINT('Ctrl Pts',(-19.9232953680866,13.0430567814907,122.272140616113)) ;
#16351 = CARTESIAN_POINT('Ctrl Pts',(-19.8827606791136,13.041028033727,122.254786968767)) ;
#16352 = CARTESIAN_POINT('Ctrl Pts',(-19.8641018238544,13.0401032834668,122.247325744044)) ;
#16353 = CARTESIAN_POINT('Ctrl Pts',(-19.8370544133023,13.0387763300771,122.237259439374)) ;
#16354 = CARTESIAN_POINT('Ctrl Pts',(-19.8288056227823,13.0383734293611,122.234287888713)) ;
#16355 = CARTESIAN_POINT('Ctrl Pts',(-19.819577315835,13.0379247506337,122.231072755854)) ;
#16356 = CARTESIAN_POINT('Ctrl Pts',(-19.8186279901786,13.0378786188541,122.2307432949)) ;
#16357 = CARTESIAN_POINT('Ctrl Pts',(-19.8168267041893,13.037791132955,122.23012059603)) ;
#16358 = CARTESIAN_POINT('Ctrl Pts',(-19.8159748220509,13.0377497778537,122.229827133824)) ;
#16359 = CARTESIAN_POINT('Ctrl Pts',(-19.8140710536562,13.0376574023267,122.229173612418)) ;
#16360 = CARTESIAN_POINT('Ctrl Pts',(-19.8130190027272,13.0376063842296,122.228814034991)) ;
#16361 = CARTESIAN_POINT('Ctrl Pts',(-19.8055448821177,13.0372441481705,122.226270608562)) ;
#16362 = CARTESIAN_POINT('Ctrl Pts',(-19.7991056000856,13.0369331808838,122.224137659408)) ;
#16363 = CARTESIAN_POINT('Ctrl Pts',(-19.7900598760826,13.0364977577974,122.22122284369)) ;
#16364 = CARTESIAN_POINT('Ctrl Pts',(-19.7874677668294,13.0363731466514,122.220396915938)) ;
#16365 = CARTESIAN_POINT('Ctrl Pts',(-19.7617315938096,13.0351374677625,122.212289012309)) ;
#16366 = CARTESIAN_POINT('Ctrl Pts',(-19.7383827968355,13.0340287048108,122.205673861513)) ;
#16367 = CARTESIAN_POINT('Ctrl Pts',(-19.6942375807687,13.0319476481019,122.194544098501)) ;
#16368 = CARTESIAN_POINT('Ctrl Pts',(-19.673489620474,13.0309757755871,122.189872745543)) ;
#16369 = CARTESIAN_POINT('Ctrl Pts',(-19.6364815259975,13.0292493797788,122.182527144479)) ;
#16370 = CARTESIAN_POINT('Ctrl Pts',(-19.6202686646467,13.0284954717176,122.179640823168)) ;
#16371 = CARTESIAN_POINT('Ctrl Pts',(-19.6022976823653,13.027661616081,122.176806609706)) ;
#16372 = CARTESIAN_POINT('Ctrl Pts',(-19.6005912530173,13.0275824556779,122.176541110896)) ;
#16373 = CARTESIAN_POINT('Ctrl Pts',(-19.5976149459336,13.0274444165535,122.176084350409)) ;
#16374 = CARTESIAN_POINT('Ctrl Pts',(-19.596345313313,13.0273855414425,122.175891507743)) ;
#16375 = CARTESIAN_POINT('Ctrl Pts',(-19.593487886595,13.0272530584297,122.175462001246)) ;
#16376 = CARTESIAN_POINT('Ctrl Pts',(-19.591899929316,13.0271794481916,122.175226438924)) ;
#16377 = CARTESIAN_POINT('Ctrl Pts',(-19.5714744332639,13.0262327976296,122.172236661951)) ;
#16378 = CARTESIAN_POINT('Ctrl Pts',(-19.5525768533619,13.025358891184,122.169910094061)) ;
#16379 = CARTESIAN_POINT('Ctrl Pts',(-19.4970543984554,13.0227947785655,122.164358674257)) ;
#16380 = CARTESIAN_POINT('Ctrl Pts',(-19.4603317164738,13.0211029801371,122.162316733384)) ;
#16381 = CARTESIAN_POINT('Ctrl Pts',(-19.4119781567302,13.0188790327024,122.161763516417)) ;
#16382 = CARTESIAN_POINT('Ctrl Pts',(-19.4003823613712,13.0183460185202,122.161792198416)) ;
#16383 = CARTESIAN_POINT('Ctrl Pts',(-19.3882597526607,13.0177891852922,122.161990876862)) ;
#16384 = CARTESIAN_POINT('Ctrl Pts',(-19.3877308783924,13.0177648930705,122.161999880419)) ;
#16385 = CARTESIAN_POINT('Ctrl Pts',(-19.3865241254111,13.0177094664024,122.162021190389)) ;
#16386 = CARTESIAN_POINT('Ctrl Pts',(-19.3858462506889,13.0176783326659,122.162033712625)) ;
#16387 = CARTESIAN_POINT('Ctrl Pts',(-19.3841699374231,13.0176013452949,122.162066043118)) ;
#16388 = CARTESIAN_POINT('Ctrl Pts',(-19.383171511717,13.0175554937149,122.162086496369)) ;
#16389 = CARTESIAN_POINT('Ctrl Pts',(-19.3805211783401,13.017433786664,122.162143967248)) ;
#16390 = CARTESIAN_POINT('Ctrl Pts',(-19.3788693174578,13.0173579376186,122.162183063823)) ;
#16391 = CARTESIAN_POINT('Ctrl Pts',(-19.3759793380935,13.0172252472493,122.162257198133)) ;
#16392 = CARTESIAN_POINT('Ctrl Pts',(-19.3747411853149,13.0171684019035,122.162290801053)) ;
#16393 = CARTESIAN_POINT('Ctrl Pts',(-19.3719442822547,13.0170399981373,122.16237086812)) ;
#16394 = CARTESIAN_POINT('Ctrl Pts',(-19.3703855647219,13.0169684427767,122.162418409018)) ;
#16395 = CARTESIAN_POINT('Ctrl Pts',(-19.3615548536221,13.0165630737479,122.162704287283)) ;
#16396 = CARTESIAN_POINT('Ctrl Pts',(-19.3542849546739,13.0162294236945,122.16300319676)) ;
#16397 = CARTESIAN_POINT('Ctrl Pts',(-19.3120330825369,13.014290162207,122.165110095221)) ;
#16398 = CARTESIAN_POINT('Ctrl Pts',(-19.2771367987849,13.0126877295686,122.168324427429)) ;
#16399 = CARTESIAN_POINT('Ctrl Pts',(-19.1956810388155,13.0089264329111,122.179295353745)) ;
#16400 = CARTESIAN_POINT('Ctrl Pts',(-19.1493341988922,13.0067723538331,122.188230890597)) ;
#16401 = CARTESIAN_POINT('Ctrl Pts',(-19.0901293426453,13.0039758566922,122.203161846975)) ;
#16402 = CARTESIAN_POINT('Ctrl Pts',(-19.0767128216625,13.0033389811045,122.20678435273)) ;
#16403 = CARTESIAN_POINT('Ctrl Pts',(-19.0626349751978,13.0026670308939,122.210838439235)) ;
#16404 = CARTESIAN_POINT('Ctrl Pts',(-19.0619106250721,13.0026324466501,122.211047744837)) ;
#16405 = CARTESIAN_POINT('Ctrl Pts',(-19.027951217023,13.0010105651996,122.220893833009)) ;
#16406 = CARTESIAN_POINT('Ctrl Pts',(-18.9951304778569,12.999420487923,122.231905879089)) ;
#16407 = CARTESIAN_POINT('Ctrl Pts',(-18.9457163206155,12.9969958633874,122.250801535115)) ;
#16408 = CARTESIAN_POINT('Ctrl Pts',(-18.928769184131,12.9961588816672,122.257712247526)) ;
#16409 = CARTESIAN_POINT('Ctrl Pts',(-18.8926559513687,12.9943582312864,122.273371903399)) ;
#16410 = CARTESIAN_POINT('Ctrl Pts',(-18.8735469465325,12.9933947708513,122.282238322564)) ;
#16411 = CARTESIAN_POINT('Ctrl Pts',(-18.843319986932,12.9918494458271,122.297203007569)) ;
#16412 = CARTESIAN_POINT('Ctrl Pts',(-18.8320549271127,12.9912686851965,122.302994901097)) ;
#16413 = CARTESIAN_POINT('Ctrl Pts',(-18.7779523075682,12.9884543504816,122.331859529778)) ;
#16414 = CARTESIAN_POINT('Ctrl Pts',(-18.7363986331257,12.9862155933072,122.35724886596)) ;
#16415 = CARTESIAN_POINT('Ctrl Pts',(-18.6832536210952,12.9832401877453,122.394143349128)) ;
#16416 = CARTESIAN_POINT('Ctrl Pts',(-18.670253570575,12.982502785968,122.40354419319)) ;
#16417 = CARTESIAN_POINT('Ctrl Pts',(-18.6568542700139,12.9817324570081,122.413632149447)) ;
#16418 = CARTESIAN_POINT('Ctrl Pts',(-18.6562708796068,12.9816988970731,122.414072169713)) ;
#16419 = CARTESIAN_POINT('Ctrl Pts',(-18.6552280583346,12.9816388710275,122.414860149748)) ;
#16420 = CARTESIAN_POINT('Ctrl Pts',(-18.6547684816316,12.9816124043525,122.415207916182)) ;
#16421 = CARTESIAN_POINT('Ctrl Pts',(-18.6539431552673,12.9815648512559,122.415833347259)) ;
#16422 = CARTESIAN_POINT('Ctrl Pts',(-18.6535773177867,12.9815437644863,122.416110895844)) ;
#16423 = CARTESIAN_POINT('Ctrl Pts',(-18.652917595774,12.981505723505,122.416611977756)) ;
#16424 = CARTESIAN_POINT('Ctrl Pts',(-18.6526236571881,12.9814887690753,122.416835439821)) ;
#16425 = CARTESIAN_POINT('Ctrl Pts',(-18.6520916392232,12.9814580725791,122.417240269984)) ;
#16426 = CARTESIAN_POINT('Ctrl Pts',(-18.6518535258812,12.9814443303732,122.417421593418)) ;
#16427 = CARTESIAN_POINT('Ctrl Pts',(-18.6514211573751,12.9814193708071,122.417751087661)) ;
#16428 = CARTESIAN_POINT('Ctrl Pts',(-18.651226880506,12.9814081533581,122.41789922992)) ;
#16429 = CARTESIAN_POINT('Ctrl Pts',(-18.6505383182002,12.9813683878704,122.418424599783)) ;
#16430 = CARTESIAN_POINT('Ctrl Pts',(-18.6500442707932,12.981339840836,122.418802139241)) ;
#16431 = CARTESIAN_POINT('Ctrl Pts',(-18.6490926691779,12.9812848263507,122.419530456217)) ;
#16432 = CARTESIAN_POINT('Ctrl Pts',(-18.6486350755503,12.9812583587371,122.419881181974)) ;
#16433 = CARTESIAN_POINT('Ctrl Pts',(-18.647750956529,12.9812071954238,122.420559792556)) ;
#16434 = CARTESIAN_POINT('Ctrl Pts',(-18.6473243998143,12.9811824995908,122.420887636422)) ;
#16435 = CARTESIAN_POINT('Ctrl Pts',(-18.6464975854278,12.9811346085761,122.421523960694)) ;
#16436 = CARTESIAN_POINT('Ctrl Pts',(-18.6460973028754,12.9811114132861,122.421832408666)) ;
#16437 = CARTESIAN_POINT('Ctrl Pts',(-18.6453187930819,12.9810662812955,122.422433062091)) ;
#16438 = CARTESIAN_POINT('Ctrl Pts',(-18.644940546199,12.9810443445111,122.422725241888)) ;
#16439 = CARTESIAN_POINT('Ctrl Pts',(-18.6442022752297,12.9810015103051,122.423296201526)) ;
#16440 = CARTESIAN_POINT('Ctrl Pts',(-18.6438422357157,12.9809806128162,122.423574961285)) ;
#16441 = CARTESIAN_POINT('Ctrl Pts',(-18.6431368540126,12.9809396549576,122.424121718167)) ;
#16442 = CARTESIAN_POINT('Ctrl Pts',(-18.6427914999497,12.9809195945366,122.42438969982)) ;
#16443 = CARTESIAN_POINT('Ctrl Pts',(-18.6421121710587,12.9808801199055,122.424917404414)) ;
#16444 = CARTESIAN_POINT('Ctrl Pts',(-18.6417781874006,12.9808607056574,122.425177115845)) ;
#16445 = CARTESIAN_POINT('Ctrl Pts',(-18.6411183874357,12.9808223380162,122.425690725379)) ;
#16446 = CARTESIAN_POINT('Ctrl Pts',(-18.6407925649553,12.9808033845936,122.425944615553)) ;
#16447 = CARTESIAN_POINT('Ctrl Pts',(-18.640145871009,12.9807657524226,122.426449053314)) ;
#16448 = CARTESIAN_POINT('Ctrl Pts',(-18.6398249960202,12.9807470736617,122.426699596211)) ;
#16449 = CARTESIAN_POINT('Ctrl Pts',(-18.6391848458334,12.9807097962395,122.42719993645)) ;
#16450 = CARTESIAN_POINT('Ctrl Pts',(-18.6388655696197,12.9806911975741,122.427449732458)) ;
#16451 = CARTESIAN_POINT('Ctrl Pts',(-18.6382249639607,12.9806538676342,122.42795143346)) ;
#16452 = CARTESIAN_POINT('Ctrl Pts',(-18.6379036362931,12.9806351363697,122.428203340679)) ;
#16453 = CARTESIAN_POINT('Ctrl Pts',(-18.6372547426427,12.9805972969007,122.428712559218)) ;
#16454 = CARTESIAN_POINT('Ctrl Pts',(-18.6369271817776,12.9805781887261,122.428969876894)) ;
#16455 = CARTESIAN_POINT('Ctrl Pts',(-18.6362607636861,12.9805392994611,122.429493925064)) ;
#16456 = CARTESIAN_POINT('Ctrl Pts',(-18.6359219157202,12.9805195184189,122.429760667299)) ;
#16457 = CARTESIAN_POINT('Ctrl Pts',(-18.635226450761,12.9804789039328,122.430308722763)) ;
#16458 = CARTESIAN_POINT('Ctrl Pts',(-18.6348698489277,12.9804580705699,122.430590055126)) ;
#16459 = CARTESIAN_POINT('Ctrl Pts',(-18.6343297402126,12.9804265040148,122.431016638618)) ;
#16460 = CARTESIAN_POINT('Ctrl Pts',(-18.6341461206411,12.9804157702345,122.431161747025)) ;
#16461 = CARTESIAN_POINT('Ctrl Pts',(-18.6336578666299,12.9803872227858,122.431547820649)) ;
#16462 = CARTESIAN_POINT('Ctrl Pts',(-18.6333533036907,12.9803694094925,122.431788876335)) ;
#16463 = CARTESIAN_POINT('Ctrl Pts',(-18.6320800479274,12.9802949142445,122.432797599279)) ;
#16464 = CARTESIAN_POINT('Ctrl Pts',(-18.6311123814247,12.9802382377696,122.433566561274)) ;
#16465 = CARTESIAN_POINT('Ctrl Pts',(-18.6234797433569,12.979790713378,122.439650374163)) ;
#16466 = CARTESIAN_POINT('Ctrl Pts',(-18.6168681460405,12.9794001674855,122.44503185309)) ;
#16467 = CARTESIAN_POINT('Ctrl Pts',(-18.6041453408943,12.9786429798368,122.455605718184)) ;
#16468 = CARTESIAN_POINT('Ctrl Pts',(-18.5980280233729,12.9782763130836,122.460790116357)) ;
#16469 = CARTESIAN_POINT('Ctrl Pts',(-18.5675857788878,12.9764385012305,122.487097241842)) ;
#16470 = CARTESIAN_POINT('Ctrl Pts',(-18.5440338962702,12.9749740577999,122.509095980903)) ;
#16471 = CARTESIAN_POINT('Ctrl Pts',(-18.5075320730355,12.9726134887217,122.545933009054)) ;
#16472 = CARTESIAN_POINT('Ctrl Pts',(-18.4940368669183,12.9717190257007,122.56020996154)) ;
#16473 = CARTESIAN_POINT('Ctrl Pts',(-18.4735195841935,12.9703212760591,122.58296702056)) ;
#16474 = CARTESIAN_POINT('Ctrl Pts',(-18.4662635579141,12.9698191604314,122.591231902454)) ;
#16475 = CARTESIAN_POINT('Ctrl Pts',(-18.4526278932898,12.9688599725934,122.607183176556)) ;
#16476 = CARTESIAN_POINT('Ctrl Pts',(-18.4462294645572,12.9684030344231,122.614852403913)) ;
#16477 = CARTESIAN_POINT('Ctrl Pts',(-18.4365858263844,12.9677034888554,122.626697116171)) ;
#16478 = CARTESIAN_POINT('Ctrl Pts',(-18.4332740517988,12.9674612371538,122.630817892419)) ;
#16479 = CARTESIAN_POINT('Ctrl Pts',(-18.4236239785505,12.966749325402,122.642982532909)) ;
#16480 = CARTESIAN_POINT('Ctrl Pts',(-18.417358283924,12.9662793296657,122.651083411056)) ;
#16481 = CARTESIAN_POINT('Ctrl Pts',(-18.3971954033054,12.9647408224713,122.677824555117)) ;
#16482 = CARTESIAN_POINT('Ctrl Pts',(-18.3837186616704,12.9636706487908,122.696775613893)) ;
#16483 = CARTESIAN_POINT('Ctrl Pts',(-18.3566449155309,12.9614295702289,122.737188136417)) ;
#16484 = CARTESIAN_POINT('Ctrl Pts',(-18.3431576106487,12.9602589686713,122.75871067245)) ;
#16485 = CARTESIAN_POINT('Ctrl Pts',(-18.3270206646114,12.9587889819773,122.786294883082)) ;
#16486 = CARTESIAN_POINT('Ctrl Pts',(-18.323750793524,12.9584872474056,122.791986740363)) ;
#16487 = CARTESIAN_POINT('Ctrl Pts',(-18.320511645787,12.9581844576396,122.797729373897)) ;
#16488 = CARTESIAN_POINT('Ctrl Pts',(-18.3204973895175,12.9581831249122,122.797754650668)) ;
#16489 = CARTESIAN_POINT('Ctrl Pts',(-18.3204691408688,12.9581804839746,122.7978047404)) ;
#16490 = CARTESIAN_POINT('Ctrl Pts',(-18.3204551484335,12.9581791757621,122.797829553387)) ;
#16491 = CARTESIAN_POINT('Ctrl Pts',(-18.3204274204869,12.9581765832113,122.797878727682)) ;
#16492 = CARTESIAN_POINT('Ctrl Pts',(-18.3204136850449,12.9581752988823,122.797903088795)) ;
#16493 = CARTESIAN_POINT('Ctrl Pts',(-18.3203864645046,12.9581727534913,122.797951370802)) ;
#16494 = CARTESIAN_POINT('Ctrl Pts',(-18.3203729794039,12.9581714924316,122.79797529163)) ;
#16495 = CARTESIAN_POINT('Ctrl Pts',(-18.3203462532489,12.9581689929981,122.798022704032)) ;
#16496 = CARTESIAN_POINT('Ctrl Pts',(-18.3203330120995,12.9581677546178,122.798046195708)) ;
#16497 = CARTESIAN_POINT('Ctrl Pts',(-18.3203067676139,12.9581652999673,122.79809276067)) ;
#16498 = CARTESIAN_POINT('Ctrl Pts',(-18.3202937642996,12.9581640837015,122.798115833853)) ;
#16499 = CARTESIAN_POINT('Ctrl Pts',(-18.3202679893627,12.9581616727145,122.798161572502)) ;
#16500 = CARTESIAN_POINT('Ctrl Pts',(-18.3202552178929,12.9581604780098,122.798184237637)) ;
#16501 = CARTESIAN_POINT('Ctrl Pts',(-18.3202299010075,12.9581581096243,122.798229170014)) ;
#16502 = CARTESIAN_POINT('Ctrl Pts',(-18.320217355408,12.9581569359284,122.798251437526)) ;
#16503 = CARTESIAN_POINT('Ctrl Pts',(-18.3201924845428,12.9581546090318,122.79829558464)) ;
#16504 = CARTESIAN_POINT('Ctrl Pts',(-18.3201801593888,12.9581534558435,122.798317463988)) ;
#16505 = CARTESIAN_POINT('Ctrl Pts',(-18.3201557240377,12.9581511694652,122.798360844154)) ;
#16506 = CARTESIAN_POINT('Ctrl Pts',(-18.3201436136676,12.958150036261,122.798382345226)) ;
#16507 = CARTESIAN_POINT('Ctrl Pts',(-18.320119602475,12.9581477893504,122.798424978287)) ;
#16508 = CARTESIAN_POINT('Ctrl Pts',(-18.3201077017835,12.9581466756582,122.798446109992)) ;
#16509 = CARTESIAN_POINT('Ctrl Pts',(-18.3200841050796,12.9581444673218,122.798488012811)) ;
#16510 = CARTESIAN_POINT('Ctrl Pts',(-18.3200724086253,12.958143372638,122.798508784662)) ;
#16511 = CARTESIAN_POINT('Ctrl Pts',(-18.3200408206558,12.9581404161459,122.798564885807)) ;
#16512 = CARTESIAN_POINT('Ctrl Pts',(-18.3200209304437,12.9581385543615,122.798600215418)) ;
#16513 = CARTESIAN_POINT('Ctrl Pts',(-18.3199812996294,12.9581348444979,122.798670616911)) ;
#16514 = CARTESIAN_POINT('Ctrl Pts',(-18.3199615590029,12.9581329964186,122.798705688777)) ;
#16515 = CARTESIAN_POINT('Ctrl Pts',(-18.3199222249075,12.9581293137423,122.79877557896)) ;
#16516 = CARTESIAN_POINT('Ctrl Pts',(-18.3199026313337,12.9581274791376,122.798810397407)) ;
#16517 = CARTESIAN_POINT('Ctrl Pts',(-18.3198635887295,12.9581238231721,122.798879785223)) ;
#16518 = CARTESIAN_POINT('Ctrl Pts',(-18.3198441397624,12.9581220018193,122.798914354426)) ;
#16519 = CARTESIAN_POINT('Ctrl Pts',(-18.3198053839813,12.95811837214,122.798983247836)) ;
#16520 = CARTESIAN_POINT('Ctrl Pts',(-18.3197860769893,12.9581165637989,122.799017572306)) ;
#16521 = CARTESIAN_POINT('Ctrl Pts',(-18.3197476025284,12.9581129599028,122.799085980764)) ;
#16522 = CARTESIAN_POINT('Ctrl Pts',(-18.3197284352537,12.958111164368,122.799120064353)) ;
#16523 = CARTESIAN_POINT('Ctrl Pts',(-18.3196902379257,12.9581075858748,122.799187994982)) ;
#16524 = CARTESIAN_POINT('Ctrl Pts',(-18.3196712076845,12.9581058029009,122.799221842304)) ;
#16525 = CARTESIAN_POINT('Ctrl Pts',(-18.3196332820241,12.9581022493103,122.799289304511)) ;
#16526 = CARTESIAN_POINT('Ctrl Pts',(-18.319614386617,12.9581004786969,122.799322919324)) ;
#16527 = CARTESIAN_POINT('Ctrl Pts',(-18.319576728093,12.9580969495959,122.799389920864)) ;
#16528 = CARTESIAN_POINT('Ctrl Pts',(-18.319557965132,12.9580951911248,122.799423307264)) ;
#16529 = CARTESIAN_POINT('Ctrl Pts',(-18.3195205692749,12.9580916861055,122.79948985579)) ;
#16530 = CARTESIAN_POINT('Ctrl Pts',(-18.3195019362965,12.9580899395515,122.799523018014)) ;
#16531 = CARTESIAN_POINT('Ctrl Pts',(-18.3194647981766,12.9580864581629,122.799589122009)) ;
#16532 = CARTESIAN_POINT('Ctrl Pts',(-18.3194462929502,12.9580847233222,122.799622063884)) ;
#16533 = CARTESIAN_POINT('Ctrl Pts',(-18.319409408017,12.9580812651482,122.799687731163)) ;
#16534 = CARTESIAN_POINT('Ctrl Pts',(-18.319391028292,12.9580795418151,122.799720456554)) ;
#16535 = CARTESIAN_POINT('Ctrl Pts',(-18.3193543920568,12.9580761064453,122.799785694832)) ;
#16536 = CARTESIAN_POINT('Ctrl Pts',(-18.3193361355751,12.9580743944131,122.799818207623)) ;
#16537 = CARTESIAN_POINT('Ctrl Pts',(-18.3192997436849,12.9580709814495,122.799883024381)) ;
#16538 = CARTESIAN_POINT('Ctrl Pts',(-18.31928160816,12.9580692805088,122.79991532851)) ;
#16539 = CARTESIAN_POINT('Ctrl Pts',(-18.3192454558336,12.9580658895128,122.799979732)) ;
#16540 = CARTESIAN_POINT('Ctrl Pts',(-18.3192274392185,12.9580641994765,122.800011830984)) ;
#16541 = CARTESIAN_POINT('Ctrl Pts',(-18.3191915225708,12.9580608300932,122.800075827869)) ;
#16542 = CARTESIAN_POINT('Ctrl Pts',(-18.3191736225289,12.9580591507469,122.800107725744)) ;
#16543 = CARTESIAN_POINT('Ctrl Pts',(-18.3191379370034,12.9580558025584,122.800171323891)) ;
#16544 = CARTESIAN_POINT('Ctrl Pts',(-18.3191201514281,12.9580541337091,122.800203024287)) ;
#16545 = CARTESIAN_POINT('Ctrl Pts',(-18.3190846927604,12.9580508063243,122.800266231052)) ;
#16546 = CARTESIAN_POINT('Ctrl Pts',(-18.3190670195495,12.9580491477793,122.800297737594)) ;
#16547 = CARTESIAN_POINT('Ctrl Pts',(-18.3190317834253,12.9580458408024,122.80036056043)) ;
#16548 = CARTESIAN_POINT('Ctrl Pts',(-18.3190142205457,12.9580441923752,122.800391876624)) ;
#16549 = CARTESIAN_POINT('Ctrl Pts',(-18.318979203096,12.9580409054517,122.800454322194)) ;
#16550 = CARTESIAN_POINT('Ctrl Pts',(-18.3189617483507,12.9580392669405,122.800485451844)) ;
#16551 = CARTESIAN_POINT('Ctrl Pts',(-18.3189269448545,12.9580359996359,122.800547528339)) ;
#16552 = CARTESIAN_POINT('Ctrl Pts',(-18.3189095964382,12.9580343708753,122.800578474552)) ;
#16553 = CARTESIAN_POINT('Ctrl Pts',(-18.3188750037851,12.9580311229058,122.8006401873)) ;
#16554 = CARTESIAN_POINT('Ctrl Pts',(-18.3188577592977,12.9580295036747,122.800670954246)) ;
#16555 = CARTESIAN_POINT('Ctrl Pts',(-18.3188233724603,12.9580262745764,122.800732311998)) ;
#16556 = CARTESIAN_POINT('Ctrl Pts',(-18.3188062302139,12.9580246647203,122.800762902584)) ;
#16557 = CARTESIAN_POINT('Ctrl Pts',(-18.3187720458929,12.9580214541912,122.800823911017)) ;
#16558 = CARTESIAN_POINT('Ctrl Pts',(-18.3187550037101,12.9580198535094,122.800854329023)) ;
#16559 = CARTESIAN_POINT('Ctrl Pts',(-18.3187210176789,12.9580166611602,122.800914995474)) ;
#16560 = CARTESIAN_POINT('Ctrl Pts',(-18.3187040736376,12.9580150694761,122.80094524423)) ;
#16561 = CARTESIAN_POINT('Ctrl Pts',(-18.3186702818322,12.9580118949326,122.801005575753)) ;
#16562 = CARTESIAN_POINT('Ctrl Pts',(-18.3186534340845,12.9580103120762,122.801035658459)) ;
#16563 = CARTESIAN_POINT('Ctrl Pts',(-18.3186198328771,12.958007155005,122.801095661336)) ;
#16564 = CARTESIAN_POINT('Ctrl Pts',(-18.3186030794223,12.9580055807919,122.801125581467)) ;
#16565 = CARTESIAN_POINT('Ctrl Pts',(-18.3185696648586,12.9580024408285,122.801185262568)) ;
#16566 = CARTESIAN_POINT('Ctrl Pts',(-18.3185530038092,12.9580008750849,122.801215023402)) ;
#16567 = CARTESIAN_POINT('Ctrl Pts',(-18.3185197722134,12.9579977518908,122.801274389108)) ;
#16568 = CARTESIAN_POINT('Ctrl Pts',(-18.3185032016251,12.9579961944375,122.801303994025)) ;
#16569 = CARTESIAN_POINT('Ctrl Pts',(-18.3184701490802,12.9579930876513,122.801363051152)) ;
#16570 = CARTESIAN_POINT('Ctrl Pts',(-18.3184536671329,12.9579915383205,122.801392503316)) ;
#16571 = CARTESIAN_POINT('Ctrl Pts',(-18.3184207900036,12.9579884476071,122.801451258183)) ;
#16572 = CARTESIAN_POINT('Ctrl Pts',(-18.3184043948167,12.9579869062252,122.801480560867)) ;
#16573 = CARTESIAN_POINT('Ctrl Pts',(-18.3183716893758,12.9579838312407,122.801539019963)) ;
#16574 = CARTESIAN_POINT('Ctrl Pts',(-18.3183553791066,12.9579822976377,122.801568176376)) ;
#16575 = CARTESIAN_POINT('Ctrl Pts',(-18.3183228416279,12.957979238038,122.801626346195)) ;
#16576 = CARTESIAN_POINT('Ctrl Pts',(-18.3183066144865,12.9579777120487,122.801655359453)) ;
#16577 = CARTESIAN_POINT('Ctrl Pts',(-18.3182742414877,12.9579746675123,122.801713246059)) ;
#16578 = CARTESIAN_POINT('Ctrl Pts',(-18.3182580955985,12.9579731489632,122.801742119436)) ;
#16579 = CARTESIAN_POINT('Ctrl Pts',(-18.3182258833002,12.9579701191407,122.801799729426)) ;
#16580 = CARTESIAN_POINT('Ctrl Pts',(-18.3182098169197,12.9579686078709,122.801828465963)) ;
#16581 = CARTESIAN_POINT('Ctrl Pts',(-18.318177761933,12.9579655924493,122.801885805246)) ;
#16582 = CARTESIAN_POINT('Ctrl Pts',(-18.3181617732108,12.9579640882874,122.801914408175)) ;
#16583 = CARTESIAN_POINT('Ctrl Pts',(-18.3181298717196,12.9579610869133,122.801971483426)) ;
#16584 = CARTESIAN_POINT('Ctrl Pts',(-18.3181139589831,12.9579595897049,122.801999955666)) ;
#16585 = CARTESIAN_POINT('Ctrl Pts',(-18.3180822072798,12.9579566020348,122.802056773373)) ;
#16586 = CARTESIAN_POINT('Ctrl Pts',(-18.3180663683915,12.9579551115814,122.802085118677)) ;
#16587 = CARTESIAN_POINT('Ctrl Pts',(-18.3180347599055,12.9579521370024,122.802141690458)) ;
#16588 = CARTESIAN_POINT('Ctrl Pts',(-18.3180189903425,12.9579506528809,122.802169916852)) ;
#16589 = CARTESIAN_POINT('Ctrl Pts',(-18.317987515633,12.9579476905094,122.802226259472)) ;
#16590 = CARTESIAN_POINT('Ctrl Pts',(-18.3179718104936,12.9579462122609,122.802254375665)) ;
#16591 = CARTESIAN_POINT('Ctrl Pts',(-18.3179404598983,12.9579432611921,122.802310506299)) ;
#16592 = CARTESIAN_POINT('Ctrl Pts',(-18.3179248142511,12.9579417883546,122.802338521063)) ;
#16593 = CARTESIAN_POINT('Ctrl Pts',(-18.3178935777475,12.9579388476493,122.802394457543)) ;
#16594 = CARTESIAN_POINT('Ctrl Pts',(-18.3178779868653,12.9579373797797,122.802422379288)) ;
#16595 = CARTESIAN_POINT('Ctrl Pts',(-18.3178468549704,12.9579344485489,122.802478138494)) ;
#16596 = CARTESIAN_POINT('Ctrl Pts',(-18.3178313139951,12.9579329851917,122.802505975872)) ;
#16597 = CARTESIAN_POINT('Ctrl Pts',(-18.3178002771128,12.9579300625354,122.802561574899)) ;
#16598 = CARTESIAN_POINT('Ctrl Pts',(-18.3177847811949,12.9579286032356,122.802589336553)) ;
#16599 = CARTESIAN_POINT('Ctrl Pts',(-18.3177538295913,12.9579256882402,122.802644792755)) ;
#16600 = CARTESIAN_POINT('Ctrl Pts',(-18.3177383739782,12.9579242325517,122.80267248716)) ;
#16601 = CARTESIAN_POINT('Ctrl Pts',(-18.3177074983048,12.9579213243395,122.802727817214)) ;
#16602 = CARTESIAN_POINT('Ctrl Pts',(-18.3176920781,12.9579198718025,122.80275545311)) ;
#16603 = CARTESIAN_POINT('Ctrl Pts',(-18.3176612684483,12.9579169694427,122.802810674706)) ;
#16604 = CARTESIAN_POINT('Ctrl Pts',(-18.3176458789701,12.9579155196172,122.802838260454)) ;
#16605 = CARTESIAN_POINT('Ctrl Pts',(-18.3176151259614,12.9579126222283,122.802893390349)) ;
#16606 = CARTESIAN_POINT('Ctrl Pts',(-18.3175997623536,12.9579111746578,122.802920934628)) ;
#16607 = CARTESIAN_POINT('Ctrl Pts',(-18.3175689857566,12.9579082746817,122.802976116626)) ;
#16608 = CARTESIAN_POINT('Ctrl Pts',(-18.3175535730068,12.957906822298,122.803003753934)) ;
#16609 = CARTESIAN_POINT('Ctrl Pts',(-18.3175226870624,12.9579039116511,122.803059141879)) ;
#16610 = CARTESIAN_POINT('Ctrl Pts',(-18.3175072138764,12.9579024533879,122.803086892521)) ;
#16611 = CARTESIAN_POINT('Ctrl Pts',(-18.3174762059163,12.9578995308718,122.803142509248)) ;
#16612 = CARTESIAN_POINT('Ctrl Pts',(-18.3174606711264,12.9578980666167,122.803170375381)) ;
#16613 = CARTESIAN_POINT('Ctrl Pts',(-18.3174295382349,12.957895131952,122.803226226241)) ;
#16614 = CARTESIAN_POINT('Ctrl Pts',(-18.3174139403413,12.9578936615613,122.803254210618)) ;
#16615 = CARTESIAN_POINT('Ctrl Pts',(-18.3173826802084,12.9578907145256,122.803310299884)) ;
#16616 = CARTESIAN_POINT('Ctrl Pts',(-18.3173670179411,12.9578892378772,122.803338404846)) ;
#16617 = CARTESIAN_POINT('Ctrl Pts',(-18.3173356275022,12.9578862781766,122.803394738146)) ;
#16618 = CARTESIAN_POINT('Ctrl Pts',(-18.3173198993763,12.957884795128,122.803422966424)) ;
#16619 = CARTESIAN_POINT('Ctrl Pts',(-18.317288376136,12.9578818225223,122.80347954837)) ;
#16620 = CARTESIAN_POINT('Ctrl Pts',(-18.3172725808613,12.9578803329492,122.803507902347)) ;
#16621 = CARTESIAN_POINT('Ctrl Pts',(-18.3172409216345,12.9578773471329,122.803564738791)) ;
#16622 = CARTESIAN_POINT('Ctrl Pts',(-18.3172250577093,12.9578758508913,122.803593221233)) ;
#16623 = CARTESIAN_POINT('Ctrl Pts',(-18.3171932596826,12.9578728515937,122.803650317367)) ;
#16624 = CARTESIAN_POINT('Ctrl Pts',(-18.3171773256136,12.9578713485399,122.803678931025)) ;
#16625 = CARTESIAN_POINT('Ctrl Pts',(-18.3171453859397,12.9578683354871,122.803736292105)) ;
#16626 = CARTESIAN_POINT('Ctrl Pts',(-18.3171293802991,12.9578668254838,122.803765039616)) ;
#16627 = CARTESIAN_POINT('Ctrl Pts',(-18.3170972958036,12.9578637983708,122.803822671491)) ;
#16628 = CARTESIAN_POINT('Ctrl Pts',(-18.3170812170452,12.9578622812693,122.803851555707)) ;
#16629 = CARTESIAN_POINT('Ctrl Pts',(-18.3170489846219,12.9578592397973,122.803909464108)) ;
#16630 = CARTESIAN_POINT('Ctrl Pts',(-18.317032831108,12.9578577154401,122.803938488047)) ;
#16631 = CARTESIAN_POINT('Ctrl Pts',(-18.3170004478664,12.9578546593306,122.803996678322)) ;
#16632 = CARTESIAN_POINT('Ctrl Pts',(-18.3169842180737,12.9578531275711,122.804025844801)) ;
#16633 = CARTESIAN_POINT('Ctrl Pts',(-18.3169516808187,12.9578500565165,122.804084322851)) ;
#16634 = CARTESIAN_POINT('Ctrl Pts',(-18.3169353732382,12.9578485172092,122.804113634662)) ;
#16635 = CARTESIAN_POINT('Ctrl Pts',(-18.316902678415,12.9578454308678,122.804172407039)) ;
#16636 = CARTESIAN_POINT('Ctrl Pts',(-18.3168862912965,12.9578438838444,122.80420186741)) ;
#16637 = CARTESIAN_POINT('Ctrl Pts',(-18.3168534359091,12.9578407819271,122.804260939667)) ;
#16638 = CARTESIAN_POINT('Ctrl Pts',(-18.3168369676573,12.9578392270338,122.804290551552)) ;
#16639 = CARTESIAN_POINT('Ctrl Pts',(-18.316803948079,12.9578361091918,122.804349930383)) ;
#16640 = CARTESIAN_POINT('Ctrl Pts',(-18.3167873968819,12.9578345462542,122.804379697126)) ;
#16641 = CARTESIAN_POINT('Ctrl Pts',(-18.3167542100353,12.9578314121902,122.804439388242)) ;
#16642 = CARTESIAN_POINT('Ctrl Pts',(-18.3167375742817,12.9578298410529,122.804469312831)) ;
#16643 = CARTESIAN_POINT('Ctrl Pts',(-18.3167042163813,12.9578266904026,122.80452932322)) ;
#16644 = CARTESIAN_POINT('Ctrl Pts',(-18.3166874942634,12.9578251108913,122.804559408999)) ;
#16645 = CARTESIAN_POINT('Ctrl Pts',(-18.3166539617726,12.9578219433137,122.804619745211)) ;
#16646 = CARTESIAN_POINT('Ctrl Pts',(-18.3166371514269,12.9578203552488,122.804649995627)) ;
#16647 = CARTESIAN_POINT('Ctrl Pts',(-18.316603440968,12.9578171704177,122.80471066393)) ;
#16648 = CARTESIAN_POINT('Ctrl Pts',(-18.3165865406907,12.9578155736347,122.804741082145)) ;
#16649 = CARTESIAN_POINT('Ctrl Pts',(-18.316552648186,12.9578123711574,122.804802090074)) ;
#16650 = CARTESIAN_POINT('Ctrl Pts',(-18.3165356559975,12.9578107654655,122.804832679751)) ;
#16651 = CARTESIAN_POINT('Ctrl Pts',(-18.3165015779855,12.9578075450074,122.804894033737)) ;
#16652 = CARTESIAN_POINT('Ctrl Pts',(-18.3164844920787,12.957805930232,122.804924798231)) ;
#16653 = CARTESIAN_POINT('Ctrl Pts',(-18.3164502243585,12.9578026913883,122.804986506045)) ;
#16654 = CARTESIAN_POINT('Ctrl Pts',(-18.3164330426506,12.9578010673286,122.80501744921)) ;
#16655 = CARTESIAN_POINT('Ctrl Pts',(-18.3163985817227,12.9577978097606,122.805079517366)) ;
#16656 = CARTESIAN_POINT('Ctrl Pts',(-18.3163813023888,12.9577961762401,122.805110642597)) ;
#16657 = CARTESIAN_POINT('Ctrl Pts',(-18.3163466437754,12.9577928995163,122.805173079376)) ;
#16658 = CARTESIAN_POINT('Ctrl Pts',(-18.3163292646603,12.9577912563271,122.805204390666)) ;
#16659 = CARTESIAN_POINT('Ctrl Pts',(-18.3162944045629,12.95778796008,122.805267203136)) ;
#16660 = CARTESIAN_POINT('Ctrl Pts',(-18.3162769236473,12.9577863070269,122.805298704235)) ;
#16661 = CARTESIAN_POINT('Ctrl Pts',(-18.3162418576804,12.9577829908332,122.805361900527)) ;
#16662 = CARTESIAN_POINT('Ctrl Pts',(-18.3162242727583,12.9577813277032,122.805393595527)) ;
#16663 = CARTESIAN_POINT('Ctrl Pts',(-18.316188996903,12.9577779911739,122.805457183121)) ;
#16664 = CARTESIAN_POINT('Ctrl Pts',(-18.3161713058894,12.9577763177654,122.8054890759)) ;
#16665 = CARTESIAN_POINT('Ctrl Pts',(-18.31613581567,12.957772960468,122.805553063104)) ;
#16666 = CARTESIAN_POINT('Ctrl Pts',(-18.3161180164072,12.9577712765722,122.805585157674)) ;
#16667 = CARTESIAN_POINT('Ctrl Pts',(-18.3160823071395,12.9577678980544,122.805649553184)) ;
#16668 = CARTESIAN_POINT('Ctrl Pts',(-18.316064397259,12.9577662034425,122.805681853942)) ;
#16669 = CARTESIAN_POINT('Ctrl Pts',(-18.3160324290167,12.95776317842,122.805739515208)) ;
#16670 = CARTESIAN_POINT('Ctrl Pts',(-18.3160183700517,12.9577618480006,122.805764875509)) ;
#16671 = CARTESIAN_POINT('Ctrl Pts',(-18.3159899011619,12.9577591537927,122.805816233405)) ;
#16672 = CARTESIAN_POINT('Ctrl Pts',(-18.3159754912136,12.957757789998,122.805842231148)) ;
#16673 = CARTESIAN_POINT('Ctrl Pts',(-18.3159463075245,12.957755027813,122.8058948874)) ;
#16674 = CARTESIAN_POINT('Ctrl Pts',(-18.3159315339375,12.9577536294331,122.805921545745)) ;
#16675 = CARTESIAN_POINT('Ctrl Pts',(-18.3159016099104,12.9577507968285,122.805975547108)) ;
#16676 = CARTESIAN_POINT('Ctrl Pts',(-18.3158864595222,12.9577493626044,122.806002890153)) ;
#16677 = CARTESIAN_POINT('Ctrl Pts',(-18.3158557680647,12.9577464569889,122.806058286236)) ;
#16678 = CARTESIAN_POINT('Ctrl Pts',(-18.3158402270104,12.9577449855942,122.806086339374)) ;
#16679 = CARTESIAN_POINT('Ctrl Pts',(-18.3158087398723,12.9577420042647,122.806143181929)) ;
#16680 = CARTESIAN_POINT('Ctrl Pts',(-18.3157927937014,12.9577404943166,122.806171971638)) ;
#16681 = CARTESIAN_POINT('Ctrl Pts',(-18.3157604808174,12.9577374343961,122.806230315753)) ;
#16682 = CARTESIAN_POINT('Ctrl Pts',(-18.3157441142046,12.9577358844277,122.806259870121)) ;
#16683 = CARTESIAN_POINT('Ctrl Pts',(-18.3157109441543,12.9577327429083,122.806319773394)) ;
#16684 = CARTESIAN_POINT('Ctrl Pts',(-18.3156941409143,12.9577311513702,122.806350122095)) ;
#16685 = CARTESIAN_POINT('Ctrl Pts',(-18.3156600808917,12.9577279251104,122.806411644695)) ;
#16686 = CARTESIAN_POINT('Ctrl Pts',(-18.3156428241278,12.9577262903843,122.806442818723)) ;
#16687 = CARTESIAN_POINT('Ctrl Pts',(-18.3156078393083,12.9577229760484,122.806506024537)) ;
#16688 = CARTESIAN_POINT('Ctrl Pts',(-18.3155901112489,12.9577212964318,122.806538056505)) ;
#16689 = CARTESIAN_POINT('Ctrl Pts',(-18.3155541645785,12.9577178904702,122.806603013531)) ;
#16690 = CARTESIAN_POINT('Ctrl Pts',(-18.315535946212,12.9577161641414,122.806635938334)) ;
#16691 = CARTESIAN_POINT('Ctrl Pts',(-18.3154989995035,12.9577126628936,122.806702716702)) ;
#16692 = CARTESIAN_POINT('Ctrl Pts',(-18.3154802711214,12.9577108879633,122.80673657054)) ;
#16693 = CARTESIAN_POINT('Ctrl Pts',(-18.3154422829925,12.9577072874628,122.806805246248)) ;
#16694 = CARTESIAN_POINT('Ctrl Pts',(-18.3154230234525,12.957705461904,122.806840067961)) ;
#16695 = CARTESIAN_POINT('Ctrl Pts',(-18.315383951108,12.9577017580462,122.806910719666)) ;
#16696 = CARTESIAN_POINT('Ctrl Pts',(-18.3153641383384,12.9576998797418,122.806946549827)) ;
#16697 = CARTESIAN_POINT('Ctrl Pts',(-18.3153239356422,12.9576960681015,122.807019262336)) ;
#16698 = CARTESIAN_POINT('Ctrl Pts',(-18.3153035459935,12.9576941347826,122.807056144429)) ;
#16699 = CARTESIAN_POINT('Ctrl Pts',(-18.3152621649308,12.9576902107518,122.807131006068)) ;
#16700 = CARTESIAN_POINT('Ctrl Pts',(-18.3152411735959,12.9576882200374,122.807168985737)) ;
#16701 = CARTESIAN_POINT('Ctrl Pts',(-18.3151985626186,12.9576841786682,122.807246091354)) ;
#16702 = CARTESIAN_POINT('Ctrl Pts',(-18.3151769431235,12.9576821280167,122.807285217323)) ;
#16703 = CARTESIAN_POINT('Ctrl Pts',(-18.3151330481096,12.9576779641117,122.80736466657)) ;
#16704 = CARTESIAN_POINT('Ctrl Pts',(-18.3151107725755,12.9576758508452,122.807404990183)) ;
#16705 = CARTESIAN_POINT('Ctrl Pts',(-18.3150655353323,12.957671558815,122.807486890234)) ;
#16706 = CARTESIAN_POINT('Ctrl Pts',(-18.3150425738581,12.957669380061,122.807528466577)) ;
#16707 = CARTESIAN_POINT('Ctrl Pts',(-18.3149959333314,12.9576649540381,122.807612929959)) ;
#16708 = CARTESIAN_POINT('Ctrl Pts',(-18.314972254352,12.9576627067626,122.807655817222)) ;
#16709 = CARTESIAN_POINT('Ctrl Pts',(-18.3149241449129,12.9576581404384,122.807742964933)) ;
#16710 = CARTESIAN_POINT('Ctrl Pts',(-18.314899714647,12.9576558213935,122.807787225418)) ;
#16711 = CARTESIAN_POINT('Ctrl Pts',(-18.3148500668834,12.9576511080926,122.807877185519)) ;
#16712 = CARTESIAN_POINT('Ctrl Pts',(-18.3148248494684,12.9576487138287,122.807922885405)) ;
#16713 = CARTESIAN_POINT('Ctrl Pts',(-18.3147735889681,12.9576438463923,122.808015795242)) ;
#16714 = CARTESIAN_POINT('Ctrl Pts',(-18.3147475460057,12.9576413732145,122.808063005424)) ;
#16715 = CARTESIAN_POINT('Ctrl Pts',(-18.314694593362,12.9576363440003,122.808159011647)) ;
#16716 = CARTESIAN_POINT('Ctrl Pts',(-18.3146676839348,12.9576337879696,122.808207807719)) ;
#16717 = CARTESIAN_POINT('Ctrl Pts',(-18.3146129545306,12.95762858883,122.808307066698)) ;
#16718 = CARTESIAN_POINT('Ctrl Pts',(-18.3145851347164,12.9576259457165,122.808357529846)) ;
#16719 = CARTESIAN_POINT('Ctrl Pts',(-18.3145285375267,12.9576205678836,122.808460209882)) ;
#16720 = CARTESIAN_POINT('Ctrl Pts',(-18.3144997604089,12.9576178331669,122.808512426885)) ;
#16721 = CARTESIAN_POINT('Ctrl Pts',(-18.3144411981411,12.9576122672647,122.808618707985)) ;
#16722 = CARTESIAN_POINT('Ctrl Pts',(-18.3144114132964,12.9576094360844,122.808672772163)) ;
#16723 = CARTESIAN_POINT('Ctrl Pts',(-18.3143507814169,12.9576036720343,122.808782847852)) ;
#16724 = CARTESIAN_POINT('Ctrl Pts',(-18.3143199346509,12.9576007391641,122.808838859568)) ;
#16725 = CARTESIAN_POINT('Ctrl Pts',(-18.3142571205621,12.9575947661053,122.808952938428)) ;
#16726 = CARTESIAN_POINT('Ctrl Pts',(-18.3142251536367,12.9575917259261,122.809011005608)) ;
#16727 = CARTESIAN_POINT('Ctrl Pts',(-18.3141600363797,12.9575855321851,122.809129311873)) ;
#16728 = CARTESIAN_POINT('Ctrl Pts',(-18.3141268863937,12.9575823786251,122.809189551159)) ;
#16729 = CARTESIAN_POINT('Ctrl Pts',(-18.3140593351694,12.957575951573,122.809312327458)) ;
#16730 = CARTESIAN_POINT('Ctrl Pts',(-18.3140249342908,12.9575726780808,122.809374864729)) ;
#16731 = CARTESIAN_POINT('Ctrl Pts',(-18.3104970887637,12.9572369292352,122.815789427175)) ;
#16732 = CARTESIAN_POINT('Ctrl Pts',(-18.3070589554122,12.956904803191,122.822171731532)) ;
#16733 = CARTESIAN_POINT('Ctrl Pts',(-18.2961610813973,12.9558355002876,122.842830179727)) ;
#16734 = CARTESIAN_POINT('Ctrl Pts',(-18.2889216865892,12.9550993590262,122.857220735031)) ;
#16735 = CARTESIAN_POINT('Ctrl Pts',(-18.27147266284,12.9532542762629,122.893642974524)) ;
#16736 = CARTESIAN_POINT('Ctrl Pts',(-18.2616230735756,12.9521459955161,122.915839710725)) ;
#16737 = CARTESIAN_POINT('Ctrl Pts',(-18.2459725991599,12.950257428141,122.95407622725)) ;
#16738 = CARTESIAN_POINT('Ctrl Pts',(-18.2398420577145,12.9494781401921,122.969973552403)) ;
#16739 = CARTESIAN_POINT('Ctrl Pts',(-18.2295216232024,12.948090626654,122.998457026655)) ;
#16740 = CARTESIAN_POINT('Ctrl Pts',(-18.2252034973743,12.947482880953,123.010993933247)) ;
#16741 = CARTESIAN_POINT('Ctrl Pts',(-18.2142783325241,12.9458689441818,123.044431744035)) ;
#16742 = CARTESIAN_POINT('Ctrl Pts',(-18.2080202126451,12.9448619942941,123.0654417458)) ;
#16743 = CARTESIAN_POINT('Ctrl Pts',(-18.1943463949412,12.9424452373669,123.116189647364)) ;
#16744 = CARTESIAN_POINT('Ctrl Pts',(-18.1874654466672,12.941035227401,123.146057058026)) ;
#16745 = CARTESIAN_POINT('Ctrl Pts',(-18.1816683493887,12.9396231975372,123.176253950506)) ;
#16746 = CARTESIAN_POINT('Ctrl Pts',(-18.1816478436446,12.9396181994907,123.176360839662)) ;
#16747 = CARTESIAN_POINT('Ctrl Pts',(-18.1816080473459,12.9396084930705,123.176568430149)) ;
#16748 = CARTESIAN_POINT('Ctrl Pts',(-18.1815887552277,12.9396037846932,123.176669131141)) ;
#16749 = CARTESIAN_POINT('Ctrl Pts',(-18.1815512981532,12.9395946372377,123.176864779826)) ;
#16750 = CARTESIAN_POINT('Ctrl Pts',(-18.1815331318249,12.9395901981559,123.176959727234)) ;
#16751 = CARTESIAN_POINT('Ctrl Pts',(-18.1814978459639,12.9395815706274,123.177144266888)) ;
#16752 = CARTESIAN_POINT('Ctrl Pts',(-18.1814807252205,12.939577382176,123.177233858916)) ;
#16753 = CARTESIAN_POINT('Ctrl Pts',(-18.181447457043,12.9395692387868,123.177408053108)) ;
#16754 = CARTESIAN_POINT('Ctrl Pts',(-18.1814313085426,12.9395652838446,123.177492655087)) ;
#16755 = CARTESIAN_POINT('Ctrl Pts',(-18.1813999175518,12.9395575917456,123.177657204805)) ;
#16756 = CARTESIAN_POINT('Ctrl Pts',(-18.1813846741313,12.9395538545871,123.177737152332)) ;
#16757 = CARTESIAN_POINT('Ctrl Pts',(-18.1813550316109,12.9395465835969,123.17789270173)) ;
#16758 = CARTESIAN_POINT('Ctrl Pts',(-18.1813406316666,12.9395430497578,123.177968303538)) ;
#16759 = CARTESIAN_POINT('Ctrl Pts',(-18.1813126194362,12.9395361720888,123.178115445765)) ;
#16760 = CARTESIAN_POINT('Ctrl Pts',(-18.1812990064273,12.9395328282582,123.178186986005)) ;
#16761 = CARTESIAN_POINT('Ctrl Pts',(-18.1812725159887,12.9395263183341,123.178326267087)) ;
#16762 = CARTESIAN_POINT('Ctrl Pts',(-18.1812596379002,12.9395231522354,123.178394007869)) ;
#16763 = CARTESIAN_POINT('Ctrl Pts',(-18.1812345693507,12.9395169864471,123.178525931897)) ;
#16764 = CARTESIAN_POINT('Ctrl Pts',(-18.1812223783251,12.9395139867577,123.178590114987)) ;
#16765 = CARTESIAN_POINT('Ctrl Pts',(-18.1811986397071,12.9395081433232,123.1787151471)) ;
#16766 = CARTESIAN_POINT('Ctrl Pts',(-18.1811870916137,12.9395052995784,123.178775995981)) ;
#16767 = CARTESIAN_POINT('Ctrl Pts',(-18.1811645981009,12.9394997583599,123.178894566255)) ;
#16768 = CARTESIAN_POINT('Ctrl Pts',(-18.1811536522131,12.9394970608809,123.178952287643)) ;
#16769 = CARTESIAN_POINT('Ctrl Pts',(-18.1811323254288,12.9394918032316,123.179064794358)) ;
#16770 = CARTESIAN_POINT('Ctrl Pts',(-18.181121944146,12.9394892430643,123.179119579517)) ;
#16771 = CARTESIAN_POINT('Ctrl Pts',(-18.1810892024377,12.939481165697,123.17929243061)) ;
#16772 = CARTESIAN_POINT('Ctrl Pts',(-18.1810668553675,12.9394756485441,123.179410499093)) ;
#16773 = CARTESIAN_POINT('Ctrl Pts',(-18.181022666351,12.9394647307492,123.179644151669)) ;
#16774 = CARTESIAN_POINT('Ctrl Pts',(-18.181000823699,12.9394593301059,123.179759735601)) ;
#16775 = CARTESIAN_POINT('Ctrl Pts',(-18.1809576226227,12.9394486406781,123.179988518082)) ;
#16776 = CARTESIAN_POINT('Ctrl Pts',(-18.1809362635275,12.9394433518906,123.180101716519)) ;
#16777 = CARTESIAN_POINT('Ctrl Pts',(-18.1808940096477,12.9394328817271,123.180325822676)) ;
#16778 = CARTESIAN_POINT('Ctrl Pts',(-18.1808731141226,12.9394277003212,123.180436730871)) ;
#16779 = CARTESIAN_POINT('Ctrl Pts',(-18.1794581206302,12.9390765796052,123.187952755114)) ;
#16780 = CARTESIAN_POINT('Ctrl Pts',(-18.1781309923844,12.9387308918906,123.195370336562)) ;
#16781 = CARTESIAN_POINT('Ctrl Pts',(-18.1757657578108,12.9380826164572,123.209316318956)) ;
#16782 = CARTESIAN_POINT('Ctrl Pts',(-18.1747122112557,12.9377799831221,123.21584182609)) ;
#16783 = CARTESIAN_POINT('Ctrl Pts',(-18.1717069603954,12.9368728810166,123.235442720272)) ;
#16784 = CARTESIAN_POINT('Ctrl Pts',(-18.1699108725588,12.9362692023525,123.248541032574)) ;
#16785 = CARTESIAN_POINT('Ctrl Pts',(-18.1649658156275,12.9343905396532,123.289410877513)) ;
#16786 = CARTESIAN_POINT('Ctrl Pts',(-18.1625402001211,12.9331172882892,123.317261138592)) ;
#16787 = CARTESIAN_POINT('Ctrl Pts',(-18.1603588706949,12.9312498209466,123.358116088442)) ;
#16788 = CARTESIAN_POINT('Ctrl Pts',(-18.1598690864403,12.930657652216,123.37107289146)) ;
#16789 = CARTESIAN_POINT('Ctrl Pts',(-18.1593242379878,12.9295366741171,123.395583561866)) ;
#16790 = CARTESIAN_POINT('Ctrl Pts',(-18.1592276205016,12.9290080527271,123.40713516286)) ;
#16791 = CARTESIAN_POINT('Ctrl Pts',(-18.1593138238008,12.9282897303717,123.422814981604)) ;
#16792 = CARTESIAN_POINT('Ctrl Pts',(-18.1593569757214,12.92810052608,123.426943405856)) ;
#16793 = CARTESIAN_POINT('Ctrl Pts',(-18.1595960598034,12.9273890608911,123.442460723563)) ;
#16794 = CARTESIAN_POINT('Ctrl Pts',(-18.159927205597,12.9268663684156,123.453846955133)) ;
#16795 = CARTESIAN_POINT('Ctrl Pts',(-18.161235129003,12.9254604078605,123.48442791674)) ;
#16796 = CARTESIAN_POINT('Ctrl Pts',(-18.1624990362419,12.9245763576782,123.503607245375)) ;
#16797 = CARTESIAN_POINT('Ctrl Pts',(-18.1664096371934,12.9225474469302,123.547497327835)) ;
#16798 = CARTESIAN_POINT('Ctrl Pts',(-18.1693519972108,12.9214024106477,123.572173672582)) ;
#16799 = CARTESIAN_POINT('Ctrl Pts',(-18.1739785388711,12.9199629074833,123.603101533229)) ;
#16800 = CARTESIAN_POINT('Ctrl Pts',(-18.1749782874093,12.9196672107574,123.60944975546)) ;
#16801 = CARTESIAN_POINT('Ctrl Pts',(-18.1774139353592,12.9189808291118,123.624175786378)) ;
#16802 = CARTESIAN_POINT('Ctrl Pts',(-18.1788864237521,12.9185902941876,123.632547234821)) ;
#16803 = CARTESIAN_POINT('Ctrl Pts',(-18.1804477772138,12.9181993395347,123.640922310696)) ;
#16804 = CARTESIAN_POINT('Ctrl Pts',(-18.1804513722318,12.9181984394775,123.640941591798)) ;
#16805 = CARTESIAN_POINT('Ctrl Pts',(-18.1804585570762,12.918196640895,123.640980121126)) ;
#16806 = CARTESIAN_POINT('Ctrl Pts',(-18.1804621468857,12.9181957423737,123.640999369269)) ;
#16807 = CARTESIAN_POINT('Ctrl Pts',(-18.1804693213972,12.9181939468408,123.641037833157)) ;
#16808 = CARTESIAN_POINT('Ctrl Pts',(-18.1804729061151,12.9181930498249,123.641057048993)) ;
#16809 = CARTESIAN_POINT('Ctrl Pts',(-18.1804800705661,12.9181912572712,123.64109544895)) ;
#16810 = CARTESIAN_POINT('Ctrl Pts',(-18.1804836502603,12.9181903617427,123.641114632869)) ;
#16811 = CARTESIAN_POINT('Ctrl Pts',(-18.1804908047521,12.9181885721404,123.641152969487)) ;
#16812 = CARTESIAN_POINT('Ctrl Pts',(-18.1804943795522,12.9181876780656,123.641172122208)) ;
#16813 = CARTESIAN_POINT('Ctrl Pts',(-18.1805015243192,12.9181858913539,123.641210396793)) ;
#16814 = CARTESIAN_POINT('Ctrl Pts',(-18.1805050943191,12.9181849987084,123.641229518842)) ;
#16815 = CARTESIAN_POINT('Ctrl Pts',(-18.1805122296001,12.9181832148254,123.64126773272)) ;
#16816 = CARTESIAN_POINT('Ctrl Pts',(-18.1805157948734,12.9181823235896,123.641286824515)) ;
#16817 = CARTESIAN_POINT('Ctrl Pts',(-18.1805229208078,12.9181805424983,123.641324978479)) ;
#16818 = CARTESIAN_POINT('Ctrl Pts',(-18.1805264814681,12.9181796526427,123.641344040652)) ;
#16819 = CARTESIAN_POINT('Ctrl Pts',(-18.1805335982779,12.9181778742855,123.641382135936)) ;
#16820 = CARTESIAN_POINT('Ctrl Pts',(-18.180537154418,12.918176985786,123.641401169006)) ;
#16821 = CARTESIAN_POINT('Ctrl Pts',(-18.1805442622957,12.9181752101128,123.641439206686)) ;
#16822 = CARTESIAN_POINT('Ctrl Pts',(-18.1805478140121,12.9181743229441,123.641458211191)) ;
#16823 = CARTESIAN_POINT('Ctrl Pts',(-18.1805549131316,12.9181725499094,123.641496192242)) ;
#16824 = CARTESIAN_POINT('Ctrl Pts',(-18.1805584605333,12.9181716640434,123.641515168787)) ;
#16825 = CARTESIAN_POINT('Ctrl Pts',(-18.1805655510948,12.9181698935952,123.641553094322)) ;
#16826 = CARTESIAN_POINT('Ctrl Pts',(-18.1805690942831,12.9181690090056,123.641572043471)) ;
#16827 = CARTESIAN_POINT('Ctrl Pts',(-18.1805761765045,12.9181672410876,123.641609914697)) ;
#16828 = CARTESIAN_POINT('Ctrl Pts',(-18.1805797155685,12.9181663577511,123.641628836947)) ;
#16829 = CARTESIAN_POINT('Ctrl Pts',(-18.1805867897101,12.9181645922965,123.641666655297)) ;
#16830 = CARTESIAN_POINT('Ctrl Pts',(-18.1805903247121,12.9181637101967,123.641685551001)) ;
#16831 = CARTESIAN_POINT('Ctrl Pts',(-18.1805973908086,12.9181619471949,123.641723316701)) ;
#16832 = CARTESIAN_POINT('Ctrl Pts',(-18.1806009219106,12.9181610662905,123.641742186745)) ;
#16833 = CARTESIAN_POINT('Ctrl Pts',(-18.1806079802736,12.9181593056619,123.641779901501)) ;
#16834 = CARTESIAN_POINT('Ctrl Pts',(-18.180611507549,12.9181584259337,123.641798746296)) ;
#16835 = CARTESIAN_POINT('Ctrl Pts',(-18.180618558347,12.9181566676345,123.641836411045)) ;
#16836 = CARTESIAN_POINT('Ctrl Pts',(-18.1806220818969,12.9181557890565,123.641855231151)) ;
#16837 = CARTESIAN_POINT('Ctrl Pts',(-18.1806291253781,12.9181540330231,123.641892847257)) ;
#16838 = CARTESIAN_POINT('Ctrl Pts',(-18.1806326452775,12.9181531555755,123.641911643092)) ;
#16839 = CARTESIAN_POINT('Ctrl Pts',(-18.1809539616441,12.9180730672334,123.643627215908)) ;
#16840 = CARTESIAN_POINT('Ctrl Pts',(-18.1812752722338,12.9179938774841,123.645323332608)) ;
#16841 = CARTESIAN_POINT('Ctrl Pts',(-18.1816065659832,12.9179131305516,123.647052552315)) ;
#16842 = CARTESIAN_POINT('Ctrl Pts',(-18.1816130377265,12.9179115535273,123.647086324663)) ;
#16843 = CARTESIAN_POINT('Ctrl Pts',(-18.182969480035,12.9175810906054,123.654163245793)) ;
#16844 = CARTESIAN_POINT('Ctrl Pts',(-18.1843800374522,12.9172525519745,123.661194660238)) ;
#16845 = CARTESIAN_POINT('Ctrl Pts',(-18.1890235626927,12.9162161904394,123.683351466648)) ;
#16846 = CARTESIAN_POINT('Ctrl Pts',(-18.1924767942197,12.9155093084493,123.698429223739)) ;
#16847 = CARTESIAN_POINT('Ctrl Pts',(-18.2018417324611,12.9137361373218,123.736092797363)) ;
#16848 = CARTESIAN_POINT('Ctrl Pts',(-18.2081079994041,12.9126704373141,123.758584315276)) ;
#16849 = CARTESIAN_POINT('Ctrl Pts',(-18.2189372055151,12.9109937672517,123.793626229474)) ;
#16850 = CARTESIAN_POINT('Ctrl Pts',(-18.2230776127245,12.9103838947887,123.806301499499)) ;
#16851 = CARTESIAN_POINT('Ctrl Pts',(-18.2316673068012,12.9091763649064,123.831238630323)) ;
#16852 = CARTESIAN_POINT('Ctrl Pts',(-18.2361073175613,12.9085788070171,123.843501933227)) ;
#16853 = CARTESIAN_POINT('Ctrl Pts',(-18.2452420675944,12.9073990018184,123.867549616553)) ;
#16854 = CARTESIAN_POINT('Ctrl Pts',(-18.2499259084114,12.9068168544759,123.879336497236)) ;
#16855 = CARTESIAN_POINT('Ctrl Pts',(-18.2620303679774,12.9053665360661,123.908496272049)) ;
#16856 = CARTESIAN_POINT('Ctrl Pts',(-18.2696669653528,12.9044979794044,123.925776081124)) ;
#16857 = CARTESIAN_POINT('Ctrl Pts',(-18.2788860231544,12.903499878364,123.945419938184)) ;
#16858 = CARTESIAN_POINT('Ctrl Pts',(-18.2800884222473,12.9033706262114,123.947959692957)) ;
#16859 = CARTESIAN_POINT('Ctrl Pts',(-18.2851283176188,12.9028326886442,123.958512998435)) ;
#16860 = CARTESIAN_POINT('Ctrl Pts',(-18.2890426365442,12.9024240169746,123.966489575971)) ;
#16861 = CARTESIAN_POINT('Ctrl Pts',(-18.2994759865159,12.9013581159805,123.987189593902)) ;
#16862 = CARTESIAN_POINT('Ctrl Pts',(-18.3061288452239,12.900701145255,123.999844152114)) ;
#16863 = CARTESIAN_POINT('Ctrl Pts',(-18.3162308743147,12.8997362908999,124.018284380569)) ;
#16864 = CARTESIAN_POINT('Ctrl Pts',(-18.3195120663737,12.8994276798789,124.024160730369)) ;
#16865 = CARTESIAN_POINT('Ctrl Pts',(-18.3228570573256,12.899117844315,124.030039293946)) ;
#16866 = CARTESIAN_POINT('Ctrl Pts',(-18.3228735541318,12.8991163163849,124.030068283111)) ;
#16867 = CARTESIAN_POINT('Ctrl Pts',(-18.32290637926,12.8991132763587,124.03012596)) ;
#16868 = CARTESIAN_POINT('Ctrl Pts',(-18.3229227074044,12.8991117642766,124.030154647467)) ;
#16869 = CARTESIAN_POINT('Ctrl Pts',(-18.3229551986617,12.8991087556196,124.030211727194)) ;
#16870 = CARTESIAN_POINT('Ctrl Pts',(-18.3229713620229,12.8991072590194,124.030240119942)) ;
#16871 = CARTESIAN_POINT('Ctrl Pts',(-18.3230035273146,12.8991042809858,124.030296616717)) ;
#16872 = CARTESIAN_POINT('Ctrl Pts',(-18.323019529296,12.8991027995455,124.030324720885)) ;
#16873 = CARTESIAN_POINT('Ctrl Pts',(-18.323051375567,12.8990998514791,124.030380647219)) ;
#16874 = CARTESIAN_POINT('Ctrl Pts',(-18.3230672196567,12.8990983848692,124.030408469085)) ;
#16875 = CARTESIAN_POINT('Ctrl Pts',(-18.3230987535156,12.8990954661453,124.030463836887)) ;
#16876 = CARTESIAN_POINT('Ctrl Pts',(-18.323114443261,12.8990940140312,124.030491382829)) ;
#16877 = CARTESIAN_POINT('Ctrl Pts',(-18.3231456716406,12.8990911239955,124.030546204565)) ;
#16878 = CARTESIAN_POINT('Ctrl Pts',(-18.3231612103119,12.8990896860685,124.03057348047)) ;
#16879 = CARTESIAN_POINT('Ctrl Pts',(-18.3231921396949,12.899086824109,124.030627767804)) ;
#16880 = CARTESIAN_POINT('Ctrl Pts',(-18.3232075305103,12.8990854000651,124.03065477946)) ;
#16881 = CARTESIAN_POINT('Ctrl Pts',(-18.3245493294304,12.8989612580724,124.033009499938)) ;
#16882 = CARTESIAN_POINT('Ctrl Pts',(-18.3258832176993,12.8988385899037,124.035332941119)) ;
#16883 = CARTESIAN_POINT('Ctrl Pts',(-18.3298950327256,12.8984718678071,124.042269204339)) ;
#16884 = CARTESIAN_POINT('Ctrl Pts',(-18.3325950296598,12.8982279842675,124.046869201278)) ;
#16885 = CARTESIAN_POINT('Ctrl Pts',(-18.3388262284224,12.8976717668316,124.057331350921)) ;
#16886 = CARTESIAN_POINT('Ctrl Pts',(-18.3423762941214,12.8973595810617,124.063182067527)) ;
#16887 = CARTESIAN_POINT('Ctrl Pts',(-18.354025380079,12.8963497021812,124.08202969001)) ;
#16888 = CARTESIAN_POINT('Ctrl Pts',(-18.3623152447091,12.8956531781392,124.094907015862)) ;
#16889 = CARTESIAN_POINT('Ctrl Pts',(-18.3914065642736,12.8932768979946,124.138322865386)) ;
#16890 = CARTESIAN_POINT('Ctrl Pts',(-18.4133241694576,12.8915987489053,124.168089815719)) ;
#16891 = CARTESIAN_POINT('Ctrl Pts',(-18.4418758265974,12.8895228903143,124.203468773847)) ;
#16892 = CARTESIAN_POINT('Ctrl Pts',(-18.4472912978354,12.8891336910807,124.210040642423)) ;
#16893 = CARTESIAN_POINT('Ctrl Pts',(-18.4572290045737,12.8884273879469,124.221852379309)) ;
#16894 = CARTESIAN_POINT('Ctrl Pts',(-18.4617284192692,12.8881104450006,124.227111006818)) ;
#16895 = CARTESIAN_POINT('Ctrl Pts',(-18.4666832069913,12.887764441578,124.232805424004)) ;
#16896 = CARTESIAN_POINT('Ctrl Pts',(-18.467095506948,12.8877356723225,124.233278550346)) ;
#16897 = CARTESIAN_POINT('Ctrl Pts',(-18.4675648714596,12.8877029468146,124.233816341727)) ;
#16898 = CARTESIAN_POINT('Ctrl Pts',(-18.4676215866458,12.8876989928851,124.233881311632)) ;
#16899 = CARTESIAN_POINT('Ctrl Pts',(-18.4677318916404,12.8876913037381,124.234007644781)) ;
#16900 = CARTESIAN_POINT('Ctrl Pts',(-18.4677854810087,12.8876875685056,124.234069008982)) ;
#16901 = CARTESIAN_POINT('Ctrl Pts',(-18.4678889337335,12.8876803584776,124.234187447423)) ;
#16902 = CARTESIAN_POINT('Ctrl Pts',(-18.4679387961866,12.887676883694,124.234244522259)) ;
#16903 = CARTESIAN_POINT('Ctrl Pts',(-18.4680349418722,12.8876701841842,124.234354554794)) ;
#16904 = CARTESIAN_POINT('Ctrl Pts',(-18.4680812244232,12.8876669594601,124.234407513167)) ;
#16905 = CARTESIAN_POINT('Ctrl Pts',(-18.4681703672058,12.8876607490035,124.234509496583)) ;
#16906 = CARTESIAN_POINT('Ctrl Pts',(-18.4682132266936,12.8876577632826,124.234558522063)) ;
#16907 = CARTESIAN_POINT('Ctrl Pts',(-18.468295687275,12.8876520192948,124.234652830986)) ;
#16908 = CARTESIAN_POINT('Ctrl Pts',(-18.4683352878139,12.8876492610311,124.234698114928)) ;
#16909 = CARTESIAN_POINT('Ctrl Pts',(-18.468411399551,12.8876439600789,124.234785137415)) ;
#16910 = CARTESIAN_POINT('Ctrl Pts',(-18.4684479103416,12.8876414173877,124.234826876486)) ;
#16911 = CARTESIAN_POINT('Ctrl Pts',(-18.4685180147853,12.8876365354972,124.234907009001)) ;
#16912 = CARTESIAN_POINT('Ctrl Pts',(-18.4685516080128,12.8876341963005,124.234945402819)) ;
#16913 = CARTESIAN_POINT('Ctrl Pts',(-18.4686160507956,12.8876297092412,124.235019045605)) ;
#16914 = CARTESIAN_POINT('Ctrl Pts',(-18.4686468998015,12.8876275613936,124.235054294689)) ;
#16915 = CARTESIAN_POINT('Ctrl Pts',(-18.4687060259814,12.8876234450001,124.235121846536)) ;
#16916 = CARTESIAN_POINT('Ctrl Pts',(-18.4687343029867,12.8876214764459,124.235154149746)) ;
#16917 = CARTESIAN_POINT('Ctrl Pts',(-18.468790884058,12.8876175376635,124.235218780361)) ;
#16918 = CARTESIAN_POINT('Ctrl Pts',(-18.4688191884352,12.8876155674136,124.235251108115)) ;
#16919 = CARTESIAN_POINT('Ctrl Pts',(-18.4688752008435,12.8876116686328,124.235315075854)) ;
#16920 = CARTESIAN_POINT('Ctrl Pts',(-18.4689029109598,12.8876097399525,124.235346718361)) ;
#16921 = CARTESIAN_POINT('Ctrl Pts',(-18.4689577443706,12.8876059236345,124.2354093269)) ;
#16922 = CARTESIAN_POINT('Ctrl Pts',(-18.4689848653394,12.8876040361545,124.235440290412)) ;
#16923 = CARTESIAN_POINT('Ctrl Pts',(-18.4690385145869,12.8876003026333,124.23550153467)) ;
#16924 = CARTESIAN_POINT('Ctrl Pts',(-18.4690650454101,12.8875984564108,124.235531818454)) ;
#16925 = CARTESIAN_POINT('Ctrl Pts',(-18.4691175258074,12.8875948045957,124.235591716712)) ;
#16926 = CARTESIAN_POINT('Ctrl Pts',(-18.4691434722948,12.8875929992139,124.235621327792)) ;
#16927 = CARTESIAN_POINT('Ctrl Pts',(-18.4699224641026,12.8875387988499,124.236510257003)) ;
#16928 = CARTESIAN_POINT('Ctrl Pts',(-18.4706766859725,12.8874863960561,124.237368543549)) ;
#16929 = CARTESIAN_POINT('Ctrl Pts',(-18.4757060554748,12.8871374506776,124.243076045287)) ;
#16930 = CARTESIAN_POINT('Ctrl Pts',(-18.4800175818452,12.8868406696014,124.247893058657)) ;
#16931 = CARTESIAN_POINT('Ctrl Pts',(-18.4898500289464,12.8861690840557,124.258708256137)) ;
#16932 = CARTESIAN_POINT('Ctrl Pts',(-18.4953926474036,12.8857941488287,124.264686310065)) ;
#16933 = CARTESIAN_POINT('Ctrl Pts',(-18.5101231320875,12.8848070781492,124.280265561429)) ;
#16934 = CARTESIAN_POINT('Ctrl Pts',(-18.5194062998423,12.8841944007577,124.289775187233)) ;
#16935 = CARTESIAN_POINT('Ctrl Pts',(-18.5550983049626,12.8818736011182,124.32519014002)) ;
#16936 = CARTESIAN_POINT('Ctrl Pts',(-18.5825009328651,12.880161273313,124.350066794169)) ;
#16937 = CARTESIAN_POINT('Ctrl Pts',(-18.6212524488809,12.8778392074262,124.382228452977)) ;
#16938 = CARTESIAN_POINT('Ctrl Pts',(-18.6316748627251,12.877224095369,124.390599843998)) ;
#16939 = CARTESIAN_POINT('Ctrl Pts',(-18.6524795894873,12.8760131830291,124.406768339183)) ;
#16940 = CARTESIAN_POINT('Ctrl Pts',(-18.6628530867348,12.8754173924744,124.414574044891)) ;
#16941 = CARTESIAN_POINT('Ctrl Pts',(-18.7467658024364,12.8706560174457,124.475691817207)) ;
#16942 = CARTESIAN_POINT('Ctrl Pts',(-18.8257959080712,12.866506260928,124.521005702758)) ;
#16943 = CARTESIAN_POINT('Ctrl Pts',(-18.9215326984024,12.8617196442192,124.562812243808)) ;
#16944 = CARTESIAN_POINT('Ctrl Pts',(-18.9341186520534,12.8610952313076,124.56806479059)) ;
#16945 = CARTESIAN_POINT('Ctrl Pts',(-18.9585064594863,12.8598946991652,124.577777194201)) ;
#16946 = CARTESIAN_POINT('Ctrl Pts',(-18.9702948770285,12.8593185422153,124.582266407866)) ;
#16947 = CARTESIAN_POINT('Ctrl Pts',(-18.9933300089094,12.8582009555687,124.590641579749)) ;
#16948 = CARTESIAN_POINT('Ctrl Pts',(-19.0045682200008,12.8576596143712,124.594546878756)) ;
#16949 = CARTESIAN_POINT('Ctrl Pts',(-19.0547419910352,12.8552571323346,124.611183486482)) ;
#16950 = CARTESIAN_POINT('Ctrl Pts',(-19.0942336129539,12.8534025960457,124.622156733051)) ;
#16951 = CARTESIAN_POINT('Ctrl Pts',(-19.147482036072,12.8509166562023,124.634169261791)) ;
#16952 = CARTESIAN_POINT('Ctrl Pts',(-19.1608195927546,12.8502952981591,124.636949820319)) ;
#16953 = CARTESIAN_POINT('Ctrl Pts',(-19.1812816780191,12.8493431719853,124.640867781224)) ;
#16954 = CARTESIAN_POINT('Ctrl Pts',(-19.1883750582263,12.8490133199613,124.642162458373)) ;
#16955 = CARTESIAN_POINT('Ctrl Pts',(-19.1993763911068,12.8485019728867,124.644072204825)) ;
#16956 = CARTESIAN_POINT('Ctrl Pts',(-19.203276739423,12.8483207277948,124.644730219724)) ;
#16957 = CARTESIAN_POINT('Ctrl Pts',(-19.2073727034653,12.848130430802,124.645401257275)) ;
#16958 = CARTESIAN_POINT('Ctrl Pts',(-19.2075652738395,12.8481214841415,124.64543275958)) ;
#16959 = CARTESIAN_POINT('Ctrl Pts',(-19.2078963833416,12.8481061012184,124.645486845695)) ;
#16960 = CARTESIAN_POINT('Ctrl Pts',(-19.2080349189704,12.848099665076,124.645509451272)) ;
#16961 = CARTESIAN_POINT('Ctrl Pts',(-19.2082911550508,12.8480877608434,124.645551218334)) ;
#16962 = CARTESIAN_POINT('Ctrl Pts',(-19.2084088545248,12.8480822927861,124.645570386326)) ;
#16963 = CARTESIAN_POINT('Ctrl Pts',(-19.2086254579747,12.8480722299281,124.645605629543)) ;
#16964 = CARTESIAN_POINT('Ctrl Pts',(-19.2087243611196,12.8480676351566,124.645621709716)) ;
#16965 = CARTESIAN_POINT('Ctrl Pts',(-19.2089055418012,12.8480592180358,124.645651144626)) ;
#16966 = CARTESIAN_POINT('Ctrl Pts',(-19.2089878186411,12.8480553957119,124.645664503009)) ;
#16967 = CARTESIAN_POINT('Ctrl Pts',(-19.2091379278608,12.8480484221368,124.645688859178)) ;
#16968 = CARTESIAN_POINT('Ctrl Pts',(-19.2092057599288,12.8480452708951,124.645699859618)) ;
#16969 = CARTESIAN_POINT('Ctrl Pts',(-19.2093290753509,12.8480395421093,124.645719847451)) ;
#16970 = CARTESIAN_POINT('Ctrl Pts',(-19.2093845585461,12.848036964569,124.645728836718)) ;
#16971 = CARTESIAN_POINT('Ctrl Pts',(-19.209510775576,12.8480311010172,124.645749277391)) ;
#16972 = CARTESIAN_POINT('Ctrl Pts',(-19.2095815099182,12.8480278149865,124.645760726479)) ;
#16973 = CARTESIAN_POINT('Ctrl Pts',(-19.2097196683629,12.8480213967277,124.645783076665)) ;
#16974 = CARTESIAN_POINT('Ctrl Pts',(-19.2097870922423,12.848018264509,124.6457939783)) ;
#16975 = CARTESIAN_POINT('Ctrl Pts',(-19.2099186765971,12.8480121516952,124.645815242849)) ;
#16976 = CARTESIAN_POINT('Ctrl Pts',(-19.2099828370863,12.8480091710985,124.645825606302)) ;
#16977 = CARTESIAN_POINT('Ctrl Pts',(-19.2101079518054,12.8480033588711,124.645845805308)) ;
#16978 = CARTESIAN_POINT('Ctrl Pts',(-19.2101689056141,12.8480005272591,124.645855641294)) ;
#16979 = CARTESIAN_POINT('Ctrl Pts',(-19.2102876702736,12.8479950100576,124.645874797064)) ;
#16980 = CARTESIAN_POINT('Ctrl Pts',(-19.2103454815312,12.8479923244485,124.645884117381)) ;
#16981 = CARTESIAN_POINT('Ctrl Pts',(-19.2161162292188,12.8477242463938,124.64681405981)) ;
#16982 = CARTESIAN_POINT('Ctrl Pts',(-19.2218354778886,12.8474586336503,124.647695002688)) ;
#16983 = CARTESIAN_POINT('Ctrl Pts',(-19.2345582346726,12.8468678811711,124.649564358063)) ;
#16984 = CARTESIAN_POINT('Ctrl Pts',(-19.2415644276858,12.8465426422506,124.650533105558)) ;
#16985 = CARTESIAN_POINT('Ctrl Pts',(-19.259456908882,12.845712178287,124.652852519616)) ;
#16986 = CARTESIAN_POINT('Ctrl Pts',(-19.2703534272261,12.8452065484907,124.654119438914)) ;
#16987 = CARTESIAN_POINT('Ctrl Pts',(-19.3050349554443,12.8435975211568,124.657689793635)) ;
#16988 = CARTESIAN_POINT('Ctrl Pts',(-19.3288699377701,12.8424920380273,124.659454720743)) ;
#16989 = CARTESIAN_POINT('Ctrl Pts',(-19.3745494290596,12.8403758739273,124.661522700791)) ;
#16990 = CARTESIAN_POINT('Ctrl Pts',(-19.3963803122365,12.8393656325211,124.661938519652)) ;
#16991 = CARTESIAN_POINT('Ctrl Pts',(-19.432945950675,12.837678722305,124.66167703405)) ;
#16992 = CARTESIAN_POINT('Ctrl Pts',(-19.4476780266782,12.837000512866,124.661311117628)) ;
#16993 = CARTESIAN_POINT('Ctrl Pts',(-19.477091111899,12.8356472640861,124.660059860304)) ;
#16994 = CARTESIAN_POINT('Ctrl Pts',(-19.4917698531057,12.8349723267023,124.659175724632)) ;
#16995 = CARTESIAN_POINT('Ctrl Pts',(-19.5267989942869,12.8333605140487,124.656444791742)) ;
#16996 = CARTESIAN_POINT('Ctrl Pts',(-19.5471264172699,12.8324242243262,124.654357589391)) ;
#16997 = CARTESIAN_POINT('Ctrl Pts',(-19.6182032101922,12.8291402385589,124.645293775542)) ;
#16998 = CARTESIAN_POINT('Ctrl Pts',(-19.6685666298544,12.8267934440379,124.635697538319)) ;
#16999 = CARTESIAN_POINT('Ctrl Pts',(-19.7237530651233,12.824182748023,124.62162206394)) ;
#17000 = CARTESIAN_POINT('Ctrl Pts',(-19.729297502019,12.8239200336279,124.620167247834)) ;
#17001 = CARTESIAN_POINT('Ctrl Pts',(-19.7453102774323,12.8231600512955,124.615847681961)) ;
#17002 = CARTESIAN_POINT('Ctrl Pts',(-19.7557515722823,12.8226629523962,124.612884664246)) ;
#17003 = CARTESIAN_POINT('Ctrl Pts',(-19.7776792348842,12.8216157457921,124.606352322668)) ;
#17004 = CARTESIAN_POINT('Ctrl Pts',(-19.7891553756961,12.8210657723521,124.60275241991)) ;
#17005 = CARTESIAN_POINT('Ctrl Pts',(-19.8160271673877,12.8197736585971,124.593895176047)) ;
#17006 = CARTESIAN_POINT('Ctrl Pts',(-19.831375760289,12.8190322555227,124.588501766008)) ;
#17007 = CARTESIAN_POINT('Ctrl Pts',(-19.8892021343457,12.8162272661075,124.566904820949)) ;
#17008 = CARTESIAN_POINT('Ctrl Pts',(-19.930890129217,12.8141775002152,124.548687916848)) ;
#17009 = CARTESIAN_POINT('Ctrl Pts',(-19.9862120828362,12.8113637638717,124.520828344151)) ;
#17010 = CARTESIAN_POINT('Ctrl Pts',(-20.0007829108018,12.8106136312639,124.513125723737)) ;
#17011 = CARTESIAN_POINT('Ctrl Pts',(-20.0206311839269,12.8095776576652,124.502125714621)) ;
#17012 = CARTESIAN_POINT('Ctrl Pts',(-20.0260427212809,12.8092937326215,124.499073658109)) ;
#17013 = CARTESIAN_POINT('Ctrl Pts',(-20.035858034968,12.8087759827119,124.493441051767)) ;
#17014 = CARTESIAN_POINT('Ctrl Pts',(-20.0402691930536,12.8085422657929,124.490873627959)) ;
#17015 = CARTESIAN_POINT('Ctrl Pts',(-20.0485942994345,12.8080991758376,124.485959665455)) ;
#17016 = CARTESIAN_POINT('Ctrl Pts',(-20.052511365692,12.8078898494702,124.483618567812)) ;
#17017 = CARTESIAN_POINT('Ctrl Pts',(-20.0608231855,12.8074438352094,124.478588898318)) ;
#17018 = CARTESIAN_POINT('Ctrl Pts',(-20.0652143134094,12.8072071044632,124.475894500893)) ;
#17019 = CARTESIAN_POINT('Ctrl Pts',(-20.0756650115014,12.8066410225639,124.469392676705)) ;
#17020 = CARTESIAN_POINT('Ctrl Pts',(-20.0817087801683,12.8063114827346,124.465560212044)) ;
#17021 = CARTESIAN_POINT('Ctrl Pts',(-20.0981953601386,12.8054065086142,124.45490616916)) ;
#17022 = CARTESIAN_POINT('Ctrl Pts',(-20.108569470628,12.8048303290835,124.447979872099)) ;
#17023 = CARTESIAN_POINT('Ctrl Pts',(-20.1460575515924,12.8027234604015,124.422131413952)) ;
#17024 = CARTESIAN_POINT('Ctrl Pts',(-20.1725215412225,12.8011874577774,124.40229082695)) ;
#17025 = CARTESIAN_POINT('Ctrl Pts',(-20.2212601773955,12.7982733269864,124.362636042478)) ;
#17026 = CARTESIAN_POINT('Ctrl Pts',(-20.2436741976618,12.7968980591233,124.343028447747)) ;
#17027 = CARTESIAN_POINT('Ctrl Pts',(-20.278705135832,12.7946837528688,124.310102465427)) ;
#17028 = CARTESIAN_POINT('Ctrl Pts',(-20.2917663602418,12.7938421796276,124.297274247366)) ;
#17029 = CARTESIAN_POINT('Ctrl Pts',(-20.3177657482889,12.7921310504403,124.270591769246)) ;
#17030 = CARTESIAN_POINT('Ctrl Pts',(-20.3306800159469,12.7912617719045,124.256720748975)) ;
#17031 = CARTESIAN_POINT('Ctrl Pts',(-20.3630764839494,12.7890269111174,124.220297683454)) ;
#17032 = CARTESIAN_POINT('Ctrl Pts',(-20.3820766671837,12.7876626907649,124.197332897656)) ;
#17033 = CARTESIAN_POINT('Ctrl Pts',(-20.4182038309825,12.7849502876743,124.150343874601)) ;
#17034 = CARTESIAN_POINT('Ctrl Pts',(-20.4353375002655,12.7836029411305,124.126348396332)) ;
#17035 = CARTESIAN_POINT('Ctrl Pts',(-20.4697376095668,12.7807578157418,124.074379195959)) ;
#17036 = CARTESIAN_POINT('Ctrl Pts',(-20.4867817015409,12.779262053449,124.046284493577)) ;
#17037 = CARTESIAN_POINT('Ctrl Pts',(-20.5230877319292,12.7758603065869,123.980747753984)) ;
#17038 = CARTESIAN_POINT('Ctrl Pts',(-20.541604763314,12.7739546870016,123.94293882141)) ;
#17039 = CARTESIAN_POINT('Ctrl Pts',(-20.5621348410788,12.7715779299649,123.895041629938)) ;
#17040 = CARTESIAN_POINT('Ctrl Pts',(-20.5659783913867,12.7711194890167,123.885767574364)) ;
#17041 = CARTESIAN_POINT('Ctrl Pts',(-20.571910552757,12.7703895793769,123.870951817134)) ;
#17042 = CARTESIAN_POINT('Ctrl Pts',(-20.5740722190011,12.7701185660944,123.865439821601)) ;
#17043 = CARTESIAN_POINT('Ctrl Pts',(-20.5783397596512,12.7695731654723,123.854326437396)) ;
#17044 = CARTESIAN_POINT('Ctrl Pts',(-20.5804447348212,12.7692987800961,123.848724867049)) ;
#17045 = CARTESIAN_POINT('Ctrl Pts',(-20.5847002094871,12.7687327577329,123.837148817864)) ;
#17046 = CARTESIAN_POINT('Ctrl Pts',(-20.5868455715947,12.7684410990576,123.831172632627)) ;
#17047 = CARTESIAN_POINT('Ctrl Pts',(-20.5918500775142,12.7677453575245,123.816890662744)) ;
#17048 = CARTESIAN_POINT('Ctrl Pts',(-20.5946673850309,12.7673410620299,123.808570585047)) ;
#17049 = CARTESIAN_POINT('Ctrl Pts',(-20.6023936864466,12.7661953980693,123.784936087112)) ;
#17050 = CARTESIAN_POINT('Ctrl Pts',(-20.6070951589504,12.7654531286899,123.76955569206)) ;
#17051 = CARTESIAN_POINT('Ctrl Pts',(-20.6205219745194,12.7631875501231,123.722394515124)) ;
#17052 = CARTESIAN_POINT('Ctrl Pts',(-20.6282885327783,12.7616623429431,123.690355627853)) ;
#17053 = CARTESIAN_POINT('Ctrl Pts',(-20.6360870201024,12.7598387539018,123.651542354722)) ;
#17054 = CARTESIAN_POINT('Ctrl Pts',(-20.6373422095278,12.7595334695377,123.645027066479)) ;
#17055 = CARTESIAN_POINT('Ctrl Pts',(-20.6392240234138,12.7590567365784,123.634822439879)) ;
#17056 = CARTESIAN_POINT('Ctrl Pts',(-20.639886053901,12.7588849807024,123.63113976734)) ;
#17057 = CARTESIAN_POINT('Ctrl Pts',(-20.6409475265519,12.7586028129954,123.625078974985)) ;
#17058 = CARTESIAN_POINT('Ctrl Pts',(-20.6413566394029,12.7584923035238,123.622702577425)) ;
#17059 = CARTESIAN_POINT('Ctrl Pts',(-20.6423489989286,12.7582198229145,123.616836834334)) ;
#17060 = CARTESIAN_POINT('Ctrl Pts',(-20.6429243141292,12.7580579273651,123.61334616499)) ;
#17061 = CARTESIAN_POINT('Ctrl Pts',(-20.6450986418836,12.7574303499593,123.599795367796)) ;
#17062 = CARTESIAN_POINT('Ctrl Pts',(-20.6465894837429,12.7569655719389,123.58971825148)) ;
#17063 = CARTESIAN_POINT('Ctrl Pts',(-20.6520137578833,12.7551243987104,123.549679039718)) ;
#17064 = CARTESIAN_POINT('Ctrl Pts',(-20.654983329489,12.7537530258065,123.519596740252)) ;
#17065 = CARTESIAN_POINT('Ctrl Pts',(-20.6582655644916,12.7513491962733,123.466842689343)) ;
#17066 = CARTESIAN_POINT('Ctrl Pts',(-20.6590572717309,12.750318552095,123.444215089052)) ;
#17067 = CARTESIAN_POINT('Ctrl Pts',(-20.6592991453929,12.7489043762898,123.413251758331)) ;
#17068 = CARTESIAN_POINT('Ctrl Pts',(-20.6592809837611,12.7485236808201,123.404924505231)) ;
#17069 = CARTESIAN_POINT('Ctrl Pts',(-20.6591047730988,12.7478611164033,123.390450084068)) ;
#17070 = CARTESIAN_POINT('Ctrl Pts',(-20.6589845682959,12.7475794597131,123.384302740036)) ;
#17071 = CARTESIAN_POINT('Ctrl Pts',(-20.6586615394446,12.7470294081541,123.372310292645)) ;
#17072 = CARTESIAN_POINT('Ctrl Pts',(-20.6584630376171,12.7467610437371,123.366465228349)) ;
#17073 = CARTESIAN_POINT('Ctrl Pts',(-20.6579435639546,12.7461785126314,123.353791570327)) ;
#17074 = CARTESIAN_POINT('Ctrl Pts',(-20.6576075802162,12.745864273721,123.346963783305)) ;
#17075 = CARTESIAN_POINT('Ctrl Pts',(-20.6566344107474,12.7450833683746,123.330019855304)) ;
#17076 = CARTESIAN_POINT('Ctrl Pts',(-20.6559301558479,12.7446163757512,123.319908072816)) ;
#17077 = CARTESIAN_POINT('Ctrl Pts',(-20.6516201662555,12.7421801010544,123.267270058961)) ;
#17078 = CARTESIAN_POINT('Ctrl Pts',(-20.6459611978017,12.7402017054295,123.224940545904)) ;
#17079 = CARTESIAN_POINT('Ctrl Pts',(-20.6316045218902,12.7365752730097,123.14784170075)) ;
#17080 = CARTESIAN_POINT('Ctrl Pts',(-20.6235562276742,12.7349267210823,123.112996372846)) ;
#17081 = CARTESIAN_POINT('Ctrl Pts',(-20.6073664514362,12.7321292633185,123.054471273078)) ;
#17082 = CARTESIAN_POINT('Ctrl Pts',(-20.5999902727943,12.73098059351,123.030613108942)) ;
#17083 = CARTESIAN_POINT('Ctrl Pts',(-20.5919011387506,12.7298327524269,123.006982452872)) ;
#17084 = CARTESIAN_POINT('Ctrl Pts',(-20.5919010929902,12.6697683433082,123.006982319192)) ;
#17085 = CARTESIAN_POINT('Ctrl Pts',(-20.5960841911158,12.670359945217,123.019202331386)) ;
#17086 = CARTESIAN_POINT('Ctrl Pts',(-20.6000745876603,12.670951590307,123.03147690456)) ;
#17087 = CARTESIAN_POINT('Ctrl Pts',(-20.6095371759573,12.6724264498721,123.062194962408)) ;
#17088 = CARTESIAN_POINT('Ctrl Pts',(-20.6147726348497,12.6733097112788,123.080697409861)) ;
#17089 = CARTESIAN_POINT('Ctrl Pts',(-20.6262171461193,12.6754144557165,123.125021633689)) ;
#17090 = CARTESIAN_POINT('Ctrl Pts',(-20.6320342620921,12.6766361409836,123.150935055497)) ;
#17091 = CARTESIAN_POINT('Ctrl Pts',(-20.6383947320466,12.6781917078399,123.184193370554)) ;
#17092 = CARTESIAN_POINT('Ctrl Pts',(-20.6397047453997,12.6785273148293,123.1913846312)) ;
#17093 = CARTESIAN_POINT('Ctrl Pts',(-20.6419465529887,12.6791302266929,123.204334131621)) ;
#17094 = CARTESIAN_POINT('Ctrl Pts',(-20.6429012601135,12.6793976240357,123.210088188933)) ;
#17095 = CARTESIAN_POINT('Ctrl Pts',(-20.6448184532083,12.6799577788107,123.222166113018)) ;
#17096 = CARTESIAN_POINT('Ctrl Pts',(-20.6457727400574,12.6802504575829,123.2284911037)) ;
#17097 = CARTESIAN_POINT('Ctrl Pts',(-20.6509979349282,12.681937339407,123.265022233269)) ;
#17098 = CARTESIAN_POINT('Ctrl Pts',(-20.6542104815208,12.6833254213589,123.295369434085)) ;
#17099 = CARTESIAN_POINT('Ctrl Pts',(-20.6575714221632,12.6855504427503,123.344098551755)) ;
#17100 = CARTESIAN_POINT('Ctrl Pts',(-20.6584304990138,12.6863860329828,123.362418808225)) ;
#17101 = CARTESIAN_POINT('Ctrl Pts',(-20.6591438126329,12.6876960563132,123.391114177311)) ;
#17102 = CARTESIAN_POINT('Ctrl Pts',(-20.6592724971882,12.6881695188179,123.401479855197)) ;
#17103 = CARTESIAN_POINT('Ctrl Pts',(-20.6592720305176,12.6890150091815,123.419971766697)) ;
#17104 = CARTESIAN_POINT('Ctrl Pts',(-20.6591925900471,12.6893868245354,123.428097411713)) ;
#17105 = CARTESIAN_POINT('Ctrl Pts',(-20.6588800036677,12.6901199812654,123.444103201659)) ;
#17106 = CARTESIAN_POINT('Ctrl Pts',(-20.6586515286575,12.6904812870742,123.451983067533)) ;
#17107 = CARTESIAN_POINT('Ctrl Pts',(-20.6579463760958,12.6913228529623,123.47031532929)) ;
#17108 = CARTESIAN_POINT('Ctrl Pts',(-20.657412968387,12.6918033144494,123.480764942856)) ;
#17109 = CARTESIAN_POINT('Ctrl Pts',(-20.6545300396442,12.6938898653405,123.526063893808)) ;
#17110 = CARTESIAN_POINT('Ctrl Pts',(-20.6508516386006,12.6955006384372,123.5608127491)) ;
#17111 = CARTESIAN_POINT('Ctrl Pts',(-20.6434453671924,12.6978273649608,123.610704464615)) ;
#17112 = CARTESIAN_POINT('Ctrl Pts',(-20.6408823918687,12.6985426801364,123.626003569198)) ;
#17113 = CARTESIAN_POINT('Ctrl Pts',(-20.6360773279863,12.699748176064,123.65173740467)) ;
#17114 = CARTESIAN_POINT('Ctrl Pts',(-20.6339851356085,12.7002387717928,123.662198297223)) ;
#17115 = CARTESIAN_POINT('Ctrl Pts',(-20.6295931646807,12.7012055395411,123.682784116522)) ;
#17116 = CARTESIAN_POINT('Ctrl Pts',(-20.6273006372482,12.7016817804223,123.692909704444)) ;
#17117 = CARTESIAN_POINT('Ctrl Pts',(-20.6192555467027,12.7032649767667,123.72649482735)) ;
#17118 = CARTESIAN_POINT('Ctrl Pts',(-20.6129492002108,12.7043702405481,123.74981610374)) ;
#17119 = CARTESIAN_POINT('Ctrl Pts',(-20.5987616512748,12.7066181825287,123.796830832246)) ;
#17120 = CARTESIAN_POINT('Ctrl Pts',(-20.5908383556585,12.7077603904967,123.820500370868)) ;
#17121 = CARTESIAN_POINT('Ctrl Pts',(-20.5691859489112,12.7106306795419,123.879275708034)) ;
#17122 = CARTESIAN_POINT('Ctrl Pts',(-20.554567805643,12.7123593141006,123.914027442314)) ;
#17123 = CARTESIAN_POINT('Ctrl Pts',(-20.5312799784474,12.714851400869,123.963062274047)) ;
#17124 = CARTESIAN_POINT('Ctrl Pts',(-20.5238595910577,12.7156134915765,123.977915645908)) ;
#17125 = CARTESIAN_POINT('Ctrl Pts',(-20.5115265343122,12.7168310374864,124.001419561266)) ;
#17126 = CARTESIAN_POINT('Ctrl Pts',(-20.5068026689408,12.7172867938634,124.010166915736)) ;
#17127 = CARTESIAN_POINT('Ctrl Pts',(-20.4978981798395,12.7181267113076,124.026195377235)) ;
#17128 = CARTESIAN_POINT('Ctrl Pts',(-20.4937475718544,12.7185109603369,124.033492513457)) ;
#17129 = CARTESIAN_POINT('Ctrl Pts',(-20.484074561646,12.7193900331888,124.050106819316)) ;
#17130 = CARTESIAN_POINT('Ctrl Pts',(-20.4785039340141,12.7198845012148,124.059395150944)) ;
#17131 = CARTESIAN_POINT('Ctrl Pts',(-20.4577249953554,12.7216871083823,124.093042230999)) ;
#17132 = CARTESIAN_POINT('Ctrl Pts',(-20.4417992473004,12.7229909559485,124.116947384176)) ;
#17133 = CARTESIAN_POINT('Ctrl Pts',(-20.4153099550804,12.7250583774299,124.153884621786)) ;
#17134 = CARTESIAN_POINT('Ctrl Pts',(-20.4052833669348,12.725820179281,124.167289038643)) ;
#17135 = CARTESIAN_POINT('Ctrl Pts',(-20.3892704711107,12.7270075392837,124.187823378824)) ;
#17136 = CARTESIAN_POINT('Ctrl Pts',(-20.3834685953634,12.7274320816729,124.195094636064)) ;
#17137 = CARTESIAN_POINT('Ctrl Pts',(-20.3732279861567,12.728172005311,124.20763897346)) ;
#17138 = CARTESIAN_POINT('Ctrl Pts',(-20.3688257917484,12.728487152105,124.212941364308)) ;
#17139 = CARTESIAN_POINT('Ctrl Pts',(-20.3600054097702,12.7291129549736,124.223388402231)) ;
#17140 = CARTESIAN_POINT('Ctrl Pts',(-20.3555887555784,12.7294235916436,124.228534041554)) ;
#17141 = CARTESIAN_POINT('Ctrl Pts',(-20.3459834859214,12.7300934440423,124.239542172173)) ;
#17142 = CARTESIAN_POINT('Ctrl Pts',(-20.3407812242484,12.7304527372553,124.245392371438)) ;
#17143 = CARTESIAN_POINT('Ctrl Pts',(-20.3258658971748,12.7314731713045,124.2618513899)) ;
#17144 = CARTESIAN_POINT('Ctrl Pts',(-20.3160242279232,12.7321350948293,124.272341939088)) ;
#17145 = CARTESIAN_POINT('Ctrl Pts',(-20.2812999062747,12.734432249313,124.308098429861)) ;
#17146 = CARTESIAN_POINT('Ctrl Pts',(-20.2555248551346,12.7360719711633,124.332473842558)) ;
#17147 = CARTESIAN_POINT('Ctrl Pts',(-20.2211458861119,12.7381733695348,124.362320833883)) ;
#17148 = CARTESIAN_POINT('Ctrl Pts',(-20.2134636698923,12.7386377109107,124.368829260275)) ;
#17149 = CARTESIAN_POINT('Ctrl Pts',(-20.2015341545535,12.7393504866588,124.378690944663)) ;
#17150 = CARTESIAN_POINT('Ctrl Pts',(-20.1973423201663,12.7395994024534,124.382110613887)) ;
#17151 = CARTESIAN_POINT('Ctrl Pts',(-20.1890785660805,12.7400870287261,124.388763248654)) ;
#17152 = CARTESIAN_POINT('Ctrl Pts',(-20.1850084127581,12.7403257569446,124.391998234485)) ;
#17153 = CARTESIAN_POINT('Ctrl Pts',(-20.176100047614,12.7408452668696,124.398988421823)) ;
#17154 = CARTESIAN_POINT('Ctrl Pts',(-20.1712541781852,12.7411259647486,124.402733650917)) ;
#17155 = CARTESIAN_POINT('Ctrl Pts',(-20.1571358542692,12.7419385723428,124.413480481145)) ;
#17156 = CARTESIAN_POINT('Ctrl Pts',(-20.1477930444285,12.7424698975658,124.420388614398)) ;
#17157 = CARTESIAN_POINT('Ctrl Pts',(-20.1151790775322,12.7443047457421,124.443807399264)) ;
#17158 = CARTESIAN_POINT('Ctrl Pts',(-20.0914398751812,12.7456060970084,124.459650900859)) ;
#17159 = CARTESIAN_POINT('Ctrl Pts',(-20.0556172272129,12.7475308243228,124.481825141139)) ;
#17160 = CARTESIAN_POINT('Ctrl Pts',(-20.0439390903719,12.7481523714528,124.488792958826)) ;
#17161 = CARTESIAN_POINT('Ctrl Pts',(-20.0222919202932,12.7492947459734,124.501234460079)) ;
#17162 = CARTESIAN_POINT('Ctrl Pts',(-20.0123573959929,12.7498153332996,124.506765307206)) ;
#17163 = CARTESIAN_POINT('Ctrl Pts',(-19.9921044066942,12.7508697151045,124.517681491241)) ;
#17164 = CARTESIAN_POINT('Ctrl Pts',(-19.9817834003166,12.7514034805954,124.523059795089)) ;
#17165 = CARTESIAN_POINT('Ctrl Pts',(-19.9403110568032,12.7535349213214,124.54393998708)) ;
#17166 = CARTESIAN_POINT('Ctrl Pts',(-19.9085936151727,12.7551357689768,124.558282332323)) ;
#17167 = CARTESIAN_POINT('Ctrl Pts',(-19.8649452523373,12.7573006602749,124.575864393316)) ;
#17168 = CARTESIAN_POINT('Ctrl Pts',(-19.8535042902745,12.7578646144217,124.580278420503)) ;
#17169 = CARTESIAN_POINT('Ctrl Pts',(-19.8354973285712,12.7587465139232,124.586922964131)) ;
#17170 = CARTESIAN_POINT('Ctrl Pts',(-19.8289745737445,12.7590648080492,124.589268396916)) ;
#17171 = CARTESIAN_POINT('Ctrl Pts',(-19.8160890946309,12.7596912209761,124.593781041037)) ;
#17172 = CARTESIAN_POINT('Ctrl Pts',(-19.8097277340896,12.7599993211959,124.59595142382)) ;
#17173 = CARTESIAN_POINT('Ctrl Pts',(-19.7924203720171,12.7608346137997,124.601700968439)) ;
#17174 = CARTESIAN_POINT('Ctrl Pts',(-19.7814419096567,12.761361320123,124.605180343383)) ;
#17175 = CARTESIAN_POINT('Ctrl Pts',(-19.7415587011706,12.7632654326589,124.617216518696)) ;
#17176 = CARTESIAN_POINT('Ctrl Pts',(-19.7123948864096,12.7646403719188,124.624878793787)) ;
#17177 = CARTESIAN_POINT('Ctrl Pts',(-19.6690142600122,12.7666717374937,124.634614032808)) ;
#17178 = CARTESIAN_POINT('Ctrl Pts',(-19.654993057669,12.767326163707,124.637508545113)) ;
#17179 = CARTESIAN_POINT('Ctrl Pts',(-19.6289971539258,12.7685366841072,124.642411091961)) ;
#17180 = CARTESIAN_POINT('Ctrl Pts',(-19.6170369337289,12.7690925279948,124.644486735641)) ;
#17181 = CARTESIAN_POINT('Ctrl Pts',(-19.5938211084317,12.7701699042363,124.648168254323)) ;
#17182 = CARTESIAN_POINT('Ctrl Pts',(-19.5825700660305,12.7706913232976,124.649795417854)) ;
#17183 = CARTESIAN_POINT('Ctrl Pts',(-19.5340414165973,12.772938014668,124.656139266378)) ;
#17184 = CARTESIAN_POINT('Ctrl Pts',(-19.4965838483847,12.7746668440938,124.659327280877)) ;
#17185 = CARTESIAN_POINT('Ctrl Pts',(-19.4466341005257,12.7769666458711,124.661317563188)) ;
#17186 = CARTESIAN_POINT('Ctrl Pts',(-19.4342216473971,12.7775376245486,124.661627022527)) ;
#17187 = CARTESIAN_POINT('Ctrl Pts',(-19.4200629558388,12.7781881799603,124.661769006205)) ;
#17188 = CARTESIAN_POINT('Ctrl Pts',(-19.4183192425384,12.7782682859684,124.661782843155)) ;
#17189 = CARTESIAN_POINT('Ctrl Pts',(-19.4155790323222,12.7783941494927,124.661798853423)) ;
#17190 = CARTESIAN_POINT('Ctrl Pts',(-19.4145825523688,12.7784399154207,124.66180348396)) ;
#17191 = CARTESIAN_POINT('Ctrl Pts',(-19.4130294681036,12.7785112377391,124.661808843788)) ;
#17192 = CARTESIAN_POINT('Ctrl Pts',(-19.4124728671917,12.7785367971106,124.661810392895)) ;
#17193 = CARTESIAN_POINT('Ctrl Pts',(-19.4111369635157,12.7785981389672,124.661813218636)) ;
#17194 = CARTESIAN_POINT('Ctrl Pts',(-19.4103576601202,12.7786339200973,124.661814138262)) ;
#17195 = CARTESIAN_POINT('Ctrl Pts',(-19.4033948987358,12.7789535843599,124.661815843416)) ;
#17196 = CARTESIAN_POINT('Ctrl Pts',(-19.3972115053518,12.7792372867439,124.661771475524)) ;
#17197 = CARTESIAN_POINT('Ctrl Pts',(-19.3837819763669,12.7798529971387,124.661575452831)) ;
#17198 = CARTESIAN_POINT('Ctrl Pts',(-19.3765363228649,12.7801848822632,124.661406654615)) ;
#17199 = CARTESIAN_POINT('Ctrl Pts',(-19.3497108423677,12.7814129872106,124.660548235554)) ;
#17200 = CARTESIAN_POINT('Ctrl Pts',(-19.3301465385876,12.7823074962193,124.659461337073)) ;
#17201 = CARTESIAN_POINT('Ctrl Pts',(-19.2880638559818,12.784234764284,124.65612956335)) ;
#17202 = CARTESIAN_POINT('Ctrl Pts',(-19.2655645192677,12.7852671702212,124.653732186074)) ;
#17203 = CARTESIAN_POINT('Ctrl Pts',(-19.2311176840881,12.7868556544937,124.649113100317)) ;
#17204 = CARTESIAN_POINT('Ctrl Pts',(-19.2191168125422,12.787410521221,124.64732564328)) ;
#17205 = CARTESIAN_POINT('Ctrl Pts',(-19.1955740162531,12.7885025974153,124.643467940859)) ;
#17206 = CARTESIAN_POINT('Ctrl Pts',(-19.1840314116677,12.7890397178046,124.641409432529)) ;
#17207 = CARTESIAN_POINT('Ctrl Pts',(-19.1586869820179,12.7902233490391,124.636520653156)) ;
#17208 = CARTESIAN_POINT('Ctrl Pts',(-19.1449005902117,12.790870004571,124.633618806386)) ;
#17209 = CARTESIAN_POINT('Ctrl Pts',(-19.0983886574912,12.7930620641666,124.623004574635)) ;
#17210 = CARTESIAN_POINT('Ctrl Pts',(-19.0659262492723,12.7946099096908,124.614205253279)) ;
#17211 = CARTESIAN_POINT('Ctrl Pts',(-19.0237681370969,12.7966434077663,124.600931052706)) ;
#17212 = CARTESIAN_POINT('Ctrl Pts',(-19.0137187708793,12.7971298798037,124.597626054994)) ;
#17213 = CARTESIAN_POINT('Ctrl Pts',(-18.9976052074849,12.7979125334102,124.592099055018)) ;
#17214 = CARTESIAN_POINT('Ctrl Pts',(-18.9915141721302,12.7982089905183,124.58995692521)) ;
#17215 = CARTESIAN_POINT('Ctrl Pts',(-18.9803258451703,12.7987545965281,124.585924474665)) ;
#17216 = CARTESIAN_POINT('Ctrl Pts',(-18.9752237614047,12.7990038112658,124.584047907311)) ;
#17217 = CARTESIAN_POINT('Ctrl Pts',(-18.9644313744561,12.7995317874279,124.579998302248)) ;
#17218 = CARTESIAN_POINT('Ctrl Pts',(-18.9587443938632,12.799810463628,124.577816838011)) ;
#17219 = CARTESIAN_POINT('Ctrl Pts',(-18.9256333390202,12.8014360006373,124.564837386973)) ;
#17220 = CARTESIAN_POINT('Ctrl Pts',(-18.8985820134551,12.8027767993694,124.553113705154)) ;
#17221 = CARTESIAN_POINT('Ctrl Pts',(-18.8558699778635,12.8049312152057,124.532779982081)) ;
#17222 = CARTESIAN_POINT('Ctrl Pts',(-18.839935527488,12.8057435595496,124.524771544718)) ;
#17223 = CARTESIAN_POINT('Ctrl Pts',(-18.8153499744578,12.8070130804467,124.511748975838)) ;
#17224 = CARTESIAN_POINT('Ctrl Pts',(-18.8065784404411,12.807469289257,124.506967317279)) ;
#17225 = CARTESIAN_POINT('Ctrl Pts',(-18.7911142894719,12.8082798229713,124.498295227069)) ;
#17226 = CARTESIAN_POINT('Ctrl Pts',(-18.7843987140776,12.8086339352717,124.494446801091)) ;
#17227 = CARTESIAN_POINT('Ctrl Pts',(-18.7713762521518,12.8093249321281,124.486822617535)) ;
#17228 = CARTESIAN_POINT('Ctrl Pts',(-18.7650660677071,12.8096617727325,124.483053106636)) ;
#17229 = CARTESIAN_POINT('Ctrl Pts',(-18.7504283843418,12.8104479788474,124.474132892003)) ;
#17230 = CARTESIAN_POINT('Ctrl Pts',(-18.742127435643,12.8108975360351,124.468939564859)) ;
#17231 = CARTESIAN_POINT('Ctrl Pts',(-18.7027397971061,12.8130489198317,124.443648737006)) ;
#17232 = CARTESIAN_POINT('Ctrl Pts',(-18.6724951513233,12.8147566502298,124.422274537197)) ;
#17233 = CARTESIAN_POINT('Ctrl Pts',(-18.6326722836895,12.8170813965894,124.391391564076)) ;
#17234 = CARTESIAN_POINT('Ctrl Pts',(-18.6222329658112,12.8176982802149,124.38302400425)) ;
#17235 = CARTESIAN_POINT('Ctrl Pts',(-18.6069019144491,12.8186149139447,124.370325968801)) ;
#17236 = CARTESIAN_POINT('Ctrl Pts',(-18.6019065631736,12.8189153133053,124.366122123626)) ;
#17237 = CARTESIAN_POINT('Ctrl Pts',(-18.5930292678969,12.8194521687923,124.358531827554)) ;
#17238 = CARTESIAN_POINT('Ctrl Pts',(-18.5891348980241,12.8196887243887,124.355160157333)) ;
#17239 = CARTESIAN_POINT('Ctrl Pts',(-18.5807880113737,12.8201980365719,124.347842828215)) ;
#17240 = CARTESIAN_POINT('Ctrl Pts',(-18.5763426001166,12.82047073064,124.343889263449)) ;
#17241 = CARTESIAN_POINT('Ctrl Pts',(-18.564347902368,12.8212106848589,124.333067335709)) ;
#17242 = CARTESIAN_POINT('Ctrl Pts',(-18.5568542285001,12.8216775159828,124.326137998624)) ;
#17243 = CARTESIAN_POINT('Ctrl Pts',(-18.5425264467297,12.8225797307972,124.312559959872)) ;
#17244 = CARTESIAN_POINT('Ctrl Pts',(-18.5356818918536,12.8230151294021,124.305923307416)) ;
#17245 = CARTESIAN_POINT('Ctrl Pts',(-18.5242856482261,12.8237480503756,124.294617426755)) ;
#17246 = CARTESIAN_POINT('Ctrl Pts',(-18.5196933662955,12.8240456319155,124.289989712524)) ;
#17247 = CARTESIAN_POINT('Ctrl Pts',(-18.4996292911165,12.8253561124514,124.269451942769)) ;
#17248 = CARTESIAN_POINT('Ctrl Pts',(-18.4845465990051,12.8263686717888,124.253167439685)) ;
#17249 = CARTESIAN_POINT('Ctrl Pts',(-18.4615839543545,12.8279589485158,124.227011285135)) ;
#17250 = CARTESIAN_POINT('Ctrl Pts',(-18.4534064174256,12.828535602789,124.217407086905)) ;
#17251 = CARTESIAN_POINT('Ctrl Pts',(-18.4383242250919,12.8296196212799,124.19914061251)) ;
#17252 = CARTESIAN_POINT('Ctrl Pts',(-18.4313866247621,12.8301268102426,124.190507109525)) ;
#17253 = CARTESIAN_POINT('Ctrl Pts',(-18.4173167616063,12.8311737882064,124.17251324898)) ;
#17254 = CARTESIAN_POINT('Ctrl Pts',(-18.4102000964298,12.8317135837244,124.163142065915)) ;
#17255 = CARTESIAN_POINT('Ctrl Pts',(-18.3785915210041,12.8341590400966,124.120276717119)) ;
#17256 = CARTESIAN_POINT('Ctrl Pts',(-18.3556443403483,12.8360695219318,124.085676277074)) ;
#17257 = CARTESIAN_POINT('Ctrl Pts',(-18.3275920554326,12.8385982385192,124.038431452916)) ;
#17258 = CARTESIAN_POINT('Ctrl Pts',(-18.320910784028,12.8392169989039,124.026753662401)) ;
#17259 = CARTESIAN_POINT('Ctrl Pts',(-18.2999386576922,12.8412137193077,123.988684908242)) ;
#17260 = CARTESIAN_POINT('Ctrl Pts',(-18.2864092655001,12.8425889950063,123.961886513872)) ;
#17261 = CARTESIAN_POINT('Ctrl Pts',(-18.2561390929588,12.8459075576379,123.896147498959)) ;
#17262 = CARTESIAN_POINT('Ctrl Pts',(-18.2403883533361,12.8478499286865,123.856791991268)) ;
#17263 = CARTESIAN_POINT('Ctrl Pts',(-18.2159181794863,12.8513191239244,123.785320842823)) ;
#17264 = CARTESIAN_POINT('Ctrl Pts',(-18.2064243658445,12.8528431832765,123.753513062738)) ;
#17265 = CARTESIAN_POINT('Ctrl Pts',(-18.1965692307665,12.8546680305787,123.714956539527)) ;
#17266 = CARTESIAN_POINT('Ctrl Pts',(-18.1949820290037,12.8549712114887,123.708534856787)) ;
#17267 = CARTESIAN_POINT('Ctrl Pts',(-18.1914072689346,12.8556763185502,123.693562450381)) ;
#17268 = CARTESIAN_POINT('Ctrl Pts',(-18.189458661781,12.8560780887129,123.68500277319)) ;
#17269 = CARTESIAN_POINT('Ctrl Pts',(-18.1852034382759,12.8569970743002,123.665356847336)) ;
#17270 = CARTESIAN_POINT('Ctrl Pts',(-18.1829569675309,12.8575139552109,123.654258329805)) ;
#17271 = CARTESIAN_POINT('Ctrl Pts',(-18.1796945423303,12.8583170926136,123.636933153194)) ;
#17272 = CARTESIAN_POINT('Ctrl Pts',(-18.1785744105169,12.8586040579667,123.630726759156)) ;
#17273 = CARTESIAN_POINT('Ctrl Pts',(-18.1748597197803,12.8595960697717,123.609214318925)) ;
#17274 = CARTESIAN_POINT('Ctrl Pts',(-18.1725033720112,12.8602986929342,123.593868700848)) ;
#17275 = CARTESIAN_POINT('Ctrl Pts',(-18.1639997962845,12.8631805185092,123.530662102417)) ;
#17276 = CARTESIAN_POINT('Ctrl Pts',(-18.1603405148723,12.865351269217,123.482509207639)) ;
#17277 = CARTESIAN_POINT('Ctrl Pts',(-18.1593282957932,12.8679179022969,123.426161558769)) ;
#17278 = CARTESIAN_POINT('Ctrl Pts',(-18.1592615433982,12.8682876430093,123.418056403349)) ;
#17279 = CARTESIAN_POINT('Ctrl Pts',(-18.1592804871582,12.8688684674536,123.40534702554)) ;
#17280 = CARTESIAN_POINT('Ctrl Pts',(-18.1593127879161,12.8690790917927,123.400742933181)) ;
#17281 = CARTESIAN_POINT('Ctrl Pts',(-18.1594151706232,12.8694529712368,123.392579205984)) ;
#17282 = CARTESIAN_POINT('Ctrl Pts',(-18.1594750249168,12.8696161365814,123.389019490853)) ;
#17283 = CARTESIAN_POINT('Ctrl Pts',(-18.159632765082,12.869959302323,123.381539439266)) ;
#17284 = CARTESIAN_POINT('Ctrl Pts',(-18.1597338933685,12.8701393287889,123.377619210777)) ;
#17285 = CARTESIAN_POINT('Ctrl Pts',(-18.1600664474139,12.8706404508407,123.36671796321)) ;
#17286 = CARTESIAN_POINT('Ctrl Pts',(-18.1603379409469,12.8709618823952,123.359738327528)) ;
#17287 = CARTESIAN_POINT('Ctrl Pts',(-18.1610858282145,12.8716915036932,123.343925157774)) ;
#17288 = CARTESIAN_POINT('Ctrl Pts',(-18.1615975234618,12.8720999681551,123.335093680034)) ;
#17289 = CARTESIAN_POINT('Ctrl Pts',(-18.1635094233256,12.8733921735138,123.307222442001)) ;
#17290 = CARTESIAN_POINT('Ctrl Pts',(-18.1652520719457,12.8742783891576,123.288209034038)) ;
#17291 = CARTESIAN_POINT('Ctrl Pts',(-18.1742895560144,12.8779645148339,123.209489550242)) ;
#17292 = CARTESIAN_POINT('Ctrl Pts',(-18.1854536468484,12.880764858379,123.150307440896)) ;
#17293 = CARTESIAN_POINT('Ctrl Pts',(-18.2051839412113,12.8843217173769,123.075718257719)) ;
#17294 = CARTESIAN_POINT('Ctrl Pts',(-18.2098679568054,12.885104230482,123.059367781973)) ;
#17295 = CARTESIAN_POINT('Ctrl Pts',(-18.2188151390036,12.8864981714979,123.030383482486)) ;
#17296 = CARTESIAN_POINT('Ctrl Pts',(-18.2229495608453,12.8871098980653,123.017712690547)) ;
#17297 = CARTESIAN_POINT('Ctrl Pts',(-18.2312369557602,12.8882780263911,122.993627386663)) ;
#17298 = CARTESIAN_POINT('Ctrl Pts',(-18.2353552290918,12.8888344541128,122.982202526046)) ;
#17299 = CARTESIAN_POINT('Ctrl Pts',(-18.2447155077819,12.8900493585435,122.957375511653)) ;
#17300 = CARTESIAN_POINT('Ctrl Pts',(-18.2500238013672,12.8907075928925,122.944000178725)) ;
#17301 = CARTESIAN_POINT('Ctrl Pts',(-18.2628071722129,12.8922258766517,122.913344464763)) ;
#17302 = CARTESIAN_POINT('Ctrl Pts',(-18.2704441053724,12.8930853963541,122.896135321457)) ;
#17303 = CARTESIAN_POINT('Ctrl Pts',(-18.289582210683,12.8951337624835,122.8555100139)) ;
#17304 = CARTESIAN_POINT('Ctrl Pts',(-18.3014334469546,12.89632135519,122.832268412208)) ;
#17305 = CARTESIAN_POINT('Ctrl Pts',(-18.3327522209393,12.8992749106568,122.775325356876)) ;
#17306 = CARTESIAN_POINT('Ctrl Pts',(-18.3530825246731,12.9010333462363,122.742130189385)) ;
#17307 = CARTESIAN_POINT('Ctrl Pts',(-18.3894936180088,12.9039728161439,122.688471779208)) ;
#17308 = CARTESIAN_POINT('Ctrl Pts',(-18.4047240157505,12.9051508716758,122.667465130711)) ;
#17309 = CARTESIAN_POINT('Ctrl Pts',(-18.4257461752842,12.9067181083841,122.640291647039)) ;
#17310 = CARTESIAN_POINT('Ctrl Pts',(-18.4309625618981,12.9071024941052,122.63368777043)) ;
#17311 = CARTESIAN_POINT('Ctrl Pts',(-18.4394885333965,12.9077237505213,122.623115270299)) ;
#17312 = CARTESIAN_POINT('Ctrl Pts',(-18.4427567443871,12.907960276725,122.619113604254)) ;
#17313 = CARTESIAN_POINT('Ctrl Pts',(-18.4492906270678,12.9084299999391,122.611213861411)) ;
#17314 = CARTESIAN_POINT('Ctrl Pts',(-18.4525554640106,12.9086631861876,122.607315220292)) ;
#17315 = CARTESIAN_POINT('Ctrl Pts',(-18.4558540804007,12.9088972815569,122.603424719808)) ;
#17316 = CARTESIAN_POINT('Ctrl Pts',(-18.4558641674244,12.9088979973962,122.603412823281)) ;
#17317 = CARTESIAN_POINT('Ctrl Pts',(-18.4558843566946,12.9088994301272,122.603389013175)) ;
#17318 = CARTESIAN_POINT('Ctrl Pts',(-18.4558944592937,12.9089001470437,122.603377099183)) ;
#17319 = CARTESIAN_POINT('Ctrl Pts',(-18.4559146813778,12.9089015820471,122.60335325219)) ;
#17320 = CARTESIAN_POINT('Ctrl Pts',(-18.4559248003457,12.9089023000971,122.603341319802)) ;
#17321 = CARTESIAN_POINT('Ctrl Pts',(-18.455945056138,12.9089037374361,122.603317434877)) ;
#17322 = CARTESIAN_POINT('Ctrl Pts',(-18.455955192484,12.908904456691,122.603305482907)) ;
#17323 = CARTESIAN_POINT('Ctrl Pts',(-18.4559754810373,12.9089058962981,122.603281561176)) ;
#17324 = CARTESIAN_POINT('Ctrl Pts',(-18.4559856343577,12.9089066167292,122.603269590104)) ;
#17325 = CARTESIAN_POINT('Ctrl Pts',(-18.4560059588853,12.9089080588321,122.603245627787)) ;
#17326 = CARTESIAN_POINT('Ctrl Pts',(-18.4560161301038,12.9089087805047,122.603233636529)) ;
#17327 = CARTESIAN_POINT('Ctrl Pts',(-18.4560364903646,12.9089102250861,122.603209633919)) ;
#17328 = CARTESIAN_POINT('Ctrl Pts',(-18.4560466796096,12.9089109480092,122.603197622329)) ;
#17329 = CARTESIAN_POINT('Ctrl Pts',(-18.4560670777304,12.9089123952197,122.603173576929)) ;
#17330 = CARTESIAN_POINT('Ctrl Pts',(-18.4560772858882,12.908913119456,122.603161543966)) ;
#17331 = CARTESIAN_POINT('Ctrl Pts',(-18.4560977223255,12.9089145693275,122.603137455248)) ;
#17332 = CARTESIAN_POINT('Ctrl Pts',(-18.4561079501488,12.9089152949304,122.603125400031)) ;
#17333 = CARTESIAN_POINT('Ctrl Pts',(-18.456128425055,12.9089167474735,122.603101267825)) ;
#17334 = CARTESIAN_POINT('Ctrl Pts',(-18.4561386727124,12.9089174744546,122.60308919016)) ;
#17335 = CARTESIAN_POINT('Ctrl Pts',(-18.456159187164,12.9089189297455,122.603065013207)) ;
#17336 = CARTESIAN_POINT('Ctrl Pts',(-18.4561694545687,12.9089196580985,122.603052913202)) ;
#17337 = CARTESIAN_POINT('Ctrl Pts',(-18.4561900120466,12.9089211163836,122.603028687412)) ;
#17338 = CARTESIAN_POINT('Ctrl Pts',(-18.4562003009971,12.908921846236,122.603016562952)) ;
#17339 = CARTESIAN_POINT('Ctrl Pts',(-18.4562208987565,12.9089233073204,122.60299229157)) ;
#17340 = CARTESIAN_POINT('Ctrl Pts',(-18.4562312086243,12.9089240386274,122.602980143403)) ;
#17341 = CARTESIAN_POINT('Ctrl Pts',(-18.4562518503084,12.908925502769,122.602955822147)) ;
#17342 = CARTESIAN_POINT('Ctrl Pts',(-18.4562621819516,12.9089262355913,122.602943649266)) ;
#17343 = CARTESIAN_POINT('Ctrl Pts',(-18.4562828682643,12.9089277028398,122.60291927732)) ;
#17344 = CARTESIAN_POINT('Ctrl Pts',(-18.4562932226001,12.9089284372423,122.60290707865)) ;
#17345 = CARTESIAN_POINT('Ctrl Pts',(-18.4563139528768,12.9089299075501,122.602882656808)) ;
#17346 = CARTESIAN_POINT('Ctrl Pts',(-18.4563243295604,12.9089306435081,122.602870432763)) ;
#17347 = CARTESIAN_POINT('Ctrl Pts',(-18.4563451072982,12.908932117123,122.602845956917)) ;
#17348 = CARTESIAN_POINT('Ctrl Pts',(-18.456355507598,12.9089328547263,122.602833706007)) ;
#17349 = CARTESIAN_POINT('Ctrl Pts',(-18.4563763318937,12.9089343315837,122.602809177235)) ;
#17350 = CARTESIAN_POINT('Ctrl Pts',(-18.4563867559345,12.9089350708409,122.602796899321)) ;
#17351 = CARTESIAN_POINT('Ctrl Pts',(-18.4564076289155,12.9089365510913,122.602772315129)) ;
#17352 = CARTESIAN_POINT('Ctrl Pts',(-18.4564180775277,12.9089372920612,122.602760009239)) ;
#17353 = CARTESIAN_POINT('Ctrl Pts',(-18.4564389991234,12.9089387756992,122.602735369723)) ;
#17354 = CARTESIAN_POINT('Ctrl Pts',(-18.4564494723635,12.9089395183855,122.602723035797)) ;
#17355 = CARTESIAN_POINT('Ctrl Pts',(-18.4564704452369,12.9089410055996,122.602698337835)) ;
#17356 = CARTESIAN_POINT('Ctrl Pts',(-18.4564809443246,12.9089417500887,122.602685974444)) ;
#17357 = CARTESIAN_POINT('Ctrl Pts',(-18.4565019674821,12.9089432408079,122.60266121922)) ;
#17358 = CARTESIAN_POINT('Ctrl Pts',(-18.4565124923333,12.9089439870934,122.602648826469)) ;
#17359 = CARTESIAN_POINT('Ctrl Pts',(-18.4565335679513,12.9089454814717,122.602624011434)) ;
#17360 = CARTESIAN_POINT('Ctrl Pts',(-18.4565441189964,12.9089462295841,122.602611588825)) ;
#17361 = CARTESIAN_POINT('Ctrl Pts',(-18.4565652487466,12.9089477277395,122.602586712025)) ;
#17362 = CARTESIAN_POINT('Ctrl Pts',(-18.4565758269448,12.9089484777465,122.602574258435)) ;
#17363 = CARTESIAN_POINT('Ctrl Pts',(-18.4565970109862,12.9089499796898,122.602549319699)) ;
#17364 = CARTESIAN_POINT('Ctrl Pts',(-18.4566076168602,12.9089507316283,122.602536834519)) ;
#17365 = CARTESIAN_POINT('Ctrl Pts',(-18.4566288557991,12.9089522374021,122.602511833148)) ;
#17366 = CARTESIAN_POINT('Ctrl Pts',(-18.4566394894094,12.908952991276,122.602499316316)) ;
#17367 = CARTESIAN_POINT('Ctrl Pts',(-18.456660785507,12.9089545010401,122.602474249663)) ;
#17368 = CARTESIAN_POINT('Ctrl Pts',(-18.4566714476506,12.9089552569058,122.602461700249)) ;
#17369 = CARTESIAN_POINT('Ctrl Pts',(-18.456692801756,12.9089567707199,122.60243656733)) ;
#17370 = CARTESIAN_POINT('Ctrl Pts',(-18.456703493267,12.9089575286362,122.602423984359)) ;
#17371 = CARTESIAN_POINT('Ctrl Pts',(-18.4567249053252,12.9089590464959,122.602398785257)) ;
#17372 = CARTESIAN_POINT('Ctrl Pts',(-18.4567356262341,12.9089598064648,122.602386168702)) ;
#17373 = CARTESIAN_POINT('Ctrl Pts',(-18.4567570988112,12.9089613285514,122.602360900411)) ;
#17374 = CARTESIAN_POINT('Ctrl Pts',(-18.4567678501102,12.9089620906429,122.602348249113)) ;
#17375 = CARTESIAN_POINT('Ctrl Pts',(-18.4567893831584,12.9089636169527,122.602322911708)) ;
#17376 = CARTESIAN_POINT('Ctrl Pts',(-18.456800165178,12.90896438119,122.602310225286)) ;
#17377 = CARTESIAN_POINT('Ctrl Pts',(-18.4568217602641,12.9089659118333,122.60228481694)) ;
#17378 = CARTESIAN_POINT('Ctrl Pts',(-18.4568325735926,12.9089666782578,122.602272094711)) ;
#17379 = CARTESIAN_POINT('Ctrl Pts',(-18.4568542313575,12.9089682132796,122.602246614688)) ;
#17380 = CARTESIAN_POINT('Ctrl Pts',(-18.4568650761759,12.9089689819039,122.602233856447)) ;
#17381 = CARTESIAN_POINT('Ctrl Pts',(-18.4568867992335,12.9089705214889,122.602208301689)) ;
#17382 = CARTESIAN_POINT('Ctrl Pts',(-18.4568976768567,12.9089712924059,122.6021955059)) ;
#17383 = CARTESIAN_POINT('Ctrl Pts',(-18.4569194638754,12.9089728364592,122.602169877992)) ;
#17384 = CARTESIAN_POINT('Ctrl Pts',(-18.4569303739604,12.9089736096443,122.602157045066)) ;
#17385 = CARTESIAN_POINT('Ctrl Pts',(-18.456952228497,12.9089751584173,122.602131339843)) ;
#17386 = CARTESIAN_POINT('Ctrl Pts',(-18.4569631722283,12.9089759339541,122.602118468397)) ;
#17387 = CARTESIAN_POINT('Ctrl Pts',(-18.4569850941584,12.9089774874374,122.602092686025)) ;
#17388 = CARTESIAN_POINT('Ctrl Pts',(-18.4569960721004,12.9089782653657,122.602079775404)) ;
#17389 = CARTESIAN_POINT('Ctrl Pts',(-18.4570180622743,12.908979823619,122.602053914902)) ;
#17390 = CARTESIAN_POINT('Ctrl Pts',(-18.4570290747303,12.9089806039599,122.60204096476)) ;
#17391 = CARTESIAN_POINT('Ctrl Pts',(-18.4570511350328,12.9089821671162,122.602015023931)) ;
#17392 = CARTESIAN_POINT('Ctrl Pts',(-18.4570621827805,12.9089829499245,122.602002033364)) ;
#17393 = CARTESIAN_POINT('Ctrl Pts',(-18.4570843139133,12.9089845180328,122.601976011403)) ;
#17394 = CARTESIAN_POINT('Ctrl Pts',(-18.4570953975003,12.908985303347,122.601962979776)) ;
#17395 = CARTESIAN_POINT('Ctrl Pts',(-18.45711760032,12.9089868764674,122.601936875698)) ;
#17396 = CARTESIAN_POINT('Ctrl Pts',(-18.4571287199829,12.908987664304,122.601923802743)) ;
#17397 = CARTESIAN_POINT('Ctrl Pts',(-18.4571509967091,12.9089892425931,122.601897613958)) ;
#17398 = CARTESIAN_POINT('Ctrl Pts',(-18.4571621533885,12.9089900330183,122.601884498581)) ;
#17399 = CARTESIAN_POINT('Ctrl Pts',(-18.4571845043054,12.9089916164956,122.601858224776)) ;
#17400 = CARTESIAN_POINT('Ctrl Pts',(-18.4571956984338,12.9089924095398,122.60184506648)) ;
#17401 = CARTESIAN_POINT('Ctrl Pts',(-18.4572181253768,12.9089939983346,122.60181870552)) ;
#17402 = CARTESIAN_POINT('Ctrl Pts',(-18.4572293578823,12.9089947940632,122.601805503223)) ;
#17403 = CARTESIAN_POINT('Ctrl Pts',(-18.4572518608785,12.9089963881768,122.601779055099)) ;
#17404 = CARTESIAN_POINT('Ctrl Pts',(-18.4572631318871,12.9089971865984,122.601765808666)) ;
#17405 = CARTESIAN_POINT('Ctrl Pts',(-18.4572857132798,12.908998786196,122.601739270645)) ;
#17406 = CARTESIAN_POINT('Ctrl Pts',(-18.4572970235877,12.9089995873666,122.601725979151)) ;
#17407 = CARTESIAN_POINT('Ctrl Pts',(-18.4573196841441,12.9090011925019,122.601699350356)) ;
#17408 = CARTESIAN_POINT('Ctrl Pts',(-18.4573310343277,12.909001996462,122.601686013135)) ;
#17409 = CARTESIAN_POINT('Ctrl Pts',(-18.45735377563,12.9090036072463,122.601659291729)) ;
#17410 = CARTESIAN_POINT('Ctrl Pts',(-18.4573651665971,12.9090044140598,122.601645907727)) ;
#17411 = CARTESIAN_POINT('Ctrl Pts',(-18.4573879885289,12.9090060304842,122.601619093872)) ;
#17412 = CARTESIAN_POINT('Ctrl Pts',(-18.4573994201699,12.9090068401429,122.601605663229)) ;
#17413 = CARTESIAN_POINT('Ctrl Pts',(-18.4574223260808,12.9090084624439,122.601578753014)) ;
#17414 = CARTESIAN_POINT('Ctrl Pts',(-18.457433799672,12.9090092750379,122.601565274243)) ;
#17415 = CARTESIAN_POINT('Ctrl Pts',(-18.4574567891932,12.9090109031885,122.601538268126)) ;
#17416 = CARTESIAN_POINT('Ctrl Pts',(-18.4574683050772,12.9090117187417,122.601524740838)) ;
#17417 = CARTESIAN_POINT('Ctrl Pts',(-18.4574913803924,12.9090133528958,122.601497636278)) ;
#17418 = CARTESIAN_POINT('Ctrl Pts',(-18.4575029395734,12.9090141714789,122.601484059305)) ;
#17419 = CARTESIAN_POINT('Ctrl Pts',(-18.4575261006358,12.9090158116324,122.601456856385)) ;
#17420 = CARTESIAN_POINT('Ctrl Pts',(-18.4575377031876,12.9090166332502,122.601443229654)) ;
#17421 = CARTESIAN_POINT('Ctrl Pts',(-18.4575609527486,12.9090182795971,122.601415925167)) ;
#17422 = CARTESIAN_POINT('Ctrl Pts',(-18.4575725996707,12.90901910432,122.601402247517)) ;
#17423 = CARTESIAN_POINT('Ctrl Pts',(-18.4575959378497,12.9090207568679,122.60137484135)) ;
#17424 = CARTESIAN_POINT('Ctrl Pts',(-18.4576076293573,12.9090215847107,122.601361112543)) ;
#17425 = CARTESIAN_POINT('Ctrl Pts',(-18.4576310589047,12.9090232436536,122.601333601494)) ;
#17426 = CARTESIAN_POINT('Ctrl Pts',(-18.4576427962344,12.9090240747034,122.60131982009)) ;
#17427 = CARTESIAN_POINT('Ctrl Pts',(-18.4576663171573,12.9090257400409,122.601292204178)) ;
#17428 = CARTESIAN_POINT('Ctrl Pts',(-18.4576781008623,12.9090265743365,122.601278369543)) ;
#17429 = CARTESIAN_POINT('Ctrl Pts',(-18.4577017142152,12.9090282461424,122.601250647559)) ;
#17430 = CARTESIAN_POINT('Ctrl Pts',(-18.4577135445022,12.9090290836979,122.601236759464)) ;
#17431 = CARTESIAN_POINT('Ctrl Pts',(-18.4577372527087,12.9090307621429,122.60120892859)) ;
#17432 = CARTESIAN_POINT('Ctrl Pts',(-18.4577491304199,12.9090316030176,122.601194986061)) ;
#17433 = CARTESIAN_POINT('Ctrl Pts',(-18.4577729347397,12.9090332881899,122.601167044849)) ;
#17434 = CARTESIAN_POINT('Ctrl Pts',(-18.4577848608323,12.909034132451,122.601153046777)) ;
#17435 = CARTESIAN_POINT('Ctrl Pts',(-18.457808761954,12.9090358243986,122.601124994448)) ;
#17436 = CARTESIAN_POINT('Ctrl Pts',(-18.4578207370233,12.9090366720878,122.601110940149)) ;
#17437 = CARTESIAN_POINT('Ctrl Pts',(-18.4578447362279,12.9090383709002,122.601082775231)) ;
#17438 = CARTESIAN_POINT('Ctrl Pts',(-18.4578567607262,12.9090392220491,122.60106866419)) ;
#17439 = CARTESIAN_POINT('Ctrl Pts',(-18.457880859675,12.9090409278431,122.601040384763)) ;
#17440 = CARTESIAN_POINT('Ctrl Pts',(-18.4578929341062,12.9090417824868,122.601026216404)) ;
#17441 = CARTESIAN_POINT('Ctrl Pts',(-18.457917135395,12.9090434954452,122.600997819454)) ;
#17442 = CARTESIAN_POINT('Ctrl Pts',(-18.4579292613029,12.9090443536925,122.600983591983)) ;
#17443 = CARTESIAN_POINT('Ctrl Pts',(-18.4579535637288,12.9090460737291,122.600955078953)) ;
#17444 = CARTESIAN_POINT('Ctrl Pts',(-18.4579657409352,12.9090469355669,122.600940792593)) ;
#17445 = CARTESIAN_POINT('Ctrl Pts',(-18.4579901481554,12.9090486629395,122.600912159226)) ;
#17446 = CARTESIAN_POINT('Ctrl Pts',(-18.4580023778348,12.9090495284504,122.600897812616)) ;
#17447 = CARTESIAN_POINT('Ctrl Pts',(-18.4580268902977,12.9090512631897,122.600869058419)) ;
#17448 = CARTESIAN_POINT('Ctrl Pts',(-18.4580391731387,12.909052132422,122.600854650769)) ;
#17449 = CARTESIAN_POINT('Ctrl Pts',(-18.4580637922039,12.9090538746233,122.60082577418)) ;
#17450 = CARTESIAN_POINT('Ctrl Pts',(-18.4580761288096,12.909054747619,122.600811304799)) ;
#17451 = CARTESIAN_POINT('Ctrl Pts',(-18.4581008560335,12.9090564973912,122.600782304028)) ;
#17452 = CARTESIAN_POINT('Ctrl Pts',(-18.4581132470015,12.9090573741923,122.600767772233)) ;
#17453 = CARTESIAN_POINT('Ctrl Pts',(-18.458138084327,12.9090591316718,122.600738645035)) ;
#17454 = CARTESIAN_POINT('Ctrl Pts',(-18.4581505306124,12.9090600123451,122.600724049723)) ;
#17455 = CARTESIAN_POINT('Ctrl Pts',(-18.4581754788481,12.9090617775882,122.600694795187)) ;
#17456 = CARTESIAN_POINT('Ctrl Pts',(-18.4581879809698,12.90906266217,122.600680135768)) ;
#17457 = CARTESIAN_POINT('Ctrl Pts',(-18.4582130421042,12.9090644353161,122.600650751598)) ;
#17458 = CARTESIAN_POINT('Ctrl Pts',(-18.4582256008775,12.9090653238634,122.600636027134)) ;
#17459 = CARTESIAN_POINT('Ctrl Pts',(-18.4582507766476,12.9090671050344,122.60060651133)) ;
#17460 = CARTESIAN_POINT('Ctrl Pts',(-18.4582633931829,12.9090679976252,122.600591720538)) ;
#17461 = CARTESIAN_POINT('Ctrl Pts',(-18.4582886840692,12.9090697868538,122.600562072575)) ;
#17462 = CARTESIAN_POINT('Ctrl Pts',(-18.4583013588228,12.9090706835199,122.600547214938)) ;
#17463 = CARTESIAN_POINT('Ctrl Pts',(-18.4583267667073,12.9090724809382,122.600517432648)) ;
#17464 = CARTESIAN_POINT('Ctrl Pts',(-18.4583395001851,12.9090733817147,122.600502507594)) ;
#17465 = CARTESIAN_POINT('Ctrl Pts',(-18.4583650277375,12.9090751875102,122.600472587887)) ;
#17466 = CARTESIAN_POINT('Ctrl Pts',(-18.4583778212882,12.9090760924919,122.600457593854)) ;
#17467 = CARTESIAN_POINT('Ctrl Pts',(-18.4584034682777,12.9090779066471,122.600427537039)) ;
#17468 = CARTESIAN_POINT('Ctrl Pts',(-18.4584163220759,12.9090788158458,122.600412473842)) ;
#17469 = CARTESIAN_POINT('Ctrl Pts',(-18.4584420920024,12.9090806386071,122.600382275859)) ;
#17470 = CARTESIAN_POINT('Ctrl Pts',(-18.4584550075113,12.9090815521256,122.600367141805)) ;
#17471 = CARTESIAN_POINT('Ctrl Pts',(-18.4584808999983,12.909083383465,122.600336803135)) ;
#17472 = CARTESIAN_POINT('Ctrl Pts',(-18.4584938774174,12.9090843013168,122.60032159801)) ;
#17473 = CARTESIAN_POINT('Ctrl Pts',(-18.4585198958153,12.90908614147,122.600291114771)) ;
#17474 = CARTESIAN_POINT('Ctrl Pts',(-18.4585329364719,12.9090870637484,122.600275837041)) ;
#17475 = CARTESIAN_POINT('Ctrl Pts',(-18.4585590810185,12.9090889127309,122.600245208995)) ;
#17476 = CARTESIAN_POINT('Ctrl Pts',(-18.4585721853996,12.9090898394696,122.600229858111)) ;
#17477 = CARTESIAN_POINT('Ctrl Pts',(-18.4585984582777,12.9090916974344,122.600199082746)) ;
#17478 = CARTESIAN_POINT('Ctrl Pts',(-18.4586116270783,12.9090926286819,122.600183657916)) ;
#17479 = CARTESIAN_POINT('Ctrl Pts',(-18.4586380302734,12.9090944957681,122.600152732949)) ;
#17480 = CARTESIAN_POINT('Ctrl Pts',(-18.4586512643879,12.9090954315869,122.600137233148)) ;
#17481 = CARTESIAN_POINT('Ctrl Pts',(-18.4586778000525,12.9090973079453,122.600106156103)) ;
#17482 = CARTESIAN_POINT('Ctrl Pts',(-18.4586911009341,12.9090982484375,122.600090579651)) ;
#17483 = CARTESIAN_POINT('Ctrl Pts',(-18.4587177686679,12.9091001340384,122.600059351043)) ;
#17484 = CARTESIAN_POINT('Ctrl Pts',(-18.4587311362994,12.9091010792021,122.600043697983)) ;
#17485 = CARTESIAN_POINT('Ctrl Pts',(-18.4587579402238,12.9091029743355,122.600012313033)) ;
#17486 = CARTESIAN_POINT('Ctrl Pts',(-18.4587713761281,12.9091039242776,122.599996581605)) ;
#17487 = CARTESIAN_POINT('Ctrl Pts',(-18.4587983161713,12.9091058289369,122.599965040444)) ;
#17488 = CARTESIAN_POINT('Ctrl Pts',(-18.4588118207581,12.9091067836856,122.599949230193)) ;
#17489 = CARTESIAN_POINT('Ctrl Pts',(-18.4588388997442,12.9091086980691,122.599917529561)) ;
#17490 = CARTESIAN_POINT('Ctrl Pts',(-18.4588524740382,12.9091096576961,122.599901639312)) ;
#17491 = CARTESIAN_POINT('Ctrl Pts',(-18.4588796934132,12.9091115819044,122.599869777567)) ;
#17492 = CARTESIAN_POINT('Ctrl Pts',(-18.4588933382743,12.9091125464698,122.599853806338)) ;
#17493 = CARTESIAN_POINT('Ctrl Pts',(-18.4589207003143,12.9091144806623,122.599821780865)) ;
#17494 = CARTESIAN_POINT('Ctrl Pts',(-18.458934417088,12.9091154502604,122.599805727105)) ;
#17495 = CARTESIAN_POINT('Ctrl Pts',(-18.4589619220333,12.9091173944524,122.599773537675)) ;
#17496 = CARTESIAN_POINT('Ctrl Pts',(-18.4589757109707,12.9091183691002,122.599757401116)) ;
#17497 = CARTESIAN_POINT('Ctrl Pts',(-18.4590033621648,12.9091203235266,122.599725043866)) ;
#17498 = CARTESIAN_POINT('Ctrl Pts',(-18.4590172243706,12.9091213033013,122.599708823243)) ;
#17499 = CARTESIAN_POINT('Ctrl Pts',(-18.4590450235525,12.9091232680833,122.599676296191)) ;
#17500 = CARTESIAN_POINT('Ctrl Pts',(-18.4590589602244,12.9091242530688,122.599659990128)) ;
#17501 = CARTESIAN_POINT('Ctrl Pts',(-18.4590869084532,12.9091262282796,122.599627292089)) ;
#17502 = CARTESIAN_POINT('Ctrl Pts',(-18.4591009202929,12.9091272185246,122.599610899792)) ;
#17503 = CARTESIAN_POINT('Ctrl Pts',(-18.4591290198551,12.9091292043242,122.599578028145)) ;
#17504 = CARTESIAN_POINT('Ctrl Pts',(-18.4591431077237,12.9091301998887,122.599561548634)) ;
#17505 = CARTESIAN_POINT('Ctrl Pts',(-18.4591713608469,12.9091321964327,122.599528500829)) ;
#17506 = CARTESIAN_POINT('Ctrl Pts',(-18.4591855258646,12.9091331973951,122.599511932822)) ;
#17507 = CARTESIAN_POINT('Ctrl Pts',(-18.4592139342817,12.9091352048042,122.599478706888)) ;
#17508 = CARTESIAN_POINT('Ctrl Pts',(-18.4592281775396,12.9091362112407,122.599462049137)) ;
#17509 = CARTESIAN_POINT('Ctrl Pts',(-18.459256742632,12.9091382296108,122.599428643517)) ;
#17510 = CARTESIAN_POINT('Ctrl Pts',(-18.4592710648103,12.9091392415685,122.599411895256)) ;
#17511 = CARTESIAN_POINT('Ctrl Pts',(-18.4592997893301,12.9091412710922,122.599378306789)) ;
#17512 = CARTESIAN_POINT('Ctrl Pts',(-18.459314191593,12.9091422886525,122.599361466685)) ;
#17513 = CARTESIAN_POINT('Ctrl Pts',(-18.4593430770686,12.909144329436,122.599327693644)) ;
#17514 = CARTESIAN_POINT('Ctrl Pts',(-18.4593575603095,12.909145352661,122.599310760684)) ;
#17515 = CARTESIAN_POINT('Ctrl Pts',(-18.4593866090798,12.9091474048677,122.599276800394)) ;
#17516 = CARTESIAN_POINT('Ctrl Pts',(-18.4594011744278,12.9091484338363,122.599259773288)) ;
#17517 = CARTESIAN_POINT('Ctrl Pts',(-18.4594303883272,12.9091504975939,122.599225623668)) ;
#17518 = CARTESIAN_POINT('Ctrl Pts',(-18.459445036834,12.9091515323793,122.599208501217)) ;
#17519 = CARTESIAN_POINT('Ctrl Pts',(-18.4594744175564,12.9091536078055,122.599174160349)) ;
#17520 = CARTESIAN_POINT('Ctrl Pts',(-18.4594891499515,12.9091546484584,122.599156941732)) ;
#17521 = CARTESIAN_POINT('Ctrl Pts',(-18.4595187004174,12.9091567357574,122.599122406267)) ;
#17522 = CARTESIAN_POINT('Ctrl Pts',(-18.4595335179825,12.9091577823674,122.599105090019)) ;
#17523 = CARTESIAN_POINT('Ctrl Pts',(-18.45956324037,12.9091598816911,122.599070357476)) ;
#17524 = CARTESIAN_POINT('Ctrl Pts',(-18.4595781446964,12.9091609343695,122.59905294177)) ;
#17525 = CARTESIAN_POINT('Ctrl Pts',(-18.4596080389952,12.9091630457151,122.599018012227)) ;
#17526 = CARTESIAN_POINT('Ctrl Pts',(-18.4596230301123,12.9091641044629,122.599000497063)) ;
#17527 = CARTESIAN_POINT('Ctrl Pts',(-18.4596531011768,12.9091662281713,122.598965364916)) ;
#17528 = CARTESIAN_POINT('Ctrl Pts',(-18.4596681807437,12.9091672931047,122.598947748389)) ;
#17529 = CARTESIAN_POINT('Ctrl Pts',(-18.4596984295507,12.9091694292426,122.598912412566)) ;
#17530 = CARTESIAN_POINT('Ctrl Pts',(-18.4597135986353,12.9091705004358,122.598894693463)) ;
#17531 = CARTESIAN_POINT('Ctrl Pts',(-18.459744027297,12.9091726491504,122.598859151566)) ;
#17532 = CARTESIAN_POINT('Ctrl Pts',(-18.4597592868648,12.9091737266706,122.598841328795)) ;
#17533 = CARTESIAN_POINT('Ctrl Pts',(-18.4597898983033,12.9091758881658,122.598805577483)) ;
#17534 = CARTESIAN_POINT('Ctrl Pts',(-18.459805249875,12.9091769721193,122.598787649303)) ;
#17535 = CARTESIAN_POINT('Ctrl Pts',(-18.459836044968,12.909179146455,122.598751687623)) ;
#17536 = CARTESIAN_POINT('Ctrl Pts',(-18.4598514891151,12.9091802368809,122.598733653404)) ;
#17537 = CARTESIAN_POINT('Ctrl Pts',(-18.4598824715749,12.9091824243169,122.598697477095)) ;
#17538 = CARTESIAN_POINT('Ctrl Pts',(-18.4598980097247,12.9091835213149,122.598679335208)) ;
#17539 = CARTESIAN_POINT('Ctrl Pts',(-18.4599291813399,12.9091857219751,122.598642942256)) ;
#17540 = CARTESIAN_POINT('Ctrl Pts',(-18.4599448147177,12.9091868256306,122.598624691308)) ;
#17541 = CARTESIAN_POINT('Ctrl Pts',(-18.4599761776266,12.9091890396635,122.598588079295)) ;
#17542 = CARTESIAN_POINT('Ctrl Pts',(-18.4599919073227,12.9091901500522,122.598569718051)) ;
#17543 = CARTESIAN_POINT('Ctrl Pts',(-18.4600234638922,12.9091923776227,122.598532884291)) ;
#17544 = CARTESIAN_POINT('Ctrl Pts',(-18.4600392909431,12.9091934948166,122.598514411581)) ;
#17545 = CARTESIAN_POINT('Ctrl Pts',(-18.4600710442307,12.9091957361379,122.598477352586)) ;
#17546 = CARTESIAN_POINT('Ctrl Pts',(-18.4600869701876,12.9091968602452,122.59845876664)) ;
#17547 = CARTESIAN_POINT('Ctrl Pts',(-18.4601189216041,12.9091991154144,122.598421480843)) ;
#17548 = CARTESIAN_POINT('Ctrl Pts',(-18.4601349473819,12.9092002464985,122.598402780634)) ;
#17549 = CARTESIAN_POINT('Ctrl Pts',(-18.4601670999788,12.9092025157285,122.598365264557)) ;
#17550 = CARTESIAN_POINT('Ctrl Pts',(-18.4601832268061,12.9092036538747,122.598346448693)) ;
#17551 = CARTESIAN_POINT('Ctrl Pts',(-18.460215583374,12.9092059373599,122.598308699164)) ;
#17552 = CARTESIAN_POINT('Ctrl Pts',(-18.4602318127925,12.9092070826757,122.598289765889)) ;
#17553 = CARTESIAN_POINT('Ctrl Pts',(-18.4602643749783,12.9092093805296,122.598251781072)) ;
#17554 = CARTESIAN_POINT('Ctrl Pts',(-18.4602807079974,12.909210533085,122.598232729251)) ;
#17555 = CARTESIAN_POINT('Ctrl Pts',(-18.4603134788421,12.9092128455195,122.598194505686)) ;
#17556 = CARTESIAN_POINT('Ctrl Pts',(-18.4603299167182,12.9092140054018,122.598175333898)) ;
#17557 = CARTESIAN_POINT('Ctrl Pts',(-18.4603628989903,12.9092163326095,122.598136868444)) ;
#17558 = CARTESIAN_POINT('Ctrl Pts',(-18.4603794431861,12.9092174999204,122.598117575028)) ;
#17559 = CARTESIAN_POINT('Ctrl Pts',(-18.4604126391193,12.9092198420563,122.598078865172)) ;
#17560 = CARTESIAN_POINT('Ctrl Pts',(-18.4604292909056,12.9092210168841,122.598059448691)) ;
#17561 = CARTESIAN_POINT('Ctrl Pts',(-18.4604627030195,12.9092233741229,122.598020491586)) ;
#17562 = CARTESIAN_POINT('Ctrl Pts',(-18.4604794635528,12.9092245565479,122.598000950738)) ;
#17563 = CARTESIAN_POINT('Ctrl Pts',(-18.4605130950949,12.9092269291159,122.597961742691)) ;
#17564 = CARTESIAN_POINT('Ctrl Pts',(-18.4605299659331,12.9092281192464,122.597942075708)) ;
#17565 = CARTESIAN_POINT('Ctrl Pts',(-18.4605638189522,12.9092305072852,122.597902614427)) ;
#17566 = CARTESIAN_POINT('Ctrl Pts',(-18.4605808012713,12.9092317052027,122.597882819985)) ;
#17567 = CARTESIAN_POINT('Ctrl Pts',(-18.4606148789107,12.909234108931,122.597843101903)) ;
#17568 = CARTESIAN_POINT('Ctrl Pts',(-18.4606319741094,12.9092353147327,122.597823178422)) ;
#17569 = CARTESIAN_POINT('Ctrl Pts',(-18.4606662793476,12.9092377343575,122.597783200167)) ;
#17570 = CARTESIAN_POINT('Ctrl Pts',(-18.460683489093,12.9092389481594,122.597763145753)) ;
#17571 = CARTESIAN_POINT('Ctrl Pts',(-18.4607180237009,12.9092413838026,122.597722905362)) ;
#17572 = CARTESIAN_POINT('Ctrl Pts',(-18.4607353489293,12.9092426056691,122.597702718976)) ;
#17573 = CARTESIAN_POINT('Ctrl Pts',(-18.4607701171478,12.9092450576265,122.597662211611)) ;
#17574 = CARTESIAN_POINT('Ctrl Pts',(-18.4607875597353,12.9092462876885,122.597641891119)) ;
#17575 = CARTESIAN_POINT('Ctrl Pts',(-18.4608225632399,12.909248756075,122.597601114933)) ;
#17576 = CARTESIAN_POINT('Ctrl Pts',(-18.4608401243544,12.9092499944131,122.597580659026)) ;
#17577 = CARTESIAN_POINT('Ctrl Pts',(-18.4608753667552,12.9092524794801,122.59753960992)) ;
#17578 = CARTESIAN_POINT('Ctrl Pts',(-18.4608930480052,12.909253726206,122.59751901678)) ;
#17579 = CARTESIAN_POINT('Ctrl Pts',(-18.460928531824,12.9092562281279,122.597477691926)) ;
#17580 = CARTESIAN_POINT('Ctrl Pts',(-18.4609463345614,12.9092574833353,122.597456960033)) ;
#17581 = CARTESIAN_POINT('Ctrl Pts',(-18.4609820631147,12.9092600023425,122.597415355679)) ;
#17582 = CARTESIAN_POINT('Ctrl Pts',(-18.4609999889301,12.9092612661418,122.597394483237)) ;
#17583 = CARTESIAN_POINT('Ctrl Pts',(-18.4610359650053,12.9092638024274,122.597352596251)) ;
#17584 = CARTESIAN_POINT('Ctrl Pts',(-18.4610540153673,12.9092650749203,122.597331581607)) ;
#17585 = CARTESIAN_POINT('Ctrl Pts',(-18.4610902420817,12.9092676287005,122.597289408474)) ;
#17586 = CARTESIAN_POINT('Ctrl Pts',(-18.4611084184928,12.9092689099912,122.597268249937)) ;
#17587 = CARTESIAN_POINT('Ctrl Pts',(-18.4611448989465,12.9092714814809,122.597225787166)) ;
#17588 = CARTESIAN_POINT('Ctrl Pts',(-18.4611632029019,12.909272771673,122.597204483055)) ;
#17589 = CARTESIAN_POINT('Ctrl Pts',(-18.4611999407044,12.9092753611229,122.597161726565)) ;
#17590 = CARTESIAN_POINT('Ctrl Pts',(-18.461218374137,12.9092766603507,122.59714027469)) ;
#17591 = CARTESIAN_POINT('Ctrl Pts',(-18.4612553713637,12.9092792679033,122.597097222188)) ;
#17592 = CARTESIAN_POINT('Ctrl Pts',(-18.4612739354962,12.9092805762512,122.597075621188)) ;
#17593 = CARTESIAN_POINT('Ctrl Pts',(-18.4613111963032,12.9092832021956,122.597032267961)) ;
#17594 = CARTESIAN_POINT('Ctrl Pts',(-18.4613298929496,12.9092845197895,122.597010515788)) ;
#17595 = CARTESIAN_POINT('Ctrl Pts',(-18.4613674200902,12.9092871643158,122.59696685876)) ;
#17596 = CARTESIAN_POINT('Ctrl Pts',(-18.4613862507815,12.9092884912615,122.596944953698)) ;
#17597 = CARTESIAN_POINT('Ctrl Pts',(-18.4614240476814,12.9092911546072,122.596900989013)) ;
#17598 = CARTESIAN_POINT('Ctrl Pts',(-18.4614430139965,12.909292491014,122.596878929289)) ;
#17599 = CARTESIAN_POINT('Ctrl Pts',(-18.4614810843628,12.9092951734362,122.596834652767)) ;
#17600 = CARTESIAN_POINT('Ctrl Pts',(-18.4615001881808,12.9092965194344,122.596812436262)) ;
#17601 = CARTESIAN_POINT('Ctrl Pts',(-18.4615385348547,12.9092992211292,122.596767844733)) ;
#17602 = CARTESIAN_POINT('Ctrl Pts',(-18.4615577777627,12.9093005768286,122.596745469671)) ;
#17603 = CARTESIAN_POINT('Ctrl Pts',(-18.4615964045957,12.9093032980631,122.596700558792)) ;
#17604 = CARTESIAN_POINT('Ctrl Pts',(-18.4616157885023,12.909304663596,122.596678023022)) ;
#17605 = CARTESIAN_POINT('Ctrl Pts',(-18.4616546980943,12.909307404549,122.596632789911)) ;
#17606 = CARTESIAN_POINT('Ctrl Pts',(-18.4616742242616,12.9093087800022,122.596610092035)) ;
#17607 = CARTESIAN_POINT('Ctrl Pts',(-18.4617134215183,12.9093115410149,122.596564531132)) ;
#17608 = CARTESIAN_POINT('Ctrl Pts',(-18.4617330921166,12.9093129265391,122.5965416687)) ;
#17609 = CARTESIAN_POINT('Ctrl Pts',(-18.4674875411176,12.9097182335068,122.589853968253)) ;
#17610 = CARTESIAN_POINT('Ctrl Pts',(-18.473292462641,12.9101227053002,122.583249842278)) ;
#17611 = CARTESIAN_POINT('Ctrl Pts',(-18.4872082049094,12.9110821196766,122.567751093745)) ;
#17612 = CARTESIAN_POINT('Ctrl Pts',(-18.495378772698,12.9116374674313,122.558911311203)) ;
#17613 = CARTESIAN_POINT('Ctrl Pts',(-18.5255320502739,12.9136583732359,122.527219155736)) ;
#17614 = CARTESIAN_POINT('Ctrl Pts',(-18.5482545240481,12.9151279126444,122.505087344132)) ;
#17615 = CARTESIAN_POINT('Ctrl Pts',(-18.5834615782862,12.9173213746547,122.473313552973)) ;
#17616 = CARTESIAN_POINT('Ctrl Pts',(-18.5953270213179,12.9180472819376,122.463004474182)) ;
#17617 = CARTESIAN_POINT('Ctrl Pts',(-18.6111133294123,12.9189944941176,122.449802933513)) ;
#17618 = CARTESIAN_POINT('Ctrl Pts',(-18.6148610700442,12.9192180186811,122.44670580419)) ;
#17619 = CARTESIAN_POINT('Ctrl Pts',(-18.6199527977924,12.9195198879582,122.442547759573)) ;
#17620 = CARTESIAN_POINT('Ctrl Pts',(-18.6212810162356,12.9195984690759,122.441467640624)) ;
#17621 = CARTESIAN_POINT('Ctrl Pts',(-18.623556650964,12.9197328262149,122.439624828017)) ;
#17622 = CARTESIAN_POINT('Ctrl Pts',(-18.6245029685735,12.9197886170874,122.43886078271)) ;
#17623 = CARTESIAN_POINT('Ctrl Pts',(-18.6276810450864,12.9199757136843,122.436302495557)) ;
#17624 = CARTESIAN_POINT('Ctrl Pts',(-18.6299178563148,12.9201069525261,122.434514539952)) ;
#17625 = CARTESIAN_POINT('Ctrl Pts',(-18.6356317807976,12.9204411004961,122.429979307164)) ;
#17626 = CARTESIAN_POINT('Ctrl Pts',(-18.6391173987332,12.9206439058288,122.427242802604)) ;
#17627 = CARTESIAN_POINT('Ctrl Pts',(-18.6544951624273,12.9215342969607,122.415301588195)) ;
#17628 = CARTESIAN_POINT('Ctrl Pts',(-18.6665383447217,12.9222202964339,122.406293348238)) ;
#17629 = CARTESIAN_POINT('Ctrl Pts',(-18.7059019576485,12.9244311582386,122.377942697902)) ;
#17630 = CARTESIAN_POINT('Ctrl Pts',(-18.7338374985042,12.9259529893569,122.359479681101)) ;
#17631 = CARTESIAN_POINT('Ctrl Pts',(-18.7750620373161,12.9281503928211,122.334552279372)) ;
#17632 = CARTESIAN_POINT('Ctrl Pts',(-18.7877770182112,12.9288217515954,122.327167017206)) ;
#17633 = CARTESIAN_POINT('Ctrl Pts',(-18.8072714322977,12.9298425449056,122.316299402806)) ;
#17634 = CARTESIAN_POINT('Ctrl Pts',(-18.8139573259136,12.930191145774,122.312651884988)) ;
#17635 = CARTESIAN_POINT('Ctrl Pts',(-18.8259528867814,12.9308140718044,122.30624921072)) ;
#17636 = CARTESIAN_POINT('Ctrl Pts',(-18.8312497904658,12.9310882719835,122.303470634121)) ;
#17637 = CARTESIAN_POINT('Ctrl Pts',(-18.8366485738281,12.9313669002543,122.300687843529)) ;
#17638 = CARTESIAN_POINT('Ctrl Pts',(-18.8367307270997,12.9313711399417,122.300645509344)) ;
#17639 = CARTESIAN_POINT('Ctrl Pts',(-18.8368947521112,12.931379604392,122.300561009068)) ;
#17640 = CARTESIAN_POINT('Ctrl Pts',(-18.8369766237777,12.9313838291524,122.300518842934)) ;
#17641 = CARTESIAN_POINT('Ctrl Pts',(-18.837140121316,12.9313922655971,122.300434660116)) ;
#17642 = CARTESIAN_POINT('Ctrl Pts',(-18.8372217471904,12.9313964772827,122.30039264336)) ;
#17643 = CARTESIAN_POINT('Ctrl Pts',(-18.8373847881378,12.9314048893872,122.300308741077)) ;
#17644 = CARTESIAN_POINT('Ctrl Pts',(-18.837466203088,12.9314090898007,122.300266855552)) ;
#17645 = CARTESIAN_POINT('Ctrl Pts',(-18.8376288558034,12.9314174810986,122.300183198257)) ;
#17646 = CARTESIAN_POINT('Ctrl Pts',(-18.8377100935985,12.9314216719854,122.300141426421)) ;
#17647 = CARTESIAN_POINT('Ctrl Pts',(-18.8378724244463,12.9314300459062,122.300057979671)) ;
#17648 = CARTESIAN_POINT('Ctrl Pts',(-18.8379535176861,12.9314342289506,122.300016304618)) ;
#17649 = CARTESIAN_POINT('Ctrl Pts',(-18.8381155922966,12.9314425888847,122.29993303442)) ;
#17650 = CARTESIAN_POINT('Ctrl Pts',(-18.838196573277,12.9314467657548,122.299891439441)) ;
#17651 = CARTESIAN_POINT('Ctrl Pts',(-18.8383584540782,12.931455114926,122.299808313518)) ;
#17652 = CARTESIAN_POINT('Ctrl Pts',(-18.8384393538655,12.9314592872258,122.299766782567)) ;
#17653 = CARTESIAN_POINT('Ctrl Pts',(-18.838601103016,12.931467628843,122.299683768853)) ;
#17654 = CARTESIAN_POINT('Ctrl Pts',(-18.8386819522676,12.9314717981549,122.29964228613)) ;
#17655 = CARTESIAN_POINT('Ctrl Pts',(-18.8388436296266,12.9314801353072,122.299559353803)) ;
#17656 = CARTESIAN_POINT('Ctrl Pts',(-18.8389244580086,12.9314843031619,122.29951790405)) ;
#17657 = CARTESIAN_POINT('Ctrl Pts',(-18.8390861230783,12.9314926389188,122.29943502254)) ;
#17658 = CARTESIAN_POINT('Ctrl Pts',(-18.8391669598491,12.9314968068253,122.29939359074)) ;
#17659 = CARTESIAN_POINT('Ctrl Pts',(-18.8393286708288,12.9315051441881,122.299310730208)) ;
#17660 = CARTESIAN_POINT('Ctrl Pts',(-18.83940954489,12.9315093136366,122.299269301559)) ;
#17661 = CARTESIAN_POINT('Ctrl Pts',(-18.8395713582431,12.931517655516,122.29918643312)) ;
#17662 = CARTESIAN_POINT('Ctrl Pts',(-18.8396522976801,12.931521827954,122.29914499327)) ;
#17663 = CARTESIAN_POINT('Ctrl Pts',(-18.8398142699771,12.931530177265,122.299062088046)) ;
#17664 = CARTESIAN_POINT('Ctrl Pts',(-18.8398953027382,12.9315343541325,122.299020622745)) ;
#17665 = CARTESIAN_POINT('Ctrl Pts',(-18.8400574889383,12.9315427137062,122.298937652743)) ;
#17666 = CARTESIAN_POINT('Ctrl Pts',(-18.8401386424167,12.9315468964139,122.298896148054)) ;
#17667 = CARTESIAN_POINT('Ctrl Pts',(-18.8403010971093,12.9315552690612,122.298813085534)) ;
#17668 = CARTESIAN_POINT('Ctrl Pts',(-18.8403823983439,12.9315594590012,122.298771527731)) ;
#17669 = CARTESIAN_POINT('Ctrl Pts',(-18.8405451757876,12.931567847515,122.29868834518)) ;
#17670 = CARTESIAN_POINT('Ctrl Pts',(-18.8406266518086,12.9315720460783,122.298646720574)) ;
#17671 = CARTESIAN_POINT('Ctrl Pts',(-18.8407898045557,12.9315804531624,122.298563391411)) ;
#17672 = CARTESIAN_POINT('Ctrl Pts',(-18.8408714815939,12.9315846616984,122.298521686749)) ;
#17673 = CARTESIAN_POINT('Ctrl Pts',(-18.8410350633922,12.9315930901173,122.298438183843)) ;
#17674 = CARTESIAN_POINT('Ctrl Pts',(-18.841116967973,12.93159730999,122.298396385751)) ;
#17675 = CARTESIAN_POINT('Ctrl Pts',(-18.8412810308414,12.9316057624182,122.298312682912)) ;
#17676 = CARTESIAN_POINT('Ctrl Pts',(-18.8413631890634,12.9316099949692,122.298270778265)) ;
#17677 = CARTESIAN_POINT('Ctrl Pts',(-18.8415277853316,12.931618474096,122.298186849202)) ;
#17678 = CARTESIAN_POINT('Ctrl Pts',(-18.8416102233135,12.9316227206673,122.298144824894)) ;
#17679 = CARTESIAN_POINT('Ctrl Pts',(-18.8417754043808,12.9316312291333,122.298060643852)) ;
#17680 = CARTESIAN_POINT('Ctrl Pts',(-18.841858147757,12.9316354910416,122.298018487053)) ;
#17681 = CARTESIAN_POINT('Ctrl Pts',(-18.8420239660036,12.9316440315367,122.297934027836)) ;
#17682 = CARTESIAN_POINT('Ctrl Pts',(-18.8421070407767,12.931648310117,122.297891725558)) ;
#17683 = CARTESIAN_POINT('Ctrl Pts',(-18.8422735472217,12.9316568852601,122.297806962722)) ;
#17684 = CARTESIAN_POINT('Ctrl Pts',(-18.8423569790373,12.9316611818287,122.297764502188)) ;
#17685 = CARTESIAN_POINT('Ctrl Pts',(-18.8425242254762,12.9316697942777,122.297679409955)) ;
#17686 = CARTESIAN_POINT('Ctrl Pts',(-18.8426080401333,12.9316741101582,122.297636778343)) ;
#17687 = CARTESIAN_POINT('Ctrl Pts',(-18.8427760776543,12.9316827625335,122.297551331354)) ;
#17688 = CARTESIAN_POINT('Ctrl Pts',(-18.8428603007136,12.9316870990366,122.297508515991)) ;
#17689 = CARTESIAN_POINT('Ctrl Pts',(-18.8430291814528,12.9316957940116,122.297422688417)) ;
#17690 = CARTESIAN_POINT('Ctrl Pts',(-18.8431138389162,12.9317001524703,122.297379676438)) ;
#17691 = CARTESIAN_POINT('Ctrl Pts',(-18.8432836139418,12.9317088926623,122.297293443054)) ;
#17692 = CARTESIAN_POINT('Ctrl Pts',(-18.8433687315986,12.9317132743982,122.297250221731)) ;
#17693 = CARTESIAN_POINT('Ctrl Pts',(-18.8435394526221,12.9317220624565,122.297163557048)) ;
#17694 = CARTESIAN_POINT('Ctrl Pts',(-18.843625056254,12.9317264687902,122.297120113691)) ;
#17695 = CARTESIAN_POINT('Ctrl Pts',(-18.8437967757305,12.9317353074015,122.297032991906)) ;
#17696 = CARTESIAN_POINT('Ctrl Pts',(-18.8438828915313,12.9317397396743,122.296989313646)) ;
#17697 = CARTESIAN_POINT('Ctrl Pts',(-18.8440556613335,12.931748631494,122.296901709317)) ;
#17698 = CARTESIAN_POINT('Ctrl Pts',(-18.8441423154511,12.9317530910443,122.296857783343)) ;
#17699 = CARTESIAN_POINT('Ctrl Pts',(-18.84431618814,12.9317620387624,122.296769670745)) ;
#17700 = CARTESIAN_POINT('Ctrl Pts',(-18.8444034068392,12.9317665269339,122.296725484219)) ;
#17701 = CARTESIAN_POINT('Ctrl Pts',(-18.8445784358176,12.9317755332823,122.296636837266)) ;
#17702 = CARTESIAN_POINT('Ctrl Pts',(-18.8446662459436,12.9317800514484,122.296592377089)) ;
#17703 = CARTESIAN_POINT('Ctrl Pts',(-18.8448424835274,12.9317891191021,122.296503170317)) ;
#17704 = CARTESIAN_POINT('Ctrl Pts',(-18.844930911437,12.93179366861,122.296458423674)) ;
#17705 = CARTESIAN_POINT('Ctrl Pts',(-18.8451084126807,12.9318028003837,122.2963686303)) ;
#17706 = CARTESIAN_POINT('Ctrl Pts',(-18.8451974857573,12.9318073826331,122.29632358389)) ;
#17707 = CARTESIAN_POINT('Ctrl Pts',(-18.8453283074218,12.9318141122521,122.296257443886)) ;
#17708 = CARTESIAN_POINT('Ctrl Pts',(-18.8453700518626,12.9318162595851,122.296236341932)) ;
#17709 = CARTESIAN_POINT('Ctrl Pts',(-18.845454195118,12.9318205878119,122.296193813167)) ;
#17710 = CARTESIAN_POINT('Ctrl Pts',(-18.8454965939828,12.9318227687067,122.296172386423)) ;
#17711 = CARTESIAN_POINT('Ctrl Pts',(-18.845582071843,12.9318271653772,122.29612919534)) ;
#17712 = CARTESIAN_POINT('Ctrl Pts',(-18.8456251512476,12.9318293811723,122.296107430891)) ;
#17713 = CARTESIAN_POINT('Ctrl Pts',(-18.8457120188534,12.9318338491129,122.296063550215)) ;
#17714 = CARTESIAN_POINT('Ctrl Pts',(-18.8457558066999,12.9318361012385,122.296041434268)) ;
#17715 = CARTESIAN_POINT('Ctrl Pts',(-18.8458441192737,12.9318406432791,122.295996836724)) ;
#17716 = CARTESIAN_POINT('Ctrl Pts',(-18.8458886440798,12.9318429331964,122.295974355195)) ;
#17717 = CARTESIAN_POINT('Ctrl Pts',(-18.8459784598595,12.9318475523212,122.29592901203)) ;
#17718 = CARTESIAN_POINT('Ctrl Pts',(-18.8460237511192,12.9318498815415,122.295906150365)) ;
#17719 = CARTESIAN_POINT('Ctrl Pts',(-18.8461151315823,12.9318545809005,122.295860031236)) ;
#17720 = CARTESIAN_POINT('Ctrl Pts',(-18.8461612205627,12.9318569510258,122.295836774008)) ;
#17721 = CARTESIAN_POINT('Ctrl Pts',(-18.8462542277535,12.9318617337975,122.295789848339)) ;
#17722 = CARTESIAN_POINT('Ctrl Pts',(-18.8463011462655,12.9318641464572,122.295766179875)) ;
#17723 = CARTESIAN_POINT('Ctrl Pts',(-18.8463958472504,12.9318690160772,122.295718414605)) ;
#17724 = CARTESIAN_POINT('Ctrl Pts',(-18.8464436293148,12.9318714730142,122.295694318142)) ;
#17725 = CARTESIAN_POINT('Ctrl Pts',(-18.846540091158,12.9318764329172,122.295645680271)) ;
#17726 = CARTESIAN_POINT('Ctrl Pts',(-18.8465887713337,12.9318789359012,122.295621138807)) ;
#17727 = CARTESIAN_POINT('Ctrl Pts',(-18.8466870664997,12.9318839897986,122.295571592669)) ;
#17728 = CARTESIAN_POINT('Ctrl Pts',(-18.8467366814487,12.9318865407072,122.29554658817)) ;
#17729 = CARTESIAN_POINT('Ctrl Pts',(-18.8468368836946,12.9318916923757,122.295496097515)) ;
#17730 = CARTESIAN_POINT('Ctrl Pts',(-18.8468874712014,12.9318942931435,122.295470611416)) ;
#17731 = CARTESIAN_POINT('Ctrl Pts',(-18.8469896591545,12.931899546609,122.295419137605)) ;
#17732 = CARTESIAN_POINT('Ctrl Pts',(-18.8470412593468,12.9319021992906,122.295393150196)) ;
#17733 = CARTESIAN_POINT('Ctrl Pts',(-18.847145512571,12.931907558626,122.295340654195)) ;
#17734 = CARTESIAN_POINT('Ctrl Pts',(-18.8471981662542,12.9319102653101,122.295314145461)) ;
#17735 = CARTESIAN_POINT('Ctrl Pts',(-18.8473045713181,12.9319157349471,122.295260584787)) ;
#17736 = CARTESIAN_POINT('Ctrl Pts',(-18.8473583223143,12.9319184978769,122.295233533236)) ;
#17737 = CARTESIAN_POINT('Ctrl Pts',(-18.847466966332,12.9319240822737,122.295178865213)) ;
#17738 = CARTESIAN_POINT('Ctrl Pts',(-18.847521859613,12.9319269037506,122.295151248819)) ;
#17739 = CARTESIAN_POINT('Ctrl Pts',(-18.8476328359797,12.931932607687,122.295095427702)) ;
#17740 = CARTESIAN_POINT('Ctrl Pts',(-18.8476889190898,12.931935490144,122.295067223189)) ;
#17741 = CARTESIAN_POINT('Ctrl Pts',(-18.8478023237632,12.9319413185296,122.295010202041)) ;
#17742 = CARTESIAN_POINT('Ctrl Pts',(-18.8478596458301,12.9319442644802,122.294981385388)) ;
#17743 = CARTESIAN_POINT('Ctrl Pts',(-18.8479755811761,12.9319502225524,122.294923114152)) ;
#17744 = CARTESIAN_POINT('Ctrl Pts',(-18.8480341942732,12.9319532346606,122.294893659911)) ;
#17745 = CARTESIAN_POINT('Ctrl Pts',(-18.8481527658151,12.9319593278172,122.294834087056)) ;
#17746 = CARTESIAN_POINT('Ctrl Pts',(-18.8482127241924,12.9319624088578,122.294803968743)) ;
#17747 = CARTESIAN_POINT('Ctrl Pts',(-18.8483340431089,12.9319686427852,122.294743040015)) ;
#17748 = CARTESIAN_POINT('Ctrl Pts',(-18.8483954036568,12.9319717956678,122.29471222988)) ;
#17749 = CARTESIAN_POINT('Ctrl Pts',(-18.8485195862066,12.9319781763113,122.294649888603)) ;
#17750 = CARTESIAN_POINT('Ctrl Pts',(-18.8485824084158,12.9319814040778,122.294618357659)) ;
#17751 = CARTESIAN_POINT('Ctrl Pts',(-18.8487095769781,12.9319879376948,122.294554544222)) ;
#17752 = CARTESIAN_POINT('Ctrl Pts',(-18.848773923437,12.9319912435453,122.294522261999)) ;
#17753 = CARTESIAN_POINT('Ctrl Pts',(-18.8489042056603,12.9319979366616,122.294456914295)) ;
#17754 = CARTESIAN_POINT('Ctrl Pts',(-18.8489701417443,12.9320013239379,122.294423849)) ;
#17755 = CARTESIAN_POINT('Ctrl Pts',(-18.8491036725522,12.9320081834502,122.294356901436)) ;
#17756 = CARTESIAN_POINT('Ctrl Pts',(-18.8491712672356,12.9320116556778,122.294323019558)) ;
#17757 = CARTESIAN_POINT('Ctrl Pts',(-18.8493081872479,12.9320186887725,122.294254403857)) ;
#17758 = CARTESIAN_POINT('Ctrl Pts',(-18.8493775127453,12.9320222496417,122.294219670347)) ;
#17759 = CARTESIAN_POINT('Ctrl Pts',(-18.8495179701918,12.9320294638932,122.294149314607)) ;
#17760 = CARTESIAN_POINT('Ctrl Pts',(-18.8495891023662,12.93203311728,122.294113692688)) ;
#17761 = CARTESIAN_POINT('Ctrl Pts',(-18.849733252841,12.9320405206374,122.294041521519)) ;
#17762 = CARTESIAN_POINT('Ctrl Pts',(-18.84980627137,12.9320442706121,122.294004972608)) ;
#17763 = CARTESIAN_POINT('Ctrl Pts',(-18.8499542789408,12.9320518714562,122.293930906596)) ;
#17764 = CARTESIAN_POINT('Ctrl Pts',(-18.8500292679488,12.9320557223156,122.293893389999)) ;
#17765 = CARTESIAN_POINT('Ctrl Pts',(-18.8501813037246,12.9320635293847,122.293817346445)) ;
#17766 = CARTESIAN_POINT('Ctrl Pts',(-18.8502583510448,12.932067485614,122.293778819734)) ;
#17767 = CARTESIAN_POINT('Ctrl Pts',(-18.8504145971473,12.9320755082078,122.293700710685)) ;
#17768 = CARTESIAN_POINT('Ctrl Pts',(-18.8504937958913,12.9320795745609,122.293661128928)) ;
#17769 = CARTESIAN_POINT('Ctrl Pts',(-18.8506544420563,12.9320878223653,122.293580862905)) ;
#17770 = CARTESIAN_POINT('Ctrl Pts',(-18.8507358897974,12.9320920038229,122.293540179083)) ;
#17771 = CARTESIAN_POINT('Ctrl Pts',(-18.8509011369854,12.9321004870952,122.293457659299)) ;
#17772 = CARTESIAN_POINT('Ctrl Pts',(-18.8509849366996,12.9321047889128,122.293415823852)) ;
#17773 = CARTESIAN_POINT('Ctrl Pts',(-18.8511549958087,12.9321135184149,122.293330948885)) ;
#17774 = CARTESIAN_POINT('Ctrl Pts',(-18.8512412556717,12.9321179461119,122.29328790983)) ;
#17775 = CARTESIAN_POINT('Ctrl Pts',(-18.8514163501207,12.9321269332427,122.293200572365)) ;
#17776 = CARTESIAN_POINT('Ctrl Pts',(-18.8515051846889,12.932131492663,122.293156274718)) ;
#17777 = CARTESIAN_POINT('Ctrl Pts',(-18.8516855484862,12.9321407493585,122.293066362546)) ;
#17778 = CARTESIAN_POINT('Ctrl Pts',(-18.8517770781079,12.9321454466401,122.293020748638)) ;
#17779 = CARTESIAN_POINT('Ctrl Pts',(-18.851962958982,12.9321549855332,122.292928143131)) ;
#17780 = CARTESIAN_POINT('Ctrl Pts',(-18.8520573107043,12.9321598271542,122.292881152174)) ;
#17781 = CARTESIAN_POINT('Ctrl Pts',(-18.8522489698198,12.93216966156,122.292785728469)) ;
#17782 = CARTESIAN_POINT('Ctrl Pts',(-18.8523462776524,12.9321746543516,122.292737296447)) ;
#17783 = CARTESIAN_POINT('Ctrl Pts',(-18.8525439910054,12.9321847983378,122.292638922798)) ;
#17784 = CARTESIAN_POINT('Ctrl Pts',(-18.8526443967264,12.9321899495258,122.292588982091)) ;
#17785 = CARTESIAN_POINT('Ctrl Pts',(-18.8528484545785,12.9322004178831,122.292487520199)) ;
#17786 = CARTESIAN_POINT('Ctrl Pts',(-18.8529521074033,12.9322057350698,122.292435999771)) ;
#17787 = CARTESIAN_POINT('Ctrl Pts',(-18.853162817694,12.932216543486,122.292331303142)) ;
#17788 = CARTESIAN_POINT('Ctrl Pts',(-18.8532698755792,12.9322220347172,122.292278127926)) ;
#17789 = CARTESIAN_POINT('Ctrl Pts',(-18.8534875630272,12.9322331997299,122.292170042383)) ;
#17790 = CARTESIAN_POINT('Ctrl Pts',(-18.8535981929083,12.9322388735062,122.292115133191)) ;
#17791 = CARTESIAN_POINT('Ctrl Pts',(-18.8538232005821,12.9322504125824,122.292003496157)) ;
#17792 = CARTESIAN_POINT('Ctrl Pts',(-18.8539375788908,12.9322562778855,122.291946769461)) ;
#17793 = CARTESIAN_POINT('Ctrl Pts',(-18.8541702693955,12.9322682094813,122.291831409446)) ;
#17794 = CARTESIAN_POINT('Ctrl Pts',(-18.8542885824548,12.9322742757931,122.29177277722)) ;
#17795 = CARTESIAN_POINT('Ctrl Pts',(-18.8545293401758,12.9322866194675,122.29165351279)) ;
#17796 = CARTESIAN_POINT('Ctrl Pts',(-18.8546517854035,12.9322928968316,122.291592881956)) ;
#17797 = CARTESIAN_POINT('Ctrl Pts',(-18.8549010162086,12.9323056732292,122.291469521972)) ;
#17798 = CARTESIAN_POINT('Ctrl Pts',(-18.8550278024044,12.9323121722647,122.29140679431)) ;
#17799 = CARTESIAN_POINT('Ctrl Pts',(-18.8552859360825,12.9323254032399,122.291279136819)) ;
#17800 = CARTESIAN_POINT('Ctrl Pts',(-18.8554172842975,12.9323321351848,122.291214208582)) ;
#17801 = CARTESIAN_POINT('Ctrl Pts',(-18.8556847757652,12.9323458438613,122.291082040335)) ;
#17802 = CARTESIAN_POINT('Ctrl Pts',(-18.8558209199634,12.932352820606,122.291014801985)) ;
#17803 = CARTESIAN_POINT('Ctrl Pts',(-18.8560982512303,12.9323670314755,122.290877897584)) ;
#17804 = CARTESIAN_POINT('Ctrl Pts',(-18.8562394392617,12.9323742656111,122.290808233376)) ;
#17805 = CARTESIAN_POINT('Ctrl Pts',(-18.8565271208855,12.9323890046059,122.290666354694)) ;
#17806 = CARTESIAN_POINT('Ctrl Pts',(-18.856673615425,12.9323965094716,122.290594142281)) ;
#17807 = CARTESIAN_POINT('Ctrl Pts',(-18.8569721882283,12.93241180405,122.290447037766)) ;
#17808 = CARTESIAN_POINT('Ctrl Pts',(-18.8571242675855,12.9324195937729,122.290372147883)) ;
#17809 = CARTESIAN_POINT('Ctrl Pts',(-18.8574343049127,12.9324354730321,122.290219551611)) ;
#17810 = CARTESIAN_POINT('Ctrl Pts',(-18.857592264099,12.9324435625807,122.290141847635)) ;
#17811 = CARTESIAN_POINT('Ctrl Pts',(-18.8579143741494,12.9324600573732,122.289983478348)) ;
#17812 = CARTESIAN_POINT('Ctrl Pts',(-18.8580785261881,12.9324684626227,122.289902815753)) ;
#17813 = CARTESIAN_POINT('Ctrl Pts',(-18.8584133532803,12.9324856056179,122.289738376444)) ;
#17814 = CARTESIAN_POINT('Ctrl Pts',(-18.858584029907,12.9324943433845,122.289654602562)) ;
#17815 = CARTESIAN_POINT('Ctrl Pts',(-18.8589322584015,12.9325121692658,122.289483778775)) ;
#17816 = CARTESIAN_POINT('Ctrl Pts',(-18.8591098118056,12.9325212573938,122.289396732065)) ;
#17817 = CARTESIAN_POINT('Ctrl Pts',(-18.8594721673803,12.9325398029194,122.289219191528)) ;
#17818 = CARTESIAN_POINT('Ctrl Pts',(-18.8596569712518,12.9325492603327,122.289128701196)) ;
#17819 = CARTESIAN_POINT('Ctrl Pts',(-18.8600342243982,12.9325685645106,122.288944092386)) ;
#17820 = CARTESIAN_POINT('Ctrl Pts',(-18.8602266754899,12.93257841129,122.288849977767)) ;
#17821 = CARTESIAN_POINT('Ctrl Pts',(-18.8606196441781,12.9325985155088,122.288657928924)) ;
#17822 = CARTESIAN_POINT('Ctrl Pts',(-18.8608201637914,12.9326087729655,122.288559998927)) ;
#17823 = CARTESIAN_POINT('Ctrl Pts',(-18.8704120783376,12.933099389029,122.283878669612)) ;
#17824 = CARTESIAN_POINT('Ctrl Pts',(-18.8798605336001,12.9335802702349,122.279413176892)) ;
#17825 = CARTESIAN_POINT('Ctrl Pts',(-18.9068396207035,12.9349468081373,122.267073891715)) ;
#17826 = CARTESIAN_POINT('Ctrl Pts',(-18.9244973367847,12.9358334611394,122.259485168479)) ;
#17827 = CARTESIAN_POINT('Ctrl Pts',(-19.0120424708204,12.9401914228891,122.22422957043)) ;
#17828 = CARTESIAN_POINT('Ctrl Pts',(-19.084152996879,12.9436502135292,122.202497728059)) ;
#17829 = CARTESIAN_POINT('Ctrl Pts',(-19.1798876361204,12.9481446493443,122.182834225966)) ;
#17830 = CARTESIAN_POINT('Ctrl Pts',(-19.2021167447081,12.9491817115664,122.178892597979)) ;
#17831 = CARTESIAN_POINT('Ctrl Pts',(-19.2357943629815,12.9507444199954,122.173857492605)) ;
#17832 = CARTESIAN_POINT('Ctrl Pts',(-19.2471711954837,12.951270874863,122.172316465083)) ;
#17833 = CARTESIAN_POINT('Ctrl Pts',(-19.2684751569415,12.9522541226503,122.169729108203)) ;
#17834 = CARTESIAN_POINT('Ctrl Pts',(-19.2783967332762,12.9527109950239,122.168644543059)) ;
#17835 = CARTESIAN_POINT('Ctrl Pts',(-19.3008372961763,12.9537420636157,122.166463103544)) ;
#17836 = CARTESIAN_POINT('Ctrl Pts',(-19.313362005199,12.9543159331095,122.165435959296)) ;
#17837 = CARTESIAN_POINT('Ctrl Pts',(-19.3537240736603,12.9561602188178,122.162737893979)) ;
#17838 = CARTESIAN_POINT('Ctrl Pts',(-19.3816027879756,12.9574264055357,122.161809539956)) ;
#17839 = CARTESIAN_POINT('Ctrl Pts',(-19.4512552245047,12.9605698802966,122.161821642425)) ;
#17840 = CARTESIAN_POINT('Ctrl Pts',(-19.4929943814269,12.962434938441,122.16392214131)) ;
#17841 = CARTESIAN_POINT('Ctrl Pts',(-19.5589099914151,12.9654189939075,122.170561787472)) ;
#17842 = CARTESIAN_POINT('Ctrl Pts',(-19.5831921538476,12.9665262986323,122.173730662339)) ;
#17843 = CARTESIAN_POINT('Ctrl Pts',(-19.6132613713239,12.9679136321864,122.178556854359)) ;
#17844 = CARTESIAN_POINT('Ctrl Pts',(-19.6191505208534,12.968186107096,122.17954541711)) ;
#17845 = CARTESIAN_POINT('Ctrl Pts',(-19.628474040098,12.9686187602559,122.181179254851)) ;
#17846 = CARTESIAN_POINT('Ctrl Pts',(-19.6319131883064,12.9687786286577,122.181796799472)) ;
#17847 = CARTESIAN_POINT('Ctrl Pts',(-19.6383363147696,12.9690777377784,122.18297797818)) ;
#17848 = CARTESIAN_POINT('Ctrl Pts',(-19.6413209177538,12.9692169380229,122.183538082161)) ;
#17849 = CARTESIAN_POINT('Ctrl Pts',(-19.6480727531287,12.9695323353698,122.184830649697)) ;
#17850 = CARTESIAN_POINT('Ctrl Pts',(-19.6518387094439,12.9697086037091,122.185569597253)) ;
#17851 = CARTESIAN_POINT('Ctrl Pts',(-19.6628268223413,12.9702239522019,122.187778259695)) ;
#17852 = CARTESIAN_POINT('Ctrl Pts',(-19.670039430323,12.9705635458441,122.189294514544)) ;
#17853 = CARTESIAN_POINT('Ctrl Pts',(-19.7000703661138,12.9719831286628,122.195885557967)) ;
#17854 = CARTESIAN_POINT('Ctrl Pts',(-19.7227571849713,12.9730693314094,122.20153605961)) ;
#17855 = CARTESIAN_POINT('Ctrl Pts',(-19.8094878681108,12.9772723613184,122.225740049305)) ;
#17856 = CARTESIAN_POINT('Ctrl Pts',(-19.872169205209,12.9804045347924,122.248770262787)) ;
#17857 = CARTESIAN_POINT('Ctrl Pts',(-19.9534618610653,12.9845532872059,122.286256883173)) ;
#17858 = CARTESIAN_POINT('Ctrl Pts',(-19.9739433774441,12.9856084637886,122.296391346827)) ;
#17859 = CARTESIAN_POINT('Ctrl Pts',(-20.0017133809356,12.9870552141847,122.311093237271)) ;
#17860 = CARTESIAN_POINT('Ctrl Pts',(-20.0092495684584,12.987449501757,122.315182835022)) ;
#17861 = CARTESIAN_POINT('Ctrl Pts',(-20.0221058496954,12.9881251632742,122.322331639189)) ;
#17862 = CARTESIAN_POINT('Ctrl Pts',(-20.0274465779288,12.9884067549695,122.325353076606)) ;
#17863 = CARTESIAN_POINT('Ctrl Pts',(-20.0379365902499,12.9889617089518,122.331390035552)) ;
#17864 = CARTESIAN_POINT('Ctrl Pts',(-20.0430869601818,12.9892350770928,122.33440334889)) ;
#17865 = CARTESIAN_POINT('Ctrl Pts',(-20.0535780213267,12.9897938183034,122.340642586843)) ;
#17866 = CARTESIAN_POINT('Ctrl Pts',(-20.0589165353511,12.9900791625694,122.343871853466)) ;
#17867 = CARTESIAN_POINT('Ctrl Pts',(-20.0710288206462,12.9907289793603,122.351323005343)) ;
#17868 = CARTESIAN_POINT('Ctrl Pts',(-20.0777867885088,12.9910932811806,122.35557007748)) ;
#17869 = CARTESIAN_POINT('Ctrl Pts',(-20.0948774979195,12.9920192198657,122.366540534747)) ;
#17870 = CARTESIAN_POINT('Ctrl Pts',(-20.1051523315045,12.9925802556669,122.373352593796)) ;
#17871 = CARTESIAN_POINT('Ctrl Pts',(-20.134259171672,12.9941829003336,122.393275988063)) ;
#17872 = CARTESIAN_POINT('Ctrl Pts',(-20.1528332651535,12.9952219042424,122.406755415464)) ;
#17873 = CARTESIAN_POINT('Ctrl Pts',(-20.1953433956368,12.997642355661,122.439429249522)) ;
#17874 = CARTESIAN_POINT('Ctrl Pts',(-20.2189647590874,12.9990191712639,122.459008656394)) ;
#17875 = CARTESIAN_POINT('Ctrl Pts',(-20.2489818399481,13.0008229873648,122.48581253063)) ;
#17876 = CARTESIAN_POINT('Ctrl Pts',(-20.2560479852833,13.0012519697605,122.492269669813)) ;
#17877 = CARTESIAN_POINT('Ctrl Pts',(-20.2909306306717,13.0033940407219,122.524888971852)) ;
#17878 = CARTESIAN_POINT('Ctrl Pts',(-20.3176116774352,13.0051122985087,122.552234490449)) ;
#17879 = CARTESIAN_POINT('Ctrl Pts',(-20.3472930089684,13.007145055823,122.585582712459)) ;
#17880 = CARTESIAN_POINT('Ctrl Pts',(-20.351549669853,13.0074396586775,122.590440545582)) ;
#17881 = CARTESIAN_POINT('Ctrl Pts',(-20.3581920643393,13.007904352087,122.598140644171)) ;
#17882 = CARTESIAN_POINT('Ctrl Pts',(-20.3606031275432,13.0080740787272,122.600960926167)) ;
#17883 = CARTESIAN_POINT('Ctrl Pts',(-20.3648611428621,13.0083757119404,122.605986769328)) ;
#17884 = CARTESIAN_POINT('Ctrl Pts',(-20.3667131074318,13.0085075465504,122.608188052261)) ;
#17885 = CARTESIAN_POINT('Ctrl Pts',(-20.3704947100324,13.008778075814,122.612714569607)) ;
#17886 = CARTESIAN_POINT('Ctrl Pts',(-20.3724235485874,13.0089167805941,122.615040446887)) ;
#17887 = CARTESIAN_POINT('Ctrl Pts',(-20.3766866224998,13.0092249519798,122.620219146849)) ;
#17888 = CARTESIAN_POINT('Ctrl Pts',(-20.3790167089273,13.0093944741667,122.623075344965)) ;
#17889 = CARTESIAN_POINT('Ctrl Pts',(-20.3884700562282,13.0100866988123,122.634768384046)) ;
#17890 = CARTESIAN_POINT('Ctrl Pts',(-20.3954853887506,13.0106108313071,122.643691691344)) ;
#17891 = CARTESIAN_POINT('Ctrl Pts',(-20.4084567331962,13.0115999618398,122.660661566689)) ;
#17892 = CARTESIAN_POINT('Ctrl Pts',(-20.4144395185823,13.0120645938256,122.66868657116)) ;
#17893 = CARTESIAN_POINT('Ctrl Pts',(-20.4410931707525,13.0141729511637,122.705349275846)) ;
#17894 = CARTESIAN_POINT('Ctrl Pts',(-20.4606409254937,13.0158274690159,122.734783197618)) ;
#17895 = CARTESIAN_POINT('Ctrl Pts',(-20.491024875738,13.0185720224918,122.785029832403)) ;
#17896 = CARTESIAN_POINT('Ctrl Pts',(-20.5025692118449,13.0196619659135,122.805390942654)) ;
#17897 = CARTESIAN_POINT('Ctrl Pts',(-20.5240951216122,13.0217916569603,122.845971852595)) ;
#17898 = CARTESIAN_POINT('Ctrl Pts',(-20.5341147387331,13.0228321625972,122.866161385836)) ;
#17899 = CARTESIAN_POINT('Ctrl Pts',(-20.5486990264017,13.0244307390882,122.897659873808)) ;
#17900 = CARTESIAN_POINT('Ctrl Pts',(-20.5536532004924,13.0249906160355,122.908783092264)) ;
#17901 = CARTESIAN_POINT('Ctrl Pts',(-20.5625761816843,13.0260321613578,122.929631523645)) ;
#17902 = CARTESIAN_POINT('Ctrl Pts',(-20.566586452295,13.026513955654,122.939337816036)) ;
#17903 = CARTESIAN_POINT('Ctrl Pts',(-20.5740330793367,13.027436072693,122.95802518626)) ;
#17904 = CARTESIAN_POINT('Ctrl Pts',(-20.5774890521294,13.0278764301476,122.966997647652)) ;
#17905 = CARTESIAN_POINT('Ctrl Pts',(-20.5846647335729,13.0288184617986,122.986287927234)) ;
#17906 = CARTESIAN_POINT('Ctrl Pts',(-20.5883495459185,13.0293195521975,122.996607223224)) ;
#17907 = CARTESIAN_POINT('Ctrl Pts',(-20.5919013672999,13.0298207905518,123.006983120529)) ;
#17908 = CARTESIAN_POINT('Origin',(-19.4092722359532,16.5113612779716,123.411814366564)) ;
#17909 = CARTESIAN_POINT('',(-20.5919008187226,12.3097986802463,123.006981518046)) ;
#17910 = CARTESIAN_POINT('',(-20.591900864533,12.3699275081008,123.006981651869)) ;
#17911 = CARTESIAN_POINT('',(-20.5919021064381,16.5113612779716,123.006985279772)) ;
#17912 = CARTESIAN_POINT('',(-18.1677926225402,12.1420303928368,123.557513887265)) ;
#17913 = CARTESIAN_POINT('Ctrl Pts',(-18.1677926148176,12.1420303769689,123.557513887431)) ;
#17914 = CARTESIAN_POINT('Ctrl Pts',(-18.1645228320525,12.1433302273642,123.529652651895)) ;
#17915 = CARTESIAN_POINT('Ctrl Pts',(-18.1621918274906,12.1446319180994,123.501688885341)) ;
#17916 = CARTESIAN_POINT('Ctrl Pts',(-18.1605900595685,12.1461231432797,123.46935956271)) ;
#17917 = CARTESIAN_POINT('Ctrl Pts',(-18.1603988140212,12.1463217701979,123.465047846456)) ;
#17918 = CARTESIAN_POINT('Ctrl Pts',(-18.1601009307609,12.1466716722533,123.457442320227)) ;
#17919 = CARTESIAN_POINT('Ctrl Pts',(-18.1599849810047,12.1468230373754,123.454148921874)) ;
#17920 = CARTESIAN_POINT('Ctrl Pts',(-18.1597798801821,12.1471244037961,123.447585239556)) ;
#17921 = CARTESIAN_POINT('Ctrl Pts',(-18.1596905410702,12.1472744058144,123.444314987744)) ;
#17922 = CARTESIAN_POINT('Ctrl Pts',(-18.1595265963476,12.1475955886168,123.437305938292)) ;
#17923 = CARTESIAN_POINT('Ctrl Pts',(-18.1594559280288,12.147766727388,123.433567079176)) ;
#17924 = CARTESIAN_POINT('Ctrl Pts',(-18.1593105106464,12.1482280747479,123.423477313111)) ;
#17925 = CARTESIAN_POINT('Ctrl Pts',(-18.1592673857191,12.1485179544301,123.417126051257)) ;
#17926 = CARTESIAN_POINT('Ctrl Pts',(-18.1592916562,12.1498477125098,123.387945093611)) ;
#17927 = CARTESIAN_POINT('Ctrl Pts',(-18.1599360703523,12.1508814866486,123.36512017961)) ;
#17928 = CARTESIAN_POINT('Ctrl Pts',(-18.161259740427,12.1519589376578,123.341346121815)) ;
#17929 = CARTESIAN_POINT('Ctrl Pts',(-18.1613154302979,12.1520033290725,123.340366667329)) ;
#17930 = CARTESIAN_POINT('Ctrl Pts',(-18.1623541770848,12.1528145355369,123.322469329078)) ;
#17931 = CARTESIAN_POINT('Ctrl Pts',(-18.1636800155036,12.1535813892693,123.305573137795)) ;
#17932 = CARTESIAN_POINT('Ctrl Pts',(-18.1660691461184,12.1546833930302,123.281432032133)) ;
#17933 = CARTESIAN_POINT('Ctrl Pts',(-18.1668531734841,12.155016086958,123.274161367388)) ;
#17934 = CARTESIAN_POINT('Ctrl Pts',(-18.1683731377733,12.1556136837441,123.261139067942)) ;
#17935 = CARTESIAN_POINT('Ctrl Pts',(-18.1690853820572,12.1558783464076,123.255384879309)) ;
#17936 = CARTESIAN_POINT('Ctrl Pts',(-18.1698791912853,12.1561580650851,123.249318263516)) ;
#17937 = CARTESIAN_POINT('Ctrl Pts',(-18.1699208718392,12.1561727105025,123.249000672589)) ;
#17938 = CARTESIAN_POINT('Ctrl Pts',(-18.1703951832096,12.1563388981152,123.245397325292)) ;
#17939 = CARTESIAN_POINT('Ctrl Pts',(-18.1708407567144,12.1564905715711,123.242113292349)) ;
#17940 = CARTESIAN_POINT('Ctrl Pts',(-18.1717536802671,12.156792752142,123.235579860305)) ;
#17941 = CARTESIAN_POINT('Ctrl Pts',(-18.1722207812292,12.1569432555277,123.232330453215)) ;
#17942 = CARTESIAN_POINT('Ctrl Pts',(-18.1733413883875,12.1572949972217,123.224747133327)) ;
#17943 = CARTESIAN_POINT('Ctrl Pts',(-18.1740048982661,12.1574963338795,123.220414748016)) ;
#17944 = CARTESIAN_POINT('Ctrl Pts',(-18.176220707127,12.1581470900796,123.206438261038)) ;
#17945 = CARTESIAN_POINT('Ctrl Pts',(-18.1778632635612,12.1585973562675,123.196808881856)) ;
#17946 = CARTESIAN_POINT('Ctrl Pts',(-18.1803766629264,12.1592432274774,123.18304926372)) ;
#17947 = CARTESIAN_POINT('Ctrl Pts',(-18.1811558254033,12.159438190199,123.178902615624)) ;
#17948 = CARTESIAN_POINT('Ctrl Pts',(-18.185495245598,12.160496098832,123.156435866658)) ;
#17949 = CARTESIAN_POINT('Ctrl Pts',(-18.1894444480382,12.161361062067,123.138193336859)) ;
#17950 = CARTESIAN_POINT('Ctrl Pts',(-18.1960672856455,12.1626720506994,123.110603393496)) ;
#17951 = CARTESIAN_POINT('Ctrl Pts',(-18.1984439196893,12.1631199756946,123.101187433458)) ;
#17952 = CARTESIAN_POINT('Ctrl Pts',(-18.2032493208257,12.1639844506056,123.083042714816)) ;
#17953 = CARTESIAN_POINT('Ctrl Pts',(-18.2056637430767,12.1644010634853,123.074310784912)) ;
#17954 = CARTESIAN_POINT('Ctrl Pts',(-18.2097924770936,12.1650857327849,123.059986990096)) ;
#17955 = CARTESIAN_POINT('Ctrl Pts',(-18.2114514850232,12.1653540857128,123.054379556268)) ;
#17956 = CARTESIAN_POINT('Ctrl Pts',(-18.214057171405,12.165765521525,123.045794269898)) ;
#17957 = CARTESIAN_POINT('Ctrl Pts',(-18.2149757674291,12.165908741072,123.042807988586)) ;
#17958 = CARTESIAN_POINT('Ctrl Pts',(-18.2168873050962,12.1662030805942,123.036675645351)) ;
#17959 = CARTESIAN_POINT('Ctrl Pts',(-18.2178815247523,12.1663541935308,123.033530006875)) ;
#17960 = CARTESIAN_POINT('Ctrl Pts',(-18.2277045729832,12.167828260825,123.002873473018)) ;
#17961 = CARTESIAN_POINT('Ctrl Pts',(-18.2374722997836,12.1691466736145,122.975672517264)) ;
#17962 = CARTESIAN_POINT('Ctrl Pts',(-18.2517635928554,12.1709094370337,122.939831656671)) ;
#17963 = CARTESIAN_POINT('Ctrl Pts',(-18.2554579799746,12.1713523598241,122.930870919293)) ;
#17964 = CARTESIAN_POINT('Ctrl Pts',(-18.2595555461703,12.1718306571154,122.921251305588)) ;
#17965 = CARTESIAN_POINT('Ctrl Pts',(-18.2598555385629,12.1718656017964,122.920548817884)) ;
#17966 = CARTESIAN_POINT('Ctrl Pts',(-18.2605742227398,12.1719491452172,122.918870147864)) ;
#17967 = CARTESIAN_POINT('Ctrl Pts',(-18.2609935151812,12.1719977464906,122.917894223493)) ;
#17968 = CARTESIAN_POINT('Ctrl Pts',(-18.2641936761055,12.1723676321057,122.910471786482)) ;
#17969 = CARTESIAN_POINT('Ctrl Pts',(-18.2670275633275,12.1726891559544,122.904048280276)) ;
#17970 = CARTESIAN_POINT('Ctrl Pts',(-18.2766027056258,12.1737558853549,122.882830391168)) ;
#17971 = CARTESIAN_POINT('Ctrl Pts',(-18.283578450434,12.1745018651069,122.868143684651)) ;
#17972 = CARTESIAN_POINT('Ctrl Pts',(-18.3008589420707,12.1762783256065,122.833520807817)) ;
#17973 = CARTESIAN_POINT('Ctrl Pts',(-18.3114179902996,12.1773088320195,122.813717779776)) ;
#17974 = CARTESIAN_POINT('Ctrl Pts',(-18.327646145792,12.1788154804924,122.785161909371)) ;
#17975 = CARTESIAN_POINT('Ctrl Pts',(-18.3329007623534,12.1792925311924,122.776178659087)) ;
#17976 = CARTESIAN_POINT('Ctrl Pts',(-18.3428180928227,12.1801732727208,122.759699758564)) ;
#17977 = CARTESIAN_POINT('Ctrl Pts',(-18.3474492136124,12.1805770762111,122.752185856506)) ;
#17978 = CARTESIAN_POINT('Ctrl Pts',(-18.3646853118381,12.1820529446047,122.724872565516)) ;
#17979 = CARTESIAN_POINT('Ctrl Pts',(-18.3777675134087,12.1831202428263,122.705380445828)) ;
#17980 = CARTESIAN_POINT('Ctrl Pts',(-18.3973055966241,12.1846527491358,122.677970131367)) ;
#17981 = CARTESIAN_POINT('Ctrl Pts',(-18.4033216118026,12.185116969702,122.669744840478)) ;
#17982 = CARTESIAN_POINT('Ctrl Pts',(-18.4129162732998,12.1858463967867,122.656957829174)) ;
#17983 = CARTESIAN_POINT('Ctrl Pts',(-18.4164272301395,12.1861110921839,122.652345874445)) ;
#17984 = CARTESIAN_POINT('Ctrl Pts',(-18.420041004912,12.1863813662252,122.647666746629)) ;
#17985 = CARTESIAN_POINT('Ctrl Pts',(-18.420111891752,12.186386667003,122.647574988503)) ;
#17986 = CARTESIAN_POINT('Ctrl Pts',(-18.4202521364862,12.1863971525557,122.647393503566)) ;
#17987 = CARTESIAN_POINT('Ctrl Pts',(-18.4203214938545,12.1864023373279,122.647303776291)) ;
#17988 = CARTESIAN_POINT('Ctrl Pts',(-18.4204587764218,12.1864125982132,122.647126224475)) ;
#17989 = CARTESIAN_POINT('Ctrl Pts',(-18.420526701111,12.1864176743217,122.647038399543)) ;
#17990 = CARTESIAN_POINT('Ctrl Pts',(-18.4206612104076,12.1864277248613,122.646864530246)) ;
#17991 = CARTESIAN_POINT('Ctrl Pts',(-18.4207277944761,12.186432699283,122.646778485616)) ;
#17992 = CARTESIAN_POINT('Ctrl Pts',(-18.4208597100436,12.1864425530785,122.646608060991)) ;
#17993 = CARTESIAN_POINT('Ctrl Pts',(-18.4209250410815,12.1864474324461,122.646523680711)) ;
#17994 = CARTESIAN_POINT('Ctrl Pts',(-18.4210545342517,12.1864571024661,122.646356474126)) ;
#17995 = CARTESIAN_POINT('Ctrl Pts',(-18.4211186959259,12.18646189311,122.646273647605)) ;
#17996 = CARTESIAN_POINT('Ctrl Pts',(-18.4212459298864,12.1864713916966,122.646109443506)) ;
#17997 = CARTESIAN_POINT('Ctrl Pts',(-18.4213090019489,12.1864760996461,122.646028065478)) ;
#17998 = CARTESIAN_POINT('Ctrl Pts',(-18.4214341334466,12.186485438644,122.645866657143)) ;
#17999 = CARTESIAN_POINT('Ctrl Pts',(-18.4214961924914,12.1864900696847,122.645786626665)) ;
#18000 = CARTESIAN_POINT('Ctrl Pts',(-18.4216193713305,12.1864992604048,122.645627816813)) ;
#18001 = CARTESIAN_POINT('Ctrl Pts',(-18.421680490808,12.1865038200801,122.645549037231)) ;
#18002 = CARTESIAN_POINT('Ctrl Pts',(-18.4218018609868,12.1865128733855,122.645392636513)) ;
#18003 = CARTESIAN_POINT('Ctrl Pts',(-18.421862111496,12.1865173670192,122.645315015064)) ;
#18004 = CARTESIAN_POINT('Ctrl Pts',(-18.4247301928209,12.1867312470328,122.641620931058)) ;
#18005 = CARTESIAN_POINT('Ctrl Pts',(-18.4275578574986,12.1869408064192,122.638019922427)) ;
#18006 = CARTESIAN_POINT('Ctrl Pts',(-18.432909717685,12.1873350404602,122.631280926748)) ;
#18007 = CARTESIAN_POINT('Ctrl Pts',(-18.4354294184834,12.1875196702613,122.62813944384)) ;
#18008 = CARTESIAN_POINT('Ctrl Pts',(-18.4415875171941,12.1879685633477,122.620537284786)) ;
#18009 = CARTESIAN_POINT('Ctrl Pts',(-18.4452416263481,12.1882329747225,122.616089465293)) ;
#18010 = CARTESIAN_POINT('Ctrl Pts',(-18.4554550410091,12.1889666793585,122.603831208705)) ;
#18011 = CARTESIAN_POINT('Ctrl Pts',(-18.4620793939813,12.1894365720639,122.596075595045)) ;
#18012 = CARTESIAN_POINT('Ctrl Pts',(-18.4834781031392,12.190935347645,122.571634699625)) ;
#18013 = CARTESIAN_POINT('Ctrl Pts',(-18.4986040563497,12.1919666004084,122.555263075848)) ;
#18014 = CARTESIAN_POINT('Ctrl Pts',(-18.5219361861099,12.1935103138716,122.531326512936)) ;
#18015 = CARTESIAN_POINT('Ctrl Pts',(-18.5298191447238,12.1940242968596,122.523452735519)) ;
#18016 = CARTESIAN_POINT('Ctrl Pts',(-18.5441774619311,12.1949467881151,122.509489585183)) ;
#18017 = CARTESIAN_POINT('Ctrl Pts',(-18.5506145026092,12.195355573551,122.503361903832)) ;
#18018 = CARTESIAN_POINT('Ctrl Pts',(-18.5612083052461,12.1960206591927,122.493490430241)) ;
#18019 = CARTESIAN_POINT('Ctrl Pts',(-18.5653258024633,12.1962773126799,122.489704991146)) ;
#18020 = CARTESIAN_POINT('Ctrl Pts',(-18.5710013053714,12.1966285987161,122.484557051096)) ;
#18021 = CARTESIAN_POINT('Ctrl Pts',(-18.5725374861609,12.1967234345237,122.483170602438)) ;
#18022 = CARTESIAN_POINT('Ctrl Pts',(-18.5748995165934,12.1968688794334,122.481049419282)) ;
#18023 = CARTESIAN_POINT('Ctrl Pts',(-18.5757229089568,12.1969195113214,122.480311955742)) ;
#18024 = CARTESIAN_POINT('Ctrl Pts',(-18.5817032191462,12.197286749831,122.474970026566)) ;
#18025 = CARTESIAN_POINT('Ctrl Pts',(-18.5868972891204,12.1976030028579,122.470407312092)) ;
#18026 = CARTESIAN_POINT('Ctrl Pts',(-18.6097881440936,12.1989853968337,122.450632932986)) ;
#18027 = CARTESIAN_POINT('Ctrl Pts',(-18.6278710570068,12.2000477396646,122.435875452628)) ;
#18028 = CARTESIAN_POINT('Ctrl Pts',(-18.6565981779941,12.2016995526509,122.413741762877)) ;
#18029 = CARTESIAN_POINT('Ctrl Pts',(-18.6669616198807,12.2022887508295,122.406010157)) ;
#18030 = CARTESIAN_POINT('Ctrl Pts',(-18.6847886219544,12.2032925103567,122.393136012444)) ;
#18031 = CARTESIAN_POINT('Ctrl Pts',(-18.6921915544269,12.2037064914759,122.387911347904)) ;
#18032 = CARTESIAN_POINT('Ctrl Pts',(-18.69990698398,12.2041351326502,122.3825908552)) ;
#18033 = CARTESIAN_POINT('Ctrl Pts',(-18.7001634145111,12.2041493758014,122.382414164308)) ;
#18034 = CARTESIAN_POINT('Ctrl Pts',(-18.70067945401,12.2041780322253,122.382058876777)) ;
#18035 = CARTESIAN_POINT('Ctrl Pts',(-18.7009390645633,12.2041924455099,122.381880282422)) ;
#18036 = CARTESIAN_POINT('Ctrl Pts',(-18.7014625314209,12.2042215012206,122.381520464463)) ;
#18037 = CARTESIAN_POINT('Ctrl Pts',(-18.7017263897835,12.2042361436569,122.381339244057)) ;
#18038 = CARTESIAN_POINT('Ctrl Pts',(-18.7022594983657,12.2042657209516,122.380973401359)) ;
#18039 = CARTESIAN_POINT('Ctrl Pts',(-18.70252875142,12.2042806558321,122.380788783115)) ;
#18040 = CARTESIAN_POINT('Ctrl Pts',(-18.7093338711574,12.2046580327664,122.376126647569)) ;
#18041 = CARTESIAN_POINT('Ctrl Pts',(-18.7159120750066,12.2050207724632,122.371711269472)) ;
#18042 = CARTESIAN_POINT('Ctrl Pts',(-18.7306319494098,12.205828002473,122.362032798999)) ;
#18043 = CARTESIAN_POINT('Ctrl Pts',(-18.738793770146,12.2062726075636,122.356801284005)) ;
#18044 = CARTESIAN_POINT('Ctrl Pts',(-18.7664242306082,12.2077678053906,122.339541018082)) ;
#18045 = CARTESIAN_POINT('Ctrl Pts',(-18.7861621285198,12.208819668736,122.327952067438)) ;
#18046 = CARTESIAN_POINT('Ctrl Pts',(-18.8153085662974,12.2103479166225,122.311898401772)) ;
#18047 = CARTESIAN_POINT('Ctrl Pts',(-18.8244723425432,12.2108248883029,122.306998972057)) ;
#18048 = CARTESIAN_POINT('Ctrl Pts',(-18.8389253835496,12.2115713244619,122.29950183374)) ;
#18049 = CARTESIAN_POINT('Ctrl Pts',(-18.8441737320509,12.2118411751851,122.296826302062)) ;
#18050 = CARTESIAN_POINT('Ctrl Pts',(-18.8627668017161,12.2127928880342,122.287512827957)) ;
#18051 = CARTESIAN_POINT('Ctrl Pts',(-18.8762111380298,12.2134735730895,122.281076551096)) ;
#18052 = CARTESIAN_POINT('Ctrl Pts',(-18.9008902714506,12.2147131183202,122.269799774599)) ;
#18053 = CARTESIAN_POINT('Ctrl Pts',(-18.9120871344803,12.2152718330016,122.264880835652)) ;
#18054 = CARTESIAN_POINT('Ctrl Pts',(-18.9237710317051,12.2158518287665,122.259951186637)) ;
#18055 = CARTESIAN_POINT('Ctrl Pts',(-18.9241878009281,12.2158725134481,122.259775610491)) ;
#18056 = CARTESIAN_POINT('Ctrl Pts',(-18.9249915696815,12.2159123976629,122.259437513042)) ;
#18057 = CARTESIAN_POINT('Ctrl Pts',(-18.9253785559055,12.2159315970852,122.259274960441)) ;
#18058 = CARTESIAN_POINT('Ctrl Pts',(-18.9261280064668,12.2159687727633,122.258960599595)) ;
#18059 = CARTESIAN_POINT('Ctrl Pts',(-18.9264904607414,12.2159867489388,122.258808767261)) ;
#18060 = CARTESIAN_POINT('Ctrl Pts',(-18.9271952010047,12.2160216952847,122.258513941671)) ;
#18061 = CARTESIAN_POINT('Ctrl Pts',(-18.9275374791285,12.2160386653868,122.258370929828)) ;
#18062 = CARTESIAN_POINT('Ctrl Pts',(-18.9282055447689,12.2160717828812,122.258092145542)) ;
#18063 = CARTESIAN_POINT('Ctrl Pts',(-18.9285313261947,12.2160879302194,122.257956358692)) ;
#18064 = CARTESIAN_POINT('Ctrl Pts',(-18.929169564206,12.2161195598355,122.257690656053)) ;
#18065 = CARTESIAN_POINT('Ctrl Pts',(-18.9294820160998,12.2161350420713,122.257560729136)) ;
#18066 = CARTESIAN_POINT('Ctrl Pts',(-18.9300963749889,12.2161654797999,122.257305552748)) ;
#18067 = CARTESIAN_POINT('Ctrl Pts',(-18.9303982784671,12.2161804352628,122.257180294768)) ;
#18068 = CARTESIAN_POINT('Ctrl Pts',(-18.9309940349823,12.2162099434465,122.256933392741)) ;
#18069 = CARTESIAN_POINT('Ctrl Pts',(-18.9312878854123,12.2162244961448,122.256811742385)) ;
#18070 = CARTESIAN_POINT('Ctrl Pts',(-18.9318698271665,12.2162533125961,122.256571085987)) ;
#18071 = CARTESIAN_POINT('Ctrl Pts',(-18.932157916626,12.2162675763311,122.256452075537)) ;
#18072 = CARTESIAN_POINT('Ctrl Pts',(-18.9327304953461,12.216295921971,122.256215792568)) ;
#18073 = CARTESIAN_POINT('Ctrl Pts',(-18.9330149834148,12.2163100038627,122.256098517332)) ;
#18074 = CARTESIAN_POINT('Ctrl Pts',(-18.9335824493013,12.2163380894059,122.255864834544)) ;
#18075 = CARTESIAN_POINT('Ctrl Pts',(-18.9338654267041,12.2163520930564,122.255748425788)) ;
#18076 = CARTESIAN_POINT('Ctrl Pts',(-18.93443195383,12.2163801252376,122.255515616025)) ;
#18077 = CARTESIAN_POINT('Ctrl Pts',(-18.9347155036718,12.2163941537683,122.255399215387)) ;
#18078 = CARTESIAN_POINT('Ctrl Pts',(-18.9352853123423,12.2164223414045,122.255165546906)) ;
#18079 = CARTESIAN_POINT('Ctrl Pts',(-18.9355715719559,12.216436500517,122.255048281005)) ;
#18080 = CARTESIAN_POINT('Ctrl Pts',(-18.9433240163868,12.2168199085375,122.251875861885)) ;
#18081 = CARTESIAN_POINT('Ctrl Pts',(-18.9508195454011,12.217189431199,122.248892955615)) ;
#18082 = CARTESIAN_POINT('Ctrl Pts',(-18.9594342632914,12.2176128970995,122.245560892225)) ;
#18083 = CARTESIAN_POINT('Ctrl Pts',(-18.9605257069928,12.2176665255784,122.245140495766)) ;
#18084 = CARTESIAN_POINT('Ctrl Pts',(-18.9621261687957,12.2177451319789,122.244526616593)) ;
#18085 = CARTESIAN_POINT('Ctrl Pts',(-18.9626347260644,12.217770104821,122.244331933562)) ;
#18086 = CARTESIAN_POINT('Ctrl Pts',(-18.9673729995085,12.2180027339373,122.242521603515)) ;
#18087 = CARTESIAN_POINT('Ctrl Pts',(-18.9716113334257,12.2182104841213,122.240928618418)) ;
#18088 = CARTESIAN_POINT('Ctrl Pts',(-18.9942224841391,12.2193170749833,122.232570102365)) ;
#18089 = CARTESIAN_POINT('Ctrl Pts',(-19.0127436520792,12.220217578565,122.226213924235)) ;
#18090 = CARTESIAN_POINT('Ctrl Pts',(-19.0515907926042,12.2220924950652,122.213894348849)) ;
#18091 = CARTESIAN_POINT('Ctrl Pts',(-19.071934638872,12.2230659205256,122.208007183392)) ;
#18092 = CARTESIAN_POINT('Ctrl Pts',(-19.1057136292822,12.2246688135965,122.199155685149)) ;
#18093 = CARTESIAN_POINT('Ctrl Pts',(-19.1190655972305,12.2252990883806,122.195891254894)) ;
#18094 = CARTESIAN_POINT('Ctrl Pts',(-19.1677225864566,12.2275854979155,122.184842202695)) ;
#18095 = CARTESIAN_POINT('Ctrl Pts',(-19.2033071707242,12.2292373528706,122.178369873062)) ;
#18096 = CARTESIAN_POINT('Ctrl Pts',(-19.2443297510396,12.2311329501925,122.172733413564)) ;
#18097 = CARTESIAN_POINT('Ctrl Pts',(-19.2495418353335,12.2313736456963,122.17205074778)) ;
#18098 = CARTESIAN_POINT('Ctrl Pts',(-19.269469403528,12.232293533661,122.1695684369)) ;
#18099 = CARTESIAN_POINT('Ctrl Pts',(-19.2842121442157,12.2329734011545,122.167997759009)) ;
#18100 = CARTESIAN_POINT('Ctrl Pts',(-19.3261818803678,12.2349069048186,122.16428008652)) ;
#18101 = CARTESIAN_POINT('Ctrl Pts',(-19.3534561389592,12.236161044958,122.162762585656)) ;
#18102 = CARTESIAN_POINT('Ctrl Pts',(-19.3854043401168,12.2376270461804,122.162033617022)) ;
#18103 = CARTESIAN_POINT('Ctrl Pts',(-19.3900510857168,12.2378401950327,122.161953515986)) ;
#18104 = CARTESIAN_POINT('Ctrl Pts',(-19.4042099196831,12.238489435588,122.161788423365)) ;
#18105 = CARTESIAN_POINT('Ctrl Pts',(-19.4137226380546,12.238925311864,122.161786094804)) ;
#18106 = CARTESIAN_POINT('Ctrl Pts',(-19.4236828948241,12.2393813517582,122.16189735568)) ;
#18107 = CARTESIAN_POINT('Ctrl Pts',(-19.4241313187826,12.2394018825517,122.161902606141)) ;
#18108 = CARTESIAN_POINT('Ctrl Pts',(-19.43481762074,12.2398911304649,122.162033480441)) ;
#18109 = CARTESIAN_POINT('Ctrl Pts',(-19.4450535984701,12.2403593816135,122.162284644999)) ;
#18110 = CARTESIAN_POINT('Ctrl Pts',(-19.4650656910383,12.2412741002838,122.163021799644)) ;
#18111 = CARTESIAN_POINT('Ctrl Pts',(-19.4748414735195,12.2417205339493,122.1634969145)) ;
#18112 = CARTESIAN_POINT('Ctrl Pts',(-19.5101735512852,12.2433332668824,122.165630284742)) ;
#18113 = CARTESIAN_POINT('Ctrl Pts',(-19.5356828364579,12.2444975683689,122.16795898834)) ;
#18114 = CARTESIAN_POINT('Ctrl Pts',(-19.5670788919768,12.245942413207,122.171800935203)) ;
#18115 = CARTESIAN_POINT('Ctrl Pts',(-19.5730497812065,12.2462176921639,122.17257542027)) ;
#18116 = CARTESIAN_POINT('Ctrl Pts',(-19.5830888528739,12.2466814763301,122.173951412425)) ;
#18117 = CARTESIAN_POINT('Ctrl Pts',(-19.5871600885699,12.2468698213672,122.174529912069)) ;
#18118 = CARTESIAN_POINT('Ctrl Pts',(-19.5960297390353,12.2472807554412,122.175834922107)) ;
#18119 = CARTESIAN_POINT('Ctrl Pts',(-19.6008269242351,12.2475033964753,122.176569308568)) ;
#18120 = CARTESIAN_POINT('Ctrl Pts',(-19.6118824274516,12.2480174128346,122.178327713083)) ;
#18121 = CARTESIAN_POINT('Ctrl Pts',(-19.6181374656133,12.2483089197332,122.179371455317)) ;
#18122 = CARTESIAN_POINT('Ctrl Pts',(-19.6326959910645,12.2489890051571,122.181914769569)) ;
#18123 = CARTESIAN_POINT('Ctrl Pts',(-19.6409927663036,12.2493778053678,122.183450907276)) ;
#18124 = CARTESIAN_POINT('Ctrl Pts',(-19.6695561075008,12.2507203181433,122.189039062843)) ;
#18125 = CARTESIAN_POINT('Ctrl Pts',(-19.6897373188593,12.2516758609037,122.193509612739)) ;
#18126 = CARTESIAN_POINT('Ctrl Pts',(-19.7266671776703,12.2534321971237,122.202656616647)) ;
#18127 = CARTESIAN_POINT('Ctrl Pts',(-19.7434470677064,12.2542333066548,122.207186125052)) ;
#18128 = CARTESIAN_POINT('Ctrl Pts',(-19.7673306764107,12.2553776010228,122.214170645652)) ;
#18129 = CARTESIAN_POINT('Ctrl Pts',(-19.774515124887,12.2557223579459,122.216342091005)) ;
#18130 = CARTESIAN_POINT('Ctrl Pts',(-19.786802523401,12.256312972159,122.220176970858)) ;
#18131 = CARTESIAN_POINT('Ctrl Pts',(-19.7919151072575,12.2565590119332,122.221808806064)) ;
#18132 = CARTESIAN_POINT('Ctrl Pts',(-19.803032729246,12.2570947320051,122.225436384868)) ;
#18133 = CARTESIAN_POINT('Ctrl Pts',(-19.8090334453629,12.2573843278035,122.227444906771)) ;
#18134 = CARTESIAN_POINT('Ctrl Pts',(-19.8152179863916,12.2576833057436,122.22956731447)) ;
#18135 = CARTESIAN_POINT('Ctrl Pts',(-19.8154172922062,12.2576929412929,122.229635768481)) ;
#18136 = CARTESIAN_POINT('Ctrl Pts',(-19.8158264704854,12.2577127243783,122.229776421438)) ;
#18137 = CARTESIAN_POINT('Ctrl Pts',(-19.8160363409848,12.2577228718798,122.229848625862)) ;
#18138 = CARTESIAN_POINT('Ctrl Pts',(-19.8164678811901,12.257743738657,122.229997222692)) ;
#18139 = CARTESIAN_POINT('Ctrl Pts',(-19.8166895486924,12.2577544578976,122.230073621591)) ;
#18140 = CARTESIAN_POINT('Ctrl Pts',(-19.8171460621064,12.257776535075,122.230231105113)) ;
#18141 = CARTESIAN_POINT('Ctrl Pts',(-19.817380905454,12.2577878929727,122.230312197425)) ;
#18142 = CARTESIAN_POINT('Ctrl Pts',(-19.8178653185846,12.2578113226024,122.230479628803)) ;
#18143 = CARTESIAN_POINT('Ctrl Pts',(-19.8181148853065,12.2578233942877,122.230565976984)) ;
#18144 = CARTESIAN_POINT('Ctrl Pts',(-19.8257395270663,12.2581922296512,122.233206750634)) ;
#18145 = CARTESIAN_POINT('Ctrl Pts',(-19.833090557614,12.2585486001865,122.235830120235)) ;
#18146 = CARTESIAN_POINT('Ctrl Pts',(-19.8539029521174,12.2595601497174,122.243477955619)) ;
#18147 = CARTESIAN_POINT('Ctrl Pts',(-19.8673029248661,12.2602145014084,122.248665909766)) ;
#18148 = CARTESIAN_POINT('Ctrl Pts',(-19.9060376920783,12.2621184626908,122.264435707635)) ;
#18149 = CARTESIAN_POINT('Ctrl Pts',(-19.931116818952,12.2633675442307,122.275622512465)) ;
#18150 = CARTESIAN_POINT('Ctrl Pts',(-19.9631384724602,12.2649943851343,122.291190146319)) ;
#18151 = CARTESIAN_POINT('Ctrl Pts',(-19.9704346873014,12.2653672269055,122.294825936211)) ;
#18152 = CARTESIAN_POINT('Ctrl Pts',(-19.9834768149942,12.2660377602939,122.301485024137)) ;
#18153 = CARTESIAN_POINT('Ctrl Pts',(-19.9892357318739,12.2663352864247,122.304482216601)) ;
#18154 = CARTESIAN_POINT('Ctrl Pts',(-20.0017259720429,12.2669837836874,122.311106850548)) ;
#18155 = CARTESIAN_POINT('Ctrl Pts',(-20.0084478865366,12.267334839778,122.31475146749)) ;
#18156 = CARTESIAN_POINT('Ctrl Pts',(-20.0239105945599,12.2681471562515,122.323319844205)) ;
#18157 = CARTESIAN_POINT('Ctrl Pts',(-20.0326263957985,12.2686086028019,122.328287612043)) ;
#18158 = CARTESIAN_POINT('Ctrl Pts',(-20.058118491202,12.2699685184745,122.343226802386)) ;
#18159 = CARTESIAN_POINT('Ctrl Pts',(-20.0747221784813,12.270867654615,122.353486808107)) ;
#18160 = CARTESIAN_POINT('Ctrl Pts',(-20.1010857275969,12.272313816415,122.370643564332)) ;
#18161 = CARTESIAN_POINT('Ctrl Pts',(-20.1109988064159,12.2728619851654,122.377298843122)) ;
#18162 = CARTESIAN_POINT('Ctrl Pts',(-20.1445612175643,12.2747347802739,122.400535823734)) ;
#18163 = CARTESIAN_POINT('Ctrl Pts',(-20.1677305109691,12.2760569511258,122.417794633536)) ;
#18164 = CARTESIAN_POINT('Ctrl Pts',(-20.2727534369062,12.2822167198327,122.501837704674)) ;
#18165 = CARTESIAN_POINT('Ctrl Pts',(-20.3465286166676,12.2870386308518,122.578023182883)) ;
#18166 = CARTESIAN_POINT('Ctrl Pts',(-20.4323847470827,12.293605133144,122.692679227499)) ;
#18167 = CARTESIAN_POINT('Ctrl Pts',(-20.4535580323012,12.2953292495682,122.723786946419)) ;
#18168 = CARTESIAN_POINT('Ctrl Pts',(-20.4833812613681,12.2979356525796,122.772158942524)) ;
#18169 = CARTESIAN_POINT('Ctrl Pts',(-20.4930875715225,12.2988167664969,122.78874648869)) ;
#18170 = CARTESIAN_POINT('Ctrl Pts',(-20.5068966632968,12.3001207856383,122.81364525862)) ;
#18171 = CARTESIAN_POINT('Ctrl Pts',(-20.5112956719335,12.3005444128992,122.821788932931)) ;
#18172 = CARTESIAN_POINT('Ctrl Pts',(-20.5246851473785,12.3018597350152,122.847248443507)) ;
#18173 = CARTESIAN_POINT('Ctrl Pts',(-20.5333609025052,12.3027491591494,122.864726334894)) ;
#18174 = CARTESIAN_POINT('Ctrl Pts',(-20.5484219081126,12.3043714020717,122.89693997333)) ;
#18175 = CARTESIAN_POINT('Ctrl Pts',(-20.5549390719354,12.305103978519,122.911609293826)) ;
#18176 = CARTESIAN_POINT('Ctrl Pts',(-20.5639447883878,12.3061647490169,122.932980070922)) ;
#18177 = CARTESIAN_POINT('Ctrl Pts',(-20.5666612096697,12.306491641395,122.939583756425)) ;
#18178 = CARTESIAN_POINT('Ctrl Pts',(-20.571603098209,12.3070996427502,122.951896431715)) ;
#18179 = CARTESIAN_POINT('Ctrl Pts',(-20.5738434595775,12.3073806560075,122.957599213814)) ;
#18180 = CARTESIAN_POINT('Ctrl Pts',(-20.5784317875143,12.307967686466,122.969535819076)) ;
#18181 = CARTESIAN_POINT('Ctrl Pts',(-20.5807720339025,12.3082737386583,122.97577240339)) ;
#18182 = CARTESIAN_POINT('Ctrl Pts',(-20.586097636059,12.3089860108875,122.990317141197)) ;
#18183 = CARTESIAN_POINT('Ctrl Pts',(-20.5890417450682,12.3093919517987,122.998629374036)) ;
#18184 = CARTESIAN_POINT('Ctrl Pts',(-20.591900818743,12.3097986802335,123.00698151804)) ;
#18185 = CARTESIAN_POINT('',(-18.1733329886729,12.2002114096132,123.598774520568)) ;
#18186 = CARTESIAN_POINT('Ctrl Pts',(-18.1677926155534,12.1420304143771,123.5575138937)) ;
#18187 = CARTESIAN_POINT('Ctrl Pts',(-18.169135727965,12.1629836299978,123.568958314418)) ;
#18188 = CARTESIAN_POINT('Ctrl Pts',(-18.1709219229379,12.182512173169,123.58283582176)) ;
#18189 = CARTESIAN_POINT('Ctrl Pts',(-18.1733328671508,12.200210692235,123.598773925614)) ;
#18190 = CARTESIAN_POINT('Ctrl Pts',(-20.5919008645526,12.3699275081133,123.006981651862)) ;
#18191 = CARTESIAN_POINT('Ctrl Pts',(-20.588467048387,12.3694413279222,122.99695052257)) ;
#18192 = CARTESIAN_POINT('Ctrl Pts',(-20.5849091447236,12.3689552610106,122.986972898729)) ;
#18193 = CARTESIAN_POINT('Ctrl Pts',(-20.5698738748206,12.3669703159962,122.946445527993)) ;
#18194 = CARTESIAN_POINT('Ctrl Pts',(-20.5573333724681,12.3654693923714,122.916314680899)) ;
#18195 = CARTESIAN_POINT('Ctrl Pts',(-20.5391761439346,12.3634817537078,122.877090607563)) ;
#18196 = CARTESIAN_POINT('Ctrl Pts',(-20.5346014928025,12.3629945400929,122.867529143557)) ;
#18197 = CARTESIAN_POINT('Ctrl Pts',(-20.5269913366345,12.3622056239413,122.852129376477)) ;
#18198 = CARTESIAN_POINT('Ctrl Pts',(-20.5240303683542,12.3619036716072,122.84625483596)) ;
#18199 = CARTESIAN_POINT('Ctrl Pts',(-20.5183841361507,12.3613371956875,122.835269380443)) ;
#18200 = CARTESIAN_POINT('Ctrl Pts',(-20.5157095679168,12.3610726226028,122.830153160319)) ;
#18201 = CARTESIAN_POINT('Ctrl Pts',(-20.5101047504447,12.360525924615,122.819610171444)) ;
#18202 = CARTESIAN_POINT('Ctrl Pts',(-20.507169587209,12.3602438538138,122.814186187643)) ;
#18203 = CARTESIAN_POINT('Ctrl Pts',(-20.4945872284831,12.3590523216907,122.79134039582)) ;
#18204 = CARTESIAN_POINT('Ctrl Pts',(-20.4845645338713,12.3581457997232,122.774128658132)) ;
#18205 = CARTESIAN_POINT('Ctrl Pts',(-20.4532563116821,12.3554263223768,122.723202330166)) ;
#18206 = CARTESIAN_POINT('Ctrl Pts',(-20.4307651059345,12.3536159843102,122.690259388991)) ;
#18207 = CARTESIAN_POINT('Ctrl Pts',(-20.4021529489442,12.3514481267618,122.652376565067)) ;
#18208 = CARTESIAN_POINT('Ctrl Pts',(-20.3975122219132,12.3511004161684,122.646347440896)) ;
#18209 = CARTESIAN_POINT('Ctrl Pts',(-20.3887647950201,12.3504520301483,122.635195134209)) ;
#18210 = CARTESIAN_POINT('Ctrl Pts',(-20.3846722088182,12.3501514498756,122.63006120989)) ;
#18211 = CARTESIAN_POINT('Ctrl Pts',(-20.376131643927,12.3495297687297,122.619519020634)) ;
#18212 = CARTESIAN_POINT('Ctrl Pts',(-20.3716782842844,12.3492086436625,122.614115408473)) ;
#18213 = CARTESIAN_POINT('Ctrl Pts',(-20.3617186080977,12.3484970327808,122.602235360749)) ;
#18214 = CARTESIAN_POINT('Ctrl Pts',(-20.3561911563641,12.3481064272172,122.595777102711)) ;
#18215 = CARTESIAN_POINT('Ctrl Pts',(-20.3333834307839,12.3465118842596,122.569672411961)) ;
#18216 = CARTESIAN_POINT('Ctrl Pts',(-20.3155542965339,12.3453047223799,122.550514543849)) ;
#18217 = CARTESIAN_POINT('Ctrl Pts',(-20.2782081435285,12.3428528304214,122.512829639854)) ;
#18218 = CARTESIAN_POINT('Ctrl Pts',(-20.2586676016641,12.3416086114623,122.494344658606)) ;
#18219 = CARTESIAN_POINT('Ctrl Pts',(-20.2183254075472,12.3391198137629,122.458576062302)) ;
#18220 = CARTESIAN_POINT('Ctrl Pts',(-20.1975285548273,12.3378761032523,122.441308165068)) ;
#18221 = CARTESIAN_POINT('Ctrl Pts',(-20.1460043562943,12.3348761268626,122.401276478576)) ;
#18222 = CARTESIAN_POINT('Ctrl Pts',(-20.1147605172763,12.3331224335785,122.379221833841)) ;
#18223 = CARTESIAN_POINT('Ctrl Pts',(-20.0620911182597,12.3302543283572,122.34555105895)) ;
#18224 = CARTESIAN_POINT('Ctrl Pts',(-20.0412499364868,12.329140632997,122.333067814715)) ;
#18225 = CARTESIAN_POINT('Ctrl Pts',(-20.0032253422425,12.327143406379,122.31177258232)) ;
#18226 = CARTESIAN_POINT('Ctrl Pts',(-19.9861763379106,12.3262599298032,122.302736425427)) ;
#18227 = CARTESIAN_POINT('Ctrl Pts',(-19.9538417565517,12.3246057809125,122.286546140861)) ;
#18228 = CARTESIAN_POINT('Ctrl Pts',(-19.9386071313741,12.3238350590984,122.279299857031)) ;
#18229 = CARTESIAN_POINT('Ctrl Pts',(-19.8922897410144,12.3215172354616,122.258408023563)) ;
#18230 = CARTESIAN_POINT('Ctrl Pts',(-19.8607933567466,12.319977302789,122.245717969921)) ;
#18231 = CARTESIAN_POINT('Ctrl Pts',(-19.8058604983243,12.317337094044,122.226145029492)) ;
#18232 = CARTESIAN_POINT('Ctrl Pts',(-19.7826674169025,12.3162341222542,122.218637909037)) ;
#18233 = CARTESIAN_POINT('Ctrl Pts',(-19.7495244487148,12.3146656782143,122.208971283558)) ;
#18234 = CARTESIAN_POINT('Ctrl Pts',(-19.7397448889059,12.3142038406693,122.206247746719)) ;
#18235 = CARTESIAN_POINT('Ctrl Pts',(-19.7241202988396,12.3134670066372,122.202100818508)) ;
#18236 = CARTESIAN_POINT('Ctrl Pts',(-19.7182962793939,12.3131925825627,122.200599971301)) ;
#18237 = CARTESIAN_POINT('Ctrl Pts',(-19.7095960001252,12.3127828935473,122.198424749774)) ;
#18238 = CARTESIAN_POINT('Ctrl Pts',(-19.7067278040873,12.3126478750999,122.197718443499)) ;
#18239 = CARTESIAN_POINT('Ctrl Pts',(-19.7037467265872,12.312507581474,122.196995537541)) ;
#18240 = CARTESIAN_POINT('Ctrl Pts',(-19.7036363146429,12.3125023853904,122.19696877878)) ;
#18241 = CARTESIAN_POINT('Ctrl Pts',(-19.7034191767295,12.3124921667962,122.196916185906)) ;
#18242 = CARTESIAN_POINT('Ctrl Pts',(-19.703312451234,12.3124871443043,122.196890350861)) ;
#18243 = CARTESIAN_POINT('Ctrl Pts',(-19.7031025646948,12.3124772671633,122.196839572895)) ;
#18244 = CARTESIAN_POINT('Ctrl Pts',(-19.70299940392,12.3124724125236,122.196814629059)) ;
#18245 = CARTESIAN_POINT('Ctrl Pts',(-19.7027965279017,12.3124628654805,122.196765601849)) ;
#18246 = CARTESIAN_POINT('Ctrl Pts',(-19.7026968130805,12.3124581730937,122.196741517663)) ;
#18247 = CARTESIAN_POINT('Ctrl Pts',(-19.7025007143907,12.312448945155,122.196694179365)) ;
#18248 = CARTESIAN_POINT('Ctrl Pts',(-19.7024043305009,12.3124444095992,122.196670924393)) ;
#18249 = CARTESIAN_POINT('Ctrl Pts',(-19.702214780929,12.3124354900077,122.196625214785)) ;
#18250 = CARTESIAN_POINT('Ctrl Pts',(-19.7021216155958,12.3124311059859,122.196602759434)) ;
#18251 = CARTESIAN_POINT('Ctrl Pts',(-19.7019383943474,12.312422484335,122.196558620482)) ;
#18252 = CARTESIAN_POINT('Ctrl Pts',(-19.7018483385442,12.3124182467087,122.19653693616)) ;
#18253 = CARTESIAN_POINT('Ctrl Pts',(-19.7016712305259,12.3124099128612,122.196494311572)) ;
#18254 = CARTESIAN_POINT('Ctrl Pts',(-19.7015841783424,12.3124058166393,122.196473370617)) ;
#18255 = CARTESIAN_POINT('Ctrl Pts',(-19.701412973721,12.312397760707,122.196432205718)) ;
#18256 = CARTESIAN_POINT('Ctrl Pts',(-19.7013288217064,12.3123938010145,122.196411981227)) ;
#18257 = CARTESIAN_POINT('Ctrl Pts',(-19.7011633180545,12.3123860134588,122.196372223447)) ;
#18258 = CARTESIAN_POINT('Ctrl Pts',(-19.7010819663145,12.3123821855888,122.196352689529)) ;
#18259 = CARTESIAN_POINT('Ctrl Pts',(-19.700921965019,12.3123746570517,122.196314287521)) ;
#18260 = CARTESIAN_POINT('Ctrl Pts',(-19.7008433158003,12.3123709563986,122.196295418948)) ;
#18261 = CARTESIAN_POINT('Ctrl Pts',(-19.7006886257722,12.3123636778772,122.196258323457)) ;
#18262 = CARTESIAN_POINT('Ctrl Pts',(-19.7006125847527,12.3123600999972,122.196240095961)) ;
#18263 = CARTESIAN_POINT('Ctrl Pts',(-19.7004630188019,12.3123530626729,122.196204258933)) ;
#18264 = CARTESIAN_POINT('Ctrl Pts',(-19.7003894940058,12.3123496032333,122.19618664894)) ;
#18265 = CARTESIAN_POINT('Ctrl Pts',(-19.7002448708444,12.3123427985663,122.196152023985)) ;
#18266 = CARTESIAN_POINT('Ctrl Pts',(-19.7001737727723,12.3123394533511,122.196135008634)) ;
#18267 = CARTESIAN_POINT('Ctrl Pts',(-19.7000339175844,12.3123328731067,122.196101551147)) ;
#18268 = CARTESIAN_POINT('Ctrl Pts',(-19.6999651600884,12.3123296380582,122.196085108493)) ;
#18269 = CARTESIAN_POINT('Ctrl Pts',(-19.699829901114,12.3123232741464,122.196052774817)) ;
#18270 = CARTESIAN_POINT('Ctrl Pts',(-19.6997633999366,12.3123201452961,122.19603688347)) ;
#18271 = CARTESIAN_POINT('Ctrl Pts',(-19.6996325719889,12.3123139899369,122.196005631727)) ;
#18272 = CARTESIAN_POINT('Ctrl Pts',(-19.6995682454869,12.3123109634396,122.195990271023)) ;
#18273 = CARTESIAN_POINT('Ctrl Pts',(-19.6994416886969,12.3123050091039,122.195960060793)) ;
#18274 = CARTESIAN_POINT('Ctrl Pts',(-19.6993794581854,12.312302081254,122.195945210866)) ;
#18275 = CARTESIAN_POINT('Ctrl Pts',(-19.6992570161039,12.3122963205741,122.195916002724)) ;
#18276 = CARTESIAN_POINT('Ctrl Pts',(-19.6991968047329,12.3122934877525,122.195901644234)) ;
#18277 = CARTESIAN_POINT('Ctrl Pts',(-19.695037932913,12.3120978224063,122.194910212487)) ;
#18278 = CARTESIAN_POINT('Ctrl Pts',(-19.6909343665839,12.3119048291196,122.19395386642)) ;
#18279 = CARTESIAN_POINT('Ctrl Pts',(-19.6827682213374,12.3115208845478,122.192094207692)) ;
#18280 = CARTESIAN_POINT('Ctrl Pts',(-19.6787058098706,12.3113299397366,122.191190399446)) ;
#18281 = CARTESIAN_POINT('Ctrl Pts',(-19.669033246936,12.3108754120162,122.189089080806)) ;
#18282 = CARTESIAN_POINT('Ctrl Pts',(-19.6634192234708,12.3106116884295,122.187909870423)) ;
#18283 = CARTESIAN_POINT('Ctrl Pts',(-19.6420652691515,12.3096088300584,122.183577790628)) ;
#18284 = CARTESIAN_POINT('Ctrl Pts',(-19.6262733308779,12.3088676866191,122.18068959581)) ;
#18285 = CARTESIAN_POINT('Ctrl Pts',(-19.6086221891221,12.3080397782311,122.177811549611)) ;
#18286 = CARTESIAN_POINT('Ctrl Pts',(-19.606813481942,12.3079549489677,122.177520717467)) ;
#18287 = CARTESIAN_POINT('Ctrl Pts',(-19.5651027493367,12.3059988467742,122.170907846769)) ;
#18288 = CARTESIAN_POINT('Ctrl Pts',(-19.5249184829976,12.3041158481762,122.166520003657)) ;
#18289 = CARTESIAN_POINT('Ctrl Pts',(-19.4745760993058,12.3017763554151,122.163481037315)) ;
#18290 = CARTESIAN_POINT('Ctrl Pts',(-19.4645526576686,12.3013116081471,122.162997017124)) ;
#18291 = CARTESIAN_POINT('Ctrl Pts',(-19.4494450108058,12.30061333689,122.162449734982)) ;
#18292 = CARTESIAN_POINT('Ctrl Pts',(-19.4443645042219,12.3003789067837,122.162296712571)) ;
#18293 = CARTESIAN_POINT('Ctrl Pts',(-19.4354623917786,12.2999688480163,122.162082922384)) ;
#18294 = CARTESIAN_POINT('Ctrl Pts',(-19.4316412048991,12.299793051477,122.16200868719)) ;
#18295 = CARTESIAN_POINT('Ctrl Pts',(-19.4242244275214,12.2994522061578,122.16189862497)) ;
#18296 = CARTESIAN_POINT('Ctrl Pts',(-19.4206289054718,12.2992871386862,122.161860785317)) ;
#18297 = CARTESIAN_POINT('Ctrl Pts',(-19.4129827002951,12.2989364149981,122.161813310474)) ;
#18298 = CARTESIAN_POINT('Ctrl Pts',(-19.4089320310557,12.2987507982878,122.161807849719)) ;
#18299 = CARTESIAN_POINT('Ctrl Pts',(-19.3996007625189,12.2983235503752,122.161840627581)) ;
#18300 = CARTESIAN_POINT('Ctrl Pts',(-19.3943202852577,12.2980820295986,122.161892639038)) ;
#18301 = CARTESIAN_POINT('Ctrl Pts',(-19.3637500698311,12.2966848516152,122.162387499916)) ;
#18302 = CARTESIAN_POINT('Ctrl Pts',(-19.3384780035975,12.2955339128568,122.163564411745)) ;
#18303 = CARTESIAN_POINT('Ctrl Pts',(-19.2906845727353,12.2933512318317,122.167246330981)) ;
#18304 = CARTESIAN_POINT('Ctrl Pts',(-19.2681616561263,12.2923200618826,122.16959843275)) ;
#18305 = CARTESIAN_POINT('Ctrl Pts',(-19.2401756423187,12.2910301254465,122.173292036207)) ;
#18306 = CARTESIAN_POINT('Ctrl Pts',(-19.2346411055983,12.2907746070115,122.174060275935)) ;
#18307 = CARTESIAN_POINT('Ctrl Pts',(-19.2223537945282,12.2902062672279,122.175849910196)) ;
#18308 = CARTESIAN_POINT('Ctrl Pts',(-19.2156038663577,12.2898933420975,122.176889590148)) ;
#18309 = CARTESIAN_POINT('Ctrl Pts',(-19.1904972080944,12.2887270000533,122.180967632988)) ;
#18310 = CARTESIAN_POINT('Ctrl Pts',(-19.1722005295293,12.2878722713777,122.184360417084)) ;
#18311 = CARTESIAN_POINT('Ctrl Pts',(-19.1403098492094,12.2863757976791,122.191013635334)) ;
#18312 = CARTESIAN_POINT('Ctrl Pts',(-19.1266825098048,12.2857341492844,122.194095921746)) ;
#18313 = CARTESIAN_POINT('Ctrl Pts',(-19.110813865766,12.2849845803541,122.197965870317)) ;
#18314 = CARTESIAN_POINT('Ctrl Pts',(-19.1085168015902,12.284876020602,122.198532961923)) ;
#18315 = CARTESIAN_POINT('Ctrl Pts',(-19.1015386210917,12.2845460392018,122.200276781587)) ;
#18316 = CARTESIAN_POINT('Ctrl Pts',(-19.096862691438,12.2843246784062,122.201474094536)) ;
#18317 = CARTESIAN_POINT('Ctrl Pts',(-19.0827599510133,12.2836562933839,122.205172395672)) ;
#18318 = CARTESIAN_POINT('Ctrl Pts',(-19.0733553516249,12.2832095543121,122.20775665796)) ;
#18319 = CARTESIAN_POINT('Ctrl Pts',(-19.0523916685137,12.2822113184325,122.213781941223)) ;
#18320 = CARTESIAN_POINT('Ctrl Pts',(-19.0408501819625,12.281660090464,122.217280724036)) ;
#18321 = CARTESIAN_POINT('Ctrl Pts',(-19.0153625143223,12.2804385890047,122.225411806087)) ;
#18322 = CARTESIAN_POINT('Ctrl Pts',(-19.0014437770044,12.2797688841339,122.230124114127)) ;
#18323 = CARTESIAN_POINT('Ctrl Pts',(-18.9712843919364,12.2783081133726,122.240931176282)) ;
#18324 = CARTESIAN_POINT('Ctrl Pts',(-18.9550810446259,12.2775169566702,122.247120777925)) ;
#18325 = CARTESIAN_POINT('Ctrl Pts',(-18.9323864157559,12.2763968647427,122.25633565762)) ;
#18326 = CARTESIAN_POINT('Ctrl Pts',(-18.9257842783509,12.2760695777695,122.259082599512)) ;
#18327 = CARTESIAN_POINT('Ctrl Pts',(-18.918638433755,12.2757136824681,122.262127951505)) ;
#18328 = CARTESIAN_POINT('Ctrl Pts',(-18.9180709595142,12.2756854083269,122.262370289258)) ;
#18329 = CARTESIAN_POINT('Ctrl Pts',(-18.9117455598407,12.2753701210517,122.265077067178)) ;
#18330 = CARTESIAN_POINT('Ctrl Pts',(-18.9060060664993,12.2750828608151,122.267584324291)) ;
#18331 = CARTESIAN_POINT('Ctrl Pts',(-18.9002450930505,12.2747933090545,122.270152696087)) ;
#18332 = CARTESIAN_POINT('Ctrl Pts',(-18.9002045177652,12.2747912696429,122.270170788056)) ;
#18333 = CARTESIAN_POINT('Ctrl Pts',(-18.9001238435967,12.2747872146438,122.270206764731)) ;
#18334 = CARTESIAN_POINT('Ctrl Pts',(-18.9000837447658,12.2747851990603,122.270224649351)) ;
#18335 = CARTESIAN_POINT('Ctrl Pts',(-18.9000039974015,12.2747811904094,122.270260222792)) ;
#18336 = CARTESIAN_POINT('Ctrl Pts',(-18.8999643486846,12.2747791973341,122.270277911637)) ;
#18337 = CARTESIAN_POINT('Ctrl Pts',(-18.8998854756348,12.2747752324008,122.270313104921)) ;
#18338 = CARTESIAN_POINT('Ctrl Pts',(-18.8998462514276,12.2747732605504,122.270330609251)) ;
#18339 = CARTESIAN_POINT('Ctrl Pts',(-18.8997682031301,12.2747693368507,122.270365444176)) ;
#18340 = CARTESIAN_POINT('Ctrl Pts',(-18.8997293789889,12.274767385,122.270382774746)) ;
#18341 = CARTESIAN_POINT('Ctrl Pts',(-18.8996521075579,12.2747635001334,122.270417272393)) ;
#18342 = CARTESIAN_POINT('Ctrl Pts',(-18.8996136600522,12.2747615671078,122.27043443952)) ;
#18343 = CARTESIAN_POINT('Ctrl Pts',(-18.8901227457624,12.2742843787962,122.274672785936)) ;
#18344 = CARTESIAN_POINT('Ctrl Pts',(-18.8807231096184,12.2738084572363,122.279011211801)) ;
#18345 = CARTESIAN_POINT('Ctrl Pts',(-18.8584552144583,12.2726730772487,122.289626515565)) ;
#18346 = CARTESIAN_POINT('Ctrl Pts',(-18.8456387735708,12.2720131872733,122.296008701345)) ;
#18347 = CARTESIAN_POINT('Ctrl Pts',(-18.8034859099685,12.2698233381113,122.317911124905)) ;
#18348 = CARTESIAN_POINT('Ctrl Pts',(-18.7746579481472,12.268296215917,122.334379405317)) ;
#18349 = CARTESIAN_POINT('Ctrl Pts',(-18.729774918897,12.2658636237062,122.36244626291)) ;
#18350 = CARTESIAN_POINT('Ctrl Pts',(-18.7132808206666,12.2649570395387,122.373312573618)) ;
#18351 = CARTESIAN_POINT('Ctrl Pts',(-18.6858255325879,12.2634248487849,122.392348106488)) ;
#18352 = CARTESIAN_POINT('Ctrl Pts',(-18.6747282917063,12.2627989047404,122.400314597226)) ;
#18353 = CARTESIAN_POINT('Ctrl Pts',(-18.6588867192605,12.2618953578861,122.412085156003)) ;
#18354 = CARTESIAN_POINT('Ctrl Pts',(-18.6540360857326,12.2616173103472,122.41574445152)) ;
#18355 = CARTESIAN_POINT('Ctrl Pts',(-18.6196057881474,12.2596336692377,122.442114602542)) ;
#18356 = CARTESIAN_POINT('Ctrl Pts',(-18.5910288274408,12.25793525988,122.46610380482)) ;
#18357 = CARTESIAN_POINT('Ctrl Pts',(-18.5446811999161,12.2550642157518,122.508686412553)) ;
#18358 = CARTESIAN_POINT('Ctrl Pts',(-18.5263338269143,12.2538936811264,122.526615225297)) ;
#18359 = CARTESIAN_POINT('Ctrl Pts',(-18.5004252806398,12.2521846431382,122.553540196993)) ;
#18360 = CARTESIAN_POINT('Ctrl Pts',(-18.4924186937888,12.2516482177633,122.562098579029)) ;
#18361 = CARTESIAN_POINT('Ctrl Pts',(-18.4765275394243,12.2505661431255,122.579571061819)) ;
#18362 = CARTESIAN_POINT('Ctrl Pts',(-18.4686475438167,12.2500205336862,122.588487715261)) ;
#18363 = CARTESIAN_POINT('Ctrl Pts',(-18.4596648071987,12.2493877277592,122.598949492375)) ;
#18364 = CARTESIAN_POINT('Ctrl Pts',(-18.4584367967134,12.2493009783825,122.600386279844)) ;
#18365 = CARTESIAN_POINT('Ctrl Pts',(-18.4540964245262,12.2489935107512,122.605487951596)) ;
#18366 = CARTESIAN_POINT('Ctrl Pts',(-18.4510019563454,12.248772737706,122.609168000239)) ;
#18367 = CARTESIAN_POINT('Ctrl Pts',(-18.4364374526138,12.2477261432029,122.626692895836)) ;
#18368 = CARTESIAN_POINT('Ctrl Pts',(-18.4252457743225,12.2468996133807,122.640766274439)) ;
#18369 = CARTESIAN_POINT('Ctrl Pts',(-18.3970626550235,12.2447585189469,122.677819622791)) ;
#18370 = CARTESIAN_POINT('Ctrl Pts',(-18.3805486588605,12.2434439300822,122.7011496581)) ;
#18371 = CARTESIAN_POINT('Ctrl Pts',(-18.3641079048297,12.2420706366636,122.72615166601)) ;
#18372 = CARTESIAN_POINT('Ctrl Pts',(-18.363368930255,12.2420087663343,122.727279419964)) ;
#18373 = CARTESIAN_POINT('Ctrl Pts',(-18.3618263016116,12.2418793090405,122.729641965138)) ;
#18374 = CARTESIAN_POINT('Ctrl Pts',(-18.3610230029253,12.241811723894,122.730876986113)) ;
#18375 = CARTESIAN_POINT('Ctrl Pts',(-18.3592869206189,12.2416652856262,122.733556455323)) ;
#18376 = CARTESIAN_POINT('Ctrl Pts',(-18.3583549299985,12.2415864367627,122.735001414096)) ;
#18377 = CARTESIAN_POINT('Ctrl Pts',(-18.35578853018,12.2413686612092,122.738998443687)) ;
#18378 = CARTESIAN_POINT('Ctrl Pts',(-18.3541604150833,12.2412297703263,122.741554543885)) ;
#18379 = CARTESIAN_POINT('Ctrl Pts',(-18.34901876643,12.2407888109909,122.749691963831)) ;
#18380 = CARTESIAN_POINT('Ctrl Pts',(-18.3455401023303,12.2404869920065,122.755295178696)) ;
#18381 = CARTESIAN_POINT('Ctrl Pts',(-18.3379625151143,12.2398216208448,122.767719032272)) ;
#18382 = CARTESIAN_POINT('Ctrl Pts',(-18.3338840517041,12.2394581818918,122.774551805886)) ;
#18383 = CARTESIAN_POINT('Ctrl Pts',(-18.3203920329754,12.2382369966701,122.797653806684)) ;
#18384 = CARTESIAN_POINT('Ctrl Pts',(-18.311280246106,12.2373803772665,122.814096304466)) ;
#18385 = CARTESIAN_POINT('Ctrl Pts',(-18.2911935706694,12.2354100982693,122.85235378503)) ;
#18386 = CARTESIAN_POINT('Ctrl Pts',(-18.2804801919914,12.2342965057199,122.874297335255)) ;
#18387 = CARTESIAN_POINT('Ctrl Pts',(-18.2662453165183,12.2327174067882,122.905759187717)) ;
#18388 = CARTESIAN_POINT('Ctrl Pts',(-18.2621864058117,12.2322543060521,122.915028215334)) ;
#18389 = CARTESIAN_POINT('Ctrl Pts',(-18.2550235982066,12.2314127743658,122.931941333661)) ;
#18390 = CARTESIAN_POINT('Ctrl Pts',(-18.251881982541,12.2310345295728,122.939568830559)) ;
#18391 = CARTESIAN_POINT('Ctrl Pts',(-18.2479664032967,12.2305510393385,122.949349243928)) ;
#18392 = CARTESIAN_POINT('Ctrl Pts',(-18.2471225296527,12.2304460958085,122.951473963436)) ;
#18393 = CARTESIAN_POINT('Ctrl Pts',(-18.2454472212734,12.2302362570263,122.955726050333)) ;
#18394 = CARTESIAN_POINT('Ctrl Pts',(-18.2446157789638,12.2301313622132,122.957853405489)) ;
#18395 = CARTESIAN_POINT('Ctrl Pts',(-18.2430841197492,12.2299367181332,122.961804263218)) ;
#18396 = CARTESIAN_POINT('Ctrl Pts',(-18.2423823371754,12.2298469755033,122.963627151649)) ;
#18397 = CARTESIAN_POINT('Ctrl Pts',(-18.233728298671,12.2287333183734,122.986264228168)) ;
#18398 = CARTESIAN_POINT('Ctrl Pts',(-18.2263297036955,12.2277073069662,123.007285718844)) ;
#18399 = CARTESIAN_POINT('Ctrl Pts',(-18.214337801579,12.2259042432553,123.044506945988)) ;
#18400 = CARTESIAN_POINT('Ctrl Pts',(-18.2095024578894,12.2251279733657,123.060622791061)) ;
#18401 = CARTESIAN_POINT('Ctrl Pts',(-18.1998067486145,12.2234591172079,123.095479277654)) ;
#18402 = CARTESIAN_POINT('Ctrl Pts',(-18.1950534336388,12.2225668174507,123.114245284689)) ;
#18403 = CARTESIAN_POINT('Ctrl Pts',(-18.1893717760513,12.2213952032092,123.139086654396)) ;
#18404 = CARTESIAN_POINT('Ctrl Pts',(-18.1880496822321,12.2211137745665,123.145069147926)) ;
#18405 = CARTESIAN_POINT('Ctrl Pts',(-18.1857893972217,12.2206166445939,123.155666139424)) ;
#18406 = CARTESIAN_POINT('Ctrl Pts',(-18.1848331988293,12.220400819434,123.160276664812)) ;
#18407 = CARTESIAN_POINT('Ctrl Pts',(-18.1824333868243,12.2198443859124,123.172185919867)) ;
#18408 = CARTESIAN_POINT('Ctrl Pts',(-18.1810288431811,12.2195040264401,123.17949234274)) ;
#18409 = CARTESIAN_POINT('Ctrl Pts',(-18.1766059563161,12.2183807461962,123.20366221221)) ;
#18410 = CARTESIAN_POINT('Ctrl Pts',(-18.1738690426115,12.2175989178843,123.22057517632)) ;
#18411 = CARTESIAN_POINT('Ctrl Pts',(-18.1691061808155,12.21603901677,123.254403436511)) ;
#18412 = CARTESIAN_POINT('Ctrl Pts',(-18.1670766631612,12.2152611132664,123.27131453819)) ;
#18413 = CARTESIAN_POINT('Ctrl Pts',(-18.1646428192148,12.2141343776665,123.295817523801)) ;
#18414 = CARTESIAN_POINT('Ctrl Pts',(-18.1639611801692,12.2137866922403,123.303379932456)) ;
#18415 = CARTESIAN_POINT('Ctrl Pts',(-18.1628689072857,12.2131663096348,123.316871938782)) ;
#18416 = CARTESIAN_POINT('Ctrl Pts',(-18.1624315836002,12.2128937404882,123.322799144614)) ;
#18417 = CARTESIAN_POINT('Ctrl Pts',(-18.1614290089668,12.2122014674298,123.337849332735)) ;
#18418 = CARTESIAN_POINT('Ctrl Pts',(-18.1609215222235,12.2117815076055,123.346975797005)) ;
#18419 = CARTESIAN_POINT('Ctrl Pts',(-18.1602635259034,12.2111023445527,123.361725694803)) ;
#18420 = CARTESIAN_POINT('Ctrl Pts',(-18.1600507988238,12.2108434482576,123.36734602186)) ;
#18421 = CARTESIAN_POINT('Ctrl Pts',(-18.15929935674,12.2097297218122,123.391514022561)) ;
#18422 = CARTESIAN_POINT('Ctrl Pts',(-18.1591357380438,12.2088736550973,123.410070988659)) ;
#18423 = CARTESIAN_POINT('Ctrl Pts',(-18.1595676857259,12.2073935829303,123.442187280998)) ;
#18424 = CARTESIAN_POINT('Ctrl Pts',(-18.1599708359102,12.2067691775243,123.455746029733)) ;
#18425 = CARTESIAN_POINT('Ctrl Pts',(-18.1608769099055,12.2058638878957,123.475428887471)) ;
#18426 = CARTESIAN_POINT('Ctrl Pts',(-18.1612044345401,12.205582049248,123.481560052821)) ;
#18427 = CARTESIAN_POINT('Ctrl Pts',(-18.1618840520735,12.2050686225412,123.492735860338)) ;
#18428 = CARTESIAN_POINT('Ctrl Pts',(-18.1622216097911,12.2048369459569,123.497781252151)) ;
#18429 = CARTESIAN_POINT('Ctrl Pts',(-18.1629363815045,12.2043875693017,123.507572400197)) ;
#18430 = CARTESIAN_POINT('Ctrl Pts',(-18.1633101105923,12.2041698487456,123.512318323823)) ;
#18431 = CARTESIAN_POINT('Ctrl Pts',(-18.1642130828346,12.2036798223058,123.5230046184)) ;
#18432 = CARTESIAN_POINT('Ctrl Pts',(-18.1647577459922,12.2034076348197,123.528943575076)) ;
#18433 = CARTESIAN_POINT('Ctrl Pts',(-18.1674587481127,12.2021569478018,123.556245214178)) ;
#18434 = CARTESIAN_POINT('Ctrl Pts',(-18.1701214789119,12.2011833699327,123.577544331091)) ;
#18435 = CARTESIAN_POINT('Ctrl Pts',(-18.1733329056176,12.2002114875201,123.598774179907)) ;
#18436 = CARTESIAN_POINT('Origin',(-19.409269639048,-13.9999999999504,123.411833654989)) ;
#18437 = CARTESIAN_POINT('',(-17.409466984686,-13.6999999999504,123.383738395492)) ;
#18438 = CARTESIAN_POINT('Origin',(-19.4092696390481,-13.6999999999504,123.411833654989)) ;
#18439 = CARTESIAN_POINT('',(-17.409466984686,13.7000000000496,123.383738395492)) ;
#18440 = CARTESIAN_POINT('',(-17.4094669846859,-13.9999999999504,123.383738395492)) ;
#18441 = CARTESIAN_POINT('Origin',(-19.4092696390481,13.7000000000496,123.411833654989)) ;
#18442 = CARTESIAN_POINT('',(-21.3014729215226,12.450000004364,122.764093940449)) ;
#18443 = CARTESIAN_POINT('Ctrl Pts',(-21.3014729215226,12.4500000043639,122.764093940449)) ;
#18444 = CARTESIAN_POINT('Ctrl Pts',(-21.2417386817332,12.4533908072994,122.58468313231)) ;
#18445 = CARTESIAN_POINT('Ctrl Pts',(-21.1183669661588,12.3003323944147,122.368106075024)) ;
#18446 = CARTESIAN_POINT('Ctrl Pts',(-21.0828841600767,12.0313004597594,122.317703938634)) ;
#18447 = CARTESIAN_POINT('Ctrl Pts',(-21.0912110587446,11.9055147635765,122.329236338449)) ;
#18448 = CARTESIAN_POINT('Ctrl Pts',(-21.1188098709144,11.7623911882616,122.373395814998)) ;
#18449 = CARTESIAN_POINT('Ctrl Pts',(-21.1966797848952,11.6016650881281,122.503047298049)) ;
#18450 = CARTESIAN_POINT('Ctrl Pts',(-21.3085421953233,11.5240330679577,122.761739092861)) ;
#18451 = CARTESIAN_POINT('Ctrl Pts',(-21.3785516269951,11.6016367477315,123.03446770917)) ;
#18452 = CARTESIAN_POINT('Ctrl Pts',(-21.3966874043036,11.7624517905451,123.184919968199)) ;
#18453 = CARTESIAN_POINT('Ctrl Pts',(-21.4016453124917,11.905416630659,123.236367319138)) ;
#18454 = CARTESIAN_POINT('Ctrl Pts',(-21.4027247828246,12.0315229430405,123.251325161369)) ;
#18455 = CARTESIAN_POINT('Ctrl Pts',(-21.3995856881047,12.2128162203883,123.208193040234)) ;
#18456 = CARTESIAN_POINT('Ctrl Pts',(-21.3783532801531,12.3983256286576,123.034306001354)) ;
#18457 = CARTESIAN_POINT('Ctrl Pts',(-21.3321155076486,12.450187696004,122.852788427119)) ;
#18458 = CARTESIAN_POINT('Ctrl Pts',(-21.3014729215226,12.4500000043639,122.764093940449)) ;
#18459 = CARTESIAN_POINT('',(-17.5170663566028,12.4500000035941,124.059573369615)) ;
#18460 = CARTESIAN_POINT('Ctrl Pts',(-17.5170663566028,12.4500000035941,124.059573369615)) ;
#18461 = CARTESIAN_POINT('Ctrl Pts',(-17.5768010750503,12.4533889497169,124.238978500622)) ;
#18462 = CARTESIAN_POINT('Ctrl Pts',(-17.7001719976827,12.3003338187364,124.455565035223)) ;
#18463 = CARTESIAN_POINT('Ctrl Pts',(-17.735655182611,12.0313017495778,124.505966784337)) ;
#18464 = CARTESIAN_POINT('Ctrl Pts',(-17.727328311671,11.9055139654912,124.494427918119)) ;
#18465 = CARTESIAN_POINT('Ctrl Pts',(-17.6997289374594,11.7623915473154,124.450272614137)) ;
#18466 = CARTESIAN_POINT('Ctrl Pts',(-17.6218598761679,11.6016648611214,124.320619335508)) ;
#18467 = CARTESIAN_POINT('Ctrl Pts',(-17.5099968647986,11.5240331921794,124.061928577266)) ;
#18468 = CARTESIAN_POINT('Ctrl Pts',(-17.4399877214087,11.6016367193622,123.789199422435)) ;
#18469 = CARTESIAN_POINT('Ctrl Pts',(-17.4218519288077,11.7624517529768,123.638747342328)) ;
#18470 = CARTESIAN_POINT('Ctrl Pts',(-17.4168941310285,11.9054163828466,123.587299846138)) ;
#18471 = CARTESIAN_POINT('Ctrl Pts',(-17.415814460062,12.0315228305656,123.572342418142)) ;
#18472 = CARTESIAN_POINT('Ctrl Pts',(-17.4189536889037,12.2128158889338,123.615474365746)) ;
#18473 = CARTESIAN_POINT('Ctrl Pts',(-17.4401858916256,12.3983259401867,123.789361234211)) ;
#18474 = CARTESIAN_POINT('Ctrl Pts',(-17.486423826463,12.4501875413069,123.970878916215)) ;
#18475 = CARTESIAN_POINT('Ctrl Pts',(-17.5170663566028,12.4500000035941,124.059573369615)) ;
#18476 = CARTESIAN_POINT('',(-17.5170663564952,-12.4500000035939,124.059573369301)) ;
#18477 = CARTESIAN_POINT('Ctrl Pts',(-17.5170663564952,-12.4500000035939,
124.059573369301)) ;
#18478 = CARTESIAN_POINT('Ctrl Pts',(-17.4543214499664,-12.4533908062079,
123.881193173708)) ;
#18479 = CARTESIAN_POINT('Ctrl Pts',(-17.4190874317839,-12.3003323949396,
123.634444787988)) ;
#18480 = CARTESIAN_POINT('Ctrl Pts',(-17.4162387146148,-12.0313004596384,
123.572871338394)) ;
#18481 = CARTESIAN_POINT('Ctrl Pts',(-17.4167260337872,-11.905514763682,123.587087385896)) ;
#18482 = CARTESIAN_POINT('Ctrl Pts',(-17.4219791397424,-11.76239118819,123.638896252699)) ;
#18483 = CARTESIAN_POINT('Ctrl Pts',(-17.4398990467708,-11.6016650883087,
123.789069843982)) ;
#18484 = CARTESIAN_POINT('Ctrl Pts',(-17.5100369831582,-11.5240330679591,
124.062044775725)) ;
#18485 = CARTESIAN_POINT('Ctrl Pts',(-17.6218499912451,-11.6016367475424,
124.320463176737)) ;
#18486 = CARTESIAN_POINT('Ctrl Pts',(-17.6997200962288,-11.7624517905878,
124.450467158943)) ;
#18487 = CARTESIAN_POINT('Ctrl Pts',(-17.7273306316869,-11.9054166305896,
124.494160054312)) ;
#18488 = CARTESIAN_POINT('Ctrl Pts',(-17.7356441949461,-12.0315229428807,
124.50664151924)) ;
#18489 = CARTESIAN_POINT('Ctrl Pts',(-17.7116922052291,-12.2128162206925,
124.470634075889)) ;
#18490 = CARTESIAN_POINT('Ctrl Pts',(-17.6219076292031,-12.3983256278298,
124.320213840095)) ;
#18491 = CARTESIAN_POINT('Ctrl Pts',(-17.5472065053376,-12.4501876978419,
124.148439850519)) ;
#18492 = CARTESIAN_POINT('Ctrl Pts',(-17.5170663564952,-12.4500000035939,
124.059573369301)) ;
#18493 = CARTESIAN_POINT('',(-21.3014729215271,-12.4500000013844,122.764093940462)) ;
#18494 = CARTESIAN_POINT('Ctrl Pts',(-21.3014729215271,-12.4500000013844,
122.764093940462)) ;
#18495 = CARTESIAN_POINT('Ctrl Pts',(-21.3642139707748,-12.4533889553457,
122.942469943529)) ;
#18496 = CARTESIAN_POINT('Ctrl Pts',(-21.3994544235377,-12.3003338159049,
123.189225332334)) ;
#18497 = CARTESIAN_POINT('Ctrl Pts',(-21.4023026040227,-12.031301750527,123.250798708205)) ;
#18498 = CARTESIAN_POINT('Ctrl Pts',(-21.4018113001397,-11.9055139651401,
123.236577567789)) ;
#18499 = CARTESIAN_POINT('Ctrl Pts',(-21.3965611953891,-11.7623915476468,
123.184771653818)) ;
#18500 = CARTESIAN_POINT('Ctrl Pts',(-21.3786395141694,-11.6016648610055,
123.034597166172)) ;
#18501 = CARTESIAN_POINT('Ctrl Pts',(-21.3085026878959,-11.5240331923606,
122.761622685277)) ;
#18502 = CARTESIAN_POINT('Ctrl Pts',(-21.1966891219787,-11.6016367190622,
122.503204035368)) ;
#18503 = CARTESIAN_POINT('Ctrl Pts',(-21.118819138729,-11.7624517530713,122.373200185185)) ;
#18504 = CARTESIAN_POINT('Ctrl Pts',(-21.0912084270103,-11.9054163827587,
122.329507242695)) ;
#18505 = CARTESIAN_POINT('Ctrl Pts',(-21.0828952761476,-12.0315228306677,
122.317025982144)) ;
#18506 = CARTESIAN_POINT('Ctrl Pts',(-21.1068470535444,-12.212815888551,122.353033370586)) ;
#18507 = CARTESIAN_POINT('Ctrl Pts',(-21.1966316872743,-12.3983259410573,
122.503453345861)) ;
#18508 = CARTESIAN_POINT('Ctrl Pts',(-21.2713327489301,-12.450187539844,122.675227520146)) ;
#18509 = CARTESIAN_POINT('Ctrl Pts',(-21.3014729215271,-12.4500000013844,
122.764093940462)) ;
#18510 = CARTESIAN_POINT('Origin',(-17.409466984686,-13.9999999999504,123.383738395492)) ;
#18511 = CARTESIAN_POINT('',(-17.7094373828403,-13.9999999999504,123.387952684416)) ;
#18512 = CARTESIAN_POINT('Ctrl Pts',(-17.7094373828403,-13.9999999999504,
123.387952684416)) ;
#18513 = CARTESIAN_POINT('Ctrl Pts',(-17.7124365161054,-13.9999999999504,
123.165469985201)) ;
#18514 = CARTESIAN_POINT('Ctrl Pts',(-17.8073115029348,-13.9999999999504,
122.721754746081)) ;
#18515 = CARTESIAN_POINT('Ctrl Pts',(-18.1932733581975,-13.9999999999504,
122.161208794752)) ;
#18516 = CARTESIAN_POINT('Ctrl Pts',(-18.7644631958589,-13.9999999999504,
121.791079731755)) ;
#18517 = CARTESIAN_POINT('Ctrl Pts',(-19.4337624984685,-13.9999999999504,
121.66769040749)) ;
#18518 = CARTESIAN_POINT('Ctrl Pts',(-20.0993607034912,-13.9999999999504,
121.809828608283)) ;
#18519 = CARTESIAN_POINT('Ctrl Pts',(-20.659887032884,-13.9999999999504,122.195860778204)) ;
#18520 = CARTESIAN_POINT('Ctrl Pts',(-21.0300277648269,-13.9999999999504,
122.767014628009)) ;
#18521 = CARTESIAN_POINT('Ctrl Pts',(-21.153410552117,-13.9999999999504,123.436333440585)) ;
#18522 = CARTESIAN_POINT('Ctrl Pts',(-21.0112760309154,-13.9999999999504,
124.101920740338)) ;
#18523 = CARTESIAN_POINT('Ctrl Pts',(-20.6252417466303,-13.9999999999504,
124.66245330923)) ;
#18524 = CARTESIAN_POINT('Ctrl Pts',(-20.0540890803186,-13.9999999999504,
125.032590535832)) ;
#18525 = CARTESIAN_POINT('Ctrl Pts',(-19.3847696171533,-13.9999999999504,
125.155975257797)) ;
#18526 = CARTESIAN_POINT('Ctrl Pts',(-18.7191817607919,-13.9999999999504,
125.013838725625)) ;
#18527 = CARTESIAN_POINT('Ctrl Pts',(-18.1586286713331,-13.9999999999504,
124.627806965402)) ;
#18528 = CARTESIAN_POINT('Ctrl Pts',(-17.7885531153341,-13.9999999999504,
124.056641767528)) ;
#18529 = CARTESIAN_POINT('Ctrl Pts',(-17.7061836816795,-13.9999999999504,
123.610445192173)) ;
#18530 = CARTESIAN_POINT('Ctrl Pts',(-17.7094373828403,-13.9999999999504,
123.387952684416)) ;
#18531 = CARTESIAN_POINT('',(-18.6398461652381,-13.9999999999504,124.699448408814)) ;
#18532 = CARTESIAN_POINT('Ctrl Pts',(-20.5016202458523,-13.9999999999504,
122.804133672988)) ;
#18533 = CARTESIAN_POINT('Ctrl Pts',(-20.5261753546306,-13.9999999972095,
122.841288201641)) ;
#18534 = CARTESIAN_POINT('Ctrl Pts',(-20.5488739735137,-13.9999999999504,
122.87995874555)) ;
#18535 = CARTESIAN_POINT('Ctrl Pts',(-20.569533497391,-13.9999999999504,122.92000295199)) ;
#18536 = CARTESIAN_POINT('Ctrl Pts',(-20.5959199140017,-13.9999999999504,
122.971147553399)) ;
#18537 = CARTESIAN_POINT('Ctrl Pts',(-20.6189710732946,-14.0000000058558,
123.02451774586)) ;
#18538 = CARTESIAN_POINT('Ctrl Pts',(-20.6383380498207,-14.000000002076,123.079380090936)) ;
#18539 = CARTESIAN_POINT('Ctrl Pts',(-20.6436137949561,-14.0000000010463,
123.094325105702)) ;
#18540 = CARTESIAN_POINT('Ctrl Pts',(-20.6486160641444,-13.9999999999504,
123.109380562199)) ;
#18541 = CARTESIAN_POINT('Ctrl Pts',(-20.6533376246053,-13.9999999999504,
123.124530986896)) ;
#18542 = CARTESIAN_POINT('Ctrl Pts',(-20.6753389534758,-13.9999999999504,
123.195128298747)) ;
#18543 = CARTESIAN_POINT('Ctrl Pts',(-20.6912550483959,-13.9999999999504,
123.267816352402)) ;
#18544 = CARTESIAN_POINT('Ctrl Pts',(-20.7007692461713,-13.9999999999504,
123.342502211065)) ;
#18545 = CARTESIAN_POINT('Ctrl Pts',(-20.7075651409922,-13.9999999999504,
123.395849561211)) ;
#18546 = CARTESIAN_POINT('Ctrl Pts',(-20.7110948242437,-14.0000000154151,
123.450221687122)) ;
#18547 = CARTESIAN_POINT('Ctrl Pts',(-20.7112100367005,-14.0000000076297,
123.504837175163)) ;
#18548 = CARTESIAN_POINT('Ctrl Pts',(-20.7112556701211,-14.000000004546,123.526469311179)) ;
#18549 = CARTESIAN_POINT('Ctrl Pts',(-20.7107656107305,-13.9999999999504,
123.548139053146)) ;
#18550 = CARTESIAN_POINT('Ctrl Pts',(-20.7097305817929,-13.9999999999504,
123.569795580814)) ;
#18551 = CARTESIAN_POINT('Ctrl Pts',(-20.7060894144257,-13.9999999999504,
123.645981896936)) ;
#18552 = CARTESIAN_POINT('Ctrl Pts',(-20.6957047852943,-13.9999999999504,
123.721939102819)) ;
#18553 = CARTESIAN_POINT('Ctrl Pts',(-20.6787691492058,-13.9999999999504,
123.796817076466)) ;
#18554 = CARTESIAN_POINT('Ctrl Pts',(-20.6618718109643,-13.9999999999504,
123.871525722834)) ;
#18555 = CARTESIAN_POINT('Ctrl Pts',(-20.6384362784418,-13.9999999999504,
123.945249174943)) ;
#18556 = CARTESIAN_POINT('Ctrl Pts',(-20.6081226092438,-13.9999999999504,
124.017450827467)) ;
#18557 = CARTESIAN_POINT('Ctrl Pts',(-20.5874065939798,-13.9999999999504,
124.06679261206)) ;
#18558 = CARTESIAN_POINT('Ctrl Pts',(-20.5634867253231,-14.0000000147266,
124.115399835518)) ;
#18559 = CARTESIAN_POINT('Ctrl Pts',(-20.5367348692554,-14.000000008255,124.162498288013)) ;
#18560 = CARTESIAN_POINT('Ctrl Pts',(-20.5244438287527,-14.0000000052816,
124.184137496364)) ;
#18561 = CARTESIAN_POINT('Ctrl Pts',(-20.511555350795,-13.9999999999504,124.205457596068)) ;
#18562 = CARTESIAN_POINT('Ctrl Pts',(-20.4981075052899,-13.9999999999504,
124.226380393993)) ;
#18563 = CARTESIAN_POINT('Ctrl Pts',(-20.4617166845242,-13.9999999999504,
124.282998964521)) ;
#18564 = CARTESIAN_POINT('Ctrl Pts',(-20.421232808245,-13.9999999879782,124.33670346053)) ;
#18565 = CARTESIAN_POINT('Ctrl Pts',(-20.376464367816,-13.9999999971152,124.38762656574)) ;
#18566 = CARTESIAN_POINT('Ctrl Pts',(-20.3687787652624,-13.9999999986838,
124.396368767695)) ;
#18567 = CARTESIAN_POINT('Ctrl Pts',(-20.3609668115105,-13.9999999999504,
124.405029094405)) ;
#18568 = CARTESIAN_POINT('Ctrl Pts',(-20.3530274377726,-13.9999999999504,
124.413608334624)) ;
#18569 = CARTESIAN_POINT('Ctrl Pts',(-20.3133866407383,-13.9999999999504,
124.456443945021)) ;
#18570 = CARTESIAN_POINT('Ctrl Pts',(-20.2705399280199,-14.0000000149581,
124.497290243693)) ;
#18571 = CARTESIAN_POINT('Ctrl Pts',(-20.224931493167,-14.0000000069191,124.535470774106)) ;
#18572 = CARTESIAN_POINT('Ctrl Pts',(-20.2082439815189,-14.0000000039777,
124.549440515625)) ;
#18573 = CARTESIAN_POINT('Ctrl Pts',(-20.1911870824665,-13.9999999999504,
124.563053006214)) ;
#18574 = CARTESIAN_POINT('Ctrl Pts',(-20.1737837366749,-13.9999999999504,
124.576273823417)) ;
#18575 = CARTESIAN_POINT('Ctrl Pts',(-20.1180757041767,-13.9999999999504,
124.618593600501)) ;
#18576 = CARTESIAN_POINT('Ctrl Pts',(-20.0588712508305,-14.0000000011967,
124.656857916382)) ;
#18577 = CARTESIAN_POINT('Ctrl Pts',(-19.9969857205583,-14.0000000002329,
124.690555964017)) ;
#18578 = CARTESIAN_POINT('Ctrl Pts',(-19.9868756103298,-14.0000000000754,
124.696061143896)) ;
#18579 = CARTESIAN_POINT('Ctrl Pts',(-19.9766940496221,-13.9999999999504,
124.70144441283)) ;
#18580 = CARTESIAN_POINT('Ctrl Pts',(-19.9664447168996,-13.9999999999504,
124.706703495921)) ;
#18581 = CARTESIAN_POINT('Ctrl Pts',(-19.8937152512031,-13.9999999999504,
124.744022052514)) ;
#18582 = CARTESIAN_POINT('Ctrl Pts',(-19.8175500316,-13.9999999999504,124.77509885579)) ;
#18583 = CARTESIAN_POINT('Ctrl Pts',(-19.7385237038216,-13.9999999999504,
124.799520306937)) ;
#18584 = CARTESIAN_POINT('Ctrl Pts',(-19.6697538216838,-13.9999999999504,
124.820772215817)) ;
#18585 = CARTESIAN_POINT('Ctrl Pts',(-19.5987827926167,-14.0000000007161,
124.83699506817)) ;
#18586 = CARTESIAN_POINT('Ctrl Pts',(-19.5264286897744,-14.0000000001071,
124.84774949464)) ;
#18587 = CARTESIAN_POINT('Ctrl Pts',(-19.5158346133764,-14.000000000018,124.849324156078)) ;
#18588 = CARTESIAN_POINT('Ctrl Pts',(-19.5052109717312,-13.9999999999504,
124.850781551346)) ;
#18589 = CARTESIAN_POINT('Ctrl Pts',(-19.4945604218811,-13.9999999999504,
124.852120270616)) ;
#18590 = CARTESIAN_POINT('Ctrl Pts',(-19.4278676945074,-13.9999999999504,
124.860503203003)) ;
#18591 = CARTESIAN_POINT('Ctrl Pts',(-19.3601518171623,-14.0000000039356,
124.864227805718)) ;
#18592 = CARTESIAN_POINT('Ctrl Pts',(-19.2923487645647,-14.0000000012686,
124.863241788224)) ;
#18593 = CARTESIAN_POINT('Ctrl Pts',(-19.2755599993829,-14.0000000006082,
124.862997639686)) ;
#18594 = CARTESIAN_POINT('Ctrl Pts',(-19.2587661385357,-13.9999999999504,
124.86246469874)) ;
#18595 = CARTESIAN_POINT('Ctrl Pts',(-19.2419818835215,-13.9999999999504,
124.861642219978)) ;
#18596 = CARTESIAN_POINT('Ctrl Pts',(-19.1575942447879,-13.9999999999504,
124.857506972949)) ;
#18597 = CARTESIAN_POINT('Ctrl Pts',(-19.0734016471759,-13.9999999999504,
124.846051708994)) ;
#18598 = CARTESIAN_POINT('Ctrl Pts',(-18.9895877266166,-13.9999999999504,
124.826900874729)) ;
#18599 = CARTESIAN_POINT('Ctrl Pts',(-18.93283525063,-13.9999999999504,124.813933371784)) ;
#18600 = CARTESIAN_POINT('Ctrl Pts',(-18.8762727270043,-14.0000000137146,
124.797440124957)) ;
#18601 = CARTESIAN_POINT('Ctrl Pts',(-18.8208080269445,-14.000000007885,124.777687193927)) ;
#18602 = CARTESIAN_POINT('Ctrl Pts',(-18.7945365568883,-14.0000000051237,
124.768330999166)) ;
#18603 = CARTESIAN_POINT('Ctrl Pts',(-18.7685120965147,-13.9999999999504,
124.758243741055)) ;
#18604 = CARTESIAN_POINT('Ctrl Pts',(-18.7428349004259,-13.9999999999504,
124.747455264173)) ;
#18605 = CARTESIAN_POINT('Ctrl Pts',(-18.7078593253204,-13.9999999999504,
124.732759999854)) ;
#18606 = CARTESIAN_POINT('Ctrl Pts',(-18.6735444651903,-13.9999999999504,
124.716770596899)) ;
#18607 = CARTESIAN_POINT('Ctrl Pts',(-18.6398461652381,-13.9999999999504,
124.699448408814)) ;
#18608 = CARTESIAN_POINT('Ctrl Pts',(-18.6398461652382,-13.9999999999504,
124.699448408814)) ;
#18609 = CARTESIAN_POINT('Ctrl Pts',(-18.5997926981249,-13.9999999999504,
124.671930427777)) ;
#18610 = CARTESIAN_POINT('Ctrl Pts',(-18.561258889765,-13.9999999999504,124.642528114611)) ;
#18611 = CARTESIAN_POINT('Ctrl Pts',(-18.524128777116,-13.9999999999504,124.611194750015)) ;
#18612 = CARTESIAN_POINT('Ctrl Pts',(-18.4794937216306,-13.9999999999504,
124.573528113221)) ;
#18613 = CARTESIAN_POINT('Ctrl Pts',(-18.4369157182474,-13.9999999853488,
124.533094940628)) ;
#18614 = CARTESIAN_POINT('Ctrl Pts',(-18.3970571422208,-13.999999991476,124.490600337269)) ;
#18615 = CARTESIAN_POINT('Ctrl Pts',(-18.3778529676017,-13.9999999944282,
124.470126104001)) ;
#18616 = CARTESIAN_POINT('Ctrl Pts',(-18.3592794755442,-13.9999999999504,
124.449172836299)) ;
#18617 = CARTESIAN_POINT('Ctrl Pts',(-18.3414075317087,-13.9999999999504,
124.427816522051)) ;
#18618 = CARTESIAN_POINT('Ctrl Pts',(-18.2894331035833,-13.9999999999504,
124.365708995856)) ;
#18619 = CARTESIAN_POINT('Ctrl Pts',(-18.2434081158356,-14.0000000065016,
124.300213424349)) ;
#18620 = CARTESIAN_POINT('Ctrl Pts',(-18.2030563822716,-14.0000000005206,
124.231473841747)) ;
#18621 = CARTESIAN_POINT('Ctrl Pts',(-18.2006458781398,-14.0000000001633,
124.227367523796)) ;
#18622 = CARTESIAN_POINT('Ctrl Pts',(-18.1982556304668,-13.9999999999504,
124.223249639981)) ;
#18623 = CARTESIAN_POINT('Ctrl Pts',(-18.1958855844258,-13.9999999999504,
124.219120225186)) ;
#18624 = CARTESIAN_POINT('Ctrl Pts',(-18.1630908596863,-13.9999999999504,
124.161980819791)) ;
#18625 = CARTESIAN_POINT('Ctrl Pts',(-18.1341509923775,-13.9999999953418,
124.102610264843)) ;
#18626 = CARTESIAN_POINT('Ctrl Pts',(-18.1094883112385,-13.9999999982308,
124.041868197465)) ;
#18627 = CARTESIAN_POINT('Ctrl Pts',(-18.1024710551584,-13.9999999990528,
124.02458529788)) ;
#18628 = CARTESIAN_POINT('Ctrl Pts',(-18.0957998868859,-13.9999999999504,
124.007191095672)) ;
#18629 = CARTESIAN_POINT('Ctrl Pts',(-18.0894841182542,-13.9999999999504,
123.989704744565)) ;
#18630 = CARTESIAN_POINT('Ctrl Pts',(-18.0670051782666,-13.9999999999504,
123.927467721639)) ;
#18631 = CARTESIAN_POINT('Ctrl Pts',(-18.0490499339531,-13.99999999282,123.864126752265)) ;
#18632 = CARTESIAN_POINT('Ctrl Pts',(-18.0355492695492,-13.9999999973936,
123.800543037458)) ;
#18633 = CARTESIAN_POINT('Ctrl Pts',(-18.0318820335418,-13.9999999986359,
123.783271555)) ;
#18634 = CARTESIAN_POINT('Ctrl Pts',(-18.0285434563634,-13.9999999999504,
123.765981864865)) ;
#18635 = CARTESIAN_POINT('Ctrl Pts',(-18.0255321109708,-13.9999999999504,
123.748690566905)) ;
#18636 = CARTESIAN_POINT('Ctrl Pts',(-18.0129887910751,-13.9999999999504,
123.676666187951)) ;
#18637 = CARTESIAN_POINT('Ctrl Pts',(-18.0061094945016,-14.0000000069732,
123.604532181164)) ;
#18638 = CARTESIAN_POINT('Ctrl Pts',(-18.0048778853208,-14.0000000012078,
123.532119117361)) ;
#18639 = CARTESIAN_POINT('Ctrl Pts',(-18.0047217791523,-14.000000000477,123.52294077888)) ;
#18640 = CARTESIAN_POINT('Ctrl Pts',(-18.0046564044181,-13.9999999999504,
123.513758025963)) ;
#18641 = CARTESIAN_POINT('Ctrl Pts',(-18.0046817237998,-13.9999999999504,
123.504570573996)) ;
#18642 = CARTESIAN_POINT('Ctrl Pts',(-18.0048326442755,-13.9999999999504,
123.44980720584)) ;
#18643 = CARTESIAN_POINT('Ctrl Pts',(-18.0082057180376,-13.9999999818479,
123.394893776504)) ;
#18644 = CARTESIAN_POINT('Ctrl Pts',(-18.0146634978623,-13.9999999892263,
123.340725835409)) ;
#18645 = CARTESIAN_POINT('Ctrl Pts',(-18.0178533092883,-13.9999999928708,
123.313969655713)) ;
#18646 = CARTESIAN_POINT('Ctrl Pts',(-18.0217957519895,-13.9999999999504,
123.287394556249)) ;
#18647 = CARTESIAN_POINT('Ctrl Pts',(-18.0264744991499,-13.9999999999504,
123.261103782795)) ;
#18648 = CARTESIAN_POINT('Ctrl Pts',(-18.0390326664452,-13.9999999999504,
123.190537043442)) ;
#18649 = CARTESIAN_POINT('Ctrl Pts',(-18.0568929261115,-14.0000000132377,
123.122029372471)) ;
#18650 = CARTESIAN_POINT('Ctrl Pts',(-18.0798718963981,-14.0000000023747,
123.05536761155)) ;
#18651 = CARTESIAN_POINT('Ctrl Pts',(-18.0828457572662,-14.0000000009689,
123.046740471181)) ;
#18652 = CARTESIAN_POINT('Ctrl Pts',(-18.0859053428976,-13.9999999999504,
123.038144318446)) ;
#18653 = CARTESIAN_POINT('Ctrl Pts',(-18.0890502468538,-13.9999999999504,
123.029578754099)) ;
#18654 = CARTESIAN_POINT('Ctrl Pts',(-18.1100272574254,-13.9999999999504,
122.972445074865)) ;
#18655 = CARTESIAN_POINT('Ctrl Pts',(-18.1348094756135,-13.9999999944962,
122.916647791952)) ;
#18656 = CARTESIAN_POINT('Ctrl Pts',(-18.1630319807289,-13.9999999977526,
122.863018295295)) ;
#18657 = CARTESIAN_POINT('Ctrl Pts',(-18.1718071281557,-13.9999999987651,
122.846343420487)) ;
#18658 = CARTESIAN_POINT('Ctrl Pts',(-18.1809149717527,-13.9999999999504,
122.829877752249)) ;
#18659 = CARTESIAN_POINT('Ctrl Pts',(-18.1903448428654,-13.9999999999504,
122.813645300798)) ;
#18660 = CARTESIAN_POINT('Ctrl Pts',(-18.2223967198354,-13.9999999999504,
122.758471637171)) ;
#18661 = CARTESIAN_POINT('Ctrl Pts',(-18.2581335738048,-13.9999999944644,
122.706050735912)) ;
#18662 = CARTESIAN_POINT('Ctrl Pts',(-18.2968706910898,-13.9999999981482,
122.656851834518)) ;
#18663 = CARTESIAN_POINT('Ctrl Pts',(-18.3064010001469,-13.9999999990546,
122.644747662385)) ;
#18664 = CARTESIAN_POINT('Ctrl Pts',(-18.3161130895013,-13.9999999999504,
122.632838342075)) ;
#18665 = CARTESIAN_POINT('Ctrl Pts',(-18.3259971142104,-13.9999999999504,
122.621130531685)) ;
#18666 = CARTESIAN_POINT('Ctrl Pts',(-18.3734383381901,-13.9999999999504,
122.564935522933)) ;
#18667 = CARTESIAN_POINT('Ctrl Pts',(-18.4248932987606,-14.0000000041903,
122.513321647355)) ;
#18668 = CARTESIAN_POINT('Ctrl Pts',(-18.4803670960102,-14.0000000003093,
122.466234561986)) ;
#18669 = CARTESIAN_POINT('Ctrl Pts',(-18.4835871984864,-14.0000000000841,
122.463501285237)) ;
#18670 = CARTESIAN_POINT('Ctrl Pts',(-18.4868208307239,-13.9999999999504,
122.460783270347)) ;
#18671 = CARTESIAN_POINT('Ctrl Pts',(-18.4900679892232,-13.9999999999504,
122.458080509819)) ;
#18672 = CARTESIAN_POINT('Ctrl Pts',(-18.5307483671629,-13.9999999999504,
122.424220345685)) ;
#18673 = CARTESIAN_POINT('Ctrl Pts',(-18.5735407603444,-13.9999999831684,
122.392763309753)) ;
#18674 = CARTESIAN_POINT('Ctrl Pts',(-18.6177141173049,-13.9999999906428,
122.364139246752)) ;
#18675 = CARTESIAN_POINT('Ctrl Pts',(-18.637808728866,-13.999999994043,122.351118062335)) ;
#18676 = CARTESIAN_POINT('Ctrl Pts',(-18.6581896700084,-13.9999999999504,
122.338682672565)) ;
#18677 = CARTESIAN_POINT('Ctrl Pts',(-18.6787909658031,-13.9999999999504,
122.326871390036)) ;
#18678 = CARTESIAN_POINT('Ctrl Pts',(-18.7400451319779,-13.9999999999504,
122.291752712553)) ;
#18679 = CARTESIAN_POINT('Ctrl Pts',(-18.8032442560716,-14.0000000082293,
122.262152793656)) ;
#18680 = CARTESIAN_POINT('Ctrl Pts',(-18.8683619735397,-14.0000000008848,
122.237841302782)) ;
#18681 = CARTESIAN_POINT('Ctrl Pts',(-18.8734510451838,-14.0000000003108,
122.235941314213)) ;
#18682 = CARTESIAN_POINT('Ctrl Pts',(-18.8785518127922,-13.9999999999504,
122.234073639899)) ;
#18683 = CARTESIAN_POINT('Ctrl Pts',(-18.8836642521681,-13.9999999999504,
122.232238176495)) ;
#18684 = CARTESIAN_POINT('Ctrl Pts',(-18.9362326297888,-13.9999999999504,
122.213365124662)) ;
#18685 = CARTESIAN_POINT('Ctrl Pts',(-18.9900459354094,-13.9999999915247,
122.197893969736)) ;
#18686 = CARTESIAN_POINT('Ctrl Pts',(-19.0442918567496,-13.999999996242,122.186032108559)) ;
#18687 = CARTESIAN_POINT('Ctrl Pts',(-19.062980568766,-13.9999999978671,122.18194548044)) ;
#18688 = CARTESIAN_POINT('Ctrl Pts',(-19.081721049772,-13.9999999999504,122.17828707369)) ;
#18689 = CARTESIAN_POINT('Ctrl Pts',(-19.1004814153796,-13.9999999999504,
122.1750648481)) ;
#18690 = CARTESIAN_POINT('Ctrl Pts',(-19.1614800110122,-13.9999999999504,
122.164587907514)) ;
#18691 = CARTESIAN_POINT('Ctrl Pts',(-19.2226231882264,-13.9999999970496,
122.158731956407)) ;
#18692 = CARTESIAN_POINT('Ctrl Pts',(-19.283163479914,-13.9999999991458,122.157230987035)) ;
#18693 = CARTESIAN_POINT('Ctrl Pts',(-19.2955014863585,-13.999999999573,122.156925092081)) ;
#18694 = CARTESIAN_POINT('Ctrl Pts',(-19.3078146229717,-13.9999999999504,
122.156800106915)) ;
#18695 = CARTESIAN_POINT('Ctrl Pts',(-19.3200968225337,-13.9999999999504,
122.156853828668)) ;
#18696 = CARTESIAN_POINT('Ctrl Pts',(-19.3561519827403,-13.9999999999504,
122.157011532215)) ;
#18697 = CARTESIAN_POINT('Ctrl Pts',(-19.3919648957125,-14.0000000079266,
122.158709422108)) ;
#18698 = CARTESIAN_POINT('Ctrl Pts',(-19.4275508050227,-13.9999999999504,
122.161948016114)) ;
#18699 = CARTESIAN_POINT('Origin',(-17.409466984686,14.0000000000496,123.383738395492)) ;
#18700 = CARTESIAN_POINT('',(-17.7094373828403,14.0000000000496,123.387952684416)) ;
#18701 = CARTESIAN_POINT('Ctrl Pts',(-17.7094373828403,14.0000000000496,123.387952684416)) ;
#18702 = CARTESIAN_POINT('Ctrl Pts',(-17.7124365161055,14.0000000000496,123.165469985201)) ;
#18703 = CARTESIAN_POINT('Ctrl Pts',(-17.8073115029348,14.0000000000496,122.721754746081)) ;
#18704 = CARTESIAN_POINT('Ctrl Pts',(-18.1932733581975,14.0000000000496,122.161208794752)) ;
#18705 = CARTESIAN_POINT('Ctrl Pts',(-18.7644631958589,14.0000000000496,121.791079731755)) ;
#18706 = CARTESIAN_POINT('Ctrl Pts',(-19.4337624984685,14.0000000000496,121.66769040749)) ;
#18707 = CARTESIAN_POINT('Ctrl Pts',(-20.0993607034912,14.0000000000496,121.809828608283)) ;
#18708 = CARTESIAN_POINT('Ctrl Pts',(-20.659887032884,14.0000000000496,122.195860778204)) ;
#18709 = CARTESIAN_POINT('Ctrl Pts',(-21.0300277648268,14.0000000000496,122.767014628009)) ;
#18710 = CARTESIAN_POINT('Ctrl Pts',(-21.153410552117,14.0000000000496,123.436333440585)) ;
#18711 = CARTESIAN_POINT('Ctrl Pts',(-21.0112760309154,14.0000000000496,124.101920740338)) ;
#18712 = CARTESIAN_POINT('Ctrl Pts',(-20.6252417466303,14.0000000000496,124.66245330923)) ;
#18713 = CARTESIAN_POINT('Ctrl Pts',(-20.0540890803185,14.0000000000496,125.032590535832)) ;
#18714 = CARTESIAN_POINT('Ctrl Pts',(-19.3847696171534,14.0000000000496,125.155975257797)) ;
#18715 = CARTESIAN_POINT('Ctrl Pts',(-18.7191817607918,14.0000000000496,125.013838725625)) ;
#18716 = CARTESIAN_POINT('Ctrl Pts',(-18.1586286713331,14.0000000000496,124.627806965402)) ;
#18717 = CARTESIAN_POINT('Ctrl Pts',(-17.7885531153341,14.0000000000496,124.056641767528)) ;
#18718 = CARTESIAN_POINT('Ctrl Pts',(-17.7061836816795,14.0000000000496,123.610445192173)) ;
#18719 = CARTESIAN_POINT('Ctrl Pts',(-17.7094373828403,14.0000000000496,123.387952684416)) ;
#18720 = CARTESIAN_POINT('',(-20.8063667317783,14.0000000000496,123.957804304199)) ;
#18721 = CARTESIAN_POINT('Ctrl Pts',(-20.8063667317783,14.0000000000496,123.957804304199)) ;
#18722 = CARTESIAN_POINT('Ctrl Pts',(-20.7903532895648,14.0000000000496,123.992143834147)) ;
#18723 = CARTESIAN_POINT('Ctrl Pts',(-20.7730358647268,14.0000000000496,124.025808018184)) ;
#18724 = CARTESIAN_POINT('Ctrl Pts',(-20.7544032477939,14.0000000000496,124.058854457495)) ;
#18725 = CARTESIAN_POINT('Ctrl Pts',(-20.7255238457092,14.0000000000496,124.11007439143)) ;
#18726 = CARTESIAN_POINT('Ctrl Pts',(-20.6935075653374,14.0000000137776,124.159770107137)) ;
#18727 = CARTESIAN_POINT('Ctrl Pts',(-20.6589212017235,14.0000000079079,124.207153625976)) ;
#18728 = CARTESIAN_POINT('Ctrl Pts',(-20.6425389066613,14.0000000051277,124.229597465269)) ;
#18729 = CARTESIAN_POINT('Ctrl Pts',(-20.6255796316115,14.0000000000496,124.251523215916)) ;
#18730 = CARTESIAN_POINT('Ctrl Pts',(-20.6081015241412,14.0000000000496,124.272850644239)) ;
#18731 = CARTESIAN_POINT('Ctrl Pts',(-20.5536065311287,14.0000000000496,124.339347435121)) ;
#18732 = CARTESIAN_POINT('Ctrl Pts',(-20.4940962390615,14.0000000000496,124.399995126451)) ;
#18733 = CARTESIAN_POINT('Ctrl Pts',(-20.4299459192023,14.0000000000496,124.454977940252)) ;
#18734 = CARTESIAN_POINT('Ctrl Pts',(-20.3784169085553,14.0000000000496,124.499143113613)) ;
#18735 = CARTESIAN_POINT('Ctrl Pts',(-20.3238730196464,14.0000000040184,124.539669744578)) ;
#18736 = CARTESIAN_POINT('Ctrl Pts',(-20.2670953919153,14.0000000013602,124.576016790401)) ;
#18737 = CARTESIAN_POINT('Ctrl Pts',(-20.2530365163627,14.000000000702,124.58501678942)) ;
#18738 = CARTESIAN_POINT('Ctrl Pts',(-20.238840502438,14.0000000000496,124.593760699861)) ;
#18739 = CARTESIAN_POINT('Ctrl Pts',(-20.2245188440556,14.0000000000496,124.602240638756)) ;
#18740 = CARTESIAN_POINT('Ctrl Pts',(-20.1614355826137,14.0000000000496,124.63959261211)) ;
#18741 = CARTESIAN_POINT('Ctrl Pts',(-20.095955824469,14.0000000008143,124.671799735807)) ;
#18742 = CARTESIAN_POINT('Ctrl Pts',(-20.0290025115168,14.0000000002061,124.698705425819)) ;
#18743 = CARTESIAN_POINT('Ctrl Pts',(-20.0191991796927,14.000000000117,124.702644968098)) ;
#18744 = CARTESIAN_POINT('Ctrl Pts',(-20.0093641701037,14.0000000000496,124.70647088242)) ;
#18745 = CARTESIAN_POINT('Ctrl Pts',(-19.9995002913839,14.0000000000496,124.710182706931)) ;
#18746 = CARTESIAN_POINT('Ctrl Pts',(-19.9220862328323,14.0000000000496,124.739313985635)) ;
#18747 = CARTESIAN_POINT('Ctrl Pts',(-19.8428544874908,14.0000000000496,124.761432727835)) ;
#18748 = CARTESIAN_POINT('Ctrl Pts',(-19.7625126120531,14.0000000000496,124.776513608246)) ;
#18749 = CARTESIAN_POINT('Ctrl Pts',(-19.693208445859,14.0000000000496,124.789522613036)) ;
#18750 = CARTESIAN_POINT('Ctrl Pts',(-19.6230634255686,14.0000000012919,124.797297340209)) ;
#18751 = CARTESIAN_POINT('Ctrl Pts',(-19.5530430596108,14.000000000331,124.799739393028)) ;
#18752 = CARTESIAN_POINT('Ctrl Pts',(-19.5416037822131,14.000000000174,124.800138352948)) ;
#18753 = CARTESIAN_POINT('Ctrl Pts',(-19.5301677234554,14.0000000000496,124.80039501536)) ;
#18754 = CARTESIAN_POINT('Ctrl Pts',(-19.5187389662347,14.0000000000496,124.800508987162)) ;
#18755 = CARTESIAN_POINT('Ctrl Pts',(-19.4590087648072,14.0000000000496,124.801104638865)) ;
#18756 = CARTESIAN_POINT('Ctrl Pts',(-19.3995343315883,14.0000000150306,124.797803035015)) ;
#18757 = CARTESIAN_POINT('Ctrl Pts',(-19.3411000014312,14.0000000069942,124.790869863461)) ;
#18758 = CARTESIAN_POINT('Ctrl Pts',(-19.3197195910949,14.0000000040538,124.788333100357)) ;
#18759 = CARTESIAN_POINT('Ctrl Pts',(-19.2984779242726,14.0000000000496,124.785310081673)) ;
#18760 = CARTESIAN_POINT('Ctrl Pts',(-19.2774117103375,14.0000000000496,124.78181350101)) ;
#18761 = CARTESIAN_POINT('Ctrl Pts',(-19.2102415471371,14.0000000000496,124.770664563925)) ;
#18762 = CARTESIAN_POINT('Ctrl Pts',(-19.1447976238525,13.9999999879324,124.75469117092)) ;
#18763 = CARTESIAN_POINT('Ctrl Pts',(-19.0808386295641,13.9999999971719,124.733903584227)) ;
#18764 = CARTESIAN_POINT('Ctrl Pts',(-19.0698584181317,13.9999999987581,124.730334858677)) ;
#18765 = CARTESIAN_POINT('Ctrl Pts',(-19.0589220915987,14.0000000000496,124.72662427763)) ;
#18766 = CARTESIAN_POINT('Ctrl Pts',(-19.0480285772954,14.0000000000496,124.722771939096)) ;
#18767 = CARTESIAN_POINT('Ctrl Pts',(-18.9969916069748,14.0000000000496,124.704723430421)) ;
#18768 = CARTESIAN_POINT('Ctrl Pts',(-18.9468984566506,14.0000000147882,124.683564801094)) ;
#18769 = CARTESIAN_POINT('Ctrl Pts',(-18.8985399742721,14.000000008286,124.65968813236)) ;
#18770 = CARTESIAN_POINT('Ctrl Pts',(-18.87632175014,14.0000000052986,124.648718036705)) ;
#18771 = CARTESIAN_POINT('Ctrl Pts',(-18.8544690109434,14.0000000000496,124.637173952294)) ;
#18772 = CARTESIAN_POINT('Ctrl Pts',(-18.8330550061689,14.0000000000496,124.625092613764)) ;
#18773 = CARTESIAN_POINT('Ctrl Pts',(-18.7648534752608,14.0000000000496,124.586614720823)) ;
#18774 = CARTESIAN_POINT('Ctrl Pts',(-18.7011545569484,14.0000000000496,124.542719161019)) ;
#18775 = CARTESIAN_POINT('Ctrl Pts',(-18.6420184816923,14.0000000000496,124.494038304341)) ;
#18776 = CARTESIAN_POINT('Ctrl Pts',(-18.5827483683475,14.0000000000496,124.445247107418)) ;
#18777 = CARTESIAN_POINT('Ctrl Pts',(-18.5279935908249,14.0000000000496,124.391588448733)) ;
#18778 = CARTESIAN_POINT('Ctrl Pts',(-18.4784272028069,14.0000000000496,124.33361616347)) ;
#18779 = CARTESIAN_POINT('Ctrl Pts',(-18.4428545923722,14.0000000000496,124.292010841756)) ;
#18780 = CARTESIAN_POINT('Ctrl Pts',(-18.4099776244296,14.0000000154805,124.248213063441)) ;
#18781 = CARTESIAN_POINT('Ctrl Pts',(-18.3801700432554,14.0000000076918,124.202947967025)) ;
#18782 = CARTESIAN_POINT('Ctrl Pts',(-18.3683638559556,14.0000000046068,124.185019366804)) ;
#18783 = CARTESIAN_POINT('Ctrl Pts',(-18.3570388483513,14.0000000000496,124.166860110623)) ;
#18784 = CARTESIAN_POINT('Ctrl Pts',(-18.3462169473724,14.0000000000496,124.148513408658)) ;
#18785 = CARTESIAN_POINT('Ctrl Pts',(-18.307965669138,14.0000000000496,124.083664838807)) ;
#18786 = CARTESIAN_POINT('Ctrl Pts',(-18.2759975850554,14.0000000000496,124.016471705333)) ;
#18787 = CARTESIAN_POINT('Ctrl Pts',(-18.2501194198681,14.0000000000496,123.947201515044)) ;
#18788 = CARTESIAN_POINT('Ctrl Pts',(-18.2297326885799,14.0000000000496,123.892630692673)) ;
#18789 = CARTESIAN_POINT('Ctrl Pts',(-18.2131210008505,14.0000000059345,123.836756700599)) ;
#18790 = CARTESIAN_POINT('Ctrl Pts',(-18.2004633524007,14.0000000021642,123.78038614397)) ;
#18791 = CARTESIAN_POINT('Ctrl Pts',(-18.1970152704689,14.0000000011371,123.765030187564)) ;
#18792 = CARTESIAN_POINT('Ctrl Pts',(-18.1938604966817,14.0000000000496,123.749637105053)) ;
#18793 = CARTESIAN_POINT('Ctrl Pts',(-18.1910024087544,14.0000000000496,123.734222577563)) ;
#18794 = CARTESIAN_POINT('Ctrl Pts',(-18.1827738973621,14.0000000000496,123.689843741683)) ;
#18795 = CARTESIAN_POINT('Ctrl Pts',(-18.1770067892692,13.999999997305,123.645300232667)) ;
#18796 = CARTESIAN_POINT('Ctrl Pts',(-18.1736437367582,14.0000000000496,123.600817573026)) ;
#18797 = CARTESIAN_POINT('Ctrl Pts',(-18.6288026007436,14.0000000000496,122.435409149151)) ;
#18798 = CARTESIAN_POINT('Ctrl Pts',(-18.6549557016393,14.0000000080335,122.411022804977)) ;
#18799 = CARTESIAN_POINT('Ctrl Pts',(-18.6822339839383,14.0000000000496,122.387716398644)) ;
#18800 = CARTESIAN_POINT('Ctrl Pts',(-18.7106491980473,14.0000000000496,122.36548016086)) ;
#18801 = CARTESIAN_POINT('Ctrl Pts',(-18.7581113526755,14.0000000000496,122.328338798771)) ;
#18802 = CARTESIAN_POINT('Ctrl Pts',(-18.8088016844457,13.9999999971444,122.294137942038)) ;
#18803 = CARTESIAN_POINT('Ctrl Pts',(-18.8622996253852,13.9999999992434,122.263537949972)) ;
#18804 = CARTESIAN_POINT('Ctrl Pts',(-18.8732022252909,13.9999999996712,122.257301832006)) ;
#18805 = CARTESIAN_POINT('Ctrl Pts',(-18.8842213165307,14.0000000000496,122.251215395131)) ;
#18806 = CARTESIAN_POINT('Ctrl Pts',(-18.8953531606705,14.0000000000496,122.24528442688)) ;
#18807 = CARTESIAN_POINT('Ctrl Pts',(-18.9441153362962,14.0000000000496,122.219304282725)) ;
#18808 = CARTESIAN_POINT('Ctrl Pts',(-18.995000848613,13.9999999915908,122.19632965352)) ;
#18809 = CARTESIAN_POINT('Ctrl Pts',(-19.0472579864155,13.9999999963147,122.176689567072)) ;
#18810 = CARTESIAN_POINT('Ctrl Pts',(-19.0652613628245,13.9999999979422,122.169923259465)) ;
#18811 = CARTESIAN_POINT('Ctrl Pts',(-19.0834271029694,14.0000000000496,122.163552860095)) ;
#18812 = CARTESIAN_POINT('Ctrl Pts',(-19.1017230829542,14.0000000000496,122.157592198567)) ;
#18813 = CARTESIAN_POINT('Ctrl Pts',(-19.1678091301422,14.0000000000496,122.13606197393)) ;
#18814 = CARTESIAN_POINT('Ctrl Pts',(-19.2356127427886,14.0000000082481,122.119870825476)) ;
#18815 = CARTESIAN_POINT('Ctrl Pts',(-19.3052501799436,14.0000000009742,122.109217226808)) ;
#18816 = CARTESIAN_POINT('Ctrl Pts',(-19.3106926051813,14.0000000004057,122.108384608369)) ;
#18817 = CARTESIAN_POINT('Ctrl Pts',(-19.3161462578174,14.0000000000496,122.107585811876)) ;
#18818 = CARTESIAN_POINT('Ctrl Pts',(-19.3216112068833,14.0000000000496,122.106820931957)) ;
#18819 = CARTESIAN_POINT('Ctrl Pts',(-19.3733096004345,14.0000000000496,122.099585171368)) ;
#18820 = CARTESIAN_POINT('Ctrl Pts',(-19.4260182147184,13.9999999832307,122.095385120388)) ;
#18821 = CARTESIAN_POINT('Ctrl Pts',(-19.4789196753301,13.999999990678,122.094329066821)) ;
#18822 = CARTESIAN_POINT('Ctrl Pts',(-19.5029846994337,13.9999999940658,122.093848665065)) ;
#18823 = CARTESIAN_POINT('Ctrl Pts',(-19.5270889190625,14.0000000000496,122.094018890807)) ;
#18824 = CARTESIAN_POINT('Ctrl Pts',(-19.5511518125165,14.0000000000496,122.094849910452)) ;
#18825 = CARTESIAN_POINT('Ctrl Pts',(-19.6238904012892,14.0000000000496,122.097361960648)) ;
#18826 = CARTESIAN_POINT('Ctrl Pts',(-19.6962268249112,14.0000000042239,122.105911687139)) ;
#18827 = CARTESIAN_POINT('Ctrl Pts',(-19.7681953794014,14.0000000004026,122.120538847728)) ;
#18828 = CARTESIAN_POINT('Ctrl Pts',(-19.7723731078155,14.0000000001808,122.121387945016)) ;
#18829 = CARTESIAN_POINT('Ctrl Pts',(-19.776549611116,14.0000000000496,122.122257522262)) ;
#18830 = CARTESIAN_POINT('Ctrl Pts',(-19.7807249013257,14.0000000000496,122.123147587728)) ;
#18831 = CARTESIAN_POINT('Ctrl Pts',(-19.8416350175698,14.0000000000496,122.136132072222)) ;
#18832 = CARTESIAN_POINT('Ctrl Pts',(-19.9023447220298,13.9999999945544,122.153488502169)) ;
#18833 = CARTESIAN_POINT('Ctrl Pts',(-19.9620381343026,13.9999999982432,122.175266965352)) ;
#18834 = CARTESIAN_POINT('Ctrl Pts',(-19.9767240413107,13.9999999991507,122.18062495165)) ;
#18835 = CARTESIAN_POINT('Ctrl Pts',(-19.9913481896679,14.0000000000496,122.186250566072)) ;
#18836 = CARTESIAN_POINT('Ctrl Pts',(-20.0058979474292,14.0000000000496,122.192144503185)) ;
#18837 = CARTESIAN_POINT('Ctrl Pts',(-20.0618576588578,14.0000000000496,122.21481312939)) ;
#18838 = CARTESIAN_POINT('Ctrl Pts',(-20.1166667194942,13.9999999945662,122.24143163317)) ;
#18839 = CARTESIAN_POINT('Ctrl Pts',(-20.1695404077726,13.9999999978326,122.271576161658)) ;
#18840 = CARTESIAN_POINT('Ctrl Pts',(-20.1859800181873,13.9999999988481,122.280948768726)) ;
#18841 = CARTESIAN_POINT('Ctrl Pts',(-20.2022322213107,14.0000000000496,122.290662026939)) ;
#18842 = CARTESIAN_POINT('Ctrl Pts',(-20.2182726032679,14.0000000000496,122.300702584319)) ;
#18843 = CARTESIAN_POINT('Ctrl Pts',(-20.278035635958,14.0000000000496,122.338111553788)) ;
#18844 = CARTESIAN_POINT('Ctrl Pts',(-20.3348894843774,14.0000000132225,122.380082458679)) ;
#18845 = CARTESIAN_POINT('Ctrl Pts',(-20.388815293428,14.0000000024498,122.426891168377)) ;
#18846 = CARTESIAN_POINT('Ctrl Pts',(-20.395794502225,14.0000000010555,122.43294926494)) ;
#18847 = CARTESIAN_POINT('Ctrl Pts',(-20.40272471404,14.0000000000496,122.439088448526)) ;
#18848 = CARTESIAN_POINT('Ctrl Pts',(-20.4096059290759,14.0000000000496,122.445309366784)) ;
#18849 = CARTESIAN_POINT('Ctrl Pts',(-20.4497091790637,14.0000000000496,122.481564452365)) ;
#18850 = CARTESIAN_POINT('Ctrl Pts',(-20.4881440190304,13.9999999819172,122.520592261045)) ;
#18851 = CARTESIAN_POINT('Ctrl Pts',(-20.5242696457146,13.9999999892437,122.5617890429)) ;
#18852 = CARTESIAN_POINT('Ctrl Pts',(-20.5421138243492,13.9999999928626,122.58213810815)) ;
#18853 = CARTESIAN_POINT('Ctrl Pts',(-20.559394056096,14.0000000000496,122.603015774859)) ;
#18854 = CARTESIAN_POINT('Ctrl Pts',(-20.5760301136045,14.0000000000496,122.624345659934)) ;
#18855 = CARTESIAN_POINT('Ctrl Pts',(-20.6206086507397,14.0000000000496,122.681501934697)) ;
#18856 = CARTESIAN_POINT('Ctrl Pts',(-20.6605441251487,14.0000000069509,122.741883401912)) ;
#18857 = CARTESIAN_POINT('Ctrl Pts',(-20.6959233360179,14.0000000012818,122.805628776949)) ;
#18858 = CARTESIAN_POINT('Ctrl Pts',(-20.700407733753,14.0000000005632,122.813708652346)) ;
#18859 = CARTESIAN_POINT('Ctrl Pts',(-20.7048189720407,14.0000000000496,122.821842626814)) ;
#18860 = CARTESIAN_POINT('Ctrl Pts',(-20.7091572619482,14.0000000000496,122.830031031177)) ;
#18861 = CARTESIAN_POINT('Ctrl Pts',(-20.7394075255629,14.0000000000496,122.887127582083)) ;
#18862 = CARTESIAN_POINT('Ctrl Pts',(-20.7661421097676,13.9999999929068,122.94692809065)) ;
#18863 = CARTESIAN_POINT('Ctrl Pts',(-20.788786499386,13.9999999974862,123.00880613829)) ;
#18864 = CARTESIAN_POINT('Ctrl Pts',(-20.7949374004377,13.9999999987301,123.025614087398)) ;
#18865 = CARTESIAN_POINT('Ctrl Pts',(-20.8007863489826,14.0000000000496,123.042575077714)) ;
#18866 = CARTESIAN_POINT('Ctrl Pts',(-20.8063214639271,14.0000000000496,123.059675998263)) ;
#18867 = CARTESIAN_POINT('Ctrl Pts',(-20.8264435056946,14.0000000000496,123.121843711311)) ;
#18868 = CARTESIAN_POINT('Ctrl Pts',(-20.8423993087311,13.9999999954176,123.185806239041)) ;
#18869 = CARTESIAN_POINT('Ctrl Pts',(-20.8539969353865,13.9999999983166,123.250640258058)) ;
#18870 = CARTESIAN_POINT('Ctrl Pts',(-20.8572967547092,13.9999999991414,123.269087183025)) ;
#18871 = CARTESIAN_POINT('Ctrl Pts',(-20.8602437320734,14.0000000000496,123.287604337263)) ;
#18872 = CARTESIAN_POINT('Ctrl Pts',(-20.8628333957635,14.0000000000496,123.306169682356)) ;
#18873 = CARTESIAN_POINT('Ctrl Pts',(-20.8738443370904,14.0000000000496,123.385107316734)) ;
#18874 = CARTESIAN_POINT('Ctrl Pts',(-20.8784022994741,14.0000000065374,123.464956496997)) ;
#18875 = CARTESIAN_POINT('Ctrl Pts',(-20.8762013391412,14.000000000614,123.545769604119)) ;
#18876 = CARTESIAN_POINT('Ctrl Pts',(-20.8760698399773,14.0000000002601,123.5505978856)) ;
#18877 = CARTESIAN_POINT('Ctrl Pts',(-20.8759142108493,14.0000000000496,123.555429623132)) ;
#18878 = CARTESIAN_POINT('Ctrl Pts',(-20.8757343850132,14.0000000000496,123.560264833683)) ;
#18879 = CARTESIAN_POINT('Ctrl Pts',(-20.8735862885529,14.0000000000496,123.618023490037)) ;
#18880 = CARTESIAN_POINT('Ctrl Pts',(-20.8679855063018,13.9999999854137,123.676265453797)) ;
#18881 = CARTESIAN_POINT('Ctrl Pts',(-20.8590185588221,13.9999999914957,123.734052299697)) ;
#18882 = CARTESIAN_POINT('Ctrl Pts',(-20.8546982311164,13.9999999944261,123.761894339803)) ;
#18883 = CARTESIAN_POINT('Ctrl Pts',(-20.8495966167066,14.0000000000496,123.789629967368)) ;
#18884 = CARTESIAN_POINT('Ctrl Pts',(-20.8437242586452,14.0000000000496,123.817149982747)) ;
#18885 = CARTESIAN_POINT('Ctrl Pts',(-20.8335853768039,14.0000000000496,123.86466448736)) ;
#18886 = CARTESIAN_POINT('Ctrl Pts',(-20.8211538688771,14.0000000000496,123.911513268694)) ;
#18887 = CARTESIAN_POINT('Ctrl Pts',(-20.8063667317783,14.0000000000496,123.957804304199)) ;
#18888 = CARTESIAN_POINT('Ctrl Pts',(-17.409466984686,-13.6999999999504,123.383738395492)) ;
#18889 = CARTESIAN_POINT('Ctrl Pts',(-17.4129953764185,-13.6999999999504,
123.121994043902)) ;
#18890 = CARTESIAN_POINT('Ctrl Pts',(-17.524613009103,-13.6999999999504,122.599976114327)) ;
#18891 = CARTESIAN_POINT('Ctrl Pts',(-17.9786857788369,-13.6999999999504,
121.940510290626)) ;
#18892 = CARTESIAN_POINT('Ctrl Pts',(-18.6506738232679,-13.6999999999504,
121.505064333141)) ;
#18893 = CARTESIAN_POINT('Ctrl Pts',(-19.4380847682357,-13.6999999999504,
121.359900422812)) ;
#18894 = CARTESIAN_POINT('Ctrl Pts',(-20.2211414796235,-13.6999999999504,
121.527121835554)) ;
#18895 = CARTESIAN_POINT('Ctrl Pts',(-20.8805842197971,-13.6999999999504,
121.98127732928)) ;
#18896 = CARTESIAN_POINT('Ctrl Pts',(-21.3160439046833,-13.6999999999504,
122.653223034764)) ;
#18897 = CARTESIAN_POINT('Ctrl Pts',(-21.4612001247882,-13.6999999999504,
123.440656932859)) ;
#18898 = CARTESIAN_POINT('Ctrl Pts',(-21.2939830415348,-13.6999999999504,
124.223700813763)) ;
#18899 = CARTESIAN_POINT('Ctrl Pts',(-20.8398250592352,-13.6999999999504,
124.883150895787)) ;
#18900 = CARTESIAN_POINT('Ctrl Pts',(-20.1678807467438,-13.6999999999504,
125.318606455482)) ;
#18901 = CARTESIAN_POINT('Ctrl Pts',(-19.3804460839353,-13.6999999999504,
125.463764952492)) ;
#18902 = CARTESIAN_POINT('Ctrl Pts',(-18.5974015471293,-13.6999999999504,
125.296545502889)) ;
#18903 = CARTESIAN_POINT('Ctrl Pts',(-17.937927323658,-13.6999999999504,124.842390490217)) ;
#18904 = CARTESIAN_POINT('Ctrl Pts',(-17.5025443176974,-13.6999999999504,
124.17043143519)) ;
#18905 = CARTESIAN_POINT('Ctrl Pts',(-17.4056391005857,-13.6999999999504,
123.645494286554)) ;
#18906 = CARTESIAN_POINT('Ctrl Pts',(-17.409466984686,-13.6999999999504,123.383738395492)) ;
#18907 = CARTESIAN_POINT('Ctrl Pts',(-17.7094373828403,-13.9999999999504,
123.387952684416)) ;
#18908 = CARTESIAN_POINT('Ctrl Pts',(-17.7124365161054,-13.9999999999504,
123.165469985201)) ;
#18909 = CARTESIAN_POINT('Ctrl Pts',(-17.8073115029348,-13.9999999999504,
122.721754746081)) ;
#18910 = CARTESIAN_POINT('Ctrl Pts',(-18.1932733581975,-13.9999999999504,
122.161208794752)) ;
#18911 = CARTESIAN_POINT('Ctrl Pts',(-18.7644631958589,-13.9999999999504,
121.791079731755)) ;
#18912 = CARTESIAN_POINT('Ctrl Pts',(-19.4337624984685,-13.9999999999504,
121.66769040749)) ;
#18913 = CARTESIAN_POINT('Ctrl Pts',(-20.0993607034912,-13.9999999999504,
121.809828608283)) ;
#18914 = CARTESIAN_POINT('Ctrl Pts',(-20.659887032884,-13.9999999999504,122.195860778204)) ;
#18915 = CARTESIAN_POINT('Ctrl Pts',(-21.0300277648269,-13.9999999999504,
122.767014628009)) ;
#18916 = CARTESIAN_POINT('Ctrl Pts',(-21.153410552117,-13.9999999999504,123.436333440585)) ;
#18917 = CARTESIAN_POINT('Ctrl Pts',(-21.0112760309154,-13.9999999999504,
124.101920740338)) ;
#18918 = CARTESIAN_POINT('Ctrl Pts',(-20.6252417466303,-13.9999999999504,
124.66245330923)) ;
#18919 = CARTESIAN_POINT('Ctrl Pts',(-20.0540890803186,-13.9999999999504,
125.032590535832)) ;
#18920 = CARTESIAN_POINT('Ctrl Pts',(-19.3847696171533,-13.9999999999504,
125.155975257797)) ;
#18921 = CARTESIAN_POINT('Ctrl Pts',(-18.7191817607919,-13.9999999999504,
125.013838725625)) ;
#18922 = CARTESIAN_POINT('Ctrl Pts',(-18.1586286713331,-13.9999999999504,
124.627806965402)) ;
#18923 = CARTESIAN_POINT('Ctrl Pts',(-17.7885531153341,-13.9999999999504,
124.056641767528)) ;
#18924 = CARTESIAN_POINT('Ctrl Pts',(-17.7061836816795,-13.9999999999504,
123.610445192173)) ;
#18925 = CARTESIAN_POINT('Ctrl Pts',(-17.7094373828403,-13.9999999999504,
123.387952684416)) ;
#18926 = CARTESIAN_POINT('',(-17.409466984686,-13.6999999999504,123.383738395492)) ;
#18927 = CARTESIAN_POINT('Ctrl Pts',(-17.409466984686,13.7000000000496,123.383738395492)) ;
#18928 = CARTESIAN_POINT('Ctrl Pts',(-17.7094373828403,14.0000000000496,123.387952684416)) ;
#18929 = CARTESIAN_POINT('Ctrl Pts',(-17.4129953764185,13.7000000000496,123.121994043903)) ;
#18930 = CARTESIAN_POINT('Ctrl Pts',(-17.7124365161055,14.0000000000496,123.165469985201)) ;
#18931 = CARTESIAN_POINT('Ctrl Pts',(-17.524613009103,13.7000000000496,122.599976114327)) ;
#18932 = CARTESIAN_POINT('Ctrl Pts',(-17.8073115029348,14.0000000000496,122.721754746081)) ;
#18933 = CARTESIAN_POINT('Ctrl Pts',(-17.9786857788369,13.7000000000496,121.940510290626)) ;
#18934 = CARTESIAN_POINT('Ctrl Pts',(-18.1932733581975,14.0000000000496,122.161208794752)) ;
#18935 = CARTESIAN_POINT('Ctrl Pts',(-18.6506738232679,13.7000000000496,121.505064333141)) ;
#18936 = CARTESIAN_POINT('Ctrl Pts',(-18.7644631958589,14.0000000000496,121.791079731755)) ;
#18937 = CARTESIAN_POINT('Ctrl Pts',(-19.4380847682357,13.7000000000496,121.359900422812)) ;
#18938 = CARTESIAN_POINT('Ctrl Pts',(-19.4337624984685,14.0000000000496,121.66769040749)) ;
#18939 = CARTESIAN_POINT('Ctrl Pts',(-20.2211414796236,13.7000000000496,121.527121835554)) ;
#18940 = CARTESIAN_POINT('Ctrl Pts',(-20.0993607034912,14.0000000000496,121.809828608283)) ;
#18941 = CARTESIAN_POINT('Ctrl Pts',(-20.8805842197971,13.7000000000496,121.98127732928)) ;
#18942 = CARTESIAN_POINT('Ctrl Pts',(-20.659887032884,14.0000000000496,122.195860778204)) ;
#18943 = CARTESIAN_POINT('Ctrl Pts',(-21.3160439046833,13.7000000000496,122.653223034764)) ;
#18944 = CARTESIAN_POINT('Ctrl Pts',(-21.0300277648268,14.0000000000496,122.767014628009)) ;
#18945 = CARTESIAN_POINT('Ctrl Pts',(-21.4612001247882,13.7000000000496,123.440656932859)) ;
#18946 = CARTESIAN_POINT('Ctrl Pts',(-21.153410552117,14.0000000000496,123.436333440585)) ;
#18947 = CARTESIAN_POINT('Ctrl Pts',(-21.2939830415349,13.7000000000496,124.223700813763)) ;
#18948 = CARTESIAN_POINT('Ctrl Pts',(-21.0112760309154,14.0000000000496,124.101920740338)) ;
#18949 = CARTESIAN_POINT('Ctrl Pts',(-20.8398250592352,13.7000000000496,124.883150895787)) ;
#18950 = CARTESIAN_POINT('Ctrl Pts',(-20.6252417466303,14.0000000000496,124.66245330923)) ;
#18951 = CARTESIAN_POINT('Ctrl Pts',(-20.1678807467438,13.7000000000496,125.318606455482)) ;
#18952 = CARTESIAN_POINT('Ctrl Pts',(-20.0540890803185,14.0000000000496,125.032590535832)) ;
#18953 = CARTESIAN_POINT('Ctrl Pts',(-19.3804460839353,13.7000000000496,125.463764952492)) ;
#18954 = CARTESIAN_POINT('Ctrl Pts',(-19.3847696171534,14.0000000000496,125.155975257797)) ;
#18955 = CARTESIAN_POINT('Ctrl Pts',(-18.5974015471293,13.7000000000496,125.296545502889)) ;
#18956 = CARTESIAN_POINT('Ctrl Pts',(-18.7191817607918,14.0000000000496,125.013838725625)) ;
#18957 = CARTESIAN_POINT('Ctrl Pts',(-17.937927323658,13.7000000000496,124.842390490218)) ;
#18958 = CARTESIAN_POINT('Ctrl Pts',(-18.1586286713331,14.0000000000496,124.627806965402)) ;
#18959 = CARTESIAN_POINT('Ctrl Pts',(-17.5025443176974,13.7000000000496,124.17043143519)) ;
#18960 = CARTESIAN_POINT('Ctrl Pts',(-17.7885531153341,14.0000000000496,124.056641767528)) ;
#18961 = CARTESIAN_POINT('Ctrl Pts',(-17.4056391005857,13.7000000000496,123.645494286554)) ;
#18962 = CARTESIAN_POINT('Ctrl Pts',(-17.7061836816795,14.0000000000496,123.610445192173)) ;
#18963 = CARTESIAN_POINT('Ctrl Pts',(-17.409466984686,13.7000000000496,123.383738395492)) ;
#18964 = CARTESIAN_POINT('Ctrl Pts',(-17.7094373828403,14.0000000000496,123.387952684416)) ;
#18965 = CARTESIAN_POINT('',(-17.409466984686,13.7000000000496,123.383738395492)) ;
#18966 = CARTESIAN_POINT('Origin',(-19.4092722359532,-11.3545356292023,123.411814366564)) ;
#18967 = CARTESIAN_POINT('',(-19.4092722359532,-10.8644715472508,123.411814366564)) ;
#18968 = CARTESIAN_POINT('',(-18.2115676001213,-11.4089871938635,123.054038451525)) ;
#18969 = CARTESIAN_POINT('',(-18.3313380637045,-11.3545356292023,123.089816043029)) ;
#18970 = CARTESIAN_POINT('',(-18.2266423654683,-11.4089871938635,123.816643453356)) ;
#18971 = CARTESIAN_POINT('Origin',(-19.4092722359532,-11.4089871938635,123.411814366564)) ;
#18972 = CARTESIAN_POINT('Origin',(-19.4092722359532,-11.4089871938635,123.411814366564)) ;
#18973 = CARTESIAN_POINT('Origin',(-19.4092722359532,11.3545356292023,123.411814366564)) ;
#18974 = CARTESIAN_POINT('',(-20.5919021064381,11.4089871938635,123.006985279772)) ;
#18975 = CARTESIAN_POINT('',(-18.2115676001212,11.4089871938635,123.054038451525)) ;
#18976 = CARTESIAN_POINT('Origin',(-19.4092722359532,11.4089871938635,123.411814366564)) ;
#18977 = CARTESIAN_POINT('',(-19.4092722359532,10.8644715472508,123.411814366564)) ;
#18978 = CARTESIAN_POINT('',(-18.3313380637044,11.3545356292023,123.089816043029)) ;
#18979 = CARTESIAN_POINT('Origin',(-19.4092722359532,11.4089871938635,123.411814366564)) ;
#18980 = CARTESIAN_POINT('Ctrl Pts',(-20.5445170967909,10.1799890803629,123.023196933748)) ;
#18981 = CARTESIAN_POINT('Ctrl Pts',(-20.8283303706881,10.,122.926041870813)) ;
#18982 = CARTESIAN_POINT('Ctrl Pts',(-20.5894888412031,10.186615931181,123.154521494311)) ;
#18983 = CARTESIAN_POINT('Ctrl Pts',(-20.8845408159969,10.0066268508181,123.090165629856)) ;
#18984 = CARTESIAN_POINT('Ctrl Pts',(-20.6334208464893,10.199846557662,123.432353270138)) ;
#18985 = CARTESIAN_POINT('Ctrl Pts',(-20.9394617690737,10.0198574772991,123.437507823531)) ;
#18986 = CARTESIAN_POINT('Ctrl Pts',(-20.5528814488852,10.2198221789206,123.849407494597)) ;
#18987 = CARTESIAN_POINT('Ctrl Pts',(-20.8387858493119,10.0398330985578,123.958797508285)) ;
#18988 = CARTESIAN_POINT('Ctrl Pts',(-20.3351890798294,10.2397395138226,124.21264452173)) ;
#18989 = CARTESIAN_POINT('Ctrl Pts',(-20.5666727975867,10.0597504334597,124.412849839357)) ;
#18990 = CARTESIAN_POINT('Ctrl Pts',(-20.0078940908122,10.2596127905386,124.479989674566)) ;
#18991 = CARTESIAN_POINT('Ctrl Pts',(-20.157556275784,10.0796237101757,124.747029739186)) ;
#18992 = CARTESIAN_POINT('Ctrl Pts',(-19.6059540280892,10.2796372807025,124.620350189469)) ;
#18993 = CARTESIAN_POINT('Ctrl Pts',(-19.6551315118144,10.0996482003397,124.922482691163)) ;
#18994 = CARTESIAN_POINT('Ctrl Pts',(-19.1834791470516,10.2995051218533,124.615075219233)) ;
#18995 = CARTESIAN_POINT('Ctrl Pts',(-19.1270395366036,10.1195160414904,124.915890798164)) ;
#18996 = CARTESIAN_POINT('Ctrl Pts',(-18.7864839057826,10.3194507727328,124.466021113069)) ;
#18997 = CARTESIAN_POINT('Ctrl Pts',(-18.6307952228403,10.1394616923699,124.72957580943)) ;
#18998 = CARTESIAN_POINT('Ctrl Pts',(-18.4649063701951,10.3393561733498,124.190844404071)) ;
#18999 = CARTESIAN_POINT('Ctrl Pts',(-18.2288224078826,10.1593670929869,124.385607616877)) ;
#19000 = CARTESIAN_POINT('Ctrl Pts',(-18.2561330011468,10.3592304011661,123.82343533093)) ;
#19001 = CARTESIAN_POINT('Ctrl Pts',(-17.9678535157127,10.1792413208033,123.926349000794)) ;
#19002 = CARTESIAN_POINT('Ctrl Pts',(-18.1848402354332,10.3792161920437,123.40449567957)) ;
#19003 = CARTESIAN_POINT('Ctrl Pts',(-17.878734209588,10.1992271116809,123.402675114316)) ;
#19004 = CARTESIAN_POINT('Ctrl Pts',(-18.2606699010585,10.3991104347035,122.98837126667)) ;
#19005 = CARTESIAN_POINT('Ctrl Pts',(-17.973517700436,10.2191213543406,122.882519965019)) ;
#19006 = CARTESIAN_POINT('Ctrl Pts',(-18.4728612596363,10.4189891507756,122.622758653604)) ;
#19007 = CARTESIAN_POINT('Ctrl Pts',(-18.2387528910803,10.2390000704127,122.425502981447)) ;
#19008 = CARTESIAN_POINT('Ctrl Pts',(-18.7999520439114,10.4390286006202,122.349765919269)) ;
#19009 = CARTESIAN_POINT('Ctrl Pts',(-18.647614090005,10.2590395202573,122.084258749108)) ;
#19010 = CARTESIAN_POINT('Ctrl Pts',(-19.1972003355021,10.458891762158,122.205978453982)) ;
#19011 = CARTESIAN_POINT('Ctrl Pts',(-19.1441721121047,10.2789026817952,121.90452088182)) ;
#19012 = CARTESIAN_POINT('Ctrl Pts',(-19.6218813508038,10.4788711301723,122.206142579944)) ;
#19013 = CARTESIAN_POINT('Ctrl Pts',(-19.6750232066901,10.2988820498094,121.904721686728)) ;
#19014 = CARTESIAN_POINT('Ctrl Pts',(-20.0180063674985,10.4986817106951,122.349636080019)) ;
#19015 = CARTESIAN_POINT('Ctrl Pts',(-20.1701799765179,10.3186926303322,122.084083785786)) ;
#19016 = CARTESIAN_POINT('Ctrl Pts',(-20.3444408594761,10.5186626389807,122.621421727286)) ;
#19017 = CARTESIAN_POINT('Ctrl Pts',(-20.578226084171,10.3386735586178,122.423812224567)) ;
#19018 = CARTESIAN_POINT('Ctrl Pts',(-20.5574140360782,10.5385553108501,122.986919561501)) ;
#19019 = CARTESIAN_POINT('Ctrl Pts',(-20.8444469588477,10.3585662304872,122.880680954098)) ;
#19020 = CARTESIAN_POINT('Ctrl Pts',(-20.6337210602673,10.5584816411372,123.403677138751)) ;
#19021 = CARTESIAN_POINT('Ctrl Pts',(-20.9398341757817,10.3784925607743,123.40162915944)) ;
#19022 = CARTESIAN_POINT('Ctrl Pts',(-20.5626906544988,10.5784521952295,123.822322212015)) ;
#19023 = CARTESIAN_POINT('Ctrl Pts',(-20.8510572230715,10.3984631148666,123.924927290891)) ;
#19024 = CARTESIAN_POINT('Ctrl Pts',(-20.3894921739839,10.5949840343171,124.128174611121)) ;
#19025 = CARTESIAN_POINT('Ctrl Pts',(-20.6345446351863,10.4149949539542,124.307272603886)) ;
#19026 = CARTESIAN_POINT('Ctrl Pts',(-20.1931290904253,10.6083237731447,124.328455789616)) ;
#19027 = CARTESIAN_POINT('Ctrl Pts',(-20.3891097552813,10.4283346927818,124.557601822174)) ;
#19028 = CARTESIAN_POINT('Ctrl Pts',(-20.0213870270135,10.6183560153633,124.45086066554)) ;
#19029 = CARTESIAN_POINT('Ctrl Pts',(-20.1744300570267,10.4383669350004,124.710615084593)) ;
#19030 = CARTESIAN_POINT('Ctrl Pts',(-19.8344327780229,10.6282137160067,124.54030505442)) ;
#19031 = CARTESIAN_POINT('Ctrl Pts',(-19.9407404802418,10.4482246356439,124.822421617883)) ;
#19032 = CARTESIAN_POINT('Ctrl Pts',(-19.6321963819504,10.638205580646,124.597047913329)) ;
#19033 = CARTESIAN_POINT('Ctrl Pts',(-19.6879423525307,10.4582165002831,124.893352629427)) ;
#19034 = CARTESIAN_POINT('Ctrl Pts',(-19.424609722569,10.6481281304061,124.617626313307)) ;
#19035 = CARTESIAN_POINT('Ctrl Pts',(-19.4284710425139,10.4681390500432,124.919080315321)) ;
#19036 = CARTESIAN_POINT('Ctrl Pts',(-19.1462074516632,10.6614059038996,124.597234583046)) ;
#19037 = CARTESIAN_POINT('Ctrl Pts',(-19.0804105140851,10.4814168235367,124.893583985624)) ;
#19038 = CARTESIAN_POINT('Ctrl Pts',(-18.8783190629616,10.6747532428402,124.503658368855)) ;
#19039 = CARTESIAN_POINT('Ctrl Pts',(-18.7455859092888,10.4947641624773,124.776616835755)) ;
#19040 = CARTESIAN_POINT('Ctrl Pts',(-18.6486031256444,10.6879604746334,124.347593152274)) ;
#19041 = CARTESIAN_POINT('Ctrl Pts',(-18.4584522382473,10.5079713942705,124.581549246914)) ;
#19042 = CARTESIAN_POINT('Ctrl Pts',(-18.4978121198163,10.6979475907231,124.201545393376)) ;
#19043 = CARTESIAN_POINT('Ctrl Pts',(-18.269958838059,10.5179585103602,124.398989341533)) ;
#19044 = CARTESIAN_POINT('Ctrl Pts',(-18.3749610360081,10.7078984963028,124.032167626381)) ;
#19045 = CARTESIAN_POINT('Ctrl Pts',(-18.1163933969716,10.52790941594,124.187269395838)) ;
#19046 = CARTESIAN_POINT('Ctrl Pts',(-18.2826761324805,10.7179535983103,123.842018510299)) ;
#19047 = CARTESIAN_POINT('Ctrl Pts',(-18.0010345813923,10.5379645179474,123.949583784548)) ;
#19048 = CARTESIAN_POINT('Ctrl Pts',(-18.2257894495901,10.7277752716314,123.643501818388)) ;
#19049 = CARTESIAN_POINT('Ctrl Pts',(-17.9299233421522,10.5477861912685,123.701439503961)) ;
#19050 = CARTESIAN_POINT('Ctrl Pts',(-18.2033755349775,10.7378337427063,123.433255143292)) ;
#19051 = CARTESIAN_POINT('Ctrl Pts',(-17.9019040586336,10.5578446623434,123.43862866708)) ;
#19052 = CARTESIAN_POINT('Ctrl Pts',(-18.2179011335089,10.7477583538828,123.225094347349)) ;
#19053 = CARTESIAN_POINT('Ctrl Pts',(-17.9200547531203,10.5677692735199,123.178437417212)) ;
#19054 = CARTESIAN_POINT('Ctrl Pts',(-18.2846726130989,10.7610356927832,122.954084571752)) ;
#19055 = CARTESIAN_POINT('Ctrl Pts',(-18.0035329037317,10.5810466124203,122.839624585047)) ;
#19056 = CARTESIAN_POINT('Ctrl Pts',(-18.4211117191118,10.7743345720208,122.706442666777)) ;
#19057 = CARTESIAN_POINT('Ctrl Pts',(-18.174078890485,10.5943454916579,122.53009645584)) ;
#19058 = CARTESIAN_POINT('Ctrl Pts',(-18.6137282560997,10.7875734441915,122.505480302123)) ;
#19059 = CARTESIAN_POINT('Ctrl Pts',(-18.4148290889509,10.6075843638286,122.278909287836)) ;
#19060 = CARTESIAN_POINT('Ctrl Pts',(-18.7832424185157,10.7975800623281,122.380894161506)) ;
#19061 = CARTESIAN_POINT('Ctrl Pts',(-18.6267237904145,10.6175909819652,122.123170592624)) ;
#19062 = CARTESIAN_POINT('Ctrl Pts',(-18.9724474720446,10.8076110073896,122.287775791708)) ;
#19063 = CARTESIAN_POINT('Ctrl Pts',(-18.8632279358434,10.6276219270267,122.006771081612)) ;
#19064 = CARTESIAN_POINT('Ctrl Pts',(-19.1713300500782,10.8174671807414,122.229578165669)) ;
#19065 = CARTESIAN_POINT('Ctrl Pts',(-19.1118308518252,10.6374781003785,121.93402103227)) ;
#19066 = CARTESIAN_POINT('Ctrl Pts',(-19.3802073449411,10.8274664517043,122.206207727251)) ;
#19067 = CARTESIAN_POINT('Ctrl Pts',(-19.3729271808616,10.6474773713414,121.904805274484)) ;
#19068 = CARTESIAN_POINT('Ctrl Pts',(-19.5878599933699,10.8373609034616,122.219083370884)) ;
#19069 = CARTESIAN_POINT('Ctrl Pts',(-19.63249343999,10.6573718230987,121.920897070182)) ;
#19070 = CARTESIAN_POINT('Ctrl Pts',(-19.7934840277289,10.847424219271,122.268698552168)) ;
#19071 = CARTESIAN_POINT('Ctrl Pts',(-19.8895240952696,10.6674351389081,121.982913347126)) ;
#19072 = CARTESIAN_POINT('Ctrl Pts',(-19.9832086160557,10.8572630760106,122.351185619817)) ;
#19073 = CARTESIAN_POINT('Ctrl Pts',(-20.1266813029374,10.6772739956477,122.086019825898)) ;
#19074 = CARTESIAN_POINT('Ctrl Pts',(-20.1597838606521,10.8673291978282,122.467764324916)) ;
#19075 = CARTESIAN_POINT('Ctrl Pts',(-20.3474018172676,10.6873401174653,122.231740902041)) ;
#19076 = CARTESIAN_POINT('Ctrl Pts',(-20.3106209535211,10.8772124255524,122.610700532014)) ;
#19077 = CARTESIAN_POINT('Ctrl Pts',(-20.5359503275351,10.6972233451896,122.410409425907)) ;
#19078 = CARTESIAN_POINT('Ctrl Pts',(-20.4360184408181,10.8872018868312,122.779136894016)) ;
#19079 = CARTESIAN_POINT('Ctrl Pts',(-20.6926994160287,10.7072128064683,122.620953380555)) ;
#19080 = CARTESIAN_POINT('Ctrl Pts',(-20.5299682723289,10.8971655972577,122.966365986146)) ;
#19081 = CARTESIAN_POINT('Ctrl Pts',(-20.8101391925705,10.7171765168948,122.854988704109)) ;
#19082 = CARTESIAN_POINT('Ctrl Pts',(-20.5903840833054,10.9071605999886,123.167636072351)) ;
#19083 = CARTESIAN_POINT('Ctrl Pts',(-20.8856615342042,10.7271715196257,123.106575647569)) ;
#19084 = CARTESIAN_POINT('Ctrl Pts',(-20.6147046372521,10.9171969309989,123.377214474421)) ;
#19085 = CARTESIAN_POINT('Ctrl Pts',(-20.9160649147156,10.737207850636,123.368548316933)) ;
#19086 = CARTESIAN_POINT('Ctrl Pts',(-20.602840741777,10.9270431603412,123.583885830223)) ;
#19087 = CARTESIAN_POINT('Ctrl Pts',(-20.901237668564,10.7470540799783,123.626888226543)) ;
#19088 = CARTESIAN_POINT('Ctrl Pts',(-20.5549910593693,10.9370286586164,123.788252345139)) ;
#19089 = CARTESIAN_POINT('Ctrl Pts',(-20.8414280631531,10.7570395782535,123.88234711985)) ;
#19090 = CARTESIAN_POINT('Ctrl Pts',(-20.4729131510359,10.9469635615994,123.98035400042)) ;
#19091 = CARTESIAN_POINT('Ctrl Pts',(-20.7388329136923,10.7669744812365,124.122475498249)) ;
#19092 = CARTESIAN_POINT('Ctrl Pts',(-20.3571965408839,10.9570210646946,124.157283328264)) ;
#19093 = CARTESIAN_POINT('Ctrl Pts',(-20.5941893977946,10.7770319843317,124.343638489499)) ;
#19094 = CARTESIAN_POINT('Ctrl Pts',(-20.2161055904513,10.9668427210651,124.308072643193)) ;
#19095 = CARTESIAN_POINT('Ctrl Pts',(-20.4178270374552,10.7868536407023,124.532127444505)) ;
#19096 = CARTESIAN_POINT('Ctrl Pts',(-20.0473038580147,10.9768987837303,124.435324360385)) ;
#19097 = CARTESIAN_POINT('Ctrl Pts',(-20.2068264505713,10.7969097033674,124.691194003415)) ;
#19098 = CARTESIAN_POINT('Ctrl Pts',(-19.8609387437001,10.9868394484335,124.529907956578)) ;
#19099 = CARTESIAN_POINT('Ctrl Pts',(-19.9738709151238,10.8068503680706,124.809425923824)) ;
#19100 = CARTESIAN_POINT('Ctrl Pts',(-19.6619073820417,10.996743852382,124.591096321842)) ;
#19101 = CARTESIAN_POINT('Ctrl Pts',(-19.7250819168071,10.8167547720191,124.885913848072)) ;
#19102 = CARTESIAN_POINT('Ctrl Pts',(-19.4523135812511,11.0067903373756,124.6170333815)) ;
#19103 = CARTESIAN_POINT('Ctrl Pts',(-19.4630900672441,10.8268012570127,124.918337587752)) ;
#19104 = CARTESIAN_POINT('Ctrl Pts',(-19.2444994497963,11.0166865651873,124.606521749711)) ;
#19105 = CARTESIAN_POINT('Ctrl Pts',(-19.2033217042056,10.8366974848244,124.905200421478)) ;
#19106 = CARTESIAN_POINT('Ctrl Pts',(-19.038362504801,11.0267461487508,124.559366648931)) ;
#19107 = CARTESIAN_POINT('Ctrl Pts',(-18.9456501548748,10.8467570683879,124.846258925075)) ;
#19108 = CARTESIAN_POINT('Ctrl Pts',(-18.8475263552642,11.0365981584196,124.478841690953)) ;
#19109 = CARTESIAN_POINT('Ctrl Pts',(-18.7071032762899,10.8566090780567,124.745604613553)) ;
#19110 = CARTESIAN_POINT('Ctrl Pts',(-18.6712543899711,11.0465606898592,124.365745599051)) ;
#19111 = CARTESIAN_POINT('Ctrl Pts',(-18.4867618466311,10.8665716094963,124.604236201826)) ;
#19112 = CARTESIAN_POINT('Ctrl Pts',(-18.5164393691186,11.0565922380985,124.222526123336)) ;
#19113 = CARTESIAN_POINT('Ctrl Pts',(-18.2932415519936,10.8766031577357,124.425213596724)) ;
#19114 = CARTESIAN_POINT('Ctrl Pts',(-18.3904718457185,11.0664836493116,124.057073079274)) ;
#19115 = CARTESIAN_POINT('Ctrl Pts',(-18.1357799386366,10.8864945689487,124.218398117847)) ;
#19116 = CARTESIAN_POINT('Ctrl Pts',(-18.2936007393847,11.0764999030196,123.870096289376)) ;
#19117 = CARTESIAN_POINT('Ctrl Pts',(-18.0146891209222,10.8965108226567,123.984678099418)) ;
#19118 = CARTESIAN_POINT('Ctrl Pts',(-18.2310191009212,11.0865300058643,123.668736110514)) ;
#19119 = CARTESIAN_POINT('Ctrl Pts',(-17.9364599064937,10.9065409255014,123.732978598351)) ;
#19120 = CARTESIAN_POINT('Ctrl Pts',(-18.2044167485645,11.096386454818,123.463224365483)) ;
#19121 = CARTESIAN_POINT('Ctrl Pts',(-17.9032046926023,10.9163973744551,123.476088297528)) ;
#19122 = CARTESIAN_POINT('Ctrl Pts',(-18.2137726552221,11.1063854655903,123.253255515666)) ;
#19123 = CARTESIAN_POINT('Ctrl Pts',(-17.9148974747618,10.9263963852274,123.213627004979)) ;
#19124 = CARTESIAN_POINT('Ctrl Pts',(-18.2587594656026,11.1162806825083,123.050114933331)) ;
#19125 = CARTESIAN_POINT('Ctrl Pts',(-17.9711291549323,10.9362916021454,122.959700121601)) ;
#19126 = CARTESIAN_POINT('Ctrl Pts',(-18.3396629587075,11.1263411978656,122.85472528768)) ;
#19127 = CARTESIAN_POINT('Ctrl Pts',(-18.0722565351528,10.9463521175027,122.715462501341)) ;
#19128 = CARTESIAN_POINT('Ctrl Pts',(-18.4508021074728,11.1361904912527,122.67999776762)) ;
#19129 = CARTESIAN_POINT('Ctrl Pts',(-18.2111793287984,10.9562014108898,122.497051143162)) ;
#19130 = CARTESIAN_POINT('Ctrl Pts',(-18.5927075074045,11.1462176669327,122.524117766382)) ;
#19131 = CARTESIAN_POINT('Ctrl Pts',(-18.388559678523,10.9662285865698,122.302199917963)) ;
#19132 = CARTESIAN_POINT('Ctrl Pts',(-18.7598974171996,11.1562462425598,122.39565716601)) ;
#19133 = CARTESIAN_POINT('Ctrl Pts',(-18.5975457775489,10.976257162197,122.141622604304)) ;
#19134 = CARTESIAN_POINT('Ctrl Pts',(-18.9432305176374,11.1660913361057,122.299619707887)) ;
#19135 = CARTESIAN_POINT('Ctrl Pts',(-18.8267122580128,10.9861022557429,122.021573575598)) ;
#19136 = CARTESIAN_POINT('Ctrl Pts',(-19.1432259259205,11.1760825775375,122.235411488495)) ;
#19137 = CARTESIAN_POINT('Ctrl Pts',(-19.0767061726053,10.9960934971746,121.941311591283)) ;
#19138 = CARTESIAN_POINT('Ctrl Pts',(-19.3523221570473,11.1861183586808,122.207211675339)) ;
#19139 = CARTESIAN_POINT('Ctrl Pts',(-19.3380760888337,11.0061292783179,121.906059986019)) ;
#19140 = CARTESIAN_POINT('Ctrl Pts',(-19.5592805247249,11.1959705644105,122.215313540189)) ;
#19141 = CARTESIAN_POINT('Ctrl Pts',(-19.5967752495355,11.0159814840476,121.916185579079)) ;
#19142 = CARTESIAN_POINT('Ctrl Pts',(-19.7640786083089,11.2059326585275,122.259120874168)) ;
#19143 = CARTESIAN_POINT('Ctrl Pts',(-19.8527735772293,11.0259435781646,121.970943280899)) ;
#19144 = CARTESIAN_POINT('Ctrl Pts',(-19.9592440107104,11.2159552193546,122.338540115345)) ;
#19145 = CARTESIAN_POINT('Ctrl Pts',(-20.0967309229679,11.0359661389917,122.070215768955)) ;
#19146 = CARTESIAN_POINT('Ctrl Pts',(-20.1360936806095,11.2258829910061,122.449415578369)) ;
#19147 = CARTESIAN_POINT('Ctrl Pts',(-20.3177943873502,11.0458939106433,122.208809071659)) ;
#19148 = CARTESIAN_POINT('Ctrl Pts',(-20.2927527732055,11.235925375131,122.59092205436)) ;
#19149 = CARTESIAN_POINT('Ctrl Pts',(-20.513619210783,11.0559362947681,122.385690857822)) ;
#19150 = CARTESIAN_POINT('Ctrl Pts',(-20.4205680894076,11.2458145992016,122.754908938647)) ;
#19151 = CARTESIAN_POINT('Ctrl Pts',(-20.6733901753496,11.0658255188387,122.590674219405)) ;
#19152 = CARTESIAN_POINT('Ctrl Pts',(-20.5192928454941,11.2558038473689,122.940253974445)) ;
#19153 = CARTESIAN_POINT('Ctrl Pts',(-20.7967974985103,11.075814767006,122.822355021181)) ;
#19154 = CARTESIAN_POINT('Ctrl Pts',(-20.5839847168731,11.2657624244109,123.139363117153)) ;
#19155 = CARTESIAN_POINT('Ctrl Pts',(-20.8776639039544,11.085773344048,123.07124139589)) ;
#19156 = CARTESIAN_POINT('Ctrl Pts',(-20.6134608095792,11.2756619935022,123.345397790749)) ;
#19157 = CARTESIAN_POINT('Ctrl Pts',(-20.9145104547189,11.0956729131393,123.328785419539)) ;
#19158 = CARTESIAN_POINT('Ctrl Pts',(-20.6065401284065,11.2857099055862,123.556501597487)) ;
#19159 = CARTESIAN_POINT('Ctrl Pts',(-20.9058609614056,11.1057208252233,123.592665004876)) ;
#19160 = CARTESIAN_POINT('Ctrl Pts',(-20.5638788823548,11.2956052598934,123.760144762529)) ;
#19161 = CARTESIAN_POINT('Ctrl Pts',(-20.8525354819136,11.1156161795305,123.847220118537)) ;
#19162 = CARTESIAN_POINT('Ctrl Pts',(-20.4852553344784,11.3056669103846,123.956492429052)) ;
#19163 = CARTESIAN_POINT('Ctrl Pts',(-20.7542573598821,11.1256778300217,124.092654877015)) ;
#19164 = CARTESIAN_POINT('Ctrl Pts',(-20.3761505871013,11.315511525847,124.132371029593)) ;
#19165 = CARTESIAN_POINT('Ctrl Pts',(-20.6178768119318,11.1355224454842,124.31250491989)) ;
#19166 = CARTESIAN_POINT('Ctrl Pts',(-20.237114111558,11.3254716047484,124.288935623539)) ;
#19167 = CARTESIAN_POINT('Ctrl Pts',(-20.4440816600714,11.1454825243856,124.508211665868)) ;
#19168 = CARTESIAN_POINT('Ctrl Pts',(-20.0714663398208,11.3355097991068,124.419675506507)) ;
#19169 = CARTESIAN_POINT('Ctrl Pts',(-20.2370227832588,11.1555207187439,124.671637321506)) ;
#19170 = CARTESIAN_POINT('Ctrl Pts',(-19.8888323535182,11.3453835145064,124.518385640457)) ;
#19171 = CARTESIAN_POINT('Ctrl Pts',(-20.0087297938616,11.1653944341435,124.795026404838)) ;
#19172 = CARTESIAN_POINT('Ctrl Pts',(-19.6879284940433,11.3554552240407,124.585159910392)) ;
#19173 = CARTESIAN_POINT('Ctrl Pts',(-19.7576006730884,11.1754661436778,124.87849507525)) ;
#19174 = CARTESIAN_POINT('Ctrl Pts',(-19.4834310386215,11.3652876644932,124.615427060217)) ;
#19175 = CARTESIAN_POINT('Ctrl Pts',(-19.5019775459593,11.1852985841303,124.916330182897)) ;
#19176 = CARTESIAN_POINT('Ctrl Pts',(-19.2726002542326,11.3753194854186,124.610200309681)) ;
#19177 = CARTESIAN_POINT('Ctrl Pts',(-19.2384391664689,11.1953304050557,124.909797495667)) ;
#19178 = CARTESIAN_POINT('Ctrl Pts',(-19.0662276962164,11.3853398553042,124.567903119432)) ;
#19179 = CARTESIAN_POINT('Ctrl Pts',(-18.9804733109709,11.2053507749413,124.856926970494)) ;
#19180 = CARTESIAN_POINT('Ctrl Pts',(-18.8731273416045,11.3952066264379,124.492104200881)) ;
#19181 = CARTESIAN_POINT('Ctrl Pts',(-18.7390964607104,11.215217546075,124.762178595596)) ;
#19182 = CARTESIAN_POINT('Ctrl Pts',(-18.6924952829997,11.4052773976273,124.381703676241)) ;
#19183 = CARTESIAN_POINT('Ctrl Pts',(-18.5133063352698,11.2252883172644,124.624178813688)) ;
#19184 = CARTESIAN_POINT('Ctrl Pts',(-18.5373237843845,11.4151205581489,124.244779697978)) ;
#19185 = CARTESIAN_POINT('Ctrl Pts',(-18.3193404016488,11.235131477786,124.453023478491)) ;
#19186 = CARTESIAN_POINT('Ctrl Pts',(-18.4059602071296,11.4251007913353,124.081184277243)) ;
#19187 = CARTESIAN_POINT('Ctrl Pts',(-18.1551353492722,11.2451117109724,124.248529269541)) ;
#19188 = CARTESIAN_POINT('Ctrl Pts',(-18.3049653385912,11.4351193113705,123.896363057127)) ;
#19189 = CARTESIAN_POINT('Ctrl Pts',(-18.028891195577,11.2551302310076,124.017503067163)) ;
#19190 = CARTESIAN_POINT('Ctrl Pts',(-18.2380760069019,11.4450026197542,123.69961958379)) ;
#19191 = CARTESIAN_POINT('Ctrl Pts',(-17.94527872475,11.2650135393913,123.771572840937)) ;
#19192 = CARTESIAN_POINT('Ctrl Pts',(-18.2058712454328,11.455070903925,123.490451765677)) ;
#19193 = CARTESIAN_POINT('Ctrl Pts',(-17.9050223248742,11.2750818235621,123.510113552435)) ;
#19194 = CARTESIAN_POINT('Ctrl Pts',(-18.2101233464429,11.4649010305926,123.283800583045)) ;
#19195 = CARTESIAN_POINT('Ctrl Pts',(-17.9103370638304,11.2849119502298,123.251798025967)) ;
#19196 = CARTESIAN_POINT('Ctrl Pts',(-18.250874219467,11.4749676027992,123.076164349147)) ;
#19197 = CARTESIAN_POINT('Ctrl Pts',(-17.9612752714376,11.2949785224363,122.992253063296)) ;
#19198 = CARTESIAN_POINT('Ctrl Pts',(-18.3258631651741,11.4848577590399,122.882207935105)) ;
#19199 = CARTESIAN_POINT('Ctrl Pts',(-18.0550114914209,11.304868678677,122.749806436418)) ;
#19200 = CARTESIAN_POINT('Ctrl Pts',(-18.4340938733603,11.4948502866163,122.702175775169)) ;
#19201 = CARTESIAN_POINT('Ctrl Pts',(-18.1902998279982,11.3148612062534,122.524765958901)) ;
#19202 = CARTESIAN_POINT('Ctrl Pts',(-18.5716561470465,11.5048117764906,122.544271291541)) ;
#19203 = CARTESIAN_POINT('Ctrl Pts',(-18.362252777776,11.3248226961277,122.327384835979)) ;
#19204 = CARTESIAN_POINT('Ctrl Pts',(-18.733397668661,11.5147209983778,122.412963329841)) ;
#19205 = CARTESIAN_POINT('Ctrl Pts',(-18.5644303505552,11.3347319180149,122.163249256382)) ;
#19206 = CARTESIAN_POINT('Ctrl Pts',(-18.9180612846803,11.5247695781881,122.310386430444)) ;
#19207 = CARTESIAN_POINT('Ctrl Pts',(-18.7952595963488,11.3447804978252,122.035028175252)) ;
#19208 = CARTESIAN_POINT('Ctrl Pts',(-19.1144372305553,11.5346525526582,122.242490101265)) ;
#19209 = CARTESIAN_POINT('Ctrl Pts',(-19.0407305551564,11.3546634722953,121.950157334317)) ;
#19210 = CARTESIAN_POINT('Ctrl Pts',(-19.3218535876862,11.5446474638009,122.208905343626)) ;
#19211 = CARTESIAN_POINT('Ctrl Pts',(-19.3000011957523,11.364658383438,121.908176471057)) ;
#19212 = CARTESIAN_POINT('Ctrl Pts',(-19.5325030834212,11.5546678503745,122.212142964224)) ;
#19213 = CARTESIAN_POINT('Ctrl Pts',(-19.5633130308643,11.3746787700116,121.912223489131)) ;
#19214 = CARTESIAN_POINT('Ctrl Pts',(-19.7371085501306,11.5645779542315,122.251347857035)) ;
#19215 = CARTESIAN_POINT('Ctrl Pts',(-19.8190707586081,11.3845888738687,121.961229817149)) ;
#19216 = CARTESIAN_POINT('Ctrl Pts',(-19.9323591296137,11.5745056664414,122.325110819767)) ;
#19217 = CARTESIAN_POINT('Ctrl Pts',(-20.0631345837218,11.3945165860786,122.053434027889)) ;
#19218 = CARTESIAN_POINT('Ctrl Pts',(-20.1138182396832,11.5845487762087,122.433038429192)) ;
#19219 = CARTESIAN_POINT('Ctrl Pts',(-20.2899581915959,11.4045596958458,122.18834359306)) ;
#19220 = CARTESIAN_POINT('Ctrl Pts',(-20.2713872169236,11.5944351966642,122.568595596171)) ;
#19221 = CARTESIAN_POINT('Ctrl Pts',(-20.4869200798739,11.4144461163014,122.357790944953)) ;
#19222 = CARTESIAN_POINT('Ctrl Pts',(-20.4047088338096,11.6044283742699,122.730945445389)) ;
#19223 = CARTESIAN_POINT('Ctrl Pts',(-20.653571934063,11.424439293907,122.560728657171)) ;
#19224 = CARTESIAN_POINT('Ctrl Pts',(-20.5072617933259,11.6143740371738,122.913157719128)) ;
#19225 = CARTESIAN_POINT('Ctrl Pts',(-20.7817631202176,11.4343849568109,122.788494689918)) ;
#19226 = CARTESIAN_POINT('Ctrl Pts',(-20.5770363442089,11.624321333379,123.110307996559)) ;
#19227 = CARTESIAN_POINT('Ctrl Pts',(-20.8689810112581,11.4443322530161,123.034933251578)) ;
#19228 = CARTESIAN_POINT('Ctrl Pts',(-20.6116338746559,11.6343690989569,123.318685651132)) ;
#19229 = CARTESIAN_POINT('Ctrl Pts',(-20.9122274632139,11.454380018594,123.295405142899)) ;
#19230 = CARTESIAN_POINT('Ctrl Pts',(-20.6097306714455,11.6442173121745,123.525714223304)) ;
#19231 = CARTESIAN_POINT('Ctrl Pts',(-20.909847955661,11.4642282318116,123.554192250672)) ;
#19232 = CARTESIAN_POINT('Ctrl Pts',(-20.5721619278645,11.6541768849686,123.731697031123)) ;
#19233 = CARTESIAN_POINT('Ctrl Pts',(-20.8628861917845,11.4741878046057,123.811671085768)) ;
#19234 = CARTESIAN_POINT('Ctrl Pts',(-20.4984904473743,11.6642135060011,123.92941246265)) ;
#19235 = CARTESIAN_POINT('Ctrl Pts',(-20.7707963194684,11.4842244256382,124.058815012756)) ;
#19236 = CARTESIAN_POINT('Ctrl Pts',(-20.3935356094815,11.6740940208114,124.108691624986)) ;
#19237 = CARTESIAN_POINT('Ctrl Pts',(-20.6396015638057,11.4941049404486,124.282914554949)) ;
#19238 = CARTESIAN_POINT('Ctrl Pts',(-20.2567978653035,11.6841466721185,124.269794367337)) ;
#19239 = CARTESIAN_POINT('Ctrl Pts',(-20.4686789714687,11.5041575917556,124.484292270277)) ;
#19240 = CARTESIAN_POINT('Ctrl Pts',(-20.0967123068534,11.6940420703985,124.40270437159)) ;
#19241 = CARTESIAN_POINT('Ctrl Pts',(-20.2685707709031,11.5140529900356,124.650429772369)) ;
#19242 = CARTESIAN_POINT('Ctrl Pts',(-19.9132571297185,11.7040921921046,124.507462775467)) ;
#19243 = CARTESIAN_POINT('Ctrl Pts',(-20.0392516106828,11.5241031117417,124.781376915193)) ;
#19244 = CARTESIAN_POINT('Ctrl Pts',(-19.7176472157066,11.7139764716465,124.577647205215)) ;
#19245 = CARTESIAN_POINT('Ctrl Pts',(-19.794737934636,11.5339873912836,124.869107009898)) ;
#19246 = CARTESIAN_POINT('Ctrl Pts',(-19.5106395256385,11.7239712529384,124.613575520575)) ;
#19247 = CARTESIAN_POINT('Ctrl Pts',(-19.5359779545354,11.5439821725755,124.914016452958)) ;
#19248 = CARTESIAN_POINT('Ctrl Pts',(-19.3014914963835,11.7339190981252,124.612936959039)) ;
#19249 = CARTESIAN_POINT('Ctrl Pts',(-19.2745423776044,11.5539300177623,124.913217278818)) ;
#19250 = CARTESIAN_POINT('Ctrl Pts',(-19.0958351736706,11.7438560615126,124.576338079464)) ;
#19251 = CARTESIAN_POINT('Ctrl Pts',(-19.0174715357979,11.5638669811497,124.867467500935)) ;
#19252 = CARTESIAN_POINT('Ctrl Pts',(-18.8986161272856,11.7538390262498,124.504485391709)) ;
#19253 = CARTESIAN_POINT('Ctrl Pts',(-18.7709478903475,11.5738499458869,124.77765044511)) ;
#19254 = CARTESIAN_POINT('Ctrl Pts',(-18.7159988224537,11.7638828776654,124.398530286436)) ;
#19255 = CARTESIAN_POINT('Ctrl Pts',(-18.5426769439724,11.5838937973026,124.645205762056)) ;
#19256 = CARTESIAN_POINT('Ctrl Pts',(-18.5576631664198,11.7737110790002,124.265735860728)) ;
#19257 = CARTESIAN_POINT('Ctrl Pts',(-18.3447570490132,11.5937219986373,124.479210868658)) ;
#19258 = CARTESIAN_POINT('Ctrl Pts',(-18.4214033173466,11.7837876515982,124.103588886124)) ;
#19259 = CARTESIAN_POINT('Ctrl Pts',(-18.1744334770806,11.6037985712354,124.27652667465)) ;
#19260 = CARTESIAN_POINT('Ctrl Pts',(-18.3175955543511,11.7936397316058,123.92430715972)) ;
#19261 = CARTESIAN_POINT('Ctrl Pts',(-18.0446742700679,11.6136506512429,124.052422800966)) ;
#19262 = CARTESIAN_POINT('Ctrl Pts',(-18.2447567569921,11.8037130166099,123.725492716322)) ;
#19263 = CARTESIAN_POINT('Ctrl Pts',(-17.9536271837052,11.623723936247,123.80390465869)) ;
#19264 = CARTESIAN_POINT('Ctrl Pts',(-18.2084461708989,11.8135543683204,123.521791919159)) ;
#19265 = CARTESIAN_POINT('Ctrl Pts',(-17.9082400349615,11.6335652879575,123.549277141686)) ;
#19266 = CARTESIAN_POINT('Ctrl Pts',(-18.2072783331998,11.8235158677169,123.312385813251)) ;
#19267 = CARTESIAN_POINT('Ctrl Pts',(-17.9067818389188,11.643526787354,123.287519099378)) ;
#19268 = CARTESIAN_POINT('Ctrl Pts',(-18.2431187666664,11.8335516438469,123.104460989179)) ;
#19269 = CARTESIAN_POINT('Ctrl Pts',(-17.951583816689,11.653562563484,123.027613430416)) ;
#19270 = CARTESIAN_POINT('Ctrl Pts',(-18.313260700151,11.8434400704844,122.908768536338)) ;
#19271 = CARTESIAN_POINT('Ctrl Pts',(-18.0392630064654,11.6634509901216,122.782997517006)) ;
#19272 = CARTESIAN_POINT('Ctrl Pts',(-18.4172968730816,11.8534553925594,122.725703223709)) ;
#19273 = CARTESIAN_POINT('Ctrl Pts',(-18.169309686562,11.6734663121965,122.55416670281)) ;
#19274 = CARTESIAN_POINT('Ctrl Pts',(-18.5521138610027,11.8634857414596,122.563558399555)) ;
#19275 = CARTESIAN_POINT('Ctrl Pts',(-18.337832034103,11.6834966610967,122.351486710983)) ;
#19276 = CARTESIAN_POINT('Ctrl Pts',(-18.7097629865951,11.8733291170662,122.429511598476)) ;
#19277 = CARTESIAN_POINT('Ctrl Pts',(-18.5348954406339,11.6933400367034,122.18392868398)) ;
#19278 = CARTESIAN_POINT('Ctrl Pts',(-18.8914357075047,11.8833585539634,122.322486366911)) ;
#19279 = CARTESIAN_POINT('Ctrl Pts',(-18.7619871989816,11.7033694736005,122.05014873987)) ;
#19280 = CARTESIAN_POINT('Ctrl Pts',(-19.0891853403317,11.8933904318963,122.249153011441)) ;
#19281 = CARTESIAN_POINT('Ctrl Pts',(-19.0091747229,11.7134013515334,121.958483598159)) ;
#19282 = CARTESIAN_POINT('Ctrl Pts',(-19.2923854095674,11.9032200550018,122.211622723258)) ;
#19283 = CARTESIAN_POINT('Ctrl Pts',(-19.2631763810942,11.7232309746389,121.91157223852)) ;
#19284 = CARTESIAN_POINT('Ctrl Pts',(-19.5023882087078,11.9132095261549,122.209287327401)) ;
#19285 = CARTESIAN_POINT('Ctrl Pts',(-19.5256800788775,11.733220445792,121.908654949481)) ;
#19286 = CARTESIAN_POINT('Ctrl Pts',(-19.7106392401679,11.9232533749173,122.244164803758)) ;
#19287 = CARTESIAN_POINT('Ctrl Pts',(-19.7859934259949,11.7432642945544,121.95225353693)) ;
#19288 = CARTESIAN_POINT('Ctrl Pts',(-19.9054125620073,11.933075080449,122.312709524051)) ;
#19289 = CARTESIAN_POINT('Ctrl Pts',(-20.0294606191008,11.7530860000861,122.037936667196)) ;
#19290 = CARTESIAN_POINT('Ctrl Pts',(-20.0894867289459,11.9431101202768,122.415781902165)) ;
#19291 = CARTESIAN_POINT('Ctrl Pts',(-20.2595522204667,11.7631210399139,122.166778899388)) ;
#19292 = CARTESIAN_POINT('Ctrl Pts',(-20.2523369083129,11.9531348271682,122.54956886486)) ;
#19293 = CARTESIAN_POINT('Ctrl Pts',(-20.4631137171743,11.7731457468054,122.334014058184)) ;
#19294 = CARTESIAN_POINT('Ctrl Pts',(-20.3874578810136,11.962987531509,122.706561960871)) ;
#19295 = CARTESIAN_POINT('Ctrl Pts',(-20.6320140503155,11.7829984511461,122.530257519376)) ;
#19296 = CARTESIAN_POINT('Ctrl Pts',(-20.4950292100305,11.9729756537167,122.88687951836)) ;
#19297 = CARTESIAN_POINT('Ctrl Pts',(-20.7664764699797,11.7929865733538,122.755655719711)) ;
#19298 = CARTESIAN_POINT('Ctrl Pts',(-20.5692290588118,11.982904123824,123.081978843733)) ;
#19299 = CARTESIAN_POINT('Ctrl Pts',(-20.8592244692304,11.8029150434611,122.999531121806)) ;
#19300 = CARTESIAN_POINT('Ctrl Pts',(-20.6090083992339,11.9928931009912,123.28818688241)) ;
#19301 = CARTESIAN_POINT('Ctrl Pts',(-20.9089464870837,11.8129040206283,123.257291767332)) ;
#19302 = CARTESIAN_POINT('Ctrl Pts',(-20.6120343021104,12.0029309082709,123.499185950342)) ;
#19303 = CARTESIAN_POINT('Ctrl Pts',(-20.912726728438,11.822941827908,123.521040547069)) ;
#19304 = CARTESIAN_POINT('Ctrl Pts',(-20.5793530027892,12.0127772091342,123.703591668076)) ;
#19305 = CARTESIAN_POINT('Ctrl Pts',(-20.8718727620384,11.8327881287713,123.776548267499)) ;
#19306 = CARTESIAN_POINT('Ctrl Pts',(-20.5108877173329,12.0228029525135,123.902937612404)) ;
#19307 = CARTESIAN_POINT('Ctrl Pts',(-20.7862889531826,11.8428138721506,124.025729898005)) ;
#19308 = CARTESIAN_POINT('Ctrl Pts',(-20.4083149981522,12.0328338189525,124.087198060114)) ;
#19309 = CARTESIAN_POINT('Ctrl Pts',(-20.6580711492051,11.8528447385896,124.256054351195)) ;
#19310 = CARTESIAN_POINT('Ctrl Pts',(-20.278204027201,12.0426711777513,124.247942559337)) ;
#19311 = CARTESIAN_POINT('Ctrl Pts',(-20.4954300469777,11.8626820973884,124.456984258248)) ;
#19312 = CARTESIAN_POINT('Ctrl Pts',(-20.1200700787013,12.052663138685,124.386216766339)) ;
#19313 = CARTESIAN_POINT('Ctrl Pts',(-20.2977609080492,11.8726740583222,124.62982526479)) ;
#19314 = CARTESIAN_POINT('Ctrl Pts',(-19.9393758024445,12.0626955012416,124.495014747097)) ;
#19315 = CARTESIAN_POINT('Ctrl Pts',(-20.0718918884167,11.8827064208787,124.765820716401)) ;
#19316 = CARTESIAN_POINT('Ctrl Pts',(-19.7459234684514,12.072560661816,124.569749829319)) ;
#19317 = CARTESIAN_POINT('Ctrl Pts',(-19.830074922632,11.8925715814531,124.859237594725)) ;
#19318 = CARTESIAN_POINT('Ctrl Pts',(-19.5405372405183,12.0825225663937,124.610739722099)) ;
#19319 = CARTESIAN_POINT('Ctrl Pts',(-19.5733413955139,11.9025334860308,124.910472534242)) ;
#19320 = CARTESIAN_POINT('Ctrl Pts',(-19.3296285023073,12.0925574964694,124.615133939641)) ;
#19321 = CARTESIAN_POINT('Ctrl Pts',(-19.3097054567228,11.9125684161065,124.915962853087)) ;
#19322 = CARTESIAN_POINT('Ctrl Pts',(-19.12418262518,12.102442443323,124.58366381539)) ;
#19323 = CARTESIAN_POINT('Ctrl Pts',(-19.0528979312036,11.9224533629601,124.876622619197)) ;
#19324 = CARTESIAN_POINT('Ctrl Pts',(-18.9237994034088,12.1125081196345,124.515756077525)) ;
#19325 = CARTESIAN_POINT('Ctrl Pts',(-18.8024198540435,11.9325190392716,124.791735612442)) ;
#19326 = CARTESIAN_POINT('Ctrl Pts',(-18.7422682640068,12.1223470392694,124.416531181598)) ;
#19327 = CARTESIAN_POINT('Ctrl Pts',(-18.5755065294971,11.9423579589065,124.667701912514)) ;
#19328 = CARTESIAN_POINT('Ctrl Pts',(-18.5769155643104,12.1324105490038,124.284598448374)) ;
#19329 = CARTESIAN_POINT('Ctrl Pts',(-18.3688173844643,11.9524214686409,124.502784044984)) ;
#19330 = CARTESIAN_POINT('Ctrl Pts',(-18.4394382528722,12.1423041621656,124.128483209612)) ;
#19331 = CARTESIAN_POINT('Ctrl Pts',(-18.1969723593472,11.9623150818027,124.307637940785)) ;
#19332 = CARTESIAN_POINT('Ctrl Pts',(-18.330159277488,12.152248168979,123.950297968068)) ;
#19333 = CARTESIAN_POINT('Ctrl Pts',(-18.0603757685369,11.9722590886161,124.08490476088)) ;
#19334 = CARTESIAN_POINT('Ctrl Pts',(-18.2529261348415,12.1622491233333,123.754711085262)) ;
#19335 = CARTESIAN_POINT('Ctrl Pts',(-17.9638367967476,11.9822600429704,123.840420099808)) ;
#19336 = CARTESIAN_POINT('Ctrl Pts',(-18.2110463667562,12.1722878810256,123.547880865785)) ;
#19337 = CARTESIAN_POINT('Ctrl Pts',(-17.9114896578375,11.9922988006627,123.58188181945)) ;
#19338 = CARTESIAN_POINT('Ctrl Pts',(-18.2053758043967,12.1821120651956,123.341406321408)) ;
#19339 = CARTESIAN_POINT('Ctrl Pts',(-17.9044041219212,12.0021229848327,123.323787975382)) ;
#19340 = CARTESIAN_POINT('Ctrl Pts',(-18.2360503167514,12.192170130795,123.132209463155)) ;
#19341 = CARTESIAN_POINT('Ctrl Pts',(-17.9427499485555,12.0121810504321,123.062292370625)) ;
#19342 = CARTESIAN_POINT('Ctrl Pts',(-18.302006424845,12.2021001775697,122.934128152636)) ;
#19343 = CARTESIAN_POINT('Ctrl Pts',(-18.0251977237691,12.0221110972068,122.814691316201)) ;
#19344 = CARTESIAN_POINT('Ctrl Pts',(-18.4010777311963,12.2120516199068,122.749859407281)) ;
#19345 = CARTESIAN_POINT('Ctrl Pts',(-18.1490393731302,12.0320625395439,122.584356522223)) ;
#19346 = CARTESIAN_POINT('Ctrl Pts',(-18.5321045118858,12.2220984170861,122.584200624693)) ;
#19347 = CARTESIAN_POINT('Ctrl Pts',(-18.3128249788135,12.0421093367232,122.377284739554)) ;
#19348 = CARTESIAN_POINT('Ctrl Pts',(-18.6866546754837,12.2319463577662,122.446441479111)) ;
#19349 = CARTESIAN_POINT('Ctrl Pts',(-18.5060148098008,12.0519572774033,122.205087588693)) ;
#19350 = CARTESIAN_POINT('Ctrl Pts',(-18.8644598958187,12.2419079891088,122.335805361285)) ;
#19351 = CARTESIAN_POINT('Ctrl Pts',(-18.7282729224672,12.0619189087459,122.066794754727)) ;
#19352 = CARTESIAN_POINT('Ctrl Pts',(-19.0602009714326,12.2519366484847,122.257435573529)) ;
#19353 = CARTESIAN_POINT('Ctrl Pts',(-18.9729503385559,12.0719475681218,121.968835081685)) ;
#19354 = CARTESIAN_POINT('Ctrl Pts',(-19.2641055065429,12.2618469513729,122.214691358915)) ;
#19355 = CARTESIAN_POINT('Ctrl Pts',(-19.227831787757,12.08185787101,121.915407496624)) ;
#19356 = CARTESIAN_POINT('Ctrl Pts',(-19.472848854405,12.2717818459351,122.20743693277)) ;
#19357 = CARTESIAN_POINT('Ctrl Pts',(-19.4887612039821,12.0917927655722,121.906342273827)) ;
#19358 = CARTESIAN_POINT('Ctrl Pts',(-19.6818517454895,12.281822944602,122.237040740592)) ;
#19359 = CARTESIAN_POINT('Ctrl Pts',(-19.7500144690061,12.1018338642391,121.943349818059)) ;
#19360 = CARTESIAN_POINT('Ctrl Pts',(-19.8795274393584,12.2917102271064,122.301350610276)) ;
#19361 = CARTESIAN_POINT('Ctrl Pts',(-19.9971083719985,12.1117211467435,122.023739879768)) ;
#19362 = CARTESIAN_POINT('Ctrl Pts',(-20.0651177529335,12.3017019676169,122.399712129327)) ;
#19363 = CARTESIAN_POINT('Ctrl Pts',(-20.2290950029525,12.121712887254,122.146694306298)) ;
#19364 = CARTESIAN_POINT('Ctrl Pts',(-20.2301016245503,12.3116525168523,122.52834286884)) ;
#19365 = CARTESIAN_POINT('Ctrl Pts',(-20.4353231818005,12.1316634364894,122.307485013012)) ;
#19366 = CARTESIAN_POINT('Ctrl Pts',(-20.3702511436106,12.3215881944871,122.68320837822)) ;
#19367 = CARTESIAN_POINT('Ctrl Pts',(-20.6105080303125,12.1415991141242,122.501068844292)) ;
#19368 = CARTESIAN_POINT('Ctrl Pts',(-20.4821440049613,12.3315736122799,122.86084640938)) ;
#19369 = CARTESIAN_POINT('Ctrl Pts',(-20.750371753253,12.151584531917,122.723117938316)) ;
#19370 = CARTESIAN_POINT('Ctrl Pts',(-20.561588894867,12.3416024051504,123.056141240279)) ;
#19371 = CARTESIAN_POINT('Ctrl Pts',(-20.8496752814087,12.1616133247875,122.967237619846)) ;
#19372 = CARTESIAN_POINT('Ctrl Pts',(-20.605473389762,12.3514819163783,123.25914772635)) ;
#19373 = CARTESIAN_POINT('Ctrl Pts',(-20.9045281450594,12.1714928360155,123.220996340645)) ;
#19374 = CARTESIAN_POINT('Ctrl Pts',(-20.6140174461044,12.3614754530513,123.469077690765)) ;
#19375 = CARTESIAN_POINT('Ctrl Pts',(-20.9152054113298,12.1814863726884,123.483408955597)) ;
#19376 = CARTESIAN_POINT('Ctrl Pts',(-20.5854395929456,12.3715077213151,123.67803354945)) ;
#19377 = CARTESIAN_POINT('Ctrl Pts',(-20.8794802827671,12.1915186409522,123.744603500789)) ;
#19378 = CARTESIAN_POINT('Ctrl Pts',(-20.5225086633852,12.381371683321,123.875648773567)) ;
#19379 = CARTESIAN_POINT('Ctrl Pts',(-20.8008139737887,12.2013826029581,123.991621606298)) ;
#19380 = CARTESIAN_POINT('Ctrl Pts',(-20.4242612791623,12.3914417446659,124.063150375643)) ;
#19381 = CARTESIAN_POINT('Ctrl Pts',(-20.678002189668,12.211452664303,124.225997440401)) ;
#19382 = CARTESIAN_POINT('Ctrl Pts',(-20.2978479151584,12.4012841090146,124.22697472228)) ;
#19383 = CARTESIAN_POINT('Ctrl Pts',(-20.5199833626838,12.2212950286517,124.430776031763)) ;
#19384 = CARTESIAN_POINT('Ctrl Pts',(-20.1436024751154,12.4112447815171,124.368597953825)) ;
#19385 = CARTESIAN_POINT('Ctrl Pts',(-20.327174746647,12.2312557011542,124.607803018266)) ;
#19386 = CARTESIAN_POINT('Ctrl Pts',(-19.9655160234336,12.4212828525849,124.481805478694)) ;
#19387 = CARTESIAN_POINT('Ctrl Pts',(-20.1045650508631,12.241293772222,124.749310160051)) ;
#19388 = CARTESIAN_POINT('Ctrl Pts',(-19.7737887271615,12.4311564675453,124.561434581507)) ;
#19389 = CARTESIAN_POINT('Ctrl Pts',(-19.8649051459857,12.2511673871824,124.84884392232)) ;
#19390 = CARTESIAN_POINT('Ctrl Pts',(-19.5671291833791,12.4412287021266,124.607402354197)) ;
#19391 = CARTESIAN_POINT('Ctrl Pts',(-19.6065797304044,12.2612396217637,124.906300997495)) ;
#19392 = CARTESIAN_POINT('Ctrl Pts',(-19.3607684693909,12.4510527205754,124.616796315158)) ;
#19393 = CARTESIAN_POINT('Ctrl Pts',(-19.3486297183306,12.2710636402125,124.918040759663)) ;
#19394 = CARTESIAN_POINT('Ctrl Pts',(-19.1509428265166,12.4611176415514,124.589849021404)) ;
#19395 = CARTESIAN_POINT('Ctrl Pts',(-19.0863456687476,12.2811285611885,124.884353810211)) ;
#19396 = CARTESIAN_POINT('Ctrl Pts',(-18.8857365452566,12.4743279398461,124.507174456424)) ;
#19397 = CARTESIAN_POINT('Ctrl Pts',(-18.7548496615759,12.2943388594833,124.781008020348)) ;
#19398 = CARTESIAN_POINT('Ctrl Pts',(-18.6462382926402,12.4876433865781,124.356312359537)) ;
#19399 = CARTESIAN_POINT('Ctrl Pts',(-18.4555083325038,12.3076543062152,124.592460114452)) ;
#19400 = CARTESIAN_POINT('Ctrl Pts',(-18.4564387488717,12.5009336318454,124.15121232202)) ;
#19401 = CARTESIAN_POINT('Ctrl Pts',(-18.2182158984291,12.3209445514825,124.336043204847)) ;
#19402 = CARTESIAN_POINT('Ctrl Pts',(-18.3421528810108,12.5109843814525,123.973529884011)) ;
#19403 = CARTESIAN_POINT('Ctrl Pts',(-18.0753697674858,12.3309953010896,124.113946532571)) ;
#19404 = CARTESIAN_POINT('Ctrl Pts',(-18.261991671417,12.5207969884347,123.783417454446)) ;
#19405 = CARTESIAN_POINT('Ctrl Pts',(-17.9751686262583,12.3408079080718,123.876303265546)) ;
#19406 = CARTESIAN_POINT('Ctrl Pts',(-18.2145854633708,12.530868086429,123.5770937702)) ;
#19407 = CARTESIAN_POINT('Ctrl Pts',(-17.9159132713503,12.3508790060661,123.61839959421)) ;
#19408 = CARTESIAN_POINT('Ctrl Pts',(-18.2041287449214,12.5407576592038,123.369434972959)) ;
#19409 = CARTESIAN_POINT('Ctrl Pts',(-17.9028470180164,12.360768578841,123.358821518713)) ;
#19410 = CARTESIAN_POINT('Ctrl Pts',(-18.2378495819674,12.5540277660071,123.092473664091)) ;
#19411 = CARTESIAN_POINT('Ctrl Pts',(-17.9449900324593,12.3740386856443,123.012644489447)) ;
#19412 = CARTESIAN_POINT('Ctrl Pts',(-18.3698646515677,12.5706444529296,122.764802678493)) ;
#19413 = CARTESIAN_POINT('Ctrl Pts',(-18.1100382420715,12.3906553725668,122.603018959482)) ;
#19414 = CARTESIAN_POINT('Ctrl Pts',(-18.6050396672439,12.5872184962459,122.502279793378)) ;
#19415 = CARTESIAN_POINT('Ctrl Pts',(-18.403953809166,12.407229415883,122.274921978595)) ;
#19416 = CARTESIAN_POINT('Ctrl Pts',(-18.8388843969827,12.6005150636777,122.349174786392)) ;
#19417 = CARTESIAN_POINT('Ctrl Pts',(-18.6963080999561,12.4205259833148,122.083501484983)) ;
#19418 = CARTESIAN_POINT('Ctrl Pts',(-19.032708382408,12.6105451272551,122.266104245232)) ;
#19419 = CARTESIAN_POINT('Ctrl Pts',(-18.9385791929077,12.4305560468922,121.979673523522)) ;
#19420 = CARTESIAN_POINT('Ctrl Pts',(-19.2351868358827,12.6204390191043,122.218590201878)) ;
#19421 = CARTESIAN_POINT('Ctrl Pts',(-19.1916818709481,12.4404499387414,121.920281628208)) ;
#19422 = CARTESIAN_POINT('Ctrl Pts',(-19.5133724231769,12.6336917748899,122.2020040059)) ;
#19423 = CARTESIAN_POINT('Ctrl Pts',(-19.5394009792638,12.453702694527,121.899549493621)) ;
#19424 = CARTESIAN_POINT('Ctrl Pts',(-19.8616244702295,12.6504198798823,122.274010765671)) ;
#19425 = CARTESIAN_POINT('Ctrl Pts',(-19.9747293753154,12.4704307995194,121.989564308867)) ;
#19426 = CARTESIAN_POINT('Ctrl Pts',(-20.2206924205023,12.6702507163608,122.495213042442)) ;
#19427 = CARTESIAN_POINT('Ctrl Pts',(-20.423556659189,12.4902616359979,122.266069036656)) ;
#19428 = CARTESIAN_POINT('Ctrl Pts',(-20.4846749217705,12.690176108251,122.826464817505)) ;
#19429 = CARTESIAN_POINT('Ctrl Pts',(-20.7535327226879,12.5101870278881,122.680135635484)) ;
#19430 = CARTESIAN_POINT('Ctrl Pts',(-20.6197750422256,12.710101321603,123.228081726851)) ;
#19431 = CARTESIAN_POINT('Ctrl Pts',(-20.9224041261077,12.5301122412401,123.18215712058)) ;
#19432 = CARTESIAN_POINT('Ctrl Pts',(-20.6098235900098,12.7300263350881,123.651575664266)) ;
#19433 = CARTESIAN_POINT('Ctrl Pts',(-20.9099617273115,12.5500372547252,123.711523704258)) ;
#19434 = CARTESIAN_POINT('Ctrl Pts',(-20.4568446708067,12.7499028067881,124.045572962216)) ;
#19435 = CARTESIAN_POINT('Ctrl Pts',(-20.7187360422604,12.5699137264252,124.204018044716)) ;
#19436 = CARTESIAN_POINT('Ctrl Pts',(-20.1773211945259,12.7698821246969,124.36546202135)) ;
#19437 = CARTESIAN_POINT('Ctrl Pts',(-20.3693300643289,12.5898930443341,124.603877601687)) ;
#19438 = CARTESIAN_POINT('Ctrl Pts',(-19.8060899945786,12.7898151282729,124.57002813045)) ;
#19439 = CARTESIAN_POINT('Ctrl Pts',(-19.9052905888142,12.6098260479101,124.859582769263)) ;
#19440 = CARTESIAN_POINT('Ctrl Pts',(-19.3882558614324,12.8097103983006,124.635945221289)) ;
#19441 = CARTESIAN_POINT('Ctrl Pts',(-19.3829989743676,12.6297213179378,124.941977004567)) ;
#19442 = CARTESIAN_POINT('Ctrl Pts',(-18.9723404365734,12.8296317362065,124.55563458962)) ;
#19443 = CARTESIAN_POINT('Ctrl Pts',(-18.8631060156455,12.6496426558436,124.841587523865)) ;
#19444 = CARTESIAN_POINT('Ctrl Pts',(-18.6081781423476,12.8495893594727,124.337737107174)) ;
#19445 = CARTESIAN_POINT('Ctrl Pts',(-18.4079042835162,12.6696002791098,124.569214868981)) ;
#19446 = CARTESIAN_POINT('Ctrl Pts',(-18.3412557610278,12.8694691914299,124.010060659351)) ;
#19447 = CARTESIAN_POINT('Ctrl Pts',(-18.0742532724176,12.689480111067,124.15962015315)) ;
#19448 = CARTESIAN_POINT('Ctrl Pts',(-18.2010112247405,12.8893510427268,123.611173077498)) ;
#19449 = CARTESIAN_POINT('Ctrl Pts',(-17.8989480657597,12.7093619623639,123.661012507451)) ;
#19450 = CARTESIAN_POINT('Ctrl Pts',(-18.2061520734863,12.9094220598306,123.184494838161)) ;
#19451 = CARTESIAN_POINT('Ctrl Pts',(-17.9053743363839,12.7294329794677,123.127663535506)) ;
#19452 = CARTESIAN_POINT('Ctrl Pts',(-18.3545914950356,12.9292292835837,122.790282514626)) ;
#19453 = CARTESIAN_POINT('Ctrl Pts',(-18.0909224032866,12.7492402032208,122.634900991628)) ;
#19454 = CARTESIAN_POINT('Ctrl Pts',(-18.6302173582225,12.9492104191524,122.467021464749)) ;
#19455 = CARTESIAN_POINT('Ctrl Pts',(-18.4354537167374,12.7692213387896,122.230824135122)) ;
#19456 = CARTESIAN_POINT('Ctrl Pts',(-18.9990267978771,12.9691379124917,122.258503177642)) ;
#19457 = CARTESIAN_POINT('Ctrl Pts',(-18.8964641846084,12.7891488321288,121.970176160961)) ;
#19458 = CARTESIAN_POINT('Ctrl Pts',(-19.414525111865,12.9889585738495,122.187284802443)) ;
#19459 = CARTESIAN_POINT('Ctrl Pts',(-19.415834432645,12.8089694934866,121.881151656097)) ;
#19460 = CARTESIAN_POINT('Ctrl Pts',(-19.8347816721657,13.0090557630713,122.26378936849)) ;
#19461 = CARTESIAN_POINT('Ctrl Pts',(-19.9411566590933,12.8290666827084,121.976780870031)) ;
#19462 = CARTESIAN_POINT('Ctrl Pts',(-20.1980367737812,13.0288194420796,122.475474924502)) ;
#19463 = CARTESIAN_POINT('Ctrl Pts',(-20.3952240684518,12.8488303617167,122.241384544964)) ;
#19464 = CARTESIAN_POINT('Ctrl Pts',(-20.47137453339,13.0488767207527,122.802591270838)) ;
#19465 = CARTESIAN_POINT('Ctrl Pts',(-20.7368987004041,12.8688876403898,122.650278783027)) ;
#19466 = CARTESIAN_POINT('Ctrl Pts',(-20.6146542104524,13.0686721445001,123.198479778478)) ;
#19467 = CARTESIAN_POINT('Ctrl Pts',(-20.915999998585,12.8886830641372,123.145136393717)) ;
#19468 = CARTESIAN_POINT('Ctrl Pts',(-20.6155493708649,13.0886357892277,123.622911309277)) ;
#19469 = CARTESIAN_POINT('Ctrl Pts',(-20.9171224626081,12.9086467088648,123.675675466344)) ;
#19470 = CARTESIAN_POINT('Ctrl Pts',(-20.4704208826885,13.1086192805018,124.022266658295)) ;
#19471 = CARTESIAN_POINT('Ctrl Pts',(-20.7357148689362,12.9286302001389,124.174870580485)) ;
#19472 = CARTESIAN_POINT('Ctrl Pts',(-20.2007675400314,13.1284267756511,124.345835412524)) ;
#19473 = CARTESIAN_POINT('Ctrl Pts',(-20.3986521463145,12.9484376952882,124.579332558867)) ;
#19474 = CARTESIAN_POINT('Ctrl Pts',(-19.834022972994,13.1484093663712,124.560193591737)) ;
#19475 = CARTESIAN_POINT('Ctrl Pts',(-19.9402235763069,12.9684202860083,124.847283742868)) ;
#19476 = CARTESIAN_POINT('Ctrl Pts',(-19.4180361300331,13.1682920203624,124.636116448361)) ;
#19477 = CARTESIAN_POINT('Ctrl Pts',(-19.4202416053834,12.9883029399995,124.942191223807)) ;
#19478 = CARTESIAN_POINT('Ctrl Pts',(-18.9996554886756,13.1882502652255,124.565604893307)) ;
#19479 = CARTESIAN_POINT('Ctrl Pts',(-18.8972653738817,13.0082611848626,124.854056149815)) ;
#19480 = CARTESIAN_POINT('Ctrl Pts',(-18.6317218676168,13.2081258522671,124.357573974673)) ;
#19481 = CARTESIAN_POINT('Ctrl Pts',(-18.4373467193133,13.0281367719042,124.594021898923)) ;
#19482 = CARTESIAN_POINT('Ctrl Pts',(-18.3552399068354,13.2281067404023,124.035038294504)) ;
#19483 = CARTESIAN_POINT('Ctrl Pts',(-18.0917408140289,13.0481176600395,124.190855292359)) ;
#19484 = CARTESIAN_POINT('Ctrl Pts',(-18.206044297576,13.2480418815133,123.638227388492)) ;
#19485 = CARTESIAN_POINT('Ctrl Pts',(-17.9052414355018,13.0680528011505,123.694844185524)) ;
#19486 = CARTESIAN_POINT('Ctrl Pts',(-18.2009152531286,13.2679538995244,123.214915566106)) ;
#19487 = CARTESIAN_POINT('Ctrl Pts',(-17.8988271166947,13.0879648191615,123.165702838927)) ;
#19488 = CARTESIAN_POINT('Ctrl Pts',(-18.3399734278226,13.287842117768,122.815536644445)) ;
#19489 = CARTESIAN_POINT('Ctrl Pts',(-18.072637630343,13.1078530374051,122.666485551976)) ;
#19490 = CARTESIAN_POINT('Ctrl Pts',(-18.5625167302271,13.3044404216149,122.541702141202)) ;
#19491 = CARTESIAN_POINT('Ctrl Pts',(-18.3508356377982,13.124451341252,122.324166060085)) ;
#19492 = CARTESIAN_POINT('Ctrl Pts',(-18.7884633242958,13.3177130115177,122.377888779236)) ;
#19493 = CARTESIAN_POINT('Ctrl Pts',(-18.6332461345771,13.1377239311548,122.119417599801)) ;
#19494 = CARTESIAN_POINT('Ctrl Pts',(-18.9775497688346,13.3277204264686,122.285661961006)) ;
#19495 = CARTESIAN_POINT('Ctrl Pts',(-18.8696106143661,13.1477313461057,122.004127651261)) ;
#19496 = CARTESIAN_POINT('Ctrl Pts',(-19.1798541137618,13.3377277732012,122.227841226343)) ;
#19497 = CARTESIAN_POINT('Ctrl Pts',(-19.1224757065835,13.1577386928383,121.931849416177)) ;
#19498 = CARTESIAN_POINT('Ctrl Pts',(-19.4571882805755,13.3509941330028,122.198742528533)) ;
#19499 = CARTESIAN_POINT('Ctrl Pts',(-19.4692111889447,13.1710050526399,121.895476582139)) ;
#19500 = CARTESIAN_POINT('Ctrl Pts',(-19.8041191619441,13.3675087906257,122.253086418136)) ;
#19501 = CARTESIAN_POINT('Ctrl Pts',(-19.9027886653172,13.1875197102629,121.963391453896)) ;
#19502 = CARTESIAN_POINT('Ctrl Pts',(-20.1135332813589,13.3841062238684,122.422657976203)) ;
#19503 = CARTESIAN_POINT('Ctrl Pts',(-20.2896179416635,13.2041171435055,122.175375538865)) ;
#19504 = CARTESIAN_POINT('Ctrl Pts',(-20.3161488488574,13.3974542210134,122.616898131359)) ;
#19505 = CARTESIAN_POINT('Ctrl Pts',(-20.5428541366256,13.2174651406505,122.418153018463)) ;
#19506 = CARTESIAN_POINT('Ctrl Pts',(-20.4392682471211,13.407349975365,122.78458790923)) ;
#19507 = CARTESIAN_POINT('Ctrl Pts',(-20.6967627804406,13.2273608950021,122.62776755716)) ;
#19508 = CARTESIAN_POINT('Ctrl Pts',(-20.5324892710804,13.4173379292963,122.972722988984)) ;
#19509 = CARTESIAN_POINT('Ctrl Pts',(-20.8132896637095,13.2373488489335,122.862934128972)) ;
#19510 = CARTESIAN_POINT('Ctrl Pts',(-20.5915443850433,13.4272951530011,123.173577963998)) ;
#19511 = CARTESIAN_POINT('Ctrl Pts',(-20.887111769064,13.2473060726382,123.114002366625)) ;
#19512 = CARTESIAN_POINT('Ctrl Pts',(-20.6149084211195,13.4373306995577,123.383244466026)) ;
#19513 = CARTESIAN_POINT('Ctrl Pts',(-20.9163194697392,13.2573416191949,123.376085199788)) ;
#19514 = CARTESIAN_POINT('Ctrl Pts',(-20.6018663431854,13.4472178108339,123.590706984687)) ;
#19515 = CARTESIAN_POINT('Ctrl Pts',(-20.9000197111728,13.267228730471,123.635413520908)) ;
#19516 = CARTESIAN_POINT('Ctrl Pts',(-20.5528158490788,13.4572092159347,123.794940084393)) ;
#19517 = CARTESIAN_POINT('Ctrl Pts',(-20.8387093067046,13.2772201355718,123.890705618829)) ;
#19518 = CARTESIAN_POINT('Ctrl Pts',(-20.4693700177335,13.4671548371495,123.986654821614)) ;
#19519 = CARTESIAN_POINT('Ctrl Pts',(-20.7344045824693,13.2871657567866,124.130350209159)) ;
#19520 = CARTESIAN_POINT('Ctrl Pts',(-20.3542090233936,13.4771040854178,124.161276470942)) ;
#19521 = CARTESIAN_POINT('Ctrl Pts',(-20.5904556480587,13.2971150050549,124.348628887742)) ;
#19522 = CARTESIAN_POINT('Ctrl Pts',(-20.2089077397589,13.4871505805864,124.314549867347)) ;
#19523 = CARTESIAN_POINT('Ctrl Pts',(-20.4088310489179,13.3071615002235,124.540222615066)) ;
#19524 = CARTESIAN_POINT('Ctrl Pts',(-20.0426037732206,13.4970019233779,124.438001198331)) ;
#19525 = CARTESIAN_POINT('Ctrl Pts',(-20.2009526790891,13.3170128430151,124.69453910851)) ;
#19526 = CARTESIAN_POINT('Ctrl Pts',(-19.8553954660048,13.5069737035053,124.532292944024)) ;
#19527 = CARTESIAN_POINT('Ctrl Pts',(-19.9669434550335,13.3269846231424,124.812406349802)) ;
#19528 = CARTESIAN_POINT('Ctrl Pts',(-19.6541253092378,13.516968903483,124.592783946963)) ;
#19529 = CARTESIAN_POINT('Ctrl Pts',(-19.7153564891379,13.3369798231201,124.888022808457)) ;
#19530 = CARTESIAN_POINT('Ctrl Pts',(-19.444620176713,13.527002895179,124.617242515377)) ;
#19531 = CARTESIAN_POINT('Ctrl Pts',(-19.4534753611638,13.3470138148161,124.918598821052)) ;
#19532 = CARTESIAN_POINT('Ctrl Pts',(-19.2377415370854,13.5368583001515,124.605497638602)) ;
#19533 = CARTESIAN_POINT('Ctrl Pts',(-19.1948766730221,13.3568692197886,124.903920505576)) ;
#19534 = CARTESIAN_POINT('Ctrl Pts',(-19.0330890851524,13.5468575979973,124.557608984223)) ;
#19535 = CARTESIAN_POINT('Ctrl Pts',(-18.9390603846793,13.3668685176344,124.844062381727)) ;
#19536 = CARTESIAN_POINT('Ctrl Pts',(-18.8417203854023,13.5567527106025,124.475953276878)) ;
#19537 = CARTESIAN_POINT('Ctrl Pts',(-18.6998481883594,13.3767636302396,124.741995186928)) ;
#19538 = CARTESIAN_POINT('Ctrl Pts',(-18.6645864621206,13.5668133561375,124.360423798942)) ;
#19539 = CARTESIAN_POINT('Ctrl Pts',(-18.4784292945889,13.3868242757746,124.597585675323)) ;
#19540 = CARTESIAN_POINT('Ctrl Pts',(-18.5133398637062,13.5766622331267,124.218993175225)) ;
#19541 = CARTESIAN_POINT('Ctrl Pts',(-18.2893688821215,13.3966731527638,124.420799145494)) ;
#19542 = CARTESIAN_POINT('Ctrl Pts',(-18.3862631485546,13.5866909442203,124.050762009217)) ;
#19543 = CARTESIAN_POINT('Ctrl Pts',(-18.1305208053495,13.4067018638574,124.210511784196)) ;
#19544 = CARTESIAN_POINT('Ctrl Pts',(-18.2908283109245,13.5967203454764,123.862742118593)) ;
#19545 = CARTESIAN_POINT('Ctrl Pts',(-18.0112247910287,13.4167312651135,123.975488167396)) ;
#19546 = CARTESIAN_POINT('Ctrl Pts',(-18.2302062670491,13.6065605372724,123.664948493123)) ;
#19547 = CARTESIAN_POINT('Ctrl Pts',(-17.9354445009214,13.4265714569095,123.72824647118)) ;
#19548 = CARTESIAN_POINT('Ctrl Pts',(-18.2040444170886,13.6165639664654,123.456299673931)) ;
#19549 = CARTESIAN_POINT('Ctrl Pts',(-17.9027395319079,13.4365748861025,123.467435684465)) ;
#19550 = CARTESIAN_POINT('Ctrl Pts',(-18.2145600866286,13.6265494789316,123.246600447077)) ;
#19551 = CARTESIAN_POINT('Ctrl Pts',(-17.9158814573718,13.4465603985687,123.205311390375)) ;
#19552 = CARTESIAN_POINT('Ctrl Pts',(-18.2617823017495,13.6365905753156,123.040875922897)) ;
#19553 = CARTESIAN_POINT('Ctrl Pts',(-17.9749065837832,13.4566014949527,122.948155155583)) ;
#19554 = CARTESIAN_POINT('Ctrl Pts',(-18.3421364497269,13.6464337712666,122.850159429394)) ;
#19555 = CARTESIAN_POINT('Ctrl Pts',(-18.0753470360815,13.4664446909037,122.709757985454)) ;
#19556 = CARTESIAN_POINT('Ctrl Pts',(-18.4556351281271,13.656420082321,122.67358245955)) ;
#19557 = CARTESIAN_POINT('Ctrl Pts',(-18.217218281521,13.4764310019581,122.489035231126)) ;
#19558 = CARTESIAN_POINT('Ctrl Pts',(-18.5972804388859,13.6663547675787,122.520040996224)) ;
#19559 = CARTESIAN_POINT('Ctrl Pts',(-18.3942732512551,13.4863656872158,122.297106419642)) ;
#19560 = CARTESIAN_POINT('Ctrl Pts',(-18.7655457253041,13.6764123287957,122.392050964971)) ;
#19561 = CARTESIAN_POINT('Ctrl Pts',(-18.6046031877743,13.4964232484328,122.137116873894)) ;
#19562 = CARTESIAN_POINT('Ctrl Pts',(-18.948971596639,13.6862339704043,122.297188134367)) ;
#19563 = CARTESIAN_POINT('Ctrl Pts',(-18.8338850495127,13.5062448900414,122.018535713195)) ;
#19564 = CARTESIAN_POINT('Ctrl Pts',(-19.150630895694,13.6962900339953,122.233780317479)) ;
#19565 = CARTESIAN_POINT('Ctrl Pts',(-19.0859583258846,13.5163009536324,121.939273611562)) ;
#19566 = CARTESIAN_POINT('Ctrl Pts',(-19.3579055678042,13.7062307097571,122.207035465086)) ;
#19567 = CARTESIAN_POINT('Ctrl Pts',(-19.3450516698222,13.5262416293942,121.905839973782)) ;
#19568 = CARTESIAN_POINT('Ctrl Pts',(-19.5659365047634,13.7161350685454,122.215998316577)) ;
#19569 = CARTESIAN_POINT('Ctrl Pts',(-19.6050909750196,13.5361459881825,121.917041144644)) ;
#19570 = CARTESIAN_POINT('Ctrl Pts',(-19.7721240618805,13.7261817231212,122.26171766678)) ;
#19571 = CARTESIAN_POINT('Ctrl Pts',(-19.862825851585,13.5461926427583,121.97418792217)) ;
#19572 = CARTESIAN_POINT('Ctrl Pts',(-19.9644220298839,13.7360773177641,122.341175721282)) ;
#19573 = CARTESIAN_POINT('Ctrl Pts',(-20.1031997643857,13.5560882374012,122.073508487898)) ;
#19574 = CARTESIAN_POINT('Ctrl Pts',(-20.1429187786372,13.7461392644209,122.454645564807)) ;
#19575 = CARTESIAN_POINT('Ctrl Pts',(-20.3263218440362,13.5661501840581,122.215343672236)) ;
#19576 = CARTESIAN_POINT('Ctrl Pts',(-20.2957594945872,13.7559888883531,122.594367289572)) ;
#19577 = CARTESIAN_POINT('Ctrl Pts',(-20.5173749645332,13.5759998079902,122.38999462014)) ;
#19578 = CARTESIAN_POINT('Ctrl Pts',(-20.4240087228008,13.7659521273829,122.75995684231)) ;
#19579 = CARTESIAN_POINT('Ctrl Pts',(-20.6776884554839,13.5859630470201,122.596980439567)) ;
#19580 = CARTESIAN_POINT('Ctrl Pts',(-20.5219126757159,13.7759767021588,122.946597688754)) ;
#19581 = CARTESIAN_POINT('Ctrl Pts',(-20.8000704181908,13.5959876217959,122.830280403309)) ;
#19582 = CARTESIAN_POINT('Ctrl Pts',(-20.5853680857787,13.7858952648465,123.145221491814)) ;
#19583 = CARTESIAN_POINT('Ctrl Pts',(-20.8793920083737,13.6059061844836,123.07855998187)) ;
#19584 = CARTESIAN_POINT('Ctrl Pts',(-20.6139486861192,13.7958874515705,123.353347867714)) ;
#19585 = CARTESIAN_POINT('Ctrl Pts',(-20.9151199375489,13.6158983712076,123.338717822216)) ;
#19586 = CARTESIAN_POINT('Ctrl Pts',(-20.6055443985715,13.8059222501547,123.564135174219)) ;
#19587 = CARTESIAN_POINT('Ctrl Pts',(-20.9046168525977,13.6259331697918,123.6022019633)) ;
#19588 = CARTESIAN_POINT('Ctrl Pts',(-20.5618138969041,13.8157774408283,123.766670893346)) ;
#19589 = CARTESIAN_POINT('Ctrl Pts',(-20.8499556627768,13.6357883604655,123.855372966742)) ;
#19590 = CARTESIAN_POINT('Ctrl Pts',(-20.4827162908005,13.8257767889813,123.961402445332)) ;
#19591 = CARTESIAN_POINT('Ctrl Pts',(-20.7510855573927,13.6457877086185,124.098788324435)) ;
#19592 = CARTESIAN_POINT('Ctrl Pts',(-20.3723265103831,13.8356719146565,124.137764210175)) ;
#19593 = CARTESIAN_POINT('Ctrl Pts',(-20.6130996723433,13.6556828342936,124.319242233489)) ;
#19594 = CARTESIAN_POINT('Ctrl Pts',(-20.2306869988819,13.8457324576046,124.294801970209)) ;
#19595 = CARTESIAN_POINT('Ctrl Pts',(-20.4360519660016,13.6657433772417,124.515540628893)) ;
#19596 = CARTESIAN_POINT('Ctrl Pts',(-20.0674724058813,13.8555817318715,124.422248257044)) ;
#19597 = CARTESIAN_POINT('Ctrl Pts',(-20.2320341456861,13.6755926515086,124.674850714962)) ;
#19598 = CARTESIAN_POINT('Ctrl Pts',(-19.8815742262112,13.8656089564414,124.521635316517)) ;
#19599 = CARTESIAN_POINT('Ctrl Pts',(-19.9996623311131,13.6856198760785,124.799086161189)) ;
#19600 = CARTESIAN_POINT('Ctrl Pts',(-19.6810321497663,13.8756373556292,124.586723666077)) ;
#19601 = CARTESIAN_POINT('Ctrl Pts',(-19.7489854254844,13.6956482752663,124.880448501815)) ;
#19602 = CARTESIAN_POINT('Ctrl Pts',(-19.4761166290859,13.8854831060427,124.615846164903)) ;
#19603 = CARTESIAN_POINT('Ctrl Pts',(-19.4928401900497,13.7054940256798,124.916853671087)) ;
#19604 = CARTESIAN_POINT('Ctrl Pts',(-19.2662085926654,13.8954718964434,124.609433443135)) ;
#19605 = CARTESIAN_POINT('Ctrl Pts',(-19.230454887784,13.7154828160805,124.908839488335)) ;
#19606 = CARTESIAN_POINT('Ctrl Pts',(-19.0595750845739,13.9055168248431,124.565911416118)) ;
#19607 = CARTESIAN_POINT('Ctrl Pts',(-18.9721627761797,13.7255277444802,124.854438840815)) ;
#19608 = CARTESIAN_POINT('Ctrl Pts',(-18.8677390185657,13.9153413096321,124.489339185228)) ;
#19609 = CARTESIAN_POINT('Ctrl Pts',(-18.7323658376547,13.7353522292692,124.758724681303)) ;
#19610 = CARTESIAN_POINT('Ctrl Pts',(-18.6878125716597,13.9253987071733,124.378319657156)) ;
#19611 = CARTESIAN_POINT('Ctrl Pts',(-18.507457139982,13.7454096268104,124.619951807237)) ;
#19612 = CARTESIAN_POINT('Ctrl Pts',(-18.5321161135312,13.9353247987595,124.239354765055)) ;
#19613 = CARTESIAN_POINT('Ctrl Pts',(-18.3128349524813,13.7553357183966,124.44624656969)) ;
#19614 = CARTESIAN_POINT('Ctrl Pts',(-18.4021255349772,13.945279583904,124.075342585797)) ;
#19615 = CARTESIAN_POINT('Ctrl Pts',(-18.1503452309715,13.7652905035412,124.241231958245)) ;
#19616 = CARTESIAN_POINT('Ctrl Pts',(-18.3019676622171,13.9553169535617,123.889610890228)) ;
#19617 = CARTESIAN_POINT('Ctrl Pts',(-18.0251465109341,13.7753278731988,124.009068223143)) ;
#19618 = CARTESIAN_POINT('Ctrl Pts',(-18.2364086645203,13.9652057636833,123.692318961985)) ;
#19619 = CARTESIAN_POINT('Ctrl Pts',(-17.9431959784106,13.7852166833204,123.762452941019)) ;
#19620 = CARTESIAN_POINT('Ctrl Pts',(-18.2054221774035,13.9751951227343,123.484614442852)) ;
#19621 = CARTESIAN_POINT('Ctrl Pts',(-17.9044614031139,13.7952060423715,123.502822293364)) ;
#19622 = CARTESIAN_POINT('Ctrl Pts',(-18.2111097202979,13.9851536701904,123.275338157667)) ;
#19623 = CARTESIAN_POINT('Ctrl Pts',(-17.9115693386521,13.8051645898276,123.241226463732)) ;
#19624 = CARTESIAN_POINT('Ctrl Pts',(-18.2523005245241,13.9950532467415,123.071321965387)) ;
#19625 = CARTESIAN_POINT('Ctrl Pts',(-17.9630567197968,13.8150641663786,122.986205100608)) ;
#19626 = CARTESIAN_POINT('Ctrl Pts',(-18.3294851382835,14.0051011585722,122.874712691268)) ;
#19627 = CARTESIAN_POINT('Ctrl Pts',(-18.0595361492998,13.8251120782093,122.740443216478)) ;
#19628 = CARTESIAN_POINT('Ctrl Pts',(-18.4378511245041,14.0149965064327,122.697097031468)) ;
#19629 = CARTESIAN_POINT('Ctrl Pts',(-18.1949930036132,13.8350074260699,122.518422190268)) ;
#19630 = CARTESIAN_POINT('Ctrl Pts',(-18.5776635026499,14.0250581829639,122.538393890947)) ;
#19631 = CARTESIAN_POINT('Ctrl Pts',(-18.3697572977927,13.845069102601,122.320042659935)) ;
#19632 = CARTESIAN_POINT('Ctrl Pts',(-18.7393445312316,14.0349027007131,122.409181627727)) ;
#19633 = CARTESIAN_POINT('Ctrl Pts',(-18.5718588198519,13.8549136203502,122.158525512922)) ;
#19634 = CARTESIAN_POINT('Ctrl Pts',(-18.9227751263348,14.0448631444279,122.308189876658)) ;
#19635 = CARTESIAN_POINT('Ctrl Pts',(-18.8011469810602,13.864874064065,122.032284729829)) ;
#19636 = CARTESIAN_POINT('Ctrl Pts',(-19.1226020522299,14.0548999772461,122.240434925921)) ;
#19637 = CARTESIAN_POINT('Ctrl Pts',(-19.0509301231226,13.8749108968832,121.947590007007)) ;
#19638 = CARTESIAN_POINT('Ctrl Pts',(-19.3278464181783,14.0647787739929,122.208569582796)) ;
#19639 = CARTESIAN_POINT('Ctrl Pts',(-19.3074865101994,13.88478969363,121.907757156992)) ;
#19640 = CARTESIAN_POINT('Ctrl Pts',(-19.5392604494556,14.0748380901212,122.212835075085)) ;
#19641 = CARTESIAN_POINT('Ctrl Pts',(-19.5717537455678,13.8948490097584,121.91308802529)) ;
#19642 = CARTESIAN_POINT('Ctrl Pts',(-19.7428603551298,14.0847085368744,122.252978784912)) ;
#19643 = CARTESIAN_POINT('Ctrl Pts',(-19.8262549511952,13.9047194565116,121.963266910915)) ;
#19644 = CARTESIAN_POINT('Ctrl Pts',(-19.9389874347738,14.0947011751325,122.328256871601)) ;
#19645 = CARTESIAN_POINT('Ctrl Pts',(-20.0714142577279,13.9147120947696,122.057363864517)) ;
#19646 = CARTESIAN_POINT('Ctrl Pts',(-20.1195329190691,14.1047331906804,122.437257388524)) ;
#19647 = CARTESIAN_POINT('Ctrl Pts',(-20.2970965036502,13.9247441103175,122.193613633218)) ;
#19648 = CARTESIAN_POINT('Ctrl Pts',(-20.2760952863307,14.114599046987,122.573331296322)) ;
#19649 = CARTESIAN_POINT('Ctrl Pts',(-20.4928009018349,13.9346099666241,122.363706237578)) ;
#19650 = CARTESIAN_POINT('Ctrl Pts',(-20.4093323895338,14.1246683364561,122.737799807902)) ;
#19651 = CARTESIAN_POINT('Ctrl Pts',(-20.6593476164435,13.9446792560932,122.569291069351)) ;
#19652 = CARTESIAN_POINT('Ctrl Pts',(-20.5097252080318,14.1345118940074,122.918773104725)) ;
#19653 = CARTESIAN_POINT('Ctrl Pts',(-20.7848399902421,13.9545228136445,122.795508554596)) ;
#19654 = CARTESIAN_POINT('Ctrl Pts',(-20.5787488120301,14.1444920207952,123.116900923629)) ;
#19655 = CARTESIAN_POINT('Ctrl Pts',(-20.871120064522,13.9645029404324,123.043168459414)) ;
#19656 = CARTESIAN_POINT('Ctrl Pts',(-20.6120524726319,14.1545105693952,123.324867150909)) ;
#19657 = CARTESIAN_POINT('Ctrl Pts',(-20.9127502836893,13.9745214890323,123.303126129535)) ;
#19658 = CARTESIAN_POINT('Ctrl Pts',(-20.6092267809851,14.1643938699184,123.532651027033)) ;
#19659 = CARTESIAN_POINT('Ctrl Pts',(-20.9092186327094,13.9844047895555,123.562857078074)) ;
#19660 = CARTESIAN_POINT('Ctrl Pts',(-20.5695586363973,14.1744621569665,123.740532636129)) ;
#19661 = CARTESIAN_POINT('Ctrl Pts',(-20.8596340362664,13.9944730766036,123.822708783211)) ;
#19662 = CARTESIAN_POINT('Ctrl Pts',(-20.4963791598284,14.1842922799851,123.933839607261)) ;
#19663 = CARTESIAN_POINT('Ctrl Pts',(-20.7681595371697,14.0043031996223,124.064344085627)) ;
#19664 = CARTESIAN_POINT('Ctrl Pts',(-20.3884763220446,14.1943588639105,124.115856989045)) ;
#19665 = CARTESIAN_POINT('Ctrl Pts',(-20.6332814623007,14.0143697835476,124.291865630646)) ;
#19666 = CARTESIAN_POINT('Ctrl Pts',(-20.2528909010088,14.2042489769249,124.273525084078)) ;
#19667 = CARTESIAN_POINT('Ctrl Pts',(-20.4637992773007,14.0242598965621,124.488951781943)) ;
#19668 = CARTESIAN_POINT('Ctrl Pts',(-20.0906371997248,14.2142416656876,124.406937747112)) ;
#19669 = CARTESIAN_POINT('Ctrl Pts',(-20.2609821100153,14.0342525853247,124.655717889191)) ;
#19670 = CARTESIAN_POINT('Ctrl Pts',(-19.9081695184652,14.2242025540433,124.509708404688)) ;
#19671 = CARTESIAN_POINT('Ctrl Pts',(-20.0328972096088,14.0442134736805,124.784181661414)) ;
#19672 = CARTESIAN_POINT('Ctrl Pts',(-19.7116219047513,14.2341204989233,124.579266374256)) ;
#19673 = CARTESIAN_POINT('Ctrl Pts',(-19.7872119388903,14.0541314185605,124.87112949854)) ;
#19674 = CARTESIAN_POINT('Ctrl Pts',(-19.5041267455453,14.2441282520195,124.61419846985)) ;
#19675 = CARTESIAN_POINT('Ctrl Pts',(-19.527842932523,14.0641391716567,124.914794637581)) ;
#19676 = CARTESIAN_POINT('Ctrl Pts',(-19.2932629141695,14.2541593459786,124.612140808349)) ;
#19677 = CARTESIAN_POINT('Ctrl Pts',(-19.2642632651857,14.0741702656157,124.912222739613)) ;
#19678 = CARTESIAN_POINT('Ctrl Pts',(-19.0896342106667,14.2640073140066,124.57465995118)) ;
#19679 = CARTESIAN_POINT('Ctrl Pts',(-19.0097259981526,14.0840182336437,124.865371406458)) ;
#19680 = CARTESIAN_POINT('Ctrl Pts',(-18.8913548972053,14.2740692701324,124.501004306892)) ;
#19681 = CARTESIAN_POINT('Ctrl Pts',(-18.7618772164016,14.0940801897696,124.773301901415)) ;
#19682 = CARTESIAN_POINT('Ctrl Pts',(-18.7119419266118,14.2839664817336,124.395611023166)) ;
#19683 = CARTESIAN_POINT('Ctrl Pts',(-18.5376101429091,14.1039774013707,124.641559789166)) ;
#19684 = CARTESIAN_POINT('Ctrl Pts',(-18.5525741212308,14.2938976483982,124.260736428545)) ;
#19685 = CARTESIAN_POINT('Ctrl Pts',(-18.3384000135968,14.1139085680353,124.472965869001)) ;
#19686 = CARTESIAN_POINT('Ctrl Pts',(-18.4177287010278,14.3039398326024,124.098297375406)) ;
#19687 = CARTESIAN_POINT('Ctrl Pts',(-18.169843513441,14.1239507522395,124.269917095288)) ;
#19688 = CARTESIAN_POINT('Ctrl Pts',(-18.3146195122506,14.3138265008555,123.917815954086)) ;
#19689 = CARTESIAN_POINT('Ctrl Pts',(-18.0409566998773,14.1338374204927,124.044314253981)) ;
#19690 = CARTESIAN_POINT('Ctrl Pts',(-18.2433338154398,14.3238196128338,123.720204704618)) ;
#19691 = CARTESIAN_POINT('Ctrl Pts',(-17.9518498698231,14.1438305324709,123.797299870393)) ;
#19692 = CARTESIAN_POINT('Ctrl Pts',(-18.2076886193533,14.3337652904496,123.514175880864)) ;
#19693 = CARTESIAN_POINT('Ctrl Pts',(-17.9072936184703,14.1537762100867,123.539763194409)) ;
#19694 = CARTESIAN_POINT('Ctrl Pts',(-18.2079318857893,14.3437125934346,123.305042620039)) ;
#19695 = CARTESIAN_POINT('Ctrl Pts',(-17.9075982211722,14.1637235130717,123.278346044345)) ;
#19696 = CARTESIAN_POINT('Ctrl Pts',(-18.2450800860336,14.3537603171813,123.09710524755)) ;
#19697 = CARTESIAN_POINT('Ctrl Pts',(-17.9540338467725,14.1737712368185,123.018424649771)) ;
#19698 = CARTESIAN_POINT('Ctrl Pts',(-18.3161751561514,14.3636086909439,122.902654315691)) ;
#19699 = CARTESIAN_POINT('Ctrl Pts',(-18.0429036250617,14.183619610581,122.775359841272)) ;
#19700 = CARTESIAN_POINT('Ctrl Pts',(-18.420516020689,14.3735676633896,122.72113759086)) ;
#19701 = CARTESIAN_POINT('Ctrl Pts',(-18.1733306008267,14.1935785830267,122.54846390798)) ;
#19702 = CARTESIAN_POINT('Ctrl Pts',(-18.5561553946168,14.3836065252707,122.559457330409)) ;
#19703 = CARTESIAN_POINT('Ctrl Pts',(-18.3428801887918,14.2036174449079,122.346364098552)) ;
#19704 = CARTESIAN_POINT('Ctrl Pts',(-18.7150352575607,14.3934851294425,122.425678518084)) ;
#19705 = CARTESIAN_POINT('Ctrl Pts',(-18.5414813532127,14.2134960490797,122.179140432255)) ;
#19706 = CARTESIAN_POINT('Ctrl Pts',(-18.8977873014348,14.4035366706458,122.319642116266)) ;
#19707 = CARTESIAN_POINT('Ctrl Pts',(-18.7699215575239,14.223547590283,122.046595739492)) ;
#19708 = CARTESIAN_POINT('Ctrl Pts',(-19.0931303673642,14.4134320686262,122.247993391467)) ;
#19709 = CARTESIAN_POINT('Ctrl Pts',(-19.0141015690712,14.2334429882633,121.957035255779)) ;
#19710 = CARTESIAN_POINT('Ctrl Pts',(-19.3010884804579,14.4234833011715,122.21067275502)) ;
#19711 = CARTESIAN_POINT('Ctrl Pts',(-19.2740491001981,14.2434942208086,121.910385335695)) ;
#19712 = CARTESIAN_POINT('Ctrl Pts',(-19.5089481133767,14.4333694917958,122.210014197756)) ;
#19713 = CARTESIAN_POINT('Ctrl Pts',(-19.5338747027506,14.2533804114329,121.909562985904)) ;
#19714 = CARTESIAN_POINT('Ctrl Pts',(-19.7159932801428,14.4433620311115,122.245450565557)) ;
#19715 = CARTESIAN_POINT('Ctrl Pts',(-19.7926811889532,14.2633729507487,121.953859464746)) ;
#19716 = CARTESIAN_POINT('Ctrl Pts',(-19.9128752055225,14.4533104770063,122.316060788436)) ;
#19717 = CARTESIAN_POINT('Ctrl Pts',(-20.0387837794866,14.2733213966434,122.042123340413)) ;
#19718 = CARTESIAN_POINT('Ctrl Pts',(-20.0944137100652,14.4632472795382,122.419388130175)) ;
#19719 = CARTESIAN_POINT('Ctrl Pts',(-20.2657069288235,14.2832581991753,122.171283774759)) ;
#19720 = CARTESIAN_POINT('Ctrl Pts',(-20.2562053966534,14.4732302869895,122.553111371439)) ;
#19721 = CARTESIAN_POINT('Ctrl Pts',(-20.4679459835233,14.2932412066266,122.338438899069)) ;
#19722 = CARTESIAN_POINT('Ctrl Pts',(-20.3928213225405,14.4832741284043,122.714082144546)) ;
#19723 = CARTESIAN_POINT('Ctrl Pts',(-20.6387149774407,14.3032850480414,122.539652891498)) ;
#19724 = CARTESIAN_POINT('Ctrl Pts',(-20.4975727490238,14.4931023270282,122.892216003962)) ;
#19725 = CARTESIAN_POINT('Ctrl Pts',(-20.7696539436816,14.3131132466653,122.762322078436)) ;
#19726 = CARTESIAN_POINT('Ctrl Pts',(-20.5716961928806,14.5031789204704,123.09062015157)) ;
#19727 = CARTESIAN_POINT('Ctrl Pts',(-20.8623069213888,14.3231898401075,123.010327296333)) ;
#19728 = CARTESIAN_POINT('Ctrl Pts',(-20.6095053348988,14.513030919812,123.29430613063)) ;
#19729 = CARTESIAN_POINT('Ctrl Pts',(-20.909567306365,14.3330418394491,123.264936220785)) ;
#19730 = CARTESIAN_POINT('Ctrl Pts',(-20.6115890759441,14.5231045066358,123.506038201766)) ;
#19731 = CARTESIAN_POINT('Ctrl Pts',(-20.9121706248892,14.343115426273,123.529600919858)) ;
#19732 = CARTESIAN_POINT('Ctrl Pts',(-20.5776337189286,14.5329447317333,123.710123522401)) ;
#19733 = CARTESIAN_POINT('Ctrl Pts',(-20.8697248958235,14.3529556513705,123.784708643342)) ;
#19734 = CARTESIAN_POINT('Ctrl Pts',(-20.5085876603415,14.542910435762,123.907911470471)) ;
#19735 = CARTESIAN_POINT('Ctrl Pts',(-20.7834156858806,14.3629213553991,124.031943418832)) ;
#19736 = CARTESIAN_POINT('Ctrl Pts',(-20.4053409396209,14.5529370690686,124.091700513601)) ;
#19737 = CARTESIAN_POINT('Ctrl Pts',(-20.6543560175008,14.3729479887057,124.26167893838)) ;
#19738 = CARTESIAN_POINT('Ctrl Pts',(-20.2733679541214,14.5628513647804,124.253019570529)) ;
#19739 = CARTESIAN_POINT('Ctrl Pts',(-20.4893881315526,14.3828622844175,124.463327357308)) ;
#19740 = CARTESIAN_POINT('Ctrl Pts',(-20.1144447570708,14.5728396534728,124.390287718717)) ;
#19741 = CARTESIAN_POINT('Ctrl Pts',(-20.29073289972,14.39285057311,124.634911409917)) ;
#19742 = CARTESIAN_POINT('Ctrl Pts',(-19.93300982332,14.5828783866312,124.498080446046)) ;
#19743 = CARTESIAN_POINT('Ctrl Pts',(-20.0639385669575,14.4028893062683,124.769650931547)) ;
#19744 = CARTESIAN_POINT('Ctrl Pts',(-19.739575472665,14.5927217184587,124.571609128069)) ;
#19745 = CARTESIAN_POINT('Ctrl Pts',(-19.8221438934761,14.4127326380959,124.861560677325)) ;
#19746 = CARTESIAN_POINT('Ctrl Pts',(-19.5325945345893,14.6027494443383,124.611640004367)) ;
#19747 = CARTESIAN_POINT('Ctrl Pts',(-19.5634174500474,14.4227603639755,124.911597480083)) ;
#19748 = CARTESIAN_POINT('Ctrl Pts',(-19.3216956220107,14.6127817807269,124.614552263941)) ;
#19749 = CARTESIAN_POINT('Ctrl Pts',(-19.2997938732283,14.432792700364,124.915236180486)) ;
#19750 = CARTESIAN_POINT('Ctrl Pts',(-19.1176575039999,14.6226112810275,124.581899390616)) ;
#19751 = CARTESIAN_POINT('Ctrl Pts',(-19.0447452472327,14.4426222006646,124.874418148553)) ;
#19752 = CARTESIAN_POINT('Ctrl Pts',(-18.9189866148987,14.6326007849443,124.513805611947)) ;
#19753 = CARTESIAN_POINT('Ctrl Pts',(-18.796407103076,14.4526117045814,124.789299015739)) ;
#19754 = CARTESIAN_POINT('Ctrl Pts',(-18.7344236623876,14.6426446254567,124.411231786097)) ;
#19755 = CARTESIAN_POINT('Ctrl Pts',(-18.5657044122553,14.4626555450938,124.661080239922)) ;
#19756 = CARTESIAN_POINT('Ctrl Pts',(-18.5738301995033,14.6524663312247,124.281444401144)) ;
#19757 = CARTESIAN_POINT('Ctrl Pts',(-18.3649628204512,14.4724772508619,124.498843726449)) ;
#19758 = CARTESIAN_POINT('Ctrl Pts',(-18.4348762560386,14.6625013783571,124.122702247143)) ;
#19759 = CARTESIAN_POINT('Ctrl Pts',(-18.1912720235427,14.4825122979942,124.300414746533)) ;
#19760 = CARTESIAN_POINT('Ctrl Pts',(-18.3262031256769,14.672526055794,123.942122520734)) ;
#19761 = CARTESIAN_POINT('Ctrl Pts',(-18.055432254409,14.4925369754311,124.074689127998)) ;
#19762 = CARTESIAN_POINT('Ctrl Pts',(-18.2514273159942,14.6823788706484,123.748954040769)) ;
#19763 = CARTESIAN_POINT('Ctrl Pts',(-17.9619640242889,14.5023897902856,123.833226852752)) ;
#19764 = CARTESIAN_POINT('Ctrl Pts',(-18.2104197904952,14.692366580256,123.543040108188)) ;
#19765 = CARTESIAN_POINT('Ctrl Pts',(-17.9107066774369,14.5123774998931,123.575833839664)) ;
#19766 = CARTESIAN_POINT('Ctrl Pts',(-18.2058049225117,14.7022965902501,123.334323737137)) ;
#19767 = CARTESIAN_POINT('Ctrl Pts',(-17.9049402191342,14.5223075098872,123.314937805648)) ;
#19768 = CARTESIAN_POINT('Ctrl Pts',(-18.2373702335,14.7122863454692,123.126689249675)) ;
#19769 = CARTESIAN_POINT('Ctrl Pts',(-17.9443990827381,14.5322972651064,123.055394867544)) ;
#19770 = CARTESIAN_POINT('Ctrl Pts',(-18.3050137193924,14.7223129541521,122.927042802694)) ;
#19771 = CARTESIAN_POINT('Ctrl Pts',(-18.0289554645481,14.5423238737893,122.80583753216)) ;
#19772 = CARTESIAN_POINT('Ctrl Pts',(-18.4046749189677,14.732196894174,122.744715504703)) ;
#19773 = CARTESIAN_POINT('Ctrl Pts',(-18.1535342537274,14.5522078138111,122.577928818094)) ;
#19774 = CARTESIAN_POINT('Ctrl Pts',(-18.5354880156566,14.7421861217125,122.580419937995)) ;
#19775 = CARTESIAN_POINT('Ctrl Pts',(-18.3170525414426,14.5621970413496,122.372560685954)) ;
#19776 = CARTESIAN_POINT('Ctrl Pts',(-18.6939694465223,14.7522289922362,122.44092045882)) ;
#19777 = CARTESIAN_POINT('Ctrl Pts',(-18.5151557257719,14.5722399118733,122.198188061704)) ;
#19778 = CARTESIAN_POINT('Ctrl Pts',(-18.8703137137284,14.7620613789916,122.333079749863)) ;
#19779 = CARTESIAN_POINT('Ctrl Pts',(-18.7355880780577,14.5820722986287,122.063388638443)) ;
#19780 = CARTESIAN_POINT('Ctrl Pts',(-19.0656282841589,14.7720546721632,122.255693489157)) ;
#19781 = CARTESIAN_POINT('Ctrl Pts',(-18.9797323076057,14.5920655918003,121.966658037112)) ;
#19782 = CARTESIAN_POINT('Ctrl Pts',(-19.2723122403626,14.7820866778116,122.213661473494)) ;
#19783 = CARTESIAN_POINT('Ctrl Pts',(-19.2380876823601,14.6020975974487,121.914120317295)) ;
#19784 = CARTESIAN_POINT('Ctrl Pts',(-19.4796224788741,14.7919519337806,122.207990741201)) ;
#19785 = CARTESIAN_POINT('Ctrl Pts',(-19.4972262784199,14.6119628534177,121.907034280981)) ;
#19786 = CARTESIAN_POINT('Ctrl Pts',(-19.686880956539,14.8019138136881,122.238115152982)) ;
#19787 = CARTESIAN_POINT('Ctrl Pts',(-19.7562992627137,14.6219247333252,121.944692330567)) ;
#19788 = CARTESIAN_POINT('Ctrl Pts',(-19.8870940592205,14.81194874705,122.304572113576)) ;
#19789 = CARTESIAN_POINT('Ctrl Pts',(-20.0065648350329,14.6319596666871,122.027765848265)) ;
#19790 = CARTESIAN_POINT('Ctrl Pts',(-20.0701544259768,14.8218337054293,122.402996415654)) ;
#19791 = CARTESIAN_POINT('Ctrl Pts',(-20.2353895991265,14.6418446250664,122.150798715635)) ;
#19792 = CARTESIAN_POINT('Ctrl Pts',(-20.2362472111695,14.8318993323519,122.534060407699)) ;
#19793 = CARTESIAN_POINT('Ctrl Pts',(-20.4430039039663,14.6519102519891,122.314630587451)) ;
#19794 = CARTESIAN_POINT('Ctrl Pts',(-20.3740932209751,14.8417384380163,122.688329422969)) ;
#19795 = CARTESIAN_POINT('Ctrl Pts',(-20.6153099874822,14.6617493576534,122.507469086936)) ;
#19796 = CARTESIAN_POINT('Ctrl Pts',(-20.4857432775784,14.8518012530216,122.867986014556)) ;
#19797 = CARTESIAN_POINT('Ctrl Pts',(-20.7548702754188,14.6718121726588,122.732041086105)) ;
#19798 = CARTESIAN_POINT('Ctrl Pts',(-20.5630404308717,14.8616974590703,123.061166562861)) ;
#19799 = CARTESIAN_POINT('Ctrl Pts',(-20.8514895076296,14.6817083787074,122.973518167656)) ;
#19800 = CARTESIAN_POINT('Ctrl Pts',(-20.6063727048954,14.8716382820956,123.265587679795)) ;
#19801 = CARTESIAN_POINT('Ctrl Pts',(-20.905652298732,14.6916492017327,123.229045388477)) ;
#19802 = CARTESIAN_POINT('Ctrl Pts',(-20.6136516344617,14.8816428650742,123.47581329813)) ;
#19803 = CARTESIAN_POINT('Ctrl Pts',(-20.9147482972179,14.7016537847114,123.49182757385)) ;
#19804 = CARTESIAN_POINT('Ctrl Pts',(-20.5840199308421,14.891663759519,123.684384900853)) ;
#19805 = CARTESIAN_POINT('Ctrl Pts',(-20.8777060565819,14.7116746791561,123.752541737872)) ;
#19806 = CARTESIAN_POINT('Ctrl Pts',(-20.5197082244626,14.9015556801084,123.882155751433)) ;
#19807 = CARTESIAN_POINT('Ctrl Pts',(-20.7973137583484,14.7215665997455,123.999754867603)) ;
#19808 = CARTESIAN_POINT('Ctrl Pts',(-20.4213024996246,14.9115491124538,124.067769431274)) ;
#19809 = CARTESIAN_POINT('Ctrl Pts',(-20.6743041569518,14.7315600320909,124.231770792966)) ;
#19810 = CARTESIAN_POINT('Ctrl Pts',(-20.2927239230316,14.9214947173536,124.232648085746)) ;
#19811 = CARTESIAN_POINT('Ctrl Pts',(-20.5135786631871,14.7415056369908,124.437867633095)) ;
#19812 = CARTESIAN_POINT('Ctrl Pts',(-20.1377200748608,14.9314419908352,124.373043867283)) ;
#19813 = CARTESIAN_POINT('Ctrl Pts',(-20.3198218573511,14.7514529104723,124.613360457444)) ;
#19814 = CARTESIAN_POINT('Ctrl Pts',(-19.9587916673367,14.9414899053115,124.485309172283)) ;
#19815 = CARTESIAN_POINT('Ctrl Pts',(-20.0961599099383,14.7615008249487,124.753689774848)) ;
#19816 = CARTESIAN_POINT('Ctrl Pts',(-19.7670469759163,14.9513375456589,124.563382819774)) ;
#19817 = CARTESIAN_POINT('Ctrl Pts',(-19.8564776376663,14.771348465296,124.851279444888)) ;
#19818 = CARTESIAN_POINT('Ctrl Pts',(-19.5624646344758,14.9612992610355,124.608121127697)) ;
#19819 = CARTESIAN_POINT('Ctrl Pts',(-19.6007489896213,14.7813101806726,124.907199618394)) ;
#19820 = CARTESIAN_POINT('Ctrl Pts',(-19.3517826029045,14.9713278846083,124.61644912002)) ;
#19821 = CARTESIAN_POINT('Ctrl Pts',(-19.3373962978428,14.7913388042454,124.917606836282)) ;
#19822 = CARTESIAN_POINT('Ctrl Pts',(-19.145332332827,14.9812382466747,124.588473295284)) ;
#19823 = CARTESIAN_POINT('Ctrl Pts',(-19.0793336231031,14.8012491663118,124.882634265756)) ;
#19824 = CARTESIAN_POINT('Ctrl Pts',(-18.9462038692032,14.9911729403271,124.525440044832)) ;
#19825 = CARTESIAN_POINT('Ctrl Pts',(-18.8304237660988,14.8111838599642,124.803839977348)) ;
#19826 = CARTESIAN_POINT('Ctrl Pts',(-18.7591614865791,15.001214783455,124.427569567412)) ;
#19827 = CARTESIAN_POINT('Ctrl Pts',(-18.5966220485025,14.8212257030921,124.681499373881)) ;
#19828 = CARTESIAN_POINT('Ctrl Pts',(-18.5944360678556,15.0110992890254,124.300855256588)) ;
#19829 = CARTESIAN_POINT('Ctrl Pts',(-18.390716860511,14.8311102086625,124.523104155642)) ;
#19830 = CARTESIAN_POINT('Ctrl Pts',(-18.4524001316479,15.0211013928106,124.145842998901)) ;
#19831 = CARTESIAN_POINT('Ctrl Pts',(-18.2131739736385,14.8411123124477,124.329336878928)) ;
#19832 = CARTESIAN_POINT('Ctrl Pts',(-18.3402023620306,15.0310197442256,123.970045804479)) ;
#19833 = CARTESIAN_POINT('Ctrl Pts',(-18.0729290956816,14.8510306638627,124.109588770675)) ;
#19834 = CARTESIAN_POINT('Ctrl Pts',(-18.2592672869496,15.0410674002465,123.774968507367)) ;
#19835 = CARTESIAN_POINT('Ctrl Pts',(-17.9717628132547,14.8610783198836,123.865741080711)) ;
#19836 = CARTESIAN_POINT('Ctrl Pts',(-18.2139943917343,15.0509385932747,123.572398931231)) ;
#19837 = CARTESIAN_POINT('Ctrl Pts',(-17.9151745106479,14.8709495129118,123.612528140335)) ;
#19838 = CARTESIAN_POINT('Ctrl Pts',(-18.2043671465967,15.0610043064182,123.361053655738)) ;
#19839 = CARTESIAN_POINT('Ctrl Pts',(-17.9031429831484,14.8810152260553,123.34834743098)) ;
#19840 = CARTESIAN_POINT('Ctrl Pts',(-18.2307795956915,15.0708567669908,123.155558216153)) ;
#19841 = CARTESIAN_POINT('Ctrl Pts',(-17.9361624249687,14.890867686628,123.091474379834)) ;
#19842 = CARTESIAN_POINT('Ctrl Pts',(-18.314927021648,15.0842852297134,122.886155404172)) ;
#19843 = CARTESIAN_POINT('Ctrl Pts',(-18.0413449335706,14.9042961493505,122.754742299802)) ;
#19844 = CARTESIAN_POINT('Ctrl Pts',(-18.4633001207492,15.0973661772305,122.650732206668)) ;
#19845 = CARTESIAN_POINT('Ctrl Pts',(-18.2267874470069,14.9173770968676,122.460483907588)) ;
#19846 = CARTESIAN_POINT('Ctrl Pts',(-18.6709215131284,15.110840675465,122.458175069999)) ;
#19847 = CARTESIAN_POINT('Ctrl Pts',(-18.4863543902938,14.9308515951022,122.219747666857)) ;
#19848 = CARTESIAN_POINT('Ctrl Pts',(-18.8447665738617,15.1206727790745,122.346277793249)) ;
#19849 = CARTESIAN_POINT('Ctrl Pts',(-18.7036544341988,14.9406836987116,122.079886991967)) ;
#19850 = CARTESIAN_POINT('Ctrl Pts',(-19.0375991766532,15.1306386822012,122.264426190155)) ;
#19851 = CARTESIAN_POINT('Ctrl Pts',(-18.9446987351203,14.9506496018383,121.977572951031)) ;
#19852 = CARTESIAN_POINT('Ctrl Pts',(-19.2431027809361,15.1406660915114,122.217314375215)) ;
#19853 = CARTESIAN_POINT('Ctrl Pts',(-19.2015765911018,14.9606770111485,121.918685704724)) ;
#19854 = CARTESIAN_POINT('Ctrl Pts',(-19.4511603917055,15.150577122878,122.206669239406)) ;
#19855 = CARTESIAN_POINT('Ctrl Pts',(-19.4616556588049,14.9705880425151,121.905384721623)) ;
#19856 = CARTESIAN_POINT('Ctrl Pts',(-19.7276733496542,15.163821430499,122.240072867962)) ;
#19857 = CARTESIAN_POINT('Ctrl Pts',(-19.8072618039374,14.9838323501362,121.947128778354)) ;
#19858 = CARTESIAN_POINT('Ctrl Pts',(-20.0569080569754,15.1805219131702,122.372778838028)) ;
#19859 = CARTESIAN_POINT('Ctrl Pts',(-20.2188550941679,15.0005328328073,122.113045312188)) ;
#19860 = CARTESIAN_POINT('Ctrl Pts',(-20.3183298277955,15.197028742326,122.607156814012)) ;
#19861 = CARTESIAN_POINT('Ctrl Pts',(-20.5455679441702,15.0170396619631,122.405960959497)) ;
#19862 = CARTESIAN_POINT('Ctrl Pts',(-20.4717021929632,15.2103393705636,122.841112767138)) ;
#19863 = CARTESIAN_POINT('Ctrl Pts',(-20.7373262391937,15.0303502902007,122.698457845509)) ;
#19864 = CARTESIAN_POINT('Ctrl Pts',(-20.5546889086436,15.2203319341037,123.034149268203)) ;
#19865 = CARTESIAN_POINT('Ctrl Pts',(-20.8410482037776,15.0403428537408,122.939743261889)) ;
#19866 = CARTESIAN_POINT('Ctrl Pts',(-20.6028117634593,15.2303620171052,123.239415681091)) ;
#19867 = CARTESIAN_POINT('Ctrl Pts',(-20.9012011780977,15.0503729367423,123.196334518998)) ;
#19868 = CARTESIAN_POINT('Ctrl Pts',(-20.6188231290724,15.243535621103,123.51597584994)) ;
#19869 = CARTESIAN_POINT('Ctrl Pts',(-20.9212136813736,15.0635465407401,123.542009444152)) ;
#19870 = CARTESIAN_POINT('Ctrl Pts',(-20.5476924046879,15.2601733263344,123.862358698214)) ;
#19871 = CARTESIAN_POINT('Ctrl Pts',(-20.8322977307926,15.0801842459715,123.97501211203)) ;
#19872 = CARTESIAN_POINT('Ctrl Pts',(-20.3266298052787,15.2800550889018,124.222868771879)) ;
#19873 = CARTESIAN_POINT('Ctrl Pts',(-20.5559470864143,15.1000660085389,124.425649304088)) ;
#19874 = CARTESIAN_POINT('Ctrl Pts',(-20.0488038588937,15.2967514411183,124.443780899376)) ;
#19875 = CARTESIAN_POINT('Ctrl Pts',(-20.2087222530336,15.1167623607554,124.70175262575)) ;
#19876 = CARTESIAN_POINT('Ctrl Pts',(-19.7952370287234,15.3099084689074,124.554316113986)) ;
#19877 = CARTESIAN_POINT('Ctrl Pts',(-19.8917080630513,15.1299193885445,124.839949683673)) ;
#19878 = CARTESIAN_POINT('Ctrl Pts',(-19.5219729563658,15.3232858235509,124.620769738121)) ;
#19879 = CARTESIAN_POINT('Ctrl Pts',(-19.5501536847632,15.1432967431881,124.92300774244)) ;
#19880 = CARTESIAN_POINT('Ctrl Pts',(-19.1705511769297,15.3398166578097,124.612563673835)) ;
#19881 = CARTESIAN_POINT('Ctrl Pts',(-19.1108554066313,15.1598275774469,124.912748434119)) ;
#19882 = CARTESIAN_POINT('Ctrl Pts',(-18.7747945960682,15.3597813475528,124.459104510139)) ;
#19883 = CARTESIAN_POINT('Ctrl Pts',(-18.616168502824,15.17979226719,124.720920100906)) ;
#19884 = CARTESIAN_POINT('Ctrl Pts',(-18.4561643055464,15.3796978409765,124.180149863833)) ;
#19885 = CARTESIAN_POINT('Ctrl Pts',(-18.2178819295255,15.1997087606136,124.372224270615)) ;
#19886 = CARTESIAN_POINT('Ctrl Pts',(-18.2513709239315,15.399587560326,123.810085056575)) ;
#19887 = CARTESIAN_POINT('Ctrl Pts',(-17.9618943674429,15.2195984799632,123.909642300137)) ;
#19888 = CARTESIAN_POINT('Ctrl Pts',(-18.185122044345,15.4195942899739,123.38994096914)) ;
#19889 = CARTESIAN_POINT('Ctrl Pts',(-17.8790867340295,15.239605209611,123.384461553137)) ;
#19890 = CARTESIAN_POINT('Ctrl Pts',(-18.2652543652805,15.4394323436208,122.975722101847)) ;
#19891 = CARTESIAN_POINT('Ctrl Pts',(-17.9792551414852,15.2594432632579,122.866690154571)) ;
#19892 = CARTESIAN_POINT('Ctrl Pts',(-18.4831677244092,15.4594256818344,122.610800320768)) ;
#19893 = CARTESIAN_POINT('Ctrl Pts',(-18.2516493430185,15.2794366014715,122.410539526417)) ;
#19894 = CARTESIAN_POINT('Ctrl Pts',(-18.8109961180814,15.479308481241,122.343735818946)) ;
#19895 = CARTESIAN_POINT('Ctrl Pts',(-18.661435692982,15.2993194008781,122.076711965965)) ;
#19896 = CARTESIAN_POINT('Ctrl Pts',(-19.2100433870964,15.4992006621597,122.203893854528)) ;
#19897 = CARTESIAN_POINT('Ctrl Pts',(-19.1602442446391,15.3192115817968,121.901912195536)) ;
#19898 = CARTESIAN_POINT('Ctrl Pts',(-19.6333249972784,15.5191028406548,122.207913004512)) ;
#19899 = CARTESIAN_POINT('Ctrl Pts',(-19.6893450348153,15.3391137602919,121.906937811211)) ;
#19900 = CARTESIAN_POINT('Ctrl Pts',(-20.0320344555378,15.5391401518585,122.357748545318)) ;
#19901 = CARTESIAN_POINT('Ctrl Pts',(-20.1877316480936,15.3591510714956,122.094234259217)) ;
#19902 = CARTESIAN_POINT('Ctrl Pts',(-20.3526586672201,15.5589525933994,122.631285692703)) ;
#19903 = CARTESIAN_POINT('Ctrl Pts',(-20.5885091138174,15.3789635130365,122.4361550605)) ;
#19904 = CARTESIAN_POINT('Ctrl Pts',(-20.5630361294496,15.5790178341343,123.002216406184)) ;
#19905 = CARTESIAN_POINT('Ctrl Pts',(-20.8514802727897,15.3990287537714,122.899819819407)) ;
#19906 = CARTESIAN_POINT('Ctrl Pts',(-20.633508538707,15.5987750389901,123.416561760013)) ;
#19907 = CARTESIAN_POINT('Ctrl Pts',(-20.939569466923,15.4187859586272,123.417748054594)) ;
#19908 = CARTESIAN_POINT('Ctrl Pts',(-20.5580007528934,15.6188083116358,123.835558911533)) ;
#19909 = CARTESIAN_POINT('Ctrl Pts',(-20.8451846342489,15.4388192312729,123.941494843128)) ;
#19910 = CARTESIAN_POINT('Ctrl Pts',(-20.3461462838386,15.6386212200896,124.199911351364)) ;
#19911 = CARTESIAN_POINT('Ctrl Pts',(-20.5803681949361,15.4586321397268,124.396932991369)) ;
#19912 = CARTESIAN_POINT('Ctrl Pts',(-20.0203388845668,15.6586173662171,124.472784286855)) ;
#19913 = CARTESIAN_POINT('Ctrl Pts',(-20.1731096405733,15.4786282858542,124.738024765008)) ;
#19914 = CARTESIAN_POINT('Ctrl Pts',(-19.6233743789427,15.6784791194396,124.617449122825)) ;
#19915 = CARTESIAN_POINT('Ctrl Pts',(-19.6769061894164,15.4984900390767,124.918856330261)) ;
#19916 = CARTESIAN_POINT('Ctrl Pts',(-19.1967590474696,15.6985476365677,124.617705022532)) ;
#19917 = CARTESIAN_POINT('Ctrl Pts',(-19.1436360482035,15.5185585562048,124.919177517765)) ;
#19918 = CARTESIAN_POINT('Ctrl Pts',(-18.8003320264179,15.7183785095645,124.473760456347)) ;
#19919 = CARTESIAN_POINT('Ctrl Pts',(-18.6481039856445,15.5383894292016,124.739248841471)) ;
#19920 = CARTESIAN_POINT('Ctrl Pts',(-18.4747503929125,15.7383004203812,124.20293742243)) ;
#19921 = CARTESIAN_POINT('Ctrl Pts',(-18.2411262734598,15.5583113400183,124.400722475563)) ;
#19922 = CARTESIAN_POINT('Ctrl Pts',(-18.2610720953533,15.7582298638165,123.836921398904)) ;
#19923 = CARTESIAN_POINT('Ctrl Pts',(-17.9740267390617,15.5782407834536,123.943204335233)) ;
#19924 = CARTESIAN_POINT('Ctrl Pts',(-18.185068198707,15.7781395339329,123.420531358687)) ;
#19925 = CARTESIAN_POINT('Ctrl Pts',(-17.8790194223619,15.59815045357,123.422718308582)) ;
#19926 = CARTESIAN_POINT('Ctrl Pts',(-18.2548638512684,15.7980128911957,123.003722761479)) ;
#19927 = CARTESIAN_POINT('Ctrl Pts',(-17.9662605748662,15.6180238108329,122.901708304058)) ;
#19928 = CARTESIAN_POINT('Ctrl Pts',(-18.4639568410273,15.8180044258137,122.633696412297)) ;
#19929 = CARTESIAN_POINT('Ctrl Pts',(-18.2276238439571,15.6380153454508,122.439173769157)) ;
#19930 = CARTESIAN_POINT('Ctrl Pts',(-18.7847146040937,15.8378700432244,122.358763046612)) ;
#19931 = CARTESIAN_POINT('Ctrl Pts',(-18.6285678009232,15.6578809628615,122.095505124988)) ;
#19932 = CARTESIAN_POINT('Ctrl Pts',(-19.182109206407,15.8578509730526,122.208558793697)) ;
#19933 = CARTESIAN_POINT('Ctrl Pts',(-19.1253095706751,15.6778618926898,121.907746174012)) ;
#19934 = CARTESIAN_POINT('Ctrl Pts',(-19.606033490729,15.8777894351358,122.203463863361)) ;
#19935 = CARTESIAN_POINT('Ctrl Pts',(-19.6552143908038,15.6978003547729,121.901373660419)) ;
#19936 = CARTESIAN_POINT('Ctrl Pts',(-20.0055761170638,15.8976816283575,122.342403399768)) ;
#19937 = CARTESIAN_POINT('Ctrl Pts',(-20.1546433032014,15.7176925479946,122.075043824401)) ;
#19938 = CARTESIAN_POINT('Ctrl Pts',(-20.3347791009066,15.9176523433929,122.61046686242)) ;
#19939 = CARTESIAN_POINT('Ctrl Pts',(-20.5661496331982,15.73766326303,122.410119645807)) ;
#19940 = CARTESIAN_POINT('Ctrl Pts',(-20.551706715397,15.937462015059,122.971635608473)) ;
#19941 = CARTESIAN_POINT('Ctrl Pts',(-20.8373123753955,15.7574729346961,122.861577302707)) ;
#19942 = CARTESIAN_POINT('Ctrl Pts',(-20.6333723481961,15.9574552317502,123.388667733852)) ;
#19943 = CARTESIAN_POINT('Ctrl Pts',(-20.9393997364478,15.7774661513873,123.382866096592)) ;
#19944 = CARTESIAN_POINT('Ctrl Pts',(-20.5685874573327,15.9773061439465,123.805925874308)) ;
#19945 = CARTESIAN_POINT('Ctrl Pts',(-20.8584216081124,15.7973170635836,123.904440437728)) ;
#19946 = CARTESIAN_POINT('Ctrl Pts',(-20.3629339575336,15.9973807502655,124.179831486359)) ;
#19947 = CARTESIAN_POINT('Ctrl Pts',(-20.6013666268889,15.8173916699027,124.371819409561)) ;
#19948 = CARTESIAN_POINT('Ctrl Pts',(-20.0986057487275,16.0138973821489,124.411216269807)) ;
#19949 = CARTESIAN_POINT('Ctrl Pts',(-20.2709357008999,15.833908301786,124.661071335312)) ;
#19950 = CARTESIAN_POINT('Ctrl Pts',(-19.8472305510429,16.027236089843,124.535405517903)) ;
#19951 = CARTESIAN_POINT('Ctrl Pts',(-19.9567400193657,15.8472470094801,124.816295036982)) ;
#19952 = CARTESIAN_POINT('Ctrl Pts',(-19.648689899929,16.0370784641513,124.593781061793)) ;
#19953 = CARTESIAN_POINT('Ctrl Pts',(-19.7085577801769,15.8570893837884,124.889269258747)) ;
#19954 = CARTESIAN_POINT('Ctrl Pts',(-19.4386553018546,16.047133484134,124.61748484339)) ;
#19955 = CARTESIAN_POINT('Ctrl Pts',(-19.4460289923727,15.8671444037711,124.918903925048)) ;
#19956 = CARTESIAN_POINT('Ctrl Pts',(-19.1610280376061,16.0603656407916,124.600218445625)) ;
#19957 = CARTESIAN_POINT('Ctrl Pts',(-19.0989283678214,15.8803765604287,124.897309206157)) ;
#19958 = CARTESIAN_POINT('Ctrl Pts',(-18.825889100884,16.0769806081367,124.488333617129)) ;
#19959 = CARTESIAN_POINT('Ctrl Pts',(-18.680086550223,15.8969915277738,124.757481852894)) ;
#19960 = CARTESIAN_POINT('Ctrl Pts',(-18.5495711916303,16.0935751951479,124.269005818189)) ;
#19961 = CARTESIAN_POINT('Ctrl Pts',(-18.3346327392559,15.913586114785,124.48329340641)) ;
#19962 = CARTESIAN_POINT('Ctrl Pts',(-18.383354158807,16.1068087635033,124.045842736508)) ;
#19963 = CARTESIAN_POINT('Ctrl Pts',(-18.1268897362054,15.9268196831404,124.204366870051)) ;
#19964 = CARTESIAN_POINT('Ctrl Pts',(-18.2885245171761,16.1168523813119,123.857213437139)) ;
#19965 = CARTESIAN_POINT('Ctrl Pts',(-18.0083439444997,15.9368633009491,123.968576154149)) ;
#19966 = CARTESIAN_POINT('Ctrl Pts',(-18.2287506235429,16.1267393055468,123.658118953478)) ;
#19967 = CARTESIAN_POINT('Ctrl Pts',(-17.9336253681816,15.9467502251839,123.719711066793)) ;
#19968 = CARTESIAN_POINT('Ctrl Pts',(-18.2038316638123,16.1367299599936,123.449583936804)) ;
#19969 = CARTESIAN_POINT('Ctrl Pts',(-17.9024744065932,15.9567408796307,123.459039355824)) ;
#19970 = CARTESIAN_POINT('Ctrl Pts',(-18.2155127325471,16.1466917184475,123.240472594879)) ;
#19971 = CARTESIAN_POINT('Ctrl Pts',(-17.9170694041595,15.9667026380847,123.197660756749)) ;
#19972 = CARTESIAN_POINT('Ctrl Pts',(-18.2792368886857,16.1600315835148,122.967353209043)) ;
#19973 = CARTESIAN_POINT('Ctrl Pts',(-17.9967391763496,15.9800425031519,122.856207482281)) ;
#19974 = CARTESIAN_POINT('Ctrl Pts',(-18.41302923077,16.1733403664281,122.718017566954)) ;
#19975 = CARTESIAN_POINT('Ctrl Pts',(-18.1639736695918,15.9933512860652,122.544568270991)) ;
#19976 = CARTESIAN_POINT('Ctrl Pts',(-18.6026009651151,16.1865361238721,122.515452306746)) ;
#19977 = CARTESIAN_POINT('Ctrl Pts',(-18.4009205226991,16.0065470435093,122.291373958012)) ;
#19978 = CARTESIAN_POINT('Ctrl Pts',(-18.7697316480871,16.1964980075486,122.389244608376)) ;
#19979 = CARTESIAN_POINT('Ctrl Pts',(-18.6098352782094,16.0165089271858,122.133609050801)) ;
#19980 = CARTESIAN_POINT('Ctrl Pts',(-18.9579132109796,16.2065411170633,122.293505577334)) ;
#19981 = CARTESIAN_POINT('Ctrl Pts',(-18.8450601920169,16.0265520367004,122.013933523829)) ;
#19982 = CARTESIAN_POINT('Ctrl Pts',(-19.1559583596013,16.2163933670625,122.232828073835)) ;
#19983 = CARTESIAN_POINT('Ctrl Pts',(-19.0926161288735,16.0364042866996,121.938083702946)) ;
#19984 = CARTESIAN_POINT('Ctrl Pts',(-19.3639266023041,16.226364904013,122.20664426832)) ;
#19985 = CARTESIAN_POINT('Ctrl Pts',(-19.3525761374353,16.0463758236501,121.90535120371)) ;
#19986 = CARTESIAN_POINT('Ctrl Pts',(-19.5738352772956,16.2363601694905,122.217013254614)) ;
#19987 = CARTESIAN_POINT('Ctrl Pts',(-19.6149622143192,16.0563710891276,121.918309627861)) ;
#19988 = CARTESIAN_POINT('Ctrl Pts',(-19.7794415898056,16.2463941423641,122.264093918599)) ;
#19989 = CARTESIAN_POINT('Ctrl Pts',(-19.8719707676213,16.0664050620013,121.977157725234)) ;
#19990 = CARTESIAN_POINT('Ctrl Pts',(-19.9704548769762,16.2562495571265,122.344410165683)) ;
#19991 = CARTESIAN_POINT('Ctrl Pts',(-20.1107386746183,16.0762604767636,122.077550542983)) ;
#19992 = CARTESIAN_POINT('Ctrl Pts',(-20.1472714092236,16.2662488346353,122.458039635008)) ;
#19993 = CARTESIAN_POINT('Ctrl Pts',(-20.3317609231274,16.0862597542724,122.219585083318)) ;
#19994 = CARTESIAN_POINT('Ctrl Pts',(-20.3002692337498,16.2761440187983,122.599043469478)) ;
#19995 = CARTESIAN_POINT('Ctrl Pts',(-20.5230102658078,16.0961549384354,122.395838020282)) ;
#19996 = CARTESIAN_POINT('Ctrl Pts',(-20.4285086882037,16.2862043984391,122.767195696691)) ;
#19997 = CARTESIAN_POINT('Ctrl Pts',(-20.6833117694189,16.1062153180762,122.606026601043)) ;
#19998 = CARTESIAN_POINT('Ctrl Pts',(-20.5237070485476,16.2960542674472,122.951113827602)) ;
#19999 = CARTESIAN_POINT('Ctrl Pts',(-20.8023123453152,16.1160651870843,122.835923343469)) ;
#20000 = CARTESIAN_POINT('Ctrl Pts',(-20.5871150710927,16.3060858286551,123.152237015231)) ;
#20001 = CARTESIAN_POINT('Ctrl Pts',(-20.8815749658397,16.1260967482922,123.087326542233)) ;
#20002 = CARTESIAN_POINT('Ctrl Pts',(-20.6141638262457,16.3160962775374,123.360962196681)) ;
#20003 = CARTESIAN_POINT('Ctrl Pts',(-20.9153886455586,16.1361071971745,123.3482327168)) ;
#20004 = CARTESIAN_POINT('Ctrl Pts',(-20.6048907446535,16.3260030169544,123.569019571295)) ;
#20005 = CARTESIAN_POINT('Ctrl Pts',(-20.9038000062041,16.1460139365915,123.608304860459)) ;
#20006 = CARTESIAN_POINT('Ctrl Pts',(-20.5598881669259,16.3359410330228,123.773031366739)) ;
#20007 = CARTESIAN_POINT('Ctrl Pts',(-20.8475493442764,16.1559519526599,123.863320444448)) ;
#20008 = CARTESIAN_POINT('Ctrl Pts',(-20.4797215293116,16.3459462794739,123.967521538131)) ;
#20009 = CARTESIAN_POINT('Ctrl Pts',(-20.7473434745622,16.1659571991111,124.106434248665)) ;
#20010 = CARTESIAN_POINT('Ctrl Pts',(-20.3663921716625,16.3559803405302,124.145428527425)) ;
#20011 = CARTESIAN_POINT('Ctrl Pts',(-20.6056840713685,16.1759912601674,124.328819428175)) ;
#20012 = CARTESIAN_POINT('Ctrl Pts',(-20.2268261020098,16.3658254215884,124.29828451982)) ;
#20013 = CARTESIAN_POINT('Ctrl Pts',(-20.4312280688443,16.1858363412255,124.519891626386)) ;
#20014 = CARTESIAN_POINT('Ctrl Pts',(-20.0607710857715,16.3758112275419,124.42667346357)) ;
#20015 = CARTESIAN_POINT('Ctrl Pts',(-20.2236607634961,16.195822147179,124.680379963816)) ;
#20016 = CARTESIAN_POINT('Ctrl Pts',(-19.8759009892187,16.3857460480961,124.523947203319)) ;
#20017 = CARTESIAN_POINT('Ctrl Pts',(-19.9925740517516,16.2057569677332,124.801974564811)) ;
#20018 = CARTESIAN_POINT('Ctrl Pts',(-19.6745001645774,16.3958035732283,124.588229437951)) ;
#20019 = CARTESIAN_POINT('Ctrl Pts',(-19.7408239243177,16.2158144928654,124.88232980859)) ;
#20020 = CARTESIAN_POINT('Ctrl Pts',(-19.4699018787836,16.4056252238796,124.616221674398)) ;
#20021 = CARTESIAN_POINT('Ctrl Pts',(-19.4850756391553,16.2256361435168,124.917322735119)) ;
#20022 = CARTESIAN_POINT('Ctrl Pts',(-19.2586509012011,16.4156812873844,124.608469860798)) ;
#20023 = CARTESIAN_POINT('Ctrl Pts',(-19.2210119356238,16.2356922070215,124.90763544783)) ;
#20024 = CARTESIAN_POINT('Ctrl Pts',(-19.0543812444969,16.4256219544483,124.56429049855)) ;
#20025 = CARTESIAN_POINT('Ctrl Pts',(-18.965674000184,16.2456328740854,124.852413667813)) ;
#20026 = CARTESIAN_POINT('Ctrl Pts',(-18.861349537296,16.4355263481143,124.486210004502)) ;
#20027 = CARTESIAN_POINT('Ctrl Pts',(-18.7243829673979,16.2555372677514,124.754815092852)) ;
#20028 = CARTESIAN_POINT('Ctrl Pts',(-18.6823656137702,16.4455728718773,124.374110855955)) ;
#20029 = CARTESIAN_POINT('Ctrl Pts',(-18.5006518515227,16.2655837915144,124.614693286642)) ;
#20030 = CARTESIAN_POINT('Ctrl Pts',(-18.5277366886048,16.4554689548937,124.234866899934)) ;
#20031 = CARTESIAN_POINT('Ctrl Pts',(-18.3073636533246,16.2754798745308,124.440639733717)) ;
#20032 = CARTESIAN_POINT('Ctrl Pts',(-18.397512504775,16.4655356541237,124.068090149014)) ;
#20033 = CARTESIAN_POINT('Ctrl Pts',(-18.1445816442607,16.2855465737608,124.232170442766)) ;
#20034 = CARTESIAN_POINT('Ctrl Pts',(-18.3003784994557,16.4753592645248,123.885799724295)) ;
#20035 = CARTESIAN_POINT('Ctrl Pts',(-18.0231616074987,16.2953701841619,124.004307681981)) ;
#20036 = CARTESIAN_POINT('Ctrl Pts',(-18.2345231615704,16.4854151247023,123.684941160413)) ;
#20037 = CARTESIAN_POINT('Ctrl Pts',(-17.9408403240638,16.3054260443394,123.753235338654)) ;
#20038 = CARTESIAN_POINT('Ctrl Pts',(-18.2051689662618,16.4953482710072,123.478162940321)) ;
#20039 = CARTESIAN_POINT('Ctrl Pts',(-17.904145201317,16.3153591906443,123.494762458891)) ;
#20040 = CARTESIAN_POINT('Ctrl Pts',(-18.2117436428783,16.5052935267778,123.269210161589)) ;
#20041 = CARTESIAN_POINT('Ctrl Pts',(-17.9123613233359,16.3253044464149,123.233570994404)) ;
#20042 = CARTESIAN_POINT('Ctrl Pts',(-18.2545082390918,16.5152768252163,123.063705916951)) ;
#20043 = CARTESIAN_POINT('Ctrl Pts',(-17.9658149650056,16.3352877448534,122.976690048544)) ;
#20044 = CARTESIAN_POINT('Ctrl Pts',(-18.3329769113409,16.5253140053629,122.867842390834)) ;
#20045 = CARTESIAN_POINT('Ctrl Pts',(-18.0638986666255,16.345324925,122.731859880856)) ;
#20046 = CARTESIAN_POINT('Ctrl Pts',(-18.4419820599427,16.5351685580724,122.691641388023)) ;
#20047 = CARTESIAN_POINT('Ctrl Pts',(-18.2001537297579,16.3551794777095,122.511606700127)) ;
#20048 = CARTESIAN_POINT('Ctrl Pts',(-18.581699061968,16.5451680765197,122.534616193338)) ;
#20049 = CARTESIAN_POINT('Ctrl Pts',(-18.3747984971053,16.3651789961568,122.315323705892)) ;
#20050 = CARTESIAN_POINT('Ctrl Pts',(-18.7447549291817,16.5550631589818,122.405380089369)) ;
#20051 = CARTESIAN_POINT('Ctrl Pts',(-18.5786176379803,16.3750740786189,122.153776522294)) ;
#20052 = CARTESIAN_POINT('Ctrl Pts',(-18.9307890892371,16.5651237044879,122.304812169695)) ;
#20053 = CARTESIAN_POINT('Ctrl Pts',(-18.8111591522696,16.385134624125,122.028064933009)) ;
#20054 = CARTESIAN_POINT('Ctrl Pts',(-19.1272493004739,16.5749730117359,122.239351514005)) ;
#20055 = CARTESIAN_POINT('Ctrl Pts',(-19.0567347651697,16.394983931373,121.946236873333)) ;
#20056 = CARTESIAN_POINT('Ctrl Pts',(-19.3356895472675,16.5850001018232,122.207921910754)) ;
#20057 = CARTESIAN_POINT('Ctrl Pts',(-19.3172847594668,16.4050110214604,121.906948036796)) ;
#20058 = CARTESIAN_POINT('Ctrl Pts',(-19.5464580747962,16.5950290059602,122.213723078869)) ;
#20059 = CARTESIAN_POINT('Ctrl Pts',(-19.5807454043777,16.4150399255973,121.91419747043)) ;
#20060 = CARTESIAN_POINT('Ctrl Pts',(-19.7492714933066,16.6048728710595,122.254846303391)) ;
#20061 = CARTESIAN_POINT('Ctrl Pts',(-19.8342636546748,16.4248837906966,121.965599859095)) ;
#20062 = CARTESIAN_POINT('Ctrl Pts',(-19.9450340387056,16.6148686977679,122.331249053741)) ;
#20063 = CARTESIAN_POINT('Ctrl Pts',(-20.0789676317228,16.434879617405,122.0611017389)) ;
#20064 = CARTESIAN_POINT('Ctrl Pts',(-20.1248865780728,16.6248939144169,122.441136839792)) ;
#20065 = CARTESIAN_POINT('Ctrl Pts',(-20.3037842341569,16.444904834054,122.198459857618)) ;
#20066 = CARTESIAN_POINT('Ctrl Pts',(-20.28097718897,16.6347837465745,122.57849001676)) ;
#20067 = CARTESIAN_POINT('Ctrl Pts',(-20.4988993121104,16.4547946662116,122.370150559373)) ;
#20068 = CARTESIAN_POINT('Ctrl Pts',(-20.4123923595961,16.6447746026592,122.742330187419)) ;
#20069 = CARTESIAN_POINT('Ctrl Pts',(-20.6631697043296,16.4647855222963,122.574949866266)) ;
#20070 = CARTESIAN_POINT('Ctrl Pts',(-20.5128694027826,16.6547196972521,122.925680754585)) ;
#20071 = CARTESIAN_POINT('Ctrl Pts',(-20.7887677400445,16.4747306168892,122.804137700936)) ;
#20072 = CARTESIAN_POINT('Ctrl Pts',(-20.5804045472884,16.6646716010202,123.12370981409)) ;
#20073 = CARTESIAN_POINT('Ctrl Pts',(-20.8731883104183,16.4846825206573,123.051673973059)) ;
#20074 = CARTESIAN_POINT('Ctrl Pts',(-20.6126176827345,16.6747080004896,123.332227708226)) ;
#20075 = CARTESIAN_POINT('Ctrl Pts',(-20.9134563188917,16.4947189201267,123.312320962728)) ;
#20076 = CARTESIAN_POINT('Ctrl Pts',(-20.6083540179915,16.6845970705783,123.540090086078)) ;
#20077 = CARTESIAN_POINT('Ctrl Pts',(-20.9081282976239,16.5046079902154,123.572149884728)) ;
#20078 = CARTESIAN_POINT('Ctrl Pts',(-20.5680279223368,16.6945863599492,123.746183169029)) ;
#20079 = CARTESIAN_POINT('Ctrl Pts',(-20.8577220598271,16.5145972795863,123.829766727629)) ;
#20080 = CARTESIAN_POINT('Ctrl Pts',(-20.4926169706463,16.7045449261589,123.941483709514)) ;
#20081 = CARTESIAN_POINT('Ctrl Pts',(-20.76345961891,16.524555845796,124.073893348995)) ;
#20082 = CARTESIAN_POINT('Ctrl Pts',(-20.3855116246943,16.7144444973757,124.119942910735)) ;
#20083 = CARTESIAN_POINT('Ctrl Pts',(-20.6295786198911,16.5344554170128,124.296968784774)) ;
#20084 = CARTESIAN_POINT('Ctrl Pts',(-20.2469681262543,16.7244924117899,124.279374314369)) ;
#20085 = CARTESIAN_POINT('Ctrl Pts',(-20.4564004098396,16.5445033314271,124.49625876178)) ;
#20086 = CARTESIAN_POINT('Ctrl Pts',(-20.0853998211911,16.7343877546505,124.410470530884)) ;
#20087 = CARTESIAN_POINT('Ctrl Pts',(-20.254440134761,16.5543986742876,124.660130610446)) ;
#20088 = CARTESIAN_POINT('Ctrl Pts',(-19.9005296097113,16.7444494485979,124.513218405503)) ;
#20089 = CARTESIAN_POINT('Ctrl Pts',(-20.0233532789183,16.5644603682351,124.788566418278)) ;
#20090 = CARTESIAN_POINT('Ctrl Pts',(-19.7049244472247,16.7542939016821,124.580859195891)) ;
#20091 = CARTESIAN_POINT('Ctrl Pts',(-19.7788459931032,16.5743048213192,124.873119039239)) ;
#20092 = CARTESIAN_POINT('Ctrl Pts',(-19.4982683090675,16.7642545866405,124.614617061562)) ;
#20093 = CARTESIAN_POINT('Ctrl Pts',(-19.5205255375102,16.5842655062777,124.915317433973)) ;
#20094 = CARTESIAN_POINT('Ctrl Pts',(-19.2872959543148,16.7742905191491,124.611604709264)) ;
#20095 = CARTESIAN_POINT('Ctrl Pts',(-19.2568102129339,16.5943014387862,124.911553126493)) ;
#20096 = CARTESIAN_POINT('Ctrl Pts',(-19.083065641411,16.7841791348371,124.572793885594)) ;
#20097 = CARTESIAN_POINT('Ctrl Pts',(-19.0015211293968,16.6041900544743,124.863040443295)) ;
#20098 = CARTESIAN_POINT('Ctrl Pts',(-18.8860375470221,16.7941935439796,124.498559615146)) ;
#20099 = CARTESIAN_POINT('Ctrl Pts',(-18.7552356821971,16.6142044636167,124.770248444018)) ;
#20100 = CARTESIAN_POINT('Ctrl Pts',(-18.7048442029777,16.8042273529374,124.390576815252)) ;
#20101 = CARTESIAN_POINT('Ctrl Pts',(-18.5287435554736,16.6242382725745,124.635270964711)) ;
#20102 = CARTESIAN_POINT('Ctrl Pts',(-18.5479851568458,16.8140578071936,124.255979370359)) ;
#20103 = CARTESIAN_POINT('Ctrl Pts',(-18.3326680459431,16.6340687268307,124.467023867572)) ;
#20104 = CARTESIAN_POINT('Ctrl Pts',(-18.4135706987232,16.8241354747718,124.092266151809)) ;
#20105 = CARTESIAN_POINT('Ctrl Pts',(-18.164649593129,16.6441463944089,124.262383242805)) ;
#20106 = CARTESIAN_POINT('Ctrl Pts',(-18.3118178527469,16.833987342894,123.911815748702)) ;
#20107 = CARTESIAN_POINT('Ctrl Pts',(-18.037457177748,16.6539982625311,124.03681949593)) ;
#20108 = CARTESIAN_POINT('Ctrl Pts',(-18.2412580423385,16.8440603804594,123.712187854895)) ;
#20109 = CARTESIAN_POINT('Ctrl Pts',(-17.949256848314,16.6640713000965,123.787285292001)) ;
#20110 = CARTESIAN_POINT('Ctrl Pts',(-18.2072505630093,16.8539029338102,123.508062557237)) ;
#20111 = CARTESIAN_POINT('Ctrl Pts',(-17.9067465102641,16.6739138534474,123.53212739955)) ;
#20112 = CARTESIAN_POINT('Ctrl Pts',(-18.2085239591176,16.8638833293037,123.298256187537)) ;
#20113 = CARTESIAN_POINT('Ctrl Pts',(-17.908337764321,16.6838942489408,123.269869124294)) ;
#20114 = CARTESIAN_POINT('Ctrl Pts',(-18.2467556082462,16.8739018072815,123.091139951509)) ;
#20115 = CARTESIAN_POINT('Ctrl Pts',(-17.9561266808866,16.6939127269186,123.010973721011)) ;
#20116 = CARTESIAN_POINT('Ctrl Pts',(-18.3189697446899,16.8837851215876,122.896288022926)) ;
#20117 = CARTESIAN_POINT('Ctrl Pts',(-18.046394284067,16.7037960412247,122.767407615452)) ;
#20118 = CARTESIAN_POINT('Ctrl Pts',(-18.425934681268,16.8938534241263,122.713676624745)) ;
#20119 = CARTESIAN_POINT('Ctrl Pts',(-18.1800998015951,16.7138643437634,122.539143460683)) ;
#20120 = CARTESIAN_POINT('Ctrl Pts',(-18.5595970562926,16.9036834713997,122.556016451482)) ;
#20121 = CARTESIAN_POINT('Ctrl Pts',(-18.3471784469217,16.7236943910368,122.342066798614)) ;
#20122 = CARTESIAN_POINT('Ctrl Pts',(-18.722208363347,16.9137503428152,122.42061719112)) ;
#20123 = CARTESIAN_POINT('Ctrl Pts',(-18.5504420735912,16.7337612624523,122.172817736648)) ;
#20124 = CARTESIAN_POINT('Ctrl Pts',(-18.9027264908965,16.9236393816143,122.317430530049)) ;
#20125 = CARTESIAN_POINT('Ctrl Pts',(-18.7760904676618,16.7436503012514,122.043833574538)) ;
#20126 = CARTESIAN_POINT('Ctrl Pts',(-19.1003612730022,16.9336360797484,122.246020456028)) ;
#20127 = CARTESIAN_POINT('Ctrl Pts',(-19.0231340623094,16.7536469993855,121.95457073187)) ;
#20128 = CARTESIAN_POINT('Ctrl Pts',(-19.3065267658046,16.9435885054603,122.210251377386)) ;
#20129 = CARTESIAN_POINT('Ctrl Pts',(-19.2808414151497,16.7635994250975,121.909859064209)) ;
#20130 = CARTESIAN_POINT('Ctrl Pts',(-19.5155081682475,16.9535298076933,122.210531944557)) ;
#20131 = CARTESIAN_POINT('Ctrl Pts',(-19.5420687997964,16.7735407273304,121.910209653822)) ;
#20132 = CARTESIAN_POINT('Ctrl Pts',(-19.7222133629213,16.9635130467772,122.24703377313)) ;
#20133 = CARTESIAN_POINT('Ctrl Pts',(-19.8004505578449,16.7835239664143,121.955836958364)) ;
#20134 = CARTESIAN_POINT('Ctrl Pts',(-19.9203861587656,16.9735518483458,122.319565863544)) ;
#20135 = CARTESIAN_POINT('Ctrl Pts',(-20.0481664431086,16.7935627679829,122.04650185724)) ;
#20136 = CARTESIAN_POINT('Ctrl Pts',(-20.0997203161893,16.9833999544674,122.423063092642)) ;
#20137 = CARTESIAN_POINT('Ctrl Pts',(-20.27233537467,16.8034108741046,122.175874106053)) ;
#20138 = CARTESIAN_POINT('Ctrl Pts',(-20.2618757976447,16.9934601500428,122.558817396899)) ;
#20139 = CARTESIAN_POINT('Ctrl Pts',(-20.4750293998556,16.8134710696799,122.345566817946)) ;
#20140 = CARTESIAN_POINT('Ctrl Pts',(-20.3956688355369,17.0033578333542,122.718192247894)) ;
#20141 = CARTESIAN_POINT('Ctrl Pts',(-20.6422713390571,16.8233687529913,122.544786148084)) ;
#20142 = CARTESIAN_POINT('Ctrl Pts',(-20.5006942150535,17.0132888737282,122.898630233536)) ;
#20143 = CARTESIAN_POINT('Ctrl Pts',(-20.7735531876702,16.8332997933653,122.770334392659)) ;
#20144 = CARTESIAN_POINT('Ctrl Pts',(-20.5733879414346,17.0233310913848,123.096836226167)) ;
#20145 = CARTESIAN_POINT('Ctrl Pts',(-20.864420100794,16.8433420110219,123.018091751125)) ;
#20146 = CARTESIAN_POINT('Ctrl Pts',(-20.61013604455,17.0332177521188,123.301420117355)) ;
#20147 = CARTESIAN_POINT('Ctrl Pts',(-20.9103551819919,16.8532286717559,123.273822728003)) ;
#20148 = CARTESIAN_POINT('Ctrl Pts',(-20.6111628873651,17.0432108607212,123.511493426387)) ;
#20149 = CARTESIAN_POINT('Ctrl Pts',(-20.9116383536201,16.8632217803584,123.536414570098)) ;
#20150 = CARTESIAN_POINT('Ctrl Pts',(-20.5757869989794,17.0531565593595,123.717568908306)) ;
#20151 = CARTESIAN_POINT('Ctrl Pts',(-20.8674180471858,16.8731674789966,123.794009449891)) ;
#20152 = CARTESIAN_POINT('Ctrl Pts',(-20.5055557491606,17.0631037816305,123.91455588214)) ;
#20153 = CARTESIAN_POINT('Ctrl Pts',(-20.7796283027966,16.8831147012677,124.04024353424)) ;
#20154 = CARTESIAN_POINT('Ctrl Pts',(-20.400941475518,17.0731518072107,124.098065903988)) ;
#20155 = CARTESIAN_POINT('Ctrl Pts',(-20.6488602156385,16.8931627268478,124.269630633099)) ;
#20156 = CARTESIAN_POINT('Ctrl Pts',(-20.2688802244909,17.0829990543536,124.257492396339)) ;
#20157 = CARTESIAN_POINT('Ctrl Pts',(-20.4837823786232,16.9030099739907,124.468914512535)) ;
#20158 = CARTESIAN_POINT('Ctrl Pts',(-20.1097187274717,17.0929622314443,124.39364708618)) ;
#20159 = CARTESIAN_POINT('Ctrl Pts',(-20.2848296697992,16.9129731510814,124.639107596571)) ;
#20160 = CARTESIAN_POINT('Ctrl Pts',(-19.9279652479733,17.1029919524777,124.500535991782)) ;
#20161 = CARTESIAN_POINT('Ctrl Pts',(-20.0576375877666,16.9230028721148,124.772718133945)) ;
#20162 = CARTESIAN_POINT('Ctrl Pts',(-19.7329501884367,17.1128964200106,124.573568512816)) ;
#20163 = CARTESIAN_POINT('Ctrl Pts',(-19.8138676646833,16.9329073396477,124.864008421836)) ;
#20164 = CARTESIAN_POINT('Ctrl Pts',(-19.5257911753333,17.1229209058404,124.612154491612)) ;
#20165 = CARTESIAN_POINT('Ctrl Pts',(-19.5549188176407,16.9429318254775,124.912240141092)) ;
#20166 = CARTESIAN_POINT('Ctrl Pts',(-19.31756391383,17.1328247409643,124.61433347866)) ;
#20167 = CARTESIAN_POINT('Ctrl Pts',(-19.2946338276999,16.9528356606014,124.914963066489)) ;
#20168 = CARTESIAN_POINT('Ctrl Pts',(-19.1091090081414,17.1428759316743,124.579872920246)) ;
#20169 = CARTESIAN_POINT('Ctrl Pts',(-19.0340655773043,16.9628868513114,124.871886584455)) ;
#20170 = CARTESIAN_POINT('Ctrl Pts',(-18.9130563367156,17.1527603743326,124.510927123554)) ;
#20171 = CARTESIAN_POINT('Ctrl Pts',(-18.7889990253017,16.9727712939697,124.785703184415)) ;
#20172 = CARTESIAN_POINT('Ctrl Pts',(-18.7298067492815,17.1627533821844,124.408227429551)) ;
#20173 = CARTESIAN_POINT('Ctrl Pts',(-18.5599373549121,16.9827643018216,124.657327597577)) ;
#20174 = CARTESIAN_POINT('Ctrl Pts',(-18.5679203831117,17.1727017019007,124.275788607794)) ;
#20175 = CARTESIAN_POINT('Ctrl Pts',(-18.3575795915092,16.9927126215379,124.491777975001)) ;
#20176 = CARTESIAN_POINT('Ctrl Pts',(-18.4314404984795,17.1826385406102,124.117654900574)) ;
#20177 = CARTESIAN_POINT('Ctrl Pts',(-18.186980138861,17.0026494602473,124.294109650112)) ;
#20178 = CARTESIAN_POINT('Ctrl Pts',(-18.3237434951537,17.1926215295298,123.937489058372)) ;
#20179 = CARTESIAN_POINT('Ctrl Pts',(-18.0523597654586,17.0126324491669,124.06890152174)) ;
#20180 = CARTESIAN_POINT('Ctrl Pts',(-18.2488910018654,17.2026654088939,123.740073906393)) ;
#20181 = CARTESIAN_POINT('Ctrl Pts',(-17.9587951854769,17.022676328531,123.82213239202)) ;
#20182 = CARTESIAN_POINT('Ctrl Pts',(-18.2098074279025,17.2124934742523,123.537154265796)) ;
#20183 = CARTESIAN_POINT('Ctrl Pts',(-17.9099416408422,17.0325043938894,123.568481191394)) ;
#20184 = CARTESIAN_POINT('Ctrl Pts',(-18.2063795196312,17.2225705628072,123.325376725486)) ;
#20185 = CARTESIAN_POINT('Ctrl Pts',(-17.9056580144789,17.0425814824443,123.303759681484)) ;
#20186 = CARTESIAN_POINT('Ctrl Pts',(-18.2389039387934,17.2324207149635,123.120811528731)) ;
#20187 = CARTESIAN_POINT('Ctrl Pts',(-17.9463150166963,17.0524316346006,123.048052157451)) ;
#20188 = CARTESIAN_POINT('Ctrl Pts',(-18.3079172661289,17.2425011954158,122.920496194751)) ;
#20189 = CARTESIAN_POINT('Ctrl Pts',(-18.032582786432,17.062512115053,122.797658849589)) ;
#20190 = CARTESIAN_POINT('Ctrl Pts',(-18.4078418322244,17.2523156931847,122.739922505072)) ;
#20191 = CARTESIAN_POINT('Ctrl Pts',(-18.1574904407852,17.0723266128218,122.571941098829)) ;
#20192 = CARTESIAN_POINT('Ctrl Pts',(-18.5406376489348,17.2623839892048,122.575157598147)) ;
#20193 = CARTESIAN_POINT('Ctrl Pts',(-18.3234861663821,17.0823949088419,122.36598619016)) ;
#20194 = CARTESIAN_POINT('Ctrl Pts',(-18.6974563857139,17.2722828216876,122.43827365892)) ;
#20195 = CARTESIAN_POINT('Ctrl Pts',(-18.5195111943069,17.0922937413247,122.194881832912)) ;
#20196 = CARTESIAN_POINT('Ctrl Pts',(-18.878314400253,17.2823357017021,122.329011502217)) ;
#20197 = CARTESIAN_POINT('Ctrl Pts',(-18.7455842875903,17.1023466213392,122.058305557914)) ;
#20198 = CARTESIAN_POINT('Ctrl Pts',(-19.0718160918219,17.2922055171983,122.253987097039)) ;
#20199 = CARTESIAN_POINT('Ctrl Pts',(-18.9874629412991,17.1122164368354,121.964526142813)) ;
#20200 = CARTESIAN_POINT('Ctrl Pts',(-19.2795008716947,17.3022781982811,122.212830255507)) ;
#20201 = CARTESIAN_POINT('Ctrl Pts',(-19.2470688770235,17.1222891179182,121.913081725806)) ;
#20202 = CARTESIAN_POINT('Ctrl Pts',(-19.4861827851385,17.312110676852,122.208383210554)) ;
#20203 = CARTESIAN_POINT('Ctrl Pts',(-19.505422587486,17.1321215964892,121.907524515032)) ;
#20204 = CARTESIAN_POINT('Ctrl Pts',(-19.6946785789896,17.3221413108381,122.23992020577)) ;
#20205 = CARTESIAN_POINT('Ctrl Pts',(-19.7660419704814,17.1421522304753,121.946947546496)) ;
#20206 = CARTESIAN_POINT('Ctrl Pts',(-19.8943714717527,17.3321728680573,122.307777090262)) ;
#20207 = CARTESIAN_POINT('Ctrl Pts',(-20.0156574864725,17.1521837876944,122.031770159067)) ;
#20208 = CARTESIAN_POINT('Ctrl Pts',(-20.0757133418564,17.342002576929,122.406842625941)) ;
#20209 = CARTESIAN_POINT('Ctrl Pts',(-20.2423350956265,17.1620134965661,122.155604235088)) ;
#20210 = CARTESIAN_POINT('Ctrl Pts',(-20.2401293619726,17.3519920257311,122.53751027012)) ;
#20211 = CARTESIAN_POINT('Ctrl Pts',(-20.4478540416198,17.1720029453682,122.318940433098)) ;
#20212 = CARTESIAN_POINT('Ctrl Pts',(-20.3797110879383,17.3620358781311,122.695945873639)) ;
#20213 = CARTESIAN_POINT('Ctrl Pts',(-20.6223297569369,17.1820467977682,122.516986010216)) ;
#20214 = CARTESIAN_POINT('Ctrl Pts',(-20.4875963394876,17.3718575914632,122.872002282074)) ;
#20215 = CARTESIAN_POINT('Ctrl Pts',(-20.7571853342976,17.1918685111003,122.737058592109)) ;
#20216 = CARTESIAN_POINT('Ctrl Pts',(-20.565398754166,17.3818925964519,123.068098579527)) ;
#20217 = CARTESIAN_POINT('Ctrl Pts',(-20.8544363834582,17.201903516089,122.982179630652)) ;
#20218 = CARTESIAN_POINT('Ctrl Pts',(-20.6073560537494,17.3919174348995,123.274640875661)) ;
#20219 = CARTESIAN_POINT('Ctrl Pts',(-20.9068811373926,17.2119283545366,123.240357855693)) ;
#20220 = CARTESIAN_POINT('Ctrl Pts',(-20.6131626095599,17.4017696478547,123.481683897343)) ;
#20221 = CARTESIAN_POINT('Ctrl Pts',(-20.9141373279082,17.2217805674918,123.499162698651)) ;
#20222 = CARTESIAN_POINT('Ctrl Pts',(-20.5828638631299,17.4117596040485,123.689490947812)) ;
#20223 = CARTESIAN_POINT('Ctrl Pts',(-20.8762617532287,17.2317705236856,123.758921385039)) ;
#20224 = CARTESIAN_POINT('Ctrl Pts',(-20.5173607069601,17.4216877143317,123.887673199299)) ;
#20225 = CARTESIAN_POINT('Ctrl Pts',(-20.7943806135892,17.2416986339689,124.006649024893)) ;
#20226 = CARTESIAN_POINT('Ctrl Pts',(-20.4181341555085,17.4316763144113,124.072748693797)) ;
#20227 = CARTESIAN_POINT('Ctrl Pts',(-20.670345385213,17.2516872340484,124.237992487124)) ;
#20228 = CARTESIAN_POINT('Ctrl Pts',(-20.2875580116088,17.4417029063388,124.238230031649)) ;
#20229 = CARTESIAN_POINT('Ctrl Pts',(-20.5071235397933,17.2617138259759,124.444842800166)) ;
#20230 = CARTESIAN_POINT('Ctrl Pts',(-20.1326042864627,17.451588034403,124.376702910318)) ;
#20231 = CARTESIAN_POINT('Ctrl Pts',(-20.3134293623449,17.2715989540401,124.617932746978)) ;
#20232 = CARTESIAN_POINT('Ctrl Pts',(-19.9543077801982,17.4615791518765,124.487754355148)) ;
#20233 = CARTESIAN_POINT('Ctrl Pts',(-20.0905573668405,17.2815900715136,124.756745161351)) ;
#20234 = CARTESIAN_POINT('Ctrl Pts',(-19.7583141539382,17.4716197677283,124.566132788164)) ;
#20235 = CARTESIAN_POINT('Ctrl Pts',(-19.8455645964301,17.2916306873654,124.854716110604)) ;
#20236 = CARTESIAN_POINT('Ctrl Pts',(-19.5560340189507,17.481452758582,124.608731196182)) ;
#20237 = CARTESIAN_POINT('Ctrl Pts',(-19.5927130154484,17.3014636782191,124.907962066392)) ;
#20238 = CARTESIAN_POINT('Ctrl Pts',(-19.3460857373288,17.4914458900323,124.61627350105)) ;
#20239 = CARTESIAN_POINT('Ctrl Pts',(-19.330277450202,17.3114568096694,124.917387511024)) ;
#20240 = CARTESIAN_POINT('Ctrl Pts',(-19.1372544365684,17.5014779384677,124.586697623401)) ;
#20241 = CARTESIAN_POINT('Ctrl Pts',(-19.0692386893252,17.3214888581048,124.88041535309)) ;
#20242 = CARTESIAN_POINT('Ctrl Pts',(-18.9400052555549,17.5113431850101,124.522647715946)) ;
#20243 = CARTESIAN_POINT('Ctrl Pts',(-18.822677257513,17.3313541046472,124.800350459875)) ;
#20244 = CARTESIAN_POINT('Ctrl Pts',(-18.7547863337693,17.5213050598369,124.424885268183)) ;
#20245 = CARTESIAN_POINT('Ctrl Pts',(-18.5911545600622,17.341315979474,124.678145049276)) ;
#20246 = CARTESIAN_POINT('Ctrl Pts',(-18.5883681930039,17.5313400229482,124.295243637519)) ;
#20247 = CARTESIAN_POINT('Ctrl Pts',(-18.38313341919,17.3513509425853,124.516091097511)) ;
#20248 = CARTESIAN_POINT('Ctrl Pts',(-18.4488134106994,17.5412248674106,124.141223324118)) ;
#20249 = CARTESIAN_POINT('Ctrl Pts',(-18.2086914290502,17.3612357870477,124.323563591818)) ;
#20250 = CARTESIAN_POINT('Ctrl Pts',(-18.3361743130609,17.5512909202513,123.962114608032)) ;
#20251 = CARTESIAN_POINT('Ctrl Pts',(-18.0678947666769,17.3713018398884,124.099676485538)) ;
#20252 = CARTESIAN_POINT('Ctrl Pts',(-18.2579149300862,17.5611284361603,123.770636276305)) ;
#20253 = CARTESIAN_POINT('Ctrl Pts',(-17.9700726313909,17.3811393557974,123.860326944384)) ;
#20254 = CARTESIAN_POINT('Ctrl Pts',(-18.2128572603931,17.5711971842692,123.563847910291)) ;
#20255 = CARTESIAN_POINT('Ctrl Pts',(-17.9137531151006,17.3912081039063,123.601841075206)) ;
#20256 = CARTESIAN_POINT('Ctrl Pts',(-18.2046218359309,17.5810777013002,123.356259866829)) ;
#20257 = CARTESIAN_POINT('Ctrl Pts',(-17.9034613928053,17.4010886209373,123.342355402501)) ;
#20258 = CARTESIAN_POINT('Ctrl Pts',(-18.2324382002903,17.5910688882346,123.148094680984)) ;
#20259 = CARTESIAN_POINT('Ctrl Pts',(-17.9382344928248,17.4110798078718,123.082149155382)) ;
#20260 = CARTESIAN_POINT('Ctrl Pts',(-18.2957212303086,17.6010219545096,122.948615518676)) ;
#20261 = CARTESIAN_POINT('Ctrl Pts',(-18.0173408799565,17.4210328741467,122.832800782693)) ;
#20262 = CARTESIAN_POINT('Ctrl Pts',(-18.3935237813903,17.6110577920422,122.761687553403)) ;
#20263 = CARTESIAN_POINT('Ctrl Pts',(-18.1395964065383,17.4310687116793,122.599142062341)) ;
#20264 = CARTESIAN_POINT('Ctrl Pts',(-18.5203340583895,17.6209479182536,122.596896263532)) ;
#20265 = CARTESIAN_POINT('Ctrl Pts',(-18.2981116221672,17.4409588378907,122.393154239559)) ;
#20266 = CARTESIAN_POINT('Ctrl Pts',(-18.6751694912199,17.6309401001616,122.454946682161)) ;
#20267 = CARTESIAN_POINT('Ctrl Pts',(-18.4916578231572,17.4509510197987,122.215719190812)) ;
#20268 = CARTESIAN_POINT('Ctrl Pts',(-18.8515274887847,17.6408860401002,122.342614062486)) ;
#20269 = CARTESIAN_POINT('Ctrl Pts',(-18.7121069676179,17.4608969597373,122.075305569039)) ;
#20270 = CARTESIAN_POINT('Ctrl Pts',(-19.0445828832562,17.6508332238642,122.262203190812)) ;
#20271 = CARTESIAN_POINT('Ctrl Pts',(-18.9534274542707,17.4708441435014,121.974794440461)) ;
#20272 = CARTESIAN_POINT('Ctrl Pts',(-19.2507687647506,17.6608811621717,122.21630679009)) ;
#20273 = CARTESIAN_POINT('Ctrl Pts',(-19.211160386698,17.4808920818088,121.917426601221)) ;
#20274 = CARTESIAN_POINT('Ctrl Pts',(-19.4575859789318,17.670728796912,122.206920104581)) ;
#20275 = CARTESIAN_POINT('Ctrl Pts',(-19.4696824314095,17.4907397165491,121.905695967141)) ;
#20276 = CARTESIAN_POINT('Ctrl Pts',(-19.6653420100825,17.6806905108858,122.233242738369)) ;
#20277 = CARTESIAN_POINT('Ctrl Pts',(-19.7293772423961,17.5007014305229,121.938602055784)) ;
#20278 = CARTESIAN_POINT('Ctrl Pts',(-19.8666582474384,17.6907191456766,122.295917378937)) ;
#20279 = CARTESIAN_POINT('Ctrl Pts',(-19.9810217545707,17.5107300653138,122.016948020053)) ;
#20280 = CARTESIAN_POINT('Ctrl Pts',(-20.0518343532791,17.7006294642738,122.391384008924)) ;
#20281 = CARTESIAN_POINT('Ctrl Pts',(-20.2124907996332,17.5206403839109,122.136283881726)) ;
#20282 = CARTESIAN_POINT('Ctrl Pts',(-20.2183778744694,17.7105643205853,122.517438880118)) ;
#20283 = CARTESIAN_POINT('Ctrl Pts',(-20.4206686080383,17.5305752402224,122.293854796919)) ;
#20284 = CARTESIAN_POINT('Ctrl Pts',(-20.3618650760254,17.720605556546,122.672260820024)) ;
#20285 = CARTESIAN_POINT('Ctrl Pts',(-20.6000255828736,17.5406164761831,122.487384162176)) ;
#20286 = CARTESIAN_POINT('Ctrl Pts',(-20.4746913192289,17.730492328126,122.846848178747)) ;
#20287 = CARTESIAN_POINT('Ctrl Pts',(-20.7410561133952,17.5505032477631,122.70562002418)) ;
#20288 = CARTESIAN_POINT('Ctrl Pts',(-20.5566303036143,17.7404925068322,123.040424795211)) ;
#20289 = CARTESIAN_POINT('Ctrl Pts',(-20.8434772707178,17.5605034264693,122.947591960567)) ;
#20290 = CARTESIAN_POINT('Ctrl Pts',(-20.6035135712802,17.7504097850418,123.243613328282)) ;
#20291 = CARTESIAN_POINT('Ctrl Pts',(-20.9020786278622,17.5704207046789,123.201578349681)) ;
#20292 = CARTESIAN_POINT('Ctrl Pts',(-20.6144792344301,17.7604570314554,123.454524019583)) ;
#20293 = CARTESIAN_POINT('Ctrl Pts',(-20.91578288945,17.5804679510926,123.465216930615)) ;
#20294 = CARTESIAN_POINT('Ctrl Pts',(-20.5893156501157,17.7703309204367,123.660606188454)) ;
#20295 = CARTESIAN_POINT('Ctrl Pts',(-20.8843256015444,17.5903418400739,123.722819361991)) ;
#20296 = CARTESIAN_POINT('Ctrl Pts',(-20.5277259008089,17.7803929380173,123.862949653921)) ;
#20297 = CARTESIAN_POINT('Ctrl Pts',(-20.8073356878369,17.6004038576544,123.975747950634)) ;
#20298 = CARTESIAN_POINT('Ctrl Pts',(-20.4337117630159,17.7902639997516,124.047969554099)) ;
#20299 = CARTESIAN_POINT('Ctrl Pts',(-20.6898154915697,17.6102749193887,124.207021563565)) ;
#20300 = CARTESIAN_POINT('Ctrl Pts',(-20.3079243206762,17.8002580631119,124.216261726582)) ;
#20301 = CARTESIAN_POINT('Ctrl Pts',(-20.5325789116341,17.620268982749,124.417385133982)) ;
#20302 = CARTESIAN_POINT('Ctrl Pts',(-20.1539268427788,17.8102902211453,124.360359874933)) ;
#20303 = CARTESIAN_POINT('Ctrl Pts',(-20.3400800616733,17.6303011407824,124.597505830153)) ;
#20304 = CARTESIAN_POINT('Ctrl Pts',(-19.9804372227752,17.8201540973854,124.473993821074)) ;
#20305 = CARTESIAN_POINT('Ctrl Pts',(-20.1232165512678,17.6401650170226,124.739545873156)) ;
#20306 = CARTESIAN_POINT('Ctrl Pts',(-19.7859124945591,17.8302246120237,124.557495151561)) ;
#20307 = CARTESIAN_POINT('Ctrl Pts',(-19.8800594521067,17.6502355316608,124.843920027478)) ;
#20308 = CARTESIAN_POINT('Ctrl Pts',(-19.5845131324371,17.8400652489647,124.604874841152)) ;
#20309 = CARTESIAN_POINT('Ctrl Pts',(-19.6283095577294,17.6600761686018,124.90314183829)) ;
#20310 = CARTESIAN_POINT('Ctrl Pts',(-19.3753651784529,17.8500323778049,124.617404469325)) ;
#20311 = CARTESIAN_POINT('Ctrl Pts',(-19.366875274711,17.670043297442,124.918801259543)) ;
#20312 = CARTESIAN_POINT('Ctrl Pts',(-19.1662372548247,17.8600463509294,124.593093186389)) ;
#20313 = CARTESIAN_POINT('Ctrl Pts',(-19.1054626465016,17.6800572705665,124.888408905222)) ;
#20314 = CARTESIAN_POINT('Ctrl Pts',(-18.8985829814894,17.8733310847927,124.513236748648)) ;
#20315 = CARTESIAN_POINT('Ctrl Pts',(-18.7709105569482,17.6933420044298,124.788587304081)) ;
#20316 = CARTESIAN_POINT('Ctrl Pts',(-18.6588816082281,17.8865563495074,124.366233166193)) ;
#20317 = CARTESIAN_POINT('Ctrl Pts',(-18.4713115759659,17.7065672691446,124.604860086354)) ;
#20318 = CARTESIAN_POINT('Ctrl Pts',(-18.4660643936239,17.8998668720623,124.16345986531)) ;
#20319 = CARTESIAN_POINT('Ctrl Pts',(-18.23024753484,17.7198777916994,124.351352544017)) ;
#20320 = CARTESIAN_POINT('Ctrl Pts',(-18.3496539207817,17.9098955169645,123.987675168725)) ;
#20321 = CARTESIAN_POINT('Ctrl Pts',(-18.0847456433107,17.7299064366016,124.131627885447)) ;
#20322 = CARTESIAN_POINT('Ctrl Pts',(-18.2666046768902,17.9197765493184,123.797265561307)) ;
#20323 = CARTESIAN_POINT('Ctrl Pts',(-17.9809344252587,17.7397874689555,123.893612632043)) ;
#20324 = CARTESIAN_POINT('Ctrl Pts',(-18.2169614950972,17.9297575219985,123.593391497918)) ;
#20325 = CARTESIAN_POINT('Ctrl Pts',(-17.9188829813947,17.7497684416356,123.638771587196)) ;
#20326 = CARTESIAN_POINT('Ctrl Pts',(-18.203650414156,17.9397386495845,123.383995886292)) ;
#20327 = CARTESIAN_POINT('Ctrl Pts',(-17.9022490540845,17.7597495692216,123.377020959202)) ;
#20328 = CARTESIAN_POINT('Ctrl Pts',(-18.2339270986067,17.9529818398459,123.107154473442)) ;
#20329 = CARTESIAN_POINT('Ctrl Pts',(-17.940086062115,17.772992759483,123.030998917188)) ;
#20330 = CARTESIAN_POINT('Ctrl Pts',(-18.3623848961341,17.9696498352067,122.77698011445)) ;
#20331 = CARTESIAN_POINT('Ctrl Pts',(-18.1006895820262,17.7896607548438,122.618237447441)) ;
#20332 = CARTESIAN_POINT('Ctrl Pts',(-18.5937018814127,17.9861703352187,122.512467682985)) ;
#20333 = CARTESIAN_POINT('Ctrl Pts',(-18.3897812209932,17.8061812548558,122.28765824502)) ;
#20334 = CARTESIAN_POINT('Ctrl Pts',(-18.8258934089198,17.9994833515347,122.356347563406)) ;
#20335 = CARTESIAN_POINT('Ctrl Pts',(-18.6800705190158,17.8194942711718,122.092466331838)) ;
#20336 = CARTESIAN_POINT('Ctrl Pts',(-19.0164028181987,18.0093999097677,122.271568361071)) ;
#20337 = CARTESIAN_POINT('Ctrl Pts',(-18.9181973224567,17.8294108294048,121.986503440751)) ;
#20338 = CARTESIAN_POINT('Ctrl Pts',(-19.2209294726659,18.0194275780706,122.220690420935)) ;
#20339 = CARTESIAN_POINT('Ctrl Pts',(-19.1738622433935,17.8394384977077,121.92290647105)) ;
#20340 = CARTESIAN_POINT('Ctrl Pts',(-19.4974318665862,18.0326081678152,122.200829010894)) ;
#20341 = CARTESIAN_POINT('Ctrl Pts',(-19.5194723945054,17.8526190874524,121.898080551952)) ;
#20342 = CARTESIAN_POINT('Ctrl Pts',(-19.8468976293333,18.0493563069346,122.268323420744)) ;
#20343 = CARTESIAN_POINT('Ctrl Pts',(-19.9563231936178,17.8693672265717,121.982455382444)) ;
#20344 = CARTESIAN_POINT('Ctrl Pts',(-20.208402785875,18.0691510494452,122.484267090907)) ;
#20345 = CARTESIAN_POINT('Ctrl Pts',(-20.4081951552472,17.8891619690823,122.252387033747)) ;
#20346 = CARTESIAN_POINT('Ctrl Pts',(-20.4779851808533,18.089195442254,122.814181391248)) ;
#20347 = CARTESIAN_POINT('Ctrl Pts',(-20.7451718132866,17.9092063618911,122.66478304066)) ;
#20348 = CARTESIAN_POINT('Ctrl Pts',(-20.6171002054309,18.1090346245527,123.212537767396)) ;
#20349 = CARTESIAN_POINT('Ctrl Pts',(-20.9190608630453,17.9290455441898,123.162728597956)) ;
#20350 = CARTESIAN_POINT('Ctrl Pts',(-20.6129501344917,18.1289599482456,123.636081201346)) ;
#20351 = CARTESIAN_POINT('Ctrl Pts',(-20.9138698455996,17.9489708678827,123.692157121899)) ;
#20352 = CARTESIAN_POINT('Ctrl Pts',(-20.4644170209885,18.1488835862971,124.032892736758)) ;
#20353 = CARTESIAN_POINT('Ctrl Pts',(-20.7282004987486,17.9688945059342,124.188169695646)) ;
#20354 = CARTESIAN_POINT('Ctrl Pts',(-20.1895488356295,18.1688084597626,124.355214759084)) ;
#20355 = CARTESIAN_POINT('Ctrl Pts',(-20.3846133570625,17.9888193793997,124.591069561661)) ;
#20356 = CARTESIAN_POINT('Ctrl Pts',(-19.8222522044971,18.1886870668415,124.564420794737)) ;
#20357 = CARTESIAN_POINT('Ctrl Pts',(-19.9254924402877,18.0086979864787,124.852574068712)) ;
#20358 = CARTESIAN_POINT('Ctrl Pts',(-19.4036094051165,18.2086645096735,124.636282835696)) ;
#20359 = CARTESIAN_POINT('Ctrl Pts',(-19.4021887856867,18.0286754293106,124.94239921452)) ;
#20360 = CARTESIAN_POINT('Ctrl Pts',(-18.9865333106449,18.2285963577582,124.560840820189)) ;
#20361 = CARTESIAN_POINT('Ctrl Pts',(-18.8808448567372,18.0486072773953,124.848094480769)) ;
#20362 = CARTESIAN_POINT('Ctrl Pts',(-18.6207574150074,18.2484916261008,124.348382771225)) ;
#20363 = CARTESIAN_POINT('Ctrl Pts',(-18.4236271458194,18.0685025457379,124.582520931676)) ;
#20364 = CARTESIAN_POINT('Ctrl Pts',(-18.3486814493143,18.2684141245129,124.02368906418)) ;
#20365 = CARTESIAN_POINT('Ctrl Pts',(-18.083533966346,18.08842504415,124.176653707817)) ;
#20366 = CARTESIAN_POINT('Ctrl Pts',(-18.2035687666535,18.2883736063889,123.62485045441)) ;
#20367 = CARTESIAN_POINT('Ctrl Pts',(-17.9021445000866,18.108384526026,123.678105539859)) ;
#20368 = CARTESIAN_POINT('Ctrl Pts',(-18.203194006856,18.3082513588482,123.202260983975)) ;
#20369 = CARTESIAN_POINT('Ctrl Pts',(-17.901677043034,18.1282622784854,123.149870596743)) ;
#20370 = CARTESIAN_POINT('Ctrl Pts',(-18.3459964134725,18.3281331495828,122.804281369069)) ;
#20371 = CARTESIAN_POINT('Ctrl Pts',(-18.0801792550787,18.1481440692199,122.65239779122)) ;
#20372 = CARTESIAN_POINT('Ctrl Pts',(-18.6191997385848,18.3482064884338,122.476442912359)) ;
#20373 = CARTESIAN_POINT('Ctrl Pts',(-18.4216843162061,18.1682174080709,122.242598944837)) ;
#20374 = CARTESIAN_POINT('Ctrl Pts',(-18.9830102331295,18.3680109556696,122.264221298364)) ;
#20375 = CARTESIAN_POINT('Ctrl Pts',(-18.8764446818162,18.1880218753067,121.977323375824)) ;
#20376 = CARTESIAN_POINT('Ctrl Pts',(-19.4008308381281,18.3879942960774,122.187305861743)) ;
#20377 = CARTESIAN_POINT('Ctrl Pts',(-19.3987200282656,18.2080052157145,121.881178045719)) ;
#20378 = CARTESIAN_POINT('Ctrl Pts',(-19.8183304642668,18.4079092606754,122.258027106077)) ;
#20379 = CARTESIAN_POINT('Ctrl Pts',(-19.9205934708167,18.2279201803125,121.969578565073)) ;
#20380 = CARTESIAN_POINT('Ctrl Pts',(-20.1864288478707,18.4277777953917,122.465496330421)) ;
#20381 = CARTESIAN_POINT('Ctrl Pts',(-20.3807158505364,18.2477887150289,122.228912632756)) ;
#20382 = CARTESIAN_POINT('Ctrl Pts',(-20.4635196115804,18.4478301796035,122.789385037709)) ;
#20383 = CARTESIAN_POINT('Ctrl Pts',(-20.7270809482803,18.2678410992406,122.6337729235)) ;
#20384 = CARTESIAN_POINT('Ctrl Pts',(-20.6120028434724,18.4676041433927,123.182923094544)) ;
#20385 = CARTESIAN_POINT('Ctrl Pts',(-20.9126860426018,18.2876150630298,123.125692137824)) ;
#20386 = CARTESIAN_POINT('Ctrl Pts',(-20.6176815723447,18.487658522414,123.609124769732)) ;
#20387 = CARTESIAN_POINT('Ctrl Pts',(-20.919787056096,18.3076694420512,123.658444810698)) ;
#20388 = CARTESIAN_POINT('Ctrl Pts',(-20.4791262983683,18.5074552599873,124.006731982983)) ;
#20389 = CARTESIAN_POINT('Ctrl Pts',(-20.7465962162573,18.3274661796244,124.155452562203)) ;
#20390 = CARTESIAN_POINT('Ctrl Pts',(-20.2119627746794,18.5274230723387,124.33658343425)) ;
#20391 = CARTESIAN_POINT('Ctrl Pts',(-20.4126446942546,18.3474339919759,124.567768827108)) ;
#20392 = CARTESIAN_POINT('Ctrl Pts',(-19.8479424439338,18.5473820484038,124.554891666292)) ;
#20393 = CARTESIAN_POINT('Ctrl Pts',(-19.9576212451287,18.3673929680409,124.840656736435)) ;
#20394 = CARTESIAN_POINT('Ctrl Pts',(-19.4327602934189,18.5672769666812,124.635860460392)) ;
#20395 = CARTESIAN_POINT('Ctrl Pts',(-19.4386451944303,18.3872878863183,124.941871042673)) ;
#20396 = CARTESIAN_POINT('Ctrl Pts',(-19.0147820526511,18.5871732791315,124.570804620221)) ;
#20397 = CARTESIAN_POINT('Ctrl Pts',(-18.9161726453232,18.4071841987686,124.860555263088)) ;
#20398 = CARTESIAN_POINT('Ctrl Pts',(-18.6435903312615,18.6070812125056,124.367280330836)) ;
#20399 = CARTESIAN_POINT('Ctrl Pts',(-18.4521815633956,18.4270921321427,124.606153931591)) ;
#20400 = CARTESIAN_POINT('Ctrl Pts',(-18.3636220458617,18.6270311027941,124.048654042255)) ;
#20401 = CARTESIAN_POINT('Ctrl Pts',(-18.1022181077,18.4470420224312,124.207874213592)) ;
#20402 = CARTESIAN_POINT('Ctrl Pts',(-18.2093224184274,18.6469083332954,123.655139111936)) ;
#20403 = CARTESIAN_POINT('Ctrl Pts',(-17.9093397630461,18.4669192529325,123.715982843254)) ;
#20404 = CARTESIAN_POINT('Ctrl Pts',(-18.1982991555925,18.6668910021664,123.230417623875)) ;
#20405 = CARTESIAN_POINT('Ctrl Pts',(-17.8955552161801,18.4869019218035,123.185081472576)) ;
#20406 = CARTESIAN_POINT('Ctrl Pts',(-18.3328317480087,18.6868238887468,122.828454448446)) ;
#20407 = CARTESIAN_POINT('Ctrl Pts',(-18.0637189576036,18.5068348083839,122.682625101242)) ;
#20408 = CARTESIAN_POINT('Ctrl Pts',(-18.5959241687473,18.7067366347647,122.496751886595)) ;
#20409 = CARTESIAN_POINT('Ctrl Pts',(-18.3925705510188,18.5267475544018,122.267998602716)) ;
#20410 = CARTESIAN_POINT('Ctrl Pts',(-18.8956709172905,18.7233063561065,122.311665038351)) ;
#20411 = CARTESIAN_POINT('Ctrl Pts',(-18.767281881698,18.5433172757436,122.036622749478)) ;
#20412 = CARTESIAN_POINT('Ctrl Pts',(-19.1634796639719,18.7366063674115,122.231169175464)) ;
#20413 = CARTESIAN_POINT('Ctrl Pts',(-19.1020056145289,18.5566172870486,121.936011376313)) ;
#20414 = CARTESIAN_POINT('Ctrl Pts',(-19.44044901437,18.7498765551614,122.198083479457)) ;
#20415 = CARTESIAN_POINT('Ctrl Pts',(-19.4482877506077,18.5698874747985,121.89465138511)) ;
#20416 = CARTESIAN_POINT('Ctrl Pts',(-19.7904919604174,18.7665039375268,122.248222801517)) ;
#20417 = CARTESIAN_POINT('Ctrl Pts',(-19.8857560482088,18.5865148571639,121.957313792384)) ;
#20418 = CARTESIAN_POINT('Ctrl Pts',(-20.1021440207609,18.783126227272,122.414835522395)) ;
#20419 = CARTESIAN_POINT('Ctrl Pts',(-20.2753787251303,18.6031371469091,122.165595250357)) ;
#20420 = CARTESIAN_POINT('Ctrl Pts',(-20.3055329334675,18.7963714416665,122.605057021473)) ;
#20421 = CARTESIAN_POINT('Ctrl Pts',(-20.5295847929134,18.6163823613036,122.403352527217)) ;
#20422 = CARTESIAN_POINT('Ctrl Pts',(-20.4311881436849,18.8062834066272,122.771300615763)) ;
#20423 = CARTESIAN_POINT('Ctrl Pts',(-20.6866624263127,18.6262943262643,122.611158628173)) ;
#20424 = CARTESIAN_POINT('Ctrl Pts',(-20.5272430540412,18.8163420297916,122.959664946299)) ;
#20425 = CARTESIAN_POINT('Ctrl Pts',(-20.8067318368115,18.6363529494288,122.846612050245)) ;
#20426 = CARTESIAN_POINT('Ctrl Pts',(-20.5880949584386,18.8261821439075,123.157414828597)) ;
#20427 = CARTESIAN_POINT('Ctrl Pts',(-20.882799746978,18.6461930635446,123.093798587262)) ;
#20428 = CARTESIAN_POINT('Ctrl Pts',(-20.6144765414881,18.8362479288651,123.367346989237)) ;
#20429 = CARTESIAN_POINT('Ctrl Pts',(-20.9157793856879,18.6562588485022,123.356213554678)) ;
#20430 = CARTESIAN_POINT('Ctrl Pts',(-20.6041033810044,18.846131246653,123.574893561351)) ;
#20431 = CARTESIAN_POINT('Ctrl Pts',(-20.9028157443252,18.6661421662901,123.615646798569)) ;
#20432 = CARTESIAN_POINT('Ctrl Pts',(-20.557811278042,18.8561206845115,123.779716355101)) ;
#20433 = CARTESIAN_POINT('Ctrl Pts',(-20.8449533316139,18.6761316041487,123.871675964814)) ;
#20434 = CARTESIAN_POINT('Ctrl Pts',(-20.4767860972541,18.8660843985643,123.972890703501)) ;
#20435 = CARTESIAN_POINT('Ctrl Pts',(-20.7436744284095,18.6860953182014,124.113145006398)) ;
#20436 = CARTESIAN_POINT('Ctrl Pts',(-20.3632771377155,18.8760794102235,124.149739579038)) ;
#20437 = CARTESIAN_POINT('Ctrl Pts',(-20.6017905558508,18.6960903298606,124.334207674781)) ;
#20438 = CARTESIAN_POINT('Ctrl Pts',(-20.2199721057436,18.8861157019177,124.304588195844)) ;
#20439 = CARTESIAN_POINT('Ctrl Pts',(-20.4226612590053,18.7061266215549,124.527770408748)) ;
#20440 = CARTESIAN_POINT('Ctrl Pts',(-20.0553231898177,18.8959620796112,124.430069749636)) ;
#20441 = CARTESIAN_POINT('Ctrl Pts',(-20.2168518529892,18.7159729992483,124.684624557531)) ;
#20442 = CARTESIAN_POINT('Ctrl Pts',(-19.8690215673185,18.9059470237619,124.526730415756)) ;
#20443 = CARTESIAN_POINT('Ctrl Pts',(-19.9839760536042,18.725957943399,124.805452933041)) ;
#20444 = CARTESIAN_POINT('Ctrl Pts',(-19.6697047219603,18.9158839948918,124.589408387716)) ;
#20445 = CARTESIAN_POINT('Ctrl Pts',(-19.7348307743134,18.735894914529,124.883803103654)) ;
#20446 = CARTESIAN_POINT('Ctrl Pts',(-19.4602197023148,18.9259337795236,124.616715999974)) ;
#20447 = CARTESIAN_POINT('Ctrl Pts',(-19.4729748038764,18.7459446991607,124.917940423187)) ;
#20448 = CARTESIAN_POINT('Ctrl Pts',(-19.2533184450846,18.9357842416011,124.607579273782)) ;
#20449 = CARTESIAN_POINT('Ctrl Pts',(-19.21434799551,18.7557951612382,124.906522324717)) ;
#20450 = CARTESIAN_POINT('Ctrl Pts',(-19.0485745773188,18.9457562551215,124.562644959168)) ;
#20451 = CARTESIAN_POINT('Ctrl Pts',(-18.9584174462669,18.7657671747586,124.850357148989)) ;
#20452 = CARTESIAN_POINT('Ctrl Pts',(-18.8542477972193,18.9557514022409,124.482609220366)) ;
#20453 = CARTESIAN_POINT('Ctrl Pts',(-18.7155078312172,18.775762321878,124.750315034863)) ;
#20454 = CARTESIAN_POINT('Ctrl Pts',(-18.6762610468344,18.965785371977,124.369422704143)) ;
#20455 = CARTESIAN_POINT('Ctrl Pts',(-18.493022848757,18.7857962916141,124.608834245128)) ;
#20456 = CARTESIAN_POINT('Ctrl Pts',(-18.5231511574649,18.9756409176476,124.229798349696)) ;
#20457 = CARTESIAN_POINT('Ctrl Pts',(-18.3016334315015,18.7956518372847,124.434305714712)) ;
#20458 = CARTESIAN_POINT('Ctrl Pts',(-18.3945701733205,18.9856396746608,124.063548623651)) ;
#20459 = CARTESIAN_POINT('Ctrl Pts',(-18.140904940295,18.8056505942979,124.226495189743)) ;
#20460 = CARTESIAN_POINT('Ctrl Pts',(-18.2975958365009,18.995536809898,123.879424723443)) ;
#20461 = CARTESIAN_POINT('Ctrl Pts',(-18.019684455447,18.8155477295351,123.99634137885)) ;
#20462 = CARTESIAN_POINT('Ctrl Pts',(-18.2330434105871,19.0055899057376,123.678199215092)) ;
#20463 = CARTESIAN_POINT('Ctrl Pts',(-17.93899129175,18.8256008253747,123.744810345997)) ;
#20464 = CARTESIAN_POINT('Ctrl Pts',(-18.2048687725473,19.0154734144682,123.472321453931)) ;
#20465 = CARTESIAN_POINT('Ctrl Pts',(-17.9037702162779,18.8354843341053,123.487463211661)) ;
#20466 = CARTESIAN_POINT('Ctrl Pts',(-18.2124671547143,19.0254682871143,123.262341510424)) ;
#20467 = CARTESIAN_POINT('Ctrl Pts',(-17.9132654845491,18.8454792067514,123.224988077224)) ;
#20468 = CARTESIAN_POINT('Ctrl Pts',(-18.2568443718026,19.03548824875,123.056405743036)) ;
#20469 = CARTESIAN_POINT('Ctrl Pts',(-17.9687343278623,18.8554991683871,122.967567757792)) ;
#20470 = CARTESIAN_POINT('Ctrl Pts',(-18.3352281082984,19.0453936125498,122.863482475236)) ;
#20471 = CARTESIAN_POINT('Ctrl Pts',(-18.0667115840973,18.865404532187,122.726412358638)) ;
#20472 = CARTESIAN_POINT('Ctrl Pts',(-18.4459450487129,19.0553342001574,122.686255011705)) ;
#20473 = CARTESIAN_POINT('Ctrl Pts',(-18.2051056278125,18.8753451197945,122.504876382137)) ;
#20474 = CARTESIAN_POINT('Ctrl Pts',(-18.5865641592456,19.065337018258,122.529862565855)) ;
#20475 = CARTESIAN_POINT('Ctrl Pts',(-18.3808775940096,18.8853479378952,122.309383985207)) ;
#20476 = CARTESIAN_POINT('Ctrl Pts',(-18.7529137805727,19.0753717299822,122.400141597635)) ;
#20477 = CARTESIAN_POINT('Ctrl Pts',(-18.5888129419843,18.8953826496193,122.147230647452)) ;
#20478 = CARTESIAN_POINT('Ctrl Pts',(-18.9355927334257,19.0852166367195,122.302823707512)) ;
#20479 = CARTESIAN_POINT('Ctrl Pts',(-18.8171608789422,18.9052275563566,122.025580674038)) ;
#20480 = CARTESIAN_POINT('Ctrl Pts',(-19.135044952863,19.0952024892885,122.237424139112)) ;
#20481 = CARTESIAN_POINT('Ctrl Pts',(-19.066475495053,18.9152134089256,121.943828689904)) ;
#20482 = CARTESIAN_POINT('Ctrl Pts',(-19.3418110241518,19.1051372977015,122.207643930743)) ;
#20483 = CARTESIAN_POINT('Ctrl Pts',(-19.3249330398174,18.9251482173387,121.906600838846)) ;
#20484 = CARTESIAN_POINT('Ctrl Pts',(-19.5531110415552,19.1151948247826,122.214485106709)) ;
#20485 = CARTESIAN_POINT('Ctrl Pts',(-19.5890580305708,18.9352057444197,121.915149697282)) ;
#20486 = CARTESIAN_POINT('Ctrl Pts',(-19.7552767450465,19.1250164797797,122.256593308277)) ;
#20487 = CARTESIAN_POINT('Ctrl Pts',(-19.8417664438443,18.9450273994168,121.967782613312)) ;
#20488 = CARTESIAN_POINT('Ctrl Pts',(-19.9517461949997,19.1350725239527,122.334610066435)) ;
#20489 = CARTESIAN_POINT('Ctrl Pts',(-20.0873540689241,18.9550834435898,122.065301218056)) ;
#20490 = CARTESIAN_POINT('Ctrl Pts',(-20.1294455067056,19.1450132639979,122.44461757867)) ;
#20491 = CARTESIAN_POINT('Ctrl Pts',(-20.3094798342934,18.965024183635,122.20280861514)) ;
#20492 = CARTESIAN_POINT('Ctrl Pts',(-20.2852002013898,19.1549173850707,122.582803466189)) ;
#20493 = CARTESIAN_POINT('Ctrl Pts',(-20.5041752042223,18.9749283047079,122.375539516404)) ;
#20494 = CARTESIAN_POINT('Ctrl Pts',(-20.4163570695297,19.164964926225,122.748363557703)) ;
#20495 = CARTESIAN_POINT('Ctrl Pts',(-20.6681231446912,18.9849758458621,122.58248803559)) ;
#20496 = CARTESIAN_POINT('Ctrl Pts',(-20.5154426781397,19.1748636778254,122.931394298921)) ;
#20497 = CARTESIAN_POINT('Ctrl Pts',(-20.7919825435621,18.9948745974625,122.811275811282)) ;
#20498 = CARTESIAN_POINT('Ctrl Pts',(-20.5823095621663,19.1849121567912,123.13175874193)) ;
#20499 = CARTESIAN_POINT('Ctrl Pts',(-20.8755683816824,19.0049230764283,123.061730492506)) ;
#20500 = CARTESIAN_POINT('Ctrl Pts',(-20.6128955919429,19.1947996538749,123.337384367782)) ;
#20501 = CARTESIAN_POINT('Ctrl Pts',(-20.9138033739238,19.014810573512,123.318762800787)) ;
#20502 = CARTESIAN_POINT('Ctrl Pts',(-20.6076449007628,19.204792744173,123.547386563793)) ;
#20503 = CARTESIAN_POINT('Ctrl Pts',(-20.9072423074913,19.0248036638101,123.581265757207)) ;
#20504 = CARTESIAN_POINT('Ctrl Pts',(-20.5661040890578,19.2147449142333,123.752459949604)) ;
#20505 = CARTESIAN_POINT('Ctrl Pts',(-20.8553184944048,19.0347558338704,123.837608299615)) ;
#20506 = CARTESIAN_POINT('Ctrl Pts',(-20.4899691627066,19.2246833341478,123.947015816567)) ;
#20507 = CARTESIAN_POINT('Ctrl Pts',(-20.7601517684657,19.0446942537849,124.080804362951)) ;
#20508 = CARTESIAN_POINT('Ctrl Pts',(-20.3808817205689,19.2346684642334,124.126388705012)) ;
#20509 = CARTESIAN_POINT('Ctrl Pts',(-20.6237942335491,19.0546793838705,124.305021774752)) ;
#20510 = CARTESIAN_POINT('Ctrl Pts',(-20.241378136144,19.2447051536475,124.284677346866)) ;
#20511 = CARTESIAN_POINT('Ctrl Pts',(-20.4494165139908,19.0647160732846,124.502884010772)) ;
#20512 = CARTESIAN_POINT('Ctrl Pts',(-20.0796809670724,19.25455983764,124.414229163885)) ;
#20513 = CARTESIAN_POINT('Ctrl Pts',(-20.2472957009717,19.0745707572771,124.664826057112)) ;
#20514 = CARTESIAN_POINT('Ctrl Pts',(-19.8954624316429,19.2645593216878,124.515427636075)) ;
#20515 = CARTESIAN_POINT('Ctrl Pts',(-20.0170234288064,19.0845702413249,124.791326058903)) ;
#20516 = CARTESIAN_POINT('Ctrl Pts',(-19.6985533037412,19.2744544104647,124.582628798739)) ;
#20517 = CARTESIAN_POINT('Ctrl Pts',(-19.7708869846679,19.0944653301018,124.875329679388)) ;
#20518 = CARTESIAN_POINT('Ctrl Pts',(-19.4895873463579,19.2845149651109,124.615123526839)) ;
#20519 = CARTESIAN_POINT('Ctrl Pts',(-19.5096800897201,19.104525884748,124.915950078661)) ;
#20520 = CARTESIAN_POINT('Ctrl Pts',(-19.2825491814808,19.2943642294838,124.611047104812)) ;
#20521 = CARTESIAN_POINT('Ctrl Pts',(-19.2508813050788,19.1143751491209,124.910856545189)) ;
#20522 = CARTESIAN_POINT('Ctrl Pts',(-19.0756100518396,19.3043914819316,124.570889809376)) ;
#20523 = CARTESIAN_POINT('Ctrl Pts',(-18.99220707569,19.1244024015687,124.86066175785)) ;
#20524 = CARTESIAN_POINT('Ctrl Pts',(-18.8789515708921,19.3144197795018,124.494880706852)) ;
#20525 = CARTESIAN_POINT('Ctrl Pts',(-18.7463833099064,19.1344306991389,124.765652294078)) ;
#20526 = CARTESIAN_POINT('Ctrl Pts',(-18.701566831824,19.3242659085078,124.388210448307)) ;
#20527 = CARTESIAN_POINT('Ctrl Pts',(-18.5246504442198,19.1442768281449,124.632315524006)) ;
#20528 = CARTESIAN_POINT('Ctrl Pts',(-18.5427028733491,19.3342598138698,124.250713710067)) ;
#20529 = CARTESIAN_POINT('Ctrl Pts',(-18.3260692253604,19.154270733507,124.460445802928)) ;
#20530 = CARTESIAN_POINT('Ctrl Pts',(-18.4100146534908,19.3442839115529,124.086985981103)) ;
#20531 = CARTESIAN_POINT('Ctrl Pts',(-18.1602075359614,19.16429483119,124.255787351941)) ;
#20532 = CARTESIAN_POINT('Ctrl Pts',(-18.3089126305251,19.3541737394069,123.90530352091)) ;
#20533 = CARTESIAN_POINT('Ctrl Pts',(-18.0338280399953,19.174184659044,124.028684394348)) ;
#20534 = CARTESIAN_POINT('Ctrl Pts',(-18.2399042502461,19.3641657208373,123.706908085251)) ;
#20535 = CARTESIAN_POINT('Ctrl Pts',(-17.947565914458,19.1841766404745,123.780690475578)) ;
#20536 = CARTESIAN_POINT('Ctrl Pts',(-18.2065905895425,19.3741127256032,123.50046117222)) ;
#20537 = CARTESIAN_POINT('Ctrl Pts',(-17.9059220811503,19.1941236452403,123.522631607328)) ;
#20538 = CARTESIAN_POINT('Ctrl Pts',(-18.2092454060776,19.384062376993,123.291296502426)) ;
#20539 = CARTESIAN_POINT('Ctrl Pts',(-17.9092390395663,19.2040732966301,123.261175270493)) ;
#20540 = CARTESIAN_POINT('Ctrl Pts',(-18.2486861191594,19.3940993799704,123.084011953046)) ;
#20541 = CARTESIAN_POINT('Ctrl Pts',(-17.958538306793,19.2141102996075,123.002069408009)) ;
#20542 = CARTESIAN_POINT('Ctrl Pts',(-18.3222825230277,19.4039882884054,122.889570998935)) ;
#20543 = CARTESIAN_POINT('Ctrl Pts',(-18.0505326598567,19.2239992080425,122.759016798404)) ;
#20544 = CARTESIAN_POINT('Ctrl Pts',(-18.4292681158825,19.4139776208829,122.708864244681)) ;
#20545 = CARTESIAN_POINT('Ctrl Pts',(-18.1842635126106,19.23398854052,122.533132432072)) ;
#20546 = CARTESIAN_POINT('Ctrl Pts',(-18.5657022346844,19.42393617632,122.550072619534)) ;
#20547 = CARTESIAN_POINT('Ctrl Pts',(-18.3548053010277,19.2439470959571,122.334641591459)) ;
#20548 = CARTESIAN_POINT('Ctrl Pts',(-18.7263649466662,19.4338357475205,122.417759602104)) ;
#20549 = CARTESIAN_POINT('Ctrl Pts',(-18.5556335270977,19.2538466671576,122.169248739393)) ;
#20550 = CARTESIAN_POINT('Ctrl Pts',(-18.9102833479291,19.4438836727725,122.313900274746)) ;
#20551 = CARTESIAN_POINT('Ctrl Pts',(-18.7855306745994,19.2638945924096,122.039423510114)) ;
#20552 = CARTESIAN_POINT('Ctrl Pts',(-19.1064125465237,19.4537789722985,122.244448286497)) ;
#20553 = CARTESIAN_POINT('Ctrl Pts',(-19.0306926009335,19.2737898919356,121.952607002251)) ;
#20554 = CARTESIAN_POINT('Ctrl Pts',(-19.3150144344435,19.4638408287464,122.209510718595)) ;
#20555 = CARTESIAN_POINT('Ctrl Pts',(-19.2914444276105,19.2838517483836,121.908933829335)) ;
#20556 = CARTESIAN_POINT('Ctrl Pts',(-19.521965316198,19.4736846751631,122.211242753843)) ;
#20557 = CARTESIAN_POINT('Ctrl Pts',(-19.5501343610573,19.2936955948002,121.911097613413)) ;
#20558 = CARTESIAN_POINT('Ctrl Pts',(-19.7280448443102,19.4836476242911,122.248623144845)) ;
#20559 = CARTESIAN_POINT('Ctrl Pts',(-19.8077343935755,19.3036585439283,121.957822195286)) ;
#20560 = CARTESIAN_POINT('Ctrl Pts',(-19.9258004100159,19.4936816607191,122.322067326375)) ;
#20561 = CARTESIAN_POINT('Ctrl Pts',(-20.0549291177178,19.3136925803563,122.049626315006)) ;
#20562 = CARTESIAN_POINT('Ctrl Pts',(-20.1052428274456,19.5035690876772,122.426981156448)) ;
#20563 = CARTESIAN_POINT('Ctrl Pts',(-20.2792335465816,19.3235800073143,122.18076820435)) ;
#20564 = CARTESIAN_POINT('Ctrl Pts',(-20.2660510972554,19.5135835220135,122.562891810069)) ;
#20565 = CARTESIAN_POINT('Ctrl Pts',(-20.4802444747173,19.3335944416507,122.350655841088)) ;
#20566 = CARTESIAN_POINT('Ctrl Pts',(-20.4006689400157,19.5236184666485,122.725307394749)) ;
#20567 = CARTESIAN_POINT('Ctrl Pts',(-20.6485175407954,19.3436293862856,122.553674509814)) ;
#20568 = CARTESIAN_POINT('Ctrl Pts',(-20.5034449260328,19.5334508166795,122.90468153521)) ;
#20569 = CARTESIAN_POINT('Ctrl Pts',(-20.7769890298325,19.3534617363166,122.777893029322)) ;
#20570 = CARTESIAN_POINT('Ctrl Pts',(-20.5752821949681,19.5435262557967,123.10390261523)) ;
#20571 = CARTESIAN_POINT('Ctrl Pts',(-20.8667862746344,19.3635371754338,123.026918659849)) ;
#20572 = CARTESIAN_POINT('Ctrl Pts',(-20.6107689996992,19.5533787210313,123.308014325579)) ;
#20573 = CARTESIAN_POINT('Ctrl Pts',(-20.9111458115105,19.3733896406684,123.282059452494)) ;
#20574 = CARTESIAN_POINT('Ctrl Pts',(-20.6104349718264,19.5634515986082,123.519742050673)) ;
#20575 = CARTESIAN_POINT('Ctrl Pts',(-20.9107290324318,19.3834625182453,123.546718673386)) ;
#20576 = CARTESIAN_POINT('Ctrl Pts',(-20.5741538852815,19.5732941948007,123.723476229926)) ;
#20577 = CARTESIAN_POINT('Ctrl Pts',(-20.8653781808651,19.3933051144378,123.801387925564)) ;
#20578 = CARTESIAN_POINT('Ctrl Pts',(-20.5027249485285,19.583274578916,123.920753137784)) ;
#20579 = CARTESIAN_POINT('Ctrl Pts',(-20.7760923678515,19.4032854985531,124.047984519831)) ;
#20580 = CARTESIAN_POINT('Ctrl Pts',(-20.3973703972249,19.5932930595648,124.10312422854)) ;
#20581 = CARTESIAN_POINT('Ctrl Pts',(-20.6443997501556,19.4133039792019,124.275948701137)) ;
#20582 = CARTESIAN_POINT('Ctrl Pts',(-20.2640988385909,19.6031763745651,124.262563519958)) ;
#20583 = CARTESIAN_POINT('Ctrl Pts',(-20.4778099653252,19.4231872942023,124.475248963833)) ;
#20584 = CARTESIAN_POINT('Ctrl Pts',(-20.1021786910339,19.6132446716556,124.398835786557)) ;
#20585 = CARTESIAN_POINT('Ctrl Pts',(-20.2754104277972,19.4332555912927,124.645589428262)) ;
#20586 = CARTESIAN_POINT('Ctrl Pts',(-19.923452222074,19.6230747400279,124.502661288851)) ;
#20587 = CARTESIAN_POINT('Ctrl Pts',(-20.0520012191522,19.443085659665,124.775372441285)) ;
#20588 = CARTESIAN_POINT('Ctrl Pts',(-19.7249017076277,19.6331415324963,124.575813941918)) ;
#20589 = CARTESIAN_POINT('Ctrl Pts',(-19.8038135625138,19.4531524521334,124.86681341649)) ;
#20590 = CARTESIAN_POINT('Ctrl Pts',(-19.5202469349877,19.6430308659848,124.612640504371)) ;
#20591 = CARTESIAN_POINT('Ctrl Pts',(-19.5479941097252,19.4630417856219,124.912847154411)) ;
#20592 = CARTESIAN_POINT('Ctrl Pts',(-19.3100107554735,19.6530329974009,124.613711705916)) ;
#20593 = CARTESIAN_POINT('Ctrl Pts',(-19.2851987471319,19.473043917038,124.914186378401)) ;
#20594 = CARTESIAN_POINT('Ctrl Pts',(-19.1043078669417,19.6629568670219,124.578660210897)) ;
#20595 = CARTESIAN_POINT('Ctrl Pts',(-19.0280693627692,19.482967786659,124.870372052193)) ;
#20596 = CARTESIAN_POINT('Ctrl Pts',(-18.9055323179189,19.6730003825391,124.507541988361)) ;
#20597 = CARTESIAN_POINT('Ctrl Pts',(-18.7796000674895,19.4930113021762,124.781474531052)) ;
#20598 = CARTESIAN_POINT('Ctrl Pts',(-18.7248906132605,19.6828825954274,124.404844874836)) ;
#20599 = CARTESIAN_POINT('Ctrl Pts',(-18.5537969176444,19.5028935150645,124.653102676941)) ;
#20600 = CARTESIAN_POINT('Ctrl Pts',(-18.5618762979718,19.6929506726468,124.269896713313)) ;
#20601 = CARTESIAN_POINT('Ctrl Pts',(-18.3500292628219,19.5129615922839,124.484417808806)) ;
#20602 = CARTESIAN_POINT('Ctrl Pts',(-18.42770753592,19.702789177381,124.112435729889)) ;
#20603 = CARTESIAN_POINT('Ctrl Pts',(-18.1823173295114,19.5228000970181,124.287590469283)) ;
#20604 = CARTESIAN_POINT('Ctrl Pts',(-18.3203002755283,19.7128519458104,123.930208646522)) ;
#20605 = CARTESIAN_POINT('Ctrl Pts',(-18.04805852035,19.5328628654475,124.059806889975)) ;
#20606 = CARTESIAN_POINT('Ctrl Pts',(-18.2475857905658,19.7227489390931,123.735249596216)) ;
#20607 = CARTESIAN_POINT('Ctrl Pts',(-17.9571650618813,19.5427598587302,123.816107138229)) ;
#20608 = CARTESIAN_POINT('Ctrl Pts',(-18.2090139650098,19.7326801667279,123.530063285988)) ;
#20609 = CARTESIAN_POINT('Ctrl Pts',(-17.9089504191746,19.552691086365,123.559623490826)) ;
#20610 = CARTESIAN_POINT('Ctrl Pts',(-18.206860266534,19.74272232537,123.318958748455)) ;
#20611 = CARTESIAN_POINT('Ctrl Pts',(-17.9062584823097,19.5627332450072,123.295743025407)) ;
#20612 = CARTESIAN_POINT('Ctrl Pts',(-18.2407132566598,19.7526090349011,123.113875533513)) ;
#20613 = CARTESIAN_POINT('Ctrl Pts',(-17.9485751372052,19.5726199545382,123.039387974114)) ;
#20614 = CARTESIAN_POINT('Ctrl Pts',(-18.3100612563688,19.7626020073297,122.915577612345)) ;
#20615 = CARTESIAN_POINT('Ctrl Pts',(-18.035260566707,19.5826129269668,122.791515506251)) ;
#20616 = CARTESIAN_POINT('Ctrl Pts',(-18.4123864646547,19.7725482018663,122.733228885072)) ;
#20617 = CARTESIAN_POINT('Ctrl Pts',(-18.1631676695922,19.5925591215034,122.563579250553)) ;
#20618 = CARTESIAN_POINT('Ctrl Pts',(-18.544466725532,19.7824935767178,122.571123242096)) ;
#20619 = CARTESIAN_POINT('Ctrl Pts',(-18.3282687771438,19.6025044963549,122.360947075224)) ;
#20620 = CARTESIAN_POINT('Ctrl Pts',(-18.7046124165122,19.7925484960777,122.433182725376)) ;
#20621 = CARTESIAN_POINT('Ctrl Pts',(-18.5284509193618,19.6125594157148,122.188521930226)) ;
#20622 = CARTESIAN_POINT('Ctrl Pts',(-18.8818996060472,19.8023700155212,122.327286077013)) ;
#20623 = CARTESIAN_POINT('Ctrl Pts',(-18.750061582201,19.6223809351583,122.056150769602)) ;
#20624 = CARTESIAN_POINT('Ctrl Pts',(-19.0795285112847,19.8124357842881,122.251735177665)) ;
#20625 = CARTESIAN_POINT('Ctrl Pts',(-18.9970975872,19.6324467039252,121.961712899097)) ;
#20626 = CARTESIAN_POINT('Ctrl Pts',(-19.2839777888797,19.8223377059431,122.212355081407)) ;
#20627 = CARTESIAN_POINT('Ctrl Pts',(-19.2526602063055,19.6423486255803,121.912488218236)) ;
#20628 = CARTESIAN_POINT('Ctrl Pts',(-19.4950664842811,19.8323807647642,122.208839746125)) ;
#20629 = CARTESIAN_POINT('Ctrl Pts',(-19.5165208729935,19.6523916844013,121.908094752818)) ;
#20630 = CARTESIAN_POINT('Ctrl Pts',(-19.7007200879061,19.8422867588069,122.241689755879)) ;
#20631 = CARTESIAN_POINT('Ctrl Pts',(-19.7735886685139,19.662297678444,121.949158051718)) ;
#20632 = CARTESIAN_POINT('Ctrl Pts',(-19.8983711923909,19.8522245318887,122.309384254829)) ;
#20633 = CARTESIAN_POINT('Ctrl Pts',(-20.0206528799151,19.6722354515258,122.033777229908)) ;
#20634 = CARTESIAN_POINT('Ctrl Pts',(-20.0830422576944,19.862264895621,122.41160883403)) ;
#20635 = CARTESIAN_POINT('Ctrl Pts',(-20.2514911587077,19.6822758152581,122.161558568198)) ;
#20636 = CARTESIAN_POINT('Ctrl Pts',(-20.2447669194783,19.8721522393445,122.542209039445)) ;
#20637 = CARTESIAN_POINT('Ctrl Pts',(-20.4536472526372,19.6921631589816,122.324810150255)) ;
#20638 = CARTESIAN_POINT('Ctrl Pts',(-20.383052541564,19.8821444699132,122.700322050731)) ;
#20639 = CARTESIAN_POINT('Ctrl Pts',(-20.6265036649569,19.7021553895503,122.522452222942)) ;
#20640 = CARTESIAN_POINT('Ctrl Pts',(-20.4912730530166,19.8920929976968,122.879309922931)) ;
#20641 = CARTESIAN_POINT('Ctrl Pts',(-20.7617787531808,19.7121039173339,122.746188030278)) ;
#20642 = CARTESIAN_POINT('Ctrl Pts',(-20.5669463250774,19.9020297814201,123.074005487427)) ;
#20643 = CARTESIAN_POINT('Ctrl Pts',(-20.856369565108,19.7220407010572,122.989558473137)) ;
#20644 = CARTESIAN_POINT('Ctrl Pts',(-20.6081237683006,19.912012782217,123.279827787106)) ;
#20645 = CARTESIAN_POINT('Ctrl Pts',(-20.9078402627332,19.7320237018542,123.246836830907)) ;
#20646 = CARTESIAN_POINT('Ctrl Pts',(-20.6125768739177,19.9220566690578,123.490910400367)) ;
#20647 = CARTESIAN_POINT('Ctrl Pts',(-20.9134056044351,19.7420675886949,123.510689929292)) ;
#20648 = CARTESIAN_POINT('Ctrl Pts',(-20.5814828811847,19.9318846926323,123.695206220071)) ;
#20649 = CARTESIAN_POINT('Ctrl Pts',(-20.8745366916682,19.7518956122695,123.766060949729)) ;
#20650 = CARTESIAN_POINT('Ctrl Pts',(-20.5138218279158,19.941961940846,123.895916711096)) ;
#20651 = CARTESIAN_POINT('Ctrl Pts',(-20.7899593277774,19.7619728604831,124.016948250578)) ;
#20652 = CARTESIAN_POINT('Ctrl Pts',(-20.4147085608249,19.9518114961513,124.077785912975)) ;
#20653 = CARTESIAN_POINT('Ctrl Pts',(-20.6660660069028,19.7718224157884,124.244285226899)) ;
#20654 = CARTESIAN_POINT('Ctrl Pts',(-20.2825893140887,19.961894204349,124.243476019033)) ;
#20655 = CARTESIAN_POINT('Ctrl Pts',(-20.5009161893016,19.7819051239861,124.451396677659)) ;
#20656 = CARTESIAN_POINT('Ctrl Pts',(-20.1280154651316,19.9717067972754,124.38015779365)) ;
#20657 = CARTESIAN_POINT('Ctrl Pts',(-20.307696830118,19.7917177169126,124.622248846254)) ;
#20658 = CARTESIAN_POINT('Ctrl Pts',(-19.9477519695599,19.9817739895334,124.49096411443)) ;
#20659 = CARTESIAN_POINT('Ctrl Pts',(-20.0823669714035,19.8017849091705,124.760755273323)) ;
#20660 = CARTESIAN_POINT('Ctrl Pts',(-19.7541568951815,19.991672818996,124.56745105753)) ;
#20661 = CARTESIAN_POINT('Ctrl Pts',(-19.8403718039497,19.8116837386331,124.856362880226)) ;
#20662 = CARTESIAN_POINT('Ctrl Pts',(-19.5471389116745,20.0017268101862,124.609885515152)) ;
#20663 = CARTESIAN_POINT('Ctrl Pts',(-19.581599257843,19.8217377298233,124.90940442077)) ;
#20664 = CARTESIAN_POINT('Ctrl Pts',(-19.3396458322229,20.0115985349694,124.615811551427)) ;
#20665 = CARTESIAN_POINT('Ctrl Pts',(-19.3222318233483,19.8316094546065,124.916810422138)) ;
#20666 = CARTESIAN_POINT('Ctrl Pts',(-19.1302124053593,20.0216689770996,124.585074256382)) ;
#20667 = CARTESIAN_POINT('Ctrl Pts',(-19.0604406240858,19.8416798967367,124.878387276188)) ;
#20668 = CARTESIAN_POINT('Ctrl Pts',(-18.9339520390974,20.0315020555299,124.520082076835)) ;
#20669 = CARTESIAN_POINT('Ctrl Pts',(-18.8151144576531,19.851512975167,124.797145106877)) ;
#20670 = CARTESIAN_POINT('Ctrl Pts',(-18.7480434856124,20.0415325290313,124.420574067109)) ;
#20671 = CARTESIAN_POINT('Ctrl Pts',(-18.5827297027157,19.8615434486684,124.672758530689)) ;
#20672 = CARTESIAN_POINT('Ctrl Pts',(-18.5825831311572,20.0515641283299,124.289788081662)) ;
#20673 = CARTESIAN_POINT('Ctrl Pts',(-18.3759053294246,19.8715750479671,124.509274829673)) ;
#20674 = CARTESIAN_POINT('Ctrl Pts',(-18.4448629357415,20.0613938293681,124.13573633142)) ;
#20675 = CARTESIAN_POINT('Ctrl Pts',(-18.2037555511074,19.8814047490052,124.31670801897)) ;
#20676 = CARTESIAN_POINT('Ctrl Pts',(-18.3336698872255,20.0713832674246,123.957571401983)) ;
#20677 = CARTESIAN_POINT('Ctrl Pts',(-18.0647658072952,19.8913941870617,124.094000670336)) ;
#20678 = CARTESIAN_POINT('Ctrl Pts',(-18.2551742977455,20.0814271706407,123.761552123901)) ;
#20679 = CARTESIAN_POINT('Ctrl Pts',(-17.9666480383149,19.9014380902778,123.848976044792)) ;
#20680 = CARTESIAN_POINT('Ctrl Pts',(-18.2124417079699,20.0912486914542,123.559542282254)) ;
#20681 = CARTESIAN_POINT('Ctrl Pts',(-17.9132339251412,19.9112596110913,123.596462120658)) ;
#20682 = CARTESIAN_POINT('Ctrl Pts',(-18.2047766515983,20.1012844157013,123.348703573776)) ;
#20683 = CARTESIAN_POINT('Ctrl Pts',(-17.9036546813369,19.9212953353384,123.332913768264)) ;
#20684 = CARTESIAN_POINT('Ctrl Pts',(-18.2343404621047,20.1113065696338,123.140074801071)) ;
#20685 = CARTESIAN_POINT('Ctrl Pts',(-17.9406113337571,19.9313174892709,123.072128085455)) ;
#20686 = CARTESIAN_POINT('Ctrl Pts',(-18.2983054280949,20.1211688013911,122.942870332528)) ;
#20687 = CARTESIAN_POINT('Ctrl Pts',(-18.0205697573143,19.9411797210282,122.825622198603)) ;
#20688 = CARTESIAN_POINT('Ctrl Pts',(-18.3959846631864,20.131127871849,122.757674344572)) ;
#20689 = CARTESIAN_POINT('Ctrl Pts',(-18.1426708877126,19.9511387914861,122.594127929803)) ;
#20690 = CARTESIAN_POINT('Ctrl Pts',(-18.525566423674,20.1411630442251,122.591200036149)) ;
#20691 = CARTESIAN_POINT('Ctrl Pts',(-18.3046496822276,19.9611739638623,122.386036391047)) ;
#20692 = CARTESIAN_POINT('Ctrl Pts',(-18.6794843882295,20.1510434293834,122.45168426529)) ;
#20693 = CARTESIAN_POINT('Ctrl Pts',(-18.4970491714254,19.9710543490205,122.211642765681)) ;
#20694 = CARTESIAN_POINT('Ctrl Pts',(-18.8583463704345,20.1611001439773,122.33899114382)) ;
#20695 = CARTESIAN_POINT('Ctrl Pts',(-18.720627652709,19.9811110636145,122.070778322321)) ;
#20696 = CARTESIAN_POINT('Ctrl Pts',(-19.0506399135892,20.1709794125494,122.260478579803)) ;
#20697 = CARTESIAN_POINT('Ctrl Pts',(-18.960996130641,19.9909903321865,121.972639347132)) ;
#20698 = CARTESIAN_POINT('Ctrl Pts',(-19.2558093771799,20.1809703700351,122.21550063428)) ;
#20699 = CARTESIAN_POINT('Ctrl Pts',(-19.2174586026876,20.0009812896722,121.916419162101)) ;
#20700 = CARTESIAN_POINT('Ctrl Pts',(-19.466736361105,20.1910110286703,122.20725269721)) ;
#20701 = CARTESIAN_POINT('Ctrl Pts',(-19.4811173295918,20.0110219483074,121.906111456795)) ;
#20702 = CARTESIAN_POINT('Ctrl Pts',(-19.6716056707991,20.2008440083783,122.234820237226)) ;
#20703 = CARTESIAN_POINT('Ctrl Pts',(-19.7372046092749,20.0208549280154,121.940573290861)) ;
#20704 = CARTESIAN_POINT('Ctrl Pts',(-19.8719676861379,20.210837141628,122.297989647427)) ;
#20705 = CARTESIAN_POINT('Ctrl Pts',(-19.9876565139675,20.0308480612651,122.019537420732)) ;
#20706 = CARTESIAN_POINT('Ctrl Pts',(-20.0588521291231,20.2208691940113,122.395761902795)) ;
#20707 = CARTESIAN_POINT('Ctrl Pts',(-20.2212609501245,20.0408801136485,122.141754795336)) ;
#20708 = CARTESIAN_POINT('Ctrl Pts',(-20.2232832799828,20.2307344229627,122.522142243572)) ;
#20709 = CARTESIAN_POINT('Ctrl Pts',(-20.4267990069944,20.0507453425998,122.29973257063)) ;
#20710 = CARTESIAN_POINT('Ctrl Pts',(-20.3650928807111,20.2406963642059,122.676265084852)) ;
#20711 = CARTESIAN_POINT('Ctrl Pts',(-20.6040593213488,20.060707283843,122.492388017739)) ;
#20712 = CARTESIAN_POINT('Ctrl Pts',(-20.4785174817246,20.2507310792426,122.854128710168)) ;
#20713 = CARTESIAN_POINT('Ctrl Pts',(-20.7458379853386,20.0707419988798,122.71471883926)) ;
#20714 = CARTESIAN_POINT('Ctrl Pts',(-20.5584598459099,20.2606168495867,123.045995752101)) ;
#20715 = CARTESIAN_POINT('Ctrl Pts',(-20.8457638320152,20.0806277692238,122.954554133205)) ;
#20716 = CARTESIAN_POINT('Ctrl Pts',(-20.6046719527906,20.2706794469754,123.252408259714)) ;
#20717 = CARTESIAN_POINT('Ctrl Pts',(-20.9035264743855,20.0906903666126,123.212570178599)) ;
#20718 = CARTESIAN_POINT('Ctrl Pts',(-20.6142327360248,20.2805298588107,123.459290301903)) ;
#20719 = CARTESIAN_POINT('Ctrl Pts',(-20.9154749497781,20.1005407784478,123.471173528851)) ;
#20720 = CARTESIAN_POINT('Ctrl Pts',(-20.5877918422668,20.2905570280966,123.668422397058)) ;
#20721 = CARTESIAN_POINT('Ctrl Pts',(-20.8824212203225,20.1105679477337,123.732588303383)) ;
#20722 = CARTESIAN_POINT('Ctrl Pts',(-20.5249072417576,20.3005845088108,123.869644711752)) ;
#20723 = CARTESIAN_POINT('Ctrl Pts',(-20.8038130480593,20.1205954284479,123.984115444725)) ;
#20724 = CARTESIAN_POINT('Ctrl Pts',(-20.4301831206918,20.3104275613901,124.053614638865)) ;
#20725 = CARTESIAN_POINT('Ctrl Pts',(-20.6854052876472,20.1304384810272,124.214077225316)) ;
#20726 = CARTESIAN_POINT('Ctrl Pts',(-20.3034580062551,20.3204214648287,124.221197227413)) ;
#20727 = CARTESIAN_POINT('Ctrl Pts',(-20.5269966913248,20.1404323844658,124.423553915828)) ;
#20728 = CARTESIAN_POINT('Ctrl Pts',(-20.1487806009657,20.3304485876051,124.364425720184)) ;
#20729 = CARTESIAN_POINT('Ctrl Pts',(-20.3336481312429,20.1504595072422,124.602587618317)) ;
#20730 = CARTESIAN_POINT('Ctrl Pts',(-19.9741372933805,20.3403392924971,124.477286085174)) ;
#20731 = CARTESIAN_POINT('Ctrl Pts',(-20.1153421998912,20.1603502121343,124.743661057522)) ;
#20732 = CARTESIAN_POINT('Ctrl Pts',(-19.7807153610016,20.3503313193475,124.559212631353)) ;
#20733 = CARTESIAN_POINT('Ctrl Pts',(-19.873563628878,20.1703422389846,124.846066786522)) ;
#20734 = CARTESIAN_POINT('Ctrl Pts',(-19.5769304517105,20.360277300836,124.606034161387)) ;
#20735 = CARTESIAN_POINT('Ctrl Pts',(-19.618831660715,20.1802882204731,124.904591118333)) ;
#20736 = CARTESIAN_POINT('Ctrl Pts',(-19.3680954416651,20.3702244734579,124.617184177661)) ;
#20737 = CARTESIAN_POINT('Ctrl Pts',(-19.3577875500338,20.190235393095,124.918525903528)) ;
#20738 = CARTESIAN_POINT('Ctrl Pts',(-19.1584407875054,20.3802724147841,124.591416106205)) ;
#20739 = CARTESIAN_POINT('Ctrl Pts',(-19.0957195762214,20.2002833344212,124.886313111744)) ;
#20740 = CARTESIAN_POINT('Ctrl Pts',(-18.9604121411015,20.3901200485918,124.531032969309)) ;
#20741 = CARTESIAN_POINT('Ctrl Pts',(-18.8481841830687,20.210130968229,124.810831448379)) ;
#20742 = CARTESIAN_POINT('Ctrl Pts',(-18.7734517586268,20.4000817632769,124.436686230099)) ;
#20743 = CARTESIAN_POINT('Ctrl Pts',(-18.6144848557031,20.220092682914,124.692895466025)) ;
#20744 = CARTESIAN_POINT('Ctrl Pts',(-18.604728389867,20.4101103961554,124.310240172556)) ;
#20745 = CARTESIAN_POINT('Ctrl Pts',(-18.4035822760522,20.2301213157925,124.534835645106)) ;
#20746 = CARTESIAN_POINT('Ctrl Pts',(-18.4621885899076,20.4200207216905,124.158296132863)) ;
#20747 = CARTESIAN_POINT('Ctrl Pts',(-18.2254094105789,20.2400316413277,124.34490354003)) ;
#20748 = CARTESIAN_POINT('Ctrl Pts',(-18.3474529168086,20.4299555521623,123.983766306947)) ;
#20749 = CARTESIAN_POINT('Ctrl Pts',(-18.0819921054121,20.2499664717994,124.126739575367)) ;
#20750 = CARTESIAN_POINT('Ctrl Pts',(-18.2640446601778,20.4399968845442,123.789842819283)) ;
#20751 = CARTESIAN_POINT('Ctrl Pts',(-17.9777343205273,20.2600078041814,123.884334153632)) ;
#20752 = CARTESIAN_POINT('Ctrl Pts',(-18.21621844815,20.4498897579831,123.587439108983)) ;
#20753 = CARTESIAN_POINT('Ctrl Pts',(-17.9179543452334,20.2699006776202,123.631328380915)) ;
#20754 = CARTESIAN_POINT('Ctrl Pts',(-18.203638204828,20.459858923801,123.378224162259)) ;
#20755 = CARTESIAN_POINT('Ctrl Pts',(-17.9022315156781,20.2798698434381,123.369810686241)) ;
#20756 = CARTESIAN_POINT('Ctrl Pts',(-18.2280625767773,20.4698876575175,123.168828358653)) ;
#20757 = CARTESIAN_POINT('Ctrl Pts',(-17.9327660607719,20.2898985771546,123.108061591331)) ;
#20758 = CARTESIAN_POINT('Ctrl Pts',(-18.3069889150334,20.4830801762886,122.902870280924)) ;
#20759 = CARTESIAN_POINT('Ctrl Pts',(-18.0314212956118,20.3030910959258,122.775637805959)) ;
#20760 = CARTESIAN_POINT('Ctrl Pts',(-18.4552942626579,20.4964400443313,122.660681326423)) ;
#20761 = CARTESIAN_POINT('Ctrl Pts',(-18.2167817772954,20.3164509639684,122.472918789065)) ;
#20762 = CARTESIAN_POINT('Ctrl Pts',(-18.657015951964,20.5096653814802,122.469309191778)) ;
#20763 = CARTESIAN_POINT('Ctrl Pts',(-18.4689719567282,20.3296763011173,122.233665328807)) ;
#20764 = CARTESIAN_POINT('Ctrl Pts',(-18.8316741273677,20.5196466073208,122.353005072726)) ;
#20765 = CARTESIAN_POINT('Ctrl Pts',(-18.6872891439649,20.3396575269579,122.0882957323)) ;
#20766 = CARTESIAN_POINT('Ctrl Pts',(-19.0250769115555,20.5296821743037,122.268720045023)) ;
#20767 = CARTESIAN_POINT('Ctrl Pts',(-18.9290457583576,20.3496930939408,121.982939786469)) ;
#20768 = CARTESIAN_POINT('Ctrl Pts',(-19.2265825671295,20.5395452522658,122.219728041552)) ;
#20769 = CARTESIAN_POINT('Ctrl Pts',(-19.1809279027677,20.3595561719029,121.921703115503)) ;
#20770 = CARTESIAN_POINT('Ctrl Pts',(-19.4378331047405,20.5496155510669,122.206147359895)) ;
#20771 = CARTESIAN_POINT('Ctrl Pts',(-19.4449915418395,20.369626470704,121.904729894139)) ;
#20772 = CARTESIAN_POINT('Ctrl Pts',(-19.6434998813334,20.5594578496347,122.228940856017)) ;
#20773 = CARTESIAN_POINT('Ctrl Pts',(-19.7020745055463,20.3794687692718,121.933224576347)) ;
#20774 = CARTESIAN_POINT('Ctrl Pts',(-19.8446762990893,20.5694185478045,122.287051453372)) ;
#20775 = CARTESIAN_POINT('Ctrl Pts',(-19.9535442296739,20.3894294674416,122.005865433082)) ;
#20776 = CARTESIAN_POINT('Ctrl Pts',(-20.0339789138857,20.579456581984,122.380301038949)) ;
#20777 = CARTESIAN_POINT('Ctrl Pts',(-20.1901714045228,20.3994675016211,122.122429978516)) ;
#20778 = CARTESIAN_POINT('Ctrl Pts',(-20.2016869726508,20.5893303188304,122.50266789996)) ;
#20779 = CARTESIAN_POINT('Ctrl Pts',(-20.3998046709007,20.4093412384676,122.275390622965)) ;
#20780 = CARTESIAN_POINT('Ctrl Pts',(-20.3484287632797,20.5994021027557,122.65527287763)) ;
#20781 = CARTESIAN_POINT('Ctrl Pts',(-20.5832300951106,20.4194130223928,122.466148916955)) ;
#20782 = CARTESIAN_POINT('Ctrl Pts',(-20.4637684790007,20.6092342239569,122.82682741127)) ;
#20783 = CARTESIAN_POINT('Ctrl Pts',(-20.7274022481108,20.429245143594,122.680593266604)) ;
#20784 = CARTESIAN_POINT('Ctrl Pts',(-20.549786388294,20.6192672479823,123.019405571818)) ;
#20785 = CARTESIAN_POINT('Ctrl Pts',(-20.83492227229,20.4392781676194,122.921317142792)) ;
#20786 = CARTESIAN_POINT('Ctrl Pts',(-20.600454739304,20.629283128179,123.223797814881)) ;
#20787 = CARTESIAN_POINT('Ctrl Pts',(-20.8982551027824,20.4492940478161,123.176808341218)) ;
#20788 = CARTESIAN_POINT('Ctrl Pts',(-20.6150583626326,20.6391666472732,123.431067002261)) ;
#20789 = CARTESIAN_POINT('Ctrl Pts',(-20.9165069215087,20.4591775669103,123.435894221683)) ;
#20790 = CARTESIAN_POINT('Ctrl Pts',(-20.5934884418527,20.6491570596368,123.639971139436)) ;
#20791 = CARTESIAN_POINT('Ctrl Pts',(-20.8895420040221,20.469167979274,123.697025786576)) ;
#20792 = CARTESIAN_POINT('Ctrl Pts',(-20.5172126026985,20.6624202228403,123.908195883155)) ;
#20793 = CARTESIAN_POINT('Ctrl Pts',(-20.7941934591565,20.4824311424774,124.032297261989)) ;
#20794 = CARTESIAN_POINT('Ctrl Pts',(-20.3727499039758,20.6756977930915,124.150760947289)) ;
#20795 = CARTESIAN_POINT('Ctrl Pts',(-20.61364497499,20.4957087127286,124.335469275498)) ;
#20796 = CARTESIAN_POINT('Ctrl Pts',(-20.1718067412588,20.6890280955981,124.346077378148)) ;
#20797 = CARTESIAN_POINT('Ctrl Pts',(-20.3624251620307,20.5090390152352,124.579659196355)) ;
#20798 = CARTESIAN_POINT('Ctrl Pts',(-19.9998354457734,20.6989267774145,124.463273965374)) ;
#20799 = CARTESIAN_POINT('Ctrl Pts',(-20.1474678125217,20.5189376970516,124.726143222167)) ;
#20800 = CARTESIAN_POINT('Ctrl Pts',(-19.8085029004183,20.708916292462,124.549834225346)) ;
#20801 = CARTESIAN_POINT('Ctrl Pts',(-19.9082988338251,20.5289272120991,124.834343756603)) ;
#20802 = CARTESIAN_POINT('Ctrl Pts',(-19.6058699471084,20.718864344237,124.601638834298)) ;
#20803 = CARTESIAN_POINT('Ctrl Pts',(-19.6550087594271,20.5388752638742,124.899096739163)) ;
#20804 = CARTESIAN_POINT('Ctrl Pts',(-19.3975069469639,20.7288057475155,124.617723893743)) ;
#20805 = CARTESIAN_POINT('Ctrl Pts',(-19.3945515389815,20.5488166671527,124.919199688652)) ;
#20806 = CARTESIAN_POINT('Ctrl Pts',(-19.1194310874959,20.7420924122965,124.5908661902)) ;
#20807 = CARTESIAN_POINT('Ctrl Pts',(-19.0469745337114,20.5621033319336,124.885630332357)) ;
#20808 = CARTESIAN_POINT('Ctrl Pts',(-18.7886547609525,20.7587028339513,124.467201444823)) ;
#20809 = CARTESIAN_POINT('Ctrl Pts',(-18.6334863377988,20.5787137535884,124.731039345078)) ;
#20810 = CARTESIAN_POINT('Ctrl Pts',(-18.4662665698674,20.7786140962021,124.192751228819)) ;
#20811 = CARTESIAN_POINT('Ctrl Pts',(-18.2305106418667,20.5986250158392,124.387975748647)) ;
#20812 = CARTESIAN_POINT('Ctrl Pts',(-18.2563995968813,20.7985582253669,123.82423191738)) ;
#20813 = CARTESIAN_POINT('Ctrl Pts',(-17.9681790722083,20.6185691450041,123.927324296484)) ;
#20814 = CARTESIAN_POINT('Ctrl Pts',(-18.1850241779996,20.8184813879721,123.406707624286)) ;
#20815 = CARTESIAN_POINT('Ctrl Pts',(-17.8789643904274,20.6384923076093,123.405418987404)) ;
#20816 = CARTESIAN_POINT('Ctrl Pts',(-18.2596109544151,20.8383715103787,122.990352378829)) ;
#20817 = CARTESIAN_POINT('Ctrl Pts',(-17.9722011638597,20.6583824300158,122.884976490813)) ;
#20818 = CARTESIAN_POINT('Ctrl Pts',(-18.4732404987063,20.8583764639788,122.622607393527)) ;
#20819 = CARTESIAN_POINT('Ctrl Pts',(-18.2392413285999,20.6783873836159,122.425297035635)) ;
#20820 = CARTESIAN_POINT('Ctrl Pts',(-18.7967167999957,20.8782147209944,122.351758323974)) ;
#20821 = CARTESIAN_POINT('Ctrl Pts',(-18.6435876221089,20.6982256406315,122.086739272797)) ;
#20822 = CARTESIAN_POINT('Ctrl Pts',(-19.1960471170997,20.8982090217809,122.206055805286)) ;
#20823 = CARTESIAN_POINT('Ctrl Pts',(-19.1427514572152,20.718219941418,121.904613931299)) ;
#20824 = CARTESIAN_POINT('Ctrl Pts',(-19.6188717893715,20.9180942638254,122.205753928318)) ;
#20825 = CARTESIAN_POINT('Ctrl Pts',(-19.6712810445263,20.7381051834625,121.904239572849)) ;
#20826 = CARTESIAN_POINT('Ctrl Pts',(-20.0166066720332,20.9379692103013,122.348559948617)) ;
#20827 = CARTESIAN_POINT('Ctrl Pts',(-20.168447470455,20.7579801299384,122.082748587511)) ;
#20828 = CARTESIAN_POINT('Ctrl Pts',(-20.3441382460836,20.9580022802424,122.620951616946)) ;
#20829 = CARTESIAN_POINT('Ctrl Pts',(-20.5778609764888,20.7780131998795,122.423240113376)) ;
#20830 = CARTESIAN_POINT('Ctrl Pts',(-20.5570102326951,20.9778907871428,122.986308371611)) ;
#20831 = CARTESIAN_POINT('Ctrl Pts',(-20.8439482662448,20.7979017067799,122.879935963145)) ;
#20832 = CARTESIAN_POINT('Ctrl Pts',(-20.6337603887322,20.9977456469241,123.401507209435)) ;
#20833 = CARTESIAN_POINT('Ctrl Pts',(-20.9398845189848,20.8177565665612,123.398932664504)) ;
#20834 = CARTESIAN_POINT('Ctrl Pts',(-20.5628715307167,21.0177964807118,123.821804823539)) ;
#20835 = CARTESIAN_POINT('Ctrl Pts',(-20.8512719992327,20.8378074003489,123.924305207163)) ;
#20836 = CARTESIAN_POINT('Ctrl Pts',(-20.356096985501,21.037562422601,124.187831810963)) ;
#20837 = CARTESIAN_POINT('Ctrl Pts',(-20.5928049104702,20.8575733422382,124.381835472892)) ;
#20838 = CARTESIAN_POINT('Ctrl Pts',(-20.0335794669859,21.0575751540604,124.465226345288)) ;
#20839 = CARTESIAN_POINT('Ctrl Pts',(-20.1896580437569,20.8775860736975,124.728578782344)) ;
#20840 = CARTESIAN_POINT('Ctrl Pts',(-19.637720643514,21.0774679890039,124.614558860712)) ;
#20841 = CARTESIAN_POINT('Ctrl Pts',(-19.6948360554275,20.8974789086411,124.915243821142)) ;
#20842 = CARTESIAN_POINT('Ctrl Pts',(-19.214589507988,21.0973750123435,124.620545648609)) ;
#20843 = CARTESIAN_POINT('Ctrl Pts',(-19.1659236264529,20.9173859319806,124.922728039924)) ;
#20844 = CARTESIAN_POINT('Ctrl Pts',(-18.8142996405734,21.1172902772442,124.482107958723)) ;
#20845 = CARTESIAN_POINT('Ctrl Pts',(-18.6655619227043,20.9373011968813,124.749682544139)) ;
#20846 = CARTESIAN_POINT('Ctrl Pts',(-18.4838027384896,21.1373219694039,124.213487981599)) ;
#20847 = CARTESIAN_POINT('Ctrl Pts',(-18.2524397020174,20.957332889041,124.413908184194)) ;
#20848 = CARTESIAN_POINT('Ctrl Pts',(-18.2668088815555,21.1571650159769,123.851596586135)) ;
#20849 = CARTESIAN_POINT('Ctrl Pts',(-17.9811972981208,20.977175935614,123.961546540794)) ;
#20850 = CARTESIAN_POINT('Ctrl Pts',(-18.1851023806558,21.1770815638767,123.436137199122)) ;
#20851 = CARTESIAN_POINT('Ctrl Pts',(-17.8790621516814,20.9970924835138,123.442223784006)) ;
#20852 = CARTESIAN_POINT('Ctrl Pts',(-18.2502145798426,21.197013806868,123.017317548737)) ;
#20853 = CARTESIAN_POINT('Ctrl Pts',(-17.9604499278885,21.0170247265051,122.918699625149)) ;
#20854 = CARTESIAN_POINT('Ctrl Pts',(-18.453820244144,21.2169176416773,122.646330539081)) ;
#20855 = CARTESIAN_POINT('Ctrl Pts',(-18.2149540834011,21.0369285613144,122.454965536719)) ;
#20856 = CARTESIAN_POINT('Ctrl Pts',(-18.771411200767,21.2368180418648,122.366728476114)) ;
#20857 = CARTESIAN_POINT('Ctrl Pts',(-18.6119399166127,21.0568289615019,122.105461255144)) ;
#20858 = CARTESIAN_POINT('Ctrl Pts',(-19.1662802143597,21.2567677182441,122.211733257638)) ;
#20859 = CARTESIAN_POINT('Ctrl Pts',(-19.1055245267092,21.0767786378812,121.91171422936)) ;
#20860 = CARTESIAN_POINT('Ctrl Pts',(-19.5899666832492,21.2767002424645,122.200890341999)) ;
#20861 = CARTESIAN_POINT('Ctrl Pts',(-19.6351319246211,21.0967111621016,121.898157078062)) ;
#20862 = CARTESIAN_POINT('Ctrl Pts',(-19.9918071979918,21.2966202514507,122.334860446379)) ;
#20863 = CARTESIAN_POINT('Ctrl Pts',(-20.1374331359232,21.1166311710878,122.065615887878)) ;
#20864 = CARTESIAN_POINT('Ctrl Pts',(-20.3243261883736,21.3165771576268,122.598408286184)) ;
#20865 = CARTESIAN_POINT('Ctrl Pts',(-20.5530840765956,21.136588077264,122.395047352195)) ;
#20866 = CARTESIAN_POINT('Ctrl Pts',(-20.5465500206849,21.3364629971283,122.958223520543)) ;
#20867 = CARTESIAN_POINT('Ctrl Pts',(-20.8308668599276,21.1564739167655,122.844813593085)) ;
#20868 = CARTESIAN_POINT('Ctrl Pts',(-20.6329313729834,21.3564341692642,123.373889795751)) ;
#20869 = CARTESIAN_POINT('Ctrl Pts',(-20.9388483133597,21.1764450889013,123.364394953387)) ;
#20870 = CARTESIAN_POINT('Ctrl Pts',(-20.5733172895036,21.3762483662486,123.791020354018)) ;
#20871 = CARTESIAN_POINT('Ctrl Pts',(-20.8643333248033,21.1962592858857,123.885809151916)) ;
#20872 = CARTESIAN_POINT('Ctrl Pts',(-20.3738339937494,21.3962295522168,124.166047638378)) ;
#20873 = CARTESIAN_POINT('Ctrl Pts',(-20.6149914724651,21.2162404718539,124.35458992427)) ;
#20874 = CARTESIAN_POINT('Ctrl Pts',(-20.1119197884198,21.4128050576061,124.401919568806)) ;
#20875 = CARTESIAN_POINT('Ctrl Pts',(-20.2875771231592,21.2328159772432,124.649450004713)) ;
#20876 = CARTESIAN_POINT('Ctrl Pts',(-19.8627851378671,21.4261145054697,124.529357888635)) ;
#20877 = CARTESIAN_POINT('Ctrl Pts',(-19.976190695121,21.2461254251068,124.808734121278)) ;
#20878 = CARTESIAN_POINT('Ctrl Pts',(-19.5941578117551,21.4394822032463,124.611771760159)) ;
#20879 = CARTESIAN_POINT('Ctrl Pts',(-19.6403422561752,21.2594931228834,124.911767929916)) ;
#20880 = CARTESIAN_POINT('Ctrl Pts',(-19.2437108626746,21.4559727749122,124.6246956008)) ;
#20881 = CARTESIAN_POINT('Ctrl Pts',(-19.2023540010426,21.2759836945493,124.927912591737)) ;
#20882 = CARTESIAN_POINT('Ctrl Pts',(-18.8402511753296,21.475893047245,124.495996346843)) ;
#20883 = CARTESIAN_POINT('Ctrl Pts',(-18.6980130161789,21.2959039668821,124.76705541604)) ;
#20884 = CARTESIAN_POINT('Ctrl Pts',(-18.5605799960303,21.492510082966,124.28007609183)) ;
#20885 = CARTESIAN_POINT('Ctrl Pts',(-18.3484015779916,21.3125210026031,124.497134075246)) ;
#20886 = CARTESIAN_POINT('Ctrl Pts',(-18.3909714744252,21.5058009332471,124.057970104108)) ;
#20887 = CARTESIAN_POINT('Ctrl Pts',(-18.1364098503999,21.3258118528842,124.219524949621)) ;
#20888 = CARTESIAN_POINT('Ctrl Pts',(-18.2945586514006,21.5157699784016,123.871912739408)) ;
#20889 = CARTESIAN_POINT('Ctrl Pts',(-18.0158871388316,21.3357808980387,123.986950081581)) ;
#20890 = CARTESIAN_POINT('Ctrl Pts',(-18.2319181244892,21.5256733690351,123.673331471138)) ;
#20891 = CARTESIAN_POINT('Ctrl Pts',(-17.9375848219816,21.3456842886722,123.7387264045)) ;
#20892 = CARTESIAN_POINT('Ctrl Pts',(-18.2044053248853,21.5357311551478,123.46370878248)) ;
#20893 = CARTESIAN_POINT('Ctrl Pts',(-17.9031917373362,21.355742074785,123.476694986446)) ;
#20894 = CARTESIAN_POINT('Ctrl Pts',(-18.213339943562,21.5455831917976,123.256751493961)) ;
#20895 = CARTESIAN_POINT('Ctrl Pts',(-17.9143537185253,21.3655941114347,123.218009520766)) ;
#20896 = CARTESIAN_POINT('Ctrl Pts',(-18.2735424653214,21.5589483159408,122.982353800711)) ;
#20897 = CARTESIAN_POINT('Ctrl Pts',(-17.9896212280947,21.3789592355779,122.874956968011)) ;
#20898 = CARTESIAN_POINT('Ctrl Pts',(-18.4029674767116,21.5721743789038,122.732632420697)) ;
#20899 = CARTESIAN_POINT('Ctrl Pts',(-18.1513956643206,21.3921852985409,122.562838107837)) ;
#20900 = CARTESIAN_POINT('Ctrl Pts',(-18.5911529593693,21.5854780271861,122.525730956398)) ;
#20901 = CARTESIAN_POINT('Ctrl Pts',(-18.3866109363659,21.4054889468232,122.304222180962)) ;
#20902 = CARTESIAN_POINT('Ctrl Pts',(-18.7572783870989,21.5954695583491,122.397143887496)) ;
#20903 = CARTESIAN_POINT('Ctrl Pts',(-18.5942688365872,21.4154804779862,122.143483381919)) ;
#20904 = CARTESIAN_POINT('Ctrl Pts',(-18.9441977840221,21.6055090061484,122.299154895599)) ;
#20905 = CARTESIAN_POINT('Ctrl Pts',(-18.8279161165822,21.4255199257855,122.020995347853)) ;
#20906 = CARTESIAN_POINT('Ctrl Pts',(-19.1413056725189,21.6153527816622,122.236053528025)) ;
#20907 = CARTESIAN_POINT('Ctrl Pts',(-19.0743002770801,21.4353637012994,121.942115783865)) ;
#20908 = CARTESIAN_POINT('Ctrl Pts',(-19.3492278326637,21.6253384230499,122.207322375982)) ;
#20909 = CARTESIAN_POINT('Ctrl Pts',(-19.3342026170286,21.445349342687,121.90619908811)) ;
#20910 = CARTESIAN_POINT('Ctrl Pts',(-19.5580238062598,21.6352752074117,122.21497981521)) ;
#20911 = CARTESIAN_POINT('Ctrl Pts',(-19.5951977714836,21.4552861270488,121.915768063468)) ;
#20912 = CARTESIAN_POINT('Ctrl Pts',(-19.7645659584739,21.645325041879,122.259368244298)) ;
#20913 = CARTESIAN_POINT('Ctrl Pts',(-19.8533761099886,21.4653359615162,121.971250859302)) ;
#20914 = CARTESIAN_POINT('Ctrl Pts',(-19.9564732011589,21.6551754913822,122.337234509043)) ;
#20915 = CARTESIAN_POINT('Ctrl Pts',(-20.0932613278945,21.4751864110193,122.068581121297)) ;
#20916 = CARTESIAN_POINT('Ctrl Pts',(-20.1343652145138,21.6651475053643,122.448110905834)) ;
#20917 = CARTESIAN_POINT('Ctrl Pts',(-20.3156279272745,21.4851584250014,122.207174295959)) ;
#20918 = CARTESIAN_POINT('Ctrl Pts',(-20.2906914128935,21.6751426632114,122.588577277018)) ;
#20919 = CARTESIAN_POINT('Ctrl Pts',(-20.5110376061981,21.4951535828485,122.382755229701)) ;
#20920 = CARTESIAN_POINT('Ctrl Pts',(-20.4205236147211,21.6851765895751,122.754811362263)) ;
#20921 = CARTESIAN_POINT('Ctrl Pts',(-20.6733301023097,21.5051875092122,122.590546133602)) ;
#20922 = CARTESIAN_POINT('Ctrl Pts',(-20.5180643029118,21.6950322980075,122.937635457501)) ;
#20923 = CARTESIAN_POINT('Ctrl Pts',(-20.7952585397872,21.5150432176446,122.819075138393)) ;
#20924 = CARTESIAN_POINT('Ctrl Pts',(-20.5835791686227,21.7050304473461,123.137322140165)) ;
#20925 = CARTESIAN_POINT('Ctrl Pts',(-20.8771547988309,21.5250413669833,123.068682710145)) ;
#20926 = CARTESIAN_POINT('Ctrl Pts',(-20.6133259213828,21.7149298505197,123.343332794389)) ;
#20927 = CARTESIAN_POINT('Ctrl Pts',(-20.9143410126104,21.5349407701568,123.326195883179)) ;
#20928 = CARTESIAN_POINT('Ctrl Pts',(-20.6067986597741,21.7249810474082,123.554517472211)) ;
#20929 = CARTESIAN_POINT('Ctrl Pts',(-20.9061846999684,21.5449919670453,123.590176807784)) ;
#20930 = CARTESIAN_POINT('Ctrl Pts',(-20.5644486467122,21.734863371221,123.757928803125)) ;
#20931 = CARTESIAN_POINT('Ctrl Pts',(-20.853249823519,21.5548742908582,123.844441837906)) ;
#20932 = CARTESIAN_POINT('Ctrl Pts',(-20.4869932248377,21.7448582668776,123.953249465948)) ;
#20933 = CARTESIAN_POINT('Ctrl Pts',(-20.7564330306425,21.5648691865148,124.088593766656)) ;
#20934 = CARTESIAN_POINT('Ctrl Pts',(-20.376239486151,21.7548793662602,124.132475484503)) ;
#20935 = CARTESIAN_POINT('Ctrl Pts',(-20.6179931768872,21.5748902858973,124.312627761359)) ;
#20936 = CARTESIAN_POINT('Ctrl Pts',(-20.2377724390061,21.7647866341222,124.288062190397)) ;
#20937 = CARTESIAN_POINT('Ctrl Pts',(-20.4449112034606,21.5847975537594,124.507113190861)) ;
#20938 = CARTESIAN_POINT('Ctrl Pts',(-20.0741502835799,21.7747249779475,124.417970243514)) ;
#20939 = CARTESIAN_POINT('Ctrl Pts',(-20.2403849662515,21.5947358975846,124.669500522451)) ;
#20940 = CARTESIAN_POINT('Ctrl Pts',(-19.8892850130631,21.784728397248,124.518280702167)) ;
#20941 = CARTESIAN_POINT('Ctrl Pts',(-20.0093045735368,21.6047393168851,124.79489097273)) ;
#20942 = CARTESIAN_POINT('Ctrl Pts',(-19.6891120590807,21.7947629479551,124.584833460336)) ;
#20943 = CARTESIAN_POINT('Ctrl Pts',(-19.7590892507398,21.6147738675922,124.878084487071)) ;
#20944 = CARTESIAN_POINT('Ctrl Pts',(-19.484395225653,21.8046078975607,124.615389634734)) ;
#20945 = CARTESIAN_POINT('Ctrl Pts',(-19.5031930456652,21.6246188171978,124.916282417656)) ;
#20946 = CARTESIAN_POINT('Ctrl Pts',(-19.2745575619711,21.8145937396736,124.610253310873)) ;
#20947 = CARTESIAN_POINT('Ctrl Pts',(-19.2408957415365,21.6346046593107,124.909864611199)) ;
#20948 = CARTESIAN_POINT('Ctrl Pts',(-19.0697507053397,21.8245285470427,124.569104542372)) ;
#20949 = CARTESIAN_POINT('Ctrl Pts',(-18.9848863453834,21.6445394666798,124.858431106566)) ;
#20950 = CARTESIAN_POINT('Ctrl Pts',(-18.8729297754626,21.834586088756,124.491928841901)) ;
#20951 = CARTESIAN_POINT('Ctrl Pts',(-18.738859338082,21.6545970083931,124.761963952245)) ;
#20952 = CARTESIAN_POINT('Ctrl Pts',(-18.6965214907536,21.8444076862681,124.384579575107)) ;
#20953 = CARTESIAN_POINT('Ctrl Pts',(-18.5183469904694,21.6644186059052,124.627779140097)) ;
#20954 = CARTESIAN_POINT('Ctrl Pts',(-18.5374995717357,21.8544639457486,124.245294446865)) ;
#20955 = CARTESIAN_POINT('Ctrl Pts',(-18.3195680415686,21.6744748653857,124.453674665829)) ;
#20956 = CARTESIAN_POINT('Ctrl Pts',(-18.4068771812102,21.864403882049,124.082167341671)) ;
#20957 = CARTESIAN_POINT('Ctrl Pts',(-18.1562878546674,21.6844148016861,124.249767117428)) ;
#20958 = CARTESIAN_POINT('Ctrl Pts',(-18.3063513222259,21.8743110027934,123.899756894152)) ;
#20959 = CARTESIAN_POINT('Ctrl Pts',(-18.0306281552504,21.6943219224305,124.021754765608)) ;
#20960 = CARTESIAN_POINT('Ctrl Pts',(-18.2381764644266,21.8843539087187,123.699938324222)) ;
#20961 = CARTESIAN_POINT('Ctrl Pts',(-17.9454073048491,21.7043648283558,123.771982422679)) ;
#20962 = CARTESIAN_POINT('Ctrl Pts',(-18.2061259507257,21.8942616898179,123.494118034549)) ;
#20963 = CARTESIAN_POINT('Ctrl Pts',(-17.9053416812303,21.714272609455,123.51470692144)) ;
#20964 = CARTESIAN_POINT('Ctrl Pts',(-18.2099726092004,21.9042720588203,123.283696769241)) ;
#20965 = CARTESIAN_POINT('Ctrl Pts',(-17.9101476585179,21.7242829784574,123.251680239082)) ;
#20966 = CARTESIAN_POINT('Ctrl Pts',(-18.250799150117,21.9143028973891,123.076808306462)) ;
#20967 = CARTESIAN_POINT('Ctrl Pts',(-17.9611784249865,21.7343138170262,122.993069233019)) ;
#20968 = CARTESIAN_POINT('Ctrl Pts',(-18.3252324167252,21.9241557370288,122.88350173726)) ;
#20969 = CARTESIAN_POINT('Ctrl Pts',(-18.0542181019441,21.7441666566659,122.751434398998)) ;
#20970 = CARTESIAN_POINT('Ctrl Pts',(-18.4332250657028,21.9341437381937,122.703441071799)) ;
#20971 = CARTESIAN_POINT('Ctrl Pts',(-18.1892070598107,21.7541546578309,122.526357242308)) ;
#20972 = CARTESIAN_POINT('Ctrl Pts',(-18.5700375225545,21.9440725571729,122.545786789656)) ;
#20973 = CARTESIAN_POINT('Ctrl Pts',(-18.3602212353183,21.76408347681,122.32928753721)) ;
#20974 = CARTESIAN_POINT('Ctrl Pts',(-18.732888520769,21.9540602598952,122.413224493809)) ;
#20975 = CARTESIAN_POINT('Ctrl Pts',(-18.5637837492857,21.7740711795323,122.163582862095)) ;
#20976 = CARTESIAN_POINT('Ctrl Pts',(-18.9173249515201,21.9640962596979,122.31077716545)) ;
#20977 = CARTESIAN_POINT('Ctrl Pts',(-18.7943281092038,21.784107179335,122.035521757821)) ;
#20978 = CARTESIAN_POINT('Ctrl Pts',(-19.1130605451374,21.9739511294993,122.242820238378)) ;
#20979 = CARTESIAN_POINT('Ctrl Pts',(-19.038997751584,21.7939620491364,121.950573239043)) ;
#20980 = CARTESIAN_POINT('Ctrl Pts',(-19.3205261715052,21.9839505599228,122.209124296924)) ;
#20981 = CARTESIAN_POINT('Ctrl Pts',(-19.2983295791008,21.80396147956,121.908451210414)) ;
#20982 = CARTESIAN_POINT('Ctrl Pts',(-19.5285708919945,21.9938456773881,122.211711498228)) ;
#20983 = CARTESIAN_POINT('Ctrl Pts',(-19.5583862373949,21.8138565970253,121.911683181411)) ;
#20984 = CARTESIAN_POINT('Ctrl Pts',(-19.7363587174108,22.0039061709051,122.251037909545)) ;
#20985 = CARTESIAN_POINT('Ctrl Pts',(-19.8181211650492,21.8239170905422,121.96083913654)) ;
#20986 = CARTESIAN_POINT('Ctrl Pts',(-19.9300913010617,22.0137556511063,122.324185172849)) ;
#20987 = CARTESIAN_POINT('Ctrl Pts',(-20.0602885784198,21.8337665707434,122.052271697296)) ;
#20988 = CARTESIAN_POINT('Ctrl Pts',(-20.1116425157324,22.0237821013701,122.431281071649)) ;
#20989 = CARTESIAN_POINT('Ctrl Pts',(-20.2872285089844,21.8437930210072,122.186139952124)) ;
#20990 = CARTESIAN_POINT('Ctrl Pts',(-20.2715450400608,22.0338133918482,122.568785511319)) ;
#20991 = CARTESIAN_POINT('Ctrl Pts',(-20.4871079315352,21.8538243114853,122.35801891506)) ;
#20992 = CARTESIAN_POINT('Ctrl Pts',(-20.4029602797824,22.0436547795,122.728588268752)) ;
#20993 = CARTESIAN_POINT('Ctrl Pts',(-20.6513791646752,21.8636656991371,122.557772038563)) ;
#20994 = CARTESIAN_POINT('Ctrl Pts',(-20.5066507219347,22.0536581803912,122.911527607421)) ;
#20995 = CARTESIAN_POINT('Ctrl Pts',(-20.7809938111829,21.8736691000283,122.786445434062)) ;
#20996 = CARTESIAN_POINT('Ctrl Pts',(-20.5768052643418,22.0636425631824,123.109399042822)) ;
#20997 = CARTESIAN_POINT('Ctrl Pts',(-20.8686887483206,21.8836534828195,123.033784325657)) ;
#20998 = CARTESIAN_POINT('Ctrl Pts',(-20.6115199861339,22.0736816531958,123.317556791633)) ;
#20999 = CARTESIAN_POINT('Ctrl Pts',(-20.9120839655183,21.8936925728329,123.293981074003)) ;
#21000 = CARTESIAN_POINT('Ctrl Pts',(-20.6098913500393,22.0835274621049,123.524555130428)) ;
#21001 = CARTESIAN_POINT('Ctrl Pts',(-20.9100499298834,21.9035383817421,123.552730180815)) ;
#21002 = CARTESIAN_POINT('Ctrl Pts',(-20.5722452970051,22.0935118849239,123.731024894997)) ;
#21003 = CARTESIAN_POINT('Ctrl Pts',(-20.8629939222876,21.9135228045611,123.810817924676)) ;
#21004 = CARTESIAN_POINT('Ctrl Pts',(-20.4997117600218,22.1034515101651,123.927025671405)) ;
#21005 = CARTESIAN_POINT('Ctrl Pts',(-20.7723283116897,21.9234624298023,124.05581995963)) ;
#21006 = CARTESIAN_POINT('Ctrl Pts',(-20.3931662714284,22.1134911996838,124.109206689079)) ;
#21007 = CARTESIAN_POINT('Ctrl Pts',(-20.6391479210158,21.9335021193209,124.283546922036)) ;
#21008 = CARTESIAN_POINT('Ctrl Pts',(-20.2587285375417,22.1233793881024,124.267780927574)) ;
#21009 = CARTESIAN_POINT('Ctrl Pts',(-20.4711013650952,21.9433903077395,124.481766445994)) ;
#21010 = CARTESIAN_POINT('Ctrl Pts',(-20.0974265999504,22.1333689141044,124.402255862019)) ;
#21011 = CARTESIAN_POINT('Ctrl Pts',(-20.2694747065142,21.9533798337416,124.649861363959)) ;
#21012 = CARTESIAN_POINT('Ctrl Pts',(-19.9157102403435,22.1433274154596,124.506217438115)) ;
#21013 = CARTESIAN_POINT('Ctrl Pts',(-20.0423296292845,21.9633383350968,124.779814856002)) ;
#21014 = CARTESIAN_POINT('Ctrl Pts',(-19.7200260725257,22.1532270094633,124.577119056446)) ;
#21015 = CARTESIAN_POINT('Ctrl Pts',(-19.7977240449736,21.9732379291004,124.868443422786)) ;
#21016 = CARTESIAN_POINT('Ctrl Pts',(-19.5119529377031,22.1632748975846,124.61342395275)) ;
#21017 = CARTESIAN_POINT('Ctrl Pts',(-19.5376330731142,21.9832858172217,124.913825837491)) ;
#21018 = CARTESIAN_POINT('Ctrl Pts',(-19.3038874510347,22.1731703228301,124.613217769104)) ;
#21019 = CARTESIAN_POINT('Ctrl Pts',(-19.2775503015537,21.9931812424672,124.913569399124)) ;
#21020 = CARTESIAN_POINT('Ctrl Pts',(-19.0956337768571,22.1832317135307,124.576318144067)) ;
#21021 = CARTESIAN_POINT('Ctrl Pts',(-19.017233305932,22.0032426331678,124.86744619023)) ;
#21022 = CARTESIAN_POINT('Ctrl Pts',(-18.9011658613922,22.1930772972174,124.505398277424)) ;
#21023 = CARTESIAN_POINT('Ctrl Pts',(-18.7741467328486,22.0130882168545,124.778797095436)) ;
#21024 = CARTESIAN_POINT('Ctrl Pts',(-18.7194990589113,22.2030402705266,124.401179624215)) ;
#21025 = CARTESIAN_POINT('Ctrl Pts',(-18.5470623486079,22.0230511901637,124.648524437436)) ;
#21026 = CARTESIAN_POINT('Ctrl Pts',(-18.5578335683124,22.2130659373523,124.265923043721)) ;
#21027 = CARTESIAN_POINT('Ctrl Pts',(-18.3449798305692,22.0330768569895,124.479454619294)) ;
#21028 = CARTESIAN_POINT('Ctrl Pts',(-18.4235409053948,22.2229804152186,124.106527257626)) ;
#21029 = CARTESIAN_POINT('Ctrl Pts',(-18.1771126653133,22.0429913348558,124.28020996493)) ;
#21030 = CARTESIAN_POINT('Ctrl Pts',(-18.3178094286118,22.2329689298936,123.925078039381)) ;
#21031 = CARTESIAN_POINT('Ctrl Pts',(-18.0449474119808,22.0529798495308,124.053398711337)) ;
#21032 = CARTESIAN_POINT('Ctrl Pts',(-18.2452217442394,22.2430130408091,123.726808026642)) ;
#21033 = CARTESIAN_POINT('Ctrl Pts',(-17.954211848732,22.0630239604462,123.805561752125)) ;
#21034 = CARTESIAN_POINT('Ctrl Pts',(-18.2084565806548,22.2528411784036,123.523457249866)) ;
#21035 = CARTESIAN_POINT('Ctrl Pts',(-17.9082542485454,22.0728520980408,123.551371969022)) ;
#21036 = CARTESIAN_POINT('Ctrl Pts',(-18.2074383421507,22.2629177464626,123.311661356134)) ;
#21037 = CARTESIAN_POINT('Ctrl Pts',(-17.9069805912369,22.0829286660997,123.286627562761)) ;
#21038 = CARTESIAN_POINT('Ctrl Pts',(-18.2423241793869,22.2727699083667,123.107451203336)) ;
#21039 = CARTESIAN_POINT('Ctrl Pts',(-17.9505873022016,22.0927808280039,123.031363437666)) ;
#21040 = CARTESIAN_POINT('Ctrl Pts',(-18.3135102543039,22.2828428703236,122.908047647564)) ;
#21041 = CARTESIAN_POINT('Ctrl Pts',(-18.0395690380517,22.1028537899607,122.782109150564)) ;
#21042 = CARTESIAN_POINT('Ctrl Pts',(-18.4158946807527,22.2926854323265,122.728210968454)) ;
#21043 = CARTESIAN_POINT('Ctrl Pts',(-18.1675496052933,22.1126963519636,122.557311692099)) ;
#21044 = CARTESIAN_POINT('Ctrl Pts',(-18.549238880053,22.3026658688203,122.566223969324)) ;
#21045 = CARTESIAN_POINT('Ctrl Pts',(-18.3342296705409,22.1226767884574,122.354827390352)) ;
#21046 = CARTESIAN_POINT('Ctrl Pts',(-18.7095577945463,22.3126841741447,122.429637874185)) ;
#21047 = CARTESIAN_POINT('Ctrl Pts',(-18.5346278830778,22.1326950937818,122.184094281001)) ;
#21048 = CARTESIAN_POINT('Ctrl Pts',(-18.8885239198384,22.3225681380641,122.324009756949)) ;
#21049 = CARTESIAN_POINT('Ctrl Pts',(-18.7583362356547,22.1425790577013,122.052058163512)) ;
#21050 = CARTESIAN_POINT('Ctrl Pts',(-19.0866690738758,22.3326340148027,122.249785568809)) ;
#21051 = CARTESIAN_POINT('Ctrl Pts',(-19.0060171333251,22.1526449344398,121.959277593487)) ;
#21052 = CARTESIAN_POINT('Ctrl Pts',(-19.2900221608687,22.3424731156636,122.211822747741)) ;
#21053 = CARTESIAN_POINT('Ctrl Pts',(-19.2602098520566,22.1624840353007,121.911823353389)) ;
#21054 = CARTESIAN_POINT('Ctrl Pts',(-19.5009224073841,22.3525061985293,122.209172430537)) ;
#21055 = CARTESIAN_POINT('Ctrl Pts',(-19.5238350449174,22.1725171181664,121.908510218283)) ;
#21056 = CARTESIAN_POINT('Ctrl Pts',(-19.7087834710141,22.3625278838048,122.243664453097)) ;
#21057 = CARTESIAN_POINT('Ctrl Pts',(-19.7836614016497,22.1825388034419,121.951624796669)) ;
#21058 = CARTESIAN_POINT('Ctrl Pts',(-19.9045062463924,22.3723945789033,122.312314874088)) ;
#21059 = CARTESIAN_POINT('Ctrl Pts',(-20.0283161574298,22.1924054985404,122.037437936202)) ;
#21060 = CARTESIAN_POINT('Ctrl Pts',(-20.0873367852254,22.3823544686378,122.414394213939)) ;
#21061 = CARTESIAN_POINT('Ctrl Pts',(-20.2568547840646,22.2023653882749,122.165037255751)) ;
#21062 = CARTESIAN_POINT('Ctrl Pts',(-20.2506677841391,22.3923894564633,122.547902606798)) ;
#21063 = CARTESIAN_POINT('Ctrl Pts',(-20.4610185638516,22.2124003761004,122.331922477437)) ;
#21064 = CARTESIAN_POINT('Ctrl Pts',(-20.3865916163423,22.4022761605376,122.705186554573)) ;
#21065 = CARTESIAN_POINT('Ctrl Pts',(-20.6309241388541,22.2222870801747,122.528528183517)) ;
#21066 = CARTESIAN_POINT('Ctrl Pts',(-20.4949858769458,22.4123413047705,122.886876646557)) ;
#21067 = CARTESIAN_POINT('Ctrl Pts',(-20.766416856272,22.2323522244076,122.755640405164)) ;
#21068 = CARTESIAN_POINT('Ctrl Pts',(-20.5687197159867,22.422180595499,123.080175375466)) ;
#21069 = CARTESIAN_POINT('Ctrl Pts',(-20.8585847061565,22.2421915151362,122.997265190441)) ;
#21070 = CARTESIAN_POINT('Ctrl Pts',(-20.6089305970685,22.4322431529375,123.287840199753)) ;
#21071 = CARTESIAN_POINT('Ctrl Pts',(-20.9088481489483,22.2522540725746,123.256845872699)) ;
#21072 = CARTESIAN_POINT('Ctrl Pts',(-20.6121922591228,22.4421402041896,123.495893346216)) ;
#21073 = CARTESIAN_POINT('Ctrl Pts',(-20.9129252441028,22.2621511238267,123.516913308371)) ;
#21074 = CARTESIAN_POINT('Ctrl Pts',(-20.5798565032163,22.4520714109378,123.702154164007)) ;
#21075 = CARTESIAN_POINT('Ctrl Pts',(-20.8725051637196,22.272082330575,123.774739999813)) ;
#21076 = CARTESIAN_POINT('Ctrl Pts',(-20.5112221625243,22.4621135951567,123.901801813168)) ;
#21077 = CARTESIAN_POINT('Ctrl Pts',(-20.786712131682,22.2821245147938,124.024299304319)) ;
#21078 = CARTESIAN_POINT('Ctrl Pts',(-20.4106758088328,22.4720002232676,124.083722626987)) ;
#21079 = CARTESIAN_POINT('Ctrl Pts',(-20.6610284500015,22.2920111429047,124.25170115506)) ;
#21080 = CARTESIAN_POINT('Ctrl Pts',(-20.278945382695,22.4819934958,124.2473690502)) ;
#21081 = CARTESIAN_POINT('Ctrl Pts',(-20.4963649928319,22.3020044154371,124.45625910245)) ;
#21082 = CARTESIAN_POINT('Ctrl Pts',(-20.1215083587096,22.4919385713414,124.384944915974)) ;
#21083 = CARTESIAN_POINT('Ctrl Pts',(-20.2995680280399,22.3119494909786,124.628229064092)) ;
#21084 = CARTESIAN_POINT('Ctrl Pts',(-19.9426983959548,22.5018881220697,124.493496277981)) ;
#21085 = CARTESIAN_POINT('Ctrl Pts',(-20.0760548364874,22.3218990417068,124.763918115327)) ;
#21086 = CARTESIAN_POINT('Ctrl Pts',(-19.7459427076918,22.5119274569177,124.569841858884)) ;
#21087 = CARTESIAN_POINT('Ctrl Pts',(-19.8301102215282,22.3319383765548,124.859349625922)) ;
#21088 = CARTESIAN_POINT('Ctrl Pts',(-19.5420901927288,22.5218135958616,124.610431047829)) ;
#21089 = CARTESIAN_POINT('Ctrl Pts',(-19.5752934234394,22.3418245154987,124.910085821145)) ;
#21090 = CARTESIAN_POINT('Ctrl Pts',(-19.331980404051,22.5318117088353,124.615326987992)) ;
#21091 = CARTESIAN_POINT('Ctrl Pts',(-19.3126560173104,22.3518226284724,124.916205138615)) ;
#21092 = CARTESIAN_POINT('Ctrl Pts',(-19.1257731714612,22.5417314711877,124.584031987848)) ;
#21093 = CARTESIAN_POINT('Ctrl Pts',(-19.0548963059002,22.3617423908249,124.877085616116)) ;
#21094 = CARTESIAN_POINT('Ctrl Pts',(-18.925760197074,22.5517708668004,124.51667777525)) ;
#21095 = CARTESIAN_POINT('Ctrl Pts',(-18.8048804750818,22.3717817864375,124.792892259255)) ;
#21096 = CARTESIAN_POINT('Ctrl Pts',(-18.7429037014523,22.5616800525887,124.416866967638)) ;
#21097 = CARTESIAN_POINT('Ctrl Pts',(-18.5763093840162,22.3816909722258,124.668127742339)) ;
#21098 = CARTESIAN_POINT('Ctrl Pts',(-18.579362600272,22.5716152367462,124.286939430316)) ;
#21099 = CARTESIAN_POINT('Ctrl Pts',(-18.3718830460784,22.3916261563833,124.505717216813)) ;
#21100 = CARTESIAN_POINT('Ctrl Pts',(-18.4395493540934,22.5816562941321,124.128790649976)) ;
#21101 = CARTESIAN_POINT('Ctrl Pts',(-18.1971172156532,22.4016672137692,124.308030847448)) ;
#21102 = CARTESIAN_POINT('Ctrl Pts',(-18.3308735820911,22.5915434521654,123.951591507098)) ;
#21103 = CARTESIAN_POINT('Ctrl Pts',(-18.0612726927552,22.4115543718025,124.086530580778)) ;
#21104 = CARTESIAN_POINT('Ctrl Pts',(-18.253489695394,22.6015357318413,123.756310473585)) ;
#21105 = CARTESIAN_POINT('Ctrl Pts',(-17.9645436848904,22.4215466514784,123.842428732897)) ;
#21106 = CARTESIAN_POINT('Ctrl Pts',(-18.2114252982926,22.6114842488863,123.551423040072)) ;
#21107 = CARTESIAN_POINT('Ctrl Pts',(-17.9119640315032,22.4314951685235,123.586318714181)) ;
#21108 = CARTESIAN_POINT('Ctrl Pts',(-18.2052879099196,22.6214210264567,123.342628586766)) ;
#21109 = CARTESIAN_POINT('Ctrl Pts',(-17.9042933598069,22.4414319460939,123.325324977717)) ;
#21110 = CARTESIAN_POINT('Ctrl Pts',(-18.2353818524349,22.6314040626037,123.134895795784)) ;
#21111 = CARTESIAN_POINT('Ctrl Pts',(-17.9419119920911,22.4514149822408,123.065658904093)) ;
#21112 = CARTESIAN_POINT('Ctrl Pts',(-18.3018390798526,22.6414478141974,122.934500268376)) ;
#21113 = CARTESIAN_POINT('Ctrl Pts',(-18.0249844510094,22.4614587338345,122.815165001349)) ;
#21114 = CARTESIAN_POINT('Ctrl Pts',(-18.3995334670519,22.65127634341,122.752393803793)) ;
#21115 = CARTESIAN_POINT('Ctrl Pts',(-18.1471041894676,22.4712872630471,122.587531223368)) ;
#21116 = CARTESIAN_POINT('Ctrl Pts',(-18.5304390769983,22.6613517043187,122.585924560108)) ;
#21117 = CARTESIAN_POINT('Ctrl Pts',(-18.310736925562,22.4813626239558,122.379445782567)) ;
#21118 = CARTESIAN_POINT('Ctrl Pts',(-18.6848484847896,22.6712083032059,122.447668513297)) ;
#21119 = CARTESIAN_POINT('Ctrl Pts',(-18.5037504475988,22.491219222843,122.2066258693)) ;
#21120 = CARTESIAN_POINT('Ctrl Pts',(-18.8644168488015,22.6812712972238,122.335891874011)) ;
#21121 = CARTESIAN_POINT('Ctrl Pts',(-18.7282113464719,22.5012822168609,122.066906399844)) ;
#21122 = CARTESIAN_POINT('Ctrl Pts',(-19.0571331275604,22.6911492315132,122.25842835509)) ;
#21123 = CARTESIAN_POINT('Ctrl Pts',(-18.9691081441337,22.5111601511503,121.970077874885)) ;
#21124 = CARTESIAN_POINT('Ctrl Pts',(-19.2627566660564,22.7011498790713,122.214769477626)) ;
#21125 = CARTESIAN_POINT('Ctrl Pts',(-19.2261379991879,22.5211607987084,121.915505689096)) ;
#21126 = CARTESIAN_POINT('Ctrl Pts',(-19.4711669419206,22.7110677255094,122.207377365738)) ;
#21127 = CARTESIAN_POINT('Ctrl Pts',(-19.4866516087189,22.5310786451465,121.906267040837)) ;
#21128 = CARTESIAN_POINT('Ctrl Pts',(-19.6803914078797,22.721118842515,122.236721719079)) ;
#21129 = CARTESIAN_POINT('Ctrl Pts',(-19.7481817747748,22.5411297621521,121.942948938101)) ;
#21130 = CARTESIAN_POINT('Ctrl Pts',(-19.8778768048327,22.7309895778256,122.300577463833)) ;
#21131 = CARTESIAN_POINT('Ctrl Pts',(-19.9950390178656,22.5510004974627,122.022770439589)) ;
#21132 = CARTESIAN_POINT('Ctrl Pts',(-20.0649458105329,22.7410602850686,122.39964958428)) ;
#21133 = CARTESIAN_POINT('Ctrl Pts',(-20.2288742155722,22.5610712047057,122.146611832965)) ;
#21134 = CARTESIAN_POINT('Ctrl Pts',(-20.2281280729297,22.7508932925205,122.526586135203)) ;
#21135 = CARTESIAN_POINT('Ctrl Pts',(-20.432852059648,22.5709042121576,122.305284591667)) ;
#21136 = CARTESIAN_POINT('Ctrl Pts',(-20.3700041193385,22.7609237848228,122.682583660361)) ;
#21137 = CARTESIAN_POINT('Ctrl Pts',(-20.6101957114275,22.5809347044599,122.50028265826)) ;
#21138 = CARTESIAN_POINT('Ctrl Pts',(-20.4821412733727,22.7709553798962,122.861209839806)) ;
#21139 = CARTESIAN_POINT('Ctrl Pts',(-20.7503657377508,22.5909662995333,122.723566173364)) ;
#21140 = CARTESIAN_POINT('Ctrl Pts',(-20.5603509074772,22.7807850790344,123.052474175343)) ;
#21141 = CARTESIAN_POINT('Ctrl Pts',(-20.848126630718,22.6007959986715,122.962648437251)) ;
#21142 = CARTESIAN_POINT('Ctrl Pts',(-20.6054919636736,22.790774528916,123.257581426922)) ;
#21143 = CARTESIAN_POINT('Ctrl Pts',(-20.904551077241,22.6107854485531,123.219033095629)) ;
#21144 = CARTESIAN_POINT('Ctrl Pts',(-20.6138461179592,22.8008183867317,123.468567262756)) ;
#21145 = CARTESIAN_POINT('Ctrl Pts',(-20.9149919746047,22.6208293063688,123.482765312887)) ;
#21146 = CARTESIAN_POINT('Ctrl Pts',(-20.5864922399839,22.8106400773219,123.673230555573)) ;
#21147 = CARTESIAN_POINT('Ctrl Pts',(-20.8807975538298,22.630650996959,123.738595413769)) ;
#21148 = CARTESIAN_POINT('Ctrl Pts',(-20.5231490604348,22.8206751678623,123.874462180045)) ;
#21149 = CARTESIAN_POINT('Ctrl Pts',(-20.8016166335874,22.6406860874994,123.990134218036)) ;
#21150 = CARTESIAN_POINT('Ctrl Pts',(-20.4254247657349,22.830699686845,124.061198211658)) ;
#21151 = CARTESIAN_POINT('Ctrl Pts',(-20.6794595798729,22.6507106064821,124.223553358068)) ;
#21152 = CARTESIAN_POINT('Ctrl Pts',(-20.2991731667971,22.8405595322552,124.225579994862)) ;
#21153 = CARTESIAN_POINT('Ctrl Pts',(-20.5216428899484,22.6605704518923,124.429030130044)) ;
#21154 = CARTESIAN_POINT('Ctrl Pts',(-20.1451242577046,22.8505193085708,124.367400091411)) ;
#21155 = CARTESIAN_POINT('Ctrl Pts',(-20.3290800370369,22.670530228208,124.606303874563)) ;
#21156 = CARTESIAN_POINT('Ctrl Pts',(-19.9674278032907,22.8605475058855,124.480844125221)) ;
#21157 = CARTESIAN_POINT('Ctrl Pts',(-20.1069583810948,22.6805584255226,124.748107125882)) ;
#21158 = CARTESIAN_POINT('Ctrl Pts',(-19.7751521418593,22.8704550481758,124.56097363697)) ;
#21159 = CARTESIAN_POINT('Ctrl Pts',(-19.8666123895492,22.6904659678129,124.848267265594)) ;
#21160 = CARTESIAN_POINT('Ctrl Pts',(-19.5693646949917,22.8804876987396,124.607138562997)) ;
#21161 = CARTESIAN_POINT('Ctrl Pts',(-19.6093776535577,22.7004986183768,124.905971284957)) ;
#21162 = CARTESIAN_POINT('Ctrl Pts',(-19.3617911177059,22.8903716551663,124.616789062193)) ;
#21163 = CARTESIAN_POINT('Ctrl Pts',(-19.349909838197,22.7103825748034,124.918032249207)) ;
#21164 = CARTESIAN_POINT('Ctrl Pts',(-19.1534263144048,22.9003613565281,124.590486564837)) ;
#21165 = CARTESIAN_POINT('Ctrl Pts',(-19.0894539708058,22.7203722761653,124.88515179817)) ;
#21166 = CARTESIAN_POINT('Ctrl Pts',(-18.9518995245256,22.9104023518042,124.527657154102)) ;
#21167 = CARTESIAN_POINT('Ctrl Pts',(-18.8375462307077,22.7304132714413,124.806612946757)) ;
#21168 = CARTESIAN_POINT('Ctrl Pts',(-18.768077928406,22.9202352410725,124.433102961583)) ;
#21169 = CARTESIAN_POINT('Ctrl Pts',(-18.6077694357356,22.7402461607097,124.68841772116)) ;
#21170 = CARTESIAN_POINT('Ctrl Pts',(-18.6004184578311,22.93022839944,124.306510185862)) ;
#21171 = CARTESIAN_POINT('Ctrl Pts',(-18.3981964690907,22.7502393190771,124.530174726569)) ;
#21172 = CARTESIAN_POINT('Ctrl Pts',(-18.4570423276391,22.9402604417921,124.151821923113)) ;
#21173 = CARTESIAN_POINT('Ctrl Pts',(-18.2189780474116,22.7602713614292,124.336812835409)) ;
#21174 = CARTESIAN_POINT('Ctrl Pts',(-18.3444002375447,22.9501256857505,123.977691444909)) ;
#21175 = CARTESIAN_POINT('Ctrl Pts',(-18.078177052041,22.7701366053876,124.11914781899)) ;
#21176 = CARTESIAN_POINT('Ctrl Pts',(-18.2623606113742,22.9600875769965,123.78499218241)) ;
#21177 = CARTESIAN_POINT('Ctrl Pts',(-17.9756297430813,22.7800984966336,123.878272519234)) ;
#21178 = CARTESIAN_POINT('Ctrl Pts',(-18.2150170839736,22.970122477015,123.579418516963)) ;
#21179 = CARTESIAN_POINT('Ctrl Pts',(-17.9164527324428,22.7901333966521,123.621304920688)) ;
#21180 = CARTESIAN_POINT('Ctrl Pts',(-18.2039051887294,22.9800075574296,123.371873650446)) ;
#21181 = CARTESIAN_POINT('Ctrl Pts',(-17.9025653496462,22.8000184770667,123.361873137659)) ;
#21182 = CARTESIAN_POINT('Ctrl Pts',(-18.2294709369507,22.9900727295544,123.161850154122)) ;
#21183 = CARTESIAN_POINT('Ctrl Pts',(-17.9345250196897,22.8100836491915,123.099344214703)) ;
#21184 = CARTESIAN_POINT('Ctrl Pts',(-18.2896793781521,22.9999199642779,122.963757686704)) ;
#21185 = CARTESIAN_POINT('Ctrl Pts',(-18.0097882001565,22.819930883915,122.851728714304)) ;
#21186 = CARTESIAN_POINT('Ctrl Pts',(-18.3846575460078,23.0099507755956,122.775493829682)) ;
#21187 = CARTESIAN_POINT('Ctrl Pts',(-18.1285132437623,22.8299616952328,122.616400101498)) ;
#21188 = CARTESIAN_POINT('Ctrl Pts',(-18.5109834152174,23.0199603915091,122.607165887845)) ;
#21189 = CARTESIAN_POINT('Ctrl Pts',(-18.2864226563192,22.8399713111463,122.40599165732)) ;
#21190 = CARTESIAN_POINT('Ctrl Pts',(-18.6629287718639,23.0298711709128,122.464629523893)) ;
#21191 = CARTESIAN_POINT('Ctrl Pts',(-18.4763564295643,22.84988209055,122.227822802769)) ;
#21192 = CARTESIAN_POINT('Ctrl Pts',(-18.8373784129168,23.0398004367019,122.349974057845)) ;
#21193 = CARTESIAN_POINT('Ctrl Pts',(-18.6944202111758,22.859811356339,122.084505529354)) ;
#21194 = CARTESIAN_POINT('Ctrl Pts',(-19.0313295538799,23.0498431300145,122.266578270263)) ;
#21195 = CARTESIAN_POINT('Ctrl Pts',(-18.9368601501301,22.8698540496516,121.980263237278)) ;
#21196 = CARTESIAN_POINT('Ctrl Pts',(-19.2336083459502,23.0597296627092,122.218742068884)) ;
#21197 = CARTESIAN_POINT('Ctrl Pts',(-19.1897096706424,22.8797405823464,121.920470478153)) ;
#21198 = CARTESIAN_POINT('Ctrl Pts',(-19.4433140464625,23.0697228078125,122.206271347254)) ;
#21199 = CARTESIAN_POINT('Ctrl Pts',(-19.4518420605083,22.8897337274496,121.904884777647)) ;
#21200 = CARTESIAN_POINT('Ctrl Pts',(-19.6510110881743,23.0796684884866,122.230368010918)) ;
#21201 = CARTESIAN_POINT('Ctrl Pts',(-19.7114632832621,22.8996794081237,121.935008316747)) ;
#21202 = CARTESIAN_POINT('Ctrl Pts',(-19.8515326787835,23.0896157461133,122.289763971548)) ;
#21203 = CARTESIAN_POINT('Ctrl Pts',(-19.9621146837926,22.9096266657504,122.009255961602)) ;
#21204 = CARTESIAN_POINT('Ctrl Pts',(-20.0404673828271,23.0996636482348,122.38422357924)) ;
#21205 = CARTESIAN_POINT('Ctrl Pts',(-20.1982818352397,22.9196745678719,122.127332902665)) ;
#21206 = CARTESIAN_POINT('Ctrl Pts',(-20.2068601688876,23.1095113538565,122.507411205616)) ;
#21207 = CARTESIAN_POINT('Ctrl Pts',(-20.4062715090379,22.9295222734936,122.281319880695)) ;
#21208 = CARTESIAN_POINT('Ctrl Pts',(-20.3514553093839,23.1194728204906,122.658891921361)) ;
#21209 = CARTESIAN_POINT('Ctrl Pts',(-20.5870134936696,22.9394837401277,122.470672801482)) ;
#21210 = CARTESIAN_POINT('Ctrl Pts',(-20.4681173020612,23.1295023737588,122.83453984717)) ;
#21211 = CARTESIAN_POINT('Ctrl Pts',(-20.7328386955894,22.9495132933959,122.690234279952)) ;
#21212 = CARTESIAN_POINT('Ctrl Pts',(-20.5515843547797,23.1394092657862,123.025360354087)) ;
#21213 = CARTESIAN_POINT('Ctrl Pts',(-20.8371700436695,22.9594201854233,122.928761227148)) ;
#21214 = CARTESIAN_POINT('Ctrl Pts',(-20.6012418234421,23.1493569098992,123.228492863603)) ;
#21215 = CARTESIAN_POINT('Ctrl Pts',(-20.8992391770811,22.9693678295363,123.182677656175)) ;
#21216 = CARTESIAN_POINT('Ctrl Pts',(-20.6150800343719,23.1593569529281,123.438296909276)) ;
#21217 = CARTESIAN_POINT('Ctrl Pts',(-20.9165341377211,22.9793678725652,123.444932969306)) ;
#21218 = CARTESIAN_POINT('Ctrl Pts',(-20.5918224314329,23.1693957189221,123.648041713659)) ;
#21219 = CARTESIAN_POINT('Ctrl Pts',(-20.8874593437994,22.9894066385592,123.707113721901)) ;
#21220 = CARTESIAN_POINT('Ctrl Pts',(-20.5341745069886,23.1792207809443,123.846402561714)) ;
#21221 = CARTESIAN_POINT('Ctrl Pts',(-20.8153966815368,22.9992317005814,123.955064177239)) ;
#21222 = CARTESIAN_POINT('Ctrl Pts',(-20.4411557623912,23.1892753282707,124.036199337756)) ;
#21223 = CARTESIAN_POINT('Ctrl Pts',(-20.6991206973961,23.0092862479078,124.192308936938)) ;
#21224 = CARTESIAN_POINT('Ctrl Pts',(-20.3176702770705,23.1992185717199,124.204874255302)) ;
#21225 = CARTESIAN_POINT('Ctrl Pts',(-20.5447615013441,23.019229491357,124.403151003466)) ;
#21226 = CARTESIAN_POINT('Ctrl Pts',(-20.1678477489804,23.2091207433278,124.349412148835)) ;
#21227 = CARTESIAN_POINT('Ctrl Pts',(-20.357481348229,23.0291316629649,124.583821375332)) ;
#21228 = CARTESIAN_POINT('Ctrl Pts',(-19.9925143602655,23.219173578938,124.467395725293)) ;
#21229 = CARTESIAN_POINT('Ctrl Pts',(-20.1383129462667,23.0391844985751,124.731298547748)) ;
#21230 = CARTESIAN_POINT('Ctrl Pts',(-19.8028310164097,23.2290466366235,124.551692861004)) ;
#21231 = CARTESIAN_POINT('Ctrl Pts',(-19.9012076725115,23.0490575562606,124.836667408501)) ;
#21232 = CARTESIAN_POINT('Ctrl Pts',(-19.599035620592,23.2390418981492,124.602895730111)) ;
#21233 = CARTESIAN_POINT('Ctrl Pts',(-19.6464624451115,23.0590528177863,124.90066823185)) ;
#21234 = CARTESIAN_POINT('Ctrl Pts',(-19.3887803257811,23.2490672675697,124.617604462307)) ;
#21235 = CARTESIAN_POINT('Ctrl Pts',(-19.3836439744441,23.0690781872068,124.919051527796)) ;
#21236 = CARTESIAN_POINT('Ctrl Pts',(-19.1819671042923,23.2589571000963,124.596152765897)) ;
#21237 = CARTESIAN_POINT('Ctrl Pts',(-19.1251242692714,23.0789680197334,124.892233416081)) ;
#21238 = CARTESIAN_POINT('Ctrl Pts',(-18.9130557461595,23.2722550709057,124.5197923832)) ;
#21239 = CARTESIAN_POINT('Ctrl Pts',(-18.7890035337137,23.0922659905428,124.796782825436)) ;
#21240 = CARTESIAN_POINT('Ctrl Pts',(-18.6717587243513,23.2854534660148,124.376385706573)) ;
#21241 = CARTESIAN_POINT('Ctrl Pts',(-18.4874072190834,23.105464385652,124.617549791502)) ;
#21242 = CARTESIAN_POINT('Ctrl Pts',(-18.4752682237642,23.2988489082943,124.174730150354)) ;
#21243 = CARTESIAN_POINT('Ctrl Pts',(-18.2417519026231,23.1188598279314,124.365440342986)) ;
#21244 = CARTESIAN_POINT('Ctrl Pts',(-18.358218981122,23.3087247465333,124.00319866305)) ;
#21245 = CARTESIAN_POINT('Ctrl Pts',(-18.0954516814504,23.1287356661704,124.151032241541)) ;
#21246 = CARTESIAN_POINT('Ctrl Pts',(-18.2710692283596,23.318786149131,123.810502936059)) ;
#21247 = CARTESIAN_POINT('Ctrl Pts',(-17.9865146772214,23.1387970687681,123.910158781384)) ;
#21248 = CARTESIAN_POINT('Ctrl Pts',(-18.2196477196924,23.3286512060661,123.609550825009)) ;
#21249 = CARTESIAN_POINT('Ctrl Pts',(-17.922240462111,23.1486621257033,123.658970587668)) ;
#21250 = CARTESIAN_POINT('Ctrl Pts',(-18.2032931252815,23.3386633020149,123.399733102314)) ;
#21251 = CARTESIAN_POINT('Ctrl Pts',(-17.9018022904604,23.1586742216521,123.396691351192)) ;
#21252 = CARTESIAN_POINT('Ctrl Pts',(-18.2303090879066,23.3519406111604,123.121854743172)) ;
#21253 = CARTESIAN_POINT('Ctrl Pts',(-17.9355630207714,23.1719515307975,123.049376976604)) ;
#21254 = CARTESIAN_POINT('Ctrl Pts',(-18.3537865412185,23.3685396366677,122.791280328664)) ;
#21255 = CARTESIAN_POINT('Ctrl Pts',(-18.0899419028751,23.1885505563048,122.636110521846)) ;
#21256 = CARTESIAN_POINT('Ctrl Pts',(-18.5826974213556,23.3851386847007,122.522589585536)) ;
#21257 = CARTESIAN_POINT('Ctrl Pts',(-18.3760258329839,23.2051496043378,122.300311520429)) ;
#21258 = CARTESIAN_POINT('Ctrl Pts',(-18.8116870577227,23.3983820967316,122.364269542791)) ;
#21259 = CARTESIAN_POINT('Ctrl Pts',(-18.6623130734036,23.2183930163688,122.102367993719)) ;
#21260 = CARTESIAN_POINT('Ctrl Pts',(-19.0034183423248,23.4084195244201,122.276133501985)) ;
#21261 = CARTESIAN_POINT('Ctrl Pts',(-18.9019676656497,23.2284304440572,121.992209381467)) ;
#21262 = CARTESIAN_POINT('Ctrl Pts',(-19.2048395995662,23.4183238263757,122.223371608911)) ;
#21263 = CARTESIAN_POINT('Ctrl Pts',(-19.1537511180854,23.2383347460128,121.926257438649)) ;
#21264 = CARTESIAN_POINT('Ctrl Pts',(-19.4827891473364,23.4315906663508,122.19988920511)) ;
#21265 = CARTESIAN_POINT('Ctrl Pts',(-19.5011668383559,23.251601585988,121.896906683047)) ;
#21266 = CARTESIAN_POINT('Ctrl Pts',(-19.8307318849537,23.4482168644408,122.262263108639)) ;
#21267 = CARTESIAN_POINT('Ctrl Pts',(-19.9361152832958,23.2682277840779,121.974875772965)) ;
#21268 = CARTESIAN_POINT('Ctrl Pts',(-20.1971528166808,23.4681359798242,122.474678281948)) ;
#21269 = CARTESIAN_POINT('Ctrl Pts',(-20.394142712814,23.2881468994613,122.240416456631)) ;
#21270 = CARTESIAN_POINT('Ctrl Pts',(-20.4241051193176,23.4847424029584,122.745236826327)) ;
#21271 = CARTESIAN_POINT('Ctrl Pts',(-20.6777956763041,23.3047533225956,122.578559316856)) ;
#21272 = CARTESIAN_POINT('Ctrl Pts',(-20.5421768965827,23.4980386234541,122.998554900509)) ;
#21273 = CARTESIAN_POINT('Ctrl Pts',(-20.8254141685684,23.3180495430913,122.895260367424)) ;
#21274 = CARTESIAN_POINT('Ctrl Pts',(-20.614959986531,23.5113074557956,123.267928258052)) ;
#21275 = CARTESIAN_POINT('Ctrl Pts',(-20.9163840285696,23.3313183754327,123.231954203337)) ;
#21276 = CARTESIAN_POINT('Ctrl Pts',(-20.6152647113257,23.5279987038287,123.622730942973)) ;
#21277 = CARTESIAN_POINT('Ctrl Pts',(-20.9167633041339,23.3480096234658,123.675476169135)) ;
#21278 = CARTESIAN_POINT('Ctrl Pts',(-20.4722994274042,23.5478084355015,124.018996186989)) ;
#21279 = CARTESIAN_POINT('Ctrl Pts',(-20.7380527826187,23.3678193551386,124.170798980292)) ;
#21280 = CARTESIAN_POINT('Ctrl Pts',(-20.2010981674225,23.56778604283,124.345907252259)) ;
#21281 = CARTESIAN_POINT('Ctrl Pts',(-20.3990487800684,23.3877969624672,124.579436972735)) ;
#21282 = CARTESIAN_POINT('Ctrl Pts',(-19.8351962742171,23.5877123518879,124.559408382312)) ;
#21283 = CARTESIAN_POINT('Ctrl Pts',(-19.9416700356385,23.407723271525,124.846309372867)) ;
#21284 = CARTESIAN_POINT('Ctrl Pts',(-19.4207969533748,23.6075292120526,124.636299831341)) ;
#21285 = CARTESIAN_POINT('Ctrl Pts',(-19.423672280542,23.4275401316897,124.942420637845)) ;
#21286 = CARTESIAN_POINT('Ctrl Pts',(-18.9994637731957,23.6276290276466,124.565563992342)) ;
#21287 = CARTESIAN_POINT('Ctrl Pts',(-18.897005210854,23.4476399472837,124.853997620555)) ;
#21288 = CARTESIAN_POINT('Ctrl Pts',(-18.6335253229913,23.6473859915291,124.358902751464)) ;
#21289 = CARTESIAN_POINT('Ctrl Pts',(-18.4395858732156,23.4673969111663,124.595670036021)) ;
#21290 = CARTESIAN_POINT('Ctrl Pts',(-18.3557767431134,23.6674229175986,124.036039149984)) ;
#21291 = CARTESIAN_POINT('Ctrl Pts',(-18.0924014778527,23.4874338372357,124.192088863914)) ;
#21292 = CARTESIAN_POINT('Ctrl Pts',(-18.2066700929233,23.6872924999801,123.640628669761)) ;
#21293 = CARTESIAN_POINT('Ctrl Pts',(-17.9060208621862,23.5073034196172,123.697826439083)) ;
#21294 = CARTESIAN_POINT('Ctrl Pts',(-18.20037309154,23.7071970717333,123.217532309015)) ;
#21295 = CARTESIAN_POINT('Ctrl Pts',(-17.8981510516399,23.5272079913704,123.168957382108)) ;
#21296 = CARTESIAN_POINT('Ctrl Pts',(-18.3392583799834,23.7271496739318,122.816587599737)) ;
#21297 = CARTESIAN_POINT('Ctrl Pts',(-18.0717585757874,23.5471605935689,122.667777463739)) ;
#21298 = CARTESIAN_POINT('Ctrl Pts',(-18.6060586541103,23.747059164902,122.488027614891)) ;
#21299 = CARTESIAN_POINT('Ctrl Pts',(-18.4052588840874,23.5670700845392,122.257079257931)) ;
#21300 = CARTESIAN_POINT('Ctrl Pts',(-18.9674540788008,23.7669105336015,122.269754789477)) ;
#21301 = CARTESIAN_POINT('Ctrl Pts',(-18.8570010753677,23.5869214532386,121.984239388305)) ;
#21302 = CARTESIAN_POINT('Ctrl Pts',(-19.3863467957852,23.7869907297375,122.187619791407)) ;
#21303 = CARTESIAN_POINT('Ctrl Pts',(-19.3806182677798,23.6070016493746,121.881570519937)) ;
#21304 = CARTESIAN_POINT('Ctrl Pts',(-19.8024562321169,23.8067916733129,122.25247266476)) ;
#21305 = CARTESIAN_POINT('Ctrl Pts',(-19.9007519851589,23.62680259295,121.962636023239)) ;
#21306 = CARTESIAN_POINT('Ctrl Pts',(-20.1751703809712,23.8267756498224,122.456380190659)) ;
#21307 = CARTESIAN_POINT('Ctrl Pts',(-20.366645013507,23.6467865694595,122.217519363045)) ;
#21308 = CARTESIAN_POINT('Ctrl Pts',(-20.4545225997992,23.846691612798,122.774634398599)) ;
#21309 = CARTESIAN_POINT('Ctrl Pts',(-20.7158350928187,23.6667025324351,122.615335633075)) ;
#21310 = CARTESIAN_POINT('Ctrl Pts',(-20.6092694572912,23.8665620476199,123.167863522626)) ;
#21311 = CARTESIAN_POINT('Ctrl Pts',(-20.909269753505,23.686572967257,123.106869748193)) ;
#21312 = CARTESIAN_POINT('Ctrl Pts',(-20.6199224875745,23.886612332853,123.593929804403)) ;
#21313 = CARTESIAN_POINT('Ctrl Pts',(-20.922587690353,23.7066232524901,123.639453176953)) ;
#21314 = CARTESIAN_POINT('Ctrl Pts',(-20.4868864023955,23.9063863016123,123.992954670448)) ;
#21315 = CARTESIAN_POINT('Ctrl Pts',(-20.7562955195823,23.7263972212494,124.138232320058)) ;
#21316 = CARTESIAN_POINT('Ctrl Pts',(-20.2223831801166,23.9264427597318,124.327253105703)) ;
#21317 = CARTESIAN_POINT('Ctrl Pts',(-20.4256681461167,23.746453679369,124.556107455173)) ;
#21318 = CARTESIAN_POINT('Ctrl Pts',(-19.8640850949148,23.9462376427228,124.548331334748)) ;
#21319 = CARTESIAN_POINT('Ctrl Pts',(-19.9777988611578,23.76624856236,124.832456311627)) ;
#21320 = CARTESIAN_POINT('Ctrl Pts',(-19.448727810941,23.9662042980252,124.63574281183)) ;
#21321 = CARTESIAN_POINT('Ctrl Pts',(-19.4586032621524,23.7862152176623,124.941723989977)) ;
#21322 = CARTESIAN_POINT('Ctrl Pts',(-19.0285651397822,23.9861632681017,124.575472295223)) ;
#21323 = CARTESIAN_POINT('Ctrl Pts',(-18.9333997951415,23.8061741877388,124.86638911577)) ;
#21324 = CARTESIAN_POINT('Ctrl Pts',(-18.6553168032142,24.0060593556918,124.376389568719)) ;
#21325 = CARTESIAN_POINT('Ctrl Pts',(-18.466838553606,23.8260702753289,124.617539311619)) ;
#21326 = CARTESIAN_POINT('Ctrl Pts',(-18.3720148561307,24.0259575256034,124.062201487962)) ;
#21327 = CARTESIAN_POINT('Ctrl Pts',(-18.1127087822637,23.8459684452405,124.224807490326)) ;
#21328 = CARTESIAN_POINT('Ctrl Pts',(-18.2124303919169,24.0458633609705,123.67015401321)) ;
#21329 = CARTESIAN_POINT('Ctrl Pts',(-17.9132245363324,23.8658742806076,123.734750368409)) ;
#21330 = CARTESIAN_POINT('Ctrl Pts',(-18.1961880168038,24.0658132859084,123.246313641307)) ;
#21331 = CARTESIAN_POINT('Ctrl Pts',(-17.8929172316979,23.8858242055455,123.204950398228)) ;
#21332 = CARTESIAN_POINT('Ctrl Pts',(-18.3247423088814,24.0856924758188,122.84360479257)) ;
#21333 = CARTESIAN_POINT('Ctrl Pts',(-18.0536055022471,23.9057033954559,122.701563671004)) ;
#21334 = CARTESIAN_POINT('Ctrl Pts',(-18.5841033382921,24.1056738000994,122.507146079178)) ;
#21335 = CARTESIAN_POINT('Ctrl Pts',(-18.3778029519875,23.9256847197365,122.280987362701)) ;
#21336 = CARTESIAN_POINT('Ctrl Pts',(-18.942010615732,24.1256035843077,122.280096072877)) ;
#21337 = CARTESIAN_POINT('Ctrl Pts',(-18.8251843464588,23.9456145039448,121.997171158723)) ;
#21338 = CARTESIAN_POINT('Ctrl Pts',(-19.3555068623215,24.1455235736985,122.188809483554)) ;
#21339 = CARTESIAN_POINT('Ctrl Pts',(-19.3420527237489,23.9655344933356,121.8830575886)) ;
#21340 = CARTESIAN_POINT('Ctrl Pts',(-19.7742904831662,24.1653787690525,122.2430041829)) ;
#21341 = CARTESIAN_POINT('Ctrl Pts',(-19.8655341729859,23.9853896886896,121.950798016933)) ;
#21342 = CARTESIAN_POINT('Ctrl Pts',(-20.1526808934445,24.1854247707119,122.438992855019)) ;
#21343 = CARTESIAN_POINT('Ctrl Pts',(-20.3385180584329,24.005435690349,122.195770834828)) ;
#21344 = CARTESIAN_POINT('Ctrl Pts',(-20.3906070125325,24.2019245179217,122.696923893817)) ;
#21345 = CARTESIAN_POINT('Ctrl Pts',(-20.6359495242104,24.0219354375588,122.518207743344)) ;
#21346 = CARTESIAN_POINT('Ctrl Pts',(-20.5216768074671,24.2153131223698,122.945999721875)) ;
#21347 = CARTESIAN_POINT('Ctrl Pts',(-20.7997715920691,24.0353240420069,122.829526935845)) ;
#21348 = CARTESIAN_POINT('Ctrl Pts',(-20.5848955736062,24.2251749507047,123.143455647205)) ;
#21349 = CARTESIAN_POINT('Ctrl Pts',(-20.8788004514205,24.0451858703418,123.076353832387)) ;
#21350 = CARTESIAN_POINT('Ctrl Pts',(-20.6138199274551,24.2351410934622,123.350985731134)) ;
#21351 = CARTESIAN_POINT('Ctrl Pts',(-20.9149604443776,24.0551520130994,123.335751428972)) ;
#21352 = CARTESIAN_POINT('Ctrl Pts',(-20.6032002789081,24.2485028395872,123.631591883731)) ;
#21353 = CARTESIAN_POINT('Ctrl Pts',(-20.9016757192965,24.0685137592243,123.68657640661)) ;
#21354 = CARTESIAN_POINT('Ctrl Pts',(-20.5008787541352,24.2649571685423,123.966355059804)) ;
#21355 = CARTESIAN_POINT('Ctrl Pts',(-20.7738010339285,24.0849680881794,124.104947280262)) ;
#21356 = CARTESIAN_POINT('Ctrl Pts',(-20.2867198767303,24.2817244135906,124.2511417434)) ;
#21357 = CARTESIAN_POINT('Ctrl Pts',(-20.506074005893,24.1017353332277,124.460989068715)) ;
#21358 = CARTESIAN_POINT('Ctrl Pts',(-20.068100156107,24.2949109788646,124.421823870107)) ;
#21359 = CARTESIAN_POINT('Ctrl Pts',(-20.2328267963323,24.1149218985017,124.674311881725)) ;
#21360 = CARTESIAN_POINT('Ctrl Pts',(-19.8829901974809,24.3049004376092,124.520886533694)) ;
#21361 = CARTESIAN_POINT('Ctrl Pts',(-20.0014355866622,24.1249113572463,124.798149275947)) ;
#21362 = CARTESIAN_POINT('Ctrl Pts',(-19.6841183586994,24.3148542100903,124.586142139234)) ;
#21363 = CARTESIAN_POINT('Ctrl Pts',(-19.7528479925732,24.1348651297274,124.879719694348)) ;
#21364 = CARTESIAN_POINT('Ctrl Pts',(-19.4750256631218,24.324902026623,124.61598118881)) ;
#21365 = CARTESIAN_POINT('Ctrl Pts',(-19.4914820582763,24.1449129462601,124.917021763208)) ;
#21366 = CARTESIAN_POINT('Ctrl Pts',(-19.2682080171776,24.3347435597455,124.609445253002)) ;
#21367 = CARTESIAN_POINT('Ctrl Pts',(-19.2329600579686,24.1547544793826,124.90885452434)) ;
#21368 = CARTESIAN_POINT('Ctrl Pts',(-19.0626517418926,24.3447298019652,124.566925901012)) ;
#21369 = CARTESIAN_POINT('Ctrl Pts',(-18.9760140363379,24.1647407216023,124.855708116863)) ;
#21370 = CARTESIAN_POINT('Ctrl Pts',(-18.8684666859137,24.3546664253901,124.489818172107)) ;
#21371 = CARTESIAN_POINT('Ctrl Pts',(-18.7332816198796,24.1746773450272,124.759326036302)) ;
#21372 = CARTESIAN_POINT('Ctrl Pts',(-18.688696650813,24.3647163027731,124.378854486706)) ;
#21373 = CARTESIAN_POINT('Ctrl Pts',(-18.5085675410313,24.1847272224102,124.620623799681)) ;
#21374 = CARTESIAN_POINT('Ctrl Pts',(-18.5339244507054,24.3745667415506,124.241242493615)) ;
#21375 = CARTESIAN_POINT('Ctrl Pts',(-18.3151003354371,24.1945776611878,124.448610838)) ;
#21376 = CARTESIAN_POINT('Ctrl Pts',(-18.4034080881523,24.3845387555194,124.077216087896)) ;
#21377 = CARTESIAN_POINT('Ctrl Pts',(-18.1519526133633,24.2045496751565,124.243579488805)) ;
#21378 = CARTESIAN_POINT('Ctrl Pts',(-18.3031188994434,24.3945339241455,123.892525344681)) ;
#21379 = CARTESIAN_POINT('Ctrl Pts',(-18.0265886284109,24.2145448437826,124.012717326557)) ;
#21380 = CARTESIAN_POINT('Ctrl Pts',(-18.2364182379383,24.4045678074067,123.692421879584)) ;
#21381 = CARTESIAN_POINT('Ctrl Pts',(-17.9432101173695,24.2245787270438,123.762588848226)) ;
#21382 = CARTESIAN_POINT('Ctrl Pts',(-18.2057083821517,24.41442367747,123.487493870639)) ;
#21383 = CARTESIAN_POINT('Ctrl Pts',(-17.9048199953682,24.2344345971071,123.506429025599)) ;
#21384 = CARTESIAN_POINT('Ctrl Pts',(-18.2107882331578,24.4244212233872,123.277398137475)) ;
#21385 = CARTESIAN_POINT('Ctrl Pts',(-17.9111670277577,24.2444321430243,123.243809194865)) ;
#21386 = CARTESIAN_POINT('Ctrl Pts',(-18.2518400342972,24.4343293502864,123.073174907185)) ;
#21387 = CARTESIAN_POINT('Ctrl Pts',(-17.9624791058961,24.2543402699236,122.988529382377)) ;
#21388 = CARTESIAN_POINT('Ctrl Pts',(-18.3281714579042,24.4443397218086,122.877045008902)) ;
#21389 = CARTESIAN_POINT('Ctrl Pts',(-18.0578908532251,24.2643506414457,122.743365948088)) ;
#21390 = CARTESIAN_POINT('Ctrl Pts',(-18.438010301051,24.454370164556,122.69704745568)) ;
#21391 = CARTESIAN_POINT('Ctrl Pts',(-18.1951870356825,24.2743810841931,122.518367543358)) ;
#21392 = CARTESIAN_POINT('Ctrl Pts',(-18.5745495647584,24.4642181171093,122.541397741827)) ;
#21393 = CARTESIAN_POINT('Ctrl Pts',(-18.3658593160879,24.2842290367464,122.323803295538)) ;
#21394 = CARTESIAN_POINT('Ctrl Pts',(-18.7394306699372,24.4742807861303,122.408888682602)) ;
#21395 = CARTESIAN_POINT('Ctrl Pts',(-18.5719589574334,24.2942917057674,122.158164871478)) ;
#21396 = CARTESIAN_POINT('Ctrl Pts',(-18.9218207597135,24.4841751615942,122.308835807993)) ;
#21397 = CARTESIAN_POINT('Ctrl Pts',(-18.7999455381362,24.3041860812313,122.033096218261)) ;
#21398 = CARTESIAN_POINT('Ctrl Pts',(-19.119533784816,24.4941169599123,122.241135188269)) ;
#21399 = CARTESIAN_POINT('Ctrl Pts',(-19.0470862012802,24.3141278795495,121.948467825779)) ;
#21400 = CARTESIAN_POINT('Ctrl Pts',(-19.327299776132,24.5041194536396,122.208506614829)) ;
#21401 = CARTESIAN_POINT('Ctrl Pts',(-19.306793360523,24.3241303732768,121.9076794678)) ;
#21402 = CARTESIAN_POINT('Ctrl Pts',(-19.5382060178291,24.5141542521466,122.212793291372)) ;
#21403 = CARTESIAN_POINT('Ctrl Pts',(-19.5704262020177,24.3341651717837,121.913035104117)) ;
#21404 = CARTESIAN_POINT('Ctrl Pts',(-19.741340693941,24.5239991361259,122.252526138907)) ;
#21405 = CARTESIAN_POINT('Ctrl Pts',(-19.8243456090835,24.3440100557631,121.962698662003)) ;
#21406 = CARTESIAN_POINT('Ctrl Pts',(-19.9373544726432,24.533984992944,122.327605162214)) ;
#21407 = CARTESIAN_POINT('Ctrl Pts',(-20.069363913774,24.3539959125811,122.056545067836)) ;
#21408 = CARTESIAN_POINT('Ctrl Pts',(-20.1165728966918,24.5439198071187,122.434935896096)) ;
#21409 = CARTESIAN_POINT('Ctrl Pts',(-20.2933885436929,24.3639307267559,122.190706447143)) ;
#21410 = CARTESIAN_POINT('Ctrl Pts',(-20.2762066027916,24.5539773069041,122.573540909043)) ;
#21411 = CARTESIAN_POINT('Ctrl Pts',(-20.4929322997301,24.3739882265412,122.363960667453)) ;
#21412 = CARTESIAN_POINT('Ctrl Pts',(-20.4065058320593,24.5637990653224,122.733750397852)) ;
#21413 = CARTESIAN_POINT('Ctrl Pts',(-20.6558088061112,24.3838099849595,122.564221525997)) ;
#21414 = CARTESIAN_POINT('Ctrl Pts',(-20.5097290699146,24.5738547231064,122.918217818253)) ;
#21415 = CARTESIAN_POINT('Ctrl Pts',(-20.7848399620391,24.3938656427435,122.794804496023)) ;
#21416 = CARTESIAN_POINT('Ctrl Pts',(-20.5782202375852,24.5837969052864,123.115704900593)) ;
#21417 = CARTESIAN_POINT('Ctrl Pts',(-20.8704564403244,24.4038078249235,123.041662828752)) ;
#21418 = CARTESIAN_POINT('Ctrl Pts',(-20.6118814894185,24.5937021139811,123.32120168517)) ;
#21419 = CARTESIAN_POINT('Ctrl Pts',(-20.9125354801232,24.4137130336182,123.298533938)) ;
#21420 = CARTESIAN_POINT('Ctrl Pts',(-20.6092481539705,24.6037439049435,123.532291786237)) ;
#21421 = CARTESIAN_POINT('Ctrl Pts',(-20.909246248355,24.4237548245807,123.562396507273)) ;
#21422 = CARTESIAN_POINT('Ctrl Pts',(-20.5705464706402,24.6136516794158,123.73696556278)) ;
#21423 = CARTESIAN_POINT('Ctrl Pts',(-20.8608714359243,24.4336625990529,123.818239689833)) ;
#21424 = CARTESIAN_POINT('Ctrl Pts',(-20.4964883343986,24.6236631796434,123.933985160015)) ;
#21425 = CARTESIAN_POINT('Ctrl Pts',(-20.7683009426795,24.4436740992805,124.064515066611)) ;
#21426 = CARTESIAN_POINT('Ctrl Pts',(-20.388743463947,24.6336959400361,124.115308071487)) ;
#21427 = CARTESIAN_POINT('Ctrl Pts',(-20.6336219825576,24.4537068596732,124.291169915681)) ;
#21428 = CARTESIAN_POINT('Ctrl Pts',(-20.2539226961547,24.643546509171,124.272507133189)) ;
#21429 = CARTESIAN_POINT('Ctrl Pts',(-20.4650972755638,24.4635574288081,124.487670909562)) ;
#21430 = CARTESIAN_POINT('Ctrl Pts',(-20.0918811514129,24.6535351187009,124.406043156148)) ;
#21431 = CARTESIAN_POINT('Ctrl Pts',(-20.262546647733,24.473546038338,124.654592807145)) ;
#21432 = CARTESIAN_POINT('Ctrl Pts',(-19.9101907899771,24.663463774725,124.50880446125)) ;
#21433 = CARTESIAN_POINT('Ctrl Pts',(-20.035434390892,24.4834746943621,124.783046651201)) ;
#21434 = CARTESIAN_POINT('Ctrl Pts',(-19.7123608153397,24.6734515209028,124.579209070927)) ;
#21435 = CARTESIAN_POINT('Ctrl Pts',(-19.788147480938,24.4934624405399,124.871054527459)) ;
#21436 = CARTESIAN_POINT('Ctrl Pts',(-19.504271624768,24.6834875098385,124.614009588062)) ;
#21437 = CARTESIAN_POINT('Ctrl Pts',(-19.5280364525962,24.5034984294756,124.914557400059)) ;
#21438 = CARTESIAN_POINT('Ctrl Pts',(-19.2970799984549,24.6933423796521,124.612527488624)) ;
#21439 = CARTESIAN_POINT('Ctrl Pts',(-19.2690459880752,24.5133532992892,124.912706949231)) ;
#21440 = CARTESIAN_POINT('Ctrl Pts',(-19.090303135345,24.7033418208939,124.574834044645)) ;
#21441 = CARTESIAN_POINT('Ctrl Pts',(-19.0105743992336,24.523352740531,124.865592193593)) ;
#21442 = CARTESIAN_POINT('Ctrl Pts',(-18.8951262772354,24.713236895074,124.502757695016)) ;
#21443 = CARTESIAN_POINT('Ctrl Pts',(-18.7666019329129,24.5332478147111,124.775498416424)) ;
#21444 = CARTESIAN_POINT('Ctrl Pts',(-18.7124871130711,24.7232975509137,124.396143715782)) ;
#21445 = CARTESIAN_POINT('Ctrl Pts',(-18.5383021509909,24.5433084705508,124.642232833805)) ;
#21446 = CARTESIAN_POINT('Ctrl Pts',(-18.5544214010454,24.7331464251093,124.262378682155)) ;
#21447 = CARTESIAN_POINT('Ctrl Pts',(-18.3407179161461,24.5531573447464,124.475027408876)) ;
#21448 = CARTESIAN_POINT('Ctrl Pts',(-18.4191678408928,24.7431751370725,124.100648450517)) ;
#21449 = CARTESIAN_POINT('Ctrl Pts',(-18.1716495641239,24.5631860567097,124.272865839476)) ;
#21450 = CARTESIAN_POINT('Ctrl Pts',(-18.3145372263734,24.7532045376556,123.917586468341)) ;
#21451 = CARTESIAN_POINT('Ctrl Pts',(-18.0408595712216,24.5732154572928,124.044039432676)) ;
#21452 = CARTESIAN_POINT('Ctrl Pts',(-18.2441926662311,24.7630447312725,123.723038994785)) ;
#21453 = CARTESIAN_POINT('Ctrl Pts',(-17.9529267054046,24.5830556509096,123.80085466428)) ;
#21454 = CARTESIAN_POINT('Ctrl Pts',(-18.2077279525062,24.7730481538477,123.515942344631)) ;
#21455 = CARTESIAN_POINT('Ctrl Pts',(-17.9073440510645,24.5930590734848,123.541984051105)) ;
#21456 = CARTESIAN_POINT('Ctrl Pts',(-18.2078442834315,24.7830336909408,123.305979629472)) ;
#21457 = CARTESIAN_POINT('Ctrl Pts',(-17.9074876720707,24.6030446105779,123.279530447817)) ;
#21458 = CARTESIAN_POINT('Ctrl Pts',(-18.244816810972,24.7930746954276,123.098169474309)) ;
#21459 = CARTESIAN_POINT('Ctrl Pts',(-17.953701474388,24.6130856150647,123.019767558698)) ;
#21460 = CARTESIAN_POINT('Ctrl Pts',(-18.3156319158811,24.8029182343688,122.903704450163)) ;
#21461 = CARTESIAN_POINT('Ctrl Pts',(-18.0422190940517,24.6229291540059,122.776684574555)) ;
#21462 = CARTESIAN_POINT('Ctrl Pts',(-18.4202205854455,24.8129032653596,122.721733922501)) ;
#21463 = CARTESIAN_POINT('Ctrl Pts',(-18.1729536422505,24.6329141849967,122.549220386111)) ;
#21464 = CARTESIAN_POINT('Ctrl Pts',(-18.5541770056788,24.8228427278816,122.561322433432)) ;
#21465 = CARTESIAN_POINT('Ctrl Pts',(-18.3403982888488,24.6428536475187,122.348704583029)) ;
#21466 = CARTESIAN_POINT('Ctrl Pts',(-18.715558190906,24.8328824601054,122.425314061368)) ;
#21467 = CARTESIAN_POINT('Ctrl Pts',(-18.5421236161833,24.6528933797425,122.178692975382)) ;
#21468 = CARTESIAN_POINT('Ctrl Pts',(-18.8953205226514,24.8427706404226,122.320888321674)) ;
#21469 = CARTESIAN_POINT('Ctrl Pts',(-18.766826532383,24.6627815600597,122.048158969798)) ;
#21470 = CARTESIAN_POINT('Ctrl Pts',(-19.0923303882549,24.8527601561251,122.248163396936)) ;
#21471 = CARTESIAN_POINT('Ctrl Pts',(-19.0130885634454,24.6727710757622,121.957251380598)) ;
#21472 = CARTESIAN_POINT('Ctrl Pts',(-19.298364039197,24.8627187067798,122.211026101757)) ;
#21473 = CARTESIAN_POINT('Ctrl Pts',(-19.2706307855915,24.6827296264169,121.910828202634)) ;
#21474 = CARTESIAN_POINT('Ctrl Pts',(-19.5064905058478,24.8726181138848,122.209713205834)) ;
#21475 = CARTESIAN_POINT('Ctrl Pts',(-19.5307897392351,24.6926290335219,121.909185754216)) ;
#21476 = CARTESIAN_POINT('Ctrl Pts',(-19.7147219092595,24.8826667003011,122.245162774326)) ;
#21477 = CARTESIAN_POINT('Ctrl Pts',(-19.7910790035536,24.7026776199382,121.953496342207)) ;
#21478 = CARTESIAN_POINT('Ctrl Pts',(-19.9106826139148,24.8925595192655,122.314960468538)) ;
#21479 = CARTESIAN_POINT('Ctrl Pts',(-20.0360311856884,24.7125704389027,122.040742561825)) ;
#21480 = CARTESIAN_POINT('Ctrl Pts',(-20.0946951962707,24.9026306367953,122.41960013013)) ;
#21481 = CARTESIAN_POINT('Ctrl Pts',(-20.2660472328048,24.7226415564325,122.171540812148)) ;
#21482 = CARTESIAN_POINT('Ctrl Pts',(-20.2538475997201,24.9124463307614,122.551014009269)) ;
#21483 = CARTESIAN_POINT('Ctrl Pts',(-20.4649896868534,24.7324572503985,122.33580820644)) ;
#21484 = CARTESIAN_POINT('Ctrl Pts',(-20.3913621573758,24.9225127082587,122.711814363181)) ;
#21485 = CARTESIAN_POINT('Ctrl Pts',(-20.6368834830163,24.7425236278958,122.536807653796)) ;
#21486 = CARTESIAN_POINT('Ctrl Pts',(-20.4970748886783,24.9324116943406,122.891133137665)) ;
#21487 = CARTESIAN_POINT('Ctrl Pts',(-20.7690258159267,24.7524226139777,122.760956322212)) ;
#21488 = CARTESIAN_POINT('Ctrl Pts',(-20.571232101278,24.9424658743341,123.089018879175)) ;
#21489 = CARTESIAN_POINT('Ctrl Pts',(-20.8617232642626,24.7624767939712,123.008312860307)) ;
#21490 = CARTESIAN_POINT('Ctrl Pts',(-20.6094160911567,24.9523366872668,123.293040667745)) ;
#21491 = CARTESIAN_POINT('Ctrl Pts',(-20.9094544648808,24.7723476069039,123.263341038962)) ;
#21492 = CARTESIAN_POINT('Ctrl Pts',(-20.6116329545151,24.9624105881206,123.504764653356)) ;
#21493 = CARTESIAN_POINT('Ctrl Pts',(-20.9122265609454,24.7824215077577,123.527995577717)) ;
#21494 = CARTESIAN_POINT('Ctrl Pts',(-20.5781600299015,24.9722307435072,123.708532107742)) ;
#21495 = CARTESIAN_POINT('Ctrl Pts',(-20.8703860648763,24.7922416631444,123.782706579754)) ;
#21496 = CARTESIAN_POINT('Ctrl Pts',(-20.508237892881,24.9823094504595,123.908493710654)) ;
#21497 = CARTESIAN_POINT('Ctrl Pts',(-20.7829843523247,24.8023203700966,124.032658419494)) ;
#21498 = CARTESIAN_POINT('Ctrl Pts',(-20.4070053264551,24.9921610389983,124.089234851178)) ;
#21499 = CARTESIAN_POINT('Ctrl Pts',(-20.6564437174401,24.8121719586354,124.258586397133)) ;
#21500 = CARTESIAN_POINT('Ctrl Pts',(-20.2731799394624,25.0022341555233,124.253310305418)) ;
#21501 = CARTESIAN_POINT('Ctrl Pts',(-20.4891628443996,24.8222450751604,124.463680852311)) ;
#21502 = CARTESIAN_POINT('Ctrl Pts',(-20.1165044718704,25.0120766726191,124.388500704501)) ;
#21503 = CARTESIAN_POINT('Ctrl Pts',(-20.2933179390205,24.8320875922562,124.632670356776)) ;
#21504 = CARTESIAN_POINT('Ctrl Pts',(-19.936630039934,25.022057134173,124.496508778481)) ;
#21505 = CARTESIAN_POINT('Ctrl Pts',(-20.0684748873038,24.8420680538102,124.767681031673)) ;
#21506 = CARTESIAN_POINT('Ctrl Pts',(-19.7398406206067,25.0320753841638,124.571552225653)) ;
#21507 = CARTESIAN_POINT('Ctrl Pts',(-19.8224883546883,24.8520863038009,124.861485946865)) ;
#21508 = CARTESIAN_POINT('Ctrl Pts',(-19.5358376882034,25.0419595443576,124.611179719753)) ;
#21509 = CARTESIAN_POINT('Ctrl Pts',(-19.5674837085229,24.8619704639947,124.911020996683)) ;
#21510 = CARTESIAN_POINT('Ctrl Pts',(-19.3242913071813,25.0520246913326,124.614802833866)) ;
#21511 = CARTESIAN_POINT('Ctrl Pts',(-19.3030511330044,24.8720356109697,124.915550386411)) ;
#21512 = CARTESIAN_POINT('Ctrl Pts',(-19.1199106240367,25.0618665149734,124.582483950528)) ;
#21513 = CARTESIAN_POINT('Ctrl Pts',(-19.0475737608601,24.8818774346105,124.875152002711)) ;
#21514 = CARTESIAN_POINT('Ctrl Pts',(-18.9203492375791,25.0718959874342,124.514427752027)) ;
#21515 = CARTESIAN_POINT('Ctrl Pts',(-18.7981220481967,24.8919069070713,124.790082006543)) ;
#21516 = CARTESIAN_POINT('Ctrl Pts',(-18.7359613362089,25.0819228426962,124.412260699821)) ;
#21517 = CARTESIAN_POINT('Ctrl Pts',(-18.5676370265376,24.9019337623334,124.662373648599)) ;
#21518 = CARTESIAN_POINT('Ctrl Pts',(-18.5748042640139,25.0917660928068,124.282445342146)) ;
#21519 = CARTESIAN_POINT('Ctrl Pts',(-18.3661893963596,24.9117770124439,124.500103756191)) ;
#21520 = CARTESIAN_POINT('Ctrl Pts',(-18.4355859909014,25.1018145323899,124.123567079919)) ;
#21521 = CARTESIAN_POINT('Ctrl Pts',(-18.1921666070184,24.9218254520271,124.30150622892)) ;
#21522 = CARTESIAN_POINT('Ctrl Pts',(-18.3274272880711,25.1117640266378,123.944530772977)) ;
#21523 = CARTESIAN_POINT('Ctrl Pts',(-18.056967678217,24.931774946275,124.077710500125)) ;
#21524 = CARTESIAN_POINT('Ctrl Pts',(-18.2517272644222,25.1216718823638,123.750467023187)) ;
#21525 = CARTESIAN_POINT('Ctrl Pts',(-17.9623422828139,24.941682802001,123.835129981)) ;
#21526 = CARTESIAN_POINT('Ctrl Pts',(-18.2104743970335,25.1317313590138,123.543070104516)) ;
#21527 = CARTESIAN_POINT('Ctrl Pts',(-17.9107761380726,24.9517422786509,123.575884197323)) ;
#21528 = CARTESIAN_POINT('Ctrl Pts',(-18.2056782190192,25.1415721684225,123.336215569633)) ;
#21529 = CARTESIAN_POINT('Ctrl Pts',(-17.9047808645182,24.9615830880596,123.317314560702)) ;
#21530 = CARTESIAN_POINT('Ctrl Pts',(-18.2373040930332,25.1516343187233,123.127077183961)) ;
#21531 = CARTESIAN_POINT('Ctrl Pts',(-17.9443132377084,24.9716452383604,123.055891956674)) ;
#21532 = CARTESIAN_POINT('Ctrl Pts',(-18.3038712513499,25.1615314798458,122.929932299027)) ;
#21533 = CARTESIAN_POINT('Ctrl Pts',(-18.027522505227,24.981542399483,122.809459900675)) ;
#21534 = CARTESIAN_POINT('Ctrl Pts',(-18.4033840340755,25.1714626542499,122.746394261675)) ;
#21535 = CARTESIAN_POINT('Ctrl Pts',(-18.15191407074,24.991473573887,122.580036852208)) ;
#21536 = CARTESIAN_POINT('Ctrl Pts',(-18.534887670248,25.1815048579749,122.581237562845)) ;
#21537 = CARTESIAN_POINT('Ctrl Pts',(-18.3162936300384,25.001515777612,122.373591256392)) ;
#21538 = CARTESIAN_POINT('Ctrl Pts',(-18.690527647173,25.1913914404053,122.443467269935)) ;
#21539 = CARTESIAN_POINT('Ctrl Pts',(-18.5108445770742,25.0114023600425,122.201377852405)) ;
#21540 = CARTESIAN_POINT('Ctrl Pts',(-18.8694400895696,25.2013848761537,122.333355299341)) ;
#21541 = CARTESIAN_POINT('Ctrl Pts',(-18.7344855027603,25.0213957957908,122.063738108185)) ;
#21542 = CARTESIAN_POINT('Ctrl Pts',(-19.0638333349581,25.2113293445118,122.256415312659)) ;
#21543 = CARTESIAN_POINT('Ctrl Pts',(-18.9774777481212,25.031340264149,121.967563232072)) ;
#21544 = CARTESIAN_POINT('Ctrl Pts',(-19.2687117383254,25.2212811607574,122.213977770171)) ;
#21545 = CARTESIAN_POINT('Ctrl Pts',(-19.2335763972328,25.0412920803945,121.914516693683)) ;
#21546 = CARTESIAN_POINT('Ctrl Pts',(-19.4796320217027,25.2313185968719,122.207898426795)) ;
#21547 = CARTESIAN_POINT('Ctrl Pts',(-19.4972265998584,25.051329516509,121.906917954592)) ;
#21548 = CARTESIAN_POINT('Ctrl Pts',(-19.6852897576632,25.2412035560482,122.237873411144)) ;
#21549 = CARTESIAN_POINT('Ctrl Pts',(-19.7542997604475,25.0612144756854,121.944387345544)) ;
#21550 = CARTESIAN_POINT('Ctrl Pts',(-19.8849152260127,25.2512016742602,122.303598681316)) ;
#21551 = CARTESIAN_POINT('Ctrl Pts',(-20.0038315528282,25.0712125938973,122.026544562977)) ;
#21552 = CARTESIAN_POINT('Ctrl Pts',(-20.0687767747122,25.2611226067721,122.402114690331)) ;
#21553 = CARTESIAN_POINT('Ctrl Pts',(-20.2336588620757,25.0811335264093,122.149690526495)) ;
#21554 = CARTESIAN_POINT('Ctrl Pts',(-20.2347377539777,25.2711639069942,122.532559750854)) ;
#21555 = CARTESIAN_POINT('Ctrl Pts',(-20.4411095234431,25.0911748266313,122.31274727971)) ;
#21556 = CARTESIAN_POINT('Ctrl Pts',(-20.3735985016344,25.2810708253842,122.687791031638)) ;
#21557 = CARTESIAN_POINT('Ctrl Pts',(-20.6146855652456,25.1010817450213,122.506787487702)) ;
#21558 = CARTESIAN_POINT('Ctrl Pts',(-20.4842246461165,25.2910066170932,122.864973861521)) ;
#21559 = CARTESIAN_POINT('Ctrl Pts',(-20.7529678400047,25.1110175367304,122.728267052382)) ;
#21560 = CARTESIAN_POINT('Ctrl Pts',(-20.5630324165797,25.3010475116711,123.060797396838)) ;
#21561 = CARTESIAN_POINT('Ctrl Pts',(-20.8514767358832,25.1210584313083,122.973046599286)) ;
#21562 = CARTESIAN_POINT('Ctrl Pts',(-20.6061255781903,25.310934713385,123.264152339049)) ;
#21563 = CARTESIAN_POINT('Ctrl Pts',(-20.9053425589782,25.1309456330221,123.227241473632)) ;
#21564 = CARTESIAN_POINT('Ctrl Pts',(-20.6136784836377,25.3209269811466,123.474070984614)) ;
#21565 = CARTESIAN_POINT('Ctrl Pts',(-20.9147827032288,25.1409379007837,123.489640019812)) ;
#21566 = CARTESIAN_POINT('Ctrl Pts',(-20.5847340091675,25.3308755021684,123.681219469277)) ;
#21567 = CARTESIAN_POINT('Ctrl Pts',(-20.8786010725189,25.1508864218055,123.748576028363)) ;
#21568 = CARTESIAN_POINT('Ctrl Pts',(-20.5206272668833,25.3408122757461,123.880023760585)) ;
#21569 = CARTESIAN_POINT('Ctrl Pts',(-20.7984664179347,25.1608231953832,123.997081667606)) ;
#21570 = CARTESIAN_POINT('Ctrl Pts',(-20.4227342551937,25.3507953238871,124.065699360491)) ;
#21571 = CARTESIAN_POINT('Ctrl Pts',(-20.6760989906385,25.1708062435242,124.229175844446)) ;
#21572 = CARTESIAN_POINT('Ctrl Pts',(-20.2930330978776,25.3608390314972,124.232290893968)) ;
#21573 = CARTESIAN_POINT('Ctrl Pts',(-20.5139718407011,25.1808499511343,124.437414474404)) ;
#21574 = CARTESIAN_POINT('Ctrl Pts',(-20.1400132496701,25.3706677246505,124.3711852769)) ;
#21575 = CARTESIAN_POINT('Ctrl Pts',(-20.3226951495202,25.1906786442876,124.611032523133)) ;
#21576 = CARTESIAN_POINT('Ctrl Pts',(-19.9609525577094,25.3807424737799,124.484253952446)) ;
#21577 = CARTESIAN_POINT('Ctrl Pts',(-20.098868954127,25.200753393417,124.752367074633)) ;
#21578 = CARTESIAN_POINT('Ctrl Pts',(-19.7689867735879,25.3906077995755,124.56282261199)) ;
#21579 = CARTESIAN_POINT('Ctrl Pts',(-19.858910190644,25.2106187192126,124.850577176108)) ;
#21580 = CARTESIAN_POINT('Ctrl Pts',(-19.5632165090055,25.4006299739324,124.608087313352)) ;
#21581 = CARTESIAN_POINT('Ctrl Pts',(-19.6016970937392,25.2206408935695,124.907156637884)) ;
#21582 = CARTESIAN_POINT('Ctrl Pts',(-19.3525876909076,25.4106560271393,124.616422421431)) ;
#21583 = CARTESIAN_POINT('Ctrl Pts',(-19.33841109203,25.2306669467765,124.91757426496)) ;
#21584 = CARTESIAN_POINT('Ctrl Pts',(-19.147287360646,25.4205097239856,124.588883432483)) ;
#21585 = CARTESIAN_POINT('Ctrl Pts',(-19.0817846505437,25.2405206436227,124.883149004069)) ;
#21586 = CARTESIAN_POINT('Ctrl Pts',(-18.9475566685195,25.4304691287386,124.526036690547)) ;
#21587 = CARTESIAN_POINT('Ctrl Pts',(-18.8321213569949,25.2504800483757,124.804588928289)) ;
#21588 = CARTESIAN_POINT('Ctrl Pts',(-18.7604916580374,25.4405073744435,124.428375640314)) ;
#21589 = CARTESIAN_POINT('Ctrl Pts',(-18.5982908950502,25.2605182940806,124.68251138002)) ;
#21590 = CARTESIAN_POINT('Ctrl Pts',(-18.5957013870381,25.4503815586055,124.302092265061)) ;
#21591 = CARTESIAN_POINT('Ctrl Pts',(-18.3923032184799,25.2703924782426,124.52465527997)) ;
#21592 = CARTESIAN_POINT('Ctrl Pts',(-18.4526055536538,25.4604513417434,124.146119088409)) ;
#21593 = CARTESIAN_POINT('Ctrl Pts',(-18.2134348354326,25.2804622613806,124.32968799242)) ;
#21594 = CARTESIAN_POINT('Ctrl Pts',(-18.3413212778129,25.4702845967642,123.971882300025)) ;
#21595 = CARTESIAN_POINT('Ctrl Pts',(-18.0743301698985,25.2902955164013,124.111890050986)) ;
#21596 = CARTESIAN_POINT('Ctrl Pts',(-18.2598482943526,25.4803150228959,123.777393425404)) ;
#21597 = CARTESIAN_POINT('Ctrl Pts',(-17.9724906536207,25.300325942533,123.868778335182)) ;
#21598 = CARTESIAN_POINT('Ctrl Pts',(-18.2139714522043,25.4903466350829,123.571535696539)) ;
#21599 = CARTESIAN_POINT('Ctrl Pts',(-17.9151462002579,25.31035755472,123.611455902983)) ;
#21600 = CARTESIAN_POINT('Ctrl Pts',(-18.2042958256806,25.5001763319375,123.365125390913)) ;
#21601 = CARTESIAN_POINT('Ctrl Pts',(-17.9030533678709,25.3201872515746,123.353441667699)) ;
#21602 = CARTESIAN_POINT('Ctrl Pts',(-18.2304147172978,25.51016577384,123.156740327135)) ;
#21603 = CARTESIAN_POINT('Ctrl Pts',(-17.935703946638,25.3301766934771,123.092960405583)) ;
#21604 = CARTESIAN_POINT('Ctrl Pts',(-18.2931661314917,25.5202096658556,122.955127632222)) ;
#21605 = CARTESIAN_POINT('Ctrl Pts',(-18.01414488107,25.3402205854928,122.840945210804)) ;
#21606 = CARTESIAN_POINT('Ctrl Pts',(-18.3874495319765,25.5300312276249,122.771432509652)) ;
#21607 = CARTESIAN_POINT('Ctrl Pts',(-18.1320014123289,25.350042147262,122.611326074322)) ;
#21608 = CARTESIAN_POINT('Ctrl Pts',(-18.5144967250623,25.5400667992491,122.60299121237)) ;
#21609 = CARTESIAN_POINT('Ctrl Pts',(-18.290812004256,25.3600777188862,122.400775785575)) ;
#21610 = CARTESIAN_POINT('Ctrl Pts',(-18.669193308683,25.5500960735309,122.459723633636)) ;
#21611 = CARTESIAN_POINT('Ctrl Pts',(-18.4841839838092,25.370106993168,122.221692735608)) ;
#21612 = CARTESIAN_POINT('Ctrl Pts',(-18.8426660315161,25.5599299106495,122.34725013946)) ;
#21613 = CARTESIAN_POINT('Ctrl Pts',(-18.7010269361118,25.3799408302867,122.081101987193)) ;
#21614 = CARTESIAN_POINT('Ctrl Pts',(-19.0371487210636,25.5699823067377,122.26458450001)) ;
#21615 = CARTESIAN_POINT('Ctrl Pts',(-18.9441309444256,25.3899932263748,121.977771975232)) ;
#21616 = CARTESIAN_POINT('Ctrl Pts',(-19.2407432881081,25.5799190736882,122.217749926032)) ;
#21617 = CARTESIAN_POINT('Ctrl Pts',(-19.1986250893084,25.3999299933253,121.919230643914)) ;
#21618 = CARTESIAN_POINT('Ctrl Pts',(-19.4492836308601,25.5898533086675,122.206441411571)) ;
#21619 = CARTESIAN_POINT('Ctrl Pts',(-19.459301128586,25.4098642283046,121.905097168243)) ;
#21620 = CARTESIAN_POINT('Ctrl Pts',(-19.6584731388207,25.5998770719943,122.231868584206)) ;
#21621 = CARTESIAN_POINT('Ctrl Pts',(-19.72078773703,25.4198879916314,121.936883279556)) ;
#21622 = CARTESIAN_POINT('Ctrl Pts',(-19.8573510139272,25.6097634133789,122.292244191361)) ;
#21623 = CARTESIAN_POINT('Ctrl Pts',(-19.9693851432808,25.429774333016,122.012355109386)) ;
#21624 = CARTESIAN_POINT('Ctrl Pts',(-20.0448786077411,25.6197524621459,122.386778679778)) ;
#21625 = CARTESIAN_POINT('Ctrl Pts',(-20.2037937296493,25.439763381783,122.130525368287)) ;
#21626 = CARTESIAN_POINT('Ctrl Pts',(-20.2137531182518,25.6297936828433,122.513441376923)) ;
#21627 = CARTESIAN_POINT('Ctrl Pts',(-20.4148854638875,25.4498046024804,122.288855457116)) ;
#21628 = CARTESIAN_POINT('Ctrl Pts',(-20.3553169833918,25.6396263230212,122.664067992544)) ;
#21629 = CARTESIAN_POINT('Ctrl Pts',(-20.5918392755866,25.4596372426583,122.477141002139)) ;
#21630 = CARTESIAN_POINT('Ctrl Pts',(-20.4709395710573,25.6496202523291,122.839494815761)) ;
#21631 = CARTESIAN_POINT('Ctrl Pts',(-20.7363655379612,25.4696311719663,122.696425976588)) ;
#21632 = CARTESIAN_POINT('Ctrl Pts',(-20.5542313166204,25.6596494600097,123.033193067616)) ;
#21633 = CARTESIAN_POINT('Ctrl Pts',(-20.8404780632738,25.4796603796468,122.93854969465)) ;
#21634 = CARTESIAN_POINT('Ctrl Pts',(-20.6022166705038,25.6695252717138,123.235204192602)) ;
#21635 = CARTESIAN_POINT('Ctrl Pts',(-20.9004575630717,25.4895361913509,123.191064817286)) ;
#21636 = CARTESIAN_POINT('Ctrl Pts',(-20.6147777399099,25.6795244986852,123.445015641522)) ;
#21637 = CARTESIAN_POINT('Ctrl Pts',(-20.9161564441938,25.4995354183223,123.453329386861)) ;
#21638 = CARTESIAN_POINT('Ctrl Pts',(-20.5911250967984,25.6894339798409,123.652027739966)) ;
#21639 = CARTESIAN_POINT('Ctrl Pts',(-20.8865881009697,25.509444899478,123.712094698215)) ;
#21640 = CARTESIAN_POINT('Ctrl Pts',(-20.531017224915,25.6994872101418,123.854627589131)) ;
#21641 = CARTESIAN_POINT('Ctrl Pts',(-20.81145089258,25.5194981297789,123.965343699702)) ;
#21642 = CARTESIAN_POINT('Ctrl Pts',(-20.4384325667578,25.7093578266928,124.040355450809)) ;
#21643 = CARTESIAN_POINT('Ctrl Pts',(-20.6957175422055,25.52936874633,124.197502953534)) ;
#21644 = CARTESIAN_POINT('Ctrl Pts',(-20.3135029459365,25.7193794884249,124.210003208649)) ;
#21645 = CARTESIAN_POINT('Ctrl Pts',(-20.5395534186836,25.539390408062,124.409561109384)) ;
#21646 = CARTESIAN_POINT('Ctrl Pts',(-20.1606542811385,25.729402301606,124.355058412312)) ;
#21647 = CARTESIAN_POINT('Ctrl Pts',(-20.3484908449209,25.5494132212431,124.590878299816)) ;
#21648 = CARTESIAN_POINT('Ctrl Pts',(-19.9878788008662,25.7392694660659,124.469843004655)) ;
#21649 = CARTESIAN_POINT('Ctrl Pts',(-20.1325195803171,25.5592803857031,124.734357216796)) ;
#21650 = CARTESIAN_POINT('Ctrl Pts',(-19.7955437673314,25.7492629082859,124.554394992238)) ;
#21651 = CARTESIAN_POINT('Ctrl Pts',(-19.8920996177146,25.569273827923,124.840044812153)) ;
#21652 = CARTESIAN_POINT('Ctrl Pts',(-19.5905777687678,25.7592945818862,124.604056660559)) ;
#21653 = CARTESIAN_POINT('Ctrl Pts',(-19.6358915111173,25.5793055015233,124.902119378316)) ;
#21654 = CARTESIAN_POINT('Ctrl Pts',(-19.3835799225067,25.7691610169992,124.617474520566)) ;
#21655 = CARTESIAN_POINT('Ctrl Pts',(-19.377143513442,25.5891719366363,124.918889100785)) ;
#21656 = CARTESIAN_POINT('Ctrl Pts',(-19.1748644935385,25.7791484675323,124.594811648332)) ;
#21657 = CARTESIAN_POINT('Ctrl Pts',(-19.1162493958071,25.5991593871694,124.890557819024)) ;
#21658 = CARTESIAN_POINT('Ctrl Pts',(-18.9740276761385,25.7890933973602,124.536594188768)) ;
#21659 = CARTESIAN_POINT('Ctrl Pts',(-18.8652039002789,25.6091043169973,124.817783333034)) ;
#21660 = CARTESIAN_POINT('Ctrl Pts',(-18.7845612887665,25.7991382924153,124.443378041818)) ;
#21661 = CARTESIAN_POINT('Ctrl Pts',(-18.6283721225821,25.6191492120525,124.701260743701)) ;
#21662 = CARTESIAN_POINT('Ctrl Pts',(-18.6171242290503,25.8090003541012,124.321077049524)) ;
#21663 = CARTESIAN_POINT('Ctrl Pts',(-18.419077049514,25.6290112737383,124.548382059341)) ;
#21664 = CARTESIAN_POINT('Ctrl Pts',(-18.4712964694787,25.818992076888,124.169910090686)) ;
#21665 = CARTESIAN_POINT('Ctrl Pts',(-18.2367942709095,25.6390029965252,124.359421375143)) ;
#21666 = CARTESIAN_POINT('Ctrl Pts',(-18.3546829235641,25.828924291128,123.996697923502)) ;
#21667 = CARTESIAN_POINT('Ctrl Pts',(-18.091029495205,25.6489352107651,124.142904444548)) ;
#21668 = CARTESIAN_POINT('Ctrl Pts',(-18.269414013462,25.8388636096937,123.805925409421)) ;
#21669 = CARTESIAN_POINT('Ctrl Pts',(-17.9844458363519,25.6588745293309,123.904437503963)) ;
#21670 = CARTESIAN_POINT('Ctrl Pts',(-18.2182183799845,25.8489077844696,123.601068446955)) ;
#21671 = CARTESIAN_POINT('Ctrl Pts',(-17.9204539831751,25.6689187041067,123.648365609469)) ;
#21672 = CARTESIAN_POINT('Ctrl Pts',(-18.2035144290787,25.8587783385346,123.394080423168)) ;
#21673 = CARTESIAN_POINT('Ctrl Pts',(-17.9020768058315,25.6787892581717,123.389630116784)) ;
#21674 = CARTESIAN_POINT('Ctrl Pts',(-18.2245755858917,25.8687433208888,123.185646036697)) ;
#21675 = CARTESIAN_POINT('Ctrl Pts',(-17.9284060681277,25.6887542405259,123.1290873224)) ;
#21676 = CARTESIAN_POINT('Ctrl Pts',(-18.2821927216553,25.8787740237786,122.982799143705)) ;
#21677 = CARTESIAN_POINT('Ctrl Pts',(-18.000430199717,25.6987849434157,122.875529417126)) ;
#21678 = CARTESIAN_POINT('Ctrl Pts',(-18.3726282398812,25.8886663638038,122.795495732635)) ;
#21679 = CARTESIAN_POINT('Ctrl Pts',(-18.1134771988756,25.7086772834409,122.641401239108)) ;
#21680 = CARTESIAN_POINT('Ctrl Pts',(-18.4961390189177,25.8987195969637,122.624026714153)) ;
#21681 = CARTESIAN_POINT('Ctrl Pts',(-18.2678679863379,25.7187305166009,122.427066576845)) ;
#21682 = CARTESIAN_POINT('Ctrl Pts',(-18.6449144456404,25.9086008414405,122.478993547401)) ;
#21683 = CARTESIAN_POINT('Ctrl Pts',(-18.4538393268546,25.7286117610776,122.245777047898)) ;
#21684 = CARTESIAN_POINT('Ctrl Pts',(-18.8191018734821,25.9186339623115,122.36011093306)) ;
#21685 = CARTESIAN_POINT('Ctrl Pts',(-18.6715752593228,25.7386448819486,122.097176077592)) ;
#21686 = CARTESIAN_POINT('Ctrl Pts',(-19.0083693285525,25.9285151725866,122.274392628594)) ;
#21687 = CARTESIAN_POINT('Ctrl Pts',(-18.9081608033064,25.7485260922237,121.990030737852)) ;
#21688 = CARTESIAN_POINT('Ctrl Pts',(-19.2132442732851,25.9385772483559,122.221858172896)) ;
#21689 = CARTESIAN_POINT('Ctrl Pts',(-19.1642552672847,25.758588167993,121.924365385186)) ;
#21690 = CARTESIAN_POINT('Ctrl Pts',(-19.41988850403,25.9484343067377,122.205946244502)) ;
#21691 = CARTESIAN_POINT('Ctrl Pts',(-19.4225607860531,25.7684452263748,121.904478285387)) ;
#21692 = CARTESIAN_POINT('Ctrl Pts',(-19.6290114818218,25.9584288620267,122.226010291668)) ;
#21693 = CARTESIAN_POINT('Ctrl Pts',(-19.6839642883553,25.7784397816638,121.929561151871)) ;
#21694 = CARTESIAN_POINT('Ctrl Pts',(-19.8301627349406,25.9683547495622,122.281640275295)) ;
#21695 = CARTESIAN_POINT('Ctrl Pts',(-19.9354025958823,25.7883656691993,121.999101330404)) ;
#21696 = CARTESIAN_POINT('Ctrl Pts',(-20.0204672700362,25.9783797695574,122.372173587935)) ;
#21697 = CARTESIAN_POINT('Ctrl Pts',(-20.1732821454297,25.7983906891946,122.112270545144)) ;
#21698 = CARTESIAN_POINT('Ctrl Pts',(-20.1900359400144,25.9882771466611,122.492771224812)) ;
#21699 = CARTESIAN_POINT('Ctrl Pts',(-20.3852412939983,25.8082880662982,122.26301982624)) ;
#21700 = CARTESIAN_POINT('Ctrl Pts',(-20.3377857345997,25.998267383742,122.642047679255)) ;
#21701 = CARTESIAN_POINT('Ctrl Pts',(-20.5699265939808,25.8182783033791,122.449617357553)) ;
#21702 = CARTESIAN_POINT('Ctrl Pts',(-20.4575881124741,26.0083039965508,122.815736066675)) ;
#21703 = CARTESIAN_POINT('Ctrl Pts',(-20.7196773404664,25.8283149161879,122.666729559919)) ;
#21704 = CARTESIAN_POINT('Ctrl Pts',(-20.5440893195705,26.0181538799688,123.003887825492)) ;
#21705 = CARTESIAN_POINT('Ctrl Pts',(-20.8278012350198,25.8381647996059,122.901920140004)) ;
#21706 = CARTESIAN_POINT('Ctrl Pts',(-20.5978286138219,26.0281574968712,123.207191914562)) ;
#21707 = CARTESIAN_POINT('Ctrl Pts',(-20.8949727103039,25.8481684165084,123.156051177432)) ;
#21708 = CARTESIAN_POINT('Ctrl Pts',(-20.6153163617937,26.0381469086364,123.416505710601)) ;
#21709 = CARTESIAN_POINT('Ctrl Pts',(-20.9168297433397,25.8581578282735,123.417692998704)) ;
#21710 = CARTESIAN_POINT('Ctrl Pts',(-20.5960135788333,26.0481656699812,123.626222930686)) ;
#21711 = CARTESIAN_POINT('Ctrl Pts',(-20.8926982525151,25.8681765896183,123.67984195633)) ;
#21712 = CARTESIAN_POINT('Ctrl Pts',(-20.5232631932467,26.0613843453623,123.894483327193)) ;
#21713 = CARTESIAN_POINT('Ctrl Pts',(-20.8017581311539,25.8813952649994,124.015153473732)) ;
#21714 = CARTESIAN_POINT('Ctrl Pts',(-20.3813483402664,26.074694652607,124.13929149955)) ;
#21715 = CARTESIAN_POINT('Ctrl Pts',(-20.6243920028856,25.8947055722441,124.321133430442)) ;
#21716 = CARTESIAN_POINT('Ctrl Pts',(-20.1842168943985,26.087932318833,124.335713981098)) ;
#21717 = CARTESIAN_POINT('Ctrl Pts',(-20.3779377392562,25.9079432384701,124.566705392269)) ;
#21718 = CARTESIAN_POINT('Ctrl Pts',(-20.0135494311699,26.0978520142437,124.455575991443)) ;
#21719 = CARTESIAN_POINT('Ctrl Pts',(-20.1646098417396,25.9178629338808,124.716521317829)) ;
#21720 = CARTESIAN_POINT('Ctrl Pts',(-19.8220452045287,26.1079048812422,124.544939686849)) ;
#21721 = CARTESIAN_POINT('Ctrl Pts',(-19.9252257840937,25.9279158008794,124.828226044214)) ;
#21722 = CARTESIAN_POINT('Ctrl Pts',(-19.6219710853917,26.1177602895715,124.598853822715)) ;
#21723 = CARTESIAN_POINT('Ctrl Pts',(-19.6751350635831,25.9377712092086,124.895616007158)) ;
#21724 = CARTESIAN_POINT('Ctrl Pts',(-19.4118059045154,26.1277989212481,124.617896062361)) ;
#21725 = CARTESIAN_POINT('Ctrl Pts',(-19.4124225556355,25.9478098408852,124.919414322609)) ;
#21726 = CARTESIAN_POINT('Ctrl Pts',(-19.1331380537758,26.1411011035151,124.594040851199)) ;
#21727 = CARTESIAN_POINT('Ctrl Pts',(-19.0641152659986,25.9611120231522,124.889602889987)) ;
#21728 = CARTESIAN_POINT('Ctrl Pts',(-18.8021064780862,26.157646116598,124.475037573678)) ;
#21729 = CARTESIAN_POINT('Ctrl Pts',(-18.6502847526992,25.9776570362351,124.740819809691)) ;
#21730 = CARTESIAN_POINT('Ctrl Pts',(-18.5297345481408,26.1742981326742,124.248799717429)) ;
#21731 = CARTESIAN_POINT('Ctrl Pts',(-18.3098802866931,25.9943090523113,124.458074394266)) ;
#21732 = CARTESIAN_POINT('Ctrl Pts',(-18.369098727454,26.1875212235794,124.021942776296)) ;
#21733 = CARTESIAN_POINT('Ctrl Pts',(-18.1090436808664,26.0075321432166,124.174455573223)) ;
#21734 = CARTESIAN_POINT('Ctrl Pts',(-18.2790691456165,26.1974821831388,123.832864887124)) ;
#21735 = CARTESIAN_POINT('Ctrl Pts',(-17.9965176539852,26.0174931027759,123.938117510176)) ;
#21736 = CARTESIAN_POINT('Ctrl Pts',(-18.2231373596907,26.2075069798899,123.629678729636)) ;
#21737 = CARTESIAN_POINT('Ctrl Pts',(-17.9266031351628,26.027517899527,123.684128674994)) ;
#21738 = CARTESIAN_POINT('Ctrl Pts',(-18.19662185451,26.2207314272857,123.352884992182)) ;
#21739 = CARTESIAN_POINT('Ctrl Pts',(-17.8934600554389,26.0407423469228,123.338151922398)) ;
#21740 = CARTESIAN_POINT('Ctrl Pts',(-18.2547370627252,26.2373652119848,123.004073948381)) ;
#21741 = CARTESIAN_POINT('Ctrl Pts',(-17.9661098980233,26.0573761316219,122.902122581917)) ;
#21742 = CARTESIAN_POINT('Ctrl Pts',(-18.4626485183739,26.2572678787097,122.635440004849)) ;
#21743 = CARTESIAN_POINT('Ctrl Pts',(-18.2260016702492,26.0772787983468,122.441338078492)) ;
#21744 = CARTESIAN_POINT('Ctrl Pts',(-18.7834207710504,26.2771681064916,122.359539756273)) ;
#21745 = CARTESIAN_POINT('Ctrl Pts',(-18.6269689740633,26.0971790261287,122.096464789941)) ;
#21746 = CARTESIAN_POINT('Ctrl Pts',(-19.1793519772945,26.2970855940231,122.209249706673)) ;
#21747 = CARTESIAN_POINT('Ctrl Pts',(-19.1218834344603,26.1170965136602,121.908606135804)) ;
#21748 = CARTESIAN_POINT('Ctrl Pts',(-19.60307943523,26.31701511984,122.202825724999)) ;
#21749 = CARTESIAN_POINT('Ctrl Pts',(-19.6515421009118,26.1370260394771,121.900579250022)) ;
#21750 = CARTESIAN_POINT('Ctrl Pts',(-20.004197714649,26.3369773877262,122.341686788595)) ;
#21751 = CARTESIAN_POINT('Ctrl Pts',(-20.1529386123422,26.1569883073634,122.074158377623)) ;
#21752 = CARTESIAN_POINT('Ctrl Pts',(-20.3326211942537,26.3568675826784,122.608053388485)) ;
#21753 = CARTESIAN_POINT('Ctrl Pts',(-20.5634651727886,26.1768785023156,122.407118082729)) ;
#21754 = CARTESIAN_POINT('Ctrl Pts',(-20.5514266364284,26.3767578274247,122.970081973903)) ;
#21755 = CARTESIAN_POINT('Ctrl Pts',(-20.8369695350651,26.1967687470618,122.859653772299)) ;
#21756 = CARTESIAN_POINT('Ctrl Pts',(-20.6334217410706,26.3968321999872,123.388909430167)) ;
#21757 = CARTESIAN_POINT('Ctrl Pts',(-20.9394612388346,26.2168431196243,123.383189522101)) ;
#21758 = CARTESIAN_POINT('Ctrl Pts',(-20.5686369856693,26.4166175773475,123.804638740479)) ;
#21759 = CARTESIAN_POINT('Ctrl Pts',(-20.858478621002,26.2366284969846,123.902848054689)) ;
#21760 = CARTESIAN_POINT('Ctrl Pts',(-20.3652722304398,26.4365794514146,124.177147234351)) ;
#21761 = CARTESIAN_POINT('Ctrl Pts',(-20.604272042101,26.2565903710517,124.368482650199)) ;
#21762 = CARTESIAN_POINT('Ctrl Pts',(-20.0459994667024,26.4565594269051,124.457421972499)) ;
#21763 = CARTESIAN_POINT('Ctrl Pts',(-20.2051802401964,26.2765703465422,124.718824795122)) ;
#21764 = CARTESIAN_POINT('Ctrl Pts',(-19.6538522670745,26.476371856783,124.611397902099)) ;
#21765 = CARTESIAN_POINT('Ctrl Pts',(-19.7149987089246,26.2963827764202,124.911292999828)) ;
#21766 = CARTESIAN_POINT('Ctrl Pts',(-19.2292568239862,26.4963519648733,124.622952036836)) ;
#21767 = CARTESIAN_POINT('Ctrl Pts',(-19.1842547999823,26.3163628845105,124.925735636618)) ;
#21768 = CARTESIAN_POINT('Ctrl Pts',(-18.8278291774401,26.5162463484706,124.489264756815)) ;
#21769 = CARTESIAN_POINT('Ctrl Pts',(-18.6824717518944,26.3362572681077,124.758627144309)) ;
#21770 = CARTESIAN_POINT('Ctrl Pts',(-18.4954865718006,26.5361732764478,124.226604674122)) ;
#21771 = CARTESIAN_POINT('Ctrl Pts',(-18.2670439988586,26.3561841960849,124.430303289928)) ;
#21772 = CARTESIAN_POINT('Ctrl Pts',(-18.2725029600721,26.556068133749,123.867014296754)) ;
#21773 = CARTESIAN_POINT('Ctrl Pts',(-17.9883141683562,26.3760790533862,123.980817223551)) ;
#21774 = CARTESIAN_POINT('Ctrl Pts',(-18.1854325985899,26.5761073273527,123.449960855483)) ;
#21775 = CARTESIAN_POINT('Ctrl Pts',(-17.8794749235701,26.3961182469898,123.459500138785)) ;
#21776 = CARTESIAN_POINT('Ctrl Pts',(-18.2454084367871,26.5959472952634,123.032350538864)) ;
#21777 = CARTESIAN_POINT('Ctrl Pts',(-17.9544430376458,26.4159582149006,122.937489228161)) ;
#21778 = CARTESIAN_POINT('Ctrl Pts',(-18.4440381416904,26.6158621122275,122.658424632547)) ;
#21779 = CARTESIAN_POINT('Ctrl Pts',(-18.2027276437108,26.4358730318646,122.470081707864)) ;
#21780 = CARTESIAN_POINT('Ctrl Pts',(-18.75897849637,26.6358043576238,122.374552553596)) ;
#21781 = CARTESIAN_POINT('Ctrl Pts',(-18.596400995126,26.4558152772609,122.115240379138)) ;
#21782 = CARTESIAN_POINT('Ctrl Pts',(-19.1503485290493,26.6556764057383,122.215041816388)) ;
#21783 = CARTESIAN_POINT('Ctrl Pts',(-19.0856111707764,26.4756873253754,121.915849802114)) ;
#21784 = CARTESIAN_POINT('Ctrl Pts',(-19.5753925439647,26.6756874706924,122.198865355149)) ;
#21785 = CARTESIAN_POINT('Ctrl Pts',(-19.6169161682822,26.4956983903295,121.895626311636)) ;
#21786 = CARTESIAN_POINT('Ctrl Pts',(-19.9769190829482,26.695498994996,122.326876472295)) ;
#21787 = CARTESIAN_POINT('Ctrl Pts',(-20.118823655691,26.5155099146331,122.055636433992)) ;
#21788 = CARTESIAN_POINT('Ctrl Pts',(-20.3149929284387,26.7155942069594,122.58789233349)) ;
#21789 = CARTESIAN_POINT('Ctrl Pts',(-20.5414187886625,26.5356051265965,122.381904092641)) ;
#21790 = CARTESIAN_POINT('Ctrl Pts',(-20.5402392709743,26.7353749308792,122.943283604957)) ;
#21791 = CARTESIAN_POINT('Ctrl Pts',(-20.8229786362358,26.5553858505163,122.826139617815)) ;
#21792 = CARTESIAN_POINT('Ctrl Pts',(-20.6325355714334,26.755366006522,123.358044401428)) ;
#21793 = CARTESIAN_POINT('Ctrl Pts',(-20.9383530388371,26.5753769261591,123.344589665565)) ;
#21794 = CARTESIAN_POINT('Ctrl Pts',(-20.5777323731222,26.775247945565,123.777341421288)) ;
#21795 = CARTESIAN_POINT('Ctrl Pts',(-20.86985320622,26.5952588652021,123.868710610695)) ;
#21796 = CARTESIAN_POINT('Ctrl Pts',(-20.3829509016501,26.7952005500682,124.154152656679)) ;
#21797 = CARTESIAN_POINT('Ctrl Pts',(-20.6263804833536,26.6152114697054,124.339726432393)) ;
#21798 = CARTESIAN_POINT('Ctrl Pts',(-20.0720296957647,26.8150994187989,124.441175273159)) ;
#21799 = CARTESIAN_POINT('Ctrl Pts',(-20.2377323609478,26.635110338436,124.698507478413)) ;
#21800 = CARTESIAN_POINT('Ctrl Pts',(-19.682246570693,26.8349928186085,124.605258451714)) ;
#21801 = CARTESIAN_POINT('Ctrl Pts',(-19.750506384729,26.6550037382456,124.903616092832)) ;
#21802 = CARTESIAN_POINT('Ctrl Pts',(-19.2594063736317,26.8549019494485,124.627157490124)) ;
#21803 = CARTESIAN_POINT('Ctrl Pts',(-19.2219548120851,26.6749128690856,124.930993209538)) ;
#21804 = CARTESIAN_POINT('Ctrl Pts',(-18.8522665349481,26.8749340492121,124.502164719981)) ;
#21805 = CARTESIAN_POINT('Ctrl Pts',(-18.7130356342311,26.6949449688492,124.774763267432)) ;
#21806 = CARTESIAN_POINT('Ctrl Pts',(-18.5715001351461,26.8914661223815,124.290581364288)) ;
#21807 = CARTESIAN_POINT('Ctrl Pts',(-18.3620528555376,26.7114770420187,124.510268121194)) ;
#21808 = CARTESIAN_POINT('Ctrl Pts',(-18.3986933822299,26.9048014629875,124.069844703011)) ;
#21809 = CARTESIAN_POINT('Ctrl Pts',(-18.1460617747501,26.7248123826246,124.234367496516)) ;
#21810 = CARTESIAN_POINT('Ctrl Pts',(-18.3010328118348,26.9146440215272,123.887397849221)) ;
#21811 = CARTESIAN_POINT('Ctrl Pts',(-18.0239800547126,26.7346549411643,124.006303612785)) ;
#21812 = CARTESIAN_POINT('Ctrl Pts',(-18.234968179349,26.9246959283771,123.68668524791)) ;
#21813 = CARTESIAN_POINT('Ctrl Pts',(-17.9413973813911,26.7447068480142,123.755428033597)) ;
#21814 = CARTESIAN_POINT('Ctrl Pts',(-18.1952008801186,26.937944442768,123.411026766241)) ;
#21815 = CARTESIAN_POINT('Ctrl Pts',(-17.891686149238,26.7579553624051,123.410787353362)) ;
#21816 = CARTESIAN_POINT('Ctrl Pts',(-18.2364062598888,26.9545436177157,123.060472721167)) ;
#21817 = CARTESIAN_POINT('Ctrl Pts',(-17.9431815127596,26.7745545373529,122.972680824458)) ;
#21818 = CARTESIAN_POINT('Ctrl Pts',(-18.3945264788303,26.9711324035108,122.745229733751)) ;
#21819 = CARTESIAN_POINT('Ctrl Pts',(-18.1408483242503,26.7911433231479,122.578566000262)) ;
#21820 = CARTESIAN_POINT('Ctrl Pts',(-18.5797786495349,26.9844082198528,122.536429267407)) ;
#21821 = CARTESIAN_POINT('Ctrl Pts',(-18.3723926843041,26.8044191394899,122.317598644227)) ;
#21822 = CARTESIAN_POINT('Ctrl Pts',(-18.7438802886562,26.9943820706466,122.405894110244)) ;
#21823 = CARTESIAN_POINT('Ctrl Pts',(-18.5775216542846,26.8143929902837,122.15442033865)) ;
#21824 = CARTESIAN_POINT('Ctrl Pts',(-18.929271898675,27.004411102739,122.305482739616)) ;
#21825 = CARTESIAN_POINT('Ctrl Pts',(-18.8092589677791,26.8244220223761,122.028905565457)) ;
#21826 = CARTESIAN_POINT('Ctrl Pts',(-19.1264590553554,27.0143012282409,122.239497823847)) ;
#21827 = CARTESIAN_POINT('Ctrl Pts',(-19.0557421895212,26.834312147878,121.946421302957)) ;
#21828 = CARTESIAN_POINT('Ctrl Pts',(-19.3341576766828,27.0242937065124,122.208161049022)) ;
#21829 = CARTESIAN_POINT('Ctrl Pts',(-19.3153650354541,26.8443046261495,121.907247691411)) ;
#21830 = CARTESIAN_POINT('Ctrl Pts',(-19.5433352481452,27.0342449216098,122.213230891029)) ;
#21831 = CARTESIAN_POINT('Ctrl Pts',(-19.5768371046668,26.8542558412469,121.913582155201)) ;
#21832 = CARTESIAN_POINT('Ctrl Pts',(-19.7503716423327,27.0442934233648,122.255105192578)) ;
#21833 = CARTESIAN_POINT('Ctrl Pts',(-19.8356332457282,26.8643043430019,121.965922317603)) ;
#21834 = CARTESIAN_POINT('Ctrl Pts',(-19.9430662208723,27.0541347729816,122.330491998155)) ;
#21835 = CARTESIAN_POINT('Ctrl Pts',(-20.0765024472187,26.8741456926187,122.060153190044)) ;
#21836 = CARTESIAN_POINT('Ctrl Pts',(-20.1225333341149,27.0641210640018,122.439364927213)) ;
#21837 = CARTESIAN_POINT('Ctrl Pts',(-20.3008378724975,26.8841319836389,122.196241980051)) ;
#21838 = CARTESIAN_POINT('Ctrl Pts',(-20.2797057557656,27.0740576757304,122.57702448676)) ;
#21839 = CARTESIAN_POINT('Ctrl Pts',(-20.4973053062689,26.8940685953675,122.368314358404)) ;
#21840 = CARTESIAN_POINT('Ctrl Pts',(-20.4119625359954,27.084107551098,122.74176172172)) ;
#21841 = CARTESIAN_POINT('Ctrl Pts',(-20.662628518743,26.9041184707351,122.574234184223)) ;
#21842 = CARTESIAN_POINT('Ctrl Pts',(-20.5117431177263,27.0939580096334,122.92324291587)) ;
#21843 = CARTESIAN_POINT('Ctrl Pts',(-20.7873567686691,26.9139689292705,122.801084418396)) ;
#21844 = CARTESIAN_POINT('Ctrl Pts',(-20.579826322129,27.1039299465862,123.121493753205)) ;
#21845 = CARTESIAN_POINT('Ctrl Pts',(-20.8724634669083,26.9239408662233,123.048897162386)) ;
#21846 = CARTESIAN_POINT('Ctrl Pts',(-20.6125055315077,27.1139254035183,123.329105646214)) ;
#21847 = CARTESIAN_POINT('Ctrl Pts',(-20.9133152577875,26.9339363231554,123.308411671272)) ;
#21848 = CARTESIAN_POINT('Ctrl Pts',(-20.6083877682446,27.1239582105714,123.539972730989)) ;
#21849 = CARTESIAN_POINT('Ctrl Pts',(-20.9081708679061,26.9439691302085,123.571995622508)) ;
#21850 = CARTESIAN_POINT('Ctrl Pts',(-20.5686916631752,27.1338180971613,123.743433100123)) ;
#21851 = CARTESIAN_POINT('Ctrl Pts',(-20.8585534427238,26.9538290167985,123.826321841959)) ;
#21852 = CARTESIAN_POINT('Ctrl Pts',(-20.4936737353725,27.1438071777266,123.939559222509)) ;
#21853 = CARTESIAN_POINT('Ctrl Pts',(-20.7647835915375,26.9638180973637,124.071480590036)) ;
#21854 = CARTESIAN_POINT('Ctrl Pts',(-20.3863494619409,27.1537386569357,124.118661541936)) ;
#21855 = CARTESIAN_POINT('Ctrl Pts',(-20.6306305349959,26.9737495765729,124.29536007837)) ;
#21856 = CARTESIAN_POINT('Ctrl Pts',(-20.2490645865285,27.1637245163817,124.277504970353)) ;
#21857 = CARTESIAN_POINT('Ctrl Pts',(-20.4590264458182,26.9837354360188,124.493916247248)) ;
#21858 = CARTESIAN_POINT('Ctrl Pts',(-20.0852193557923,27.1737626670289,124.410486117788)) ;
#21859 = CARTESIAN_POINT('Ctrl Pts',(-20.254221659418,26.993773586666,124.66014484481)) ;
#21860 = CARTESIAN_POINT('Ctrl Pts',(-19.9044415797665,27.1836107575333,124.511442323854)) ;
#21861 = CARTESIAN_POINT('Ctrl Pts',(-20.0282504284219,27.0036216771704,124.786342691733)) ;
#21862 = CARTESIAN_POINT('Ctrl Pts',(-19.7047523070118,27.1936716660512,124.581101591854)) ;
#21863 = CARTESIAN_POINT('Ctrl Pts',(-19.7786397745395,27.0136825856884,124.873419336829)) ;
#21864 = CARTESIAN_POINT('Ctrl Pts',(-19.4993833052846,27.2035665132092,124.614334962714)) ;
#21865 = CARTESIAN_POINT('Ctrl Pts',(-19.5219286374244,27.0235774328464,124.914963808306)) ;
#21866 = CARTESIAN_POINT('Ctrl Pts',(-19.2904166566976,27.2135081852543,124.611948250234)) ;
#21867 = CARTESIAN_POINT('Ctrl Pts',(-19.2607200330095,27.0335191048914,124.911983091372)) ;
#21868 = CARTESIAN_POINT('Ctrl Pts',(-19.0837134685083,27.2235107123797,124.573148992734)) ;
#21869 = CARTESIAN_POINT('Ctrl Pts',(-19.002340474553,27.0435216320169,124.863486618766)) ;
#21870 = CARTESIAN_POINT('Ctrl Pts',(-18.886408762246,27.2335455035672,124.49851245076)) ;
#21871 = CARTESIAN_POINT('Ctrl Pts',(-18.755708647713,27.0535564232043,124.770193481186)) ;
#21872 = CARTESIAN_POINT('Ctrl Pts',(-18.7082920067272,27.2433903834263,124.393076161983)) ;
#21873 = CARTESIAN_POINT('Ctrl Pts',(-18.53306086531,27.0634013030634,124.63840012197)) ;
#21874 = CARTESIAN_POINT('Ctrl Pts',(-18.548717036597,27.2533762640448,124.256715634161)) ;
#21875 = CARTESIAN_POINT('Ctrl Pts',(-18.3335903392706,27.0733871836819,124.467951336687)) ;
#21876 = CARTESIAN_POINT('Ctrl Pts',(-18.415763782662,27.263310987138,124.095588178805)) ;
#21877 = CARTESIAN_POINT('Ctrl Pts',(-18.1673965821684,27.0833219067751,124.266543402248)) ;
#21878 = CARTESIAN_POINT('Ctrl Pts',(-18.3117355785266,27.2733688274492,123.911537425513)) ;
#21879 = CARTESIAN_POINT('Ctrl Pts',(-18.0373591121067,27.0933797470863,124.03648134582)) ;
#21880 = CARTESIAN_POINT('Ctrl Pts',(-18.2425753593927,27.2831893148457,123.716980331988)) ;
#21881 = CARTESIAN_POINT('Ctrl Pts',(-17.9509061764655,27.1032002344828,123.793285094069)) ;
#21882 = CARTESIAN_POINT('Ctrl Pts',(-18.2070714729757,27.2932497161908,123.508505960271)) ;
#21883 = CARTESIAN_POINT('Ctrl Pts',(-17.9065238901742,27.1132606358279,123.532692664086)) ;
#21884 = CARTESIAN_POINT('Ctrl Pts',(-18.2085717097183,27.3031806817437,123.299707474007)) ;
#21885 = CARTESIAN_POINT('Ctrl Pts',(-17.9083966530251,27.1231916013808,123.271694164607)) ;
#21886 = CARTESIAN_POINT('Ctrl Pts',(-18.2458677394489,27.3131195440802,123.094139009505)) ;
#21887 = CARTESIAN_POINT('Ctrl Pts',(-17.9550143490479,27.1331304637173,123.014732779571)) ;
#21888 = CARTESIAN_POINT('Ctrl Pts',(-18.3185162099704,27.3231052750064,122.897153471792)) ;
#21889 = CARTESIAN_POINT('Ctrl Pts',(-18.0458227293772,27.1431161946435,122.768499870868)) ;
#21890 = CARTESIAN_POINT('Ctrl Pts',(-18.4248467767158,27.3331296604338,122.715218646708)) ;
#21891 = CARTESIAN_POINT('Ctrl Pts',(-18.1787338062467,27.1531405800709,122.54108010085)) ;
#21892 = CARTESIAN_POINT('Ctrl Pts',(-18.5592899800235,27.3430329447871,122.556213400873)) ;
#21893 = CARTESIAN_POINT('Ctrl Pts',(-18.3467863406668,27.1630438644242,122.342321573022)) ;
#21894 = CARTESIAN_POINT('Ctrl Pts',(-18.7218362744338,27.3530929493651,122.42094597078)) ;
#21895 = CARTESIAN_POINT('Ctrl Pts',(-18.5499675318017,27.1731038690022,122.173235543931)) ;
#21896 = CARTESIAN_POINT('Ctrl Pts',(-18.9014128659292,27.3629362184342,122.3180699415)) ;
#21897 = CARTESIAN_POINT('Ctrl Pts',(-18.7744378365037,27.1829471380713,122.044638016558)) ;
#21898 = CARTESIAN_POINT('Ctrl Pts',(-19.0988286897178,27.3729267840419,122.246443873207)) ;
#21899 = CARTESIAN_POINT('Ctrl Pts',(-19.0212070083882,27.192937703679,121.955103241881)) ;
#21900 = CARTESIAN_POINT('Ctrl Pts',(-19.3044292359815,27.3828549158207,122.210437107956)) ;
#21901 = CARTESIAN_POINT('Ctrl Pts',(-19.2782077784814,27.2028658354578,121.910092465526)) ;
#21902 = CARTESIAN_POINT('Ctrl Pts',(-19.5144154098307,27.3928428029016,122.21031147887)) ;
#21903 = CARTESIAN_POINT('Ctrl Pts',(-19.5406906769413,27.2128537225387,121.909933250644)) ;
#21904 = CARTESIAN_POINT('Ctrl Pts',(-19.7221490194526,27.4028787524703,122.247173181467)) ;
#21905 = CARTESIAN_POINT('Ctrl Pts',(-19.8003580009036,27.2228896721074,121.956008127035)) ;
#21906 = CARTESIAN_POINT('Ctrl Pts',(-19.916892573696,27.4127336388491,122.317923368138)) ;
#21907 = CARTESIAN_POINT('Ctrl Pts',(-20.0437890490973,27.2327445584862,122.044444124203)) ;
#21908 = CARTESIAN_POINT('Ctrl Pts',(-20.0991236220355,27.422733053197,122.422656802109)) ;
#21909 = CARTESIAN_POINT('Ctrl Pts',(-20.2715790260407,27.2427439728341,122.175359156114)) ;
#21910 = CARTESIAN_POINT('Ctrl Pts',(-20.2589164113812,27.4326282183875,122.555908904654)) ;
#21911 = CARTESIAN_POINT('Ctrl Pts',(-20.47132188163,27.2526391380246,122.341923187153)) ;
#21912 = CARTESIAN_POINT('Ctrl Pts',(-20.3953279566597,27.4426885370794,122.71750152297)) ;
#21913 = CARTESIAN_POINT('Ctrl Pts',(-20.6418377253297,27.2626994567166,122.543912452748)) ;
#21914 = CARTESIAN_POINT('Ctrl Pts',(-20.4995174983559,27.4525386688555,122.896483303571)) ;
#21915 = CARTESIAN_POINT('Ctrl Pts',(-20.7720769168341,27.2725495884926,122.767639569015)) ;
#21916 = CARTESIAN_POINT('Ctrl Pts',(-20.5728149864719,27.4625692393058,123.094198738288)) ;
#21917 = CARTESIAN_POINT('Ctrl Pts',(-20.8637005068752,27.2825801589429,123.014783157539)) ;
#21918 = CARTESIAN_POINT('Ctrl Pts',(-20.6101494969086,27.4725833899786,123.301402871192)) ;
#21919 = CARTESIAN_POINT('Ctrl Pts',(-20.9103706252309,27.2925943096157,123.273787983254)) ;
#21920 = CARTESIAN_POINT('Ctrl Pts',(-20.6112662653975,27.482476323524,123.509383815082)) ;
#21921 = CARTESIAN_POINT('Ctrl Pts',(-20.911768495837,27.3024872431611,123.533764947733)) ;
#21922 = CARTESIAN_POINT('Ctrl Pts',(-20.5761521288518,27.4924658375142,123.716418000998)) ;
#21923 = CARTESIAN_POINT('Ctrl Pts',(-20.8678776029836,27.3124767571514,123.792558185261)) ;
#21924 = CARTESIAN_POINT('Ctrl Pts',(-20.5059891635455,27.5024196081667,123.913596204343)) ;
#21925 = CARTESIAN_POINT('Ctrl Pts',(-20.7801754400193,27.3224305278038,124.03903194835)) ;
#21926 = CARTESIAN_POINT('Ctrl Pts',(-20.4015400398466,27.5124673768272,124.097177756809)) ;
#21927 = CARTESIAN_POINT('Ctrl Pts',(-20.6496157399914,27.3324782964644,124.26850963764)) ;
#21928 = CARTESIAN_POINT('Ctrl Pts',(-20.2697294375057,27.522309103267,124.256684479157)) ;
#21929 = CARTESIAN_POINT('Ctrl Pts',(-20.4848531000536,27.3423200229042,124.467895083723)) ;
#21930 = CARTESIAN_POINT('Ctrl Pts',(-20.1102592973178,27.5322946200898,124.393158289807)) ;
#21931 = CARTESIAN_POINT('Ctrl Pts',(-20.2855162962699,27.3523055397269,124.638488743857)) ;
#21932 = CARTESIAN_POINT('Ctrl Pts',(-19.9303364745535,27.5422339517853,124.499474121132)) ;
#21933 = CARTESIAN_POINT('Ctrl Pts',(-20.0606131128351,27.3622448714225,124.771385186807)) ;
#21934 = CARTESIAN_POINT('Ctrl Pts',(-19.7327382041188,27.5522737214829,124.573617862549)) ;
#21935 = CARTESIAN_POINT('Ctrl Pts',(-19.8136159800649,27.37228464112,124.864066326302)) ;
#21936 = CARTESIAN_POINT('Ctrl Pts',(-19.5283912957834,27.5621618827317,124.611847447798)) ;
#21937 = CARTESIAN_POINT('Ctrl Pts',(-19.5581817302825,27.3821728023688,124.911855032732)) ;
#21938 = CARTESIAN_POINT('Ctrl Pts',(-19.3184025008245,27.5721514372341,124.614431043553)) ;
#21939 = CARTESIAN_POINT('Ctrl Pts',(-19.2956955404914,27.3921623568712,124.915085978907)) ;
#21940 = CARTESIAN_POINT('Ctrl Pts',(-19.1118246407992,27.5821098517577,124.580462400769)) ;
#21941 = CARTESIAN_POINT('Ctrl Pts',(-19.0374725439821,27.4021207713948,124.872626590807)) ;
#21942 = CARTESIAN_POINT('Ctrl Pts',(-18.9152594132557,27.5920097645871,124.512023957247)) ;
#21943 = CARTESIAN_POINT('Ctrl Pts',(-18.7917647458714,27.4120206842242,124.787079499337)) ;
#21944 = CARTESIAN_POINT('Ctrl Pts',(-18.7309264013132,27.602056464237,124.408951439022)) ;
#21945 = CARTESIAN_POINT('Ctrl Pts',(-18.5613480077617,27.4220673838741,124.658240132733)) ;
#21946 = CARTESIAN_POINT('Ctrl Pts',(-18.5695583676357,27.6119563245426,124.277459812412)) ;
#21947 = CARTESIAN_POINT('Ctrl Pts',(-18.3596364546277,27.4319672441797,124.493876043428)) ;
#21948 = CARTESIAN_POINT('Ctrl Pts',(-18.4313772500186,27.622007728748,124.117627545932)) ;
#21949 = CARTESIAN_POINT('Ctrl Pts',(-18.186909253097,27.4420186483852,124.294086730336)) ;
#21950 = CARTESIAN_POINT('Ctrl Pts',(-18.3247881894919,27.6318887656692,123.939292964072)) ;
#21951 = CARTESIAN_POINT('Ctrl Pts',(-18.0536713291326,27.4518996853063,124.071168267617)) ;
#21952 = CARTESIAN_POINT('Ctrl Pts',(-18.2496492643862,27.6418885978467,123.742988738701)) ;
#21953 = CARTESIAN_POINT('Ctrl Pts',(-17.9597465513536,27.4618995174838,123.825788262627)) ;
#21954 = CARTESIAN_POINT('Ctrl Pts',(-18.2098807597813,27.6518066008316,123.538271728212)) ;
#21955 = CARTESIAN_POINT('Ctrl Pts',(-17.9100347106082,27.4718175204687,123.56989145949)) ;
#21956 = CARTESIAN_POINT('Ctrl Pts',(-18.2062837040758,27.6618579067061,123.327027887074)) ;
#21957 = CARTESIAN_POINT('Ctrl Pts',(-17.9055372820663,27.4818688263432,123.305836914717)) ;
#21958 = CARTESIAN_POINT('Ctrl Pts',(-18.2385839581239,27.6717277300977,123.122017781039)) ;
#21959 = CARTESIAN_POINT('Ctrl Pts',(-17.9459117765369,27.4917386497348,123.049572996332)) ;
#21960 = CARTESIAN_POINT('Ctrl Pts',(-18.307368702007,27.681801896148,122.921759006394)) ;
#21961 = CARTESIAN_POINT('Ctrl Pts',(-18.0318915985893,27.5018128157851,122.799249602971)) ;
#21962 = CARTESIAN_POINT('Ctrl Pts',(-18.4071173488075,27.6916219802896,122.74095235675)) ;
#21963 = CARTESIAN_POINT('Ctrl Pts',(-18.1565773494833,27.5116328999267,122.573239483822)) ;
#21964 = CARTESIAN_POINT('Ctrl Pts',(-18.5399396605626,27.7017007070255,122.575930572394)) ;
#21965 = CARTESIAN_POINT('Ctrl Pts',(-18.3226042808018,27.5217116266626,122.366962086733)) ;
#21966 = CARTESIAN_POINT('Ctrl Pts',(-18.6958321778564,27.711552287675,122.439501623981)) ;
#21967 = CARTESIAN_POINT('Ctrl Pts',(-18.5174703780383,27.5315632073121,122.196424414338)) ;
#21968 = CARTESIAN_POINT('Ctrl Pts',(-18.8768591143373,27.7216254159734,122.329686829936)) ;
#21969 = CARTESIAN_POINT('Ctrl Pts',(-18.7437532834736,27.5416363356105,122.05915550415)) ;
#21970 = CARTESIAN_POINT('Ctrl Pts',(-19.069748360102,27.7314678938648,122.254738925638)) ;
#21971 = CARTESIAN_POINT('Ctrl Pts',(-18.9848658829686,27.5514788135019,121.965469396346)) ;
#21972 = CARTESIAN_POINT('Ctrl Pts',(-19.275402729767,27.7414485004629,122.213172865234)) ;
#21973 = CARTESIAN_POINT('Ctrl Pts',(-19.2419340497948,27.5614594201,121.913511275121)) ;
#21974 = CARTESIAN_POINT('Ctrl Pts',(-19.4859500150315,27.7514662094817,122.208323768403)) ;
#21975 = CARTESIAN_POINT('Ctrl Pts',(-19.505118136635,27.5714771291188,121.907449255122)) ;
#21976 = CARTESIAN_POINT('Ctrl Pts',(-19.6914845982736,27.7613523885191,122.23929217762)) ;
#21977 = CARTESIAN_POINT('Ctrl Pts',(-19.7620374996728,27.5813633081562,121.946159440311)) ;
#21978 = CARTESIAN_POINT('Ctrl Pts',(-19.8919086335487,27.7714100010914,122.306601119756)) ;
#21979 = CARTESIAN_POINT('Ctrl Pts',(-20.0125674013974,27.5914209207286,122.030295059284)) ;
#21980 = CARTESIAN_POINT('Ctrl Pts',(-20.0742918881656,27.7812863944636,122.405862590949)) ;
#21981 = CARTESIAN_POINT('Ctrl Pts',(-20.2405477178494,27.6012973141007,122.154372035112)) ;
#21982 = CARTESIAN_POINT('Ctrl Pts',(-20.2389323043103,27.791281422614,122.536416615308)) ;
#21983 = CARTESIAN_POINT('Ctrl Pts',(-20.4463485472987,27.6112923422511,122.317564461287)) ;
#21984 = CARTESIAN_POINT('Ctrl Pts',(-20.3785025030073,27.80130216946,122.694229664895)) ;
#21985 = CARTESIAN_POINT('Ctrl Pts',(-20.6208115759906,27.6213130890971,122.51483046535)) ;
#21986 = CARTESIAN_POINT('Ctrl Pts',(-20.4874494476852,27.8112042381264,122.871614573746)) ;
#21987 = CARTESIAN_POINT('Ctrl Pts',(-20.7569960330264,27.6312151577635,122.736562250952)) ;
#21988 = CARTESIAN_POINT('Ctrl Pts',(-20.5649160847513,27.8211949779461,123.066844849364)) ;
#21989 = CARTESIAN_POINT('Ctrl Pts',(-20.8538296011518,27.6412058975832,122.980600241119)) ;
#21990 = CARTESIAN_POINT('Ctrl Pts',(-20.6070370985664,27.8311581741564,123.272013328294)) ;
#21991 = CARTESIAN_POINT('Ctrl Pts',(-20.9064812123952,27.6511690937935,123.237061229662)) ;
#21992 = CARTESIAN_POINT('Ctrl Pts',(-20.6133758883929,27.8410623584565,123.480152818403)) ;
#21993 = CARTESIAN_POINT('Ctrl Pts',(-20.9144047817725,27.6610732780936,123.497236530681)) ;
#21994 = CARTESIAN_POINT('Ctrl Pts',(-20.5828360532262,27.8511228188474,123.689412748153)) ;
#21995 = CARTESIAN_POINT('Ctrl Pts',(-20.8762301626549,27.6711337384845,123.758811110914)) ;
#21996 = CARTESIAN_POINT('Ctrl Pts',(-20.5181122383662,27.8609633647182,123.885935058997)) ;
#21997 = CARTESIAN_POINT('Ctrl Pts',(-20.7953249519176,27.6809742843553,124.004465402187)) ;
#21998 = CARTESIAN_POINT('Ctrl Pts',(-20.4183061486459,27.8710255854299,124.072424108861)) ;
#21999 = CARTESIAN_POINT('Ctrl Pts',(-20.6705674371017,27.6910365050671,124.237576347375)) ;
#22000 = CARTESIAN_POINT('Ctrl Pts',(-20.2895881644942,27.8809227284465,124.235913842461)) ;
#22001 = CARTESIAN_POINT('Ctrl Pts',(-20.5096693378974,27.7009336480836,124.441939302609)) ;
#22002 = CARTESIAN_POINT('Ctrl Pts',(-20.1343799700791,27.8908539048637,124.375554329111)) ;
#22003 = CARTESIAN_POINT('Ctrl Pts',(-20.315658373556,27.7108648245008,124.61649018712)) ;
#22004 = CARTESIAN_POINT('Ctrl Pts',(-19.9551790503614,27.9008961186423,124.487164722517)) ;
#22005 = CARTESIAN_POINT('Ctrl Pts',(-20.091657303987,27.7209070382794,124.756002912722)) ;
#22006 = CARTESIAN_POINT('Ctrl Pts',(-19.762401523415,27.910782658845,124.564891732212)) ;
#22007 = CARTESIAN_POINT('Ctrl Pts',(-19.8506842942627,27.7307935784821,124.85316185408)) ;
#22008 = CARTESIAN_POINT('Ctrl Pts',(-19.5569511425706,27.9207762534504,124.608757066638)) ;
#22009 = CARTESIAN_POINT('Ctrl Pts',(-19.5938710456304,27.7407871730876,124.907993194414)) ;
#22010 = CARTESIAN_POINT('Ctrl Pts',(-19.3480204997779,27.930720128608,124.616215006894)) ;
#22011 = CARTESIAN_POINT('Ctrl Pts',(-19.3327071093546,27.7507310482451,124.917315275339)) ;
#22012 = CARTESIAN_POINT('Ctrl Pts',(-19.1406090152874,27.9406806647228,124.587509478741)) ;
#22013 = CARTESIAN_POINT('Ctrl Pts',(-19.0734423500519,27.7606915843599,124.881432829596)) ;
#22014 = CARTESIAN_POINT('Ctrl Pts',(-18.9405381225761,27.9506772680455,124.523103824295)) ;
#22015 = CARTESIAN_POINT('Ctrl Pts',(-18.823353749831,27.7706881876827,124.800925220385)) ;
#22016 = CARTESIAN_POINT('Ctrl Pts',(-18.7541744874109,27.960710351,124.424327030337)) ;
#22017 = CARTESIAN_POINT('Ctrl Pts',(-18.5903995182117,27.7807212706372,124.677453935382)) ;
#22018 = CARTESIAN_POINT('Ctrl Pts',(-18.5906478671095,27.9705615197016,124.297248746626)) ;
#22019 = CARTESIAN_POINT('Ctrl Pts',(-18.3859904696139,27.7905724393387,124.518604840361)) ;
#22020 = CARTESIAN_POINT('Ctrl Pts',(-18.4496441002172,27.9805240104005,124.142390521308)) ;
#22021 = CARTESIAN_POINT('Ctrl Pts',(-18.2097360022858,27.8005349300376,124.325031213336)) ;
#22022 = CARTESIAN_POINT('Ctrl Pts',(-18.3371397750335,27.9905524388182,123.964073852674)) ;
#22023 = CARTESIAN_POINT('Ctrl Pts',(-18.0691061956658,27.8105633584554,124.102135115778)) ;
#22024 = CARTESIAN_POINT('Ctrl Pts',(-18.2581916508595,28.0004628061828,123.771274447575)) ;
#22025 = CARTESIAN_POINT('Ctrl Pts',(-17.9704213296521,27.8204737258199,123.861134793012)) ;
#22026 = CARTESIAN_POINT('Ctrl Pts',(-18.2132715984884,28.0103976737979,123.567293786419)) ;
#22027 = CARTESIAN_POINT('Ctrl Pts',(-17.9142719852206,27.830408593435,123.606158130962)) ;
#22028 = CARTESIAN_POINT('Ctrl Pts',(-18.2045541391692,28.0204388157769,123.356384171661)) ;
#22029 = CARTESIAN_POINT('Ctrl Pts',(-17.9033759753097,27.840449735414,123.342521266579)) ;
#22030 = CARTESIAN_POINT('Ctrl Pts',(-18.2320173963766,28.0303259519801,123.150336225817)) ;
#22031 = CARTESIAN_POINT('Ctrl Pts',(-17.9377060396121,27.8503368716172,123.084960416994)) ;
#22032 = CARTESIAN_POINT('Ctrl Pts',(-18.2951662826154,28.0403182343835,122.949998669832)) ;
#22033 = CARTESIAN_POINT('Ctrl Pts',(-18.0166431581778,27.8603291540206,122.834538577221)) ;
#22034 = CARTESIAN_POINT('Ctrl Pts',(-18.3917805672602,28.0502667623487,122.764488512371)) ;
#22035 = CARTESIAN_POINT('Ctrl Pts',(-18.137412126526,27.8702776819858,122.602650848213)) ;
#22036 = CARTESIAN_POINT('Ctrl Pts',(-18.5187344195011,28.0602034935108,122.598611319051)) ;
#22037 = CARTESIAN_POINT('Ctrl Pts',(-18.2961056898845,27.8802144131479,122.395304507949)) ;
#22038 = CARTESIAN_POINT('Ctrl Pts',(-18.6731352153546,28.0701867043708,122.456413854557)) ;
#22039 = CARTESIAN_POINT('Ctrl Pts',(-18.4891076721817,27.8901976240079,122.217558370946)) ;
#22040 = CARTESIAN_POINT('Ctrl Pts',(-18.8511053323271,28.0802298035207,122.342850389306)) ;
#22041 = CARTESIAN_POINT('Ctrl Pts',(-18.7115707177152,27.9002407231578,122.075605016214)) ;
#22042 = CARTESIAN_POINT('Ctrl Pts',(-19.0418370727349,28.0900607677956,122.26317827219)) ;
#22043 = CARTESIAN_POINT('Ctrl Pts',(-18.9499871891245,27.9100716874327,121.976015433695)) ;
#22044 = CARTESIAN_POINT('Ctrl Pts',(-19.2483766387023,28.1001336201815,122.216578929442)) ;
#22045 = CARTESIAN_POINT('Ctrl Pts',(-19.2081615249894,27.9201445398186,121.917767583989)) ;
#22046 = CARTESIAN_POINT('Ctrl Pts',(-19.4555437861215,28.1099977478933,122.206790899523)) ;
#22047 = CARTESIAN_POINT('Ctrl Pts',(-19.4671216625185,27.9300086675304,121.905533740892)) ;
#22048 = CARTESIAN_POINT('Ctrl Pts',(-19.6645948451265,28.1200199500282,122.233024086339)) ;
#22049 = CARTESIAN_POINT('Ctrl Pts',(-19.7284352632182,27.9400308696653,121.938326646805)) ;
#22050 = CARTESIAN_POINT('Ctrl Pts',(-19.8658877748029,28.1300471429966,122.295670934239)) ;
#22051 = CARTESIAN_POINT('Ctrl Pts',(-19.980050984628,27.9500580626337,122.016636385366)) ;
#22052 = CARTESIAN_POINT('Ctrl Pts',(-20.0501626714237,28.1399027369636,122.39036087509)) ;
#22053 = CARTESIAN_POINT('Ctrl Pts',(-20.2103950643466,27.9599136566007,122.135000592785)) ;
#22054 = CARTESIAN_POINT('Ctrl Pts',(-20.2172929353047,28.1498599088289,122.516416762394)) ;
#22055 = CARTESIAN_POINT('Ctrl Pts',(-20.4193072748828,27.969870828466,122.29257198083)) ;
#22056 = CARTESIAN_POINT('Ctrl Pts',(-20.36088775291,28.1598987528273,122.67106650366)) ;
#22057 = CARTESIAN_POINT('Ctrl Pts',(-20.5987996284151,27.9799096724644,122.485885053549)) ;
#22058 = CARTESIAN_POINT('Ctrl Pts',(-20.4738977645388,28.1697727767028,122.845224021032)) ;
#22059 = CARTESIAN_POINT('Ctrl Pts',(-20.7400613604965,27.98978369634,122.703583668428)) ;
#22060 = CARTESIAN_POINT('Ctrl Pts',(-20.5565305050554,28.1798426026932,123.040098786974)) ;
#22061 = CARTESIAN_POINT('Ctrl Pts',(-20.8433506853364,27.9998535223304,122.947177423952)) ;
#22062 = CARTESIAN_POINT('Ctrl Pts',(-20.603072347858,28.1896758465905,123.241534739974)) ;
#22063 = CARTESIAN_POINT('Ctrl Pts',(-20.9015266940339,28.0096867662276,123.198973980949)) ;
#22064 = CARTESIAN_POINT('Ctrl Pts',(-20.614743890259,28.1997062743635,123.452075818359)) ;
#22065 = CARTESIAN_POINT('Ctrl Pts',(-20.9161142994382,28.0197171940007,123.462150342134)) ;
#22066 = CARTESIAN_POINT('Ctrl Pts',(-20.5890670250738,28.2097378911087,123.661414868918)) ;
#22067 = CARTESIAN_POINT('Ctrl Pts',(-20.8840166201033,28.0297488107458,123.72382387547)) ;
#22068 = CARTESIAN_POINT('Ctrl Pts',(-20.5290926772713,28.2195675680894,123.859156375962)) ;
#22069 = CARTESIAN_POINT('Ctrl Pts',(-20.80904662986,28.0395784877265,123.971001465148)) ;
#22070 = CARTESIAN_POINT('Ctrl Pts',(-20.4347263329766,28.2295570849293,124.046779224324)) ;
#22071 = CARTESIAN_POINT('Ctrl Pts',(-20.6910868706554,28.0495680045665,124.205529304447)) ;
#22072 = CARTESIAN_POINT('Ctrl Pts',(-20.308112533224,28.2396006970691,124.215750588149)) ;
#22073 = CARTESIAN_POINT('Ctrl Pts',(-20.5328182779669,28.0596116167062,124.416742316167)) ;
#22074 = CARTESIAN_POINT('Ctrl Pts',(-20.1577648900733,28.2494233034044,124.357312030463)) ;
#22075 = CARTESIAN_POINT('Ctrl Pts',(-20.3448814894554,28.0694342230415,124.593693576125)) ;
#22076 = CARTESIAN_POINT('Ctrl Pts',(-19.9816030750299,28.2594615333036,124.473500882314)) ;
#22077 = CARTESIAN_POINT('Ctrl Pts',(-20.124678185504,28.0794724529408,124.73892784558)) ;
#22078 = CARTESIAN_POINT('Ctrl Pts',(-19.7882531660864,28.2694725680956,124.556669707045)) ;
#22079 = CARTESIAN_POINT('Ctrl Pts',(-19.8829899980489,28.0894834877327,124.842887131756)) ;
#22080 = CARTESIAN_POINT('Ctrl Pts',(-19.5858129110288,28.2793702990627,124.604775415822)) ;
#22081 = CARTESIAN_POINT('Ctrl Pts',(-19.6299384968335,28.0993812186998,124.903017471924)) ;
#22082 = CARTESIAN_POINT('Ctrl Pts',(-19.376180880844,28.2893599269132,124.617388122946)) ;
#22083 = CARTESIAN_POINT('Ctrl Pts',(-19.3678981582499,28.1093708465503,124.918781274721)) ;
#22084 = CARTESIAN_POINT('Ctrl Pts',(-19.1682588404928,28.2993157173592,124.593418733339)) ;
#22085 = CARTESIAN_POINT('Ctrl Pts',(-19.1079954571358,28.1193266369963,124.888817431813)) ;
#22086 = CARTESIAN_POINT('Ctrl Pts',(-18.96810534998,28.3092431159212,124.534261318973)) ;
#22087 = CARTESIAN_POINT('Ctrl Pts',(-18.8578037171305,28.1292540355584,124.814868421456)) ;
#22088 = CARTESIAN_POINT('Ctrl Pts',(-18.7794564522439,28.3192687110311,124.440280835038)) ;
#22089 = CARTESIAN_POINT('Ctrl Pts',(-18.6219935808609,28.1392796306682,124.697390886151)) ;
#22090 = CARTESIAN_POINT('Ctrl Pts',(-18.6122710106145,28.3291545617007,124.31681671948)) ;
#22091 = CARTESIAN_POINT('Ctrl Pts',(-18.413012495007,28.1491654813378,124.543058534145)) ;
#22092 = CARTESIAN_POINT('Ctrl Pts',(-18.4672022044828,28.3391437415449,124.164964313106)) ;
#22093 = CARTESIAN_POINT('Ctrl Pts',(-18.2316780606301,28.159154661182,124.353241304876)) ;
#22094 = CARTESIAN_POINT('Ctrl Pts',(-18.350468282265,28.3491849286484,123.98908060691)) ;
#22095 = CARTESIAN_POINT('Ctrl Pts',(-18.085762555499,28.1691958482856,124.133385523761)) ;
#22096 = CARTESIAN_POINT('Ctrl Pts',(-18.267489993905,28.3590175721244,123.799757295272)) ;
#22097 = CARTESIAN_POINT('Ctrl Pts',(-17.9820414176768,28.1790284917615,123.896729581303)) ;
#22098 = CARTESIAN_POINT('Ctrl Pts',(-18.2172586034104,28.3690115218339,123.595747330936)) ;
#22099 = CARTESIAN_POINT('Ctrl Pts',(-17.9192545217861,28.189022441471,123.641716424028)) ;
#22100 = CARTESIAN_POINT('Ctrl Pts',(-18.2036074114145,28.3790406446104,123.385343767415)) ;
#22101 = CARTESIAN_POINT('Ctrl Pts',(-17.9021928664862,28.1990515642475,123.378711840277)) ;
#22102 = CARTESIAN_POINT('Ctrl Pts',(-18.2260142937554,28.3889167755291,123.178918899559)) ;
#22103 = CARTESIAN_POINT('Ctrl Pts',(-17.9302039422221,28.2089276951662,123.120680343544)) ;
#22104 = CARTESIAN_POINT('Ctrl Pts',(-18.2843913723889,28.3989148105461,122.977024252762)) ;
#22105 = CARTESIAN_POINT('Ctrl Pts',(-18.0031776926144,28.2189257301832,122.86831261201)) ;
#22106 = CARTESIAN_POINT('Ctrl Pts',(-18.3760366799018,28.4088287403048,122.789803762381)) ;
#22107 = CARTESIAN_POINT('Ctrl Pts',(-18.117736776842,28.2288396599419,122.634287677194)) ;
#22108 = CARTESIAN_POINT('Ctrl Pts',(-18.500337734295,28.4188719280426,122.619151689602)) ;
#22109 = CARTESIAN_POINT('Ctrl Pts',(-18.2731150794606,28.2388828476797,122.420974122389)) ;
#22110 = CARTESIAN_POINT('Ctrl Pts',(-18.6502217855382,28.428771770183,122.474737172695)) ;
#22111 = CARTESIAN_POINT('Ctrl Pts',(-18.4604722427515,28.2487826898201,122.24045743561)) ;
#22112 = CARTESIAN_POINT('Ctrl Pts',(-18.8242413063613,28.438763036991,122.357101788211)) ;
#22113 = CARTESIAN_POINT('Ctrl Pts',(-18.6779981948743,28.2587739566281,122.093415286291)) ;
#22114 = CARTESIAN_POINT('Ctrl Pts',(-19.0169763775656,28.4487951391229,122.271451770785)) ;
#22115 = CARTESIAN_POINT('Ctrl Pts',(-18.918918044841,28.2688060587601,121.986355077235)) ;
#22116 = CARTESIAN_POINT('Ctrl Pts',(-19.2182110681717,28.4586620200777,122.221141613254)) ;
#22117 = CARTESIAN_POINT('Ctrl Pts',(-19.1704626082505,28.2786729397148,121.923469734543)) ;
#22118 = CARTESIAN_POINT('Ctrl Pts',(-19.4277169110003,28.4686538113658,122.205851400272)) ;
#22119 = CARTESIAN_POINT('Ctrl Pts',(-19.432345213223,28.288664731003,121.904359612356)) ;
#22120 = CARTESIAN_POINT('Ctrl Pts',(-19.6374921877922,28.4786859272774,122.227662227062)) ;
#22121 = CARTESIAN_POINT('Ctrl Pts',(-19.694564039776,28.2986968469145,121.93162572317)) ;
#22122 = CARTESIAN_POINT('Ctrl Pts',(-19.8370378148064,28.4885522440774,122.284307432454)) ;
#22123 = CARTESIAN_POINT('Ctrl Pts',(-19.943995852301,28.3085631637145,122.002434913296)) ;
#22124 = CARTESIAN_POINT('Ctrl Pts',(-20.0261278855234,28.498539725551,122.375526578932)) ;
#22125 = CARTESIAN_POINT('Ctrl Pts',(-20.1803573809643,28.3185506451881,122.116461326157)) ;
#22126 = CARTESIAN_POINT('Ctrl Pts',(-20.1958916606712,28.5084846499299,122.497612228053)) ;
#22127 = CARTESIAN_POINT('Ctrl Pts',(-20.3925607131235,28.328495569567,122.269070719418)) ;
#22128 = CARTESIAN_POINT('Ctrl Pts',(-20.3432261236584,28.5185295358406,122.64887127178)) ;
#22129 = CARTESIAN_POINT('Ctrl Pts',(-20.5767268496923,28.3385404554777,122.458146387094)) ;
#22130 = CARTESIAN_POINT('Ctrl Pts',(-20.4600658639641,28.5283916395532,122.820164450749)) ;
#22131 = CARTESIAN_POINT('Ctrl Pts',(-20.7227745276264,28.3484025591903,122.672264744843)) ;
#22132 = CARTESIAN_POINT('Ctrl Pts',(-20.546882409536,28.5383832033776,123.011421338606)) ;
#22133 = CARTESIAN_POINT('Ctrl Pts',(-20.8312927348308,28.3583941230148,122.911337082898)) ;
#22134 = CARTESIAN_POINT('Ctrl Pts',(-20.5987837541194,28.5483160114405,123.213686812683)) ;
#22135 = CARTESIAN_POINT('Ctrl Pts',(-20.8961668071842,28.3683269310777,123.164169825498)) ;
#22136 = CARTESIAN_POINT('Ctrl Pts',(-20.6152968104347,28.5582531136769,123.42195527368)) ;
#22137 = CARTESIAN_POINT('Ctrl Pts',(-20.9168053566465,28.378264033314,123.424505796562)) ;
#22138 = CARTESIAN_POINT('Ctrl Pts',(-20.5948899082448,28.5683055599473,123.632285532663)) ;
#22139 = CARTESIAN_POINT('Ctrl Pts',(-20.8912939664117,28.3883164795844,123.687418366482)) ;
#22140 = CARTESIAN_POINT('Ctrl Pts',(-20.5397117951602,28.5781516755289,123.831810652888)) ;
#22141 = CARTESIAN_POINT('Ctrl Pts',(-20.8223185569164,28.398162595166,123.936824298385)) ;
#22142 = CARTESIAN_POINT('Ctrl Pts',(-20.4492135047243,28.5881996952438,124.022668210418)) ;
#22143 = CARTESIAN_POINT('Ctrl Pts',(-20.709193147176,28.4082106148809,124.175395051952)) ;
#22144 = CARTESIAN_POINT('Ctrl Pts',(-20.3279884165152,28.5981416468727,124.192947955947)) ;
#22145 = CARTESIAN_POINT('Ctrl Pts',(-20.5576594223878,28.4181525665098,124.388243230741)) ;
#22146 = CARTESIAN_POINT('Ctrl Pts',(-20.1794561705445,28.6080804278718,124.339907298682)) ;
#22147 = CARTESIAN_POINT('Ctrl Pts',(-20.3719920554206,28.4280913475089,124.571940487482)) ;
#22148 = CARTESIAN_POINT('Ctrl Pts',(-20.0060768723233,28.6181064765979,124.459748019633)) ;
#22149 = CARTESIAN_POINT('Ctrl Pts',(-20.155266255181,28.438117396235,124.721739105602)) ;
#22150 = CARTESIAN_POINT('Ctrl Pts',(-19.8172567237363,28.6279933370061,124.546699844584)) ;
#22151 = CARTESIAN_POINT('Ctrl Pts',(-19.9192398618305,28.4480042566432,124.830426395165)) ;
#22152 = CARTESIAN_POINT('Ctrl Pts',(-19.6133539599856,28.6380246121379,124.600393761194)) ;
#22153 = CARTESIAN_POINT('Ctrl Pts',(-19.6643603212813,28.458035531775,124.897541005947)) ;
#22154 = CARTESIAN_POINT('Ctrl Pts',(-19.4062711547036,28.6479075894383,124.617827169365)) ;
#22155 = CARTESIAN_POINT('Ctrl Pts',(-19.405507635062,28.4679185090754,124.919330220156)) ;
#22156 = CARTESIAN_POINT('Ctrl Pts',(-19.1957631832706,28.6579644428455,124.598722627596)) ;
#22157 = CARTESIAN_POINT('Ctrl Pts',(-19.14236864725,28.4779753624826,124.895445755536)) ;
#22158 = CARTESIAN_POINT('Ctrl Pts',(-18.9283731228152,28.6711326839214,124.526630695589)) ;
#22159 = CARTESIAN_POINT('Ctrl Pts',(-18.8081529113529,28.4911436035585,124.80533200887)) ;
#22160 = CARTESIAN_POINT('Ctrl Pts',(-18.6817983350219,28.6845337131479,124.384021538888)) ;
#22161 = CARTESIAN_POINT('Ctrl Pts',(-18.4999549682012,28.504544632785,124.627092881207)) ;
#22162 = CARTESIAN_POINT('Ctrl Pts',(-18.4857344421306,28.6977466298788,124.187192207811)) ;
#22163 = CARTESIAN_POINT('Ctrl Pts',(-18.2548346129752,28.5177575495159,124.381018273064)) ;
#22164 = CARTESIAN_POINT('Ctrl Pts',(-18.3657858162467,28.707675024332,124.016416499208)) ;
#22165 = CARTESIAN_POINT('Ctrl Pts',(-18.1049098192041,28.5276859439691,124.167554176501)) ;
#22166 = CARTESIAN_POINT('Ctrl Pts',(-18.2766712212058,28.7176565244601,123.826404589139)) ;
#22167 = CARTESIAN_POINT('Ctrl Pts',(-17.9935167509591,28.5376674440972,123.930036177092)) ;
#22168 = CARTESIAN_POINT('Ctrl Pts',(-18.2218707889986,28.7276970677302,123.622569483315)) ;
#22169 = CARTESIAN_POINT('Ctrl Pts',(-17.9250194853092,28.5477079873673,123.675241990111)) ;
#22170 = CARTESIAN_POINT('Ctrl Pts',(-18.2033757282844,28.7375463995133,123.416330418717)) ;
#22171 = CARTESIAN_POINT('Ctrl Pts',(-17.9019033242933,28.5575573191504,123.417442838969)) ;
#22172 = CARTESIAN_POINT('Ctrl Pts',(-18.2206940069242,28.747541803985,123.206912125949)) ;
#22173 = CARTESIAN_POINT('Ctrl Pts',(-17.9235537436292,28.5675527236221,123.155670875178)) ;
#22174 = CARTESIAN_POINT('Ctrl Pts',(-18.2745872662887,28.7575581314336,123.003350839589)) ;
#22175 = CARTESIAN_POINT('Ctrl Pts',(-17.990923682755,28.5775690510707,122.901217359065)) ;
#22176 = CARTESIAN_POINT('Ctrl Pts',(-18.3909335432918,28.7707817886001,122.750824717369)) ;
#22177 = CARTESIAN_POINT('Ctrl Pts',(-18.1363563321866,28.5907927082372,122.585573838039)) ;
#22178 = CARTESIAN_POINT('Ctrl Pts',(-18.5712652888683,28.7840760799895,122.533196711622)) ;
#22179 = CARTESIAN_POINT('Ctrl Pts',(-18.361738888197,28.6040869996266,122.313564150216)) ;
#22180 = CARTESIAN_POINT('Ctrl Pts',(-18.799057046922,28.797360430921,122.371600064136)) ;
#22181 = CARTESIAN_POINT('Ctrl Pts',(-18.6465253994931,28.6173713505581,122.111531614028)) ;
#22182 = CARTESIAN_POINT('Ctrl Pts',(-18.9884277129976,28.8073328119828,122.281692967666)) ;
#22183 = CARTESIAN_POINT('Ctrl Pts',(-18.8832307222806,28.6273437316199,121.999158080089)) ;
#22184 = CARTESIAN_POINT('Ctrl Pts',(-19.1891836686621,28.8172411916084,122.226029840972)) ;
#22185 = CARTESIAN_POINT('Ctrl Pts',(-19.1341788049863,28.6372521112455,121.929579826141)) ;
#22186 = CARTESIAN_POINT('Ctrl Pts',(-19.3995659070131,28.8272951903564,122.205875393867)) ;
#22187 = CARTESIAN_POINT('Ctrl Pts',(-19.3971551455222,28.6473061099936,121.904389073441)) ;
#22188 = CARTESIAN_POINT('Ctrl Pts',(-19.6062836932465,28.8371573874727,122.222079550303)) ;
#22189 = CARTESIAN_POINT('Ctrl Pts',(-19.6555567772795,28.6571683071099,121.924649710965)) ;
#22190 = CARTESIAN_POINT('Ctrl Pts',(-19.8780826757267,28.8505045138469,122.29182043757)) ;
#22191 = CARTESIAN_POINT('Ctrl Pts',(-19.9952798306344,28.670515433484,122.011813758423)) ;
#22192 = CARTESIAN_POINT('Ctrl Pts',(-20.1845000475927,28.8670414794883,122.464288153073)) ;
#22193 = CARTESIAN_POINT('Ctrl Pts',(-20.3783371558031,28.6870523991254,122.227433848027)) ;
#22194 = CARTESIAN_POINT('Ctrl Pts',(-20.4154369591003,28.8836760836622,122.732174044355)) ;
#22195 = CARTESIAN_POINT('Ctrl Pts',(-20.6669572705968,28.7036870032994,122.562229846375)) ;
#22196 = CARTESIAN_POINT('Ctrl Pts',(-20.5367399369156,28.8969658769049,122.98386445411)) ;
#22197 = CARTESIAN_POINT('Ctrl Pts',(-20.818619503667,28.716976796542,122.876897221786)) ;
#22198 = CARTESIAN_POINT('Ctrl Pts',(-20.5937434976173,28.9069185081643,123.1851719771)) ;
#22199 = CARTESIAN_POINT('Ctrl Pts',(-20.8898646071741,28.7269294278014,123.12852052043)) ;
#22200 = CARTESIAN_POINT('Ctrl Pts',(-20.6151704596498,28.916870475469,123.393312690541)) ;
#22201 = CARTESIAN_POINT('Ctrl Pts',(-20.916646989976,28.7368813951061,123.388702342932)) ;
#22202 = CARTESIAN_POINT('Ctrl Pts',(-20.5948058201253,28.9302377339328,123.673577606172)) ;
#22203 = CARTESIAN_POINT('Ctrl Pts',(-20.891192739327,28.7502486535699,123.739016958567)) ;
#22204 = CARTESIAN_POINT('Ctrl Pts',(-20.4800520817175,28.9467545458819,124.005580786161)) ;
#22205 = CARTESIAN_POINT('Ctrl Pts',(-20.7477418810432,28.7667654655191,124.154036877155)) ;
#22206 = CARTESIAN_POINT('Ctrl Pts',(-20.2120144615373,28.9667804408883,124.336293100921)) ;
#22207 = CARTESIAN_POINT('Ctrl Pts',(-20.4126932064644,28.7867913605254,124.567418944492)) ;
#22208 = CARTESIAN_POINT('Ctrl Pts',(-19.8510301281953,28.9865911710184,124.553536596618)) ;
#22209 = CARTESIAN_POINT('Ctrl Pts',(-19.9614615275447,28.8066020906556,124.838970603354)) ;
#22210 = CARTESIAN_POINT('Ctrl Pts',(-19.4344012108349,29.0065683871483,124.636109825588)) ;
#22211 = CARTESIAN_POINT('Ctrl Pts',(-19.4406750274565,28.8265793067854,124.942183198345)) ;
#22212 = CARTESIAN_POINT('Ctrl Pts',(-19.0157681070412,29.0264952625436,124.57095034557)) ;
#22213 = CARTESIAN_POINT('Ctrl Pts',(-18.9173848458449,28.8465061821807,124.860730356123)) ;
#22214 = CARTESIAN_POINT('Ctrl Pts',(-18.6457374117665,29.0463167240198,124.369076668043)) ;
#22215 = CARTESIAN_POINT('Ctrl Pts',(-18.4548495376105,28.866327643657,124.608386572972)) ;
#22216 = CARTESIAN_POINT('Ctrl Pts',(-18.3635430708779,29.0663910418292,124.048922971134)) ;
#22217 = CARTESIAN_POINT('Ctrl Pts',(-18.1021082199431,28.8864019614663,124.20819190284)) ;
#22218 = CARTESIAN_POINT('Ctrl Pts',(-18.2096162661091,29.0862390108371,123.655849066001)) ;
#22219 = CARTESIAN_POINT('Ctrl Pts',(-17.9097030414757,28.9062499304742,123.716849978485)) ;
#22220 = CARTESIAN_POINT('Ctrl Pts',(-18.1981447189495,29.1061860449003,123.231968651957)) ;
#22221 = CARTESIAN_POINT('Ctrl Pts',(-17.8953659112392,28.9261969645374,123.187000088179)) ;
#22222 = CARTESIAN_POINT('Ctrl Pts',(-18.3318077694759,29.1260819958724,122.830562780161)) ;
#22223 = CARTESIAN_POINT('Ctrl Pts',(-18.0624463345147,28.9460929155096,122.685244684184)) ;
#22224 = CARTESIAN_POINT('Ctrl Pts',(-18.5938358537856,29.1459774754907,122.498483434728)) ;
#22225 = CARTESIAN_POINT('Ctrl Pts',(-18.3899816868081,28.9659883951278,122.270147568337)) ;
#22226 = CARTESIAN_POINT('Ctrl Pts',(-18.9545509966917,29.1659335864555,122.274963150452)) ;
#22227 = CARTESIAN_POINT('Ctrl Pts',(-18.8408757372252,28.9859445060926,121.990748528834)) ;
#22228 = CARTESIAN_POINT('Ctrl Pts',(-19.3687523473574,29.1858381344955,122.188317116435)) ;
#22229 = CARTESIAN_POINT('Ctrl Pts',(-19.3586261760562,29.0058490541326,121.882442313881)) ;
#22230 = CARTESIAN_POINT('Ctrl Pts',(-19.7873033294093,29.2057122588146,122.247090838418)) ;
#22231 = CARTESIAN_POINT('Ctrl Pts',(-19.8818129365437,29.0257231784517,121.95590917428)) ;
#22232 = CARTESIAN_POINT('Ctrl Pts',(-20.1636458920224,29.2257667888136,122.447434307739)) ;
#22233 = CARTESIAN_POINT('Ctrl Pts',(-20.3522418344828,29.0457777084507,122.206339109689)) ;
#22234 = CARTESIAN_POINT('Ctrl Pts',(-20.4457143490153,29.2455743025736,122.760308780651)) ;
#22235 = CARTESIAN_POINT('Ctrl Pts',(-20.7048254925126,29.0655852222107,122.597429836113)) ;
#22236 = CARTESIAN_POINT('Ctrl Pts',(-20.6062625022629,29.2655576583413,123.153645694702)) ;
#22237 = CARTESIAN_POINT('Ctrl Pts',(-20.9055115949536,29.0855685779784,123.089100356984)) ;
#22238 = CARTESIAN_POINT('Ctrl Pts',(-20.6222571826096,29.2854759609252,123.57685578804)) ;
#22239 = CARTESIAN_POINT('Ctrl Pts',(-20.9255057422183,29.1054868805624,123.618111697477)) ;
#22240 = CARTESIAN_POINT('Ctrl Pts',(-20.4942524999631,29.305344176371,123.97953847386)) ;
#22241 = CARTESIAN_POINT('Ctrl Pts',(-20.7655021762044,29.1253550960081,124.121463964361)) ;
#22242 = CARTESIAN_POINT('Ctrl Pts',(-20.2337505644514,29.3253944931673,124.316857983923)) ;
#22243 = CARTESIAN_POINT('Ctrl Pts',(-20.4398756731327,29.1454054128044,124.543114839599)) ;
#22244 = CARTESIAN_POINT('Ctrl Pts',(-19.8787560188095,29.3451705550497,124.542547094781)) ;
#22245 = CARTESIAN_POINT('Ctrl Pts',(-19.9961359923068,29.1651814746869,124.82522657557)) ;
#22246 = CARTESIAN_POINT('Ctrl Pts',(-19.4626770517434,29.3652251607422,124.635063105545)) ;
#22247 = CARTESIAN_POINT('Ctrl Pts',(-19.4760372478541,29.1852360803793,124.9408742549)) ;
#22248 = CARTESIAN_POINT('Ctrl Pts',(-19.0452208405963,29.3850188498981,124.580591047788)) ;
#22249 = CARTESIAN_POINT('Ctrl Pts',(-18.9542188864203,29.2050297695352,124.872787108227)) ;
#22250 = CARTESIAN_POINT('Ctrl Pts',(-18.6678065643519,29.4049855414925,124.386372516553)) ;
#22251 = CARTESIAN_POINT('Ctrl Pts',(-18.4824497195716,29.2249964611296,124.630017164074)) ;
#22252 = CARTESIAN_POINT('Ctrl Pts',(-18.379791129464,29.4249455872434,124.074550900543)) ;
#22253 = CARTESIAN_POINT('Ctrl Pts',(-18.1224282621344,29.2449565068806,124.240242601981)) ;
#22254 = CARTESIAN_POINT('Ctrl Pts',(-18.2157634731263,29.4448438473937,123.684577273612)) ;
#22255 = CARTESIAN_POINT('Ctrl Pts',(-17.9173907834527,29.2648547670308,123.752777846934)) ;
#22256 = CARTESIAN_POINT('Ctrl Pts',(-18.1941500603982,29.4647387629429,123.262128718319)) ;
#22257 = CARTESIAN_POINT('Ctrl Pts',(-17.8903701259974,29.28474968258,123.224718223152)) ;
#22258 = CARTESIAN_POINT('Ctrl Pts',(-18.3177155519128,29.4846489433565,122.85722218228)) ;
#22259 = CARTESIAN_POINT('Ctrl Pts',(-18.0448227791641,29.3046598629936,122.718584462674)) ;
#22260 = CARTESIAN_POINT('Ctrl Pts',(-18.5722210885648,29.5045847424707,122.518222965031)) ;
#22261 = CARTESIAN_POINT('Ctrl Pts',(-18.3629508949474,29.3245956621079,122.294833096222)) ;
#22262 = CARTESIAN_POINT('Ctrl Pts',(-18.9271398359767,29.5245226041249,122.286384499788)) ;
#22263 = CARTESIAN_POINT('Ctrl Pts',(-18.8065966645385,29.344533523762,122.005031573975)) ;
#22264 = CARTESIAN_POINT('Ctrl Pts',(-19.3394465637527,29.5444416507625,122.189407632929)) ;
#22265 = CARTESIAN_POINT('Ctrl Pts',(-19.3219781329333,29.3644525703997,121.88380547982)) ;
#22266 = CARTESIAN_POINT('Ctrl Pts',(-19.7607048779396,29.5643905488167,122.23896191623)) ;
#22267 = CARTESIAN_POINT('Ctrl Pts',(-19.8485530096058,29.3844014684538,121.945745518254)) ;
#22268 = CARTESIAN_POINT('Ctrl Pts',(-20.1390238650554,29.5842963762597,122.428800132525)) ;
#22269 = CARTESIAN_POINT('Ctrl Pts',(-20.3214474198052,29.4043072958969,122.18303123303)) ;
#22270 = CARTESIAN_POINT('Ctrl Pts',(-20.381503088585,29.600879071625,122.684669772167)) ;
#22271 = CARTESIAN_POINT('Ctrl Pts',(-20.6245684184595,29.4208899912622,122.502888255951)) ;
#22272 = CARTESIAN_POINT('Ctrl Pts',(-20.5148467807965,29.6141532853487,122.929890317395)) ;
#22273 = CARTESIAN_POINT('Ctrl Pts',(-20.791234180934,29.4341642049858,122.809390920718)) ;
#22274 = CARTESIAN_POINT('Ctrl Pts',(-20.5818729164079,29.624200004548,123.130156956782)) ;
#22275 = CARTESIAN_POINT('Ctrl Pts',(-20.8750220852076,29.4442109241851,123.05973121324)) ;
#22276 = CARTESIAN_POINT('Ctrl Pts',(-20.6127109296286,29.6340440391937,123.334823989138)) ;
#22277 = CARTESIAN_POINT('Ctrl Pts',(-20.9135737768039,29.4540549588308,123.315549607641)) ;
#22278 = CARTESIAN_POINT('Ctrl Pts',(-20.6063479572666,29.6473784240982,123.615020683285)) ;
#22279 = CARTESIAN_POINT('Ctrl Pts',(-20.9056110532671,29.4673893437353,123.665862635849)) ;
#22280 = CARTESIAN_POINT('Ctrl Pts',(-20.5072137738658,29.663965641398,123.953603105851)) ;
#22281 = CARTESIAN_POINT('Ctrl Pts',(-20.7817183691016,29.4839765610351,124.089008121444)) ;
#22282 = CARTESIAN_POINT('Ctrl Pts',(-20.2982490380892,29.6805988534359,124.238824540592)) ;
#22283 = CARTESIAN_POINT('Ctrl Pts',(-20.5204871039959,29.500609773073,124.445591168462)) ;
#22284 = CARTESIAN_POINT('Ctrl Pts',(-20.0804621860381,29.6938812957081,124.413688383922)) ;
#22285 = CARTESIAN_POINT('Ctrl Pts',(-20.2482786094575,29.5138922153452,124.664142759317)) ;
#22286 = CARTESIAN_POINT('Ctrl Pts',(-19.8981216436981,29.7037871836223,124.514250466141)) ;
#22287 = CARTESIAN_POINT('Ctrl Pts',(-20.0203496111071,29.5237981032594,124.789853895898)) ;
#22288 = CARTESIAN_POINT('Ctrl Pts',(-19.6995040700482,29.7137756017274,124.582447696612)) ;
#22289 = CARTESIAN_POINT('Ctrl Pts',(-19.7720804977814,29.5337865213645,124.875101645455)) ;
#22290 = CARTESIAN_POINT('Ctrl Pts',(-19.491307008318,29.7237990289661,124.615012952645)) ;
#22291 = CARTESIAN_POINT('Ctrl Pts',(-19.5118312861888,29.5438099486033,124.9158105401)) ;
#22292 = CARTESIAN_POINT('Ctrl Pts',(-19.2831262713956,29.7337034600831,124.611097510971)) ;
#22293 = CARTESIAN_POINT('Ctrl Pts',(-19.2516162816116,29.5537143797203,124.910922144998)) ;
#22294 = CARTESIAN_POINT('Ctrl Pts',(-19.0093558420609,29.7469666126936,124.55825582872)) ;
#22295 = CARTESIAN_POINT('Ctrl Pts',(-18.9093488133413,29.5669775323307,124.844857601197)) ;
#22296 = CARTESIAN_POINT('Ctrl Pts',(-18.7545952522591,29.7602915105975,124.434343951779)) ;
#22297 = CARTESIAN_POINT('Ctrl Pts',(-18.5909285364746,29.5803024302346,124.689972489664)) ;
#22298 = CARTESIAN_POINT('Ctrl Pts',(-18.5439553830956,29.7735472542131,124.251793494169)) ;
#22299 = CARTESIAN_POINT('Ctrl Pts',(-18.3276416499704,29.5935581738502,124.461801734779)) ;
#22300 = CARTESIAN_POINT('Ctrl Pts',(-18.4117225992589,29.7835066276604,124.089495823393)) ;
#22301 = CARTESIAN_POINT('Ctrl Pts',(-18.1623453454126,29.6035175472975,124.258928464813)) ;
#22302 = CARTESIAN_POINT('Ctrl Pts',(-18.3095785405791,29.7934504515873,123.907068143892)) ;
#22303 = CARTESIAN_POINT('Ctrl Pts',(-18.0346636089127,29.6134613712245,124.030895956569)) ;
#22304 = CARTESIAN_POINT('Ctrl Pts',(-18.2401254145393,29.8034983957346,123.707589819514)) ;
#22305 = CARTESIAN_POINT('Ctrl Pts',(-17.9478442966657,29.6235093153718,123.781548712612)) ;
#22306 = CARTESIAN_POINT('Ctrl Pts',(-18.2068401315693,29.8133493669528,123.503171166359)) ;
#22307 = CARTESIAN_POINT('Ctrl Pts',(-17.906234953778,29.6333602865899,123.526025793516)) ;
#22308 = CARTESIAN_POINT('Ctrl Pts',(-18.20904682234,29.8233211843949,123.293567779389)) ;
#22309 = CARTESIAN_POINT('Ctrl Pts',(-17.9089904954044,29.643332104032,123.264021399714)) ;
#22310 = CARTESIAN_POINT('Ctrl Pts',(-18.2477491639959,29.833316606687,123.086997661394)) ;
#22311 = CARTESIAN_POINT('Ctrl Pts',(-17.9573656877064,29.6533275263241,123.005808163303)) ;
#22312 = CARTESIAN_POINT('Ctrl Pts',(-18.3222034367972,29.8433496718107,122.889655956978)) ;
#22313 = CARTESIAN_POINT('Ctrl Pts',(-18.0504309097234,29.6633605914478,122.75912999775)) ;
#22314 = CARTESIAN_POINT('Ctrl Pts',(-18.427820698995,29.8532150044759,122.711168026723)) ;
#22315 = CARTESIAN_POINT('Ctrl Pts',(-18.1824501820335,29.673225924113,122.536018472183)) ;
#22316 = CARTESIAN_POINT('Ctrl Pts',(-18.5636657279792,29.8631755470735,122.551802567031)) ;
#22317 = CARTESIAN_POINT('Ctrl Pts',(-18.352254460823,29.6831864667106,122.336809734032)) ;
#22318 = CARTESIAN_POINT('Ctrl Pts',(-18.7265192984171,29.8732092325752,122.41775022895)) ;
#22319 = CARTESIAN_POINT('Ctrl Pts',(-18.5558196647205,29.6932201522123,122.169242143868)) ;
#22320 = CARTESIAN_POINT('Ctrl Pts',(-18.9073064956514,29.8830940645654,122.315216883983)) ;
#22321 = CARTESIAN_POINT('Ctrl Pts',(-18.7818025397086,29.7031049842026,122.041072921772)) ;
#22322 = CARTESIAN_POINT('Ctrl Pts',(-19.1067239041188,29.8931614913253,122.244413082228)) ;
#22323 = CARTESIAN_POINT('Ctrl Pts',(-19.0310733364163,29.7131724109624,121.952565569517)) ;
#22324 = CARTESIAN_POINT('Ctrl Pts',(-19.3106948006957,29.9029999804841,122.209895700099)) ;
#22325 = CARTESIAN_POINT('Ctrl Pts',(-19.286036901977,29.7230109001213,121.909416064618)) ;
#22326 = CARTESIAN_POINT('Ctrl Pts',(-19.5222278617027,29.9130634616742,122.211069618084)) ;
#22327 = CARTESIAN_POINT('Ctrl Pts',(-19.550453199473,29.7330743813114,121.910880737687)) ;
#22328 = CARTESIAN_POINT('Ctrl Pts',(-19.7268617704073,29.9229576194894,122.24850430312)) ;
#22329 = CARTESIAN_POINT('Ctrl Pts',(-19.8062464008285,29.7429685391265,121.957671456219)) ;
#22330 = CARTESIAN_POINT('Ctrl Pts',(-19.9229782407006,29.9328994762337,122.320699146715)) ;
#22331 = CARTESIAN_POINT('Ctrl Pts',(-20.0513931602021,29.7529103958708,122.047912589705)) ;
#22332 = CARTESIAN_POINT('Ctrl Pts',(-20.1047692037057,29.9429019539051,122.426450883275)) ;
#22333 = CARTESIAN_POINT('Ctrl Pts',(-20.27863327422,29.7629128735422,122.180100002924)) ;
#22334 = CARTESIAN_POINT('Ctrl Pts',(-20.2657090613012,29.9529367582094,122.562825912537)) ;
#22335 = CARTESIAN_POINT('Ctrl Pts',(-20.4798098359431,29.7729476778465,122.350566712122)) ;
#22336 = CARTESIAN_POINT('Ctrl Pts',(-20.3982580149733,29.962781635055,122.72180138389)) ;
#22337 = CARTESIAN_POINT('Ctrl Pts',(-20.64549843004,29.7827925546922,122.549284780308)) ;
#22338 = CARTESIAN_POINT('Ctrl Pts',(-20.5029831129388,29.9727675146106,122.903710362573)) ;
#22339 = CARTESIAN_POINT('Ctrl Pts',(-20.7764071388104,29.7927784342477,122.776669844146)) ;
#22340 = CARTESIAN_POINT('Ctrl Pts',(-20.5743335334042,29.9827022449691,123.100047335692)) ;
#22341 = CARTESIAN_POINT('Ctrl Pts',(-20.8655976909384,29.8027131646062,123.022090489185)) ;
#22342 = CARTESIAN_POINT('Ctrl Pts',(-20.6107482776223,29.992760057282,123.308299706397)) ;
#22343 = CARTESIAN_POINT('Ctrl Pts',(-20.911118673284,29.8127709769191,123.2824053866)) ;
#22344 = CARTESIAN_POINT('Ctrl Pts',(-20.6108122645727,30.0025806494063,123.514793587701)) ;
#22345 = CARTESIAN_POINT('Ctrl Pts',(-20.9112011989042,29.8225915690435,123.540523528446)) ;
#22346 = CARTESIAN_POINT('Ctrl Pts',(-20.5743946708493,30.0126472350161,123.723224917904)) ;
#22347 = CARTESIAN_POINT('Ctrl Pts',(-20.8656816934186,29.8326581546532,123.801062971402)) ;
#22348 = CARTESIAN_POINT('Ctrl Pts',(-20.5034684423452,30.0225468155979,123.918938589695)) ;
#22349 = CARTESIAN_POINT('Ctrl Pts',(-20.7770260888292,29.8425577352351,124.045706385067)) ;
#22350 = CARTESIAN_POINT('Ctrl Pts',(-20.398156180313,30.0325984152762,124.102097749828)) ;
#22351 = CARTESIAN_POINT('Ctrl Pts',(-20.6453879764234,29.8526093349133,124.274656477308)) ;
#22352 = CARTESIAN_POINT('Ctrl Pts',(-20.2651035498594,30.0424726016932,124.261488906871)) ;
#22353 = CARTESIAN_POINT('Ctrl Pts',(-20.4790736605817,29.8624835213303,124.473897491922)) ;
#22354 = CARTESIAN_POINT('Ctrl Pts',(-20.1036145885846,30.0525290775741,124.397880998235)) ;
#22355 = CARTESIAN_POINT('Ctrl Pts',(-20.2772141277769,29.8725399972112,124.644389380226)) ;
#22356 = CARTESIAN_POINT('Ctrl Pts',(-19.9238362938821,30.0624220088767,124.502541628328)) ;
#22357 = CARTESIAN_POINT('Ctrl Pts',(-20.0524919644059,29.8824329285138,124.775217544899)) ;
#22358 = CARTESIAN_POINT('Ctrl Pts',(-19.7253526604774,30.0724847875893,124.575641997785)) ;
#22359 = CARTESIAN_POINT('Ctrl Pts',(-19.8043884253136,29.8924957072264,124.866595201475)) ;
#22360 = CARTESIAN_POINT('Ctrl Pts',(-19.5217089265332,30.0823273131705,124.612461273804)) ;
#22361 = CARTESIAN_POINT('Ctrl Pts',(-19.5498333322758,29.9023382328076,124.91262179111)) ;
#22362 = CARTESIAN_POINT('Ctrl Pts',(-19.3117032501177,30.0923180785953,124.613877366419)) ;
#22363 = CARTESIAN_POINT('Ctrl Pts',(-19.2873260771025,29.9123289982325,124.914394172825)) ;
#22364 = CARTESIAN_POINT('Ctrl Pts',(-19.1059111788541,30.1022461545934,124.578985148832)) ;
#22365 = CARTESIAN_POINT('Ctrl Pts',(-19.0300851291776,29.9222570742305,124.870781057726)) ;
#22366 = CARTESIAN_POINT('Ctrl Pts',(-18.9079961280173,30.1122340649804,124.508814514259)) ;
#22367 = CARTESIAN_POINT('Ctrl Pts',(-18.7826904157509,29.9322449846175,124.783069756764)) ;
#22368 = CARTESIAN_POINT('Ctrl Pts',(-18.7245848851423,30.1222699771053,124.404544827108)) ;
#22369 = CARTESIAN_POINT('Ctrl Pts',(-18.5534253143983,29.9422808967425,124.652734665094)) ;
#22370 = CARTESIAN_POINT('Ctrl Pts',(-18.5647574103382,30.132124989953,124.272686477183)) ;
#22371 = CARTESIAN_POINT('Ctrl Pts',(-18.3536388771245,29.9521359095901,124.487912827377)) ;
#22372 = CARTESIAN_POINT('Ctrl Pts',(-18.4280975268948,30.1421239358693,124.11300608856)) ;
#22373 = CARTESIAN_POINT('Ctrl Pts',(-18.1828123336801,29.9621348555064,124.288313606199)) ;
#22374 = CARTESIAN_POINT('Ctrl Pts',(-18.3221216583478,30.1520208483173,123.933916262018)) ;
#22375 = CARTESIAN_POINT('Ctrl Pts',(-18.0503403718914,29.9720317679544,124.064451745925)) ;
#22376 = CARTESIAN_POINT('Ctrl Pts',(-18.2476869675524,30.1620746464108,123.736121592027)) ;
#22377 = CARTESIAN_POINT('Ctrl Pts',(-17.9572951648542,29.9820855660479,123.817209301492)) ;
#22378 = CARTESIAN_POINT('Ctrl Pts',(-18.209328142363,30.1719555672375,123.531942530913)) ;
#22379 = CARTESIAN_POINT('Ctrl Pts',(-17.9093444927588,29.9919664868746,123.56198502385)) ;
#22380 = CARTESIAN_POINT('Ctrl Pts',(-18.2065963316718,30.1819600932352,123.321657997475)) ;
#22381 = CARTESIAN_POINT('Ctrl Pts',(-17.9059278138796,30.0019710128723,123.299129283876)) ;
#22382 = CARTESIAN_POINT('Ctrl Pts',(-18.2404207061427,30.1919440568527,123.114471153255)) ;
#22383 = CARTESIAN_POINT('Ctrl Pts',(-17.9482064112771,30.0119549764898,123.040145215749)) ;
#22384 = CARTESIAN_POINT('Ctrl Pts',(-18.31026366629,30.201983697404,122.915313410186)) ;
#22385 = CARTESIAN_POINT('Ctrl Pts',(-18.035508186737,30.0219946170411,122.791197498885)) ;
#22386 = CARTESIAN_POINT('Ctrl Pts',(-18.4113981835528,30.2118277230187,122.734755075974)) ;
#22387 = CARTESIAN_POINT('Ctrl Pts',(-18.161925212928,30.0318386426558,122.565497657734)) ;
#22388 = CARTESIAN_POINT('Ctrl Pts',(-18.5438338536838,30.221818728836,122.571724660386)) ;
#22389 = CARTESIAN_POINT('Ctrl Pts',(-18.3274685805744,30.0418296484732,122.361708399386)) ;
#22390 = CARTESIAN_POINT('Ctrl Pts',(-18.7036229588605,30.2318565203682,122.433886669261)) ;
#22391 = CARTESIAN_POINT('Ctrl Pts',(-18.5272036340267,30.0518674400053,122.189409573137)) ;
#22392 = CARTESIAN_POINT('Ctrl Pts',(-18.8812446957364,30.2417009201566,122.327651393259)) ;
#22393 = CARTESIAN_POINT('Ctrl Pts',(-18.749230903998,30.0617118397937,122.056613364073)) ;
#22394 = CARTESIAN_POINT('Ctrl Pts',(-19.0771915548651,30.2516857207133,122.252443734513)) ;
#22395 = CARTESIAN_POINT('Ctrl Pts',(-18.994164126273,30.0716966403505,121.962602178295)) ;
#22396 = CARTESIAN_POINT('Ctrl Pts',(-19.2823241886974,30.2616252441245,122.212483119528)) ;
#22397 = CARTESIAN_POINT('Ctrl Pts',(-19.2505801464928,30.0816361637616,121.912649736868)) ;
#22398 = CARTESIAN_POINT('Ctrl Pts',(-19.4933414984696,30.2716649632255,122.20875992218)) ;
#22399 = CARTESIAN_POINT('Ctrl Pts',(-19.5143516088782,30.0916758828626,121.907994125418)) ;
#22400 = CARTESIAN_POINT('Ctrl Pts',(-19.698697204164,30.2815531351448,122.241136729093)) ;
#22401 = CARTESIAN_POINT('Ctrl Pts',(-19.7710473972636,30.1015640547819,121.948463714533)) ;
#22402 = CARTESIAN_POINT('Ctrl Pts',(-19.8974368961156,30.2915426975618,122.308992544338)) ;
#22403 = CARTESIAN_POINT('Ctrl Pts',(-20.0194726827981,30.1115536171989,122.033282181041)) ;
#22404 = CARTESIAN_POINT('Ctrl Pts',(-20.0807289084001,30.3015010697565,122.410148468044)) ;
#22405 = CARTESIAN_POINT('Ctrl Pts',(-20.2485888048623,30.1215119893936,122.159725978258)) ;
#22406 = CARTESIAN_POINT('Ctrl Pts',(-20.2430415790186,30.3114011439872,122.540440637745)) ;
#22407 = CARTESIAN_POINT('Ctrl Pts',(-20.451481155513,30.1314120636243,122.322590700227)) ;
#22408 = CARTESIAN_POINT('Ctrl Pts',(-20.3822575057102,30.3214472403608,122.699250508298)) ;
#22409 = CARTESIAN_POINT('Ctrl Pts',(-20.6255019413428,30.1414581599979,122.521102011054)) ;
#22410 = CARTESIAN_POINT('Ctrl Pts',(-20.4903053212277,30.3313558243579,122.877358635903)) ;
#22411 = CARTESIAN_POINT('Ctrl Pts',(-20.7605632740528,30.151366743995,122.743737177707)) ;
#22412 = CARTESIAN_POINT('Ctrl Pts',(-20.56692385887,30.3413664029488,123.073373311009)) ;
#22413 = CARTESIAN_POINT('Ctrl Pts',(-20.8563375787038,30.1613773225859,122.988755129718)) ;
#22414 = CARTESIAN_POINT('Ctrl Pts',(-20.6080032804155,30.3513955610616,123.280185120993)) ;
#22415 = CARTESIAN_POINT('Ctrl Pts',(-20.9076881587369,30.1714064806987,123.247269528944)) ;
#22416 = CARTESIAN_POINT('Ctrl Pts',(-20.6127668223826,30.3612484428997,123.487255373469)) ;
#22417 = CARTESIAN_POINT('Ctrl Pts',(-20.913643859901,30.1812593625368,123.506108579083)) ;
#22418 = CARTESIAN_POINT('Ctrl Pts',(-20.5818009833245,30.3712080040507,123.694340585296)) ;
#22419 = CARTESIAN_POINT('Ctrl Pts',(-20.8749374874299,30.1912189236878,123.764965708006)) ;
#22420 = CARTESIAN_POINT('Ctrl Pts',(-20.5144631349101,30.3812464386398,123.894334448527)) ;
#22421 = CARTESIAN_POINT('Ctrl Pts',(-20.7907663164554,30.2012573582769,124.014958246547)) ;
#22422 = CARTESIAN_POINT('Ctrl Pts',(-20.4154074111559,30.3911197108669,124.076778134823)) ;
#22423 = CARTESIAN_POINT('Ctrl Pts',(-20.6669470046296,30.211130630504,124.243014320118)) ;
#22424 = CARTESIAN_POINT('Ctrl Pts',(-20.283556385648,30.4011929528604,124.24244097245)) ;
#22425 = CARTESIAN_POINT('Ctrl Pts',(-20.5021342923516,30.2212038724976,124.450093173102)) ;
#22426 = CARTESIAN_POINT('Ctrl Pts',(-20.1290404897392,30.4110132843935,124.379433616432)) ;
#22427 = CARTESIAN_POINT('Ctrl Pts',(-20.3089888716899,30.2310242040306,124.621335698669)) ;
#22428 = CARTESIAN_POINT('Ctrl Pts',(-19.9486420914419,30.4210919456203,124.490474607517)) ;
#22429 = CARTESIAN_POINT('Ctrl Pts',(-20.0834917211719,30.2411028652574,124.760137415769)) ;
#22430 = CARTESIAN_POINT('Ctrl Pts',(-19.7560754413222,30.4309435409145,124.566851656652)) ;
#22431 = CARTESIAN_POINT('Ctrl Pts',(-19.8427824861803,30.2509544605516,124.855609977345)) ;
#22432 = CARTESIAN_POINT('Ctrl Pts',(-19.5487326187181,30.4410166761433,124.609735878305)) ;
#22433 = CARTESIAN_POINT('Ctrl Pts',(-19.5836045391597,30.2610275957804,124.909215904106)) ;
#22434 = CARTESIAN_POINT('Ctrl Pts',(-19.3418837703433,30.4508591116683,124.615794712703)) ;
#22435 = CARTESIAN_POINT('Ctrl Pts',(-19.3250420856673,30.2708700313055,124.916790254833)) ;
#22436 = CARTESIAN_POINT('Ctrl Pts',(-19.1341767024053,30.4608398808017,124.586121780913)) ;
#22437 = CARTESIAN_POINT('Ctrl Pts',(-19.0654078751379,30.2808508004389,124.879699535808)) ;
#22438 = CARTESIAN_POINT('Ctrl Pts',(-18.9341621364853,30.4708569820456,124.520222155215)) ;
#22439 = CARTESIAN_POINT('Ctrl Pts',(-18.8153894691253,30.2908679016827,124.797325621791)) ;
#22440 = CARTESIAN_POINT('Ctrl Pts',(-18.7508125062853,30.4807454296474,124.422211803213)) ;
#22441 = CARTESIAN_POINT('Ctrl Pts',(-18.5862012535222,30.3007563492846,124.674812609811)) ;
#22442 = CARTESIAN_POINT('Ctrl Pts',(-18.5845129446099,30.4908011438283,124.291721984471)) ;
#22443 = CARTESIAN_POINT('Ctrl Pts',(-18.378326748722,30.3108120634654,124.511700910524)) ;
#22444 = CARTESIAN_POINT('Ctrl Pts',(-18.44588508889,30.5006763502421,124.137161226805)) ;
#22445 = CARTESIAN_POINT('Ctrl Pts',(-18.2050407985295,30.3206872698793,124.31849941652)) ;
#22446 = CARTESIAN_POINT('Ctrl Pts',(-18.3344500450704,30.5106714027149,123.959022928956)) ;
#22447 = CARTESIAN_POINT('Ctrl Pts',(-18.065746667546,30.330682322352,124.095826539079)) ;
#22448 = CARTESIAN_POINT('Ctrl Pts',(-18.2557384460612,30.520693286677,123.763577906026)) ;
#22449 = CARTESIAN_POINT('Ctrl Pts',(-17.9673568014916,30.3407042063141,123.851520456621)) ;
#22450 = CARTESIAN_POINT('Ctrl Pts',(-18.2124447067718,30.5305972592063,123.559917806185)) ;
#22451 = CARTESIAN_POINT('Ctrl Pts',(-17.9132391133063,30.3506081788434,123.596944459868)) ;
#22452 = CARTESIAN_POINT('Ctrl Pts',(-18.204806352772,30.5405857558672,123.350065475818)) ;
#22453 = CARTESIAN_POINT('Ctrl Pts',(-17.9036909635563,30.3605966755043,123.334628818861)) ;
#22454 = CARTESIAN_POINT('Ctrl Pts',(-18.2337889801412,30.5505495531152,123.142620805064)) ;
#22455 = CARTESIAN_POINT('Ctrl Pts',(-17.9399190541115,30.3705604727523,123.075322497842)) ;
#22456 = CARTESIAN_POINT('Ctrl Pts',(-18.2974874686317,30.5604535764232,122.944369701572)) ;
#22457 = CARTESIAN_POINT('Ctrl Pts',(-18.019542401481,30.3804644960603,122.827507706759)) ;
#22458 = CARTESIAN_POINT('Ctrl Pts',(-18.3963113380305,30.5705140797448,122.757403023843)) ;
#22459 = CARTESIAN_POINT('Ctrl Pts',(-18.1430719623568,30.3905249993819,122.593799613876)) ;
#22460 = CARTESIAN_POINT('Ctrl Pts',(-18.5230838015688,30.5803546148847,122.593882778984)) ;
#22461 = CARTESIAN_POINT('Ctrl Pts',(-18.3015384279696,30.4003655345218,122.38939813401)) ;
#22462 = CARTESIAN_POINT('Ctrl Pts',(-18.6795561688118,30.5904168355893,122.451559837919)) ;
#22463 = CARTESIAN_POINT('Ctrl Pts',(-18.4971286724099,30.4104277552264,122.211494771059)) ;
#22464 = CARTESIAN_POINT('Ctrl Pts',(-18.8555743115362,30.6003139893655,122.340587366803)) ;
#22465 = CARTESIAN_POINT('Ctrl Pts',(-18.7171521979687,30.4203249090026,122.072778646605)) ;
#22466 = CARTESIAN_POINT('Ctrl Pts',(-19.0485703229917,30.610245122751,122.260955111829)) ;
#22467 = CARTESIAN_POINT('Ctrl Pts',(-18.9583979844501,30.4302560423881,121.973238309069)) ;
#22468 = CARTESIAN_POINT('Ctrl Pts',(-19.2547965608815,30.6202874978967,122.215768412004)) ;
#22469 = CARTESIAN_POINT('Ctrl Pts',(-19.216180617271,30.4402984175338,121.916755158295)) ;
#22470 = CARTESIAN_POINT('Ctrl Pts',(-19.4624589820246,30.6301734356628,122.207050198295)) ;
#22471 = CARTESIAN_POINT('Ctrl Pts',(-19.4757597411927,30.4501843553,121.905857590778)) ;
#22472 = CARTESIAN_POINT('Ctrl Pts',(-19.6707860504758,30.6401692786477,122.234500227154)) ;
#22473 = CARTESIAN_POINT('Ctrl Pts',(-19.7361687240311,30.4601801982848,121.940170527014)) ;
#22474 = CARTESIAN_POINT('Ctrl Pts',(-19.8701217771489,30.6501112565263,122.297396578507)) ;
#22475 = CARTESIAN_POINT('Ctrl Pts',(-19.9853388632678,30.4701221761634,122.018791502423)) ;
#22476 = CARTESIAN_POINT('Ctrl Pts',(-20.0559439542631,30.6600706310073,122.393853881732)) ;
#22477 = CARTESIAN_POINT('Ctrl Pts',(-20.2176167858868,30.4800815506444,122.139363771227)) ;
#22478 = CARTESIAN_POINT('Ctrl Pts',(-20.2229095752647,30.6700672468411,122.521521564149)) ;
#22479 = CARTESIAN_POINT('Ctrl Pts',(-20.4263236161457,30.4900781664782,122.298948878856)) ;
#22480 = CARTESIAN_POINT('Ctrl Pts',(-20.3654814517331,30.6801014654146,122.676991794271)) ;
#22481 = CARTESIAN_POINT('Ctrl Pts',(-20.6045380695498,30.5001123850517,122.493286837832)) ;
#22482 = CARTESIAN_POINT('Ctrl Pts',(-20.4770590422529,30.6899545326252,122.851511404317)) ;
#22483 = CARTESIAN_POINT('Ctrl Pts',(-20.7440103711108,30.5099654522623,122.711437778196)) ;
#22484 = CARTESIAN_POINT('Ctrl Pts',(-20.5580675426808,30.6999147905028,123.044595067161)) ;
#22485 = CARTESIAN_POINT('Ctrl Pts',(-20.8452704862501,30.5199257101399,122.952793072304)) ;
#22486 = CARTESIAN_POINT('Ctrl Pts',(-20.6044003781511,30.7099438172084,123.250294695878)) ;
#22487 = CARTESIAN_POINT('Ctrl Pts',(-20.9031858777252,30.5299547368455,123.209917654151)) ;
#22488 = CARTESIAN_POINT('Ctrl Pts',(-20.6142563398137,30.7198540242428,123.458395760156)) ;
#22489 = CARTESIAN_POINT('Ctrl Pts',(-20.9155052003231,30.5398649438799,123.470044892547)) ;
#22490 = CARTESIAN_POINT('Ctrl Pts',(-20.5883067682827,30.7297889348904,123.665646410074)) ;
#22491 = CARTESIAN_POINT('Ctrl Pts',(-20.8830672767706,30.5497998545275,123.729108750999)) ;
#22492 = CARTESIAN_POINT('Ctrl Pts',(-20.525923055177,30.7398300650696,123.867307187014)) ;
#22493 = CARTESIAN_POINT('Ctrl Pts',(-20.8050869196827,30.5598409847068,123.981184304442)) ;
#22494 = CARTESIAN_POINT('Ctrl Pts',(-20.4310732674177,30.7497172054396,124.052276123954)) ;
#22495 = CARTESIAN_POINT('Ctrl Pts',(-20.6865234424483,30.5697281250767,124.212396007676)) ;
#22496 = CARTESIAN_POINT('Ctrl Pts',(-20.3045079136013,30.7597094829755,124.219919068454)) ;
#22497 = CARTESIAN_POINT('Ctrl Pts',(-20.5283158328247,30.5797204026127,124.421949250781)) ;
#22498 = CARTESIAN_POINT('Ctrl Pts',(-20.1513705963158,30.7696580262439,124.36238740214)) ;
#22499 = CARTESIAN_POINT('Ctrl Pts',(-20.336893127493,30.589668945881,124.600034325977)) ;
#22500 = CARTESIAN_POINT('Ctrl Pts',(-19.97621673164,30.7795947010611,124.476202086606)) ;
#22501 = CARTESIAN_POINT('Ctrl Pts',(-20.117949669728,30.5996056206982,124.742302120517)) ;
#22502 = CARTESIAN_POINT('Ctrl Pts',(-19.7831216512904,30.7895781219974,124.558506793433)) ;
#22503 = CARTESIAN_POINT('Ctrl Pts',(-19.8765801266705,30.6095890416346,124.845182022236)) ;
#22504 = CARTESIAN_POINT('Ctrl Pts',(-19.577416346165,30.7996204371867,124.605973059919)) ;
#22505 = CARTESIAN_POINT('Ctrl Pts',(-19.619448424608,30.6196313568238,124.904513792509)) ;
#22506 = CARTESIAN_POINT('Ctrl Pts',(-19.3708401231471,30.8094607546259,124.617114838702)) ;
#22507 = CARTESIAN_POINT('Ctrl Pts',(-19.3612267210301,30.629471674263,124.918439915204)) ;
#22508 = CARTESIAN_POINT('Ctrl Pts',(-19.1614550331297,30.8194904586834,124.592230575313)) ;
#22509 = CARTESIAN_POINT('Ctrl Pts',(-19.0994956244019,30.6395013783205,124.887333257162)) ;
#22510 = CARTESIAN_POINT('Ctrl Pts',(-18.9599146448353,30.8295114154059,124.530878822072)) ;
#22511 = CARTESIAN_POINT('Ctrl Pts',(-18.84757050077,30.649522335043,124.810642476183)) ;
#22512 = CARTESIAN_POINT('Ctrl Pts',(-18.7747291699173,30.8393779577095,124.437402415365)) ;
#22513 = CARTESIAN_POINT('Ctrl Pts',(-18.6160882477537,30.6593888773466,124.69379526334)) ;
#22514 = CARTESIAN_POINT('Ctrl Pts',(-18.6051688450948,30.8494490576546,124.310638457262)) ;
#22515 = CARTESIAN_POINT('Ctrl Pts',(-18.4041389450964,30.6694599772918,124.535339469786)) ;
#22516 = CARTESIAN_POINT('Ctrl Pts',(-18.4634769424933,30.8592911318322,124.159844576277)) ;
#22517 = CARTESIAN_POINT('Ctrl Pts',(-18.2270241518516,30.6793020514693,124.346845255088)) ;
#22518 = CARTESIAN_POINT('Ctrl Pts',(-18.3481138935015,30.8692519264192,123.98508540905)) ;
#22519 = CARTESIAN_POINT('Ctrl Pts',(-18.0828214570917,30.6892628460564,124.128395071014)) ;
#22520 = CARTESIAN_POINT('Ctrl Pts',(-18.2645872120616,30.8792897993201,123.791299482673)) ;
#22521 = CARTESIAN_POINT('Ctrl Pts',(-17.9784145006715,30.6993007189572,123.886162207482)) ;
#22522 = CARTESIAN_POINT('Ctrl Pts',(-18.2163875155882,30.8891640848642,123.589358215528)) ;
#22523 = CARTESIAN_POINT('Ctrl Pts',(-17.9181661940265,30.7091750045013,123.63373426702)) ;
#22524 = CARTESIAN_POINT('Ctrl Pts',(-18.203753574643,30.8992338352781,123.378065938577)) ;
#22525 = CARTESIAN_POINT('Ctrl Pts',(-17.9023753757216,30.7192447549152,123.369619175597)) ;
#22526 = CARTESIAN_POINT('Ctrl Pts',(-18.2273236827773,30.9090671198127,123.172670784879)) ;
#22527 = CARTESIAN_POINT('Ctrl Pts',(-17.9318397718058,30.7290780394499,123.112874144442)) ;
#22528 = CARTESIAN_POINT('Ctrl Pts',(-18.2867987026179,30.9190974606128,122.970368878916)) ;
#22529 = CARTESIAN_POINT('Ctrl Pts',(-18.0061852690051,30.7391083802499,122.859997359419)) ;
#22530 = CARTESIAN_POINT('Ctrl Pts',(-18.3810728614528,30.9291293846124,122.781698599394)) ;
#22531 = CARTESIAN_POINT('Ctrl Pts',(-18.1240293775023,30.7491403042495,122.624160309324)) ;
#22532 = CARTESIAN_POINT('Ctrl Pts',(-18.50375518637,30.9389579195483,122.6154474201)) ;
#22533 = CARTESIAN_POINT('Ctrl Pts',(-18.2773844645063,30.7589688391854,122.416346355351)) ;
#22534 = CARTESIAN_POINT('Ctrl Pts',(-18.6555659033438,30.948951697313,122.470205569998)) ;
#22535 = CARTESIAN_POINT('Ctrl Pts',(-18.4671493140597,30.7689626169501,122.234795344671)) ;
#22536 = CARTESIAN_POINT('Ctrl Pts',(-18.8311197714127,30.9589794077985,122.353474256892)) ;
#22537 = CARTESIAN_POINT('Ctrl Pts',(-18.6865926220814,30.7789903274356,122.088882738916)) ;
#22538 = CARTESIAN_POINT('Ctrl Pts',(-19.021483587405,30.9688678186325,122.269936336135)) ;
#22539 = CARTESIAN_POINT('Ctrl Pts',(-18.924548918543,30.7888787382696,121.984461740876)) ;
#22540 = CARTESIAN_POINT('Ctrl Pts',(-19.2251633873121,30.978844669168,122.219928658385)) ;
#22541 = CARTESIAN_POINT('Ctrl Pts',(-19.1791493957345,30.7988555888051,121.921954029357)) ;
#22542 = CARTESIAN_POINT('Ctrl Pts',(-19.4347905985392,30.9888364657185,122.206004671817)) ;
#22543 = CARTESIAN_POINT('Ctrl Pts',(-19.4411836962534,30.8088473853556,121.904551040875)) ;
#22544 = CARTESIAN_POINT('Ctrl Pts',(-19.6445006365015,30.9988724718122,122.229041741586)) ;
#22545 = CARTESIAN_POINT('Ctrl Pts',(-19.7033209422536,30.8188833914493,121.933349289194)) ;
#22546 = CARTESIAN_POINT('Ctrl Pts',(-19.8434060708219,31.008723206075,122.286751984525)) ;
#22547 = CARTESIAN_POINT('Ctrl Pts',(-19.9519531581678,30.8287341257121,122.005489324719)) ;
#22548 = CARTESIAN_POINT('Ctrl Pts',(-20.0320403039582,31.0187144646032,122.379080702505)) ;
#22549 = CARTESIAN_POINT('Ctrl Pts',(-20.1877451626918,30.8387253842403,122.12090221111)) ;
#22550 = CARTESIAN_POINT('Ctrl Pts',(-20.2006501988176,31.0286323595064,122.501784715894)) ;
#22551 = CARTESIAN_POINT('Ctrl Pts',(-20.3985067246429,30.8486432791435,122.274284311981)) ;
#22552 = CARTESIAN_POINT('Ctrl Pts',(-20.3470107237814,31.0386605011694,122.65350091565)) ;
#22553 = CARTESIAN_POINT('Ctrl Pts',(-20.5814557895788,30.8586714208065,122.463931047394)) ;
#22554 = CARTESIAN_POINT('Ctrl Pts',(-20.4632104004851,31.0485456692853,122.825802329779)) ;
#22555 = CARTESIAN_POINT('Ctrl Pts',(-20.726703975958,30.8685565889224,122.679309656422)) ;
#22556 = CARTESIAN_POINT('Ctrl Pts',(-20.5490845959354,31.0585350327913,123.017454794976)) ;
#22557 = CARTESIAN_POINT('Ctrl Pts',(-20.8340446604117,30.8785459524284,122.918876333056)) ;
#22558 = CARTESIAN_POINT('Ctrl Pts',(-20.6002096975552,31.0685761678013,123.22226668955)) ;
#22559 = CARTESIAN_POINT('Ctrl Pts',(-20.8979488651774,30.8885870874385,123.174891648262)) ;
#22560 = CARTESIAN_POINT('Ctrl Pts',(-20.615028805326,31.0784088359894,123.42844428818)) ;
#22561 = CARTESIAN_POINT('Ctrl Pts',(-20.916470523059,30.8984197556265,123.432614768819)) ;
#22562 = CARTESIAN_POINT('Ctrl Pts',(-20.5940744638475,31.0884027389439,123.637499008543)) ;
#22563 = CARTESIAN_POINT('Ctrl Pts',(-20.8902751541959,30.908413658581,123.693933046635)) ;
#22564 = CARTESIAN_POINT('Ctrl Pts',(-20.5365069814263,31.0984320240284,123.840336990073)) ;
#22565 = CARTESIAN_POINT('Ctrl Pts',(-20.8183135578191,30.9184429436655,123.947479863912)) ;
#22566 = CARTESIAN_POINT('Ctrl Pts',(-20.446304755453,31.1083075524703,124.027344707869)) ;
#22567 = CARTESIAN_POINT('Ctrl Pts',(-20.705558307434,30.9283184721074,124.181239071671)) ;
#22568 = CARTESIAN_POINT('Ctrl Pts',(-20.3236808566818,31.1183078350863,124.198085320137)) ;
#22569 = CARTESIAN_POINT('Ctrl Pts',(-20.55227636311,30.9383187547235,124.394663488926)) ;
#22570 = CARTESIAN_POINT('Ctrl Pts',(-20.1746825112907,31.1282198511434,124.343800205569)) ;
#22571 = CARTESIAN_POINT('Ctrl Pts',(-20.3660263502005,30.9482307707805,124.576805636963)) ;
#22572 = CARTESIAN_POINT('Ctrl Pts',(-20.0004530429304,31.1382619264824,124.46299621068)) ;
#22573 = CARTESIAN_POINT('Ctrl Pts',(-20.148238159027,30.9582728461195,124.725798531691)) ;
#22574 = CARTESIAN_POINT('Ctrl Pts',(-19.8108716546696,31.1481617591385,124.548900830841)) ;
#22575 = CARTESIAN_POINT('Ctrl Pts',(-19.9112599341149,30.9681726787756,124.833177229003)) ;
#22576 = CARTESIAN_POINT('Ctrl Pts',(-19.6074951368638,31.1581541597165,124.601515467069)) ;
#22577 = CARTESIAN_POINT('Ctrl Pts',(-19.6570385216495,30.9781650793536,124.898943043692)) ;
#22578 = CARTESIAN_POINT('Ctrl Pts',(-19.3971675954827,31.1681881814759,124.617712800031)) ;
#22579 = CARTESIAN_POINT('Ctrl Pts',(-19.3941289164041,30.988199101113,124.91918719167)) ;
#22580 = CARTESIAN_POINT('Ctrl Pts',(-19.1907487982186,31.1780527923171,124.59775750716)) ;
#22581 = CARTESIAN_POINT('Ctrl Pts',(-19.1361050769742,30.9980637119542,124.894240456014)) ;
#22582 = CARTESIAN_POINT('Ctrl Pts',(-18.9881977091377,31.1880451917782,124.542038359077)) ;
#22583 = CARTESIAN_POINT('Ctrl Pts',(-18.8829168166101,31.0080561114154,124.824588928341)) ;
#22584 = CARTESIAN_POINT('Ctrl Pts',(-18.7978278631162,31.1980771451111,124.451266994197)) ;
#22585 = CARTESIAN_POINT('Ctrl Pts',(-18.6449556256928,31.0180880647483,124.711122383822)) ;
#22586 = CARTESIAN_POINT('Ctrl Pts',(-18.6287533564004,31.2079435040528,124.331095273272)) ;
#22587 = CARTESIAN_POINT('Ctrl Pts',(-18.433613598993,31.0279544236899,124.56090527812)) ;
#22588 = CARTESIAN_POINT('Ctrl Pts',(-18.4811055178957,31.2179309795386,124.181843664757)) ;
#22589 = CARTESIAN_POINT('Ctrl Pts',(-18.2490556295149,31.0379418991757,124.374338785496)) ;
#22590 = CARTESIAN_POINT('Ctrl Pts',(-18.3620004505735,31.2278758857271,124.009975732587)) ;
#22591 = CARTESIAN_POINT('Ctrl Pts',(-18.1001763827017,31.0478868053642,124.159502137119)) ;
#22592 = CARTESIAN_POINT('Ctrl Pts',(-18.2737974644408,31.2379208503873,123.81812345337)) ;
#22593 = CARTESIAN_POINT('Ctrl Pts',(-17.9899251037199,31.0579317700244,123.919685682728)) ;
#22594 = CARTESIAN_POINT('Ctrl Pts',(-18.2210312867946,31.2477826572922,123.617606509006)) ;
#22595 = CARTESIAN_POINT('Ctrl Pts',(-17.9239698947395,31.0677935769293,123.669038395262)) ;
#22596 = CARTESIAN_POINT('Ctrl Pts',(-18.2032568478729,31.2577753295979,123.408304026805)) ;
#22597 = CARTESIAN_POINT('Ctrl Pts',(-17.9017545884407,31.0777862492351,123.407409964502)) ;
#22598 = CARTESIAN_POINT('Ctrl Pts',(-18.222001276921,31.2677040005433,123.200401767921)) ;
#22599 = CARTESIAN_POINT('Ctrl Pts',(-17.9251878868137,31.0877149201804,123.147532162219)) ;
#22600 = CARTESIAN_POINT('Ctrl Pts',(-18.2763524420486,31.2776565427686,122.998365459932)) ;
#22601 = CARTESIAN_POINT('Ctrl Pts',(-17.9931295756622,31.0976674624057,122.894987346514)) ;
#22602 = CARTESIAN_POINT('Ctrl Pts',(-18.3653072061262,31.2876578987645,122.807825356539)) ;
#22603 = CARTESIAN_POINT('Ctrl Pts',(-18.1043255909368,31.1076688184016,122.656813330348)) ;
#22604 = CARTESIAN_POINT('Ctrl Pts',(-18.4865417491966,31.2976865110392,122.635347065935)) ;
#22605 = CARTESIAN_POINT('Ctrl Pts',(-18.2558710625769,31.1176974306763,122.441217023634)) ;
#22606 = CARTESIAN_POINT('Ctrl Pts',(-18.6332380965549,31.3075508455887,122.488744885021)) ;
#22607 = CARTESIAN_POINT('Ctrl Pts',(-18.4392436560099,31.1275617652258,122.257966085798)) ;
#22608 = CARTESIAN_POINT('Ctrl Pts',(-18.8051439882642,31.3175431696653,122.36805505233)) ;
#22609 = CARTESIAN_POINT('Ctrl Pts',(-18.6541277020736,31.1375540893024,122.107106052772)) ;
#22610 = CARTESIAN_POINT('Ctrl Pts',(-18.9941591698767,31.3274706620311,122.279486435379)) ;
#22611 = CARTESIAN_POINT('Ctrl Pts',(-18.8903979931826,31.1474815816683,121.99639777191)) ;
#22612 = CARTESIAN_POINT('Ctrl Pts',(-19.1976565576999,31.337498020582,122.224557944539)) ;
#22613 = CARTESIAN_POINT('Ctrl Pts',(-19.1447705223875,31.1575089402191,121.927739862365)) ;
#22614 = CARTESIAN_POINT('Ctrl Pts',(-19.4046860684407,31.3473844386331,122.205835676361)) ;
#22615 = CARTESIAN_POINT('Ctrl Pts',(-19.403557785468,31.1673953582702,121.904339822956)) ;
#22616 = CARTESIAN_POINT('Ctrl Pts',(-19.6148093834641,31.3574161733685,122.223490530873)) ;
#22617 = CARTESIAN_POINT('Ctrl Pts',(-19.6662117593913,31.1774270930056,121.926411212978)) ;
#22618 = CARTESIAN_POINT('Ctrl Pts',(-19.8157458443054,31.3672977546117,122.27637611023)) ;
#22619 = CARTESIAN_POINT('Ctrl Pts',(-19.9173816828502,31.1873086742489,121.992520931665)) ;
#22620 = CARTESIAN_POINT('Ctrl Pts',(-20.0078493459752,31.3773597326441,122.364859285606)) ;
#22621 = CARTESIAN_POINT('Ctrl Pts',(-20.1575099536661,31.1973706522812,122.103127502672)) ;
#22622 = CARTESIAN_POINT('Ctrl Pts',(-20.1782249889718,31.3872168110058,122.482873113296)) ;
#22623 = CARTESIAN_POINT('Ctrl Pts',(-20.3704779128565,31.2072277306429,122.250647114545)) ;
#22624 = CARTESIAN_POINT('Ctrl Pts',(-20.3278279199944,31.3972113841118,122.630365681166)) ;
#22625 = CARTESIAN_POINT('Ctrl Pts',(-20.557479635411,31.2172223037489,122.435014859895)) ;
#22626 = CARTESIAN_POINT('Ctrl Pts',(-20.4488094488748,31.4071371803994,122.800422727047)) ;
#22627 = CARTESIAN_POINT('Ctrl Pts',(-20.7087042530508,31.2271481000365,122.647587798087)) ;
#22628 = CARTESIAN_POINT('Ctrl Pts',(-20.5393550256187,31.4171625475691,122.990728200173)) ;
#22629 = CARTESIAN_POINT('Ctrl Pts',(-20.8218837391766,31.2371734672062,122.885470873075)) ;
#22630 = CARTESIAN_POINT('Ctrl Pts',(-20.5948502492867,31.427058627223,123.191245455736)) ;
#22631 = CARTESIAN_POINT('Ctrl Pts',(-20.8912500206041,31.2470695468601,123.136118325641)) ;
#22632 = CARTESIAN_POINT('Ctrl Pts',(-20.6153065851422,31.4370537069285,123.400378513475)) ;
#22633 = CARTESIAN_POINT('Ctrl Pts',(-20.916817797818,31.2570646265657,123.397534145115)) ;
#22634 = CARTESIAN_POINT('Ctrl Pts',(-20.5987327650594,31.4470787947444,123.610482201889)) ;
#22635 = CARTESIAN_POINT('Ctrl Pts',(-20.8960973227342,31.2670897143815,123.660166672547)) ;
#22636 = CARTESIAN_POINT('Ctrl Pts',(-20.5297708945593,31.4602626171116,123.878943016611)) ;
#22637 = CARTESIAN_POINT('Ctrl Pts',(-20.809893476644,31.2802735367488,123.995726533553)) ;
#22638 = CARTESIAN_POINT('Ctrl Pts',(-20.3913865952829,31.4735847352576,124.126114166337)) ;
#22639 = CARTESIAN_POINT('Ctrl Pts',(-20.6369390480152,31.2935956548947,124.30466223955)) ;
#22640 = CARTESIAN_POINT('Ctrl Pts',(-20.1945187909929,31.4869639448852,124.327003652239)) ;
#22641 = CARTESIAN_POINT('Ctrl Pts',(-20.3908148582284,31.3069748645223,124.555818133117)) ;
#22642 = CARTESIAN_POINT('Ctrl Pts',(-20.0266170027822,31.4968021821294,124.447815006563)) ;
#22643 = CARTESIAN_POINT('Ctrl Pts',(-20.1809438414753,31.3168131017665,124.706820601801)) ;
#22644 = CARTESIAN_POINT('Ctrl Pts',(-19.8359227028424,31.5068751053881,124.539840727089)) ;
#22645 = CARTESIAN_POINT('Ctrl Pts',(-19.9425721439745,31.3268860250252,124.821852782534)) ;
#22646 = CARTESIAN_POINT('Ctrl Pts',(-19.6364695609574,31.5167317468432,124.596111822066)) ;
#22647 = CARTESIAN_POINT('Ctrl Pts',(-19.6932575438715,31.3367426664803,124.89218888602)) ;
#22648 = CARTESIAN_POINT('Ctrl Pts',(-19.4276732492853,31.5267171223493,124.617725780505)) ;
#22649 = CARTESIAN_POINT('Ctrl Pts',(-19.4322556852193,31.3467280419864,124.919201640466)) ;
#22650 = CARTESIAN_POINT('Ctrl Pts',(-19.1491517758467,31.5400011538097,124.597557778909)) ;
#22651 = CARTESIAN_POINT('Ctrl Pts',(-19.0841345592013,31.3600120734468,124.893999424143)) ;
#22652 = CARTESIAN_POINT('Ctrl Pts',(-18.8168268265356,31.55651994568,124.4835998274)) ;
#22653 = CARTESIAN_POINT('Ctrl Pts',(-18.6686831095259,31.3765308653172,124.751522351196)) ;
#22654 = CARTESIAN_POINT('Ctrl Pts',(-18.5395236647983,31.5733056626867,124.258964597931)) ;
#22655 = CARTESIAN_POINT('Ctrl Pts',(-18.3221176258635,31.3933165823238,124.470780414967)) ;
#22656 = CARTESIAN_POINT('Ctrl Pts',(-18.3774782260285,31.5864188111957,124.035919217362)) ;
#22657 = CARTESIAN_POINT('Ctrl Pts',(-18.1195171640873,31.4064297308328,124.19192546978)) ;
#22658 = CARTESIAN_POINT('Ctrl Pts',(-18.2842368170373,31.5964543602758,123.846684019974)) ;
#22659 = CARTESIAN_POINT('Ctrl Pts',(-18.0029767278721,31.416465279913,123.955390640417)) ;
#22660 = CARTESIAN_POINT('Ctrl Pts',(-18.2259601248409,31.6064704164553,123.644318949324)) ;
#22661 = CARTESIAN_POINT('Ctrl Pts',(-17.930131161295,31.4264813360924,123.702427282653)) ;
#22662 = CARTESIAN_POINT('Ctrl Pts',(-18.1960923933868,31.6196484523213,123.368912551157)) ;
#22663 = CARTESIAN_POINT('Ctrl Pts',(-17.8927981854828,31.4396593719584,123.358188928687)) ;
#22664 = CARTESIAN_POINT('Ctrl Pts',(-18.2490034102453,31.6362503295084,123.019854463279)) ;
#22665 = CARTESIAN_POINT('Ctrl Pts',(-17.9589427761027,31.4562612491455,122.921846253614)) ;
#22666 = CARTESIAN_POINT('Ctrl Pts',(-18.4541225555357,31.6563134741243,122.64582032832)) ;
#22667 = CARTESIAN_POINT('Ctrl Pts',(-18.2153452936868,31.4763243937614,122.454312103361)) ;
#22668 = CARTESIAN_POINT('Ctrl Pts',(-18.7702542503997,31.676114364208,122.367683074125)) ;
#22669 = CARTESIAN_POINT('Ctrl Pts',(-18.6105119795525,31.4961252838451,122.106643007625)) ;
#22670 = CARTESIAN_POINT('Ctrl Pts',(-19.1646379113021,31.6960574894867,122.212071616699)) ;
#22671 = CARTESIAN_POINT('Ctrl Pts',(-19.1034924936999,31.5160684091238,121.912133008607)) ;
#22672 = CARTESIAN_POINT('Ctrl Pts',(-19.5875617432602,31.7159555346063,122.200691268626)) ;
#22673 = CARTESIAN_POINT('Ctrl Pts',(-19.6321465341764,31.5359664542434,121.89791137193)) ;
#22674 = CARTESIAN_POINT('Ctrl Pts',(-19.9891315337937,31.735841294233,122.333252820407)) ;
#22675 = CARTESIAN_POINT('Ctrl Pts',(-20.1341066883384,31.5558522138702,122.063616102464)) ;
#22676 = CARTESIAN_POINT('Ctrl Pts',(-20.3238700828937,31.7559064694129,122.597717645849)) ;
#22677 = CARTESIAN_POINT('Ctrl Pts',(-20.5525283110554,31.57591738905,122.394200252169)) ;
#22678 = CARTESIAN_POINT('Ctrl Pts',(-20.5455304831707,31.7757331125157,122.956392108189)) ;
#22679 = CARTESIAN_POINT('Ctrl Pts',(-20.8296000415882,31.5957440321528,122.84254361497)) ;
#22680 = CARTESIAN_POINT('Ctrl Pts',(-20.6329476537698,31.7956418219641,123.370466525032)) ;
#22681 = CARTESIAN_POINT('Ctrl Pts',(-20.9388687495492,31.6156527416012,123.360136077141)) ;
#22682 = CARTESIAN_POINT('Ctrl Pts',(-20.5737577153688,31.8155936589959,123.790666742913)) ;
#22683 = CARTESIAN_POINT('Ctrl Pts',(-20.8648791195812,31.635604578633,123.885385533411)) ;
#22684 = CARTESIAN_POINT('Ctrl Pts',(-20.3736372597136,31.835602133699,124.166043131573)) ;
#22685 = CARTESIAN_POINT('Ctrl Pts',(-20.6147262487971,31.6556130533361,124.354604940983)) ;
#22686 = CARTESIAN_POINT('Ctrl Pts',(-20.0609970576513,31.8554035924605,124.448061776785)) ;
#22687 = CARTESIAN_POINT('Ctrl Pts',(-20.2239265792252,31.6754145120976,124.70712499995)) ;
#22688 = CARTESIAN_POINT('Ctrl Pts',(-19.6682512234286,31.8753604806964,124.608723454266)) ;
#22689 = CARTESIAN_POINT('Ctrl Pts',(-19.7329944592127,31.6953714003336,124.907950846951)) ;
#22690 = CARTESIAN_POINT('Ctrl Pts',(-19.2436603324159,31.8953443181105,124.624778169694)) ;
#22691 = CARTESIAN_POINT('Ctrl Pts',(-19.2022559885623,31.7153552377477,124.928017723692)) ;
#22692 = CARTESIAN_POINT('Ctrl Pts',(-18.8422996219988,31.9151527573315,124.496909348728)) ;
#22693 = CARTESIAN_POINT('Ctrl Pts',(-18.7005580952729,31.7351636769686,124.768181953029)) ;
#22694 = CARTESIAN_POINT('Ctrl Pts',(-18.5055590914568,31.9351384667117,124.237910045326)) ;
#22695 = CARTESIAN_POINT('Ctrl Pts',(-18.2796327533169,31.7551493863488,124.444432947283)) ;
#22696 = CARTESIAN_POINT('Ctrl Pts',(-18.2784623208037,31.955007989727,123.881451590909)) ;
#22697 = CARTESIAN_POINT('Ctrl Pts',(-17.9957625956122,31.7750189093641,123.998861683797)) ;
#22698 = CARTESIAN_POINT('Ctrl Pts',(-18.1861815675504,31.9750287288442,123.466043557042)) ;
#22699 = CARTESIAN_POINT('Ctrl Pts',(-17.8804111930879,31.7950396484813,123.479601508631)) ;
#22700 = CARTESIAN_POINT('Ctrl Pts',(-18.2401047055373,31.9948327938211,123.04826047757)) ;
#22701 = CARTESIAN_POINT('Ctrl Pts',(-17.947813732566,31.8148437134583,122.957375358431)) ;
#22702 = CARTESIAN_POINT('Ctrl Pts',(-18.4356159524676,32.0148947575519,122.669266623573)) ;
#22703 = CARTESIAN_POINT('Ctrl Pts',(-18.1922019497661,31.834905677189,122.483631625261)) ;
#22704 = CARTESIAN_POINT('Ctrl Pts',(-18.7455928392011,32.0347279378404,122.383198650126)) ;
#22705 = CARTESIAN_POINT('Ctrl Pts',(-18.579670503548,31.8547388574775,122.126047237428)) ;
#22706 = CARTESIAN_POINT('Ctrl Pts',(-19.1356511664417,32.0546471351664,122.218343920433)) ;
#22707 = CARTESIAN_POINT('Ctrl Pts',(-19.0672415407129,31.8746580548036,121.919977102834)) ;
#22708 = CARTESIAN_POINT('Ctrl Pts',(-19.5590376558123,32.0745851602798,122.196738769831)) ;
#22709 = CARTESIAN_POINT('Ctrl Pts',(-19.596473798273,31.8945960799169,121.892968380712)) ;
#22710 = CARTESIAN_POINT('Ctrl Pts',(-19.9633771695477,32.0944632063358,122.319975235754)) ;
#22711 = CARTESIAN_POINT('Ctrl Pts',(-20.1018977424829,31.914474125973,122.047010861552)) ;
#22712 = CARTESIAN_POINT('Ctrl Pts',(-20.3031500801308,32.1144479406239,122.575069386705)) ;
#22713 = CARTESIAN_POINT('Ctrl Pts',(-20.5266155989396,31.934458860261,122.365876034326)) ;
#22714 = CARTESIAN_POINT('Ctrl Pts',(-20.5347790537855,32.1343587573024,122.929588130013)) ;
#22715 = CARTESIAN_POINT('Ctrl Pts',(-20.8161540516341,31.9543696769395,122.809022005469)) ;
#22716 = CARTESIAN_POINT('Ctrl Pts',(-20.6316344190319,32.1543577328211,123.343539091195)) ;
#22717 = CARTESIAN_POINT('Ctrl Pts',(-20.9372264313366,31.9743686524582,123.326459903439)) ;
#22718 = CARTESIAN_POINT('Ctrl Pts',(-20.5824108030896,32.1741626534663,123.761844882659)) ;
#22719 = CARTESIAN_POINT('Ctrl Pts',(-20.8757007542274,31.9941735731034,123.849340834267)) ;
#22720 = CARTESIAN_POINT('Ctrl Pts',(-20.3923321685515,32.1941466137575,124.141760103579)) ;
#22721 = CARTESIAN_POINT('Ctrl Pts',(-20.6381061492539,32.0141575333947,124.324236585198)) ;
#22722 = CARTESIAN_POINT('Ctrl Pts',(-20.0852664590449,32.2140328174815,124.432569654713)) ;
#22723 = CARTESIAN_POINT('Ctrl Pts',(-20.254277484515,32.0340437371186,124.687750970673)) ;
#22724 = CARTESIAN_POINT('Ctrl Pts',(-19.6964684402798,32.2339819958047,124.602063783456)) ;
#22725 = CARTESIAN_POINT('Ctrl Pts',(-19.7682819396191,32.0539929154418,124.89962239012)) ;
#22726 = CARTESIAN_POINT('Ctrl Pts',(-19.2741435561821,32.2538837950442,124.628548088097)) ;
#22727 = CARTESIAN_POINT('Ctrl Pts',(-19.2403770539516,32.0738947146813,124.932732853793)) ;
#22728 = CARTESIAN_POINT('Ctrl Pts',(-18.8683229480946,32.2737624000966,124.51031319366)) ;
#22729 = CARTESIAN_POINT('Ctrl Pts',(-18.7330993587673,32.0937733197337,124.784941725984)) ;
#22730 = CARTESIAN_POINT('Ctrl Pts',(-18.5246822894204,32.2937947598223,124.258593479938)) ;
#22731 = CARTESIAN_POINT('Ctrl Pts',(-18.3035498467669,32.1138056794594,124.470304693559)) ;
#22732 = CARTESIAN_POINT('Ctrl Pts',(-18.3288903417923,32.3103764857783,123.965395680415)) ;
#22733 = CARTESIAN_POINT('Ctrl Pts',(-18.0587930611329,32.1303874054155,124.103782576889)) ;
#22734 = CARTESIAN_POINT('Ctrl Pts',(-18.2389994739994,32.3235706560763,123.702969811419)) ;
#22735 = CARTESIAN_POINT('Ctrl Pts',(-17.9464384610694,32.1435815757134,123.775785395635)) ;
#22736 = CARTESIAN_POINT('Ctrl Pts',(-18.1952099825185,32.3368828341695,123.426608876342)) ;
#22737 = CARTESIAN_POINT('Ctrl Pts',(-17.8916962164165,32.1568937538066,123.430264324837)) ;
#22738 = CARTESIAN_POINT('Ctrl Pts',(-18.2318513898389,32.3534490137628,123.076189005305)) ;
#22739 = CARTESIAN_POINT('Ctrl Pts',(-17.9374894753685,32.1734599333999,122.99232521224)) ;
#22740 = CARTESIAN_POINT('Ctrl Pts',(-18.3860665926035,32.370077208623,122.758138167499)) ;
#22741 = CARTESIAN_POINT('Ctrl Pts',(-18.1302718088824,32.1900881282601,122.594703559392)) ;
#22742 = CARTESIAN_POINT('Ctrl Pts',(-18.5689151454784,32.3833657903327,122.546824011485)) ;
#22743 = CARTESIAN_POINT('Ctrl Pts',(-18.3588141057148,32.2033767099699,122.330591540781)) ;
#22744 = CARTESIAN_POINT('Ctrl Pts',(-18.7313456924468,32.3933340384363,122.414447869079)) ;
#22745 = CARTESIAN_POINT('Ctrl Pts',(-18.5618539277949,32.2133449580735,122.165112713871)) ;
#22746 = CARTESIAN_POINT('Ctrl Pts',(-18.9132084253142,32.4032487946925,122.312590576436)) ;
#22747 = CARTESIAN_POINT('Ctrl Pts',(-18.7891790717996,32.2232597143296,122.037790376024)) ;
#22748 = CARTESIAN_POINT('Ctrl Pts',(-19.1118736333332,32.4132619453437,122.242954847394)) ;
#22749 = CARTESIAN_POINT('Ctrl Pts',(-19.037513591275,32.2332728649808,121.95074327932)) ;
#22750 = CARTESIAN_POINT('Ctrl Pts',(-19.3196522724763,32.4232746525457,122.209207410282)) ;
#22751 = CARTESIAN_POINT('Ctrl Pts',(-19.2972230251791,32.2432855721828,121.908553873528)) ;
#22752 = CARTESIAN_POINT('Ctrl Pts',(-19.5975327146755,32.436493941237,122.212420867369)) ;
#22753 = CARTESIAN_POINT('Ctrl Pts',(-19.6446403660395,32.2565048608741,121.9125795524)) ;
#22754 = CARTESIAN_POINT('Ctrl Pts',(-19.9378232247677,32.453112622235,122.307507172536)) ;
#22755 = CARTESIAN_POINT('Ctrl Pts',(-20.0699198327109,32.2731235418722,122.031411460383)) ;
#22756 = CARTESIAN_POINT('Ctrl Pts',(-20.2246076543759,32.4696775300085,122.512015826499)) ;
#22757 = CARTESIAN_POINT('Ctrl Pts',(-20.4284615240151,32.2896884496456,122.28707638829)) ;
#22758 = CARTESIAN_POINT('Ctrl Pts',(-20.4036500534061,32.4830760016193,122.729503286316)) ;
#22759 = CARTESIAN_POINT('Ctrl Pts',(-20.6522321703216,32.3030869212564,122.55890721292)) ;
#22760 = CARTESIAN_POINT('Ctrl Pts',(-20.5055910328036,32.4929172571063,122.909552354167)) ;
#22761 = CARTESIAN_POINT('Ctrl Pts',(-20.7796679108865,32.3129281767434,122.783972393412)) ;
#22762 = CARTESIAN_POINT('Ctrl Pts',(-20.5761633681093,32.5029035726945,123.10724493237)) ;
#22763 = CARTESIAN_POINT('Ctrl Pts',(-20.8678841148157,32.3229144923316,123.031085830974)) ;
#22764 = CARTESIAN_POINT('Ctrl Pts',(-20.6112720105989,32.5128401802809,123.313207381497)) ;
#22765 = CARTESIAN_POINT('Ctrl Pts',(-20.9117732133019,32.332851099918,123.288538866815)) ;
#22766 = CARTESIAN_POINT('Ctrl Pts',(-20.6099679457665,32.5228900476492,123.524461765722)) ;
#22767 = CARTESIAN_POINT('Ctrl Pts',(-20.910145815352,32.3429009672863,123.552606824038)) ;
#22768 = CARTESIAN_POINT('Ctrl Pts',(-20.5729021146074,32.532740542324,123.728221890654)) ;
#22769 = CARTESIAN_POINT('Ctrl Pts',(-20.8638163142715,32.3527514619611,123.807307622436)) ;
#22770 = CARTESIAN_POINT('Ctrl Pts',(-20.5006629810764,32.5427123427185,123.924992058864)) ;
#22771 = CARTESIAN_POINT('Ctrl Pts',(-20.773519983493,32.3627232623556,124.053271401024)) ;
#22772 = CARTESIAN_POINT('Ctrl Pts',(-20.3950484487511,32.5527083097443,124.106711975887)) ;
#22773 = CARTESIAN_POINT('Ctrl Pts',(-20.6415042015941,32.3727192293814,124.280422776241)) ;
#22774 = CARTESIAN_POINT('Ctrl Pts',(-20.2587392018978,32.5627457691255,124.267771847846)) ;
#22775 = CARTESIAN_POINT('Ctrl Pts',(-20.4711197706811,32.3827566887626,124.481749462152)) ;
#22776 = CARTESIAN_POINT('Ctrl Pts',(-20.0999386935785,32.5725864700262,124.400395451585)) ;
#22777 = CARTESIAN_POINT('Ctrl Pts',(-20.2726207381904,32.3925973896634,124.6475312724)) ;
#22778 = CARTESIAN_POINT('Ctrl Pts',(-19.9169195431235,32.5826344912936,124.505860717618)) ;
#22779 = CARTESIAN_POINT('Ctrl Pts',(-20.0438481628859,32.4026454109307,124.779365277945)) ;
#22780 = CARTESIAN_POINT('Ctrl Pts',(-19.7202317170747,32.5925818843763,124.576913026863)) ;
#22781 = CARTESIAN_POINT('Ctrl Pts',(-19.7979892008617,32.4125928040134,124.868183348147)) ;
#22782 = CARTESIAN_POINT('Ctrl Pts',(-19.5150675447947,32.6024920304227,124.613229581171)) ;
#22783 = CARTESIAN_POINT('Ctrl Pts',(-19.5415342218403,32.4225029500598,124.913581797367)) ;
#22784 = CARTESIAN_POINT('Ctrl Pts',(-19.3036192781191,32.6125509442723,124.613134139564)) ;
#22785 = CARTESIAN_POINT('Ctrl Pts',(-19.277223918375,32.4325618639094,124.913465271175)) ;
#22786 = CARTESIAN_POINT('Ctrl Pts',(-19.0998162930448,32.6223917145616,124.5774017769)) ;
#22787 = CARTESIAN_POINT('Ctrl Pts',(-19.022469311543,32.4424026341987,124.868802452506)) ;
#22788 = CARTESIAN_POINT('Ctrl Pts',(-18.9008906926549,32.6324545841402,124.505484176666)) ;
#22789 = CARTESIAN_POINT('Ctrl Pts',(-18.7738114256327,32.4524655037773,124.778908029314)) ;
#22790 = CARTESIAN_POINT('Ctrl Pts',(-18.7205888208704,32.6423489072707,124.401712674565)) ;
#22791 = CARTESIAN_POINT('Ctrl Pts',(-18.5484324346786,32.4623598269078,124.649195864268)) ;
#22792 = CARTESIAN_POINT('Ctrl Pts',(-18.5599523550071,32.6522907143652,124.268035857057)) ;
#22793 = CARTESIAN_POINT('Ctrl Pts',(-18.3476349380033,32.4723016340023,124.482101731582)) ;
#22794 = CARTESIAN_POINT('Ctrl Pts',(-18.4240467284614,32.6622932253205,124.107533030312)) ;
#22795 = CARTESIAN_POINT('Ctrl Pts',(-18.1777508202333,32.4823041449576,124.281474853431)) ;
#22796 = CARTESIAN_POINT('Ctrl Pts',(-18.3180393506076,32.6723279461389,123.925154810979)) ;
#22797 = CARTESIAN_POINT('Ctrl Pts',(-18.0452392633268,32.492338865776,124.053503454134)) ;
#22798 = CARTESIAN_POINT('Ctrl Pts',(-18.2463535071879,32.6821731236446,123.730976061633)) ;
#22799 = CARTESIAN_POINT('Ctrl Pts',(-17.9556292696089,32.5021840432817,123.810780412352)) ;
#22800 = CARTESIAN_POINT('Ctrl Pts',(-18.2085503842841,32.6921578840457,123.524527153024)) ;
#22801 = CARTESIAN_POINT('Ctrl Pts',(-17.9083727783839,32.5121688036828,123.552719582534)) ;
#22802 = CARTESIAN_POINT('Ctrl Pts',(-18.2070734509099,32.7020967903621,123.315553842166)) ;
#22803 = CARTESIAN_POINT('Ctrl Pts',(-17.9065240318847,32.5221077099992,123.291502653985)) ;
#22804 = CARTESIAN_POINT('Ctrl Pts',(-18.2423288903742,32.7121390179978,123.107420822376)) ;
#22805 = CARTESIAN_POINT('Ctrl Pts',(-17.9505907657664,32.5321499376349,123.031335993592)) ;
#22806 = CARTESIAN_POINT('Ctrl Pts',(-18.3119535046348,32.7220242295822,122.91158798625)) ;
#22807 = CARTESIAN_POINT('Ctrl Pts',(-18.0376192936705,32.5420351492193,122.786543593569)) ;
#22808 = CARTESIAN_POINT('Ctrl Pts',(-18.4154411859655,32.7320231597841,122.728653020651)) ;
#22809 = CARTESIAN_POINT('Ctrl Pts',(-18.1669767556182,32.5520340794212,122.557873550048)) ;
#22810 = CARTESIAN_POINT('Ctrl Pts',(-18.5479494903237,32.7419405826945,122.567636304584)) ;
#22811 = CARTESIAN_POINT('Ctrl Pts',(-18.3326104946629,32.5619515023317,122.356600741746)) ;
#22812 = CARTESIAN_POINT('Ctrl Pts',(-18.7084645463627,32.7519885147733,122.430363552934)) ;
#22813 = CARTESIAN_POINT('Ctrl Pts',(-18.5332526173871,32.5719994344104,122.185007966984)) ;
#22814 = CARTESIAN_POINT('Ctrl Pts',(-18.8872415852668,32.7618658905827,122.324659315536)) ;
#22815 = CARTESIAN_POINT('Ctrl Pts',(-18.7567232187338,32.5818768102198,122.052875232647)) ;
#22816 = CARTESIAN_POINT('Ctrl Pts',(-19.0850258483024,32.7719197837506,122.25022120339)) ;
#22817 = CARTESIAN_POINT('Ctrl Pts',(-19.0039525695959,32.5919307033877,121.95982536141)) ;
#22818 = CARTESIAN_POINT('Ctrl Pts',(-19.2894783129814,32.7818134070039,122.211767437767)) ;
#22819 = CARTESIAN_POINT('Ctrl Pts',(-19.2595182815849,32.601824326641,121.911755678648)) ;
#22820 = CARTESIAN_POINT('Ctrl Pts',(-19.5009779859704,32.7918760006269,122.209324968633)) ;
#22821 = CARTESIAN_POINT('Ctrl Pts',(-19.5238926627054,32.611886920264,121.908700188409)) ;
#22822 = CARTESIAN_POINT('Ctrl Pts',(-19.7051996408792,32.8017185746159,122.242795102334)) ;
#22823 = CARTESIAN_POINT('Ctrl Pts',(-19.7791709674073,32.6217294942531,121.950535647314)) ;
#22824 = CARTESIAN_POINT('Ctrl Pts',(-19.9035645751163,32.8117093314989,122.311756543246)) ;
#22825 = CARTESIAN_POINT('Ctrl Pts',(-20.0271280441419,32.631720251136,122.036735366636)) ;
#22826 = CARTESIAN_POINT('Ctrl Pts',(-20.0858058022882,32.8216373932568,122.41352070292)) ;
#22827 = CARTESIAN_POINT('Ctrl Pts',(-20.2549311093635,32.6416483128939,122.163938821337)) ;
#22828 = CARTESIAN_POINT('Ctrl Pts',(-20.2488151784822,32.831625369146,122.545893277075)) ;
#22829 = CARTESIAN_POINT('Ctrl Pts',(-20.4586943445291,32.6516362887831,122.329402962598)) ;
#22830 = CARTESIAN_POINT('Ctrl Pts',(-20.3867446811956,32.8416610335024,122.705536508051)) ;
#22831 = CARTESIAN_POINT('Ctrl Pts',(-20.6311078851739,32.6616719531395,122.528955452347)) ;
#22832 = CARTESIAN_POINT('Ctrl Pts',(-20.4932113035389,32.8515169719221,122.883306696087)) ;
#22833 = CARTESIAN_POINT('Ctrl Pts',(-20.76419350534,32.6715278915592,122.751167847475)) ;
#22834 = CARTESIAN_POINT('Ctrl Pts',(-20.5685516723176,32.861512463319,123.079449372689)) ;
#22835 = CARTESIAN_POINT('Ctrl Pts',(-20.8583709770248,32.6815233829561,122.99634558384)) ;
#22836 = CARTESIAN_POINT('Ctrl Pts',(-20.6084146945894,32.8714222682724,123.283945522481)) ;
#22837 = CARTESIAN_POINT('Ctrl Pts',(-20.9082019158921,32.6914331879096,123.251966021349)) ;
#22838 = CARTESIAN_POINT('Ctrl Pts',(-20.6125455527865,32.8814344905392,123.494398317047)) ;
#22839 = CARTESIAN_POINT('Ctrl Pts',(-20.913367466307,32.7014454101763,123.515032024856)) ;
#22840 = CARTESIAN_POINT('Ctrl Pts',(-20.5796147863066,32.891462371232,123.702629937833)) ;
#22841 = CARTESIAN_POINT('Ctrl Pts',(-20.8722060909322,32.7114732908691,123.775321815842)) ;
#22842 = CARTESIAN_POINT('Ctrl Pts',(-20.512536676068,32.9013187672146,123.898683038546)) ;
#22843 = CARTESIAN_POINT('Ctrl Pts',(-20.7883600167789,32.7213296868517,124.02038977865)) ;
#22844 = CARTESIAN_POINT('Ctrl Pts',(-20.4111096637263,32.9113435643946,124.083427639594)) ;
#22845 = CARTESIAN_POINT('Ctrl Pts',(-20.6615779007813,32.7313544840317,124.25132140461)) ;
#22846 = CARTESIAN_POINT('Ctrl Pts',(-20.2786586384408,32.9213744943784,124.247533456191)) ;
#22847 = CARTESIAN_POINT('Ctrl Pts',(-20.4960157375153,32.7413854140155,124.456454889738)) ;
#22848 = CARTESIAN_POINT('Ctrl Pts',(-20.1229354505894,32.931219096887,124.38384374608)) ;
#22849 = CARTESIAN_POINT('Ctrl Pts',(-20.3013621684409,32.7512300165242,124.626844922445)) ;
#22850 = CARTESIAN_POINT('Ctrl Pts',(-19.9435638207466,32.9412099481111,124.493133513568)) ;
#22851 = CARTESIAN_POINT('Ctrl Pts',(-20.0771483650704,32.7612208677483,124.763458712167)) ;
#22852 = CARTESIAN_POINT('Ctrl Pts',(-19.7468547735515,32.9512477811224,124.569535084003)) ;
#22853 = CARTESIAN_POINT('Ctrl Pts',(-19.8312628601083,32.7712587007595,124.858962378708)) ;
#22854 = CARTESIAN_POINT('Ctrl Pts',(-19.5439187927745,32.9610921695878,124.610185963789)) ;
#22855 = CARTESIAN_POINT('Ctrl Pts',(-19.5775920832475,32.7811030892249,124.909777937782)) ;
#22856 = CARTESIAN_POINT('Ctrl Pts',(-19.3341011134292,32.9710769739574,124.615465585142)) ;
#22857 = CARTESIAN_POINT('Ctrl Pts',(-19.3153197757331,32.7910878935945,124.916379101424)) ;
#22858 = CARTESIAN_POINT('Ctrl Pts',(-19.1274257911367,32.9810164934402,124.584456615172)) ;
#22859 = CARTESIAN_POINT('Ctrl Pts',(-19.0569748481772,32.8010274130773,124.877619388893)) ;
#22860 = CARTESIAN_POINT('Ctrl Pts',(-18.927334989013,32.9910562244416,124.517330597724)) ;
#22861 = CARTESIAN_POINT('Ctrl Pts',(-18.8068609697535,32.8110671440787,124.793713447214)) ;
#22862 = CARTESIAN_POINT('Ctrl Pts',(-18.7446634407344,33.0009443526879,124.418083254216)) ;
#22863 = CARTESIAN_POINT('Ctrl Pts',(-18.5785199696836,32.820955272325,124.669655218426)) ;
#22864 = CARTESIAN_POINT('Ctrl Pts',(-18.5801005857967,33.0109340778964,124.28761411625)) ;
#22865 = CARTESIAN_POINT('Ctrl Pts',(-18.3728153330768,32.8309449975335,124.506569798915)) ;
#22866 = CARTESIAN_POINT('Ctrl Pts',(-18.4412469443852,33.0208918425979,124.130951753119)) ;
#22867 = CARTESIAN_POINT('Ctrl Pts',(-18.1992468678326,32.840902762235,124.310742518053)) ;
#22868 = CARTESIAN_POINT('Ctrl Pts',(-18.3318926647563,33.0307941840099,123.9538000731)) ;
#22869 = CARTESIAN_POINT('Ctrl Pts',(-18.0625524288157,32.850805103647,124.089302873787)) ;
#22870 = CARTESIAN_POINT('Ctrl Pts',(-18.2538818671851,33.0408383797163,123.757588934328)) ;
#22871 = CARTESIAN_POINT('Ctrl Pts',(-17.9650377613778,32.8608492993534,123.844039624706)) ;
#22872 = CARTESIAN_POINT('Ctrl Pts',(-18.2116804220347,33.0507457804755,123.553613209322)) ;
#22873 = CARTESIAN_POINT('Ctrl Pts',(-17.9122844842802,32.8707567001127,123.58906943826)) ;
#22874 = CARTESIAN_POINT('Ctrl Pts',(-18.2051029806548,33.0607563803499,123.343258587515)) ;
#22875 = CARTESIAN_POINT('Ctrl Pts',(-17.9040614841339,32.880767299987,123.326126151249)) ;
#22876 = CARTESIAN_POINT('Ctrl Pts',(-18.2356129749223,33.0707866762621,123.134602723717)) ;
#22877 = CARTESIAN_POINT('Ctrl Pts',(-17.9421976273555,32.8907975958992,123.065306227518)) ;
#22878 = CARTESIAN_POINT('Ctrl Pts',(-18.300450441629,33.0806414559118,122.937844780199)) ;
#22879 = CARTESIAN_POINT('Ctrl Pts',(-18.0232436735507,32.9006523755489,122.819357208247)) ;
#22880 = CARTESIAN_POINT('Ctrl Pts',(-18.3989330999902,33.0905987841293,122.753115564655)) ;
#22881 = CARTESIAN_POINT('Ctrl Pts',(-18.1463463293519,32.9106097037664,122.588444800357)) ;
#22882 = CARTESIAN_POINT('Ctrl Pts',(-18.5293347628917,33.1006378170362,122.587186806717)) ;
#22883 = CARTESIAN_POINT('Ctrl Pts',(-18.3093474042476,32.9206487366733,122.381033273986)) ;
#22884 = CARTESIAN_POINT('Ctrl Pts',(-18.6837449458525,33.1105109289255,122.44842798728)) ;
#22885 = CARTESIAN_POINT('Ctrl Pts',(-18.5023603004912,32.9305218485626,122.207583253798)) ;
#22886 = CARTESIAN_POINT('Ctrl Pts',(-18.8634428506156,33.1205842139526,122.336455552253)) ;
#22887 = CARTESIAN_POINT('Ctrl Pts',(-18.7269817759468,32.9405951335897,122.067617063673)) ;
#22888 = CARTESIAN_POINT('Ctrl Pts',(-19.0549009830223,33.1304045336893,122.259087158195)) ;
#22889 = CARTESIAN_POINT('Ctrl Pts',(-18.9663055363985,32.9504154533265,121.970905134139)) ;
#22890 = CARTESIAN_POINT('Ctrl Pts',(-19.2620617743464,33.1404831990678,122.214836805238)) ;
#22891 = CARTESIAN_POINT('Ctrl Pts',(-19.2252558871534,32.9604941187049,121.915591458617)) ;
#22892 = CARTESIAN_POINT('Ctrl Pts',(-19.4690858066591,33.1503347895516,122.207323763932)) ;
#22893 = CARTESIAN_POINT('Ctrl Pts',(-19.4840372151867,32.9703457091887,121.906199287805)) ;
#22894 = CARTESIAN_POINT('Ctrl Pts',(-19.6788221961635,33.1604079398705,122.236318117315)) ;
#22895 = CARTESIAN_POINT('Ctrl Pts',(-19.7462073716882,32.9804188595076,121.942441422299)) ;
#22896 = CARTESIAN_POINT('Ctrl Pts',(-19.8757676666468,33.1702503198455,122.29984587334)) ;
#22897 = CARTESIAN_POINT('Ctrl Pts',(-19.9923907933803,32.9902612394826,122.021850824201)) ;
#22898 = CARTESIAN_POINT('Ctrl Pts',(-20.0615568423931,33.1802312960886,122.397340048121)) ;
#22899 = CARTESIAN_POINT('Ctrl Pts',(-20.2246277641436,33.0002422157257,122.143718242006)) ;
#22900 = CARTESIAN_POINT('Ctrl Pts',(-20.2279876372291,33.1902476244439,122.526364012805)) ;
#22901 = CARTESIAN_POINT('Ctrl Pts',(-20.4326666594073,33.010258544081,122.304997705767)) ;
#22902 = CARTESIAN_POINT('Ctrl Pts',(-20.3679958704936,33.200145421435,122.680288715959)) ;
#22903 = CARTESIAN_POINT('Ctrl Pts',(-20.6076780088902,33.0201563410721,122.497403957948)) ;
#22904 = CARTESIAN_POINT('Ctrl Pts',(-20.4807568430483,33.2101579781671,122.858052147058)) ;
#22905 = CARTESIAN_POINT('Ctrl Pts',(-20.7486295700232,33.0301688978042,122.719608055138)) ;
#22906 = CARTESIAN_POINT('Ctrl Pts',(-20.5606237614743,33.2201900130135,123.053239269694)) ;
#22907 = CARTESIAN_POINT('Ctrl Pts',(-20.8484637130917,33.0402009326507,122.96359161389)) ;
#22908 = CARTESIAN_POINT('Ctrl Pts',(-20.6050359521563,33.230029413829,123.255287016282)) ;
#22909 = CARTESIAN_POINT('Ctrl Pts',(-20.9039796443904,33.0500403334661,123.216152649294)) ;
#22910 = CARTESIAN_POINT('Ctrl Pts',(-20.614049092095,33.2400951994806,123.466685199039)) ;
#22911 = CARTESIAN_POINT('Ctrl Pts',(-20.9152463774755,33.0601061191177,123.480399984258)) ;
#22912 = CARTESIAN_POINT('Ctrl Pts',(-20.5866016199623,33.2499856545952,123.672815882505)) ;
#22913 = CARTESIAN_POINT('Ctrl Pts',(-20.8809372575507,33.0699965742323,123.738064421165)) ;
#22914 = CARTESIAN_POINT('Ctrl Pts',(-20.5235744358789,33.2599777732309,123.873192435292)) ;
#22915 = CARTESIAN_POINT('Ctrl Pts',(-20.8021533889854,33.0799886928681,123.98853537261)) ;
#22916 = CARTESIAN_POINT('Ctrl Pts',(-20.4268201921986,33.269940599994,124.058949341531)) ;
#22917 = CARTESIAN_POINT('Ctrl Pts',(-20.6812106073249,33.0899515196311,124.220732031348)) ;
#22918 = CARTESIAN_POINT('Ctrl Pts',(-20.3004366840512,33.2798448832669,124.224447351388)) ;
#22919 = CARTESIAN_POINT('Ctrl Pts',(-20.5232306933288,33.099855802904,124.427605321835)) ;
#22920 = CARTESIAN_POINT('Ctrl Pts',(-20.1447295418141,33.289905317214,124.36754765931)) ;
#22921 = CARTESIAN_POINT('Ctrl Pts',(-20.3285971107455,33.1099162368511,124.606480559927)) ;
#22922 = CARTESIAN_POINT('Ctrl Pts',(-19.9705348461401,33.2997458698872,124.479200573106)) ;
#22923 = CARTESIAN_POINT('Ctrl Pts',(-20.1108525131507,33.1197567895243,124.746047511506)) ;
#22924 = CARTESIAN_POINT('Ctrl Pts',(-19.7754486620415,33.3098080898329,124.560937015525)) ;
#22925 = CARTESIAN_POINT('Ctrl Pts',(-19.8669950901314,33.12981900947,124.84821784105)) ;
#22926 = CARTESIAN_POINT('Ctrl Pts',(-19.57243885132,33.3197052291114,124.606588971433)) ;
#22927 = CARTESIAN_POINT('Ctrl Pts',(-19.6132318493154,33.1397161487486,124.905283007203)) ;
#22928 = CARTESIAN_POINT('Ctrl Pts',(-19.3639189425878,33.3296364212465,124.61702574814)) ;
#22929 = CARTESIAN_POINT('Ctrl Pts',(-19.3525812289575,33.1496473408836,124.918328736674)) ;
#22930 = CARTESIAN_POINT('Ctrl Pts',(-19.1544701914488,33.3396785758916,124.5905747195)) ;
#22931 = CARTESIAN_POINT('Ctrl Pts',(-19.090770522027,33.1596894955287,124.885264797401)) ;
#22932 = CARTESIAN_POINT('Ctrl Pts',(-18.9558448503062,33.3495653369109,124.529280922673)) ;
#22933 = CARTESIAN_POINT('Ctrl Pts',(-18.842487870914,33.169576256548,124.808646986439)) ;
#22934 = CARTESIAN_POINT('Ctrl Pts',(-18.7686911463768,33.3595646386281,124.433610207421)) ;
#22935 = CARTESIAN_POINT('Ctrl Pts',(-18.6085457635101,33.1795755582652,124.689058201042)) ;
#22936 = CARTESIAN_POINT('Ctrl Pts',(-18.6021783660485,33.3694854367949,124.307970432937)) ;
#22937 = CARTESIAN_POINT('Ctrl Pts',(-18.4004044124469,33.189496356432,124.532007686267)) ;
#22938 = CARTESIAN_POINT('Ctrl Pts',(-18.4584063019832,33.3795194903916,124.153637802788)) ;
#22939 = CARTESIAN_POINT('Ctrl Pts',(-18.2206897370185,33.1995304100287,124.339091714962)) ;
#22940 = CARTESIAN_POINT('Ctrl Pts',(-18.3447487639094,33.389442607958,123.978664957015)) ;
#22941 = CARTESIAN_POINT('Ctrl Pts',(-18.0786177880743,33.2094535275951,124.120374761366)) ;
#22942 = CARTESIAN_POINT('Ctrl Pts',(-18.262168874499,33.3994987314571,123.784072019688)) ;
#22943 = CARTESIAN_POINT('Ctrl Pts',(-17.9753934550452,33.2195096510942,123.87713368977)) ;
#22944 = CARTESIAN_POINT('Ctrl Pts',(-18.2155327305873,33.4093441731119,123.582403847225)) ;
#22945 = CARTESIAN_POINT('Ctrl Pts',(-17.9170984303965,33.2293550927491,123.625046988953)) ;
#22946 = CARTESIAN_POINT('Ctrl Pts',(-18.203805100798,33.4193064742361,123.373306871914)) ;
#22947 = CARTESIAN_POINT('Ctrl Pts',(-17.9024396209619,33.2393173938732,123.363675275733)) ;
#22948 = CARTESIAN_POINT('Ctrl Pts',(-18.2290055597389,33.4293349535112,123.163973793253)) ;
#22949 = CARTESIAN_POINT('Ctrl Pts',(-17.9339408232565,33.2493458731483,123.102009100134)) ;
#22950 = CARTESIAN_POINT('Ctrl Pts',(-18.289374518782,33.4392453070209,122.96457571185)) ;
#22951 = CARTESIAN_POINT('Ctrl Pts',(-18.009402919707,33.259256226658,122.852760854094)) ;
#22952 = CARTESIAN_POINT('Ctrl Pts',(-18.3832010117499,33.4491801791981,122.777967476055)) ;
#22953 = CARTESIAN_POINT('Ctrl Pts',(-18.1266871223674,33.2691910988352,122.61950036567)) ;
#22954 = CARTESIAN_POINT('Ctrl Pts',(-18.5094881208649,33.4592213167838,122.60882144455)) ;
#22955 = CARTESIAN_POINT('Ctrl Pts',(-18.2845465433898,33.2792322364209,122.40806845954)) ;
#22956 = CARTESIAN_POINT('Ctrl Pts',(-18.6607816210844,33.4691084659983,122.466272054033)) ;
#22957 = CARTESIAN_POINT('Ctrl Pts',(-18.4736647676083,33.2891193856355,122.229881635933)) ;
#22958 = CARTESIAN_POINT('Ctrl Pts',(-18.8361603645087,33.4791007007494,122.350665197575)) ;
#22959 = CARTESIAN_POINT('Ctrl Pts',(-18.6928889148738,33.2991116203865,122.085373784708)) ;
#22960 = CARTESIAN_POINT('Ctrl Pts',(-19.0281558133508,33.4890494063124,122.267675696057)) ;
#22961 = CARTESIAN_POINT('Ctrl Pts',(-18.9328841091275,33.3090603259495,121.981637584403)) ;
#22962 = CARTESIAN_POINT('Ctrl Pts',(-19.2312903333038,33.4989854747361,122.219054749115)) ;
#22963 = CARTESIAN_POINT('Ctrl Pts',(-19.1868031331839,33.3189963943732,121.920862306553)) ;
#22964 = CARTESIAN_POINT('Ctrl Pts',(-19.4408438884127,33.5089711589519,122.206138288306)) ;
#22965 = CARTESIAN_POINT('Ctrl Pts',(-19.4487454010854,33.328982078589,121.90471788781)) ;
#22966 = CARTESIAN_POINT('Ctrl Pts',(-19.6505310611523,33.5190115855205,122.230262302281)) ;
#22967 = CARTESIAN_POINT('Ctrl Pts',(-19.7108540776556,33.3390225051576,121.934873930191)) ;
#22968 = CARTESIAN_POINT('Ctrl Pts',(-19.8489000133317,33.5288506989843,122.288894555747)) ;
#22969 = CARTESIAN_POINT('Ctrl Pts',(-19.9588162424853,33.3488616186214,122.008165761205)) ;
#22970 = CARTESIAN_POINT('Ctrl Pts',(-20.0378734404374,33.5388804331601,122.382439401842)) ;
#22971 = CARTESIAN_POINT('Ctrl Pts',(-20.1950323307625,33.3588913527972,122.125097981869)) ;
#22972 = CARTESIAN_POINT('Ctrl Pts',(-20.2072755150805,33.548902532666,122.50771918548)) ;
#22973 = CARTESIAN_POINT('Ctrl Pts',(-20.406784218548,33.3689134523031,122.281698617158)) ;
#22974 = CARTESIAN_POINT('Ctrl Pts',(-20.3505163323491,33.5587709725594,122.657820476515)) ;
#22975 = CARTESIAN_POINT('Ctrl Pts',(-20.5858350552601,33.3787818921965,122.469326974363)) ;
#22976 = CARTESIAN_POINT('Ctrl Pts',(-20.467830910548,33.568839837245,122.833994863383)) ;
#22977 = CARTESIAN_POINT('Ctrl Pts',(-20.732476955186,33.3888507568821,122.68954538537)) ;
#22978 = CARTESIAN_POINT('Ctrl Pts',(-20.5508822742983,33.5786825103436,123.023527927505)) ;
#22979 = CARTESIAN_POINT('Ctrl Pts',(-20.8362904559934,33.3986934299808,122.926463443138)) ;
#22980 = CARTESIAN_POINT('Ctrl Pts',(-20.6010906324588,33.5886431445061,123.226819066084)) ;
#22981 = CARTESIAN_POINT('Ctrl Pts',(-20.8990494415645,33.4086540641432,123.180578146984)) ;
#22982 = CARTESIAN_POINT('Ctrl Pts',(-20.6149332523502,33.5986810601842,123.437385843915)) ;
#22983 = CARTESIAN_POINT('Ctrl Pts',(-20.916351249052,33.4186919798213,123.443786581483)) ;
#22984 = CARTESIAN_POINT('Ctrl Pts',(-20.5927561143563,33.6085553350436,123.64381161214)) ;
#22985 = CARTESIAN_POINT('Ctrl Pts',(-20.8886281343362,33.4285662546808,123.701819630219)) ;
#22986 = CARTESIAN_POINT('Ctrl Pts',(-20.5339350999099,33.6186250854188,123.847144174352)) ;
#22987 = CARTESIAN_POINT('Ctrl Pts',(-20.8151004364326,33.4386360050559,123.95598455471)) ;
#22988 = CARTESIAN_POINT('Ctrl Pts',(-20.4429721196494,33.6284583807933,124.032801166583)) ;
#22989 = CARTESIAN_POINT('Ctrl Pts',(-20.7013946872375,33.4484693004304,124.188056231771)) ;
#22990 = CARTESIAN_POINT('Ctrl Pts',(-20.3192120120837,33.6384886782729,124.203524561785)) ;
#22991 = CARTESIAN_POINT('Ctrl Pts',(-20.5466931297227,33.45849959791,124.401459336272)) ;
#22992 = CARTESIAN_POINT('Ctrl Pts',(-20.1672189301495,33.6485207647143,124.34975537749)) ;
#22993 = CARTESIAN_POINT('Ctrl Pts',(-20.3567007162318,33.4685316843515,124.58424663072)) ;
#22994 = CARTESIAN_POINT('Ctrl Pts',(-19.9959765672418,33.6583486932033,124.465347265226)) ;
#22995 = CARTESIAN_POINT('Ctrl Pts',(-20.1426457143214,33.4783596128404,124.728735741513)) ;
#22996 = CARTESIAN_POINT('Ctrl Pts',(-19.8042599262361,33.668344734314,124.551406477392)) ;
#22997 = CARTESIAN_POINT('Ctrl Pts',(-19.9029989792466,33.4883556539512,124.836308043002)) ;
#22998 = CARTESIAN_POINT('Ctrl Pts',(-19.5997986838968,33.6783705464153,124.602630095532)) ;
#22999 = CARTESIAN_POINT('Ctrl Pts',(-19.6474220237301,33.4983814660524,124.900335793291)) ;
#23000 = CARTESIAN_POINT('Ctrl Pts',(-19.3924774849365,33.6882577813101,124.617636375072)) ;
#23001 = CARTESIAN_POINT('Ctrl Pts',(-19.3882695560054,33.5082687009472,124.919091810044)) ;
#23002 = CARTESIAN_POINT('Ctrl Pts',(-19.1838086719246,33.6982346475211,124.59657238943)) ;
#23003 = CARTESIAN_POINT('Ctrl Pts',(-19.1274334857693,33.5182455671582,124.892759807624)) ;
#23004 = CARTESIAN_POINT('Ctrl Pts',(-18.9815887866603,33.7082275913929,124.539527650244)) ;
#23005 = CARTESIAN_POINT('Ctrl Pts',(-18.8746590268341,33.52823851103,124.821451907867)) ;
#23006 = CARTESIAN_POINT('Ctrl Pts',(-18.7916507877663,33.7182655140643,124.447604623788)) ;
#23007 = CARTESIAN_POINT('Ctrl Pts',(-18.6372374521722,33.5382764337014,124.706546424498)) ;
#23008 = CARTESIAN_POINT('Ctrl Pts',(-18.6235800416685,33.728113978326,124.326664479328)) ;
#23009 = CARTESIAN_POINT('Ctrl Pts',(-18.4271493677989,33.5481248979631,124.555368999614)) ;
#23010 = CARTESIAN_POINT('Ctrl Pts',(-18.4767212967357,33.73810584507,124.17651438228)) ;
#23011 = CARTESIAN_POINT('Ctrl Pts',(-18.2435773439465,33.5581167647071,124.367679767415)) ;
#23012 = CARTESIAN_POINT('Ctrl Pts',(-18.3589139649517,33.7480235771112,124.004451145981)) ;
#23013 = CARTESIAN_POINT('Ctrl Pts',(-18.096319636919,33.5680344967483,124.152599028164)) ;
#23014 = CARTESIAN_POINT('Ctrl Pts',(-18.2717798858509,33.7580517620064,123.812495005014)) ;
#23015 = CARTESIAN_POINT('Ctrl Pts',(-17.9874040348388,33.5780626816436,123.912652984584)) ;
#23016 = CARTESIAN_POINT('Ctrl Pts',(-18.2199583948153,33.7679369200553,123.611237430731)) ;
#23017 = CARTESIAN_POINT('Ctrl Pts',(-17.9226291155959,33.5879478396924,123.661079753393)) ;
#23018 = CARTESIAN_POINT('Ctrl Pts',(-18.2031899992664,33.777926280597,123.401895935145)) ;
#23019 = CARTESIAN_POINT('Ctrl Pts',(-17.9016709287819,33.5979372002341,123.399402541443)) ;
#23020 = CARTESIAN_POINT('Ctrl Pts',(-18.2235716353926,33.7879674375313,123.191785549963)) ;
#23021 = CARTESIAN_POINT('Ctrl Pts',(-17.9271501704679,33.6079783571685,123.1367648659)) ;
#23022 = CARTESIAN_POINT('Ctrl Pts',(-18.2786200114163,33.7978000209865,122.992541931651)) ;
#23023 = CARTESIAN_POINT('Ctrl Pts',(-17.9959631146861,33.6178109406236,122.887710030823)) ;
#23024 = CARTESIAN_POINT('Ctrl Pts',(-18.3683487595105,33.8077942409485,122.802558224902)) ;
#23025 = CARTESIAN_POINT('Ctrl Pts',(-18.1081263093149,33.6278051605856,122.650231330554)) ;
#23026 = CARTESIAN_POINT('Ctrl Pts',(-18.4904696258343,33.8178223427358,122.63070110739)) ;
#23027 = CARTESIAN_POINT('Ctrl Pts',(-18.2607792875272,33.6378332623729,122.435411305488)) ;
#23028 = CARTESIAN_POINT('Ctrl Pts',(-18.6381482308556,33.8277022873588,122.484636845884)) ;
#23029 = CARTESIAN_POINT('Ctrl Pts',(-18.4453797141511,33.647713206996,122.252832221367)) ;
#23030 = CARTESIAN_POINT('Ctrl Pts',(-18.8106558657306,33.8376926139159,122.364855145629)) ;
#23031 = CARTESIAN_POINT('Ctrl Pts',(-18.6610157891126,33.657703533553,122.10310705135)) ;
#23032 = CARTESIAN_POINT('Ctrl Pts',(-19.0004133748142,33.8476335455702,122.277272733612)) ;
#23033 = CARTESIAN_POINT('Ctrl Pts',(-18.8982140305105,33.6676444652073,121.993631136502)) ;
#23034 = CARTESIAN_POINT('Ctrl Pts',(-19.2033679275045,33.8576206640731,122.223428561579)) ;
#23035 = CARTESIAN_POINT('Ctrl Pts',(-19.1519080089799,33.6776315837102,121.92632833614)) ;
#23036 = CARTESIAN_POINT('Ctrl Pts',(-19.413555239702,33.8676539969703,122.205893497392)) ;
#23037 = CARTESIAN_POINT('Ctrl Pts',(-19.4146423301779,33.6876649166074,121.904411969349)) ;
#23038 = CARTESIAN_POINT('Ctrl Pts',(-19.6201683892138,33.877520101415,122.224398460952)) ;
#23039 = CARTESIAN_POINT('Ctrl Pts',(-19.6729091690056,33.6975310210521,121.927545767156)) ;
#23040 = CARTESIAN_POINT('Ctrl Pts',(-19.824456202544,33.8875862152953,122.279533485596)) ;
#23041 = CARTESIAN_POINT('Ctrl Pts',(-19.9282681240009,33.7075971349325,121.996466980296)) ;
#23042 = CARTESIAN_POINT('Ctrl Pts',(-20.0121077833752,33.8974422270637,122.367434002635)) ;
#23043 = CARTESIAN_POINT('Ctrl Pts',(-20.1628320829574,33.7174531467009,122.10634520991)) ;
#23044 = CARTESIAN_POINT('Ctrl Pts',(-20.1843716366312,33.9074369306951,122.487738822849)) ;
#23045 = CARTESIAN_POINT('Ctrl Pts',(-20.3781604555604,33.7274478503322,122.256728476995)) ;
#23046 = CARTESIAN_POINT('Ctrl Pts',(-20.3333627134761,33.9174682664199,122.63699684848)) ;
#23047 = CARTESIAN_POINT('Ctrl Pts',(-20.5643974693118,33.7374791860571,122.443302838799)) ;
#23048 = CARTESIAN_POINT('Ctrl Pts',(-20.4524620397036,33.9273347916236,122.806830884017)) ;
#23049 = CARTESIAN_POINT('Ctrl Pts',(-20.713269761922,33.7473457112607,122.655597325724)) ;
#23050 = CARTESIAN_POINT('Ctrl Pts',(-20.5416324218957,33.9373222196694,122.996895065908)) ;
#23051 = CARTESIAN_POINT('Ctrl Pts',(-20.8247303532555,33.7573331393065,122.893178808627)) ;
#23052 = CARTESIAN_POINT('Ctrl Pts',(-20.5963371639424,33.9472671493558,123.198716985131)) ;
#23053 = CARTESIAN_POINT('Ctrl Pts',(-20.8931087336896,33.767278068993,123.145457142139)) ;
#23054 = CARTESIAN_POINT('Ctrl Pts',(-20.615233404167,33.9573120674643,123.409025558996)) ;
#23055 = CARTESIAN_POINT('Ctrl Pts',(-20.9167263518425,33.7773229871015,123.408343079754)) ;
#23056 = CARTESIAN_POINT('Ctrl Pts',(-20.5978343581406,33.9671740370782,123.615640699636)) ;
#23057 = CARTESIAN_POINT('Ctrl Pts',(-20.8949748056446,33.7871849567154,123.666612207482)) ;
#23058 = CARTESIAN_POINT('Ctrl Pts',(-20.5445304522243,33.9771661050995,123.818808413641)) ;
#23059 = CARTESIAN_POINT('Ctrl Pts',(-20.8283422293108,33.7971770247366,123.920571241178)) ;
#23060 = CARTESIAN_POINT('Ctrl Pts',(-20.4572488945019,33.987097030474,124.008482314326)) ;
#23061 = CARTESIAN_POINT('Ctrl Pts',(-20.7192376865205,33.8071079501112,124.157662672187)) ;
#23062 = CARTESIAN_POINT('Ctrl Pts',(-20.3384279441806,33.9970476586975,124.180637038288)) ;
#23063 = CARTESIAN_POINT('Ctrl Pts',(-20.5707091129721,33.8170585783346,124.372854625881)) ;
#23064 = CARTESIAN_POINT('Ctrl Pts',(-20.1908473350017,34.0070478977566,124.330400148074)) ;
#23065 = CARTESIAN_POINT('Ctrl Pts',(-20.3862313186414,33.8270588173937,124.560056609312)) ;
#23066 = CARTESIAN_POINT('Ctrl Pts',(-20.0188703479351,34.0170763531258,124.452341161375)) ;
#23067 = CARTESIAN_POINT('Ctrl Pts',(-20.1712584195521,33.8370872727629,124.71248063517)) ;
#23068 = CARTESIAN_POINT('Ctrl Pts',(-19.8315368351169,34.026942387709,124.541398156012)) ;
#23069 = CARTESIAN_POINT('Ctrl Pts',(-19.9370901885251,33.8469533073462,124.823799494521)) ;
#23070 = CARTESIAN_POINT('Ctrl Pts',(-19.6291473919891,34.0369347094565,124.597606613349)) ;
#23071 = CARTESIAN_POINT('Ctrl Pts',(-19.6841021964421,33.8569456290936,124.894057284954)) ;
#23072 = CARTESIAN_POINT('Ctrl Pts',(-19.4212948778569,34.0468669991335,124.617735601843)) ;
#23073 = CARTESIAN_POINT('Ctrl Pts',(-19.424287490384,33.8668779187706,124.9192160717)) ;
#23074 = CARTESIAN_POINT('Ctrl Pts',(-19.2116608547725,34.0568686441042,124.601562538898)) ;
#23075 = CARTESIAN_POINT('Ctrl Pts',(-19.1622401128872,33.8768795637414,124.898995670993)) ;
#23076 = CARTESIAN_POINT('Ctrl Pts',(-18.9405917318877,34.0701812775203,124.531785628182)) ;
#23077 = CARTESIAN_POINT('Ctrl Pts',(-18.823429392135,33.8901921971574,124.811777112252)) ;
#23078 = CARTESIAN_POINT('Ctrl Pts',(-18.6953484784507,34.0834130269018,124.393891815293)) ;
#23079 = CARTESIAN_POINT('Ctrl Pts',(-18.5168908225473,33.903423946539,124.639429121269)) ;
#23080 = CARTESIAN_POINT('Ctrl Pts',(-18.4950002821873,34.0967362917189,124.198208396693)) ;
#23081 = CARTESIAN_POINT('Ctrl Pts',(-18.266416953034,33.916747211356,124.394788919274)) ;
#23082 = CARTESIAN_POINT('Ctrl Pts',(-18.3736497757206,34.1066119979366,124.029725845387)) ;
#23083 = CARTESIAN_POINT('Ctrl Pts',(-18.1147393757088,33.9266229175737,124.184190734435)) ;
#23084 = CARTESIAN_POINT('Ctrl Pts',(-18.2821299159748,34.1166015890366,123.840730802708)) ;
#23085 = CARTESIAN_POINT('Ctrl Pts',(-18.0003398463956,33.9366125086737,123.947943873737)) ;
#23086 = CARTESIAN_POINT('Ctrl Pts',(-18.2250270269363,34.126528685492,123.639969576889)) ;
#23087 = CARTESIAN_POINT('Ctrl Pts',(-17.9289645288639,33.9465396051291,123.69699206503)) ;
#23088 = CARTESIAN_POINT('Ctrl Pts',(-18.2034190105843,34.1365538339966,123.430338906527)) ;
#23089 = CARTESIAN_POINT('Ctrl Pts',(-17.9019571311773,33.9565647536337,123.434953214904)) ;
#23090 = CARTESIAN_POINT('Ctrl Pts',(-18.2182165399645,34.1464494881433,123.22280972338)) ;
#23091 = CARTESIAN_POINT('Ctrl Pts',(-17.920456867938,33.9664604077804,123.175542057052)) ;
#23092 = CARTESIAN_POINT('Ctrl Pts',(-18.2690763393294,34.1564530225215,123.018767205604)) ;
#23093 = CARTESIAN_POINT('Ctrl Pts',(-17.9840343132116,33.9764639421586,122.920489516577)) ;
#23094 = CARTESIAN_POINT('Ctrl Pts',(-18.3544753384947,34.1664381609615,122.826969229147)) ;
#23095 = CARTESIAN_POINT('Ctrl Pts',(-18.0907856147797,33.9864490805987,122.680743142477)) ;
#23096 = CARTESIAN_POINT('Ctrl Pts',(-18.472628068217,34.1764740855569,122.652181840679)) ;
#23097 = CARTESIAN_POINT('Ctrl Pts',(-18.2384789185145,33.996485005194,122.462260358717)) ;
#23098 = CARTESIAN_POINT('Ctrl Pts',(-18.6164655673293,34.1863253609846,122.503176356432)) ;
#23099 = CARTESIAN_POINT('Ctrl Pts',(-18.4182776203018,34.0063362806217,122.276005602402)) ;
#23100 = CARTESIAN_POINT('Ctrl Pts',(-18.7860413391488,34.1963176221459,122.379176678945)) ;
#23101 = CARTESIAN_POINT('Ctrl Pts',(-18.6302489538193,34.0163285417831,122.121008187001)) ;
#23102 = CARTESIAN_POINT('Ctrl Pts',(-18.9756890039157,34.2063575061635,122.28655058311)) ;
#23103 = CARTESIAN_POINT('Ctrl Pts',(-18.8673098715377,34.0263684258007,122.00522798075)) ;
#23104 = CARTESIAN_POINT('Ctrl Pts',(-19.1742841833314,34.216192280666,122.228937175601)) ;
#23105 = CARTESIAN_POINT('Ctrl Pts',(-19.1155543481873,34.0362032003031,121.933213929773)) ;
#23106 = CARTESIAN_POINT('Ctrl Pts',(-19.3848491923498,34.2262686616863,122.206064095347)) ;
#23107 = CARTESIAN_POINT('Ctrl Pts',(-19.3787606441446,34.0462795813234,121.904625237353)) ;
#23108 = CARTESIAN_POINT('Ctrl Pts',(-19.5914235484233,34.2361149348369,122.219725589952)) ;
#23109 = CARTESIAN_POINT('Ctrl Pts',(-19.636979964933,34.056125854474,121.921704730838)) ;
#23110 = CARTESIAN_POINT('Ctrl Pts',(-19.8644290889112,34.2494794561221,122.286150104752)) ;
#23111 = CARTESIAN_POINT('Ctrl Pts',(-19.9782262367002,34.0694903757593,122.004738916925)) ;
#23112 = CARTESIAN_POINT('Ctrl Pts',(-20.1107333011822,34.2626857005566,122.421054667692)) ;
#23113 = CARTESIAN_POINT('Ctrl Pts',(-20.2860725515586,34.0826966201937,122.173341752895)) ;
#23114 = CARTESIAN_POINT('Ctrl Pts',(-20.3128900283233,34.2759506552338,122.613069418679)) ;
#23115 = CARTESIAN_POINT('Ctrl Pts',(-20.5388137926812,34.0959615748709,122.413398914322)) ;
#23116 = CARTESIAN_POINT('Ctrl Pts',(-20.438205183774,34.2859829357855,122.782731790521)) ;
#23117 = CARTESIAN_POINT('Ctrl Pts',(-20.6954462284396,34.1059938554226,122.625471146507)) ;
#23118 = CARTESIAN_POINT('Ctrl Pts',(-20.5310032145783,34.2958916693034,122.96922602419)) ;
#23119 = CARTESIAN_POINT('Ctrl Pts',(-20.8114438350329,34.1159025889405,122.858591933872)) ;
#23120 = CARTESIAN_POINT('Ctrl Pts',(-20.5907085275571,34.3058292201709,123.169440553708)) ;
#23121 = CARTESIAN_POINT('Ctrl Pts',(-20.8860726329882,34.125840139808,123.108858926557)) ;
#23122 = CARTESIAN_POINT('Ctrl Pts',(-20.6147885837747,34.3158590677648,123.378897155107)) ;
#23123 = CARTESIAN_POINT('Ctrl Pts',(-20.9161696354576,34.1358699874019,123.370684085346)) ;
#23124 = CARTESIAN_POINT('Ctrl Pts',(-20.5984660377212,34.3290942076852,123.656745178139)) ;
#23125 = CARTESIAN_POINT('Ctrl Pts',(-20.8957675550664,34.1491051273224,123.717974610671)) ;
#23126 = CARTESIAN_POINT('Ctrl Pts',(-20.4868736795983,34.3457626720564,123.993002939098)) ;
#23127 = CARTESIAN_POINT('Ctrl Pts',(-20.7562726268257,34.1657735916935,124.138314956001)) ;
#23128 = CARTESIAN_POINT('Ctrl Pts',(-20.2251415994005,34.3656336839303,124.324854114814)) ;
#23129 = CARTESIAN_POINT('Ctrl Pts',(-20.4290861791078,34.1856446035674,124.553127465598)) ;
#23130 = CARTESIAN_POINT('Ctrl Pts',(-19.9231542481283,34.3823407683133,124.511841033235)) ;
#23131 = CARTESIAN_POINT('Ctrl Pts',(-20.0516612997823,34.2023516879504,124.786832185012)) ;
#23132 = CARTESIAN_POINT('Ctrl Pts',(-19.657904162901,34.3955180496239,124.591763757733)) ;
#23133 = CARTESIAN_POINT('Ctrl Pts',(-19.7200431655426,34.215528969261,124.88675620924)) ;
#23134 = CARTESIAN_POINT('Ctrl Pts',(-19.3810401547888,34.408785510138,124.625633782009)) ;
#23135 = CARTESIAN_POINT('Ctrl Pts',(-19.3739840223207,34.2287964297751,124.92908813568)) ;
#23136 = CARTESIAN_POINT('Ctrl Pts',(-19.0312401721135,34.4253994008252,124.576410369976)) ;
#23137 = CARTESIAN_POINT('Ctrl Pts',(-18.936720024018,34.2454103204623,124.86755517988)) ;
#23138 = CARTESIAN_POINT('Ctrl Pts',(-18.6565409852236,34.4453482002526,124.377526322459)) ;
#23139 = CARTESIAN_POINT('Ctrl Pts',(-18.4683529488932,34.2653591198897,124.618947214226)) ;
#23140 = CARTESIAN_POINT('Ctrl Pts',(-18.372722975046,34.4652693117834,124.063178650212)) ;
#23141 = CARTESIAN_POINT('Ctrl Pts',(-18.1135823385577,34.2852802314206,124.226010700003)) ;
#23142 = CARTESIAN_POINT('Ctrl Pts',(-18.2127872385282,34.4851357599563,123.672140863886)) ;
#23143 = CARTESIAN_POINT('Ctrl Pts',(-17.9136663305497,34.3051466795934,123.737213595555)) ;
#23144 = CARTESIAN_POINT('Ctrl Pts',(-18.1960174572984,34.5051621065734,123.246703868946)) ;
#23145 = CARTESIAN_POINT('Ctrl Pts',(-17.8927069831386,34.3251730262106,123.205416904764)) ;
#23146 = CARTESIAN_POINT('Ctrl Pts',(-18.3244861075331,34.525024150963,122.844320049915)) ;
#23147 = CARTESIAN_POINT('Ctrl Pts',(-18.0532950837359,34.3450350706001,122.702439446676)) ;
#23148 = CARTESIAN_POINT('Ctrl Pts',(-18.5830265246617,34.5449694536441,122.508225439242)) ;
#23149 = CARTESIAN_POINT('Ctrl Pts',(-18.3764719974847,34.3649803732812,122.282323158732)) ;
#23150 = CARTESIAN_POINT('Ctrl Pts',(-18.9399371008137,34.564864760703,122.281121704416)) ;
#23151 = CARTESIAN_POINT('Ctrl Pts',(-18.8226102498659,34.3848756803401,121.998446004947)) ;
#23152 = CARTESIAN_POINT('Ctrl Pts',(-19.3527127164133,34.5847580308706,122.188711680669)) ;
#23153 = CARTESIAN_POINT('Ctrl Pts',(-19.3385786404572,34.4047689505077,121.882935209767)) ;
#23154 = CARTESIAN_POINT('Ctrl Pts',(-19.7737254388914,34.604723623551,122.242987808738)) ;
#23155 = CARTESIAN_POINT('Ctrl Pts',(-19.864843872694,34.4247345431882,121.950781567567)) ;
#23156 = CARTESIAN_POINT('Ctrl Pts',(-20.1494199931143,34.6245989472359,122.436554500858)) ;
#23157 = CARTESIAN_POINT('Ctrl Pts',(-20.3344600160615,34.444609866873,122.192739799094)) ;
#23158 = CARTESIAN_POINT('Ctrl Pts',(-20.4382613496929,34.6445740098108,122.747966146561)) ;
#23159 = CARTESIAN_POINT('Ctrl Pts',(-20.6955112754201,34.464584929448,122.582004291072)) ;
#23160 = CARTESIAN_POINT('Ctrl Pts',(-20.6027074825129,34.6645264194419,123.139039458747)) ;
#23161 = CARTESIAN_POINT('Ctrl Pts',(-20.9010681970121,34.4845373390791,123.070845431308)) ;
#23162 = CARTESIAN_POINT('Ctrl Pts',(-20.6245230947549,34.684362473678,123.560242571632)) ;
#23163 = CARTESIAN_POINT('Ctrl Pts',(-20.9283379623324,34.5043733933152,123.597346656962)) ;
#23164 = CARTESIAN_POINT('Ctrl Pts',(-20.5008638045205,34.7043403850956,123.9666287374)) ;
#23165 = CARTESIAN_POINT('Ctrl Pts',(-20.7737648833637,34.5243513047327,124.105329355223)) ;
#23166 = CARTESIAN_POINT('Ctrl Pts',(-20.2463289326715,34.7242584345991,124.305081206645)) ;
#23167 = CARTESIAN_POINT('Ctrl Pts',(-20.4555977349369,34.5442693542362,124.528394482397)) ;
#23168 = CARTESIAN_POINT('Ctrl Pts',(-19.8929765679083,34.7441265783672,124.53677216459)) ;
#23169 = CARTESIAN_POINT('Ctrl Pts',(-20.0139097341758,34.5641374980043,124.818008765311)) ;
#23170 = CARTESIAN_POINT('Ctrl Pts',(-19.4780285765812,34.7641774349545,124.634188159113)) ;
#23171 = CARTESIAN_POINT('Ctrl Pts',(-19.4952245290992,34.5841883545916,124.939780508264)) ;
#23172 = CARTESIAN_POINT('Ctrl Pts',(-19.060179710771,34.7839578714104,124.585251419341)) ;
#23173 = CARTESIAN_POINT('Ctrl Pts',(-18.9729159061863,34.6039687910475,124.878612004196)) ;
#23174 = CARTESIAN_POINT('Ctrl Pts',(-18.6792558296266,34.8039879270882,124.394988896057)) ;
#23175 = CARTESIAN_POINT('Ctrl Pts',(-18.496759486199,34.6239988467253,124.640786108479)) ;
#23176 = CARTESIAN_POINT('Ctrl Pts',(-18.3887123278353,34.823869032263,124.087835513571)) ;
#23177 = CARTESIAN_POINT('Ctrl Pts',(-18.1335792137849,34.6438799519001,124.256847057463)) ;
#23178 = CARTESIAN_POINT('Ctrl Pts',(-18.2193821090019,34.8437494946307,123.70056629443)) ;
#23179 = CARTESIAN_POINT('Ctrl Pts',(-17.9219139096296,34.6637604142679,123.772762991353)) ;
#23180 = CARTESIAN_POINT('Ctrl Pts',(-18.1923412672095,34.8637346417751,123.276475566402)) ;
#23181 = CARTESIAN_POINT('Ctrl Pts',(-17.8881094855176,34.6837455614122,123.242649910961)) ;
#23182 = CARTESIAN_POINT('Ctrl Pts',(-18.3111763931638,34.8836252203115,122.870576698358)) ;
#23183 = CARTESIAN_POINT('Ctrl Pts',(-18.0366497415648,34.7036361399486,122.735276316463)) ;
#23184 = CARTESIAN_POINT('Ctrl Pts',(-18.5608208396316,34.9035192401859,122.529106310762)) ;
#23185 = CARTESIAN_POINT('Ctrl Pts',(-18.3487015779653,34.723530159823,122.308436690887)) ;
#23186 = CARTESIAN_POINT('Ctrl Pts',(-18.9123762892436,34.9234406849123,122.292940920012)) ;
#23187 = CARTESIAN_POINT('Ctrl Pts',(-18.7881430602527,34.7434516045494,122.013226846896)) ;
#23188 = CARTESIAN_POINT('Ctrl Pts',(-19.322937407292,34.9433388229677,122.190263489512)) ;
#23189 = CARTESIAN_POINT('Ctrl Pts',(-19.3013427498124,34.7633497426048,121.884875817397)) ;
#23190 = CARTESIAN_POINT('Ctrl Pts',(-19.7472655180878,34.9634095781838,122.235024621243)) ;
#23191 = CARTESIAN_POINT('Ctrl Pts',(-19.8317538659919,34.7834204978209,121.940822959894)) ;
#23192 = CARTESIAN_POINT('Ctrl Pts',(-20.1256368241744,34.983195128235,122.419137958029)) ;
#23193 = CARTESIAN_POINT('Ctrl Pts',(-20.3047188071783,34.8032060478722,122.170959918835)) ;
#23194 = CARTESIAN_POINT('Ctrl Pts',(-20.4220114238497,35.0031782031124,122.723491321835)) ;
#23195 = CARTESIAN_POINT('Ctrl Pts',(-20.6751904640124,34.8231891227495,122.55139832022)) ;
#23196 = CARTESIAN_POINT('Ctrl Pts',(-20.5955208583163,35.0230872857583,123.109625284551)) ;
#23197 = CARTESIAN_POINT('Ctrl Pts',(-20.8920819873269,34.8430982053954,123.034062768714)) ;
#23198 = CARTESIAN_POINT('Ctrl Pts',(-20.6279870536071,35.0429458448811,123.530675885179)) ;
#23199 = CARTESIAN_POINT('Ctrl Pts',(-20.9326680570592,34.8629567645182,123.560377307948)) ;
#23200 = CARTESIAN_POINT('Ctrl Pts',(-20.5133192729208,35.0629892887198,123.941055703616)) ;
#23201 = CARTESIAN_POINT('Ctrl Pts',(-20.7893451366516,34.8830002083569,124.073345382285)) ;
#23202 = CARTESIAN_POINT('Ctrl Pts',(-20.3093835063598,35.079489353449,124.226623757706)) ;
#23203 = CARTESIAN_POINT('Ctrl Pts',(-20.5344079580577,34.8995002730861,124.43033347796)) ;
#23204 = CARTESIAN_POINT('Ctrl Pts',(-20.092268777163,35.0928790932979,124.405758678577)) ;
#23205 = CARTESIAN_POINT('Ctrl Pts',(-20.2630356079764,34.912890012935,124.654232063007)) ;
#23206 = CARTESIAN_POINT('Ctrl Pts',(-19.9119702886458,35.1027359945063,124.507953316112)) ;
#23207 = CARTESIAN_POINT('Ctrl Pts',(-20.0376601532639,34.9227469141434,124.781982024209)) ;
#23208 = CARTESIAN_POINT('Ctrl Pts',(-19.7141970013292,35.1127275203528,124.578624517524)) ;
#23209 = CARTESIAN_POINT('Ctrl Pts',(-19.7904462531825,34.9327384399899,124.870322609915)) ;
#23210 = CARTESIAN_POINT('Ctrl Pts',(-19.5084940721676,35.1226522008037,124.613732527868)) ;
#23211 = CARTESIAN_POINT('Ctrl Pts',(-19.5333148830126,34.9426631204409,124.914209741491)) ;
#23212 = CARTESIAN_POINT('Ctrl Pts',(-19.2980655867416,35.1326627908481,124.612658643822)) ;
#23213 = CARTESIAN_POINT('Ctrl Pts',(-19.2702905171994,34.9526737104853,124.912873328828)) ;
#23214 = CARTESIAN_POINT('Ctrl Pts',(-19.0237133873326,35.1459220515518,124.563175266845)) ;
#23215 = CARTESIAN_POINT('Ctrl Pts',(-18.9272936377873,34.9659329711889,124.851006430555)) ;
#23216 = CARTESIAN_POINT('Ctrl Pts',(-18.7669990026085,35.1592731267021,124.442141475141)) ;
#23217 = CARTESIAN_POINT('Ctrl Pts',(-18.606436005865,34.9792840463392,124.69972105366)) ;
#23218 = CARTESIAN_POINT('Ctrl Pts',(-18.5548922307535,35.1724794359369,124.262885149978)) ;
#23219 = CARTESIAN_POINT('Ctrl Pts',(-18.3413122765646,34.992490355574,124.475665673841)) ;
#23220 = CARTESIAN_POINT('Ctrl Pts',(-18.4202016194479,35.1824662695272,124.101878407724)) ;
#23221 = CARTESIAN_POINT('Ctrl Pts',(-18.1729444100433,35.0024771891643,124.274406568228)) ;
#23222 = CARTESIAN_POINT('Ctrl Pts',(-18.3157421931826,35.1924189970233,123.920538588917)) ;
#23223 = CARTESIAN_POINT('Ctrl Pts',(-18.0423683362087,35.0124299166604,124.047733829672)) ;
#23224 = CARTESIAN_POINT('Ctrl Pts',(-18.243859696856,35.2024670938648,123.721927113406)) ;
#23225 = CARTESIAN_POINT('Ctrl Pts',(-17.9525123755645,35.022478013502,123.799470169266)) ;
#23226 = CARTESIAN_POINT('Ctrl Pts',(-18.2080532676477,35.2123085507367,123.518130094329)) ;
#23227 = CARTESIAN_POINT('Ctrl Pts',(-17.9077516294115,35.0323194703738,123.544724476242)) ;
#23228 = CARTESIAN_POINT('Ctrl Pts',(-18.2077298878391,35.2222948176502,123.308221872427)) ;
#23229 = CARTESIAN_POINT('Ctrl Pts',(-17.9073445683786,35.0423057372873,123.282339109367)) ;
#23230 = CARTESIAN_POINT('Ctrl Pts',(-18.2435874649064,35.2322314185506,123.102388357164)) ;
#23231 = CARTESIAN_POINT('Ctrl Pts',(-17.9521637827218,35.0522423381877,123.025046666914)) ;
#23232 = CARTESIAN_POINT('Ctrl Pts',(-18.3155310783834,35.2422813613376,122.903755486322)) ;
#23233 = CARTESIAN_POINT('Ctrl Pts',(-18.0420906679866,35.0622922809748,122.776754559742)) ;
#23234 = CARTESIAN_POINT('Ctrl Pts',(-18.4186601658913,35.2521315610234,122.724163217864)) ;
#23235 = CARTESIAN_POINT('Ctrl Pts',(-18.1709996406622,35.0721424806605,122.552262724124)) ;
#23236 = CARTESIAN_POINT('Ctrl Pts',(-18.5526102972871,35.2621044659555,122.562900255392)) ;
#23237 = CARTESIAN_POINT('Ctrl Pts',(-18.3384352196694,35.0821153855926,122.350682137594)) ;
#23238 = CARTESIAN_POINT('Ctrl Pts',(-18.7130161190752,35.2721028404351,122.427018538122)) ;
#23239 = CARTESIAN_POINT('Ctrl Pts',(-18.5389407429953,35.0921137600722,122.180827804113)) ;
#23240 = CARTESIAN_POINT('Ctrl Pts',(-18.8950233937213,35.2821230143051,122.320968913956)) ;
#23241 = CARTESIAN_POINT('Ctrl Pts',(-18.7664484679922,35.1021339339422,122.048263316574)) ;
#23242 = CARTESIAN_POINT('Ctrl Pts',(-19.0902785173193,35.2920240582471,122.248825467389)) ;
#23243 = CARTESIAN_POINT('Ctrl Pts',(-19.0105165623716,35.1120349778842,121.958081319082)) ;
#23244 = CARTESIAN_POINT('Ctrl Pts',(-19.2968437850745,35.3020128619714,122.211027115049)) ;
#23245 = CARTESIAN_POINT('Ctrl Pts',(-19.2687227454526,35.1220237816085,121.910830619248)) ;
#23246 = CARTESIAN_POINT('Ctrl Pts',(-19.5063361205008,35.3119783288032,122.209821899411)) ;
#23247 = CARTESIAN_POINT('Ctrl Pts',(-19.5305882706686,35.1319892484403,121.909321300949)) ;
#23248 = CARTESIAN_POINT('Ctrl Pts',(-19.7116863669934,35.3218818910762,122.244299443621)) ;
#23249 = CARTESIAN_POINT('Ctrl Pts',(-19.7872767838356,35.1418928107133,121.952415553993)) ;
#23250 = CARTESIAN_POINT('Ctrl Pts',(-19.9109411377999,35.3319425689542,122.31516138068)) ;
#23251 = CARTESIAN_POINT('Ctrl Pts',(-20.0363461469721,35.1519534885913,122.040990349835)) ;
#23252 = CARTESIAN_POINT('Ctrl Pts',(-20.0910169677187,35.3417828669036,122.417053554877)) ;
#23253 = CARTESIAN_POINT('Ctrl Pts',(-20.2614426416287,35.1617937865408,122.168353377903)) ;
#23254 = CARTESIAN_POINT('Ctrl Pts',(-20.2543967354931,35.3518458618131,122.551408724914)) ;
#23255 = CARTESIAN_POINT('Ctrl Pts',(-20.4656690482286,35.1718567814502,122.33629520841)) ;
#23256 = CARTESIAN_POINT('Ctrl Pts',(-20.389561216917,35.3617401559602,122.709546984576)) ;
#23257 = CARTESIAN_POINT('Ctrl Pts',(-20.6346269466373,35.1817510755973,122.533966500745)) ;
#23258 = CARTESIAN_POINT('Ctrl Pts',(-20.4961856714635,35.3716819536571,122.889282267769)) ;
#23259 = CARTESIAN_POINT('Ctrl Pts',(-20.7679099510609,35.1916928732942,122.758634465352)) ;
#23260 = CARTESIAN_POINT('Ctrl Pts',(-20.5705249428159,35.3816845311862,123.08601924968)) ;
#23261 = CARTESIAN_POINT('Ctrl Pts',(-20.8608365588192,35.2016954508233,123.004554830575)) ;
#23262 = CARTESIAN_POINT('Ctrl Pts',(-20.6093729379891,35.3917189951073,123.293356771096)) ;
#23263 = CARTESIAN_POINT('Ctrl Pts',(-20.9093992123313,35.2117299147444,123.263726218813)) ;
#23264 = CARTESIAN_POINT('Ctrl Pts',(-20.6119121965854,35.4015651336283,123.500344351237)) ;
#23265 = CARTESIAN_POINT('Ctrl Pts',(-20.912575954229,35.2215760532655,123.522461220006)) ;
#23266 = CARTESIAN_POINT('Ctrl Pts',(-20.5784797869807,35.4115463068653,123.707482594867)) ;
#23267 = CARTESIAN_POINT('Ctrl Pts',(-20.8707879748683,35.2315572265025,123.781384610257)) ;
#23268 = CARTESIAN_POINT('Ctrl Pts',(-20.5097340551168,35.4214986008226,123.905101498051)) ;
#23269 = CARTESIAN_POINT('Ctrl Pts',(-20.7848581741263,35.2415095204597,124.028409346698)) ;
#23270 = CARTESIAN_POINT('Ctrl Pts',(-20.4074763823881,35.4314973959572,124.088777449656)) ;
#23271 = CARTESIAN_POINT('Ctrl Pts',(-20.6570382603351,35.2515083155943,124.258005618651)) ;
#23272 = CARTESIAN_POINT('Ctrl Pts',(-20.2740486464451,35.441536504218,124.252287560575)) ;
#23273 = CARTESIAN_POINT('Ctrl Pts',(-20.4902556612724,35.2615474238551,124.462394870675)) ;
#23274 = CARTESIAN_POINT('Ctrl Pts',(-20.1179375824698,35.4513614456571,124.387557243279)) ;
#23275 = CARTESIAN_POINT('Ctrl Pts',(-20.2951179160963,35.2713723652943,124.631484396849)) ;
#23276 = CARTESIAN_POINT('Ctrl Pts',(-19.9367669407761,35.4614161327315,124.496432561187)) ;
#23277 = CARTESIAN_POINT('Ctrl Pts',(-20.0686559821828,35.2814270523687,124.767580615175)) ;
#23278 = CARTESIAN_POINT('Ctrl Pts',(-19.7414940311369,35.4713589376717,124.571026731004)) ;
#23279 = CARTESIAN_POINT('Ctrl Pts',(-19.8245654449264,35.2913698573088,124.860825828368)) ;
#23280 = CARTESIAN_POINT('Ctrl Pts',(-19.5371642498936,35.4812627236682,124.611053711609)) ;
#23281 = CARTESIAN_POINT('Ctrl Pts',(-19.5691531625667,35.3012736433053,124.910862029586)) ;
#23282 = CARTESIAN_POINT('Ctrl Pts',(-19.3260021505189,35.491309540233,124.614922626693)) ;
#23283 = CARTESIAN_POINT('Ctrl Pts',(-19.3052006854437,35.3113204598701,124.915700617854)) ;
#23284 = CARTESIAN_POINT('Ctrl Pts',(-19.1204374563193,35.5012050597117,124.582740242867)) ;
#23285 = CARTESIAN_POINT('Ctrl Pts',(-19.0482438728121,35.3212159793488,124.875474923149)) ;
#23286 = CARTESIAN_POINT('Ctrl Pts',(-18.9203301984494,35.5112671450361,124.514241085289)) ;
#23287 = CARTESIAN_POINT('Ctrl Pts',(-18.7981091918514,35.3312780646732,124.789853312718)) ;
#23288 = CARTESIAN_POINT('Ctrl Pts',(-18.7390904234207,35.521109855994,124.414343573593)) ;
#23289 = CARTESIAN_POINT('Ctrl Pts',(-18.571557569673,35.3411207756312,124.664983089902)) ;
#23290 = CARTESIAN_POINT('Ctrl Pts',(-18.575252732091,35.5311005733001,124.282960921875)) ;
#23291 = CARTESIAN_POINT('Ctrl Pts',(-18.3667589020139,35.3511114929372,124.500756432804)) ;
#23292 = CARTESIAN_POINT('Ctrl Pts',(-18.4375879398549,35.5410286563966,124.126065100434)) ;
#23293 = CARTESIAN_POINT('Ctrl Pts',(-18.1946758847601,35.3610395760338,124.304637787655)) ;
#23294 = CARTESIAN_POINT('Ctrl Pts',(-18.3282912493656,35.5510165865084,123.94676509158)) ;
#23295 = CARTESIAN_POINT('Ctrl Pts',(-18.0580530664321,35.3710275061455,124.080513754998)) ;
#23296 = CARTESIAN_POINT('Ctrl Pts',(-18.2517565825726,35.5610524126357,123.750158377981)) ;
#23297 = CARTESIAN_POINT('Ctrl Pts',(-17.9623826480587,35.3810633322728,123.83475626619)) ;
#23298 = CARTESIAN_POINT('Ctrl Pts',(-18.2109351619,35.5709077497493,123.547017923555)) ;
#23299 = CARTESIAN_POINT('Ctrl Pts',(-17.9113535514333,35.3909186693864,123.580830234499)) ;
#23300 = CARTESIAN_POINT('Ctrl Pts',(-18.2056029932862,35.5809054845995,123.336924382834)) ;
#23301 = CARTESIAN_POINT('Ctrl Pts',(-17.9046862415223,35.4009164042366,123.318213209581)) ;
#23302 = CARTESIAN_POINT('Ctrl Pts',(-18.2364854342571,35.5908133885839,123.130921758617)) ;
#23303 = CARTESIAN_POINT('Ctrl Pts',(-17.9432873405184,35.4108243082211,123.060708970242)) ;
#23304 = CARTESIAN_POINT('Ctrl Pts',(-18.3030212952615,35.6008244631324,122.931244855466)) ;
#23305 = CARTESIAN_POINT('Ctrl Pts',(-18.0264553068263,35.4208353827695,122.811112169827)) ;
#23306 = CARTESIAN_POINT('Ctrl Pts',(-18.4037616999809,35.610852318668,122.746053058714)) ;
#23307 = CARTESIAN_POINT('Ctrl Pts',(-18.1523789389796,35.4308632383051,122.579621476818)) ;
#23308 = CARTESIAN_POINT('Ctrl Pts',(-18.532602474964,35.6207099125732,122.583737923954)) ;
#23309 = CARTESIAN_POINT('Ctrl Pts',(-18.3134289650525,35.4407208322104,122.376725539727)) ;
#23310 = CARTESIAN_POINT('Ctrl Pts',(-18.6900489868914,35.6307365994113,122.443575063873)) ;
#23311 = CARTESIAN_POINT('Ctrl Pts',(-18.5102358433116,35.4507475190485,122.201520587918)) ;
#23312 = CARTESIAN_POINT('Ctrl Pts',(-18.8697550672844,35.6407652685651,122.333303125857)) ;
#23313 = CARTESIAN_POINT('Ctrl Pts',(-18.7348673255698,35.4607761882022,122.063678979707)) ;
#23314 = CARTESIAN_POINT('Ctrl Pts',(-19.0621320904684,35.6506104768465,122.256973154102)) ;
#23315 = CARTESIAN_POINT('Ctrl Pts',(-18.9753389392073,35.4706213964836,121.968264330612)) ;
#23316 = CARTESIAN_POINT('Ctrl Pts',(-19.2677365853568,35.6606011658096,122.214031607131)) ;
#23317 = CARTESIAN_POINT('Ctrl Pts',(-19.232344395239,35.4806120854467,121.914585662056)) ;
#23318 = CARTESIAN_POINT('Ctrl Pts',(-19.4786728867515,35.6706390420919,122.207881553144)) ;
#23319 = CARTESIAN_POINT('Ctrl Pts',(-19.4960145845419,35.490649961729,121.906896220203)) ;
#23320 = CARTESIAN_POINT('Ctrl Pts',(-19.6835091491884,35.6804834197341,122.237505000338)) ;
#23321 = CARTESIAN_POINT('Ctrl Pts',(-19.7520613231325,35.5004943393712,121.943923950967)) ;
#23322 = CARTESIAN_POINT('Ctrl Pts',(-19.8829904576665,35.6904682241255,122.302762495252)) ;
#23323 = CARTESIAN_POINT('Ctrl Pts',(-20.0014137029836,35.5104791437627,122.025494346825)) ;
#23324 = CARTESIAN_POINT('Ctrl Pts',(-20.0673637367163,35.7004077543441,122.401163727744)) ;
#23325 = CARTESIAN_POINT('Ctrl Pts',(-20.2318815338735,35.5204186739812,122.148494733348)) ;
#23326 = CARTESIAN_POINT('Ctrl Pts',(-20.2334425789832,35.710447442381,122.531393346306)) ;
#23327 = CARTESIAN_POINT('Ctrl Pts',(-20.4394809697131,35.5304583620181,122.311280393352)) ;
#23328 = CARTESIAN_POINT('Ctrl Pts',(-20.3723559056366,35.7203357317493,122.686064760268)) ;
#23329 = CARTESIAN_POINT('Ctrl Pts',(-20.6131244207075,35.5403466513864,122.504619288811)) ;
#23330 = CARTESIAN_POINT('Ctrl Pts',(-20.4837508188583,35.7303248554341,122.864079606437)) ;
#23331 = CARTESIAN_POINT('Ctrl Pts',(-20.7523694041922,35.5503357750712,122.72713725888)) ;
#23332 = CARTESIAN_POINT('Ctrl Pts',(-20.5621646542934,35.7402848651087,123.058229679049)) ;
#23333 = CARTESIAN_POINT('Ctrl Pts',(-20.8503882560538,35.5602957847458,122.969824688647)) ;
#23334 = CARTESIAN_POINT('Ctrl Pts',(-20.6059033424676,35.7501852948129,123.261726613465)) ;
#23335 = CARTESIAN_POINT('Ctrl Pts',(-20.9050630989688,35.57019621445,123.224196430447)) ;
#23336 = CARTESIAN_POINT('Ctrl Pts',(-20.6137449772283,35.7602283762197,123.472709317713)) ;
#23337 = CARTESIAN_POINT('Ctrl Pts',(-20.9148664709882,35.5802392958568,123.487924566708)) ;
#23338 = CARTESIAN_POINT('Ctrl Pts',(-20.5852260061574,35.7701357701273,123.67904320518)) ;
#23339 = CARTESIAN_POINT('Ctrl Pts',(-20.8792189654738,35.5901466897644,123.74584291802)) ;
#23340 = CARTESIAN_POINT('Ctrl Pts',(-20.5210141564566,35.7801475011165,123.879489186249)) ;
#23341 = CARTESIAN_POINT('Ctrl Pts',(-20.7989552795368,35.6001584207536,123.996400804876)) ;
#23342 = CARTESIAN_POINT('Ctrl Pts',(-20.4224008662751,35.7901797188313,124.06593183367)) ;
#23343 = CARTESIAN_POINT('Ctrl Pts',(-20.6756899073301,35.6101906384684,124.229454654533)) ;
#23344 = CARTESIAN_POINT('Ctrl Pts',(-20.2954649937383,35.8000322280774,124.229594024067)) ;
#23345 = CARTESIAN_POINT('Ctrl Pts',(-20.5170202759795,35.6200431477146,124.434034154075)) ;
#23346 = CARTESIAN_POINT('Ctrl Pts',(-20.1408226833668,35.8099901646204,124.370712894289)) ;
#23347 = CARTESIAN_POINT('Ctrl Pts',(-20.3237177193579,35.6300010842576,124.610433802406)) ;
#23348 = CARTESIAN_POINT('Ctrl Pts',(-19.9624034194556,35.8200290346287,124.483417161163)) ;
#23349 = CARTESIAN_POINT('Ctrl Pts',(-20.1006943914862,35.6400399542659,124.751315017522)) ;
#23350 = CARTESIAN_POINT('Ctrl Pts',(-19.7704532057316,35.829902189787,124.56248627394)) ;
#23351 = CARTESIAN_POINT('Ctrl Pts',(-19.8607559657353,35.6499131094241,124.850152762012)) ;
#23352 = CARTESIAN_POINT('Ctrl Pts',(-19.5636408193586,35.8399754646367,124.607848543225)) ;
#23353 = CARTESIAN_POINT('Ctrl Pts',(-19.6022411196816,35.6599863842738,124.906856510779)) ;
#23354 = CARTESIAN_POINT('Ctrl Pts',(-19.3573296065172,35.8497957818141,124.616666849155)) ;
#23355 = CARTESIAN_POINT('Ctrl Pts',(-19.3443505908473,35.6698067014512,124.917880380727)) ;
#23356 = CARTESIAN_POINT('Ctrl Pts',(-19.1473070231254,35.8598744676076,124.58902082137)) ;
#23357 = CARTESIAN_POINT('Ctrl Pts',(-19.0818227174019,35.6798853872447,124.883323751729)) ;
#23358 = CARTESIAN_POINT('Ctrl Pts',(-18.9497113689918,35.8697259789907,124.526804413324)) ;
#23359 = CARTESIAN_POINT('Ctrl Pts',(-18.8348266453424,35.6897368986278,124.805553629414)) ;
#23360 = CARTESIAN_POINT('Ctrl Pts',(-18.7617765756378,35.8797994252973,124.429271647714)) ;
#23361 = CARTESIAN_POINT('Ctrl Pts',(-18.5999081950905,35.6998103449344,124.683638544709)) ;
#23362 = CARTESIAN_POINT('Ctrl Pts',(-18.597467101793,35.889640700422,124.303505365942)) ;
#23363 = CARTESIAN_POINT('Ctrl Pts',(-18.3945197612094,35.7096516200591,124.526430434708)) ;
#23364 = CARTESIAN_POINT('Ctrl Pts',(-18.4549920931084,35.8996258000788,124.149368497595)) ;
#23365 = CARTESIAN_POINT('Ctrl Pts',(-18.2164254320828,35.7196367197159,124.333759479541)) ;
#23366 = CARTESIAN_POINT('Ctrl Pts',(-18.3414173666157,35.9096332762131,123.972250384681)) ;
#23367 = CARTESIAN_POINT('Ctrl Pts',(-18.0744564633631,35.7296441958502,124.112362113073)) ;
#23368 = CARTESIAN_POINT('Ctrl Pts',(-18.2608430560108,35.919555863922,123.779847146659)) ;
#23369 = CARTESIAN_POINT('Ctrl Pts',(-17.9737377684653,35.7395667835592,123.871857563518)) ;
#23370 = CARTESIAN_POINT('Ctrl Pts',(-18.2142645919712,35.9295424681954,123.575109420464)) ;
#23371 = CARTESIAN_POINT('Ctrl Pts',(-17.915514233427,35.7495533878325,123.61593526692)) ;
#23372 = CARTESIAN_POINT('Ctrl Pts',(-18.2042845382939,35.9395825965295,123.364287204911)) ;
#23373 = CARTESIAN_POINT('Ctrl Pts',(-17.9030386020177,35.7595935161666,123.352407710946)) ;
#23374 = CARTESIAN_POINT('Ctrl Pts',(-18.2300836682839,35.9494220310629,123.159025741679)) ;
#23375 = CARTESIAN_POINT('Ctrl Pts',(-17.9352873093838,35.7694329507,123.095829361004)) ;
#23376 = CARTESIAN_POINT('Ctrl Pts',(-18.2923429640459,35.9594860855539,122.956842133847)) ;
#23377 = CARTESIAN_POINT('Ctrl Pts',(-18.0131110083021,35.779497005191,122.843100123072)) ;
#23378 = CARTESIAN_POINT('Ctrl Pts',(-18.3872080620054,35.969377004791,122.771780131143)) ;
#23379 = CARTESIAN_POINT('Ctrl Pts',(-18.1316925352344,35.7893879244282,122.611771524711)) ;
#23380 = CARTESIAN_POINT('Ctrl Pts',(-18.5136711614344,35.9793689980971,122.604062443733)) ;
#23381 = CARTESIAN_POINT('Ctrl Pts',(-18.2897713917017,35.7993799177342,122.402124132987)) ;
#23382 = CARTESIAN_POINT('Ctrl Pts',(-18.6670229740416,35.9893318620564,122.461407293779)) ;
#23383 = CARTESIAN_POINT('Ctrl Pts',(-18.4814613118421,35.8093427816935,122.223804692162)) ;
#23384 = CARTESIAN_POINT('Ctrl Pts',(-18.8415130358515,35.9992361218741,122.347760866079)) ;
#23385 = CARTESIAN_POINT('Ctrl Pts',(-18.6995746479886,35.8192470415113,122.081746101379)) ;
#23386 = CARTESIAN_POINT('Ctrl Pts',(-19.0361390397703,36.0092966124456,122.26503638611)) ;
#23387 = CARTESIAN_POINT('Ctrl Pts',(-18.9428567780933,35.8293075320827,121.978340523878)) ;
#23388 = CARTESIAN_POINT('Ctrl Pts',(-19.2376557259542,36.0191369620766,122.218129994328)) ;
#23389 = CARTESIAN_POINT('Ctrl Pts',(-19.1947540652062,35.8391478817137,121.919707183759)) ;
#23390 = CARTESIAN_POINT('Ctrl Pts',(-19.4488594057997,36.0291999375666,122.206420949229)) ;
#23391 = CARTESIAN_POINT('Ctrl Pts',(-19.4587582959314,35.8492108572037,121.905070980687)) ;
#23392 = CARTESIAN_POINT('Ctrl Pts',(-19.6553963029658,36.03909425771,122.231316246705)) ;
#23393 = CARTESIAN_POINT('Ctrl Pts',(-19.716930430725,35.8591051773471,121.936190237955)) ;
#23394 = CARTESIAN_POINT('Ctrl Pts',(-19.8555419191766,36.0490359708416,122.291429452583)) ;
#23395 = CARTESIAN_POINT('Ctrl Pts',(-19.9671129941824,35.8690468904787,122.011332156098)) ;
#23396 = CARTESIAN_POINT('Ctrl Pts',(-20.0434534803591,36.0590388606357,122.385905221195)) ;
#23397 = CARTESIAN_POINT('Ctrl Pts',(-20.2020024297301,35.8790497802728,122.129427167199)) ;
#23398 = CARTESIAN_POINT('Ctrl Pts',(-20.2124564475029,36.0690787177962,122.512316557016)) ;
#23399 = CARTESIAN_POINT('Ctrl Pts',(-20.4132559197395,35.8890896374333,122.28744132461)) ;
#23400 = CARTESIAN_POINT('Ctrl Pts',(-20.3542066989014,36.0789028986338,122.662550738687)) ;
#23401 = CARTESIAN_POINT('Ctrl Pts',(-20.5904446049363,35.8989138182709,122.475235422024)) ;
#23402 = CARTESIAN_POINT('Ctrl Pts',(-20.4706332696789,36.088959872137,122.839015977808)) ;
#23403 = CARTESIAN_POINT('Ctrl Pts',(-20.7359772784035,35.9089707917741,122.695816923843)) ;
#23404 = CARTESIAN_POINT('Ctrl Pts',(-20.5533425088199,36.0988879963241,123.030662056921)) ;
#23405 = CARTESIAN_POINT('Ctrl Pts',(-20.8393638309279,35.9188989159612,122.935375322683)) ;
#23406 = CARTESIAN_POINT('Ctrl Pts',(-20.6021853906492,36.1088416913975,123.234141443748)) ;
#23407 = CARTESIAN_POINT('Ctrl Pts',(-20.9004170383969,35.9288526110346,123.189725205683)) ;
#23408 = CARTESIAN_POINT('Ctrl Pts',(-20.6147732903502,36.1188878849728,123.444966785403)) ;
#23409 = CARTESIAN_POINT('Ctrl Pts',(-20.9161514803797,35.9388988046099,123.453256665995)) ;
#23410 = CARTESIAN_POINT('Ctrl Pts',(-20.5912389874168,36.1287359873327,123.65066140107)) ;
#23411 = CARTESIAN_POINT('Ctrl Pts',(-20.8867329496708,35.9487469069698,123.710376268567)) ;
#23412 = CARTESIAN_POINT('Ctrl Pts',(-20.5322920817203,36.1386975755603,123.851608665551)) ;
#23413 = CARTESIAN_POINT('Ctrl Pts',(-20.813048468652,35.9587084951974,123.961560575043)) ;
#23414 = CARTESIAN_POINT('Ctrl Pts',(-20.4384766708263,36.1487262457165,124.040434185181)) ;
#23415 = CARTESIAN_POINT('Ctrl Pts',(-20.6957786698797,35.9687371653537,124.19759210035)) ;
#23416 = CARTESIAN_POINT('Ctrl Pts',(-20.3148448154568,36.1586365485983,124.208121309133)) ;
#23417 = CARTESIAN_POINT('Ctrl Pts',(-20.5412377893036,35.9786474682354,124.407201312219)) ;
#23418 = CARTESIAN_POINT('Ctrl Pts',(-20.1639673049378,36.1685714324062,124.352558297041)) ;
#23419 = CARTESIAN_POINT('Ctrl Pts',(-20.3526398125085,35.9885823520433,124.587747365873)) ;
#23420 = CARTESIAN_POINT('Ctrl Pts',(-19.9883464931502,36.1786125740968,124.4696744726)) ;
#23421 = CARTESIAN_POINT('Ctrl Pts',(-20.1331135059456,35.9986234937339,124.734141809642)) ;
#23422 = CARTESIAN_POINT('Ctrl Pts',(-19.7980654386768,36.1884996952608,124.553357993941)) ;
#23423 = CARTESIAN_POINT('Ctrl Pts',(-19.8952608881985,36.0085106148979,124.838745840386)) ;
#23424 = CARTESIAN_POINT('Ctrl Pts',(-19.5941039539844,36.1984920381093,124.603590833534)) ;
#23425 = CARTESIAN_POINT('Ctrl Pts',(-19.6403085962477,36.0185029577464,124.901535971408)) ;
#23426 = CARTESIAN_POINT('Ctrl Pts',(-19.3854139464057,36.2084403393333,124.617526696654)) ;
#23427 = CARTESIAN_POINT('Ctrl Pts',(-19.3794454821469,36.0284512589704,124.918954868183)) ;
#23428 = CARTESIAN_POINT('Ctrl Pts',(-19.1776885830865,36.2183779170154,124.595344537768)) ;
#23429 = CARTESIAN_POINT('Ctrl Pts',(-19.1197882532334,36.0383888366525,124.8912260194)) ;
#23430 = CARTESIAN_POINT('Ctrl Pts',(-18.9758949839322,36.228364491466,124.537343966283)) ;
#23431 = CARTESIAN_POINT('Ctrl Pts',(-18.8675463523897,36.0483754111031,124.818724120264)) ;
#23432 = CARTESIAN_POINT('Ctrl Pts',(-18.7865605948736,36.2383933013744,124.444585421192)) ;
#23433 = CARTESIAN_POINT('Ctrl Pts',(-18.6308789216368,36.0584042210115,124.702775017872)) ;
#23434 = CARTESIAN_POINT('Ctrl Pts',(-18.6186460163788,36.2482716226812,124.322389246568)) ;
#23435 = CARTESIAN_POINT('Ctrl Pts',(-18.4209855121877,36.0682825423183,124.550028242115)) ;
#23436 = CARTESIAN_POINT('Ctrl Pts',(-18.4724839475725,36.2582632700286,124.171514768616)) ;
#23437 = CARTESIAN_POINT('Ctrl Pts',(-18.2382837456184,36.0782741896657,124.361434085726)) ;
#23438 = CARTESIAN_POINT('Ctrl Pts',(-18.3546005152364,36.2682977934664,123.996579143374)) ;
#23439 = CARTESIAN_POINT('Ctrl Pts',(-18.0909304837619,36.0883087131035,124.142763989122)) ;
#23440 = CARTESIAN_POINT('Ctrl Pts',(-18.2699376189153,36.278161150345,123.80726784102)) ;
#23441 = CARTESIAN_POINT('Ctrl Pts',(-17.9851026047473,36.0981720699821,123.906123266323)) ;
#23442 = CARTESIAN_POINT('Ctrl Pts',(-18.2183426275422,36.2882313770253,123.601966412164)) ;
#23443 = CARTESIAN_POINT('Ctrl Pts',(-17.9206102595099,36.1082422966624,123.649496524002)) ;
#23444 = CARTESIAN_POINT('Ctrl Pts',(-18.2035300755518,36.2980736851599,123.395572554759)) ;
#23445 = CARTESIAN_POINT('Ctrl Pts',(-17.9020958099089,36.1180846047971,123.391502808904)) ;
#23446 = CARTESIAN_POINT('Ctrl Pts',(-18.2242647172834,36.3080344171834,123.187200743274)) ;
#23447 = CARTESIAN_POINT('Ctrl Pts',(-17.9280157514707,36.1280453368205,123.131037798645)) ;
#23448 = CARTESIAN_POINT('Ctrl Pts',(-18.2817044009816,36.3180723063815,122.984147670972)) ;
#23449 = CARTESIAN_POINT('Ctrl Pts',(-17.999816726095,36.1380832260186,122.877221984986)) ;
#23450 = CARTESIAN_POINT('Ctrl Pts',(-18.3716994134048,36.3279465893003,122.797053220826)) ;
#23451 = CARTESIAN_POINT('Ctrl Pts',(-18.1123123668843,36.1479575089374,122.643353698666)) ;
#23452 = CARTESIAN_POINT('Ctrl Pts',(-18.4951890966193,36.3380163339178,122.625139380423)) ;
#23453 = CARTESIAN_POINT('Ctrl Pts',(-18.2666755578384,36.1580272535549,122.428462610188)) ;
#23454 = CARTESIAN_POINT('Ctrl Pts',(-18.6430502592492,36.3478496442634,122.480641003559)) ;
#23455 = CARTESIAN_POINT('Ctrl Pts',(-18.4515040641022,36.1678605639005,122.247839904849)) ;
#23456 = CARTESIAN_POINT('Ctrl Pts',(-18.8168167962975,36.3578798876161,122.361190643597)) ;
#23457 = CARTESIAN_POINT('Ctrl Pts',(-18.6687131962433,36.1778908072532,122.098528505516)) ;
#23458 = CARTESIAN_POINT('Ctrl Pts',(-19.0089931407264,36.3679121755945,122.274279269825)) ;
#23459 = CARTESIAN_POINT('Ctrl Pts',(-18.9089342117129,36.1879230952316,121.98989079608)) ;
#23460 = CARTESIAN_POINT('Ctrl Pts',(-19.2090377913951,36.3777393520626,122.222649776035)) ;
#23461 = CARTESIAN_POINT('Ctrl Pts',(-19.1589917224903,36.1977502716997,121.925355327248)) ;
#23462 = CARTESIAN_POINT('Ctrl Pts',(-19.4186819898018,36.3877447349294,122.205814654101)) ;
#23463 = CARTESIAN_POINT('Ctrl Pts',(-19.4210472098018,36.2077556545666,121.904313326992)) ;
#23464 = CARTESIAN_POINT('Ctrl Pts',(-19.6276479448215,36.3977273739222,122.225666562334)) ;
#23465 = CARTESIAN_POINT('Ctrl Pts',(-19.6822546897857,36.2177382935593,121.929130110005)) ;
#23466 = CARTESIAN_POINT('Ctrl Pts',(-19.831109521622,36.4077714410588,122.282077039624)) ;
#23467 = CARTESIAN_POINT('Ctrl Pts',(-19.9365810271852,36.2277823606959,121.999644910744)) ;
#23468 = CARTESIAN_POINT('Ctrl Pts',(-20.0176363662993,36.4175926598628,122.370629532132)) ;
#23469 = CARTESIAN_POINT('Ctrl Pts',(-20.1697398906336,36.2376035794999,122.110337795579)) ;
#23470 = CARTESIAN_POINT('Ctrl Pts',(-20.1899535608722,36.4276294988008,122.49240362926)) ;
#23471 = CARTESIAN_POINT('Ctrl Pts',(-20.3851350977547,36.247640418438,122.262557053081)) ;
#23472 = CARTESIAN_POINT('Ctrl Pts',(-20.3379053809418,36.4376539108986,122.642492380833)) ;
#23473 = CARTESIAN_POINT('Ctrl Pts',(-20.5700735002195,36.2576648305357,122.450169309994)) ;
#23474 = CARTESIAN_POINT('Ctrl Pts',(-20.4558677797191,36.4475059953039,122.812743968213)) ;
#23475 = CARTESIAN_POINT('Ctrl Pts',(-20.7175254012894,36.267516914941,122.662985785925)) ;
#23476 = CARTESIAN_POINT('Ctrl Pts',(-20.5439760773838,36.457496892047,123.003382833653)) ;
#23477 = CARTESIAN_POINT('Ctrl Pts',(-20.827658912847,36.2775078116842,122.901285416374)) ;
#23478 = CARTESIAN_POINT('Ctrl Pts',(-20.5973974591388,36.467414883948,123.20495630849)) ;
#23479 = CARTESIAN_POINT('Ctrl Pts',(-20.894433698142,36.2874258035851,123.153253367672)) ;
#23480 = CARTESIAN_POINT('Ctrl Pts',(-20.6152498950623,36.477442999405,123.415005149614)) ;
#23481 = CARTESIAN_POINT('Ctrl Pts',(-20.9167470714456,36.2974539190421,123.415814568147)) ;
#23482 = CARTESIAN_POINT('Ctrl Pts',(-20.5967150299844,36.4873281753471,123.621999291059)) ;
#23483 = CARTESIAN_POINT('Ctrl Pts',(-20.8935762347595,36.3073390949842,123.674557784478)) ;
#23484 = CARTESIAN_POINT('Ctrl Pts',(-20.5424427129043,36.497317533754,123.824877571005)) ;
#23485 = CARTESIAN_POINT('Ctrl Pts',(-20.8257335492576,36.3173284533911,123.928155184694)) ;
#23486 = CARTESIAN_POINT('Ctrl Pts',(-20.4529063543909,36.5073586813343,124.016044649924)) ;
#23487 = CARTESIAN_POINT('Ctrl Pts',(-20.7138111338408,36.3273696009714,124.167113009814)) ;
#23488 = CARTESIAN_POINT('Ctrl Pts',(-20.3343398025796,36.5171913043407,124.185369576253)) ;
#23489 = CARTESIAN_POINT('Ctrl Pts',(-20.5656005075822,36.3372022239778,124.378768633685)) ;
#23490 = CARTESIAN_POINT('Ctrl Pts',(-20.1861956020173,36.5271853754515,124.334353336419)) ;
#23491 = CARTESIAN_POINT('Ctrl Pts',(-20.3804184420739,36.3471962950886,124.564996698335)) ;
#23492 = CARTESIAN_POINT('Ctrl Pts',(-20.013585956424,36.5372140330923,124.455438892729)) ;
#23493 = CARTESIAN_POINT('Ctrl Pts',(-20.1646550508293,36.3572249527295,124.716351716207)) ;
#23494 = CARTESIAN_POINT('Ctrl Pts',(-19.8254390215131,36.5470983592851,124.543627316343)) ;
#23495 = CARTESIAN_POINT('Ctrl Pts',(-19.9294697798766,36.3671092789223,124.82658534845)) ;
#23496 = CARTESIAN_POINT('Ctrl Pts',(-19.6233034874049,36.5570641027758,124.598757212987)) ;
#23497 = CARTESIAN_POINT('Ctrl Pts',(-19.6767994745705,36.3770750224129,124.895495364823)) ;
#23498 = CARTESIAN_POINT('Ctrl Pts',(-19.4133432163963,36.567092481907,124.617767958151)) ;
#23499 = CARTESIAN_POINT('Ctrl Pts',(-19.4143489319624,36.3871034015441,124.91925636217)) ;
#23500 = CARTESIAN_POINT('Ctrl Pts',(-19.2058808015427,36.5769933281139,124.600571301318)) ;
#23501 = CARTESIAN_POINT('Ctrl Pts',(-19.1550206095445,36.397004247751,124.897758003346)) ;
#23502 = CARTESIAN_POINT('Ctrl Pts',(-19.0014191299385,36.587051985531,124.546729537717)) ;
#23503 = CARTESIAN_POINT('Ctrl Pts',(-18.8994442732755,36.4070629051681,124.830453416065)) ;
#23504 = CARTESIAN_POINT('Ctrl Pts',(-18.813096638073,36.5969095483129,124.460143866391)) ;
#23505 = CARTESIAN_POINT('Ctrl Pts',(-18.6640416210879,36.41692046795,124.722218749263)) ;
#23506 = CARTESIAN_POINT('Ctrl Pts',(-18.6390013358373,36.6069779508661,124.339804591474)) ;
#23507 = CARTESIAN_POINT('Ctrl Pts',(-18.4464240794683,36.4269888705032,124.571792635111)) ;
#23508 = CARTESIAN_POINT('Ctrl Pts',(-18.4916105941839,36.6168333496057,124.194162637956)) ;
#23509 = CARTESIAN_POINT('Ctrl Pts',(-18.2621870024575,36.4368442692428,124.389737932051)) ;
#23510 = CARTESIAN_POINT('Ctrl Pts',(-18.3695504756262,36.6268282166796,124.023135375574)) ;
#23511 = CARTESIAN_POINT('Ctrl Pts',(-18.1096139658518,36.4468391363167,124.175952224907)) ;
#23512 = CARTESIAN_POINT('Ctrl Pts',(-18.2791165716848,36.636859511663,123.832615497264)) ;
#23513 = CARTESIAN_POINT('Ctrl Pts',(-17.9965739248701,36.4568704313002,123.937801266144)) ;
#23514 = CARTESIAN_POINT('Ctrl Pts',(-18.2237360833858,36.6467260363896,123.632712396887)) ;
#23515 = CARTESIAN_POINT('Ctrl Pts',(-17.9273507223424,36.4667369560267,123.68792118455)) ;
#23516 = CARTESIAN_POINT('Ctrl Pts',(-18.2033310226805,36.6567135070853,123.423763661605)) ;
#23517 = CARTESIAN_POINT('Ctrl Pts',(-17.9018470654154,36.4767244267224,123.426734881173)) ;
#23518 = CARTESIAN_POINT('Ctrl Pts',(-18.2193352845113,36.6666582666492,123.215274762374)) ;
#23519 = CARTESIAN_POINT('Ctrl Pts',(-17.9218551058738,36.4866691862863,123.166123729046)) ;
#23520 = CARTESIAN_POINT('Ctrl Pts',(-18.2719370323567,36.676703822598,123.010765439361)) ;
#23521 = CARTESIAN_POINT('Ctrl Pts',(-17.9876098911621,36.4967147422351,122.910487765929)) ;
#23522 = CARTESIAN_POINT('Ctrl Pts',(-18.3574522060071,36.6865634109731,122.82192143973)) ;
#23523 = CARTESIAN_POINT('Ctrl Pts',(-18.0945065089563,36.5065743306102,122.674433491217)) ;
#23524 = CARTESIAN_POINT('Ctrl Pts',(-18.4758403465642,36.6965643661092,122.648211025078)) ;
#23525 = CARTESIAN_POINT('Ctrl Pts',(-18.2424940102238,36.5165752857463,122.457296954355)) ;
#23526 = CARTESIAN_POINT('Ctrl Pts',(-18.6211027599908,36.7064685933867,122.49899007134)) ;
#23527 = CARTESIAN_POINT('Ctrl Pts',(-18.4240741922966,36.5264795130239,122.270772500049)) ;
#23528 = CARTESIAN_POINT('Ctrl Pts',(-18.7923364863628,36.7165106702819,122.37555164078)) ;
#23529 = CARTESIAN_POINT('Ctrl Pts',(-18.6381179777294,36.536521589919,122.116476705951)) ;
#23530 = CARTESIAN_POINT('Ctrl Pts',(-18.9798717838469,36.726418282968,122.28482859885)) ;
#23531 = CARTESIAN_POINT('Ctrl Pts',(-18.8725385168482,36.5464292026052,122.003075302597)) ;
#23532 = CARTESIAN_POINT('Ctrl Pts',(-19.1832128493394,36.7364728135838,122.227207958605)) ;
#23533 = CARTESIAN_POINT('Ctrl Pts',(-19.1267156102874,36.5564837332209,121.931052177972)) ;
#23534 = CARTESIAN_POINT('Ctrl Pts',(-19.3894625931079,36.7463336001326,122.206055828831)) ;
#23535 = CARTESIAN_POINT('Ctrl Pts',(-19.3845283469667,36.5663445197698,121.904614760594)) ;
#23536 = CARTESIAN_POINT('Ctrl Pts',(-19.5990077419193,36.7563273552037,122.220846428092)) ;
#23537 = CARTESIAN_POINT('Ctrl Pts',(-19.646459660601,36.5763382748409,121.923105823683)) ;
#23538 = CARTESIAN_POINT('Ctrl Pts',(-19.8014959540694,36.7662527154437,122.271364787942)) ;
#23539 = CARTESIAN_POINT('Ctrl Pts',(-19.8995693751158,36.5862636350808,121.986256533974)) ;
#23540 = CARTESIAN_POINT('Ctrl Pts',(-19.9940544316431,36.776280644839,122.357120402506)) ;
#23541 = CARTESIAN_POINT('Ctrl Pts',(-20.1402663825485,36.5962915644761,122.093453651258)) ;
#23542 = CARTESIAN_POINT('Ctrl Pts',(-20.1664982335649,36.7861669116383,122.473197134529)) ;
#23543 = CARTESIAN_POINT('Ctrl Pts',(-20.3558196617263,36.6061778312754,122.23855197328)) ;
#23544 = CARTESIAN_POINT('Ctrl Pts',(-20.3183982755101,36.7961986805365,122.619450743956)) ;
#23545 = CARTESIAN_POINT('Ctrl Pts',(-20.5456928031172,36.6162096001737,122.421371062193)) ;
#23546 = CARTESIAN_POINT('Ctrl Pts',(-20.4409436536401,36.8060802763801,122.787245264454)) ;
#23547 = CARTESIAN_POINT('Ctrl Pts',(-20.6988722845905,36.6260911960173,122.631115950227)) ;
#23548 = CARTESIAN_POINT('Ctrl Pts',(-20.5341804059787,36.8161421618481,122.977086052336)) ;
#23549 = CARTESIAN_POINT('Ctrl Pts',(-20.815415738362,36.6361530814852,122.868418182703)) ;
#23550 = CARTESIAN_POINT('Ctrl Pts',(-20.5919244424178,36.825999595867,123.176140531021)) ;
#23551 = CARTESIAN_POINT('Ctrl Pts',(-20.8875930298801,36.6460105155041,123.11723735423)) ;
#23552 = CARTESIAN_POINT('Ctrl Pts',(-20.6149712049277,36.8359928389089,123.384935530242)) ;
#23553 = CARTESIAN_POINT('Ctrl Pts',(-20.9163988743177,36.6560037585461,123.37823043788)) ;
#23554 = CARTESIAN_POINT('Ctrl Pts',(-20.6015124206239,36.8459235997953,123.593287168939)) ;
#23555 = CARTESIAN_POINT('Ctrl Pts',(-20.8995719078508,36.6659345194324,123.638673612031)) ;
#23556 = CARTESIAN_POINT('Ctrl Pts',(-20.5353308402502,36.8592725919925,123.866051377186)) ;
#23557 = CARTESIAN_POINT('Ctrl Pts',(-20.8168446966216,36.6792835116296,123.979609103864)) ;
#23558 = CARTESIAN_POINT('Ctrl Pts',(-20.3999609319661,36.8725409648089,124.11357862058)) ;
#23559 = CARTESIAN_POINT('Ctrl Pts',(-20.6476556408436,36.692551884446,124.288994177467)) ;
#23560 = CARTESIAN_POINT('Ctrl Pts',(-20.2075188150344,36.8858239061933,124.315902403528)) ;
#23561 = CARTESIAN_POINT('Ctrl Pts',(-20.4070652076398,36.7058348258304,124.541941671544)) ;
#23562 = CARTESIAN_POINT('Ctrl Pts',(-20.0375727801162,36.8958666920355,124.441171046121)) ;
#23563 = CARTESIAN_POINT('Ctrl Pts',(-20.1946380684897,36.7158776116726,124.698516250031)) ;
#23564 = CARTESIAN_POINT('Ctrl Pts',(-19.8521787979742,36.9057166345876,124.533432305183)) ;
#23565 = CARTESIAN_POINT('Ctrl Pts',(-19.9628921814832,36.7257275542247,124.813842499232)) ;
#23566 = CARTESIAN_POINT('Ctrl Pts',(-19.6507731123258,36.9157138675065,124.593480412264)) ;
#23567 = CARTESIAN_POINT('Ctrl Pts',(-19.7111366687982,36.7357247871437,124.888900023742)) ;
#23568 = CARTESIAN_POINT('Ctrl Pts',(-19.4415809415258,36.9257287628411,124.617367629168)) ;
#23569 = CARTESIAN_POINT('Ctrl Pts',(-19.4496388355441,36.7457396824782,124.918754107173)) ;
#23570 = CARTESIAN_POINT('Ctrl Pts',(-19.1637149095619,36.9389684394793,124.600711262707)) ;
#23571 = CARTESIAN_POINT('Ctrl Pts',(-19.1023419164485,36.7589793591164,124.897941856105)) ;
#23572 = CARTESIAN_POINT('Ctrl Pts',(-18.8297170296114,36.9555156638846,124.490312279794)) ;
#23573 = CARTESIAN_POINT('Ctrl Pts',(-18.6847931249913,36.7755265835217,124.759912521952)) ;
#23574 = CARTESIAN_POINT('Ctrl Pts',(-18.5515569849989,36.9721631010157,124.271299498721)) ;
#23575 = CARTESIAN_POINT('Ctrl Pts',(-18.3371603330514,36.7921740206528,124.486198909286)) ;
#23576 = CARTESIAN_POINT('Ctrl Pts',(-18.3844875359923,36.9854525984939,124.047410122767)) ;
#23577 = CARTESIAN_POINT('Ctrl Pts',(-18.1282776888068,36.805463518131,124.206288377136)) ;
#23578 = CARTESIAN_POINT('Ctrl Pts',(-18.2905524045651,36.9953260063163,123.862298699992)) ;
#23579 = CARTESIAN_POINT('Ctrl Pts',(-18.0108710102114,36.8153369259534,123.974907927257)) ;
#23580 = CARTESIAN_POINT('Ctrl Pts',(-18.2290667315247,37.005378383909,123.660120832007)) ;
#23581 = CARTESIAN_POINT('Ctrl Pts',(-17.9340138084422,36.8253893035461,123.722181735766)) ;
#23582 = CARTESIAN_POINT('Ctrl Pts',(-18.2040801154488,37.0152820374499,123.45340205248)) ;
#23583 = CARTESIAN_POINT('Ctrl Pts',(-17.9027830695279,36.835292957087,123.463785283055)) ;
#23584 = CARTESIAN_POINT('Ctrl Pts',(-18.214904553946,37.0252263064452,123.244652571559)) ;
#23585 = CARTESIAN_POINT('Ctrl Pts',(-17.9163185741068,36.8452372260823,123.20284412538)) ;
#23586 = CARTESIAN_POINT('Ctrl Pts',(-18.2776834319682,37.0385573147779,122.97143393021)) ;
#23587 = CARTESIAN_POINT('Ctrl Pts',(-17.9947816309639,36.858568234415,122.86134409118)) ;
#23588 = CARTESIAN_POINT('Ctrl Pts',(-18.4435275534842,37.0551788953021,122.659444683358)) ;
#23589 = CARTESIAN_POINT('Ctrl Pts',(-18.2021201495934,36.8751898149393,122.471324046481)) ;
#23590 = CARTESIAN_POINT('Ctrl Pts',(-18.704290384894,37.0717215660005,122.423272162924)) ;
#23591 = CARTESIAN_POINT('Ctrl Pts',(-18.5280140338344,36.8917324856377,122.176159129624)) ;
#23592 = CARTESIAN_POINT('Ctrl Pts',(-18.9539020590981,37.0850707255635,122.295120923871)) ;
#23593 = CARTESIAN_POINT('Ctrl Pts',(-18.8400831149496,36.9050816452006,122.015936356967)) ;
#23594 = CARTESIAN_POINT('Ctrl Pts',(-19.2195445907984,37.098298875723,122.212649877143)) ;
#23595 = CARTESIAN_POINT('Ctrl Pts',(-19.1721122727388,36.9183097953601,121.912858361427)) ;
#23596 = CARTESIAN_POINT('Ctrl Pts',(-19.5728022237674,37.1149295528605,122.198387297674)) ;
#23597 = CARTESIAN_POINT('Ctrl Pts',(-19.6137036972869,36.9349404724976,121.895030598863)) ;
#23598 = CARTESIAN_POINT('Ctrl Pts',(-19.9761409789066,37.1348324921486,122.326670598827)) ;
#23599 = CARTESIAN_POINT('Ctrl Pts',(-20.1178689307979,36.9548434117857,122.055389405996)) ;
#23600 = CARTESIAN_POINT('Ctrl Pts',(-20.3116476022959,37.1547353587518,122.584460179412)) ;
#23601 = CARTESIAN_POINT('Ctrl Pts',(-20.5372508618261,36.974746278389,122.377628584719)) ;
#23602 = CARTESIAN_POINT('Ctrl Pts',(-20.539804233534,37.1746485238567,122.941249904607)) ;
#23603 = CARTESIAN_POINT('Ctrl Pts',(-20.8224429652518,36.9946594434938,122.823616943194)) ;
#23604 = CARTESIAN_POINT('Ctrl Pts',(-20.6323994014347,37.194684352998,123.35701958835)) ;
#23605 = CARTESIAN_POINT('Ctrl Pts',(-20.9381837029395,37.0146952726351,123.343330198138)) ;
#23606 = CARTESIAN_POINT('Ctrl Pts',(-20.5783831690263,37.2145029278761,123.775043446031)) ;
#23607 = CARTESIAN_POINT('Ctrl Pts',(-20.870660430698,37.0345138475132,123.865857791706)) ;
#23608 = CARTESIAN_POINT('Ctrl Pts',(-20.3841900567002,37.2344732289181,124.152499639715)) ;
#23609 = CARTESIAN_POINT('Ctrl Pts',(-20.6279168053025,37.0544841485552,124.337676429547)) ;
#23610 = CARTESIAN_POINT('Ctrl Pts',(-20.0739514395831,37.2543647612826,124.440192864302)) ;
#23611 = CARTESIAN_POINT('Ctrl Pts',(-20.2401177850533,37.0743756809197,124.697290350133)) ;
#23612 = CARTESIAN_POINT('Ctrl Pts',(-19.6816910451499,37.2743878590991,124.605446609559)) ;
#23613 = CARTESIAN_POINT('Ctrl Pts',(-19.7497910668488,37.0943987787363,124.90385539926)) ;
#23614 = CARTESIAN_POINT('Ctrl Pts',(-19.2612575086077,37.2941846120191,124.626987367423)) ;
#23615 = CARTESIAN_POINT('Ctrl Pts',(-19.2242516782472,37.1141955316562,124.930779156354)) ;
#23616 = CARTESIAN_POINT('Ctrl Pts',(-18.8551235164096,37.3141457005079,124.503854762639)) ;
#23617 = CARTESIAN_POINT('Ctrl Pts',(-18.7165851062784,37.134156620145,124.77686253658)) ;
#23618 = CARTESIAN_POINT('Ctrl Pts',(-18.5155691321444,37.33412396944,124.248549659237)) ;
#23619 = CARTESIAN_POINT('Ctrl Pts',(-18.2921431805836,37.1541348890772,124.457730120068)) ;
#23620 = CARTESIAN_POINT('Ctrl Pts',(-18.2848840893229,37.353943984231,123.895912818502)) ;
#23621 = CARTESIAN_POINT('Ctrl Pts',(-18.0037890981737,37.1739549038682,124.016935959716)) ;
#23622 = CARTESIAN_POINT('Ctrl Pts',(-18.1867266757181,37.3738823934829,123.483465881593)) ;
#23623 = CARTESIAN_POINT('Ctrl Pts',(-17.8810922820256,37.19389331312,123.50137832524)) ;
#23624 = CARTESIAN_POINT('Ctrl Pts',(-18.2364290835758,37.3939295108753,123.060063699983)) ;
#23625 = CARTESIAN_POINT('Ctrl Pts',(-17.9432206011059,37.2139404305124,122.97212475137)) ;
#23626 = CARTESIAN_POINT('Ctrl Pts',(-18.425848548575,37.4137757567091,122.683031202947)) ;
#23627 = CARTESIAN_POINT('Ctrl Pts',(-18.1799938362226,37.2337866763463,122.500836491877)) ;
#23628 = CARTESIAN_POINT('Ctrl Pts',(-18.7315064002048,37.4336247252212,122.391977885503)) ;
#23629 = CARTESIAN_POINT('Ctrl Pts',(-18.5620635941251,37.2536356448583,122.137020325925)) ;
#23630 = CARTESIAN_POINT('Ctrl Pts',(-19.1222176535589,37.4536750275325,122.221508253603)) ;
#23631 = CARTESIAN_POINT('Ctrl Pts',(-19.0504528465872,37.2736859471696,121.923931865139)) ;
#23632 = CARTESIAN_POINT('Ctrl Pts',(-19.5432296563708,37.4735099499637,122.194969642124)) ;
#23633 = CARTESIAN_POINT('Ctrl Pts',(-19.5767155011093,37.2935208696008,121.890757346003)) ;
#23634 = CARTESIAN_POINT('Ctrl Pts',(-19.9499494548822,37.4934403511896,122.313396694246)) ;
#23635 = CARTESIAN_POINT('Ctrl Pts',(-20.08511494409,37.3134512708267,122.038788804448)) ;
#23636 = CARTESIAN_POINT('Ctrl Pts',(-20.2916433860762,37.5133252965484,122.562694249305)) ;
#23637 = CARTESIAN_POINT('Ctrl Pts',(-20.5122328950149,37.3333362161856,122.35040788788)) ;
#23638 = CARTESIAN_POINT('Ctrl Pts',(-20.5292680047328,37.5333979046998,122.917125700607)) ;
#23639 = CARTESIAN_POINT('Ctrl Pts',(-20.8092661802658,37.353408824337,122.793446550335)) ;
#23640 = CARTESIAN_POINT('Ctrl Pts',(-20.6303478789093,37.5531892210279,123.325688691572)) ;
#23641 = CARTESIAN_POINT('Ctrl Pts',(-20.9356180404718,37.3732001406651,123.304147384377)) ;
#23642 = CARTESIAN_POINT('Ctrl Pts',(-20.5868633210281,37.5731540107952,123.747925395275)) ;
#23643 = CARTESIAN_POINT('Ctrl Pts',(-20.8812658706226,37.3931649304323,123.8319433124)) ;
#23644 = CARTESIAN_POINT('Ctrl Pts',(-20.400758322157,37.5931369665455,124.129898349839)) ;
#23645 = CARTESIAN_POINT('Ctrl Pts',(-20.6486375255731,37.4131478861826,124.309410738548)) ;
#23646 = CARTESIAN_POINT('Ctrl Pts',(-20.0987238949301,37.6129454885216,124.423499457933)) ;
#23647 = CARTESIAN_POINT('Ctrl Pts',(-20.2710983170399,37.4329564081588,124.676413569009)) ;
#23648 = CARTESIAN_POINT('Ctrl Pts',(-19.7115115108839,37.6329310632575,124.598340112043)) ;
#23649 = CARTESIAN_POINT('Ctrl Pts',(-19.7870846025984,37.4529419828946,124.894968051368)) ;
#23650 = CARTESIAN_POINT('Ctrl Pts',(-19.2898630183284,37.6528137033259,124.630311193854)) ;
#23651 = CARTESIAN_POINT('Ctrl Pts',(-19.2600251516879,37.472824622963,124.934935958172)) ;
#23652 = CARTESIAN_POINT('Ctrl Pts',(-18.8812143689227,37.6727690154578,124.516434264361)) ;
#23653 = CARTESIAN_POINT('Ctrl Pts',(-18.7492134555832,37.4927799350949,124.792594096249)) ;
#23654 = CARTESIAN_POINT('Ctrl Pts',(-18.5370718720123,37.6926433720656,124.271071448135)) ;
#23655 = CARTESIAN_POINT('Ctrl Pts',(-18.319033254551,37.5126542917027,124.485894779788)) ;
#23656 = CARTESIAN_POINT('Ctrl Pts',(-18.295856749821,37.7126255789266,123.921365626854)) ;
#23657 = CARTESIAN_POINT('Ctrl Pts',(-18.0175106060064,37.5326364985638,124.048765115388)) ;
#23658 = CARTESIAN_POINT('Ctrl Pts',(-18.1889170459794,37.7325566568766,123.511199159604)) ;
#23659 = CARTESIAN_POINT('Ctrl Pts',(-17.8838308617942,37.5525675765137,123.536059048149)) ;
#23660 = CARTESIAN_POINT('Ctrl Pts',(-18.2282802535352,37.7524836317316,123.089417927906)) ;
#23661 = CARTESIAN_POINT('Ctrl Pts',(-17.9330320754365,37.5724945513687,123.008830582015)) ;
#23662 = CARTESIAN_POINT('Ctrl Pts',(-18.4076686429173,37.7723160906805,122.707716966432)) ;
#23663 = CARTESIAN_POINT('Ctrl Pts',(-18.157254622848,37.5923270103176,122.531709623646)) ;
#23664 = CARTESIAN_POINT('Ctrl Pts',(-18.6583803627313,37.7889737748557,122.457695839393)) ;
#23665 = CARTESIAN_POINT('Ctrl Pts',(-18.4706659458096,37.6089846944928,122.219158784054)) ;
#23666 = CARTESIAN_POINT('Ctrl Pts',(-18.8998510224225,37.8022229987628,122.318670298478)) ;
#23667 = CARTESIAN_POINT('Ctrl Pts',(-18.7724796762074,37.6222339183999,122.045392670349)) ;
#23668 = CARTESIAN_POINT('Ctrl Pts',(-19.0983967328829,37.812272020214,122.246576703272)) ;
#23669 = CARTESIAN_POINT('Ctrl Pts',(-19.0206690089167,37.6322829398511,121.955269929733)) ;
#23670 = CARTESIAN_POINT('Ctrl Pts',(-19.3025665370279,37.8221320284445,122.210682156202)) ;
#23671 = CARTESIAN_POINT('Ctrl Pts',(-19.2758657649021,37.6421429480816,121.910397904174)) ;
#23672 = CARTESIAN_POINT('Ctrl Pts',(-19.5818034711638,37.8354155416691,122.209888694931)) ;
#23673 = CARTESIAN_POINT('Ctrl Pts',(-19.6249794284296,37.6554264613062,121.909413584284)) ;
#23674 = CARTESIAN_POINT('Ctrl Pts',(-19.9238580353541,37.8520614606699,122.300927522182)) ;
#23675 = CARTESIAN_POINT('Ctrl Pts',(-20.0524638778648,37.672072380307,122.023188295616)) ;
#23676 = CARTESIAN_POINT('Ctrl Pts',(-20.2129442647701,37.868615438486,122.501691868279)) ;
#23677 = CARTESIAN_POINT('Ctrl Pts',(-20.413880776944,37.6886263581231,122.274169668414)) ;
#23678 = CARTESIAN_POINT('Ctrl Pts',(-20.3943636779236,37.8819751674576,122.716138212852)) ;
#23679 = CARTESIAN_POINT('Ctrl Pts',(-20.6406243713132,37.7019860870947,122.542201540504)) ;
#23680 = CARTESIAN_POINT('Ctrl Pts',(-20.4992200878676,37.8918682192543,122.895764414402)) ;
#23681 = CARTESIAN_POINT('Ctrl Pts',(-20.771703979078,37.7118791388914,122.766737576687)) ;
#23682 = CARTESIAN_POINT('Ctrl Pts',(-20.5722587350757,37.9018581845353,123.092651468805)) ;
#23683 = CARTESIAN_POINT('Ctrl Pts',(-20.8630031282262,37.7218691041725,123.012844193469)) ;
#23684 = CARTESIAN_POINT('Ctrl Pts',(-20.6099889776979,37.9118100653962,123.298474001835)) ;
#23685 = CARTESIAN_POINT('Ctrl Pts',(-20.9101691765086,37.7318209850333,123.270122215449)) ;
#23686 = CARTESIAN_POINT('Ctrl Pts',(-20.6112435236213,37.921858417088,123.509695858603)) ;
#23687 = CARTESIAN_POINT('Ctrl Pts',(-20.9117400295103,37.7418693367251,123.534149528085)) ;
#23688 = CARTESIAN_POINT('Ctrl Pts',(-20.5767689441837,37.9316997011942,123.713719442)) ;
#23689 = CARTESIAN_POINT('Ctrl Pts',(-20.8686496157947,37.7517106208313,123.789179451331)) ;
#23690 = CARTESIAN_POINT('Ctrl Pts',(-20.5068028273446,37.9416864043198,123.911631328625)) ;
#23691 = CARTESIAN_POINT('Ctrl Pts',(-20.7811945958756,37.761697323957,124.0365703206)) ;
#23692 = CARTESIAN_POINT('Ctrl Pts',(-20.4041443174755,37.9516214331373,124.093573751061)) ;
#23693 = CARTESIAN_POINT('Ctrl Pts',(-20.6528738763807,37.7716323527744,124.263999794878)) ;
#23694 = CARTESIAN_POINT('Ctrl Pts',(-20.2697516088806,37.9616772280442,124.256720400925)) ;
#23695 = CARTESIAN_POINT('Ctrl Pts',(-20.4848851322175,37.7816881476813,124.467934944113)) ;
#23696 = CARTESIAN_POINT('Ctrl Pts',(-20.112868940614,37.9715055913335,124.391230410189)) ;
#23697 = CARTESIAN_POINT('Ctrl Pts',(-20.2887835292672,37.7915165109706,124.636074676787)) ;
#23698 = CARTESIAN_POINT('Ctrl Pts',(-19.9310077930652,37.9815665612314,124.499176168369)) ;
#23699 = CARTESIAN_POINT('Ctrl Pts',(-20.0614584855971,37.8015774808685,124.771009318032)) ;
#23700 = CARTESIAN_POINT('Ctrl Pts',(-19.7359423603849,37.9914808401212,124.572672275179)) ;
#23701 = CARTESIAN_POINT('Ctrl Pts',(-19.8176275658583,37.8114917597583,124.862882128275)) ;
#23702 = CARTESIAN_POINT('Ctrl Pts',(-19.5292180654532,38.0014898345894,124.611953243679)) ;
#23703 = CARTESIAN_POINT('Ctrl Pts',(-19.5592226441299,37.8215007542265,124.911986102219)) ;
#23704 = CARTESIAN_POINT('Ctrl Pts',(-19.3183758075429,38.0115196691532,124.614317888065)) ;
#23705 = CARTESIAN_POINT('Ctrl Pts',(-19.2956698137528,37.8315305887903,124.914944725245)) ;
#23706 = CARTESIAN_POINT('Ctrl Pts',(-19.1138048120896,38.0213778992254,124.581009867866)) ;
#23707 = CARTESIAN_POINT('Ctrl Pts',(-19.0399553923332,37.8413888188625,124.873312424771)) ;
#23708 = CARTESIAN_POINT('Ctrl Pts',(-18.9152985830758,38.0313766049678,124.51196923972)) ;
#23709 = CARTESIAN_POINT('Ctrl Pts',(-18.7918216048471,37.8513875246049,124.787014243601)) ;
#23710 = CARTESIAN_POINT('Ctrl Pts',(-18.7335213440721,38.0412712608866,124.410757402581)) ;
#23711 = CARTESIAN_POINT('Ctrl Pts',(-18.5645984860679,37.8612821805237,124.660501733372)) ;
#23712 = CARTESIAN_POINT('Ctrl Pts',(-18.5694307222782,38.0513343252705,124.27728255479)) ;
#23713 = CARTESIAN_POINT('Ctrl Pts',(-18.3594834848053,37.8713452449077,124.493660346681)) ;
#23714 = CARTESIAN_POINT('Ctrl Pts',(-18.4338627813113,38.0611739835504,124.120992090027)) ;
#23715 = CARTESIAN_POINT('Ctrl Pts',(-18.1900212161876,37.8811849031876,124.298298757576)) ;
#23716 = CARTESIAN_POINT('Ctrl Pts',(-18.3248772146404,38.0712371506323,123.939698712811)) ;
#23717 = CARTESIAN_POINT('Ctrl Pts',(-18.0537869453756,37.8912480702694,124.071683477115)) ;
#23718 = CARTESIAN_POINT('Ctrl Pts',(-18.2504447417178,38.0811313957594,123.745439174698)) ;
#23719 = CARTESIAN_POINT('Ctrl Pts',(-17.9607436771395,37.9011423153965,123.828859729569)) ;
#23720 = CARTESIAN_POINT('Ctrl Pts',(-18.2101341066762,38.091073217364,123.54038139259)) ;
#23721 = CARTESIAN_POINT('Ctrl Pts',(-17.9103527062584,37.9110841370011,123.572537760102)) ;
#23722 = CARTESIAN_POINT('Ctrl Pts',(-18.2059368471232,38.1010757482821,123.330110491768)) ;
#23723 = CARTESIAN_POINT('Ctrl Pts',(-17.9051034699468,37.9210866679192,123.309699103469)) ;
#23724 = CARTESIAN_POINT('Ctrl Pts',(-18.238734440385,38.1111103747396,123.12172723179)) ;
#23725 = CARTESIAN_POINT('Ctrl Pts',(-17.946097783474,37.9311212943767,123.049219622139)) ;
#23726 = CARTESIAN_POINT('Ctrl Pts',(-18.305619068495,38.120955909726,122.925840042337)) ;
#23727 = CARTESIAN_POINT('Ctrl Pts',(-18.0297012300919,37.9409668293631,122.804359246479)) ;
#23728 = CARTESIAN_POINT('Ctrl Pts',(-18.4064882596098,38.130939334565,122.74180463094)) ;
#23729 = CARTESIAN_POINT('Ctrl Pts',(-18.1557855280744,37.9509502542022,122.574313582137)) ;
#23730 = CARTESIAN_POINT('Ctrl Pts',(-18.537392601509,38.1408897249301,122.578629160492)) ;
#23731 = CARTESIAN_POINT('Ctrl Pts',(-18.3194140988036,37.9609006445672,122.370342409505)) ;
#23732 = CARTESIAN_POINT('Ctrl Pts',(-18.6952097088462,38.1508873652272,122.439785210272)) ;
#23733 = CARTESIAN_POINT('Ctrl Pts',(-18.5166838775539,37.9708982848643,122.196785487703)) ;
#23734 = CARTESIAN_POINT('Ctrl Pts',(-18.8756765943063,38.1609264457904,122.330377777602)) ;
#23735 = CARTESIAN_POINT('Ctrl Pts',(-18.7422660732146,37.9809373654275,122.060023983283)) ;
#23736 = CARTESIAN_POINT('Ctrl Pts',(-19.0680799590173,38.1707525965595,122.255148656096)) ;
#23737 = CARTESIAN_POINT('Ctrl Pts',(-18.9827700674646,37.9907635161966,121.965984935098)) ;
#23738 = CARTESIAN_POINT('Ctrl Pts',(-19.2752831931946,38.1808091714886,122.213190167837)) ;
#23739 = CARTESIAN_POINT('Ctrl Pts',(-19.2417735141306,38.0008200911257,121.913534414804)) ;
#23740 = CARTESIAN_POINT('Ctrl Pts',(-19.4842136350837,38.1907497108689,122.208272468333)) ;
#23741 = CARTESIAN_POINT('Ctrl Pts',(-19.5029368385389,38.010760630506,121.907384733562)) ;
#23742 = CARTESIAN_POINT('Ctrl Pts',(-19.6901672000189,38.2006541038453,122.238947693484)) ;
#23743 = CARTESIAN_POINT('Ctrl Pts',(-19.7603796758828,38.0206650234824,121.94572645087)) ;
#23744 = CARTESIAN_POINT('Ctrl Pts',(-19.8904397603091,38.2107007580502,122.305985318567)) ;
#23745 = CARTESIAN_POINT('Ctrl Pts',(-20.0107210558662,38.0307116776873,122.029521129623)) ;
#23746 = CARTESIAN_POINT('Ctrl Pts',(-20.073374575685,38.2205963199886,122.405120062079)) ;
#23747 = CARTESIAN_POINT('Ctrl Pts',(-20.2393912303446,38.0406072396257,122.153437722029)) ;
#23748 = CARTESIAN_POINT('Ctrl Pts',(-20.239009195266,38.2306583978341,122.536650134801)) ;
#23749 = CARTESIAN_POINT('Ctrl Pts',(-20.4464358604614,38.0506693174713,122.317848314889)) ;
#23750 = CARTESIAN_POINT('Ctrl Pts',(-20.3763552173519,38.2405010962479,122.691451330782)) ;
#23751 = CARTESIAN_POINT('Ctrl Pts',(-20.6181207395519,38.060512015885,122.511348876402)) ;
#23752 = CARTESIAN_POINT('Ctrl Pts',(-20.4867630860936,38.2504918712094,122.870097720652)) ;
#23753 = CARTESIAN_POINT('Ctrl Pts',(-20.7561325943481,38.0705027908465,122.734655821582)) ;
#23754 = CARTESIAN_POINT('Ctrl Pts',(-20.5639707241842,38.2604197362285,123.064019607399)) ;
#23755 = CARTESIAN_POINT('Ctrl Pts',(-20.8526444302202,38.0804306558656,122.977057792993)) ;
#23756 = CARTESIAN_POINT('Ctrl Pts',(-20.606936524891,38.2704084809947,123.269576207478)) ;
#23757 = CARTESIAN_POINT('Ctrl Pts',(-20.9063538531691,38.0904194006318,123.234003272381)) ;
#23758 = CARTESIAN_POINT('Ctrl Pts',(-20.6132774081827,38.2804412665816,123.480405040988)) ;
#23759 = CARTESIAN_POINT('Ctrl Pts',(-20.9142822162603,38.1004521862187,123.497539173054)) ;
#23760 = CARTESIAN_POINT('Ctrl Pts',(-20.5836278378137,38.2903079512023,123.685696146507)) ;
#23761 = CARTESIAN_POINT('Ctrl Pts',(-20.8772223147212,38.1103188708394,123.754154223928)) ;
#23762 = CARTESIAN_POINT('Ctrl Pts',(-20.5187275010846,38.3002698433654,123.884820325634)) ;
#23763 = CARTESIAN_POINT('Ctrl Pts',(-20.7960987290107,38.1202807630025,124.00306041153)) ;
#23764 = CARTESIAN_POINT('Ctrl Pts',(-20.4192419119231,38.310303320278,124.070811287122)) ;
#23765 = CARTESIAN_POINT('Ctrl Pts',(-20.6717436692743,38.1303142399151,124.235550043403)) ;
#23766 = CARTESIAN_POINT('Ctrl Pts',(-20.2911476331738,38.3201876615263,124.234467456338)) ;
#23767 = CARTESIAN_POINT('Ctrl Pts',(-20.5116269403932,38.1401985811634,124.440122137364)) ;
#23768 = CARTESIAN_POINT('Ctrl Pts',(-20.1338310125617,38.3302506036474,124.375873737008)) ;
#23769 = CARTESIAN_POINT('Ctrl Pts',(-20.3149827227567,38.1502615232845,124.616881340023)) ;
#23770 = CARTESIAN_POINT('Ctrl Pts',(-19.9581597878484,38.340101005267,124.485559805927)) ;
#23771 = CARTESIAN_POINT('Ctrl Pts',(-20.0953938752767,38.1601119249041,124.75399118927)) ;
#23772 = CARTESIAN_POINT('Ctrl Pts',(-19.7628910644464,38.3501278940566,124.564952690496)) ;
#23773 = CARTESIAN_POINT('Ctrl Pts',(-19.8513087068426,38.1701388136938,124.853234002042)) ;
#23774 = CARTESIAN_POINT('Ctrl Pts',(-19.5566368100917,38.3601565090128,124.608705273283)) ;
#23775 = CARTESIAN_POINT('Ctrl Pts',(-19.593491376287,38.18016742865,124.907926696643)) ;
#23776 = CARTESIAN_POINT('Ctrl Pts',(-19.3498081641325,38.3700017321329,124.616238591243)) ;
#23777 = CARTESIAN_POINT('Ctrl Pts',(-19.3349545228551,38.19001265177,124.917345289566)) ;
#23778 = CARTESIAN_POINT('Ctrl Pts',(-19.1416901454092,38.3799924159389,124.587880295423)) ;
#23779 = CARTESIAN_POINT('Ctrl Pts',(-19.0748065717966,38.200003335576,124.88189910921)) ;
#23780 = CARTESIAN_POINT('Ctrl Pts',(-18.9408634995236,38.3900302980113,124.52306847004)) ;
#23781 = CARTESIAN_POINT('Ctrl Pts',(-18.8237728136893,38.2100412176484,124.80088615643)) ;
#23782 = CARTESIAN_POINT('Ctrl Pts',(-18.7577593662331,38.3998746576501,124.426589014127)) ;
#23783 = CARTESIAN_POINT('Ctrl Pts',(-18.5948907896328,38.2198855772873,124.680287851483)) ;
#23784 = CARTESIAN_POINT('Ctrl Pts',(-18.5916294729954,38.4098595282649,124.298321906934)) ;
#23785 = CARTESIAN_POINT('Ctrl Pts',(-18.3872272286847,38.229870447902,124.519955106578)) ;
#23786 = CARTESIAN_POINT('Ctrl Pts',(-18.4508291327248,38.4197988115935,124.14388654102)) ;
#23787 = CARTESIAN_POINT('Ctrl Pts',(-18.2112252563883,38.2398097312307,124.326911572828)) ;
#23788 = CARTESIAN_POINT('Ctrl Pts',(-18.3379263587694,38.4298394209667,123.965558708293)) ;
#23789 = CARTESIAN_POINT('Ctrl Pts',(-18.0700954992362,38.2498503406038,124.104002776353)) ;
#23790 = CARTESIAN_POINT('Ctrl Pts',(-18.2587866795904,38.4397242718799,123.77338134412)) ;
#23791 = CARTESIAN_POINT('Ctrl Pts',(-17.9711690914586,38.259735191517,123.863780801288)) ;
#23792 = CARTESIAN_POINT('Ctrl Pts',(-18.2134543934735,38.4497262280487,123.568085773831)) ;
#23793 = CARTESIAN_POINT('Ctrl Pts',(-17.9145022539865,38.2697371476858,123.607161518794)) ;
#23794 = CARTESIAN_POINT('Ctrl Pts',(-18.2043619080485,38.4596448247692,123.359731016795)) ;
#23795 = CARTESIAN_POINT('Ctrl Pts',(-17.9031351939843,38.2796557444063,123.34671741945)) ;
#23796 = CARTESIAN_POINT('Ctrl Pts',(-18.2319694185159,38.469691646845,123.150356999405)) ;
#23797 = CARTESIAN_POINT('Ctrl Pts',(-17.9376431227796,38.2897025664821,123.084999919376)) ;
#23798 = CARTESIAN_POINT('Ctrl Pts',(-18.2942537247054,38.4795659279577,122.952295745254)) ;
#23799 = CARTESIAN_POINT('Ctrl Pts',(-18.0154975116536,38.2995768475948,122.837421943665)) ;
#23800 = CARTESIAN_POINT('Ctrl Pts',(-18.3915795652772,38.4896201280023,122.764705800279)) ;
#23801 = CARTESIAN_POINT('Ctrl Pts',(-18.1371535108144,38.3096310476394,122.602934129142)) ;
#23802 = CARTESIAN_POINT('Ctrl Pts',(-18.517948341089,38.4995155576375,122.599403244728)) ;
#23803 = CARTESIAN_POINT('Ctrl Pts',(-18.2951140075871,38.3195264772746,122.396304412918)) ;
#23804 = CARTESIAN_POINT('Ctrl Pts',(-18.6735897291934,38.5095771859549,122.456195028724)) ;
#23805 = CARTESIAN_POINT('Ctrl Pts',(-18.489664634007,38.329588105592,122.217293421697)) ;
#23806 = CARTESIAN_POINT('Ctrl Pts',(-18.8479034008404,38.5194218147848,122.344605396143)) ;
#23807 = CARTESIAN_POINT('Ctrl Pts',(-18.7075571482892,38.3394327344219,122.077804596519)) ;
#23808 = CARTESIAN_POINT('Ctrl Pts',(-19.0408840506454,38.5293818623904,122.263352848004)) ;
#23809 = CARTESIAN_POINT('Ctrl Pts',(-18.9487829946581,38.3493927820275,121.976237815657)) ;
#23810 = CARTESIAN_POINT('Ctrl Pts',(-19.2467307026046,38.5394201685644,122.216882947286)) ;
#23811 = CARTESIAN_POINT('Ctrl Pts',(-19.2060908983608,38.3594310882016,121.918149353435)) ;
#23812 = CARTESIAN_POINT('Ctrl Pts',(-19.4540764654965,38.5492934679971,122.206624033393)) ;
#23813 = CARTESIAN_POINT('Ctrl Pts',(-19.4652741750424,38.3693043876342,121.905324657195)) ;
#23814 = CARTESIAN_POINT('Ctrl Pts',(-19.6641424754752,38.5593667295834,122.233106532609)) ;
#23815 = CARTESIAN_POINT('Ctrl Pts',(-19.7278563927704,38.3793776492205,121.938426707961)) ;
#23816 = CARTESIAN_POINT('Ctrl Pts',(-19.8615036156616,38.5691869555401,122.293853612687)) ;
#23817 = CARTESIAN_POINT('Ctrl Pts',(-19.9745595742938,38.3891978751772,122.014360134831)) ;
#23818 = CARTESIAN_POINT('Ctrl Pts',(-20.0501587943975,38.5792660194796,122.390213788691)) ;
#23819 = CARTESIAN_POINT('Ctrl Pts',(-20.2103785146625,38.3992769391167,122.134809378916)) ;
#23820 = CARTESIAN_POINT('Ctrl Pts',(-20.2155221291384,38.5891161094994,122.514954133078)) ;
#23821 = CARTESIAN_POINT('Ctrl Pts',(-20.4170842341087,38.4091270291365,122.29073495999)) ;
#23822 = CARTESIAN_POINT('Ctrl Pts',(-20.3599977542973,38.5991948631132,122.669874910187)) ;
#23823 = CARTESIAN_POINT('Ctrl Pts',(-20.5976790049717,38.4192057827503,122.484385049267)) ;
#23824 = CARTESIAN_POINT('Ctrl Pts',(-20.4726208048676,38.6090163303726,122.842988026387)) ;
#23825 = CARTESIAN_POINT('Ctrl Pts',(-20.7384592821363,38.4290272500098,122.700777392782)) ;
#23826 = CARTESIAN_POINT('Ctrl Pts',(-20.5557471903728,38.6190819287303,123.037535696826)) ;
#23827 = CARTESIAN_POINT('Ctrl Pts',(-20.8423676549778,38.4390928483674,122.943961403778)) ;
#23828 = CARTESIAN_POINT('Ctrl Pts',(-20.6030203243983,38.628984584505,123.240335099083)) ;
#23829 = CARTESIAN_POINT('Ctrl Pts',(-20.9014598751906,38.4489955041421,123.197461404665)) ;
#23830 = CARTESIAN_POINT('Ctrl Pts',(-20.6145926696744,38.6390354103346,123.451275235179)) ;
#23831 = CARTESIAN_POINT('Ctrl Pts',(-20.9159258761711,38.4590463299717,123.461136272486)) ;
#23832 = CARTESIAN_POINT('Ctrl Pts',(-20.5899961792857,38.6489096146735,123.657445196275)) ;
#23833 = CARTESIAN_POINT('Ctrl Pts',(-20.8851806308957,38.4689205343106,123.718849938155)) ;
#23834 = CARTESIAN_POINT('Ctrl Pts',(-20.5288093864204,38.6589820647126,123.860120703039)) ;
#23835 = CARTESIAN_POINT('Ctrl Pts',(-20.808697747039,38.4789929843497,123.972194060034)) ;
#23836 = CARTESIAN_POINT('Ctrl Pts',(-20.4358076287803,38.6688110814861,124.044689523101)) ;
#23837 = CARTESIAN_POINT('Ctrl Pts',(-20.6924452330028,38.4888220011232,124.202906653744)) ;
#23838 = CARTESIAN_POINT('Ctrl Pts',(-20.3094581014981,38.6788779274009,124.214427563999)) ;
#23839 = CARTESIAN_POINT('Ctrl Pts',(-20.5345088117265,38.498888847038,124.415079071641)) ;
#23840 = CARTESIAN_POINT('Ctrl Pts',(-20.1581204946843,38.6887680987027,124.357044093307)) ;
#23841 = CARTESIAN_POINT('Ctrl Pts',(-20.3453362910282,38.5087790183398,124.593350718177)) ;
#23842 = CARTESIAN_POINT('Ctrl Pts',(-19.9828118483022,38.6987602923265,124.472759650499)) ;
#23843 = CARTESIAN_POINT('Ctrl Pts',(-20.1262004053155,38.5187712119636,124.737995435515)) ;
#23844 = CARTESIAN_POINT('Ctrl Pts',(-19.7905552310231,38.7087231029499,124.555852659848)) ;
#23845 = CARTESIAN_POINT('Ctrl Pts',(-19.8858793197356,38.5287340225871,124.841862120209)) ;
#23846 = CARTESIAN_POINT('Ctrl Pts',(-19.5880898351678,38.7186273757934,124.604536143381)) ;
#23847 = CARTESIAN_POINT('Ctrl Pts',(-19.6327966736522,38.5386382954305,124.9027167446)) ;
#23848 = CARTESIAN_POINT('Ctrl Pts',(-19.3770005006573,38.728687867598,124.617340881454)) ;
#23849 = CARTESIAN_POINT('Ctrl Pts',(-19.3689353661875,38.5486987872351,124.918722771456)) ;
#23850 = CARTESIAN_POINT('Ctrl Pts',(-19.1714080286777,38.7385281992703,124.594087546926)) ;
#23851 = CARTESIAN_POINT('Ctrl Pts',(-19.1119433120646,38.5585391189074,124.8896559552)) ;
#23852 = CARTESIAN_POINT('Ctrl Pts',(-18.9684668170041,38.7485912453621,124.53442387862)) ;
#23853 = CARTESIAN_POINT('Ctrl Pts',(-18.858267179598,38.5686021649992,124.815076395297)) ;
#23854 = CARTESIAN_POINT('Ctrl Pts',(-18.7821841412429,38.7584853010572,124.441832669131)) ;
#23855 = CARTESIAN_POINT('Ctrl Pts',(-18.6254129262552,38.5784962206943,124.699336919331)) ;
#23856 = CARTESIAN_POINT('Ctrl Pts',(-18.613681541493,38.7684280013801,124.318182967995)) ;
#23857 = CARTESIAN_POINT('Ctrl Pts',(-18.4147842988255,38.5884389210173,124.544774213898)) ;
#23858 = CARTESIAN_POINT('Ctrl Pts',(-18.4682304496749,38.7784337423077,124.166191909922)) ;
#23859 = CARTESIAN_POINT('Ctrl Pts',(-18.2329705623296,38.5984446619449,124.354785151136)) ;
#23860 = CARTESIAN_POINT('Ctrl Pts',(-18.3514150571057,38.7884546528233,123.990879578772)) ;
#23861 = CARTESIAN_POINT('Ctrl Pts',(-18.086951476104,38.6084655724604,124.135644682199)) ;
#23862 = CARTESIAN_POINT('Ctrl Pts',(-18.2676887679517,38.7983453882732,123.800540045983)) ;
#23863 = CARTESIAN_POINT('Ctrl Pts',(-17.9822934308915,38.6183563079104,123.897719206915)) ;
#23864 = CARTESIAN_POINT('Ctrl Pts',(-18.2174815072807,38.8083369290021,123.596583556656)) ;
#23865 = CARTESIAN_POINT('Ctrl Pts',(-17.9195346698227,38.6283478486392,123.642773296593)) ;
#23866 = CARTESIAN_POINT('Ctrl Pts',(-18.2035708832846,38.8182847894237,123.387913191954)) ;
#23867 = CARTESIAN_POINT('Ctrl Pts',(-17.9021467020347,38.6382957090609,123.381934725884)) ;
#23868 = CARTESIAN_POINT('Ctrl Pts',(-18.2256918881132,38.8282314586101,123.17996466364)) ;
#23869 = CARTESIAN_POINT('Ctrl Pts',(-17.9297985346469,38.6482423782472,123.121998548221)) ;
#23870 = CARTESIAN_POINT('Ctrl Pts',(-18.2843906460259,38.8382795347457,122.977049468211)) ;
#23871 = CARTESIAN_POINT('Ctrl Pts',(-18.0031723206151,38.6582904543828,122.868354913034)) ;
#23872 = CARTESIAN_POINT('Ctrl Pts',(-18.3754224094433,38.8481271327513,122.79110855479)) ;
#23873 = CARTESIAN_POINT('Ctrl Pts',(-18.1169630845849,38.6681380523884,122.635927730738)) ;
#23874 = CARTESIAN_POINT('Ctrl Pts',(-18.4982316363328,38.8580888558358,122.621481919964)) ;
#23875 = CARTESIAN_POINT('Ctrl Pts',(-18.2704754939803,38.6780997754729,122.423894509235)) ;
#23876 = CARTESIAN_POINT('Ctrl Pts',(-18.6498412742199,38.8681174909188,122.474952850286)) ;
#23877 = CARTESIAN_POINT('Ctrl Pts',(-18.459987920288,38.6881284105559,122.240733703719)) ;
#23878 = CARTESIAN_POINT('Ctrl Pts',(-18.822471332867,38.8780277992368,122.358322296909)) ;
#23879 = CARTESIAN_POINT('Ctrl Pts',(-18.6757765964958,38.6980387188739,122.094945578105)) ;
#23880 = CARTESIAN_POINT('Ctrl Pts',(-19.0129931752722,38.8879626963727,122.272721130062)) ;
#23881 = CARTESIAN_POINT('Ctrl Pts',(-18.9139298646634,38.7079736160098,121.987944654687)) ;
#23882 = CARTESIAN_POINT('Ctrl Pts',(-19.2176845439249,38.8980037793153,122.221146163374)) ;
#23883 = CARTESIAN_POINT('Ctrl Pts',(-19.1697940908906,38.7180146989524,121.92347677505)) ;
#23884 = CARTESIAN_POINT('Ctrl Pts',(-19.4250041735291,38.9078911221435,122.205985759555)) ;
#23885 = CARTESIAN_POINT('Ctrl Pts',(-19.4289447281885,38.7279020417806,121.904527054462)) ;
#23886 = CARTESIAN_POINT('Ctrl Pts',(-19.6340005528841,38.9178826370828,122.22691350164)) ;
#23887 = CARTESIAN_POINT('Ctrl Pts',(-19.6901903067169,38.73789355672,121.930687744959)) ;
#23888 = CARTESIAN_POINT('Ctrl Pts',(-19.8353682152375,38.9278340282793,122.283672510292)) ;
#23889 = CARTESIAN_POINT('Ctrl Pts',(-19.9419001392369,38.7478449479164,122.001637581168)) ;
#23890 = CARTESIAN_POINT('Ctrl Pts',(-20.0236163341247,38.9377665616119,122.374032890848)) ;
#23891 = CARTESIAN_POINT('Ctrl Pts',(-20.1772104092053,38.7577774812491,122.114589337141)) ;
#23892 = CARTESIAN_POINT('Ctrl Pts',(-20.1944626039504,38.9477637195114,122.496427038679)) ;
#23893 = CARTESIAN_POINT('Ctrl Pts',(-20.3907677132585,38.7677746391485,122.267583026891)) ;
#23894 = CARTESIAN_POINT('Ctrl Pts',(-20.3413685794426,38.9577487296749,122.646417878081)) ;
#23895 = CARTESIAN_POINT('Ctrl Pts',(-20.5743995160923,38.777759649312,122.455072551218)) ;
#23896 = CARTESIAN_POINT('Ctrl Pts',(-20.46039600103,38.9677915562447,122.820765432393)) ;
#23897 = CARTESIAN_POINT('Ctrl Pts',(-20.7231828307075,38.7878024758818,122.673007430821)) ;
#23898 = CARTESIAN_POINT('Ctrl Pts',(-20.5459597437265,38.9776217905496,123.00891851305)) ;
#23899 = CARTESIAN_POINT('Ctrl Pts',(-20.8301369986688,38.7976327101868,122.908200598567)) ;
#23900 = CARTESIAN_POINT('Ctrl Pts',(-20.5989170245634,38.9876978157843,123.213977187539)) ;
#23901 = CARTESIAN_POINT('Ctrl Pts',(-20.8963322764258,38.8077087354214,123.164523836751)) ;
#23902 = CARTESIAN_POINT('Ctrl Pts',(-20.6152120888322,38.9975500522752,123.42050479598)) ;
#23903 = CARTESIAN_POINT('Ctrl Pts',(-20.9166999184839,38.8175609719123,123.422684680524)) ;
#23904 = CARTESIAN_POINT('Ctrl Pts',(-20.5951407332866,39.0076232587093,123.631287792169)) ;
#23905 = CARTESIAN_POINT('Ctrl Pts',(-20.8916094132905,38.8276341783464,123.686162896882)) ;
#23906 = CARTESIAN_POINT('Ctrl Pts',(-20.5400039210857,39.0174647682165,123.830719200316)) ;
#23907 = CARTESIAN_POINT('Ctrl Pts',(-20.8226867659829,38.8374756878536,123.935453060471)) ;
#23908 = CARTESIAN_POINT('Ctrl Pts',(-20.4507189099979,39.0274257149963,124.020134101284)) ;
#23909 = CARTESIAN_POINT('Ctrl Pts',(-20.711078874135,38.8474366346334,124.172221368131)) ;
#23910 = CARTESIAN_POINT('Ctrl Pts',(-20.3286238637453,39.0374635437963,124.192245807622)) ;
#23911 = CARTESIAN_POINT('Ctrl Pts',(-20.558458951886,38.8574744634334,124.387360046542)) ;
#23912 = CARTESIAN_POINT('Ctrl Pts',(-20.1811938017144,39.0473378535508,124.338423480837)) ;
#23913 = CARTESIAN_POINT('Ctrl Pts',(-20.3741695323438,38.8673487731879,124.570081720976)) ;
#23914 = CARTESIAN_POINT('Ctrl Pts',(-20.0072836350948,39.0574075512239,124.45908427213)) ;
#23915 = CARTESIAN_POINT('Ctrl Pts',(-20.1567812055592,38.8774184708611,124.72090620419)) ;
#23916 = CARTESIAN_POINT('Ctrl Pts',(-19.8195805182457,39.0672410225113,124.545752922959)) ;
#23917 = CARTESIAN_POINT('Ctrl Pts',(-19.9221504638818,38.8872519421485,124.82924108008)) ;
#23918 = CARTESIAN_POINT('Ctrl Pts',(-19.6158666766055,39.0772706690413,124.600148476529)) ;
#23919 = CARTESIAN_POINT('Ctrl Pts',(-19.6675077755331,38.8972815886784,124.897233739368)) ;
#23920 = CARTESIAN_POINT('Ctrl Pts',(-19.4056375158977,39.0873051833686,124.617714671404)) ;
#23921 = CARTESIAN_POINT('Ctrl Pts',(-19.4047212779265,38.9073161030058,124.919189865937)) ;
#23922 = CARTESIAN_POINT('Ctrl Pts',(-19.1998910206002,39.0971304688395,124.599407552797)) ;
#23923 = CARTESIAN_POINT('Ctrl Pts',(-19.1475370275011,38.9171413884767,124.896304082123)) ;
#23924 = CARTESIAN_POINT('Ctrl Pts',(-18.9967244321837,39.1071347103881,124.545112550832)) ;
#23925 = CARTESIAN_POINT('Ctrl Pts',(-18.8935792031542,38.9271456300252,124.828433457309)) ;
#23926 = CARTESIAN_POINT('Ctrl Pts',(-18.8064617759764,39.1171173554672,124.456450033526)) ;
#23927 = CARTESIAN_POINT('Ctrl Pts',(-18.6557514840931,38.9371282751043,124.717603510386)) ;
#23928 = CARTESIAN_POINT('Ctrl Pts',(-18.6335954547731,39.1271625525587,124.335184104469)) ;
#23929 = CARTESIAN_POINT('Ctrl Pts',(-18.439669749991,38.9471734721958,124.566019704998)) ;
#23930 = CARTESIAN_POINT('Ctrl Pts',(-18.4874417294713,39.1369856683188,124.189274410091)) ;
#23931 = CARTESIAN_POINT('Ctrl Pts',(-18.2569780632649,38.9569965879559,124.383630345431)) ;
#23932 = CARTESIAN_POINT('Ctrl Pts',(-18.3658597551784,39.1470202801191,124.016878296206)) ;
#23933 = CARTESIAN_POINT('Ctrl Pts',(-18.1050023548241,38.9670311997562,124.168134092341)) ;
#23934 = CARTESIAN_POINT('Ctrl Pts',(-18.2766733676231,39.1570452888922,123.825914539901)) ;
#23935 = CARTESIAN_POINT('Ctrl Pts',(-17.9935211048472,38.9770562085294,123.929428614842)) ;
#23936 = CARTESIAN_POINT('Ctrl Pts',(-18.2225068331294,39.1668972137338,123.626000802301)) ;
#23937 = CARTESIAN_POINT('Ctrl Pts',(-17.9258146375031,38.9869081333709,123.679534933401)) ;
#23938 = CARTESIAN_POINT('Ctrl Pts',(-18.2032934378515,39.1768881520565,123.416865948046)) ;
#23939 = CARTESIAN_POINT('Ctrl Pts',(-17.9017999976252,38.9968990716936,123.418116000194)) ;
#23940 = CARTESIAN_POINT('Ctrl Pts',(-18.2204270850265,39.186806137203,123.209038883101)) ;
#23941 = CARTESIAN_POINT('Ctrl Pts',(-17.9232192572526,39.0068170568401,123.158331775182)) ;
#23942 = CARTESIAN_POINT('Ctrl Pts',(-18.2739141189626,39.1968342380985,123.005131243804)) ;
#23943 = CARTESIAN_POINT('Ctrl Pts',(-17.9900801459671,39.0168451577356,122.903447812489)) ;
#23944 = CARTESIAN_POINT('Ctrl Pts',(-18.3606686893931,39.2067194790411,122.816282003128)) ;
#23945 = CARTESIAN_POINT('Ctrl Pts',(-18.0985256645866,39.0267303986782,122.66738650819)) ;
#23946 = CARTESIAN_POINT('Ctrl Pts',(-18.4797149154803,39.2167085920077,122.643274137874)) ;
#23947 = CARTESIAN_POINT('Ctrl Pts',(-18.2473354546933,39.0367195116448,122.451127866607)) ;
#23948 = CARTESIAN_POINT('Ctrl Pts',(-18.6280950699641,39.2267506563485,122.493104045599)) ;
#23949 = CARTESIAN_POINT('Ctrl Pts',(-18.4328121554963,39.0467615759856,122.263416874408)) ;
#23950 = CARTESIAN_POINT('Ctrl Pts',(-18.7964289728388,39.236579857753,122.37324034441)) ;
#23951 = CARTESIAN_POINT('Ctrl Pts',(-18.6432316642718,39.0565907773901,122.113588566168)) ;
#23952 = CARTESIAN_POINT('Ctrl Pts',(-18.9861633069281,39.2465866985112,122.282419196658)) ;
#23953 = CARTESIAN_POINT('Ctrl Pts',(-18.8804006960058,39.0665976181483,122.000064282247)) ;
#23954 = CARTESIAN_POINT('Ctrl Pts',(-19.1884846108807,39.2565742227031,122.226135721448)) ;
#23955 = CARTESIAN_POINT('Ctrl Pts',(-19.1333031196278,39.0765851423402,121.929712194851)) ;
#23956 = CARTESIAN_POINT('Ctrl Pts',(-19.3983474426324,39.2666038685117,122.205902107928)) ;
#23957 = CARTESIAN_POINT('Ctrl Pts',(-19.3956318554856,39.0866147881488,121.90442252384)) ;
#23958 = CARTESIAN_POINT('Ctrl Pts',(-19.6053336272935,39.2764778992504,122.221912828081)) ;
#23959 = CARTESIAN_POINT('Ctrl Pts',(-19.6543650766534,39.0964888188876,121.924438378725)) ;
#23960 = CARTESIAN_POINT('Ctrl Pts',(-19.8089581741731,39.2864772221145,122.274010548513)) ;
#23961 = CARTESIAN_POINT('Ctrl Pts',(-19.9088952559089,39.1064881417517,121.989562946881)) ;
#23962 = CARTESIAN_POINT('Ctrl Pts',(-19.9988971817539,39.2963880576901,122.359747483072)) ;
#23963 = CARTESIAN_POINT('Ctrl Pts',(-20.1463184204116,39.1163989773273,122.096736593804)) ;
#23964 = CARTESIAN_POINT('Ctrl Pts',(-20.173454632489,39.3064423056642,122.478884560245)) ;
#23965 = CARTESIAN_POINT('Ctrl Pts',(-20.3645137350782,39.1264532253013,122.245659936878)) ;
#23966 = CARTESIAN_POINT('Ctrl Pts',(-20.321953767156,39.3163010499269,122.623523272663)) ;
#23967 = CARTESIAN_POINT('Ctrl Pts',(-20.5501363523251,39.136311969564,122.426460600573)) ;
#23968 = CARTESIAN_POINT('Ctrl Pts',(-20.4457184725392,39.3263691359999,122.79519306141)) ;
#23969 = CARTESIAN_POINT('Ctrl Pts',(-20.7048400636721,39.146380055637,122.641049209758)) ;
#23970 = CARTESIAN_POINT('Ctrl Pts',(-20.5358574260446,39.3362246191794,122.981770543194)) ;
#23971 = CARTESIAN_POINT('Ctrl Pts',(-20.8175117263284,39.1562355388165,122.87427274074)) ;
#23972 = CARTESIAN_POINT('Ctrl Pts',(-20.593627567202,39.3462194649736,123.183789054105)) ;
#23973 = CARTESIAN_POINT('Ctrl Pts',(-20.889721867706,39.1662303846107,123.126796707764)) ;
#23974 = CARTESIAN_POINT('Ctrl Pts',(-20.6150717947813,39.3562507606361,123.393589597854)) ;
#23975 = CARTESIAN_POINT('Ctrl Pts',(-20.9165245762999,39.1762616802733,123.389047651322)) ;
#23976 = CARTESIAN_POINT('Ctrl Pts',(-20.6003432400617,39.366117303926,123.600498782211)) ;
#23977 = CARTESIAN_POINT('Ctrl Pts',(-20.8981112102425,39.1861282235631,123.647684462324)) ;
#23978 = CARTESIAN_POINT('Ctrl Pts',(-20.5496307755805,39.3761046996894,123.804223422372)) ;
#23979 = CARTESIAN_POINT('Ctrl Pts',(-20.8347179859735,39.1961156193265,123.902339731277)) ;
#23980 = CARTESIAN_POINT('Ctrl Pts',(-20.4647567854182,39.3860497404194,123.995331104397)) ;
#23981 = CARTESIAN_POINT('Ctrl Pts',(-20.728622932385,39.2060606600565,124.14122345198)) ;
#23982 = CARTESIAN_POINT('Ctrl Pts',(-20.3467526330684,39.3960942466361,124.170424565575)) ;
#23983 = CARTESIAN_POINT('Ctrl Pts',(-20.5811155220166,39.2161051662732,124.360088757602)) ;
#23984 = CARTESIAN_POINT('Ctrl Pts',(-20.2028876578197,39.4059577527734,124.31979097255)) ;
#23985 = CARTESIAN_POINT('Ctrl Pts',(-20.4012820501656,39.2259686724105,124.546795194446)) ;
#23986 = CARTESIAN_POINT('Ctrl Pts',(-20.0333359133557,39.4159506136095,124.443780975724)) ;
#23987 = CARTESIAN_POINT('Ctrl Pts',(-20.1893406639608,39.2359615332466,124.701780528445)) ;
#23988 = CARTESIAN_POINT('Ctrl Pts',(-19.8460776642137,39.4258768073284,124.535944097192)) ;
#23989 = CARTESIAN_POINT('Ctrl Pts',(-19.9552664329016,39.2458877269655,124.816982053056)) ;
#23990 = CARTESIAN_POINT('Ctrl Pts',(-19.6438526109254,39.435895733361,124.594760442334)) ;
#23991 = CARTESIAN_POINT('Ctrl Pts',(-19.7024842949339,39.2559066529981,124.890499840195)) ;
#23992 = CARTESIAN_POINT('Ctrl Pts',(-19.4366243471817,39.4458107327286,124.617535468965)) ;
#23993 = CARTESIAN_POINT('Ctrl Pts',(-19.4434484431289,39.2658216523657,124.918965884066)) ;
#23994 = CARTESIAN_POINT('Ctrl Pts',(-19.2257177733582,39.4558655042859,124.603751642872)) ;
#23995 = CARTESIAN_POINT('Ctrl Pts',(-19.1798154010535,39.275876423923,124.901733325748)) ;
#23996 = CARTESIAN_POINT('Ctrl Pts',(-19.024324659477,39.4657244665834,124.554651862093)) ;
#23997 = CARTESIAN_POINT('Ctrl Pts',(-18.9280744033614,39.2857353862206,124.840355827184)) ;
#23998 = CARTESIAN_POINT('Ctrl Pts',(-18.8318078658274,39.4757187104213,124.47057126686)) ;
#23999 = CARTESIAN_POINT('Ctrl Pts',(-18.6874294683808,39.2957296300584,124.735252472311)) ;
#24000 = CARTESIAN_POINT('Ctrl Pts',(-18.6579134178425,39.4856439398455,124.355188357993)) ;
#24001 = CARTESIAN_POINT('Ctrl Pts',(-18.4700628513266,39.3056548594826,124.591021419432)) ;
#24002 = CARTESIAN_POINT('Ctrl Pts',(-18.505167355136,39.495671903737,124.209924117878)) ;
#24003 = CARTESIAN_POINT('Ctrl Pts',(-18.2791321697973,39.3156828233741,124.409439034504)) ;
#24004 = CARTESIAN_POINT('Ctrl Pts',(-18.3815260589152,39.5055581633674,124.042821017598)) ;
#24005 = CARTESIAN_POINT('Ctrl Pts',(-18.1245827427517,39.3255690830045,124.200558385393)) ;
#24006 = CARTESIAN_POINT('Ctrl Pts',(-18.2873441788241,39.5155899264452,123.854158630485)) ;
#24007 = CARTESIAN_POINT('Ctrl Pts',(-18.0068578913663,39.3356008460823,123.964729079241)) ;
#24008 = CARTESIAN_POINT('Ctrl Pts',(-18.2280346546859,39.5254715527393,123.655023225739)) ;
#24009 = CARTESIAN_POINT('Ctrl Pts',(-17.9327236697777,39.3454824723765,123.715808953631)) ;
#24010 = CARTESIAN_POINT('Ctrl Pts',(-18.2037205041182,39.5355333222255,123.444926394971)) ;
#24011 = CARTESIAN_POINT('Ctrl Pts',(-17.9023337792867,39.3555442418626,123.453187507275)) ;
#24012 = CARTESIAN_POINT('Ctrl Pts',(-18.2159436021786,39.545391189721,123.238018443075)) ;
#24013 = CARTESIAN_POINT('Ctrl Pts',(-17.9176154685571,39.3654021093581,123.194552719115)) ;
#24014 = CARTESIAN_POINT('Ctrl Pts',(-18.2640935145991,39.5553828148383,123.033581530344)) ;
#24015 = CARTESIAN_POINT('Ctrl Pts',(-17.9778056084377,39.3753937344755,122.939007178567)) ;
#24016 = CARTESIAN_POINT('Ctrl Pts',(-18.346604236998,39.5653196139466,122.841649932194)) ;
#24017 = CARTESIAN_POINT('Ctrl Pts',(-18.0809465923163,39.3853305335837,122.699093789421)) ;
#24018 = CARTESIAN_POINT('Ctrl Pts',(-18.4615503978526,39.5753104435039,122.665852839243)) ;
#24019 = CARTESIAN_POINT('Ctrl Pts',(-18.2246316582653,39.3953213631411,122.479348914402)) ;
#24020 = CARTESIAN_POINT('Ctrl Pts',(-18.6059214023956,39.5853336792171,122.512353088395)) ;
#24021 = CARTESIAN_POINT('Ctrl Pts',(-18.4050975254076,39.4053445988542,122.287476075996)) ;
#24022 = CARTESIAN_POINT('Ctrl Pts',(-18.7725024087154,39.5952300272463,122.38771377753)) ;
#24023 = CARTESIAN_POINT('Ctrl Pts',(-18.6133254066964,39.4152409468834,122.131679228761)) ;
#24024 = CARTESIAN_POINT('Ctrl Pts',(-18.9597546314449,39.6052195897488,122.292601295741)) ;
#24025 = CARTESIAN_POINT('Ctrl Pts',(-18.8473919143103,39.4252305093859,122.012791074316)) ;
#24026 = CARTESIAN_POINT('Ctrl Pts',(-19.1618012116734,39.6152598974333,122.231549580434)) ;
#24027 = CARTESIAN_POINT('Ctrl Pts',(-19.0999512728563,39.4352708170704,121.936479082214)) ;
#24028 = CARTESIAN_POINT('Ctrl Pts',(-19.367227076232,39.6251022007805,122.206604242828)) ;
#24029 = CARTESIAN_POINT('Ctrl Pts',(-19.3567329848095,39.4451131204176,121.905300141157)) ;
#24030 = CARTESIAN_POINT('Ctrl Pts',(-19.5776342598679,39.6351259090596,122.217627035733)) ;
#24031 = CARTESIAN_POINT('Ctrl Pts',(-19.6197445019835,39.4551368286967,121.919081532484)) ;
#24032 = CARTESIAN_POINT('Ctrl Pts',(-19.8485635991152,39.6483480865273,122.280050363964)) ;
#24033 = CARTESIAN_POINT('Ctrl Pts',(-19.9583923044283,39.4683590061644,121.997113385212)) ;
#24034 = CARTESIAN_POINT('Ctrl Pts',(-20.0983757230061,39.6616406715866,122.4121455033)) ;
#24035 = CARTESIAN_POINT('Ctrl Pts',(-20.2706261181306,39.4816515912237,122.162206025503)) ;
#24036 = CARTESIAN_POINT('Ctrl Pts',(-20.3030677190675,39.6749255275082,122.602175666116)) ;
#24037 = CARTESIAN_POINT('Ctrl Pts',(-20.5265366200315,39.4949364471453,122.399782063078)) ;
#24038 = CARTESIAN_POINT('Ctrl Pts',(-20.4297258307919,39.684897754681,122.76921101663)) ;
#24039 = CARTESIAN_POINT('Ctrl Pts',(-20.6848475062148,39.5049086743181,122.608570519109)) ;
#24040 = CARTESIAN_POINT('Ctrl Pts',(-20.5251856164806,39.69480637112,122.95438797765)) ;
#24041 = CARTESIAN_POINT('Ctrl Pts',(-20.8041722375231,39.5148172907571,122.840044926829)) ;
#24042 = CARTESIAN_POINT('Ctrl Pts',(-20.587851626912,39.7048595765037,123.156213626947)) ;
#24043 = CARTESIAN_POINT('Ctrl Pts',(-20.8825021974907,39.5248704961408,123.09232602936)) ;
#24044 = CARTESIAN_POINT('Ctrl Pts',(-20.6141617899061,39.714724710264,123.361949025928)) ;
#24045 = CARTESIAN_POINT('Ctrl Pts',(-20.9153854640603,39.5347356299011,123.349500706136)) ;
#24046 = CARTESIAN_POINT('Ctrl Pts',(-20.6014061829563,39.7280637678903,123.642094545317)) ;
#24047 = CARTESIAN_POINT('Ctrl Pts',(-20.8994475638338,39.5480746875274,123.699654940672)) ;
#24048 = CARTESIAN_POINT('Ctrl Pts',(-20.4948803150655,39.7446329552234,123.977922234663)) ;
#24049 = CARTESIAN_POINT('Ctrl Pts',(-20.7662626209752,39.5646438748606,124.119481950554)) ;
#24050 = CARTESIAN_POINT('Ctrl Pts',(-20.279368944222,39.7612780950745,124.258669320355)) ;
#24051 = CARTESIAN_POINT('Ctrl Pts',(-20.4969232972869,39.5812890147116,124.470352991445)) ;
#24052 = CARTESIAN_POINT('Ctrl Pts',(-20.057952056873,39.7745503975479,124.428460036515)) ;
#24053 = CARTESIAN_POINT('Ctrl Pts',(-20.2201055636797,39.594561317185,124.682635504472)) ;
#24054 = CARTESIAN_POINT('Ctrl Pts',(-19.8719346516173,39.7845313609955,124.525525802343)) ;
#24055 = CARTESIAN_POINT('Ctrl Pts',(-19.9875926506158,39.6045422806326,124.803956293346)) ;
#24056 = CARTESIAN_POINT('Ctrl Pts',(-19.6726840160093,39.7944731930648,124.588696431075)) ;
#24057 = CARTESIAN_POINT('Ctrl Pts',(-19.7385233068285,39.6144841127019,124.882919421765)) ;
#24058 = CARTESIAN_POINT('Ctrl Pts',(-19.3951538397195,39.8077927622802,124.625793701431)) ;
#24059 = CARTESIAN_POINT('Ctrl Pts',(-19.3916274184842,39.6278036819174,124.929289096296)) ;
#24060 = CARTESIAN_POINT('Ctrl Pts',(-19.0464383279096,39.824322917213,124.581253491284)) ;
#24061 = CARTESIAN_POINT('Ctrl Pts',(-18.9557155359981,39.6443338368501,124.873608604834)) ;
#24062 = CARTESIAN_POINT('Ctrl Pts',(-18.668086969949,39.8443446427051,124.386327800272)) ;
#24063 = CARTESIAN_POINT('Ctrl Pts',(-18.4827841914937,39.6643555623422,124.629948165702)) ;
#24064 = CARTESIAN_POINT('Ctrl Pts',(-18.3816863058028,39.8641560393119,124.077284990008)) ;
#24065 = CARTESIAN_POINT('Ctrl Pts',(-18.1247857375982,39.684166958949,124.243642886315)) ;
#24066 = CARTESIAN_POINT('Ctrl Pts',(-18.2159257669221,39.8841412880207,123.686114821925)) ;
#24067 = CARTESIAN_POINT('Ctrl Pts',(-17.9175888921553,39.7041522076579,123.754678947954)) ;
#24068 = CARTESIAN_POINT('Ctrl Pts',(-18.1939835367103,39.9040353506567,123.263614550275)) ;
#24069 = CARTESIAN_POINT('Ctrl Pts',(-17.8901646194333,39.7240462702938,123.226554358752)) ;
#24070 = CARTESIAN_POINT('Ctrl Pts',(-18.317143757237,39.9239670298303,122.858111488064)) ;
#24071 = CARTESIAN_POINT('Ctrl Pts',(-18.0441177194512,39.7439779494674,122.719677099901)) ;
#24072 = CARTESIAN_POINT('Ctrl Pts',(-18.5719284249735,39.9439310843023,122.518586193573)) ;
#24073 = CARTESIAN_POINT('Ctrl Pts',(-18.3626008286604,39.7639420039394,122.295272619757)) ;
#24074 = CARTESIAN_POINT('Ctrl Pts',(-18.9256419898356,39.9638119860652,122.287076377155)) ;
#24075 = CARTESIAN_POINT('Ctrl Pts',(-18.8047431638309,39.7838229057023,122.005888410444)) ;
#24076 = CARTESIAN_POINT('Ctrl Pts',(-19.3381892305123,39.9837506476736,122.189510079094)) ;
#24077 = CARTESIAN_POINT('Ctrl Pts',(-19.3204270314315,39.8037615673107,121.883932996576)) ;
#24078 = CARTESIAN_POINT('Ctrl Pts',(-19.7583997067115,40.0036471729289,122.23841409713)) ;
#24079 = CARTESIAN_POINT('Ctrl Pts',(-19.8456885699466,39.823658092566,121.945064977875)) ;
#24080 = CARTESIAN_POINT('Ctrl Pts',(-20.1370001314726,40.0235422113832,122.427152769696)) ;
#24081 = CARTESIAN_POINT('Ctrl Pts',(-20.3189371293568,39.8435531310203,122.180988955681)) ;
#24082 = CARTESIAN_POINT('Ctrl Pts',(-20.4293996902846,40.0435060346893,122.734826780891)) ;
#24083 = CARTESIAN_POINT('Ctrl Pts',(-20.684435302286,39.8635169543264,122.565581974928)) ;
#24084 = CARTESIAN_POINT('Ctrl Pts',(-20.598804014177,40.0633801588183,123.121996946429)) ;
#24085 = CARTESIAN_POINT('Ctrl Pts',(-20.8961892011034,39.8833910784555,123.049543285432)) ;
#24086 = CARTESIAN_POINT('Ctrl Pts',(-20.6264486511241,40.0833552345456,123.545839265876)) ;
#24087 = CARTESIAN_POINT('Ctrl Pts',(-20.9307446999035,39.9033661541827,123.579345858903)) ;
#24088 = CARTESIAN_POINT('Ctrl Pts',(-20.5073509704462,40.1033088039022,123.953040176851)) ;
#24089 = CARTESIAN_POINT('Ctrl Pts',(-20.7818723368726,39.9233197235393,124.088346140046)) ;
#24090 = CARTESIAN_POINT('Ctrl Pts',(-20.2585393963816,40.12314671409,124.293652583633)) ;
#24091 = CARTESIAN_POINT('Ctrl Pts',(-20.4708597448831,39.9431576337272,124.514109737929)) ;
#24092 = CARTESIAN_POINT('Ctrl Pts',(-19.9062499760645,40.143122542661,124.530920991778)) ;
#24093 = CARTESIAN_POINT('Ctrl Pts',(-20.0304987770853,39.9631334622981,124.810695893572)) ;
#24094 = CARTESIAN_POINT('Ctrl Pts',(-19.4952472081866,40.1630405873712,124.63297354376)) ;
#24095 = CARTESIAN_POINT('Ctrl Pts',(-19.5167467254977,39.9830515070084,124.938262136295)) ;
#24096 = CARTESIAN_POINT('Ctrl Pts',(-19.0748749833404,40.1829108331589,124.58981024594)) ;
#24097 = CARTESIAN_POINT('Ctrl Pts',(-18.9912829799873,40.002921752796,124.884310017349)) ;
#24098 = CARTESIAN_POINT('Ctrl Pts',(-18.6914968706604,40.2029598362585,124.403647517381)) ;
#24099 = CARTESIAN_POINT('Ctrl Pts',(-18.512059067701,40.0229707558956,124.651607827821)) ;
#24100 = CARTESIAN_POINT('Ctrl Pts',(-18.3981552231749,40.2227390774993,124.10210693945)) ;
#24101 = CARTESIAN_POINT('Ctrl Pts',(-18.1453823899898,40.0427499971364,124.274685535331)) ;
#24102 = CARTESIAN_POINT('Ctrl Pts',(-18.2226350296879,40.2427691412082,123.714169214818)) ;
#24103 = CARTESIAN_POINT('Ctrl Pts',(-17.9259795061986,40.0627800608453,123.789764142162)) ;
#24104 = CARTESIAN_POINT('Ctrl Pts',(-18.1909445920671,40.2626514261102,123.292541082987)) ;
#24105 = CARTESIAN_POINT('Ctrl Pts',(-17.8863640755832,40.0826623457473,123.26273048994)) ;
#24106 = CARTESIAN_POINT('Ctrl Pts',(-18.3038777435817,40.2825337270031,122.885191709277)) ;
#24107 = CARTESIAN_POINT('Ctrl Pts',(-18.0275270007879,40.1025446466403,122.753544083108)) ;
#24108 = CARTESIAN_POINT('Ctrl Pts',(-18.5504210038991,40.3025168366215,122.539129314307)) ;
#24109 = CARTESIAN_POINT('Ctrl Pts',(-18.3357032518353,40.1225277562586,122.320964219485)) ;
#24110 = CARTESIAN_POINT('Ctrl Pts',(-18.8986806428871,40.3224072319994,122.29912255241)) ;
#24111 = CARTESIAN_POINT('Ctrl Pts',(-18.7710249752049,40.1424181516365,122.020953450762)) ;
#24112 = CARTESIAN_POINT('Ctrl Pts',(-19.3078266805979,40.3423040220336,122.191737778741)) ;
#24113 = CARTESIAN_POINT('Ctrl Pts',(-19.2824556627369,40.1623149416708,121.886718883341)) ;
#24114 = CARTESIAN_POINT('Ctrl Pts',(-19.7296085524883,40.3622210759752,122.230003374302)) ;
#24115 = CARTESIAN_POINT('Ctrl Pts',(-19.809682792952,40.1822319956124,121.93454660401)) ;
#24116 = CARTESIAN_POINT('Ctrl Pts',(-20.1146489811739,40.3822246241788,122.410827144587)) ;
#24117 = CARTESIAN_POINT('Ctrl Pts',(-20.290985297749,40.2022355438159,122.160572440253)) ;
#24118 = CARTESIAN_POINT('Ctrl Pts',(-20.4133927271247,40.4021629178314,122.711596083807)) ;
#24119 = CARTESIAN_POINT('Ctrl Pts',(-20.6644175476188,40.2221738374685,122.536530476513)) ;
#24120 = CARTESIAN_POINT('Ctrl Pts',(-20.5914685302538,40.4219844052643,123.093592798811)) ;
#24121 = CARTESIAN_POINT('Ctrl Pts',(-20.8870164933769,40.2419953249014,123.014022848812)) ;
#24122 = CARTESIAN_POINT('Ctrl Pts',(-20.6292190379642,40.4419627982552,123.516656820411)) ;
#24123 = CARTESIAN_POINT('Ctrl Pts',(-20.9342078753314,40.2619737178923,123.54285440319)) ;
#24124 = CARTESIAN_POINT('Ctrl Pts',(-20.5204888317716,40.4618611798689,123.925614309865)) ;
#24125 = CARTESIAN_POINT('Ctrl Pts',(-20.798306014332,40.281872099506,124.054044528013)) ;
#24126 = CARTESIAN_POINT('Ctrl Pts',(-20.3195216622248,40.4784441105988,124.215207938259)) ;
#24127 = CARTESIAN_POINT('Ctrl Pts',(-20.5470819880528,40.2984550302359,124.416062159147)) ;
#24128 = CARTESIAN_POINT('Ctrl Pts',(-20.1066630617855,40.4917183461876,124.395787910796)) ;
#24129 = CARTESIAN_POINT('Ctrl Pts',(-20.281028441282,40.3117292658247,124.641768863592)) ;
#24130 = CARTESIAN_POINT('Ctrl Pts',(-19.9242973164539,40.5017647636438,124.502269830301)) ;
#24131 = CARTESIAN_POINT('Ctrl Pts',(-20.0530654837522,40.3217756832809,124.774877815114)) ;
#24132 = CARTESIAN_POINT('Ctrl Pts',(-19.7302037187856,40.5116099888631,124.57423387795)) ;
#24133 = CARTESIAN_POINT('Ctrl Pts',(-19.810464403995,40.3316209085002,124.864833820521)) ;
#24134 = CARTESIAN_POINT('Ctrl Pts',(-19.4546005991835,40.5249449599025,124.625166757655)) ;
#24135 = CARTESIAN_POINT('Ctrl Pts',(-19.4658929191224,40.3449558795396,124.928504806225)) ;
#24136 = CARTESIAN_POINT('Ctrl Pts',(-19.102968767351,40.5415278166951,124.597279021719)) ;
#24137 = CARTESIAN_POINT('Ctrl Pts',(-19.0264390688312,40.3615387363322,124.893652813554)) ;
#24138 = CARTESIAN_POINT('Ctrl Pts',(-18.7810021390429,40.5581708190445,124.450732297002)) ;
#24139 = CARTESIAN_POINT('Ctrl Pts',(-18.6239205040509,40.3781817386816,124.71045606654)) ;
#24140 = CARTESIAN_POINT('Ctrl Pts',(-18.5658420171576,40.5714145500762,124.273876479058)) ;
#24141 = CARTESIAN_POINT('Ctrl Pts',(-18.3550031410799,40.3914254697133,124.489405088402)) ;
#24142 = CARTESIAN_POINT('Ctrl Pts',(-18.428371398618,40.5814689447508,124.113372164029)) ;
#24143 = CARTESIAN_POINT('Ctrl Pts',(-18.1831556506858,40.4014798643879,124.288773158582)) ;
#24144 = CARTESIAN_POINT('Ctrl Pts',(-18.322862621758,40.5913100061393,123.935361777761)) ;
#24145 = CARTESIAN_POINT('Ctrl Pts',(-18.0512693189918,40.4113209257765,124.066262657595)) ;
#24146 = CARTESIAN_POINT('Ctrl Pts',(-18.2480294467794,40.6013762304958,123.737449279801)) ;
#24147 = CARTESIAN_POINT('Ctrl Pts',(-17.9577246777451,40.421387150133,123.818872622899)) ;
#24148 = CARTESIAN_POINT('Ctrl Pts',(-18.2094701938353,40.6112568434155,123.533303511753)) ;
#24149 = CARTESIAN_POINT('Ctrl Pts',(-17.9095230457467,40.4312677630526,123.563691114021)) ;
#24150 = CARTESIAN_POINT('Ctrl Pts',(-18.206516541867,40.6212501365751,123.323267667439)) ;
#24151 = CARTESIAN_POINT('Ctrl Pts',(-17.9058281378729,40.4412610562122,123.30114626875)) ;
#24152 = CARTESIAN_POINT('Ctrl Pts',(-18.2398673386455,40.6312011447987,123.11670429861)) ;
#24153 = CARTESIAN_POINT('Ctrl Pts',(-17.9475138799179,40.4512120644359,123.042941598617)) ;
#24154 = CARTESIAN_POINT('Ctrl Pts',(-18.3093839574438,40.6412496591607,122.917243416711)) ;
#24155 = CARTESIAN_POINT('Ctrl Pts',(-18.0344070397604,40.4612605787978,122.793614478542)) ;
#24156 = CARTESIAN_POINT('Ctrl Pts',(-18.4101694123091,40.6510911652234,122.736528533016)) ;
#24157 = CARTESIAN_POINT('Ctrl Pts',(-18.1603863836437,40.4711020848605,122.567719550063)) ;
#24158 = CARTESIAN_POINT('Ctrl Pts',(-18.542325109746,40.6610768178531,122.573458997662)) ;
#24159 = CARTESIAN_POINT('Ctrl Pts',(-18.3255788630243,40.4810877374902,122.36388078949)) ;
#24160 = CARTESIAN_POINT('Ctrl Pts',(-18.7000440263116,40.671015826698,122.436353330348)) ;
#24161 = CARTESIAN_POINT('Ctrl Pts',(-18.5227257140879,40.4910267463351,122.192496536557)) ;
#24162 = CARTESIAN_POINT('Ctrl Pts',(-18.8809941836839,40.681056751991,122.327685783444)) ;
#24163 = CARTESIAN_POINT('Ctrl Pts',(-18.7489120153398,40.5010676716281,122.056659651422)) ;
#24164 = CARTESIAN_POINT('Ctrl Pts',(-19.0750989997885,40.6909470737459,122.253093211541)) ;
#24165 = CARTESIAN_POINT('Ctrl Pts',(-18.9915421154482,40.510957993383,121.963416273453)) ;
#24166 = CARTESIAN_POINT('Ctrl Pts',(-19.2812929576741,40.7009430470793,122.212614380291)) ;
#24167 = CARTESIAN_POINT('Ctrl Pts',(-19.249284101431,40.5209539667164,121.912814957505)) ;
#24168 = CARTESIAN_POINT('Ctrl Pts',(-19.4900519469436,40.7108744466613,122.208562124172)) ;
#24169 = CARTESIAN_POINT('Ctrl Pts',(-19.5102329048635,40.5308853662985,121.907746825893)) ;
#24170 = CARTESIAN_POINT('Ctrl Pts',(-19.6979309739298,40.7208799871384,122.240764687343)) ;
#24171 = CARTESIAN_POINT('Ctrl Pts',(-19.7700821945994,40.5408909067755,121.947997275359)) ;
#24172 = CARTESIAN_POINT('Ctrl Pts',(-19.8974653853249,40.7309129710697,122.30911862514)) ;
#24173 = CARTESIAN_POINT('Ctrl Pts',(-20.0195011590798,40.5509238907068,122.033437044935)) ;
#24174 = CARTESIAN_POINT('Ctrl Pts',(-20.0790342263548,40.7407686018965,122.40896792997)) ;
#24175 = CARTESIAN_POINT('Ctrl Pts',(-20.2464637604241,40.5607795215337,122.158246335581)) ;
#24176 = CARTESIAN_POINT('Ctrl Pts',(-20.2429931194927,40.7507680040897,122.540475873946)) ;
#24177 = CARTESIAN_POINT('Ctrl Pts',(-20.4514141919689,40.5707789237268,122.322629146748)) ;
#24178 = CARTESIAN_POINT('Ctrl Pts',(-20.3804016988981,40.7606624734508,122.696694794566)) ;
#24179 = CARTESIAN_POINT('Ctrl Pts',(-20.623177160939,40.5806733930879,122.517901168788)) ;
#24180 = CARTESIAN_POINT('Ctrl Pts',(-20.4903492131892,40.770725587615,122.877396553859)) ;
#24181 = CARTESIAN_POINT('Ctrl Pts',(-20.7606139057598,40.5907365072521,122.743776897285)) ;
#24182 = CARTESIAN_POINT('Ctrl Pts',(-20.565781026169,40.7805652333314,123.070050005765)) ;
#24183 = CARTESIAN_POINT('Ctrl Pts',(-20.8549063786372,40.6005761529685,122.984593090461)) ;
#24184 = CARTESIAN_POINT('Ctrl Pts',(-20.6077950411033,40.7906284008871,123.277366104284)) ;
#24185 = CARTESIAN_POINT('Ctrl Pts',(-20.9074265587478,40.6106393205242,123.243737629738)) ;
#24186 = CARTESIAN_POINT('Ctrl Pts',(-20.6129087024178,40.800522656682,123.485334552873)) ;
#24187 = CARTESIAN_POINT('Ctrl Pts',(-20.9138213840196,40.6205335763191,123.50369845043)) ;
#24188 = CARTESIAN_POINT('Ctrl Pts',(-20.5822552704826,40.8104644351417,123.692055896881)) ;
#24189 = CARTESIAN_POINT('Ctrl Pts',(-20.8755072031584,40.6304753547788,123.762100783259)) ;
#24190 = CARTESIAN_POINT('Ctrl Pts',(-20.5158234904619,40.8204671279719,123.891604227127)) ;
#24191 = CARTESIAN_POINT('Ctrl Pts',(-20.7924699762297,40.640478047609,124.011537115954)) ;
#24192 = CARTESIAN_POINT('Ctrl Pts',(-20.4151748597048,40.8305011499257,124.076979654914)) ;
#24193 = CARTESIAN_POINT('Ctrl Pts',(-20.6666615752292,40.6505120695628,124.243257679907)) ;
#24194 = CARTESIAN_POINT('Ctrl Pts',(-20.2865434555371,40.8403489410147,124.239210149898)) ;
#24195 = CARTESIAN_POINT('Ctrl Pts',(-20.5058740591058,40.6603598606518,124.446047890609)) ;
#24196 = CARTESIAN_POINT('Ctrl Pts',(-20.1299205089068,40.8503304655638,124.378837643327)) ;
#24197 = CARTESIAN_POINT('Ctrl Pts',(-20.3100969713907,40.6703413852009,124.620584309683)) ;
#24198 = CARTESIAN_POINT('Ctrl Pts',(-19.951972487446,40.8602796890547,124.488778577698)) ;
#24199 = CARTESIAN_POINT('Ctrl Pts',(-20.0876630799493,40.6802906086918,124.75801282759)) ;
#24200 = CARTESIAN_POINT('Ctrl Pts',(-19.7567802099133,40.8702773452713,124.566778486158)) ;
#24201 = CARTESIAN_POINT('Ctrl Pts',(-19.8436735816779,40.6902882649084,124.85551512015)) ;
#24202 = CARTESIAN_POINT('Ctrl Pts',(-19.5500818247868,40.8803175583263,124.609481079621)) ;
#24203 = CARTESIAN_POINT('Ctrl Pts',(-19.5853011891557,40.7003284779634,124.908895920478)) ;
#24204 = CARTESIAN_POINT('Ctrl Pts',(-19.3435554371878,40.8901456056026,124.615967681651)) ;
#24205 = CARTESIAN_POINT('Ctrl Pts',(-19.3271425182227,40.7101565252397,124.917006738006)) ;
#24206 = CARTESIAN_POINT('Ctrl Pts',(-19.1343072045349,40.9001999526349,124.586146876164)) ;
#24207 = CARTESIAN_POINT('Ctrl Pts',(-19.0655819825205,40.7202108722721,124.87973320103)) ;
#24208 = CARTESIAN_POINT('Ctrl Pts',(-18.9357705406544,40.9101410889635,124.520845573056)) ;
#24209 = CARTESIAN_POINT('Ctrl Pts',(-18.8174100404169,40.7301520086006,124.798108890604)) ;
#24210 = CARTESIAN_POINT('Ctrl Pts',(-18.7519690818306,40.9200453220432,124.423000581694)) ;
#24211 = CARTESIAN_POINT('Ctrl Pts',(-18.5876566119404,40.7400562416803,124.675804537039)) ;
#24212 = CARTESIAN_POINT('Ctrl Pts',(-18.585688282195,40.9300920188868,124.292792552293)) ;
#24213 = CARTESIAN_POINT('Ctrl Pts',(-18.3798041844874,40.7501029385239,124.513046489696)) ;
#24214 = CARTESIAN_POINT('Ctrl Pts',(-18.4464901568893,40.9399875701671,124.138142420818)) ;
#24215 = CARTESIAN_POINT('Ctrl Pts',(-18.2058043531865,40.7599984898042,124.319735002295)) ;
#24216 = CARTESIAN_POINT('Ctrl Pts',(-18.3344376414912,40.9500496480066,123.958756744201)) ;
#24217 = CARTESIAN_POINT('Ctrl Pts',(-18.0657367626924,40.7700605676437,124.095504335531)) ;
#24218 = CARTESIAN_POINT('Ctrl Pts',(-18.2568316622771,40.9598923571026,123.766911195192)) ;
#24219 = CARTESIAN_POINT('Ctrl Pts',(-17.9687267603788,40.7799032767398,123.855697491767)) ;
#24220 = CARTESIAN_POINT('Ctrl Pts',(-18.2125910584586,40.9698830893411,123.561614077019)) ;
#24221 = CARTESIAN_POINT('Ctrl Pts',(-17.9134237543617,40.7898940089782,123.599076400319)) ;
#24222 = CARTESIAN_POINT('Ctrl Pts',(-18.204750664211,40.9798111145698,123.353032026553)) ;
#24223 = CARTESIAN_POINT('Ctrl Pts',(-17.9036209757213,40.799822034207,123.33834843595)) ;
#24224 = CARTESIAN_POINT('Ctrl Pts',(-18.2330639112473,40.9897992612204,123.14496244916)) ;
#24225 = CARTESIAN_POINT('Ctrl Pts',(-17.9390103972283,40.8098101808575,123.07826099235)) ;
#24226 = CARTESIAN_POINT('Ctrl Pts',(-18.297681746232,40.9998342790604,122.944131359391)) ;
#24227 = CARTESIAN_POINT('Ctrl Pts',(-18.0197805146774,40.8198451986975,122.827221506658)) ;
#24228 = CARTESIAN_POINT('Ctrl Pts',(-18.3943201381265,41.0096990761655,122.760643431724)) ;
#24229 = CARTESIAN_POINT('Ctrl Pts',(-18.1405769536225,40.8297099958027,122.597859805826)) ;
#24230 = CARTESIAN_POINT('Ctrl Pts',(-18.5221077214792,41.0196598085217,122.594742227815)) ;
#24231 = CARTESIAN_POINT('Ctrl Pts',(-18.3003100262152,40.8396707281588,122.390481778754)) ;
#24232 = CARTESIAN_POINT('Ctrl Pts',(-18.6781171729852,41.0296932709187,122.452788170327)) ;
#24233 = CARTESIAN_POINT('Ctrl Pts',(-18.4953203364736,40.8497041905558,122.213037685501)) ;
#24234 = CARTESIAN_POINT('Ctrl Pts',(-18.8536177054508,41.0395788051301,122.341428905828)) ;
#24235 = CARTESIAN_POINT('Ctrl Pts',(-18.7146955767961,40.8595897247672,122.073836456238)) ;
#24236 = CARTESIAN_POINT('Ctrl Pts',(-19.0492301850846,41.0496436458101,122.260823818413)) ;
#24237 = CARTESIAN_POINT('Ctrl Pts',(-18.9592101605245,40.8696545654472,121.973078301155)) ;
#24238 = CARTESIAN_POINT('Ctrl Pts',(-19.2514386207072,41.0594917775389,122.216286024392)) ;
#24239 = CARTESIAN_POINT('Ctrl Pts',(-19.2119712899475,40.8795026971761,121.917403865115)) ;
#24240 = CARTESIAN_POINT('Ctrl Pts',(-19.4620301676676,41.0695192745291,122.206830853245)) ;
#24241 = CARTESIAN_POINT('Ctrl Pts',(-19.4752106016322,40.8895301941662,121.905583046178)) ;
#24242 = CARTESIAN_POINT('Ctrl Pts',(-19.6710285196364,41.0795477265741,122.234643377154)) ;
#24243 = CARTESIAN_POINT('Ctrl Pts',(-19.7364587404572,40.8995586462113,121.940346685251)) ;
#24244 = CARTESIAN_POINT('Ctrl Pts',(-19.8684484239612,41.0893929931382,122.29677641338)) ;
#24245 = CARTESIAN_POINT('Ctrl Pts',(-19.9832352577145,40.9094039127754,122.018011497405)) ;
#24246 = CARTESIAN_POINT('Ctrl Pts',(-20.05506817094,41.0993836660792,122.39316265703)) ;
#24247 = CARTESIAN_POINT('Ctrl Pts',(-20.2165109099258,40.9193945857163,122.138492853158)) ;
#24248 = CARTESIAN_POINT('Ctrl Pts',(-20.2226153017789,41.1094215481676,122.521458694971)) ;
#24249 = CARTESIAN_POINT('Ctrl Pts',(-20.4259458604295,40.9294324678048,122.29886132802)) ;
#24250 = CARTESIAN_POINT('Ctrl Pts',(-20.3628619913098,41.1192659186073,122.673663617627)) ;
#24251 = CARTESIAN_POINT('Ctrl Pts',(-20.6012563123727,40.9392768382444,122.489117146691)) ;
#24252 = CARTESIAN_POINT('Ctrl Pts',(-20.4764734479912,41.1292507460027,122.850139489613)) ;
#24253 = CARTESIAN_POINT('Ctrl Pts',(-20.7432721400069,40.9492616656398,122.709711313099)) ;
#24254 = CARTESIAN_POINT('Ctrl Pts',(-20.5574566491448,41.139190191408,123.042799763275)) ;
#24255 = CARTESIAN_POINT('Ctrl Pts',(-20.844502824681,40.9592011110451,122.950536538216)) ;
#24256 = CARTESIAN_POINT('Ctrl Pts',(-20.6041559807991,41.1492301956939,123.248619953668)) ;
#24257 = CARTESIAN_POINT('Ctrl Pts',(-20.9028785373405,40.969241115331,123.20781127082)) ;
#24258 = CARTESIAN_POINT('Ctrl Pts',(-20.6143967382331,41.1591173048795,123.456249137288)) ;
#24259 = CARTESIAN_POINT('Ctrl Pts',(-20.9156810985871,40.9791282245166,123.46734861019)) ;
#24260 = CARTESIAN_POINT('Ctrl Pts',(-20.5883994319064,41.169117364782,123.664835776685)) ;
#24261 = CARTESIAN_POINT('Ctrl Pts',(-20.8831859202662,40.9891282844191,123.728082234662)) ;
#24262 = CARTESIAN_POINT('Ctrl Pts',(-20.5272409128475,41.1790347806967,123.864195390867)) ;
#24263 = CARTESIAN_POINT('Ctrl Pts',(-20.8067389220528,40.9990457003338,123.977282854265)) ;
#24264 = CARTESIAN_POINT('Ctrl Pts',(-20.4311340846493,41.1890815954375,124.052246102088)) ;
#24265 = CARTESIAN_POINT('Ctrl Pts',(-20.6866067690655,41.0090925150746,124.212346711425)) ;
#24266 = CARTESIAN_POINT('Ctrl Pts',(-20.3061390393343,41.1989570726341,124.218058301868)) ;
#24267 = CARTESIAN_POINT('Ctrl Pts',(-20.5303634279957,41.0189679922713,124.419613620439)) ;
#24268 = CARTESIAN_POINT('Ctrl Pts',(-20.1516052416653,41.2090131683554,124.362275980325)) ;
#24269 = CARTESIAN_POINT('Ctrl Pts',(-20.3371972791705,41.0290240879925,124.599886515678)) ;
#24270 = CARTESIAN_POINT('Ctrl Pts',(-19.977229302393,41.2189063303704,124.475710615594)) ;
#24271 = CARTESIAN_POINT('Ctrl Pts',(-20.1192272911797,41.0389172500076,124.741681401867)) ;
#24272 = CARTESIAN_POINT('Ctrl Pts',(-19.782620580465,41.228968566393,124.558568223159)) ;
#24273 = CARTESIAN_POINT('Ctrl Pts',(-19.8759671921668,41.0489794860302,124.845254462117)) ;
#24274 = CARTESIAN_POINT('Ctrl Pts',(-19.5810123835409,41.238813032022,124.605369966311)) ;
#24275 = CARTESIAN_POINT('Ctrl Pts',(-19.6239559484601,41.0588239516591,124.903758180381)) ;
#24276 = CARTESIAN_POINT('Ctrl Pts',(-19.3719656317782,41.2487731247261,124.617339157751)) ;
#24277 = CARTESIAN_POINT('Ctrl Pts',(-19.3626471098562,41.0687840443633,124.918720690763)) ;
#24278 = CARTESIAN_POINT('Ctrl Pts',(-19.1624388090685,41.2588114137072,124.592224884282)) ;
#24279 = CARTESIAN_POINT('Ctrl Pts',(-19.1007386053563,41.0788223333443,124.887329010187)) ;
#24280 = CARTESIAN_POINT('Ctrl Pts',(-18.9636200217074,41.2686847368134,124.532486383853)) ;
#24281 = CARTESIAN_POINT('Ctrl Pts',(-18.8522137572535,41.0886956564505,124.812656518733)) ;
#24282 = CARTESIAN_POINT('Ctrl Pts',(-18.7745367667636,41.2787579208985,124.437217363327)) ;
#24283 = CARTESIAN_POINT('Ctrl Pts',(-18.6158596069558,41.0987688405356,124.693571352366)) ;
#24284 = CARTESIAN_POINT('Ctrl Pts',(-18.6088938849064,41.2885784331864,124.313905580801)) ;
#24285 = CARTESIAN_POINT('Ctrl Pts',(-18.4088042083935,41.1085893528235,124.539431437794)) ;
#24286 = CARTESIAN_POINT('Ctrl Pts',(-18.4633794200554,41.2986564293022,124.159977351109)) ;
#24287 = CARTESIAN_POINT('Ctrl Pts',(-18.2269108302998,41.1186673489393,124.347022071441)) ;
#24288 = CARTESIAN_POINT('Ctrl Pts',(-18.34929862132,41.3085105042855,123.986997787861)) ;
#24289 = CARTESIAN_POINT('Ctrl Pts',(-18.0843084263497,41.1285214239226,124.130796993338)) ;
#24290 = CARTESIAN_POINT('Ctrl Pts',(-18.2650562986397,41.3185743858692,123.79296185912)) ;
#24291 = CARTESIAN_POINT('Ctrl Pts',(-17.9790049811939,41.1385853055063,123.888252695276)) ;
#24292 = CARTESIAN_POINT('Ctrl Pts',(-18.2166879254847,41.3284578118429,123.590852828316)) ;
#24293 = CARTESIAN_POINT('Ctrl Pts',(-17.9185435301409,41.14846873148,123.63561553845)) ;
#24294 = CARTESIAN_POINT('Ctrl Pts',(-18.2036681221716,41.338458415764,123.381049020955)) ;
#24295 = CARTESIAN_POINT('Ctrl Pts',(-17.9022681371798,41.1584693354011,123.37336067713)) ;
#24296 = CARTESIAN_POINT('Ctrl Pts',(-18.2269611110855,41.3483782001018,123.173770725139)) ;
#24297 = CARTESIAN_POINT('Ctrl Pts',(-17.931383888056,41.168389119739,123.114261971927)) ;
#24298 = CARTESIAN_POINT('Ctrl Pts',(-18.2866756180986,41.3584255504587,122.971196494413)) ;
#24299 = CARTESIAN_POINT('Ctrl Pts',(-18.0060263785442,41.1784364700958,122.861044240447)) ;
#24300 = CARTESIAN_POINT('Ctrl Pts',(-18.3788795710986,41.368302892693,122.785091205517)) ;
#24301 = CARTESIAN_POINT('Ctrl Pts',(-18.1212813811983,41.1883138123301,122.62841137183)) ;
#24302 = CARTESIAN_POINT('Ctrl Pts',(-18.5043585823623,41.3783727737676,122.614637642039)) ;
#24303 = CARTESIAN_POINT('Ctrl Pts',(-18.2781294851284,41.1983836934047,122.415344458296)) ;
#24304 = CARTESIAN_POINT('Ctrl Pts',(-18.6537818292948,41.3882024789693,122.471833456278)) ;
#24305 = CARTESIAN_POINT('Ctrl Pts',(-18.4649093676713,41.2082133986064,122.236837854703)) ;
#24306 = CARTESIAN_POINT('Ctrl Pts',(-18.8296579695578,41.3982691401357,122.35418375427)) ;
#24307 = CARTESIAN_POINT('Ctrl Pts',(-18.684754038693,41.2182800597728,122.089775689271)) ;
#24308 = CARTESIAN_POINT('Ctrl Pts',(-19.0200041203782,41.408159362003,122.270450878119)) ;
#24309 = CARTESIAN_POINT('Ctrl Pts',(-18.922687539533,41.2281702816401,121.985108837478)) ;
#24310 = CARTESIAN_POINT('Ctrl Pts',(-19.2239333482095,41.4181515381132,122.220092117685)) ;
#24311 = CARTESIAN_POINT('Ctrl Pts',(-19.1775992382533,41.2381624577503,121.922160157756)) ;
#24312 = CARTESIAN_POINT('Ctrl Pts',(-19.432913401362,41.4281143682258,122.206147099919)) ;
#24313 = CARTESIAN_POINT('Ctrl Pts',(-19.4388247420797,41.2481252878629,121.904728591906)) ;
#24314 = CARTESIAN_POINT('Ctrl Pts',(-19.6399945794,41.4380185806261,122.228042536446)) ;
#24315 = CARTESIAN_POINT('Ctrl Pts',(-19.6976771545585,41.2580295002633,121.932097935364)) ;
#24316 = CARTESIAN_POINT('Ctrl Pts',(-19.84319524037,41.448079294714,122.286638879611)) ;
#24317 = CARTESIAN_POINT('Ctrl Pts',(-19.9516776747255,41.2680902143511,122.005343143406)) ;
#24318 = CARTESIAN_POINT('Ctrl Pts',(-20.0291359735094,41.4579187976968,122.377353855789)) ;
#24319 = CARTESIAN_POINT('Ctrl Pts',(-20.1841049252899,41.2779297173339,122.118737500505)) ;
#24320 = CARTESIAN_POINT('Ctrl Pts',(-20.2004294013988,41.4679849362632,122.501563731977)) ;
#24321 = CARTESIAN_POINT('Ctrl Pts',(-20.3982213435744,41.2879958559003,122.273999666852)) ;
#24322 = CARTESIAN_POINT('Ctrl Pts',(-20.3448588998162,41.4778674507492,122.650955267273)) ;
#24323 = CARTESIAN_POINT('Ctrl Pts',(-20.5787589735412,41.2978783703863,122.460739928102)) ;
#24324 = CARTESIAN_POINT('Ctrl Pts',(-20.4627539040108,41.4878597501047,122.824784252551)) ;
#24325 = CARTESIAN_POINT('Ctrl Pts',(-20.7261276816334,41.3078706697419,122.678026456324)) ;
#24326 = CARTESIAN_POINT('Ctrl Pts',(-20.5484123348916,41.4978128170581,123.01572690911)) ;
#24327 = CARTESIAN_POINT('Ctrl Pts',(-20.8332007283246,41.3178237366953,122.916705335846)) ;
#24328 = CARTESIAN_POINT('Ctrl Pts',(-20.5999387117747,41.5078475252634,123.220282510794)) ;
#24329 = CARTESIAN_POINT('Ctrl Pts',(-20.8976084793145,41.3278584449005,123.172399737523)) ;
#24330 = CARTESIAN_POINT('Ctrl Pts',(-20.6150963668154,41.5177357461675,123.42762288197)) ;
#24331 = CARTESIAN_POINT('Ctrl Pts',(-20.9165553817096,41.3377466658047,123.431576287923)) ;
#24332 = CARTESIAN_POINT('Ctrl Pts',(-20.5941420991674,41.527730169198,123.636678083396)) ;
#24333 = CARTESIAN_POINT('Ctrl Pts',(-20.8903621464779,41.3477410888351,123.692895458737)) ;
#24334 = CARTESIAN_POINT('Ctrl Pts',(-20.5374038460003,41.5376755086441,123.837915099807)) ;
#24335 = CARTESIAN_POINT('Ctrl Pts',(-20.8194388311831,41.3576864282813,123.944442205965)) ;
#24336 = CARTESIAN_POINT('Ctrl Pts',(-20.4469513423603,41.5476228532555,124.026477171833)) ;
#24337 = CARTESIAN_POINT('Ctrl Pts',(-20.7063724848582,41.3676337728926,124.180145089931)) ;
#24338 = CARTESIAN_POINT('Ctrl Pts',(-20.3237166893896,41.5576707486665,124.198034788354)) ;
#24339 = CARTESIAN_POINT('Ctrl Pts',(-20.5523289698857,41.3776816683036,124.394591659)) ;
#24340 = CARTESIAN_POINT('Ctrl Pts',(-20.1756958626887,41.5675183941458,124.342779195868)) ;
#24341 = CARTESIAN_POINT('Ctrl Pts',(-20.3673015896202,41.387529313783,124.575522794134)) ;
#24342 = CARTESIAN_POINT('Ctrl Pts',(-20.0031915988338,41.5774801080598,124.461512163313)) ;
#24343 = CARTESIAN_POINT('Ctrl Pts',(-20.1516704586702,41.397491027697,124.723938642442)) ;
#24344 = CARTESIAN_POINT('Ctrl Pts',(-19.8112800553437,41.5875087323508,124.548840187101)) ;
#24345 = CARTESIAN_POINT('Ctrl Pts',(-19.911780850099,41.4075196519879,124.833098044345)) ;
#24346 = CARTESIAN_POINT('Ctrl Pts',(-19.6095677146579,41.5974190930075,124.600957112613)) ;
#24347 = CARTESIAN_POINT('Ctrl Pts',(-19.6596394073023,41.4174300126446,124.898243770015)) ;
#24348 = CARTESIAN_POINT('Ctrl Pts',(-19.4013858198479,41.6073537915808,124.617849546448)) ;
#24349 = CARTESIAN_POINT('Ctrl Pts',(-19.3994113076568,41.4273647112179,124.91935848404)) ;
#24350 = CARTESIAN_POINT('Ctrl Pts',(-19.1912280423145,41.617395616435,124.597921301321)) ;
#24351 = CARTESIAN_POINT('Ctrl Pts',(-19.1367143515178,41.4374065360721,124.894447395017)) ;
#24352 = CARTESIAN_POINT('Ctrl Pts',(-18.990832747362,41.6272801901794,124.542852864692)) ;
#24353 = CARTESIAN_POINT('Ctrl Pts',(-18.8862194476765,41.4472911098165,124.825610729058)) ;
#24354 = CARTESIAN_POINT('Ctrl Pts',(-18.8007506253046,41.6372820395426,124.453017154148)) ;
#24355 = CARTESIAN_POINT('Ctrl Pts',(-18.6486170762246,41.4572929591797,124.713315149718)) ;
#24356 = CARTESIAN_POINT('Ctrl Pts',(-18.6304363747329,41.6472013411166,124.332637276004)) ;
#24357 = CARTESIAN_POINT('Ctrl Pts',(-18.4357242323319,41.4672122607537,124.562839022651)) ;
#24358 = CARTESIAN_POINT('Ctrl Pts',(-18.4817919543754,41.6572454494619,124.182685192246)) ;
#24359 = CARTESIAN_POINT('Ctrl Pts',(-18.2499195837942,41.477256369099,124.375398346987)) ;
#24360 = CARTESIAN_POINT('Ctrl Pts',(-18.3632889695078,41.6671298729041,124.011973794938)) ;
#24361 = CARTESIAN_POINT('Ctrl Pts',(-18.1017911287502,41.4871407925413,124.162007655832)) ;
#24362 = CARTESIAN_POINT('Ctrl Pts',(-18.2746407632442,41.6771462348136,123.820958583722)) ;
#24363 = CARTESIAN_POINT('Ctrl Pts',(-17.9909819762134,41.4971571544507,123.923238127084)) ;
#24364 = CARTESIAN_POINT('Ctrl Pts',(-18.2209377342613,41.687182890319,123.616916772057)) ;
#24365 = CARTESIAN_POINT('Ctrl Pts',(-17.9238542028585,41.5071938099561,123.66818572458)) ;
#24366 = CARTESIAN_POINT('Ctrl Pts',(-18.2032737429254,41.6970130205083,123.410988166114)) ;
#24367 = CARTESIAN_POINT('Ctrl Pts',(-17.9017753134138,41.5170239401454,123.410773438911)) ;
#24368 = CARTESIAN_POINT('Ctrl Pts',(-18.2220155993058,41.7070890735982,123.200029060193)) ;
#24369 = CARTESIAN_POINT('Ctrl Pts',(-17.9252038428856,41.5270999932353,123.147075094843)) ;
#24370 = CARTESIAN_POINT('Ctrl Pts',(-18.2757906963554,41.716941302784,122.999961670963)) ;
#24371 = CARTESIAN_POINT('Ctrl Pts',(-17.9924242809587,41.5369522224211,122.896990000681)) ;
#24372 = CARTESIAN_POINT('Ctrl Pts',(-18.3652603008448,41.7270145105833,122.808056320445)) ;
#24373 = CARTESIAN_POINT('Ctrl Pts',(-18.1042623444851,41.5470254302204,122.657109249406)) ;
#24374 = CARTESIAN_POINT('Ctrl Pts',(-18.4839724624689,41.7368560219347,122.638585553312)) ;
#24375 = CARTESIAN_POINT('Ctrl Pts',(-18.2526543868681,41.5568669415718,122.445270485562)) ;
#24376 = CARTESIAN_POINT('Ctrl Pts',(-18.6315099791709,41.7468169599722,122.489983799293)) ;
#24377 = CARTESIAN_POINT('Ctrl Pts',(-18.4370777102109,41.5668278796093,122.259519138152)) ;
#24378 = CARTESIAN_POINT('Ctrl Pts',(-18.8041736856207,41.7568548218972,122.368670001095)) ;
#24379 = CARTESIAN_POINT('Ctrl Pts',(-18.6529080737898,41.5768657415343,122.107878162832)) ;
#24380 = CARTESIAN_POINT('Ctrl Pts',(-18.9920269431984,41.7667290078943,122.280273355514)) ;
#24381 = CARTESIAN_POINT('Ctrl Pts',(-18.8877262423687,41.5867399275314,121.997383365689)) ;
#24382 = CARTESIAN_POINT('Ctrl Pts',(-19.1963027713809,41.7767991674721,122.224790072043)) ;
#24383 = CARTESIAN_POINT('Ctrl Pts',(-19.1430711045837,41.5968100871093,121.928030886543)) ;
#24384 = CARTESIAN_POINT('Ctrl Pts',(-19.4021553537775,41.786630914898,122.205937341071)) ;
#24385 = CARTESIAN_POINT('Ctrl Pts',(-19.4003882644743,41.6066418345351,121.904466477439)) ;
#24386 = CARTESIAN_POINT('Ctrl Pts',(-19.6124500007053,41.7966669949693,122.222921105174)) ;
#24387 = CARTESIAN_POINT('Ctrl Pts',(-19.6632563157754,41.6166779146064,121.925697979521)) ;
#24388 = CARTESIAN_POINT('Ctrl Pts',(-19.8161003455475,41.8066840418218,122.27657994795)) ;
#24389 = CARTESIAN_POINT('Ctrl Pts',(-19.9178188413347,41.6266949614589,121.992773118902)) ;
#24390 = CARTESIAN_POINT('Ctrl Pts',(-20.004923629097,41.8165662999884,122.363238250864)) ;
#24391 = CARTESIAN_POINT('Ctrl Pts',(-20.1538480381938,41.6365772196255,122.10109797781)) ;
#24392 = CARTESIAN_POINT('Ctrl Pts',(-20.1777719329602,41.8265539827847,122.482413681147)) ;
#24393 = CARTESIAN_POINT('Ctrl Pts',(-20.3699075386073,41.6465649024218,122.250068895617)) ;
#24394 = CARTESIAN_POINT('Ctrl Pts',(-20.326844928488,41.8365006395015,122.629102840794)) ;
#24395 = CARTESIAN_POINT('Ctrl Pts',(-20.556247785553,41.6565115591386,122.433432011487)) ;
#24396 = CARTESIAN_POINT('Ctrl Pts',(-20.4493206526294,41.8465576975816,122.801419365625)) ;
#24397 = CARTESIAN_POINT('Ctrl Pts',(-20.7093408277522,41.6665686172188,122.648828544842)) ;
#24398 = CARTESIAN_POINT('Ctrl Pts',(-20.5381348768749,41.8563758771311,122.98775540366)) ;
#24399 = CARTESIAN_POINT('Ctrl Pts',(-20.8203574276063,41.6763867967682,122.881750559428)) ;
#24400 = CARTESIAN_POINT('Ctrl Pts',(-20.5950148919747,41.86641181157,123.190925085264)) ;
#24401 = CARTESIAN_POINT('Ctrl Pts',(-20.8914554133569,41.6864227312072,123.135713115928)) ;
#24402 = CARTESIAN_POINT('Ctrl Pts',(-20.615129903165,41.876436465999,123.400720653862)) ;
#24403 = CARTESIAN_POINT('Ctrl Pts',(-20.9165972820437,41.6964473856362,123.397957733958)) ;
#24404 = CARTESIAN_POINT('Ctrl Pts',(-20.5992555683587,41.8862884855786,123.607234834638)) ;
#24405 = CARTESIAN_POINT('Ctrl Pts',(-20.8967522553727,41.7062994052157,123.656101312759)) ;
#24406 = CARTESIAN_POINT('Ctrl Pts',(-20.5473561444667,41.8962793992935,123.810736345392)) ;
#24407 = CARTESIAN_POINT('Ctrl Pts',(-20.8318758704315,41.7162903189306,123.910477841226)) ;
#24408 = CARTESIAN_POINT('Ctrl Pts',(-20.4616446993946,41.9061973881331,124.000839502752)) ;
#24409 = CARTESIAN_POINT('Ctrl Pts',(-20.7247343585358,41.7262083077702,124.148106422392)) ;
#24410 = CARTESIAN_POINT('Ctrl Pts',(-20.3429884977472,41.9162254988639,124.175080591613)) ;
#24411 = CARTESIAN_POINT('Ctrl Pts',(-20.5764123274112,41.736236418501,124.365906529172)) ;
#24412 = CARTESIAN_POINT('Ctrl Pts',(-20.1980255650348,41.9261106967723,124.323996156688)) ;
#24413 = CARTESIAN_POINT('Ctrl Pts',(-20.395206571467,41.7461216164094,124.552049981452)) ;
#24414 = CARTESIAN_POINT('Ctrl Pts',(-20.0279320557978,41.9360999720403,124.447175593972)) ;
#24415 = CARTESIAN_POINT('Ctrl Pts',(-20.1825881915492,41.7561108916774,124.706022484706)) ;
#24416 = CARTESIAN_POINT('Ctrl Pts',(-19.837857448319,41.9461414302098,124.539013945011)) ;
#24417 = CARTESIAN_POINT('Ctrl Pts',(-19.944994054816,41.7661523498469,124.820818389465)) ;
#24418 = CARTESIAN_POINT('Ctrl Pts',(-19.6390644945786,41.9559728939981,124.595621547206)) ;
#24419 = CARTESIAN_POINT('Ctrl Pts',(-19.6965012965203,41.7759838136352,124.891575936423)) ;
#24420 = CARTESIAN_POINT('Ctrl Pts',(-19.4299150619604,41.965977826302,124.617688613248)) ;
#24421 = CARTESIAN_POINT('Ctrl Pts',(-19.4350641759092,41.7859887459391,124.919157369809)) ;
#24422 = CARTESIAN_POINT('Ctrl Pts',(-19.2204473086949,41.9759641901967,124.603013545437)) ;
#24423 = CARTESIAN_POINT('Ctrl Pts',(-19.1732294916453,41.7959751098338,124.900811143185)) ;
#24424 = CARTESIAN_POINT('Ctrl Pts',(-19.0159203877433,41.9859938190826,124.551823701844)) ;
#24425 = CARTESIAN_POINT('Ctrl Pts',(-18.9175714408772,41.8060047387197,124.836821562451)) ;
#24426 = CARTESIAN_POINT('Ctrl Pts',(-18.8262081647961,41.995869041191,124.467451255716)) ;
#24427 = CARTESIAN_POINT('Ctrl Pts',(-18.6804315219461,41.8158799608281,124.731353527358)) ;
#24428 = CARTESIAN_POINT('Ctrl Pts',(-18.6517356024177,42.0058702535881,124.350176231649)) ;
#24429 = CARTESIAN_POINT('Ctrl Pts',(-18.4623421036418,41.8258811732252,124.584757637499)) ;
#24430 = CARTESIAN_POINT('Ctrl Pts',(-18.5014918306554,42.0157788328236,124.205833220851)) ;
#24431 = CARTESIAN_POINT('Ctrl Pts',(-18.2745387790295,41.8357897524607,124.404326737909)) ;
#24432 = CARTESIAN_POINT('Ctrl Pts',(-18.376872413352,42.0258336853796,124.035131663706)) ;
#24433 = CARTESIAN_POINT('Ctrl Pts',(-18.1187665880947,41.8458446050167,124.190948411598)) ;
#24434 = CARTESIAN_POINT('Ctrl Pts',(-18.285357700117,42.0356922676544,123.849131188738)) ;
#24435 = CARTESIAN_POINT('Ctrl Pts',(-18.0043751834666,41.8557031872915,123.958446111396)) ;
#24436 = CARTESIAN_POINT('Ctrl Pts',(-18.2261951447151,42.0457603970971,123.645935941914)) ;
#24437 = CARTESIAN_POINT('Ctrl Pts',(-17.93042449407,41.8657713167342,123.70445148532)) ;
#24438 = CARTESIAN_POINT('Ctrl Pts',(-18.2037096295155,42.0556158687862,123.439949227679)) ;
#24439 = CARTESIAN_POINT('Ctrl Pts',(-17.9023200741687,41.8756267884233,123.446967189866)) ;
#24440 = CARTESIAN_POINT('Ctrl Pts',(-18.2168940215252,42.0656107171724,123.230246957662)) ;
#24441 = CARTESIAN_POINT('Ctrl Pts',(-17.9188032302922,41.8856216368096,123.184839420313)) ;
#24442 = CARTESIAN_POINT('Ctrl Pts',(-18.2669137943528,42.0756420139569,123.025370929616)) ;
#24443 = CARTESIAN_POINT('Ctrl Pts',(-17.9813304619599,41.895652933594,122.928744998837)) ;
#24444 = CARTESIAN_POINT('Ctrl Pts',(-18.3500517364716,42.085508550167,122.835328127626)) ;
#24445 = CARTESIAN_POINT('Ctrl Pts',(-18.0852555186611,41.9055194698041,122.691192079478)) ;
#24446 = CARTESIAN_POINT('Ctrl Pts',(-18.4660321364788,42.0954959731278,122.660329302149)) ;
#24447 = CARTESIAN_POINT('Ctrl Pts',(-18.2302333322929,41.9155068927649,122.472444933182)) ;
#24448 = CARTESIAN_POINT('Ctrl Pts',(-18.6099789814412,42.1054409121476,122.508661371675)) ;
#24449 = CARTESIAN_POINT('Ctrl Pts',(-18.4101690101242,41.9254518317847,122.282861709824)) ;
#24450 = CARTESIAN_POINT('Ctrl Pts',(-18.7797885338698,42.1154857980076,122.383148139199)) ;
#24451 = CARTESIAN_POINT('Ctrl Pts',(-18.6224325374237,41.9354967176447,122.125972345834)) ;
#24452 = CARTESIAN_POINT('Ctrl Pts',(-18.9654610961427,42.1253543330938,122.290568762634)) ;
#24453 = CARTESIAN_POINT('Ctrl Pts',(-18.8545248231622,41.9453652527309,122.010250360349)) ;
#24454 = CARTESIAN_POINT('Ctrl Pts',(-19.1661696006187,42.1353202011005,122.230497998175)) ;
#24455 = CARTESIAN_POINT('Ctrl Pts',(-19.1054113849967,41.9553311207376,121.935164518734)) ;
#24456 = CARTESIAN_POINT('Ctrl Pts',(-19.3754959713858,42.145342848553,122.206283829226)) ;
#24457 = CARTESIAN_POINT('Ctrl Pts',(-19.3670697024523,41.9653537681901,121.904899528248)) ;
#24458 = CARTESIAN_POINT('Ctrl Pts',(-19.5837472933625,42.1552664875606,122.218600651272)) ;
#24459 = CARTESIAN_POINT('Ctrl Pts',(-19.6273839317657,41.9752774071977,121.920298317369)) ;
#24460 = CARTESIAN_POINT('Ctrl Pts',(-19.7872248880091,42.1652092125663,122.266499710306)) ;
#24461 = CARTESIAN_POINT('Ctrl Pts',(-19.8817304496807,41.9852201322034,121.980174899417)) ;
#24462 = CARTESIAN_POINT('Ctrl Pts',(-19.98116015884,42.1752548186182,122.350078644094)) ;
#24463 = CARTESIAN_POINT('Ctrl Pts',(-20.1241484576752,41.9952657382553,122.084651122132)) ;
#24464 = CARTESIAN_POINT('Ctrl Pts',(-20.1545514692075,42.1851162411393,122.463760650406)) ;
#24465 = CARTESIAN_POINT('Ctrl Pts',(-20.3408862916986,42.0051271607764,122.22675611249)) ;
#24466 = CARTESIAN_POINT('Ctrl Pts',(-20.3078045675298,42.1951098095885,122.607431591005)) ;
#24467 = CARTESIAN_POINT('Ctrl Pts',(-20.5324507967766,42.0151207292256,122.406346888385)) ;
#24468 = CARTESIAN_POINT('Ctrl Pts',(-20.4330485966864,42.2050352803438,122.774367875557)) ;
#24469 = CARTESIAN_POINT('Ctrl Pts',(-20.6890036597013,42.0250461999809,122.615019061482)) ;
#24470 = CARTESIAN_POINT('Ctrl Pts',(-20.528359134433,42.2150629542996,122.96237648736)) ;
#24471 = CARTESIAN_POINT('Ctrl Pts',(-20.808139363818,42.0350738739368,122.850031069966)) ;
#24472 = CARTESIAN_POINT('Ctrl Pts',(-20.5889282022475,42.2249501323413,123.161244468246)) ;
#24473 = CARTESIAN_POINT('Ctrl Pts',(-20.8838479741626,42.0449610519785,123.098617303755)) ;
#24474 = CARTESIAN_POINT('Ctrl Pts',(-20.6145455202288,42.2349785117095,123.370482821943)) ;
#24475 = CARTESIAN_POINT('Ctrl Pts',(-20.9158670631571,42.0549894313466,123.360164459768)) ;
#24476 = CARTESIAN_POINT('Ctrl Pts',(-20.6037026584376,42.244872754431,123.57823145244)) ;
#24477 = CARTESIAN_POINT('Ctrl Pts',(-20.9023097751863,42.0648836740681,123.619854631483)) ;
#24478 = CARTESIAN_POINT('Ctrl Pts',(-20.5408518696117,42.2582256710819,123.851819040007)) ;
#24479 = CARTESIAN_POINT('Ctrl Pts',(-20.8237470249053,42.078236590719,123.961816174747)) ;
#24480 = CARTESIAN_POINT('Ctrl Pts',(-20.4095172303577,42.2714281888286,124.099989933585)) ;
#24481 = CARTESIAN_POINT('Ctrl Pts',(-20.6595997814835,42.0914391084657,124.272009590654)) ;
#24482 = CARTESIAN_POINT('Ctrl Pts',(-20.2186534632653,42.2847840941096,124.305832996325)) ;
#24483 = CARTESIAN_POINT('Ctrl Pts',(-20.4209837962718,42.1047950137467,124.529355053645)) ;
#24484 = CARTESIAN_POINT('Ctrl Pts',(-20.0529351292621,42.2946807427474,124.431692913237)) ;
#24485 = CARTESIAN_POINT('Ctrl Pts',(-20.2138409514704,42.1146916623845,124.686668820964)) ;
#24486 = CARTESIAN_POINT('Ctrl Pts',(-19.8651277354385,42.3047288807999,124.528356903845)) ;
#24487 = CARTESIAN_POINT('Ctrl Pts',(-19.9790784982733,42.124739800437,124.807498749042)) ;
#24488 = CARTESIAN_POINT('Ctrl Pts',(-19.6665158493402,42.3146198409776,124.58996703809)) ;
#24489 = CARTESIAN_POINT('Ctrl Pts',(-19.7308134332186,42.1346307606148,124.884508092935)) ;
#24490 = CARTESIAN_POINT('Ctrl Pts',(-19.4581683197363,42.3246126768544,124.616948547445)) ;
#24491 = CARTESIAN_POINT('Ctrl Pts',(-19.4703782998092,42.1446235964915,124.918232356421)) ;
#24492 = CARTESIAN_POINT('Ctrl Pts',(-19.2473681600248,42.334651771856,124.606814985885)) ;
#24493 = CARTESIAN_POINT('Ctrl Pts',(-19.2068788945409,42.1546626914931,124.905562765929)) ;
#24494 = CARTESIAN_POINT('Ctrl Pts',(-19.0455307327722,42.3444891277071,124.561634051858)) ;
#24495 = CARTESIAN_POINT('Ctrl Pts',(-18.9545800921988,42.1645000473443,124.849083179674)) ;
#24496 = CARTESIAN_POINT('Ctrl Pts',(-18.7855849758638,42.3578820756379,124.453519111834)) ;
#24497 = CARTESIAN_POINT('Ctrl Pts',(-18.629663451881,42.177892995275,124.713940021359)) ;
#24498 = CARTESIAN_POINT('Ctrl Pts',(-18.5635083695273,42.3710487520648,124.282885771656)) ;
#24499 = CARTESIAN_POINT('Ctrl Pts',(-18.3520925365356,42.1910596717019,124.500678451702)) ;
#24500 = CARTESIAN_POINT('Ctrl Pts',(-18.392149943478,42.3844335334716,124.059804324477)) ;
#24501 = CARTESIAN_POINT('Ctrl Pts',(-18.1378563760038,42.2044444531087,124.221781306289)) ;
#24502 = CARTESIAN_POINT('Ctrl Pts',(-18.2962255678194,42.3942953161154,123.875955923581)) ;
#24503 = CARTESIAN_POINT('Ctrl Pts',(-18.0179616237773,42.2143062357526,123.991978653527)) ;
#24504 = CARTESIAN_POINT('Ctrl Pts',(-18.2325120769393,42.4042944640685,123.675676595792)) ;
#24505 = CARTESIAN_POINT('Ctrl Pts',(-17.9383202716689,42.2243053837056,123.741625973935)) ;
#24506 = CARTESIAN_POINT('Ctrl Pts',(-18.2046075101168,42.4141972566856,123.469320833634)) ;
#24507 = CARTESIAN_POINT('Ctrl Pts',(-17.9034419632737,42.2342081763227,123.483683307464)) ;
#24508 = CARTESIAN_POINT('Ctrl Pts',(-18.2131324921205,42.4242468365765,123.258275057059)) ;
#24509 = CARTESIAN_POINT('Ctrl Pts',(-17.9141036164672,42.2442577562136,123.21987047093)) ;
#24510 = CARTESIAN_POINT('Ctrl Pts',(-18.271742279274,42.437433910386,122.987181315059)) ;
#24511 = CARTESIAN_POINT('Ctrl Pts',(-17.9873542558445,42.2574448300231,122.881031053165)) ;
#24512 = CARTESIAN_POINT('Ctrl Pts',(-18.4346521343874,42.4541867003572,122.670610361465)) ;
#24513 = CARTESIAN_POINT('Ctrl Pts',(-18.1910268972478,42.2741976199943,122.48527825742)) ;
#24514 = CARTESIAN_POINT('Ctrl Pts',(-18.6920409930995,42.4706753524519,122.432258546102)) ;
#24515 = CARTESIAN_POINT('Ctrl Pts',(-18.5127023287359,42.290686272089,122.187393477367)) ;
#24516 = CARTESIAN_POINT('Ctrl Pts',(-18.9400618332129,42.4840321786353,122.300845882537)) ;
#24517 = CARTESIAN_POINT('Ctrl Pts',(-18.8227825349679,42.3040430982724,122.023091316242)) ;
#24518 = CARTESIAN_POINT('Ctrl Pts',(-19.1380453310715,42.4939285635132,122.236723926044)) ;
#24519 = CARTESIAN_POINT('Ctrl Pts',(-19.0702507619016,42.3139394831503,121.942948929694)) ;
#24520 = CARTESIAN_POINT('Ctrl Pts',(-19.346318954824,42.5039350780337,122.2075435774)) ;
#24521 = CARTESIAN_POINT('Ctrl Pts',(-19.3305991665012,42.3239459976708,121.906474651851)) ;
#24522 = CARTESIAN_POINT('Ctrl Pts',(-19.623580125889,42.5171252015501,122.216652416966)) ;
#24523 = CARTESIAN_POINT('Ctrl Pts',(-19.6771578660426,42.3371361211872,121.917859655171)) ;
#24524 = CARTESIAN_POINT('Ctrl Pts',(-19.9644761073968,42.5338917626996,122.32049383106)) ;
#24525 = CARTESIAN_POINT('Ctrl Pts',(-20.1032957575407,42.3539026823368,122.047670197675)) ;
#24526 = CARTESIAN_POINT('Ctrl Pts',(-20.3009572251947,42.5536762514077,122.573177848514)) ;
#24527 = CARTESIAN_POINT('Ctrl Pts',(-20.5238873611168,42.3736871710448,122.363526341007)) ;
#24528 = CARTESIAN_POINT('Ctrl Pts',(-20.5338536920251,42.5736216990041,122.927472083475)) ;
#24529 = CARTESIAN_POINT('Ctrl Pts',(-20.8150059840566,42.3936326186413,122.806396279347)) ;
#24530 = CARTESIAN_POINT('Ctrl Pts',(-20.6313376491033,42.5935333611601,123.339481760479)) ;
#24531 = CARTESIAN_POINT('Ctrl Pts',(-20.9368565339894,42.4135442807972,123.32140844695)) ;
#24532 = CARTESIAN_POINT('Ctrl Pts',(-20.5833429972544,42.6134255531789,123.75977761235)) ;
#24533 = CARTESIAN_POINT('Ctrl Pts',(-20.8768601174002,42.4334364728161,123.846776921239)) ;
#24534 = CARTESIAN_POINT('Ctrl Pts',(-20.3928775516324,42.6334666837336,124.140904242147)) ;
#24535 = CARTESIAN_POINT('Ctrl Pts',(-20.6387749464663,42.4534776033707,124.323184054214)) ;
#24536 = CARTESIAN_POINT('Ctrl Pts',(-20.0872595412336,42.6532850183492,124.431171962633)) ;
#24537 = CARTESIAN_POINT('Ctrl Pts',(-20.2567515623942,42.4732959379863,124.686015098705)) ;
#24538 = CARTESIAN_POINT('Ctrl Pts',(-19.6984277741902,42.6732575835688,124.601563615224)) ;
#24539 = CARTESIAN_POINT('Ctrl Pts',(-19.7707111217134,42.4932685032059,124.899002007876)) ;
#24540 = CARTESIAN_POINT('Ctrl Pts',(-19.2762631710593,42.6931467997404,124.629052850656)) ;
#24541 = CARTESIAN_POINT('Ctrl Pts',(-19.2430064355605,42.5131577193775,124.933361056965)) ;
#24542 = CARTESIAN_POINT('Ctrl Pts',(-18.8676531896362,42.7131703740631,124.5098269493)) ;
#24543 = CARTESIAN_POINT('Ctrl Pts',(-18.7322443545962,42.5331812937002,124.784326245752)) ;
#24544 = CARTESIAN_POINT('Ctrl Pts',(-18.5278123839697,42.7329675371513,124.26130431907)) ;
#24545 = CARTESIAN_POINT('Ctrl Pts',(-18.3074466869106,42.5529784567885,124.473672881631)) ;
#24546 = CARTESIAN_POINT('Ctrl Pts',(-18.2904261749242,42.7529330309751,123.909466884417)) ;
#24547 = CARTESIAN_POINT('Ctrl Pts',(-18.0107152101051,42.5729439506122,124.03387590139)) ;
#24548 = CARTESIAN_POINT('Ctrl Pts',(-18.187872486649,42.7728867387165,123.49766130319)) ;
#24549 = CARTESIAN_POINT('Ctrl Pts',(-17.8825244705871,42.5928976583536,123.51911914368)) ;
#24550 = CARTESIAN_POINT('Ctrl Pts',(-18.2318581554824,42.7927941154431,123.076763552661)) ;
#24551 = CARTESIAN_POINT('Ctrl Pts',(-17.9375074674537,42.6128050350802,122.992998485349)) ;
#24552 = CARTESIAN_POINT('Ctrl Pts',(-18.4153780545509,42.8126463269917,122.696553693905)) ;
#24553 = CARTESIAN_POINT('Ctrl Pts',(-18.1669062692067,42.6326572466288,122.517738273591)) ;
#24554 = CARTESIAN_POINT('Ctrl Pts',(-18.7212077898556,42.8327187139374,122.398884993394)) ;
#24555 = CARTESIAN_POINT('Ctrl Pts',(-18.5491943143349,42.6527296335745,122.145651577482)) ;
#24556 = CARTESIAN_POINT('Ctrl Pts',(-19.1059608983857,42.8525565835777,122.225998547386)) ;
#24557 = CARTESIAN_POINT('Ctrl Pts',(-19.0301333322148,42.6725675032148,121.929544757103)) ;
#24558 = CARTESIAN_POINT('Ctrl Pts',(-19.526741490911,42.8724072381308,122.192939772244)) ;
#24559 = CARTESIAN_POINT('Ctrl Pts',(-19.5561067931665,42.6924181577679,121.88822002276)) ;
#24560 = CARTESIAN_POINT('Ctrl Pts',(-19.9374721598721,42.8924591724712,122.307188454904)) ;
#24561 = CARTESIAN_POINT('Ctrl Pts',(-20.0695211678143,42.7124700921084,122.031029897398)) ;
#24562 = CARTESIAN_POINT('Ctrl Pts',(-20.2808472333612,42.9122923600373,122.552162407161)) ;
#24563 = CARTESIAN_POINT('Ctrl Pts',(-20.4987389792293,42.7323032796744,122.33724488066)) ;
#24564 = CARTESIAN_POINT('Ctrl Pts',(-20.5217209474624,42.932221572268,122.90060218186)) ;
#24565 = CARTESIAN_POINT('Ctrl Pts',(-20.7998323714999,42.7522324919051,122.772792578482)) ;
#24566 = CARTESIAN_POINT('Ctrl Pts',(-20.6295592118292,42.9521065374824,123.309594803802)) ;
#24567 = CARTESIAN_POINT('Ctrl Pts',(-20.9346324231233,42.7721174571195,123.284031475315)) ;
#24568 = CARTESIAN_POINT('Ctrl Pts',(-20.5903609500711,42.972180278627,123.734525663825)) ;
#24569 = CARTESIAN_POINT('Ctrl Pts',(-20.8856369561692,42.7921911982641,123.815196128951)) ;
#24570 = CARTESIAN_POINT('Ctrl Pts',(-20.4110322867297,42.9919734604074,124.115338189697)) ;
#24571 = CARTESIAN_POINT('Ctrl Pts',(-20.6614795251124,42.8119843800445,124.291210805294)) ;
#24572 = CARTESIAN_POINT('Ctrl Pts',(-20.1109437575518,43.0119361684101,124.415478901693)) ;
#24573 = CARTESIAN_POINT('Ctrl Pts',(-20.2863715695943,42.8319470880472,124.666388958395)) ;
#24574 = CARTESIAN_POINT('Ctrl Pts',(-19.7255846738428,43.0319191201525,124.594466908089)) ;
#24575 = CARTESIAN_POINT('Ctrl Pts',(-19.8046741907438,42.8519300397896,124.890126754003)) ;
#24576 = CARTESIAN_POINT('Ctrl Pts',(-19.3059710828873,43.0517297399247,124.631722413805)) ;
#24577 = CARTESIAN_POINT('Ctrl Pts',(-19.2801592562473,42.8717406595618,124.936699673532)) ;
#24578 = CARTESIAN_POINT('Ctrl Pts',(-18.8952733972345,43.0717134559576,124.523123476909)) ;
#24579 = CARTESIAN_POINT('Ctrl Pts',(-18.7667862152892,42.8917243755947,124.800954951219)) ;
#24580 = CARTESIAN_POINT('Ctrl Pts',(-18.547948160276,43.0915949198549,124.281962291053)) ;
#24581 = CARTESIAN_POINT('Ctrl Pts',(-18.3326279856665,42.911605839492,124.499507379797)) ;
#24582 = CARTESIAN_POINT('Ctrl Pts',(-18.3027271825646,43.1115502496993,123.935800002761)) ;
#24583 = CARTESIAN_POINT('Ctrl Pts',(-18.0260984755986,42.9315611693364,124.066807185146)) ;
#24584 = CARTESIAN_POINT('Ctrl Pts',(-18.1904651269619,43.1314257105047,123.528307608364)) ;
#24585 = CARTESIAN_POINT('Ctrl Pts',(-17.8857662260403,42.9514366301419,123.557444062347)) ;
#24586 = CARTESIAN_POINT('Ctrl Pts',(-18.2239197601607,43.1514100305563,123.104753802092)) ;
#24587 = CARTESIAN_POINT('Ctrl Pts',(-17.9275815086194,42.9714209501934,123.027999899649)) ;
#24588 = CARTESIAN_POINT('Ctrl Pts',(-18.3996847638181,43.1713380633459,122.719094804955)) ;
#24589 = CARTESIAN_POINT('Ctrl Pts',(-18.1472767537667,42.991348982983,122.545930346273)) ;
#24590 = CARTESIAN_POINT('Ctrl Pts',(-18.646890943322,43.1879468252857,122.467036487721)) ;
#24591 = CARTESIAN_POINT('Ctrl Pts',(-18.4563016259536,43.0079577449228,122.230836526374)) ;
#24592 = CARTESIAN_POINT('Ctrl Pts',(-18.8854093868125,43.2011344639758,122.325626761766)) ;
#24593 = CARTESIAN_POINT('Ctrl Pts',(-18.7544287787532,43.0211453836129,122.054087877132)) ;
#24594 = CARTESIAN_POINT('Ctrl Pts',(-19.0816631258239,43.2111208983359,122.25109404408)) ;
#24595 = CARTESIAN_POINT('Ctrl Pts',(-18.9997521034799,43.031131817973,121.960916807132)) ;
#24596 = CARTESIAN_POINT('Ctrl Pts',(-19.2884287473412,43.2211302722953,122.211885729769)) ;
#24597 = CARTESIAN_POINT('Ctrl Pts',(-19.2581944108813,43.0411411919324,121.911902702877)) ;
#24598 = CARTESIAN_POINT('Ctrl Pts',(-19.5677559979308,43.2344203058605,122.208091123803)) ;
#24599 = CARTESIAN_POINT('Ctrl Pts',(-19.6074202778413,43.0544312254977,121.907165841963)) ;
#24600 = CARTESIAN_POINT('Ctrl Pts',(-19.9099408495608,43.251014293523,122.294450351363)) ;
#24601 = CARTESIAN_POINT('Ctrl Pts',(-20.0350687767284,43.0710252131601,122.015093622791)) ;
#24602 = CARTESIAN_POINT('Ctrl Pts',(-20.2026638187543,43.2676465487985,122.492780810066)) ;
#24603 = CARTESIAN_POINT('Ctrl Pts',(-20.4010277793674,43.0876574684357,122.26302842487)) ;
#24604 = CARTESIAN_POINT('Ctrl Pts',(-20.3849853860425,43.2808889324664,122.703218028358)) ;
#24605 = CARTESIAN_POINT('Ctrl Pts',(-20.6289019817072,43.1008998521035,122.526052209373)) ;
#24606 = CARTESIAN_POINT('Ctrl Pts',(-20.4925880976511,43.2908031406938,122.881725152075)) ;
#24607 = CARTESIAN_POINT('Ctrl Pts',(-20.7634137015571,43.1108140603309,122.749188831555)) ;
#24608 = CARTESIAN_POINT('Ctrl Pts',(-20.5684111030146,43.3008597799655,123.079068387712)) ;
#24609 = CARTESIAN_POINT('Ctrl Pts',(-20.8581936477321,43.1208706996026,122.995865179697)) ;
#24610 = CARTESIAN_POINT('Ctrl Pts',(-20.6082199665284,43.3107055863856,123.282209920598)) ;
#24611 = CARTESIAN_POINT('Ctrl Pts',(-20.9079570487934,43.1307165060227,123.249794573028)) ;
#24612 = CARTESIAN_POINT('Ctrl Pts',(-20.6125910585015,43.3207505860188,123.493341268355)) ;
#24613 = CARTESIAN_POINT('Ctrl Pts',(-20.9134264774939,43.1407615056559,123.513697714177)) ;
#24614 = CARTESIAN_POINT('Ctrl Pts',(-20.569416287465,43.3340316083915,123.769136883137)) ;
#24615 = CARTESIAN_POINT('Ctrl Pts',(-20.8594473356749,43.1540425280286,123.858497845333)) ;
#24616 = CARTESIAN_POINT('Ctrl Pts',(-20.4566616002104,43.3472290549162,124.026134355986)) ;
#24617 = CARTESIAN_POINT('Ctrl Pts',(-20.718508196259,43.1672399745533,124.17971260659)) ;
#24618 = CARTESIAN_POINT('Ctrl Pts',(-20.2801208783856,43.3606433527231,124.246084172849)) ;
#24619 = CARTESIAN_POINT('Ctrl Pts',(-20.4978485962577,43.1806542723603,124.454637161235)) ;
#24620 = CARTESIAN_POINT('Ctrl Pts',(-20.1246767207839,43.3704824181259,124.382563644853)) ;
#24621 = CARTESIAN_POINT('Ctrl Pts',(-20.3035425807458,43.190493337763,124.625241624044)) ;
#24622 = CARTESIAN_POINT('Ctrl Pts',(-19.9456198245211,43.3804656244036,124.492010358693)) ;
#24623 = CARTESIAN_POINT('Ctrl Pts',(-20.0797235876443,43.2004765440407,124.762051652017)) ;
#24624 = CARTESIAN_POINT('Ctrl Pts',(-19.7508481450483,43.3904168593164,124.568404517536)) ;
#24625 = CARTESIAN_POINT('Ctrl Pts',(-19.8362597616934,43.2104277789535,124.8575472145)) ;
#24626 = CARTESIAN_POINT('Ctrl Pts',(-19.5447971219931,43.400417859018,124.610275376094)) ;
#24627 = CARTESIAN_POINT('Ctrl Pts',(-19.5786965198764,43.2204287786551,124.909888505183)) ;
#24628 = CARTESIAN_POINT('Ctrl Pts',(-19.3339717832248,43.4104492048053,124.615418235309)) ;
#24629 = CARTESIAN_POINT('Ctrl Pts',(-19.3151648430061,43.2304601244425,124.916319914135)) ;
#24630 = CARTESIAN_POINT('Ctrl Pts',(-19.1290970717957,43.4203029695104,124.584716305653)) ;
#24631 = CARTESIAN_POINT('Ctrl Pts',(-19.0590709276985,43.2403138891475,124.877945266862)) ;
#24632 = CARTESIAN_POINT('Ctrl Pts',(-18.9302029392523,43.4302736231787,124.518609768227)) ;
#24633 = CARTESIAN_POINT('Ctrl Pts',(-18.8104522663154,43.2502845428158,124.79531472401)) ;
#24634 = CARTESIAN_POINT('Ctrl Pts',(-18.7452726680142,43.4402708668359,124.418674434814)) ;
#24635 = CARTESIAN_POINT('Ctrl Pts',(-18.5792880259183,43.260281786473,124.670397983482)) ;
#24636 = CARTESIAN_POINT('Ctrl Pts',(-18.5801137359114,43.4503043227801,124.28749236113)) ;
#24637 = CARTESIAN_POINT('Ctrl Pts',(-18.3728375783555,43.2703152424172,124.506422572522)) ;
#24638 = CARTESIAN_POINT('Ctrl Pts',(-18.4424457993828,43.4601598270805,124.132620980022)) ;
#24639 = CARTESIAN_POINT('Ctrl Pts',(-18.2007504134058,43.2801707467176,124.31283503278)) ;
#24640 = CARTESIAN_POINT('Ctrl Pts',(-18.3319639426538,43.4701592633666,123.953818397867)) ;
#24641 = CARTESIAN_POINT('Ctrl Pts',(-18.0626456729148,43.2901701830037,124.089333194053)) ;
#24642 = CARTESIAN_POINT('Ctrl Pts',(-18.2547737206712,43.4800537228825,123.760615819088)) ;
#24643 = CARTESIAN_POINT('Ctrl Pts',(-17.9661552350075,43.3000646425196,123.847830753989)) ;
#24644 = CARTESIAN_POINT('Ctrl Pts',(-18.2116553133487,43.4901168423341,123.553535266331)) ;
#24645 = CARTESIAN_POINT('Ctrl Pts',(-17.9122545173091,43.3101277619712,123.588980661551)) ;
#24646 = CARTESIAN_POINT('Ctrl Pts',(-18.2050619663453,43.4999564767461,123.346745963906)) ;
#24647 = CARTESIAN_POINT('Ctrl Pts',(-17.9040100749574,43.3199673963832,123.330493713353)) ;
#24648 = CARTESIAN_POINT('Ctrl Pts',(-18.23486765756,43.5100196842319,123.137325469672)) ;
#24649 = CARTESIAN_POINT('Ctrl Pts',(-17.9412644855324,43.330030603869,123.068717754911)) ;
#24650 = CARTESIAN_POINT('Ctrl Pts',(-18.2996597954055,43.5199137916111,122.939643533093)) ;
#24651 = CARTESIAN_POINT('Ctrl Pts',(-18.0222521551209,43.3399247112482,122.821614169064)) ;
#24652 = CARTESIAN_POINT('Ctrl Pts',(-18.3977518129424,43.5298561238035,122.755103321263)) ;
#24653 = CARTESIAN_POINT('Ctrl Pts',(-18.1448649357578,43.3498670434406,122.590937416187)) ;
#24654 = CARTESIAN_POINT('Ctrl Pts',(-18.5271067731501,43.5398567501185,122.589320233305)) ;
#24655 = CARTESIAN_POINT('Ctrl Pts',(-18.3065565946206,43.3598676697556,122.383706851709)) ;
#24656 = CARTESIAN_POINT('Ctrl Pts',(-18.6841488510847,43.5498984844004,122.448264779539)) ;
#24657 = CARTESIAN_POINT('Ctrl Pts',(-18.5028573530525,43.3699094040375,122.207385535582)) ;
#24658 = CARTESIAN_POINT('Ctrl Pts',(-18.8592239504986,43.5597239103495,122.33861707734)) ;
#24659 = CARTESIAN_POINT('Ctrl Pts',(-18.7217003533941,43.3797348299866,122.070323331608)) ;
#24660 = CARTESIAN_POINT('Ctrl Pts',(-19.0550398152044,43.5697807368771,122.258927424476)) ;
#24661 = CARTESIAN_POINT('Ctrl Pts',(-18.9664691272905,43.3897916565143,121.970708884775)) ;
#24662 = CARTESIAN_POINT('Ctrl Pts',(-19.2591461901148,43.5797081699987,122.215302018421)) ;
#24663 = CARTESIAN_POINT('Ctrl Pts',(-19.2216018609428,43.3997190896358,121.916174470016)) ;
#24664 = CARTESIAN_POINT('Ctrl Pts',(-19.4681756382475,43.5896581624049,122.207163663793)) ;
#24665 = CARTESIAN_POINT('Ctrl Pts',(-19.4828888562582,43.4096690820421,121.905998966867)) ;
#24666 = CARTESIAN_POINT('Ctrl Pts',(-19.6775616742312,43.5997133634789,122.236109466576)) ;
#24667 = CARTESIAN_POINT('Ctrl Pts',(-19.7446216548047,43.4197242831161,121.942178613796)) ;
#24668 = CARTESIAN_POINT('Ctrl Pts',(-19.874223881596,43.6095356375312,122.299123887037)) ;
#24669 = CARTESIAN_POINT('Ctrl Pts',(-19.9904509322207,43.4295465571684,122.02094445218)) ;
#24670 = CARTESIAN_POINT('Ctrl Pts',(-20.0614519230175,43.6195915314905,122.397267586826)) ;
#24671 = CARTESIAN_POINT('Ctrl Pts',(-20.2244870380784,43.4396024511276,122.143621831466)) ;
#24672 = CARTESIAN_POINT('Ctrl Pts',(-20.2266685259505,43.6295322533356,122.525258130833)) ;
#24673 = CARTESIAN_POINT('Ctrl Pts',(-20.4310096168158,43.4495431729727,122.303608199071)) ;
#24674 = CARTESIAN_POINT('Ctrl Pts',(-20.3671176125788,43.6394365974222,122.678983059671)) ;
#24675 = CARTESIAN_POINT('Ctrl Pts',(-20.6065731184016,43.4594475170593,122.495763120482)) ;
#24676 = CARTESIAN_POINT('Ctrl Pts',(-20.4802208408433,43.6494832647217,122.857339300403)) ;
#24677 = CARTESIAN_POINT('Ctrl Pts',(-20.7479541652507,43.4694941843588,122.718707024721)) ;
#24678 = CARTESIAN_POINT('Ctrl Pts',(-20.5596229425746,43.6593788231716,123.049662217343)) ;
#24679 = CARTESIAN_POINT('Ctrl Pts',(-20.8472092355886,43.4793897428087,122.95911028977)) ;
#24680 = CARTESIAN_POINT('Ctrl Pts',(-20.6051653987093,43.6694409018763,123.256207404328)) ;
#24681 = CARTESIAN_POINT('Ctrl Pts',(-20.904139618028,43.4894518215134,123.217291078424)) ;
#24682 = CARTESIAN_POINT('Ctrl Pts',(-20.614077706757,43.6792836003421,123.462962817774)) ;
#24683 = CARTESIAN_POINT('Ctrl Pts',(-20.9152824166523,43.4992945199792,123.475736104278)) ;
#24684 = CARTESIAN_POINT('Ctrl Pts',(-20.587046897207,43.6892743742365,123.671227339976)) ;
#24685 = CARTESIAN_POINT('Ctrl Pts',(-20.8814961280243,43.5092852938737,123.736067222342)) ;
#24686 = CARTESIAN_POINT('Ctrl Pts',(-20.5246153399661,43.6992022434715,123.870395640026)) ;
#24687 = CARTESIAN_POINT('Ctrl Pts',(-20.8034587033046,43.5192131631086,123.985028739388)) ;
#24688 = CARTESIAN_POINT('Ctrl Pts',(-20.4282901507528,43.7091909724413,124.0570066794)) ;
#24689 = CARTESIAN_POINT('Ctrl Pts',(-20.6830540646815,43.5292018920784,124.218293703487)) ;
#24690 = CARTESIAN_POINT('Ctrl Pts',(-20.300083088921,43.7192303744251,124.224651641945)) ;
#24691 = CARTESIAN_POINT('Ctrl Pts',(-20.5227971110946,43.5392412940622,124.427851205494)) ;
#24692 = CARTESIAN_POINT('Ctrl Pts',(-20.1480587442798,43.7290705421618,124.364969335422)) ;
#24693 = CARTESIAN_POINT('Ctrl Pts',(-20.3327674227349,43.549081461799,124.603250592089)) ;
#24694 = CARTESIAN_POINT('Ctrl Pts',(-19.9704841404498,43.7391187525363,124.479372090359)) ;
#24695 = CARTESIAN_POINT('Ctrl Pts',(-20.1108004287422,43.5591296721735,124.746255706704)) ;
#24696 = CARTESIAN_POINT('Ctrl Pts',(-19.7775615457972,43.7490659228241,124.560080673461)) ;
#24697 = CARTESIAN_POINT('Ctrl Pts',(-19.8696476488821,43.5690768424612,124.84714360705)) ;
#24698 = CARTESIAN_POINT('Ctrl Pts',(-19.5744358323149,43.7589767710792,124.606507407475)) ;
#24699 = CARTESIAN_POINT('Ctrl Pts',(-19.6157403076391,43.5789876907163,124.905179129313)) ;
#24700 = CARTESIAN_POINT('Ctrl Pts',(-19.3632888752703,43.7690330987569,124.616913341482)) ;
#24701 = CARTESIAN_POINT('Ctrl Pts',(-19.3518069355752,43.5890440183941,124.91818859538)) ;
#24702 = CARTESIAN_POINT('Ctrl Pts',(-19.1577934192907,43.7788835115255,124.591215482131)) ;
#24703 = CARTESIAN_POINT('Ctrl Pts',(-19.0949363387433,43.5988944311626,124.886068138014)) ;
#24704 = CARTESIAN_POINT('Ctrl Pts',(-18.9561968908211,43.7889103973592,124.529628376844)) ;
#24705 = CARTESIAN_POINT('Ctrl Pts',(-18.8429401699179,43.6089213169963,124.809086046414)) ;
#24706 = CARTESIAN_POINT('Ctrl Pts',(-18.7685615510423,43.79893901299,124.433463237905)) ;
#24707 = CARTESIAN_POINT('Ctrl Pts',(-18.608395133658,43.6189499326271,124.688881455388)) ;
#24708 = CARTESIAN_POINT('Ctrl Pts',(-18.6033288718835,43.8087842363675,124.30883132978)) ;
#24709 = CARTESIAN_POINT('Ctrl Pts',(-18.4018522456686,43.6287951560046,124.53309241998)) ;
#24710 = CARTESIAN_POINT('Ctrl Pts',(-18.4597378892454,43.8187749184691,124.155537858628)) ;
#24711 = CARTESIAN_POINT('Ctrl Pts',(-18.2223621198309,43.6387858381062,124.34147662207)) ;
#24712 = CARTESIAN_POINT('Ctrl Pts',(-18.3448008532577,43.8288128071015,123.978559187435)) ;
#24713 = CARTESIAN_POINT('Ctrl Pts',(-18.0786893213183,43.6488237267386,124.120254417819)) ;
#24714 = CARTESIAN_POINT('Ctrl Pts',(-18.2635921715876,43.8386571422047,123.78819018194)) ;
#24715 = CARTESIAN_POINT('Ctrl Pts',(-17.977176387725,43.6586680618418,123.882292776737)) ;
#24716 = CARTESIAN_POINT('Ctrl Pts',(-18.2156072803135,43.8486421044022,123.583862375105)) ;
#24717 = CARTESIAN_POINT('Ctrl Pts',(-17.917193628408,43.6686530240393,123.626883148383)) ;
#24718 = CARTESIAN_POINT('Ctrl Pts',(-18.2037829776996,43.8585810459356,123.375218987753)) ;
#24719 = CARTESIAN_POINT('Ctrl Pts',(-17.9024116244684,43.6785919655727,123.366078461576)) ;
#24720 = CARTESIAN_POINT('Ctrl Pts',(-18.2286806326614,43.868622930907,123.165600430253)) ;
#24721 = CARTESIAN_POINT('Ctrl Pts',(-17.9335320666697,43.6886338505441,123.104055220491)) ;
#24722 = CARTESIAN_POINT('Ctrl Pts',(-18.2885381500914,43.8785094788153,122.96653880576)) ;
#24723 = CARTESIAN_POINT('Ctrl Pts',(-18.008352723709,43.6985203984524,122.855226846736)) ;
#24724 = CARTESIAN_POINT('Ctrl Pts',(-18.3827677761836,43.8885034043153,122.778780845212)) ;
#24725 = CARTESIAN_POINT('Ctrl Pts',(-18.1261385188554,43.7085143239524,122.620528575572)) ;
#24726 = CARTESIAN_POINT('Ctrl Pts',(-18.507397260208,43.8984394954417,122.611106118602)) ;
#24727 = CARTESIAN_POINT('Ctrl Pts',(-18.2819245676956,43.7184504150789,122.410933846051)) ;
#24728 = CARTESIAN_POINT('Ctrl Pts',(-18.6606561201383,43.9084687644217,122.466343302757)) ;
#24729 = CARTESIAN_POINT('Ctrl Pts',(-18.4734970875813,43.7284796840588,122.229979319978)) ;
#24730 = CARTESIAN_POINT('Ctrl Pts',(-18.8340470507955,43.918351146981,122.351835718989)) ;
#24731 = CARTESIAN_POINT('Ctrl Pts',(-18.6902358432055,43.7383620666181,122.086843147979)) ;
#24732 = CARTESIAN_POINT('Ctrl Pts',(-19.0278824329128,43.9284036640689,122.267711760247)) ;
#24733 = CARTESIAN_POINT('Ctrl Pts',(-18.9325293093004,43.748414583706,121.981687073779)) ;
#24734 = CARTESIAN_POINT('Ctrl Pts',(-19.2301849856646,43.9382977848928,122.219177390576)) ;
#24735 = CARTESIAN_POINT('Ctrl Pts',(-19.1854080916355,43.7583087045299,121.921017634688)) ;
#24736 = CARTESIAN_POINT('Ctrl Pts',(-19.441298301709,43.9483597643132,122.206244667768)) ;
#24737 = CARTESIAN_POINT('Ctrl Pts',(-19.4492993318414,43.7683706839503,121.904850471576)) ;
#24738 = CARTESIAN_POINT('Ctrl Pts',(-19.6469435683342,43.9582042975421,122.229626514128)) ;
#24739 = CARTESIAN_POINT('Ctrl Pts',(-19.7063573702631,43.7782152171792,121.934076663056)) ;
#24740 = CARTESIAN_POINT('Ctrl Pts',(-19.8479372841435,43.9681643764484,122.288322728641)) ;
#24741 = CARTESIAN_POINT('Ctrl Pts',(-19.9576002327423,43.7881752960855,122.007446102476)) ;
#24742 = CARTESIAN_POINT('Ctrl Pts',(-20.0369708079469,43.978202653021,122.38212312448)) ;
#24743 = CARTESIAN_POINT('Ctrl Pts',(-20.1938925036668,43.7982135726581,122.124695495129)) ;
#24744 = CARTESIAN_POINT('Ctrl Pts',(-20.2043238205213,43.9880760395588,122.504967849574)) ;
#24745 = CARTESIAN_POINT('Ctrl Pts',(-20.403085266942,43.8080869591959,122.278251260109)) ;
#24746 = CARTESIAN_POINT('Ctrl Pts',(-20.3506106823668,43.9981489823259,122.658028324524)) ;
#24747 = CARTESIAN_POINT('Ctrl Pts',(-20.5859442921562,43.818159901963,122.469575837394)) ;
#24748 = CARTESIAN_POINT('Ctrl Pts',(-20.465419038605,44.0079703964542,122.82969122843)) ;
#24749 = CARTESIAN_POINT('Ctrl Pts',(-20.7294563688574,43.8279813160913,122.684155238316)) ;
#24750 = CARTESIAN_POINT('Ctrl Pts',(-20.5510249351871,44.0180450265265,123.023378752783)) ;
#24751 = CARTESIAN_POINT('Ctrl Pts',(-20.8364643232835,43.8380559461636,122.926263897482)) ;
#24752 = CARTESIAN_POINT('Ctrl Pts',(-20.6005844279953,44.0279116638434,123.224825343159)) ;
#24753 = CARTESIAN_POINT('Ctrl Pts',(-20.8984148212984,43.8479225834805,123.178073112069)) ;
#24754 = CARTESIAN_POINT('Ctrl Pts',(-20.6151706977744,44.0379352092152,123.435036739168)) ;
#24755 = CARTESIAN_POINT('Ctrl Pts',(-20.9166483132866,43.8579461288523,123.440837266538)) ;
#24756 = CARTESIAN_POINT('Ctrl Pts',(-20.5925229977775,44.0479609607324,123.644602262895)) ;
#24757 = CARTESIAN_POINT('Ctrl Pts',(-20.8883395523817,43.8679718803695,123.702794177763)) ;
#24758 = CARTESIAN_POINT('Ctrl Pts',(-20.5351790535078,44.0578145477417,123.843648615532)) ;
#24759 = CARTESIAN_POINT('Ctrl Pts',(-20.8166599479504,43.8778254673789,123.951603594725)) ;
#24760 = CARTESIAN_POINT('Ctrl Pts',(-20.4434995838773,44.0677915079697,124.032303037785)) ;
#24761 = CARTESIAN_POINT('Ctrl Pts',(-20.702060923653,43.8878024276068,124.187422142841)) ;
#24762 = CARTESIAN_POINT('Ctrl Pts',(-20.3196315257472,44.0778126509981,124.202704231129)) ;
#24763 = CARTESIAN_POINT('Ctrl Pts',(-20.5472263847729,43.8978235706353,124.400424003541)) ;
#24764 = CARTESIAN_POINT('Ctrl Pts',(-20.1704166426939,44.0876952570181,124.347313905858)) ;
#24765 = CARTESIAN_POINT('Ctrl Pts',(-20.3607073265626,43.9077061766552,124.581187205771)) ;
#24766 = CARTESIAN_POINT('Ctrl Pts',(-19.9951290913081,44.0977637276508,124.465904961827)) ;
#24767 = CARTESIAN_POINT('Ctrl Pts',(-20.141598516524,43.9177746472879,124.729426223139)) ;
#24768 = CARTESIAN_POINT('Ctrl Pts',(-19.8065219734023,44.1075938108345,124.550461991308)) ;
#24769 = CARTESIAN_POINT('Ctrl Pts',(-19.9058383854937,43.9276047304716,124.835123522503)) ;
#24770 = CARTESIAN_POINT('Ctrl Pts',(-19.6014110884651,44.1176603705148,124.602451546472)) ;
#24771 = CARTESIAN_POINT('Ctrl Pts',(-19.6494502413749,43.937671290152,124.900110672069)) ;
#24772 = CARTESIAN_POINT('Ctrl Pts',(-19.3940171097119,44.1275506203441,124.617639758843)) ;
#24773 = CARTESIAN_POINT('Ctrl Pts',(-19.3902067493444,43.9475615399812,124.919096378298)) ;
#24774 = CARTESIAN_POINT('Ctrl Pts',(-19.1849952546928,44.1375427860929,124.596831802444)) ;
#24775 = CARTESIAN_POINT('Ctrl Pts',(-19.1289291993489,43.95755370573,124.893086593962)) ;
#24776 = CARTESIAN_POINT('Ctrl Pts',(-18.9834025895948,44.147505629689,124.540019916616)) ;
#24777 = CARTESIAN_POINT('Ctrl Pts',(-18.8769378575391,43.9675165493261,124.822071866951)) ;
#24778 = CARTESIAN_POINT('Ctrl Pts',(-18.7955966982782,44.1574097985167,124.450071701931)) ;
#24779 = CARTESIAN_POINT('Ctrl Pts',(-18.6421796236828,43.9774207181539,124.709636238937)) ;
#24780 = CARTESIAN_POINT('Ctrl Pts',(-18.6237306354897,44.1674706734111,124.326834768521)) ;
#24781 = CARTESIAN_POINT('Ctrl Pts',(-18.4273472596352,43.9874815930482,124.555590382771)) ;
#24782 = CARTESIAN_POINT('Ctrl Pts',(-18.4788866563946,44.1773095767404,124.179124043168)) ;
#24783 = CARTESIAN_POINT('Ctrl Pts',(-18.2462912417937,43.9973204963776,124.370950929424)) ;
#24784 = CARTESIAN_POINT('Ctrl Pts',(-18.3590318669185,44.1873779531143,124.004699120229)) ;
#24785 = CARTESIAN_POINT('Ctrl Pts',(-18.096473040413,44.0073888727515,124.152920066805)) ;
#24786 = CARTESIAN_POINT('Ctrl Pts',(-18.2729573990922,44.197258569747,123.815617005926)) ;
#24787 = CARTESIAN_POINT('Ctrl Pts',(-17.9888795242822,44.0172694893841,123.916566377132)) ;
#24788 = CARTESIAN_POINT('Ctrl Pts',(-18.2200454094595,44.207249729976,123.612376766819)) ;
#24789 = CARTESIAN_POINT('Ctrl Pts',(-17.9227396809683,44.0272606496131,123.662515814642)) ;
#24790 = CARTESIAN_POINT('Ctrl Pts',(-18.2032518304312,44.2172028034081,123.403775478978)) ;
#24791 = CARTESIAN_POINT('Ctrl Pts',(-17.9017478866056,44.0372137230452,123.40176367561)) ;
#24792 = CARTESIAN_POINT('Ctrl Pts',(-18.2231612060629,44.2272386390207,123.19374932302)) ;
#24793 = CARTESIAN_POINT('Ctrl Pts',(-17.9266347799871,44.0472495586578,123.139231148737)) ;
#24794 = CARTESIAN_POINT('Ctrl Pts',(-18.2782926365655,44.2371287657509,122.993256824972)) ;
#24795 = CARTESIAN_POINT('Ctrl Pts',(-17.9955495886584,44.057139685388,122.888614558069)) ;
#24796 = CARTESIAN_POINT('Ctrl Pts',(-18.368002893643,44.2471209475202,122.803320931818)) ;
#24797 = CARTESIAN_POINT('Ctrl Pts',(-18.1076878440328,44.0671318671573,122.651194666647)) ;
#24798 = CARTESIAN_POINT('Ctrl Pts',(-18.4888319440295,44.2570668874946,122.632672480447)) ;
#24799 = CARTESIAN_POINT('Ctrl Pts',(-18.2587247866769,44.0770778071318,122.437883820146)) ;
#24800 = CARTESIAN_POINT('Ctrl Pts',(-18.6371833756394,44.2670140712541,122.485268515715)) ;
#24801 = CARTESIAN_POINT('Ctrl Pts',(-18.4441648499972,44.0870249908912,122.253628827194)) ;
#24802 = CARTESIAN_POINT('Ctrl Pts',(-18.810735082372,44.2770620095444,122.364857154366)) ;
#24803 = CARTESIAN_POINT('Ctrl Pts',(-18.6611045195494,44.0970729291816,122.103115117568)) ;
#24804 = CARTESIAN_POINT('Ctrl Pts',(-18.9986676053786,44.286909644358,122.278010090229)) ;
#24805 = CARTESIAN_POINT('Ctrl Pts',(-18.8960216519544,44.1069205639951,121.9945561486)) ;
#24806 = CARTESIAN_POINT('Ctrl Pts',(-19.2009643648431,44.296871358056,122.223868979964)) ;
#24807 = CARTESIAN_POINT('Ctrl Pts',(-19.1488932353645,44.1168822776931,121.926880369107)) ;
#24808 = CARTESIAN_POINT('Ctrl Pts',(-19.4110368321455,44.3068999938771,122.205817721847)) ;
#24809 = CARTESIAN_POINT('Ctrl Pts',(-19.4114837782062,44.1269109135143,121.904316948058)) ;
#24810 = CARTESIAN_POINT('Ctrl Pts',(-19.6185576126464,44.3168103086289,122.224226084689)) ;
#24811 = CARTESIAN_POINT('Ctrl Pts',(-19.6708855677709,44.136821228266,121.927328148373)) ;
#24812 = CARTESIAN_POINT('Ctrl Pts',(-19.8203871123028,44.3267451792916,122.277995841482)) ;
#24813 = CARTESIAN_POINT('Ctrl Pts',(-19.923172854028,44.1467560989287,121.994541369525)) ;
#24814 = CARTESIAN_POINT('Ctrl Pts',(-20.0117417687553,44.3367863616933,122.367111250582)) ;
#24815 = CARTESIAN_POINT('Ctrl Pts',(-20.1623656622643,44.1567972813305,122.105936279633)) ;
#24816 = CARTESIAN_POINT('Ctrl Pts',(-20.182178194294,44.3466733331581,122.48611803753)) ;
#24817 = CARTESIAN_POINT('Ctrl Pts',(-20.3754115587803,44.1666842527952,122.254696080828)) ;
#24818 = CARTESIAN_POINT('Ctrl Pts',(-20.3311931711049,44.3566727654207,122.634359060664)) ;
#24819 = CARTESIAN_POINT('Ctrl Pts',(-20.5616797006254,44.1766836850578,122.439998156239)) ;
#24820 = CARTESIAN_POINT('Ctrl Pts',(-20.4513895888392,44.3665928306773,122.804819406772)) ;
#24821 = CARTESIAN_POINT('Ctrl Pts',(-20.7119248209942,44.1866037503144,122.653074790023)) ;
#24822 = CARTESIAN_POINT('Ctrl Pts',(-20.5412304164301,44.3766296832615,122.995731464311)) ;
#24823 = CARTESIAN_POINT('Ctrl Pts',(-20.8242248480084,44.1966406028986,122.89171516179)) ;
#24824 = CARTESIAN_POINT('Ctrl Pts',(-20.5958716500195,44.3865423426014,123.196839523156)) ;
#24825 = CARTESIAN_POINT('Ctrl Pts',(-20.8925256088344,44.2065532622386,123.143101297578)) ;
#24826 = CARTESIAN_POINT('Ctrl Pts',(-20.6153694128764,44.3965335545164,123.405991946571)) ;
#24827 = CARTESIAN_POINT('Ctrl Pts',(-20.9168966357386,44.2165444741535,123.404542148438)) ;
#24828 = CARTESIAN_POINT('Ctrl Pts',(-20.5976979683511,44.4065751959195,123.616341273831)) ;
#24829 = CARTESIAN_POINT('Ctrl Pts',(-20.8948063197256,44.2265861155566,123.667478543077)) ;
#24830 = CARTESIAN_POINT('Ctrl Pts',(-20.54540602134,44.4164039901265,123.816275966712)) ;
#24831 = CARTESIAN_POINT('Ctrl Pts',(-20.8294398407361,44.2364149097636,123.917397995982)) ;
#24832 = CARTESIAN_POINT('Ctrl Pts',(-20.4571322193429,44.4264804012478,124.008799381337)) ;
#24833 = CARTESIAN_POINT('Ctrl Pts',(-20.7190966284838,44.2464913208849,124.158051348321)) ;
#24834 = CARTESIAN_POINT('Ctrl Pts',(-20.3394898621036,44.4363325342902,124.179323371872)) ;
#24835 = CARTESIAN_POINT('Ctrl Pts',(-20.5720419186679,44.2563434539274,124.371206621261)) ;
#24836 = CARTESIAN_POINT('Ctrl Pts',(-20.1909447204641,44.4464057686315,124.330210550994)) ;
#24837 = CARTESIAN_POINT('Ctrl Pts',(-20.3863598082827,44.2664166882687,124.559814357932)) ;
#24838 = CARTESIAN_POINT('Ctrl Pts',(-20.0223534222565,44.4562472699582,124.450168274092)) ;
#24839 = CARTESIAN_POINT('Ctrl Pts',(-20.1756188492781,44.2762581895953,124.709761183194)) ;
#24840 = CARTESIAN_POINT('Ctrl Pts',(-19.8335848822427,44.466208221553,124.540812132209)) ;
#24841 = CARTESIAN_POINT('Ctrl Pts',(-19.9396571120249,44.2862191411901,124.823064731638)) ;
#24842 = CARTESIAN_POINT('Ctrl Pts',(-19.6302748014164,44.4762460392736,124.597332076024)) ;
#24843 = CARTESIAN_POINT('Ctrl Pts',(-19.6855192485354,44.2962569589108,124.893713217866)) ;
#24844 = CARTESIAN_POINT('Ctrl Pts',(-19.4236658402343,44.4861203885307,124.617747552604)) ;
#24845 = CARTESIAN_POINT('Ctrl Pts',(-19.4272568805915,44.3061313081678,124.919231077549)) ;
#24846 = CARTESIAN_POINT('Ctrl Pts',(-19.2126136916866,44.4961899392729,124.601657803566)) ;
#24847 = CARTESIAN_POINT('Ctrl Pts',(-19.1634421663118,44.31620085891,124.899117334135)) ;
#24848 = CARTESIAN_POINT('Ctrl Pts',(-19.0122816584332,44.5060239587815,124.550498030164)) ;
#24849 = CARTESIAN_POINT('Ctrl Pts',(-18.9130262792897,44.3260348784186,124.835165719918)) ;
#24850 = CARTESIAN_POINT('Ctrl Pts',(-18.8198408604291,44.516058113361,124.464118183293)) ;
#24851 = CARTESIAN_POINT('Ctrl Pts',(-18.6724761256092,44.3360690329981,124.727189304434)) ;
#24852 = CARTESIAN_POINT('Ctrl Pts',(-18.6459125382961,44.5260740391835,124.345407050209)) ;
#24853 = CARTESIAN_POINT('Ctrl Pts',(-18.4550666358706,44.3460849588206,124.578799029693)) ;
#24854 = CARTESIAN_POINT('Ctrl Pts',(-18.4969953236926,44.5359562943777,124.200536328678)) ;
#24855 = CARTESIAN_POINT('Ctrl Pts',(-18.2689206934433,44.3559672140149,124.397708730824)) ;
#24856 = CARTESIAN_POINT('Ctrl Pts',(-18.3739888329453,44.5459451008887,124.030365635577)) ;
#24857 = CARTESIAN_POINT('Ctrl Pts',(-18.1151639542311,44.3659560205258,124.184994122571)) ;
#24858 = CARTESIAN_POINT('Ctrl Pts',(-18.2825994603111,44.5558936681514,123.842202089097)) ;
#24859 = CARTESIAN_POINT('Ctrl Pts',(-18.0009287364672,44.3759045877885,123.949788452977)) ;
#24860 = CARTESIAN_POINT('Ctrl Pts',(-18.2248894304791,44.5659484734534,123.638872201841)) ;
#24861 = CARTESIAN_POINT('Ctrl Pts',(-17.9287930124207,44.3859593930905,123.695625807384)) ;
#24862 = CARTESIAN_POINT('Ctrl Pts',(-18.2035656681982,44.575767256717,123.433544830677)) ;
#24863 = CARTESIAN_POINT('Ctrl Pts',(-17.9021400804517,44.3957781763541,123.438965134921)) ;
#24864 = CARTESIAN_POINT('Ctrl Pts',(-18.2179757066852,44.5858030290775,123.223058832807)) ;
#24865 = CARTESIAN_POINT('Ctrl Pts',(-17.9201546965115,44.4058139487147,123.175857889878)) ;
#24866 = CARTESIAN_POINT('Ctrl Pts',(-18.2692459499617,44.5958277281062,123.018631696878)) ;
#24867 = CARTESIAN_POINT('Ctrl Pts',(-17.9842443392215,44.4158386477433,122.920324456169)) ;
#24868 = CARTESIAN_POINT('Ctrl Pts',(-18.3533314311282,44.6056797313652,122.829344467355)) ;
#24869 = CARTESIAN_POINT('Ctrl Pts',(-18.0893534627256,44.4256906510024,122.683715321304)) ;
#24870 = CARTESIAN_POINT('Ctrl Pts',(-18.4703557315628,44.6156706657625,122.65495463514)) ;
#24871 = CARTESIAN_POINT('Ctrl Pts',(-18.2356357013134,44.4356815853996,122.46572907487)) ;
#24872 = CARTESIAN_POINT('Ctrl Pts',(-18.6147549951052,44.6255885881936,122.504508089155)) ;
#24873 = CARTESIAN_POINT('Ctrl Pts',(-18.41613673709,44.4455995078307,122.277671975149)) ;
#24874 = CARTESIAN_POINT('Ctrl Pts',(-18.7848954850902,44.6356169438759,122.380036959605)) ;
#24875 = CARTESIAN_POINT('Ctrl Pts',(-18.6288136047377,44.455627863513,122.122084840499)) ;
#24876 = CARTESIAN_POINT('Ctrl Pts',(-18.9713236852492,44.6455012283865,122.288233366533)) ;
#24877 = CARTESIAN_POINT('Ctrl Pts',(-18.8618504936233,44.4655121480236,122.007331995514)) ;
#24878 = CARTESIAN_POINT('Ctrl Pts',(-19.1729084480282,44.6554939122944,122.229103541019)) ;
#24879 = CARTESIAN_POINT('Ctrl Pts',(-19.1138322342733,44.4755048319315,121.933421901147)) ;
#24880 = CARTESIAN_POINT('Ctrl Pts',(-19.382493485015,44.6655226493021,122.206156839358)) ;
#24881 = CARTESIAN_POINT('Ctrl Pts',(-19.3758137501504,44.4855335689392,121.904740742867)) ;
#24882 = CARTESIAN_POINT('Ctrl Pts',(-19.5898954585969,44.675408045931,122.219478540037)) ;
#24883 = CARTESIAN_POINT('Ctrl Pts',(-19.6350667634332,44.4954189655681,121.921395206069)) ;
#24884 = CARTESIAN_POINT('Ctrl Pts',(-19.793970597842,44.6853959313449,122.268821405339)) ;
#24885 = CARTESIAN_POINT('Ctrl Pts',(-19.8901602887943,44.505406850982,121.983076127047)) ;
#24886 = CARTESIAN_POINT('Ctrl Pts',(-19.9857471745296,44.6953466340055,122.352468749605)) ;
#24887 = CARTESIAN_POINT('Ctrl Pts',(-20.1298803582596,44.5153575536426,122.087637628189)) ;
#24888 = CARTESIAN_POINT('Ctrl Pts',(-20.1615504334524,44.7053869521029,122.469253001426)) ;
#24889 = CARTESIAN_POINT('Ctrl Pts',(-20.3496330623717,44.52539787174,122.233619868658)) ;
#24890 = CARTESIAN_POINT('Ctrl Pts',(-20.3120561281735,44.7152615174361,122.612267502799)) ;
#24891 = CARTESIAN_POINT('Ctrl Pts',(-20.5377640234238,44.5352724370732,122.412390214829)) ;
#24892 = CARTESIAN_POINT('Ctrl Pts',(-20.4371874370457,44.7252611774972,122.78115208881)) ;
#24893 = CARTESIAN_POINT('Ctrl Pts',(-20.6941762400211,44.5452720971343,122.62349750357)) ;
#24894 = CARTESIAN_POINT('Ctrl Pts',(-20.5304535414409,44.7351701726649,122.967466993672)) ;
#24895 = CARTESIAN_POINT('Ctrl Pts',(-20.8107568463258,44.555181092302,122.856392682696)) ;
#24896 = CARTESIAN_POINT('Ctrl Pts',(-20.5907433449701,44.7452249138281,123.170033529265)) ;
#24897 = CARTESIAN_POINT('Ctrl Pts',(-20.8861166779856,44.5652358334653,123.109601455861)) ;
#24898 = CARTESIAN_POINT('Ctrl Pts',(-20.6147190095158,44.7550835257419,123.375937676543)) ;
#24899 = CARTESIAN_POINT('Ctrl Pts',(-20.9160838152059,44.5750944453791,123.36698258296)) ;
#24900 = CARTESIAN_POINT('Ctrl Pts',(-20.60245263379,44.7651516480213,123.587214744072)) ;
#24901 = CARTESIAN_POINT('Ctrl Pts',(-20.9007482951995,44.5851625676584,123.631078613714)) ;
#24902 = CARTESIAN_POINT('Ctrl Pts',(-20.5546908139825,44.7750071187245,123.788845425538)) ;
#24903 = CARTESIAN_POINT('Ctrl Pts',(-20.8410433869187,44.5950180383616,123.883116987979)) ;
#24904 = CARTESIAN_POINT('Ctrl Pts',(-20.4720727117349,44.7850019782178,123.9820375159)) ;
#24905 = CARTESIAN_POINT('Ctrl Pts',(-20.737768269546,44.605012897855,124.124606144448)) ;
#24906 = CARTESIAN_POINT('Ctrl Pts',(-20.3563607572283,44.7950332315598,124.158351468293)) ;
#24907 = CARTESIAN_POINT('Ctrl Pts',(-20.5931261612872,44.6150441511969,124.344997164701)) ;
#24908 = CARTESIAN_POINT('Ctrl Pts',(-20.2144020973158,44.8048999304329,124.309603441992)) ;
#24909 = CARTESIAN_POINT('Ctrl Pts',(-20.4156755541826,44.62491085007,124.534060702266)) ;
#24910 = CARTESIAN_POINT('Ctrl Pts',(-20.0465467747764,44.8148867461841,124.435681086058)) ;
#24911 = CARTESIAN_POINT('Ctrl Pts',(-20.2058546846897,44.6348976658212,124.691655677439)) ;
#24912 = CARTESIAN_POINT('Ctrl Pts',(-19.8600899400834,44.8248339513795,124.530430266587)) ;
#24913 = CARTESIAN_POINT('Ctrl Pts',(-19.9727822075021,44.6448448710167,124.810089850081)) ;
#24914 = CARTESIAN_POINT('Ctrl Pts',(-19.6581014765466,44.8348769395058,124.591850093754)) ;
#24915 = CARTESIAN_POINT('Ctrl Pts',(-19.7202958616412,44.6548878591429,124.886862052342)) ;
#24916 = CARTESIAN_POINT('Ctrl Pts',(-19.4521749099809,44.8447442941273,124.616945312236)) ;
#24917 = CARTESIAN_POINT('Ctrl Pts',(-19.4628869098935,44.6647552137644,124.91822843966)) ;
#24918 = CARTESIAN_POINT('Ctrl Pts',(-19.242936933169,44.8547101874254,124.606358445387)) ;
#24919 = CARTESIAN_POINT('Ctrl Pts',(-19.201339436511,44.6747211070625,124.904992081208)) ;
#24920 = CARTESIAN_POINT('Ctrl Pts',(-19.0375566117157,44.8647339648015,124.559112347747)) ;
#24921 = CARTESIAN_POINT('Ctrl Pts',(-18.9446146117008,44.6847448844386,124.845931776589)) ;
#24922 = CARTESIAN_POINT('Ctrl Pts',(-18.8454040569223,44.8746595127332,124.477781348015)) ;
#24923 = CARTESIAN_POINT('Ctrl Pts',(-18.7044247703961,44.6946704323703,124.744265398415)) ;
#24924 = CARTESIAN_POINT('Ctrl Pts',(-18.6697413624025,44.8845999891542,124.364553604711)) ;
#24925 = CARTESIAN_POINT('Ctrl Pts',(-18.4848477732278,44.7046109087913,124.602728279973)) ;
#24926 = CARTESIAN_POINT('Ctrl Pts',(-18.5149584063942,44.8946461988171,124.220874734381)) ;
#24927 = CARTESIAN_POINT('Ctrl Pts',(-18.2913709521149,44.7146571184542,124.423127645142)) ;
#24928 = CARTESIAN_POINT('Ctrl Pts',(-18.3896255165691,44.9045074554789,124.055712470621)) ;
#24929 = CARTESIAN_POINT('Ctrl Pts',(-18.1347068986328,44.724518375116,124.216672914137)) ;
#24930 = CARTESIAN_POINT('Ctrl Pts',(-18.2933036607311,44.9145010837542,123.869030082729)) ;
#24931 = CARTESIAN_POINT('Ctrl Pts',(-18.0143070451238,44.7345120033913,123.983318570089)) ;
#24932 = CARTESIAN_POINT('Ctrl Pts',(-18.2311629194592,44.9244264810644,123.669801758037)) ;
#24933 = CARTESIAN_POINT('Ctrl Pts',(-17.936633762989,44.7444374007015,123.734282199344)) ;
#24934 = CARTESIAN_POINT('Ctrl Pts',(-18.2042856489682,44.9344543889746,123.46073131352)) ;
#24935 = CARTESIAN_POINT('Ctrl Pts',(-17.9030399617659,44.7544653086117,123.472943722699)) ;
#24936 = CARTESIAN_POINT('Ctrl Pts',(-18.2137679240456,44.9443407046438,123.253075539075)) ;
#24937 = CARTESIAN_POINT('Ctrl Pts',(-17.9148956263581,44.7643516242809,123.213374011942)) ;
#24938 = CARTESIAN_POINT('Ctrl Pts',(-18.2597049737886,44.9543722995476,123.047278072271)) ;
#24939 = CARTESIAN_POINT('Ctrl Pts',(-17.9723197114155,44.7743832191847,122.95612772885)) ;
#24940 = CARTESIAN_POINT('Ctrl Pts',(-18.339321156955,44.9642545424993,122.855346311805)) ;
#24941 = CARTESIAN_POINT('Ctrl Pts',(-18.0718425713874,44.7842654621364,122.716214046185)) ;
#24942 = CARTESIAN_POINT('Ctrl Pts',(-18.4529511231331,44.9743140135291,122.677012970206)) ;
#24943 = CARTESIAN_POINT('Ctrl Pts',(-18.2138824565932,44.7943249331663,122.493298818431)) ;
#24944 = CARTESIAN_POINT('Ctrl Pts',(-18.5931221037197,44.9841804581923,122.524103073492)) ;
#24945 = CARTESIAN_POINT('Ctrl Pts',(-18.3890982744024,44.8041913778294,122.302163339125)) ;
#24946 = CARTESIAN_POINT('Ctrl Pts',(-18.7589604520614,44.994146582641,122.3960648915)) ;
#24947 = CARTESIAN_POINT('Ctrl Pts',(-18.5963979569655,44.8141575022781,122.142117824611)) ;
#24948 = CARTESIAN_POINT('Ctrl Pts',(-18.9458650964473,45.0041768260321,122.298439068355)) ;
#24949 = CARTESIAN_POINT('Ctrl Pts',(-18.8300300927451,44.8241877456692,122.020087986119)) ;
#24950 = CARTESIAN_POINT('Ctrl Pts',(-19.1440629077566,45.0140698609852,122.235330723378)) ;
#24951 = CARTESIAN_POINT('Ctrl Pts',(-19.0777784031114,44.8340807806223,121.941205272921)) ;
#24952 = CARTESIAN_POINT('Ctrl Pts',(-19.3534531145185,45.024120775222,122.207100463021)) ;
#24953 = CARTESIAN_POINT('Ctrl Pts',(-19.3395157430304,44.8441316948591,121.905920090679)) ;
#24954 = CARTESIAN_POINT('Ctrl Pts',(-19.5612049836232,45.0340106014466,122.215495999718)) ;
#24955 = CARTESIAN_POINT('Ctrl Pts',(-19.5992088007417,44.8540215210837,121.916417743617)) ;
#24956 = CARTESIAN_POINT('Ctrl Pts',(-19.8352568409963,45.0473454164935,122.274745540189)) ;
#24957 = CARTESIAN_POINT('Ctrl Pts',(-19.9417558495349,44.8673563361306,121.990481112151)) ;
#24958 = CARTESIAN_POINT('Ctrl Pts',(-20.0861970248156,45.060622507665,122.404050574181)) ;
#24959 = CARTESIAN_POINT('Ctrl Pts',(-20.2554040575952,44.8806334273021,122.152088557895)) ;
#24960 = CARTESIAN_POINT('Ctrl Pts',(-20.2927670242742,45.0738707962633,122.590851363296)) ;
#24961 = CARTESIAN_POINT('Ctrl Pts',(-20.5136611155883,44.8938817159004,122.385626670228)) ;
#24962 = CARTESIAN_POINT('Ctrl Pts',(-20.4224319151714,45.0839256377574,122.757766119149)) ;
#24963 = CARTESIAN_POINT('Ctrl Pts',(-20.6757307463464,44.9039365573945,122.59426491759)) ;
#24964 = CARTESIAN_POINT('Ctrl Pts',(-20.5192820589709,45.0937566270649,122.940386196395)) ;
#24965 = CARTESIAN_POINT('Ctrl Pts',(-20.7967932245961,44.913767546702,122.822543238522)) ;
#24966 = CARTESIAN_POINT('Ctrl Pts',(-20.584670046844,45.1038331913881,123.141847213542)) ;
#24967 = CARTESIAN_POINT('Ctrl Pts',(-20.8785256178797,44.9238441110252,123.074368365477)) ;
#24968 = CARTESIAN_POINT('Ctrl Pts',(-20.6134250008506,45.1136825165221,123.34692196347)) ;
#24969 = CARTESIAN_POINT('Ctrl Pts',(-20.9144646604309,44.9336934361592,123.330718388823)) ;
#24970 = CARTESIAN_POINT('Ctrl Pts',(-20.6042179421268,45.1270305161593,123.627426871071)) ;
#24971 = CARTESIAN_POINT('Ctrl Pts',(-20.9029627808752,44.9470414357965,123.681317025944)) ;
#24972 = CARTESIAN_POINT('Ctrl Pts',(-20.501477245052,45.1436152756959,123.964696954444)) ;
#24973 = CARTESIAN_POINT('Ctrl Pts',(-20.7745082951822,44.963626195333,124.10295325502)) ;
#24974 = CARTESIAN_POINT('Ctrl Pts',(-20.2906509977138,45.160183827044,124.247002494003)) ;
#24975 = CARTESIAN_POINT('Ctrl Pts',(-20.5110259009966,44.9801947466811,124.455768261803)) ;
#24976 = CARTESIAN_POINT('Ctrl Pts',(-20.0699761701848,45.173543651863,124.420705346495)) ;
#24977 = CARTESIAN_POINT('Ctrl Pts',(-20.2351348038895,44.9935545715001,124.672943272086)) ;
#24978 = CARTESIAN_POINT('Ctrl Pts',(-19.8865323634229,45.1834490606937,124.519294728282)) ;
#24979 = CARTESIAN_POINT('Ctrl Pts',(-20.0058393288218,45.0034599803308,124.796167835363)) ;
#24980 = CARTESIAN_POINT('Ctrl Pts',(-19.6878012033677,45.1934090872777,124.585169308581)) ;
#24981 = CARTESIAN_POINT('Ctrl Pts',(-19.757418400852,45.0134200069148,124.878510971796)) ;
#24982 = CARTESIAN_POINT('Ctrl Pts',(-19.4120405401479,45.206666671463,124.625957687893)) ;
#24983 = CARTESIAN_POINT('Ctrl Pts',(-19.4127381950797,45.0266775911001,124.929494089017)) ;
#24984 = CARTESIAN_POINT('Ctrl Pts',(-19.0603261711488,45.2233178829577,124.585513512105)) ;
#24985 = CARTESIAN_POINT('Ctrl Pts',(-18.9730728854828,45.0433288025948,124.878933487773)) ;
#24986 = CARTESIAN_POINT('Ctrl Pts',(-18.6814904591991,45.243236097068,124.396215063051)) ;
#24987 = CARTESIAN_POINT('Ctrl Pts',(-18.4995381186548,45.0632470167051,124.642306903848)) ;
#24988 = CARTESIAN_POINT('Ctrl Pts',(-18.3898754544286,45.2631138602888,124.090194523484)) ;
#24989 = CARTESIAN_POINT('Ctrl Pts',(-18.1350210819867,45.0831247799259,124.259778759138)) ;
#24990 = CARTESIAN_POINT('Ctrl Pts',(-18.2194472690857,45.283126528076,123.70037612657)) ;
#24991 = CARTESIAN_POINT('Ctrl Pts',(-17.9219902774577,45.1031374477131,123.772503946077)) ;
#24992 = CARTESIAN_POINT('Ctrl Pts',(-18.1921410054773,45.3029390507426,123.279913832054)) ;
#24993 = CARTESIAN_POINT('Ctrl Pts',(-17.8878614143457,45.1229499703797,123.246927329174)) ;
#24994 = CARTESIAN_POINT('Ctrl Pts',(-18.3102817888919,45.3229223507425,122.871855648759)) ;
#24995 = CARTESIAN_POINT('Ctrl Pts',(-18.0355408684965,45.1429332703796,122.736855760796)) ;
#24996 = CARTESIAN_POINT('Ctrl Pts',(-18.5597996288413,45.3428166278438,122.530199318799)) ;
#24997 = CARTESIAN_POINT('Ctrl Pts',(-18.3474404946756,45.1628275474809,122.309788228837)) ;
#24998 = CARTESIAN_POINT('Ctrl Pts',(-18.9111760068349,45.3627493896015,122.293234594438)) ;
#24999 = CARTESIAN_POINT('Ctrl Pts',(-18.786662149823,45.1827603092387,122.0135853007)) ;
#25000 = CARTESIAN_POINT('Ctrl Pts',(-19.3230940340298,45.3827153953663,122.190513539357)) ;
#25001 = CARTESIAN_POINT('Ctrl Pts',(-19.3015601046736,45.2027263150034,121.885187082688)) ;
#25002 = CARTESIAN_POINT('Ctrl Pts',(-19.7435470242779,45.4025939275311,122.234031106994)) ;
#25003 = CARTESIAN_POINT('Ctrl Pts',(-19.8271247057948,45.2226048471683,121.939586650986)) ;
#25004 = CARTESIAN_POINT('Ctrl Pts',(-20.1251936183417,45.4225335941915,122.418585683632)) ;
#25005 = CARTESIAN_POINT('Ctrl Pts',(-20.3041812489775,45.2425445138286,122.170281678288)) ;
#25006 = CARTESIAN_POINT('Ctrl Pts',(-20.4204383603451,45.4424284688368,122.721592637798)) ;
#25007 = CARTESIAN_POINT('Ctrl Pts',(-20.673234757221,45.262439388474,122.549040856896)) ;
#25008 = CARTESIAN_POINT('Ctrl Pts',(-20.5949902534563,45.4623356081302,123.107099332329)) ;
#25009 = CARTESIAN_POINT('Ctrl Pts',(-20.8914226002841,45.2823465277673,123.03092366853)) ;
#25010 = CARTESIAN_POINT('Ctrl Pts',(-20.6282585414511,45.4822461562087,123.529280154733)) ;
#25011 = CARTESIAN_POINT('Ctrl Pts',(-20.933006994823,45.3022570758458,123.558648564266)) ;
#25012 = CARTESIAN_POINT('Ctrl Pts',(-20.5136884964889,45.5023147415659,123.940226483196)) ;
#25013 = CARTESIAN_POINT('Ctrl Pts',(-20.7897928711044,45.322325661203,124.072332126759)) ;
#25014 = CARTESIAN_POINT('Ctrl Pts',(-20.2695153225536,45.5220965388806,124.282881980283)) ;
#25015 = CARTESIAN_POINT('Ctrl Pts',(-20.4845776581537,45.3421074585177,124.500648372566)) ;
#25016 = CARTESIAN_POINT('Ctrl Pts',(-19.9197219519249,45.5421040858251,124.52470903084)) ;
#25017 = CARTESIAN_POINT('Ctrl Pts',(-20.0473359397164,45.3621150054623,124.802932073758)) ;
#25018 = CARTESIAN_POINT('Ctrl Pts',(-19.5119563590964,45.561925824128,124.631740685911)) ;
#25019 = CARTESIAN_POINT('Ctrl Pts',(-19.5376317009415,45.3819367437651,124.936721152217)) ;
#25020 = CARTESIAN_POINT('Ctrl Pts',(-19.0888978513631,45.5819058440321,124.593677351388)) ;
#25021 = CARTESIAN_POINT('Ctrl Pts',(-19.0088087615849,45.4019167636693,124.889143040385)) ;
#25022 = CARTESIAN_POINT('Ctrl Pts',(-18.7055922778892,45.6018232952944,124.413561871822)) ;
#25023 = CARTESIAN_POINT('Ctrl Pts',(-18.5296775435496,45.4218342149315,124.664000015216)) ;
#25024 = CARTESIAN_POINT('Ctrl Pts',(-18.4066895135121,45.6216982164671,124.114786478611)) ;
#25025 = CARTESIAN_POINT('Ctrl Pts',(-18.1560490205525,45.4417091361042,124.2905332235)) ;
#25026 = CARTESIAN_POINT('Ctrl Pts',(-18.2266120856884,45.6417225850179,123.729001322783)) ;
#25027 = CARTESIAN_POINT('Ctrl Pts',(-17.9309504550834,45.461733504655,123.80830220994)) ;
#25028 = CARTESIAN_POINT('Ctrl Pts',(-18.1894029579917,45.6615892693914,123.308154855926)) ;
#25029 = CARTESIAN_POINT('Ctrl Pts',(-17.8844372685422,45.4816001890285,123.282245957211)) ;
#25030 = CARTESIAN_POINT('Ctrl Pts',(-18.2977756961196,45.6815330912376,122.898226280014)) ;
#25031 = CARTESIAN_POINT('Ctrl Pts',(-18.0199005695342,45.5015440108747,122.769835234287)) ;
#25032 = CARTESIAN_POINT('Ctrl Pts',(-18.5392315029753,45.7014404604891,122.55056181091)) ;
#25033 = CARTESIAN_POINT('Ctrl Pts',(-18.3217175474885,45.5214513801262,122.335254029468)) ;
#25034 = CARTESIAN_POINT('Ctrl Pts',(-18.8838051537408,45.7213151582358,122.30592410139)) ;
#25035 = CARTESIAN_POINT('Ctrl Pts',(-18.7524316861596,45.5413260778729,122.029454998175)) ;
#25036 = CARTESIAN_POINT('Ctrl Pts',(-19.2933757524993,45.7412971007575,122.192842071119)) ;
#25037 = CARTESIAN_POINT('Ctrl Pts',(-19.2643939100382,45.5613080203947,121.888099189238)) ;
#25038 = CARTESIAN_POINT('Ctrl Pts',(-19.7151717006801,45.7611997676684,122.226529361424)) ;
#25039 = CARTESIAN_POINT('Ctrl Pts',(-19.7916381676523,45.5812106873055,121.930204794695)) ;
#25040 = CARTESIAN_POINT('Ctrl Pts',(-20.0998523433655,45.7810551252071,122.400620470514)) ;
#25041 = CARTESIAN_POINT('Ctrl Pts',(-20.2724895989063,45.6010660448442,122.147814462636)) ;
#25042 = CARTESIAN_POINT('Ctrl Pts',(-20.4047844549801,45.8011191639231,122.698883119931)) ;
#25043 = CARTESIAN_POINT('Ctrl Pts',(-20.6536580199716,45.6211300835602,122.520640262332)) ;
#25044 = CARTESIAN_POINT('Ctrl Pts',(-20.5876495556406,45.8209743436481,123.079572690105)) ;
#25045 = CARTESIAN_POINT('Ctrl Pts',(-20.8822424651067,45.6409852632853,122.996499598304)) ;
#25046 = CARTESIAN_POINT('Ctrl Pts',(-20.6301960454336,45.8409544483126,123.502103273831)) ;
#25047 = CARTESIAN_POINT('Ctrl Pts',(-20.9354305273725,45.6609653679497,123.524661889087)) ;
#25048 = CARTESIAN_POINT('Ctrl Pts',(-20.5273174567824,45.8607635534824,123.910665052776)) ;
#25049 = CARTESIAN_POINT('Ctrl Pts',(-20.8068347567717,45.6807744731195,124.035365380666)) ;
#25050 = CARTESIAN_POINT('Ctrl Pts',(-20.2894986913643,45.8807561738231,124.262859185796)) ;
#25051 = CARTESIAN_POINT('Ctrl Pts',(-20.5095739145416,45.7007670934602,124.475605981024)) ;
#25052 = CARTESIAN_POINT('Ctrl Pts',(-20.0050296007185,45.8972956563272,124.469758288625)) ;
#25053 = CARTESIAN_POINT('Ctrl Pts',(-20.1539637829234,45.7173065759643,124.734247767366)) ;
#25054 = CARTESIAN_POINT('Ctrl Pts',(-19.7428533033287,45.9106599743914,124.570733072106)) ;
#25055 = CARTESIAN_POINT('Ctrl Pts',(-19.826276696828,45.7306708940285,124.860455779892)) ;
#25056 = CARTESIAN_POINT('Ctrl Pts',(-19.4702042971827,45.9238775768929,124.624395490945)) ;
#25057 = CARTESIAN_POINT('Ctrl Pts',(-19.4853999049105,45.74388849653,124.927543476285)) ;
#25058 = CARTESIAN_POINT('Ctrl Pts',(-19.1168393550171,45.9405351711707,124.600762737389)) ;
#25059 = CARTESIAN_POINT('Ctrl Pts',(-19.0437646821752,45.7605460908078,124.897999792884)) ;
#25060 = CARTESIAN_POINT('Ctrl Pts',(-18.7301975068277,45.9604008732124,124.430507653493)) ;
#25061 = CARTESIAN_POINT('Ctrl Pts',(-18.5604443553513,45.7804117928495,124.685196121248)) ;
#25062 = CARTESIAN_POINT('Ctrl Pts',(-18.4743625889817,45.9770305999024,124.186562575314)) ;
#25063 = CARTESIAN_POINT('Ctrl Pts',(-18.240630590451,45.7970415195396,124.380241225691)) ;
#25064 = CARTESIAN_POINT('Ctrl Pts',(-18.3289929824002,45.9903197150403,123.947896155844)) ;
#25065 = CARTESIAN_POINT('Ctrl Pts',(-18.0589348454478,45.8103306346774,124.081934291346)) ;
#25066 = CARTESIAN_POINT('Ctrl Pts',(-18.2525232753599,46.0002840620174,123.752891385966)) ;
#25067 = CARTESIAN_POINT('Ctrl Pts',(-17.9633418369383,45.8202949816545,123.838171148512)) ;
#25068 = CARTESIAN_POINT('Ctrl Pts',(-18.2110838319254,46.0102124300189,123.548318215047)) ;
#25069 = CARTESIAN_POINT('Ctrl Pts',(-17.9115389081574,45.830223349656,123.582470100099)) ;
#25070 = CARTESIAN_POINT('Ctrl Pts',(-18.2034517091304,46.0234958631076,123.269181346863)) ;
#25071 = CARTESIAN_POINT('Ctrl Pts',(-17.9020047414413,45.8435067827447,123.233481404821)) ;
#25072 = CARTESIAN_POINT('Ctrl Pts',(-18.2859373810871,46.0401479408479,122.924806830037)) ;
#25073 = CARTESIAN_POINT('Ctrl Pts',(-18.0050894429486,45.8601588604851,122.80309786385)) ;
#25074 = CARTESIAN_POINT('Ctrl Pts',(-18.479608382182,46.0566993101488,122.631034753051)) ;
#25075 = CARTESIAN_POINT('Ctrl Pts',(-18.2472042450846,45.8767102297859,122.435821289861)) ;
#25076 = CARTESIAN_POINT('Ctrl Pts',(-18.6881326465127,46.0699867382977,122.445080340454)) ;
#25077 = CARTESIAN_POINT('Ctrl Pts',(-18.5078328375495,45.8899976579349,122.203411111269)) ;
#25078 = CARTESIAN_POINT('Ctrl Pts',(-18.8678435030827,46.0800312779978,122.334231053414)) ;
#25079 = CARTESIAN_POINT('Ctrl Pts',(-18.7324749007102,45.900042197635,122.064839904029)) ;
#25080 = CARTESIAN_POINT('Ctrl Pts',(-19.060066473483,46.0898741198217,122.257583029304)) ;
#25081 = CARTESIAN_POINT('Ctrl Pts',(-18.9727512214166,45.9098850394588,121.969029204104)) ;
#25082 = CARTESIAN_POINT('Ctrl Pts',(-19.2654570004802,46.0998584040686,122.214404145467)) ;
#25083 = CARTESIAN_POINT('Ctrl Pts',(-19.2294892302823,45.9198693237057,121.91505230479)) ;
#25084 = CARTESIAN_POINT('Ctrl Pts',(-19.474529222648,46.1098080494678,122.207609739844)) ;
#25085 = CARTESIAN_POINT('Ctrl Pts',(-19.4908293876516,45.9298189691049,121.906556619496)) ;
#25086 = CARTESIAN_POINT('Ctrl Pts',(-19.6826867659275,46.1198078111562,122.237114286998)) ;
#25087 = CARTESIAN_POINT('Ctrl Pts',(-19.7510268140243,45.9398187307933,121.943434488528)) ;
#25088 = CARTESIAN_POINT('Ctrl Pts',(-19.8830689863678,46.1298391571151,122.30284594859)) ;
#25089 = CARTESIAN_POINT('Ctrl Pts',(-20.0015055166855,45.9498500767522,122.02559641534)) ;
#25090 = CARTESIAN_POINT('Ctrl Pts',(-20.0658738233849,46.1396941115922,122.400357303943)) ;
#25091 = CARTESIAN_POINT('Ctrl Pts',(-20.230012990869,45.9597050312293,122.147483174595)) ;
#25092 = CARTESIAN_POINT('Ctrl Pts',(-20.2311978485199,46.1496666495927,122.529251790254)) ;
#25093 = CARTESIAN_POINT('Ctrl Pts',(-20.4366698390954,45.9696775692299,122.308599139529)) ;
#25094 = CARTESIAN_POINT('Ctrl Pts',(-20.371971249445,46.1596616433277,122.68529494029)) ;
#25095 = CARTESIAN_POINT('Ctrl Pts',(-20.6126387229705,45.9796725629648,122.503651259972)) ;
#25096 = CARTESIAN_POINT('Ctrl Pts',(-20.4837019140822,46.1696957021218,122.864201377535)) ;
#25097 = CARTESIAN_POINT('Ctrl Pts',(-20.7523044634586,45.9897066217589,122.727282847818)) ;
#25098 = CARTESIAN_POINT('Ctrl Pts',(-20.5615851923955,46.1795510449448,123.056218498459)) ;
#25099 = CARTESIAN_POINT('Ctrl Pts',(-20.8496612407523,45.9995619645819,122.967303410869)) ;
#25100 = CARTESIAN_POINT('Ctrl Pts',(-20.6058435319962,46.1895505242904,123.261688930267)) ;
#25101 = CARTESIAN_POINT('Ctrl Pts',(-20.9049869101856,46.0095614439275,123.224140951696)) ;
#25102 = CARTESIAN_POINT('Ctrl Pts',(-20.613909648338,46.1994449730457,123.469584195291)) ;
#25103 = CARTESIAN_POINT('Ctrl Pts',(-20.9150723248034,46.0194558926828,123.484010185289)) ;
#25104 = CARTESIAN_POINT('Ctrl Pts',(-20.5852243576683,46.2095080924802,123.679152099285)) ;
#25105 = CARTESIAN_POINT('Ctrl Pts',(-20.8792184641045,46.0295190121173,123.745970407933)) ;
#25106 = CARTESIAN_POINT('Ctrl Pts',(-20.5222181496825,46.2193477377214,123.87621952154)) ;
#25107 = CARTESIAN_POINT('Ctrl Pts',(-20.8004631964166,46.0393586573585,123.992305910844)) ;
#25108 = CARTESIAN_POINT('Ctrl Pts',(-20.4240329883721,46.2294109019075,124.06358200029)) ;
#25109 = CARTESIAN_POINT('Ctrl Pts',(-20.6777341782391,46.0494218215446,124.226510235197)) ;
#25110 = CARTESIAN_POINT('Ctrl Pts',(-20.2968048807207,46.2393051716563,124.228173665467)) ;
#25111 = CARTESIAN_POINT('Ctrl Pts',(-20.5187010120317,46.0593160912934,124.432251752361)) ;
#25112 = CARTESIAN_POINT('Ctrl Pts',(-20.1426117795388,46.2492468976701,124.369228950053)) ;
#25113 = CARTESIAN_POINT('Ctrl Pts',(-20.3259612493778,46.0692578173072,124.608573010416)) ;
#25114 = CARTESIAN_POINT('Ctrl Pts',(-19.9651819070724,46.2592497863295,124.482167683482)) ;
#25115 = CARTESIAN_POINT('Ctrl Pts',(-20.1041752620859,46.0792607059666,124.749748717296)) ;
#25116 = CARTESIAN_POINT('Ctrl Pts',(-19.7700203195679,46.2692896351235,124.562503209581)) ;
#25117 = CARTESIAN_POINT('Ctrl Pts',(-19.8602243413917,46.0893005547606,124.850170623594)) ;
#25118 = CARTESIAN_POINT('Ctrl Pts',(-19.5683677612482,46.2791138505843,124.607227073809)) ;
#25119 = CARTESIAN_POINT('Ctrl Pts',(-19.6081586045614,46.0991247702215,124.906078173757)) ;
#25120 = CARTESIAN_POINT('Ctrl Pts',(-19.3571724462641,46.2891706940779,124.61676513193)) ;
#25121 = CARTESIAN_POINT('Ctrl Pts',(-19.3441646598656,46.109181613715,124.918003343611)) ;
#25122 = CARTESIAN_POINT('Ctrl Pts',(-19.1502130268079,46.2990993034739,124.589560068272)) ;
#25123 = CARTESIAN_POINT('Ctrl Pts',(-19.0854647176779,46.119110223111,124.883999596897)) ;
#25124 = CARTESIAN_POINT('Ctrl Pts',(-18.9504791865377,46.3090511875118,124.527247497498)) ;
#25125 = CARTESIAN_POINT('Ctrl Pts',(-18.8357963857665,46.1290621071489,124.806111234111)) ;
#25126 = CARTESIAN_POINT('Ctrl Pts',(-18.7629062407361,46.3191041403194,124.429897592764)) ;
#25127 = CARTESIAN_POINT('Ctrl Pts',(-18.6013290923237,46.1391150599565,124.684426223968)) ;
#25128 = CARTESIAN_POINT('Ctrl Pts',(-18.5986696134654,46.3289270167856,124.304685324782)) ;
#25129 = CARTESIAN_POINT('Ctrl Pts',(-18.3960311454174,46.1489379364227,124.527912441961)) ;
#25130 = CARTESIAN_POINT('Ctrl Pts',(-18.4550971880899,46.3389827493557,124.149533035185)) ;
#25131 = CARTESIAN_POINT('Ctrl Pts',(-18.2165638688177,46.1589936689928,124.333973843009)) ;
#25132 = CARTESIAN_POINT('Ctrl Pts',(-18.34225300586,46.3489235143433,123.973622295558)) ;
#25133 = CARTESIAN_POINT('Ctrl Pts',(-18.0755063145666,46.1689344339805,124.114086515428)) ;
#25134 = CARTESIAN_POINT('Ctrl Pts',(-18.2613628141207,46.358827847249,123.78175251306)) ;
#25135 = CARTESIAN_POINT('Ctrl Pts',(-17.9743911402895,46.1788387668861,123.874249737998)) ;
#25136 = CARTESIAN_POINT('Ctrl Pts',(-18.2144855602519,46.3688745161297,123.575825795225)) ;
#25137 = CARTESIAN_POINT('Ctrl Pts',(-17.9157922099519,46.1888854357668,123.616841983496)) ;
#25138 = CARTESIAN_POINT('Ctrl Pts',(-18.2040405773316,46.3787700794355,123.368018792122)) ;
#25139 = CARTESIAN_POINT('Ctrl Pts',(-17.9027335515217,46.1987809990726,123.357082770937)) ;
#25140 = CARTESIAN_POINT('Ctrl Pts',(-18.2302623333417,46.3888321371358,123.158144461646)) ;
#25141 = CARTESIAN_POINT('Ctrl Pts',(-17.9355083348723,46.2088430567729,123.094739738878)) ;
#25142 = CARTESIAN_POINT('Ctrl Pts',(-18.2910726090505,46.3986749147633,122.960331021879)) ;
#25143 = CARTESIAN_POINT('Ctrl Pts',(-18.0115191596736,46.2186858344004,122.847471415839)) ;
#25144 = CARTESIAN_POINT('Ctrl Pts',(-18.3862537401612,46.4086653930151,122.773135377991)) ;
#25145 = CARTESIAN_POINT('Ctrl Pts',(-18.1304936326855,46.2286763126523,122.613475678947)) ;
#25146 = CARTESIAN_POINT('Ctrl Pts',(-18.5117634998611,46.4185943656587,122.606329099744)) ;
#25147 = CARTESIAN_POINT('Ctrl Pts',(-18.2873793152529,46.2386052852958,122.404966075839)) ;
#25148 = CARTESIAN_POINT('Ctrl Pts',(-18.6650531697513,46.4285855025382,122.462726172881)) ;
#25149 = CARTESIAN_POINT('Ctrl Pts',(-18.4789900283898,46.2485964221754,122.225460708948)) ;
#25150 = CARTESIAN_POINT('Ctrl Pts',(-18.8416348523983,46.4386076200272,122.347776529069)) ;
#25151 = CARTESIAN_POINT('Ctrl Pts',(-18.6997158872876,46.2586185396643,122.081771774985)) ;
#25152 = CARTESIAN_POINT('Ctrl Pts',(-19.033062714252,46.4485081304294,122.266054468037)) ;
#25153 = CARTESIAN_POINT('Ctrl Pts',(-18.9390004515799,46.2685190500665,121.97961691748)) ;
#25154 = CARTESIAN_POINT('Ctrl Pts',(-19.2375063165582,46.4584971231755,122.218070769825)) ;
#25155 = CARTESIAN_POINT('Ctrl Pts',(-19.1945546489749,46.2785080428126,121.919635191703)) ;
#25156 = CARTESIAN_POINT('Ctrl Pts',(-19.4466780664343,46.4684623672261,122.206487877889)) ;
#25157 = CARTESIAN_POINT('Ctrl Pts',(-19.4560195398829,46.2884732868632,121.905154403475)) ;
#25158 = CARTESIAN_POINT('Ctrl Pts',(-19.6534929917255,46.4783666317393,122.230762789135)) ;
#25159 = CARTESIAN_POINT('Ctrl Pts',(-19.7145391120576,46.2983775513764,121.93549611882)) ;
#25160 = CARTESIAN_POINT('Ctrl Pts',(-19.8559786184111,46.4884247234375,122.291626495888)) ;
#25161 = CARTESIAN_POINT('Ctrl Pts',(-19.9676465193919,46.3084356430746,122.011573715253)) ;
#25162 = CARTESIAN_POINT('Ctrl Pts',(-20.0410082512781,46.4982746638659,122.384630025382)) ;
#25163 = CARTESIAN_POINT('Ctrl Pts',(-20.1989353902242,46.318285583503,122.127826794879)) ;
#25164 = CARTESIAN_POINT('Ctrl Pts',(-20.2103627890321,46.5083016750394,122.510144547104)) ;
#25165 = CARTESIAN_POINT('Ctrl Pts',(-20.4106296400589,46.3283125946766,122.284718430549)) ;
#25166 = CARTESIAN_POINT('Ctrl Pts',(-20.354983799268,46.5183302616515,122.66357001132)) ;
#25167 = CARTESIAN_POINT('Ctrl Pts',(-20.5914073282754,46.3383411812886,122.476498822217)) ;
#25168 = CARTESIAN_POINT('Ctrl Pts',(-20.4689669278839,46.5281754757642,122.836320633626)) ;
#25169 = CARTESIAN_POINT('Ctrl Pts',(-20.7338884447941,46.3481863954013,122.692436981991)) ;
#25170 = CARTESIAN_POINT('Ctrl Pts',(-20.5529614777016,46.5381662239437,123.028836720587)) ;
#25171 = CARTESIAN_POINT('Ctrl Pts',(-20.838883297733,46.3581771435809,122.933081577216)) ;
#25172 = CARTESIAN_POINT('Ctrl Pts',(-20.6020311758152,46.5482038575292,123.234075060244)) ;
#25173 = CARTESIAN_POINT('Ctrl Pts',(-20.9002222159883,46.3682147771664,123.1896289369)) ;
#25174 = CARTESIAN_POINT('Ctrl Pts',(-20.6148200501619,46.5580491467421,123.440660845129)) ;
#25175 = CARTESIAN_POINT('Ctrl Pts',(-20.9162101455242,46.3780600663792,123.447862222641)) ;
#25176 = CARTESIAN_POINT('Ctrl Pts',(-20.5916887931145,46.568030547548,123.649206343481)) ;
#25177 = CARTESIAN_POINT('Ctrl Pts',(-20.8872976540046,46.3880414671851,123.708544539136)) ;
#25178 = CARTESIAN_POINT('Ctrl Pts',(-20.5328161463453,46.5779827805379,123.849986028359)) ;
#25179 = CARTESIAN_POINT('Ctrl Pts',(-20.8137082785738,46.397993700175,123.959520057968)) ;
#25180 = CARTESIAN_POINT('Ctrl Pts',(-20.4397820483577,46.5879815919945,124.038501912924)) ;
#25181 = CARTESIAN_POINT('Ctrl Pts',(-20.6974169783614,46.4079925116317,124.195165716517)) ;
#25182 = CARTESIAN_POINT('Ctrl Pts',(-20.3146171869605,46.5980206959252,124.208420179491)) ;
#25183 = CARTESIAN_POINT('Ctrl Pts',(-20.5409623495954,46.4180316155623,124.407564420263)) ;
#25184 = CARTESIAN_POINT('Ctrl Pts',(-20.1653985323656,46.6078456383445,124.351256112857)) ;
#25185 = CARTESIAN_POINT('Ctrl Pts',(-20.3544390959673,46.4278565579816,124.586111387913)) ;
#25186 = CARTESIAN_POINT('Ctrl Pts',(-19.989843192052,46.6179003258204,124.468971674532)) ;
#25187 = CARTESIAN_POINT('Ctrl Pts',(-20.134995919871,46.4379112454576,124.733256870576)) ;
#25188 = CARTESIAN_POINT('Ctrl Pts',(-19.7985051156906,46.6278431281773,124.553146705472)) ;
#25189 = CARTESIAN_POINT('Ctrl Pts',(-19.8958234362632,46.4478540478144,124.838477290274)) ;
#25190 = CARTESIAN_POINT('Ctrl Pts',(-19.5964092228832,46.637746924117,124.603245253759)) ;
#25191 = CARTESIAN_POINT('Ctrl Pts',(-19.6432030628621,46.4577578437542,124.901101950844)) ;
#25192 = CARTESIAN_POINT('Ctrl Pts',(-19.3856978448509,46.6477937034921,124.617570281629)) ;
#25193 = CARTESIAN_POINT('Ctrl Pts',(-19.3798141419767,46.4678046231292,124.919009575157)) ;
#25194 = CARTESIAN_POINT('Ctrl Pts',(-19.1787922985653,46.6576893617867,124.595604702868)) ;
#25195 = CARTESIAN_POINT('Ctrl Pts',(-19.1211811679258,46.4777002814238,124.891553789188)) ;
#25196 = CARTESIAN_POINT('Ctrl Pts',(-18.9755356634845,46.6677509290373,124.537120494577)) ;
#25197 = CARTESIAN_POINT('Ctrl Pts',(-18.8671103311317,46.4877618486744,124.818449852984)) ;
#25198 = CARTESIAN_POINT('Ctrl Pts',(-18.7895780705822,46.6775955734746,124.446252644844)) ;
#25199 = CARTESIAN_POINT('Ctrl Pts',(-18.6346615958398,46.4976064931117,124.704865605345)) ;
#25200 = CARTESIAN_POINT('Ctrl Pts',(-18.6198270026623,46.6875556197173,124.323663154049)) ;
#25201 = CARTESIAN_POINT('Ctrl Pts',(-18.4224718070244,46.5075665393544,124.551629282646)) ;
#25202 = CARTESIAN_POINT('Ctrl Pts',(-18.4730960397559,46.6975939157357,124.171998085648)) ;
#25203 = CARTESIAN_POINT('Ctrl Pts',(-18.2390573894743,46.5176048353728,124.362048863107)) ;
#25204 = CARTESIAN_POINT('Ctrl Pts',(-18.3565170418454,46.707467257154,124.0002223481)) ;
#25205 = CARTESIAN_POINT('Ctrl Pts',(-18.0933321835797,46.5274781767911,124.147328823137)) ;
#25206 = CARTESIAN_POINT('Ctrl Pts',(-18.2699035021467,46.7175403609533,123.807021171241)) ;
#25207 = CARTESIAN_POINT('Ctrl Pts',(-17.9850644966569,46.5375512805904,123.905828159884)) ;
#25208 = CARTESIAN_POINT('Ctrl Pts',(-18.2191778694931,46.7273611760722,123.606843477145)) ;
#25209 = CARTESIAN_POINT('Ctrl Pts',(-17.9216561766812,46.5473720957093,123.655604769692)) ;
#25210 = CARTESIAN_POINT('Ctrl Pts',(-18.2033482281936,46.7374380411502,123.395627154277)) ;
#25211 = CARTESIAN_POINT('Ctrl Pts',(-17.9018683250634,46.5574489607873,123.391584873684)) ;
#25212 = CARTESIAN_POINT('Ctrl Pts',(-18.2240747598041,46.7473027808054,123.189252605334)) ;
#25213 = CARTESIAN_POINT('Ctrl Pts',(-17.9277757499098,46.5673137004426,123.133615388447)) ;
#25214 = CARTESIAN_POINT('Ctrl Pts',(-18.2806784571676,46.7573251840468,122.986304105928)) ;
#25215 = CARTESIAN_POINT('Ctrl Pts',(-17.9985297244048,46.5773361036839,122.879929630516)) ;
#25216 = CARTESIAN_POINT('Ctrl Pts',(-18.3721757227985,46.7673509083353,122.796412957651)) ;
#25217 = CARTESIAN_POINT('Ctrl Pts',(-18.1129004945136,46.5873618279724,122.642565399525)) ;
#25218 = CARTESIAN_POINT('Ctrl Pts',(-18.4928445279093,46.7772056913566,122.628018609058)) ;
#25219 = CARTESIAN_POINT('Ctrl Pts',(-18.2637366876288,46.5972166109937,122.432070963929)) ;
#25220 = CARTESIAN_POINT('Ctrl Pts',(-18.6424131075352,46.7871845350798,122.480907272402)) ;
#25221 = CARTESIAN_POINT('Ctrl Pts',(-18.4506972916997,46.607195454717,122.248181197861)) ;
#25222 = CARTESIAN_POINT('Ctrl Pts',(-18.8161403685394,46.7972034273165,122.361831711629)) ;
#25223 = CARTESIAN_POINT('Ctrl Pts',(-18.6678559884878,46.6172143469536,122.099336220667)) ;
#25224 = CARTESIAN_POINT('Ctrl Pts',(-19.0051621248725,46.8070866363575,122.275502154482)) ;
#25225 = CARTESIAN_POINT('Ctrl Pts',(-18.9041339832422,46.6270975559946,121.991423381431)) ;
#25226 = CARTESIAN_POINT('Ctrl Pts',(-19.210031702073,46.8171549456977,122.222428926557)) ;
#25227 = CARTESIAN_POINT('Ctrl Pts',(-19.1602204279234,46.6371658653348,121.925081449906)) ;
#25228 = CARTESIAN_POINT('Ctrl Pts',(-19.4160633040709,46.8269850710304,122.205881850251)) ;
#25229 = CARTESIAN_POINT('Ctrl Pts',(-19.4177614318243,46.6469959906675,121.904397063364)) ;
#25230 = CARTESIAN_POINT('Ctrl Pts',(-19.6267444353502,46.8370516234074,122.22554880192)) ;
#25231 = CARTESIAN_POINT('Ctrl Pts',(-19.6811124793488,46.6570625430445,121.928980404509)) ;
#25232 = CARTESIAN_POINT('Ctrl Pts',(-19.8272585672866,46.8469418603011,122.280657735595)) ;
#25233 = CARTESIAN_POINT('Ctrl Pts',(-19.93175625164,46.6669527799382,121.997866497326)) ;
#25234 = CARTESIAN_POINT('Ctrl Pts',(-20.0172576560397,46.8569340850951,122.370232887069)) ;
#25235 = CARTESIAN_POINT('Ctrl Pts',(-20.1692553844016,46.6769450047322,122.109835361796)) ;
#25236 = CARTESIAN_POINT('Ctrl Pts',(-20.1882040593248,46.866896705446,122.491242308474)) ;
#25237 = CARTESIAN_POINT('Ctrl Pts',(-20.3829389131417,46.6869076250832,122.261097188161)) ;
#25238 = CARTESIAN_POINT('Ctrl Pts',(-20.3350687567512,46.8768017082092,122.638883740388)) ;
#25239 = CARTESIAN_POINT('Ctrl Pts',(-20.5665204839457,46.6968126278463,122.445649602459)) ;
#25240 = CARTESIAN_POINT('Ctrl Pts',(-20.4557645798383,46.8868594706073,122.812475638472)) ;
#25241 = CARTESIAN_POINT('Ctrl Pts',(-20.7173901651887,46.7068703902444,122.662639131591)) ;
#25242 = CARTESIAN_POINT('Ctrl Pts',(-20.5428264939987,46.8967099899861,123.000391779581)) ;
#25243 = CARTESIAN_POINT('Ctrl Pts',(-20.8262181894773,46.7167209096232,122.89753556539)) ;
#25244 = CARTESIAN_POINT('Ctrl Pts',(-20.5973539637941,46.9067415669843,123.204102169364)) ;
#25245 = CARTESIAN_POINT('Ctrl Pts',(-20.8943773618054,46.7267524866214,123.15217347503)) ;
#25246 = CARTESIAN_POINT('Ctrl Pts',(-20.6152416325616,46.9167513020892,123.413800001265)) ;
#25247 = CARTESIAN_POINT('Ctrl Pts',(-20.9167369790523,46.7367622217263,123.414295804395)) ;
#25248 = CARTESIAN_POINT('Ctrl Pts',(-20.5968220041765,46.9266608787155,123.621296181329)) ;
#25249 = CARTESIAN_POINT('Ctrl Pts',(-20.8937123153054,46.7466717983526,123.673666920638)) ;
#25250 = CARTESIAN_POINT('Ctrl Pts',(-20.5430662397492,46.9365882645721,123.822968750851)) ;
#25251 = CARTESIAN_POINT('Ctrl Pts',(-20.8265171674148,46.7565991842093,123.925758286608)) ;
#25252 = CARTESIAN_POINT('Ctrl Pts',(-20.4539206450829,46.9466331990624,124.014396648142)) ;
#25253 = CARTESIAN_POINT('Ctrl Pts',(-20.7150850922258,46.7666441186995,124.165042883978)) ;
#25254 = CARTESIAN_POINT('Ctrl Pts',(-20.3348959674513,46.9565191312504,124.184787009017)) ;
#25255 = CARTESIAN_POINT('Ctrl Pts',(-20.566303423748,46.7765300508875,124.378031588581)) ;
#25256 = CARTESIAN_POINT('Ctrl Pts',(-20.1867731077761,46.9665124372034,124.333759281434)) ;
#25257 = CARTESIAN_POINT('Ctrl Pts',(-20.3811494336437,46.7865233568405,124.56424680321)) ;
#25258 = CARTESIAN_POINT('Ctrl Pts',(-20.0157955120954,46.9764580749853,124.454112395529)) ;
#25259 = CARTESIAN_POINT('Ctrl Pts',(-20.167426750717,46.7964689946224,124.714688252167)) ;
#25260 = CARTESIAN_POINT('Ctrl Pts',(-19.8266604007549,46.9864053433312,124.543356690271)) ;
#25261 = CARTESIAN_POINT('Ctrl Pts',(-19.9310071201226,46.8064162629683,124.826243396208)) ;
#25262 = CARTESIAN_POINT('Ctrl Pts',(-19.6228151224958,46.9964532454683,124.598728489148)) ;
#25263 = CARTESIAN_POINT('Ctrl Pts',(-19.6762006528589,46.8164641651054,124.895457669008)) ;
#25264 = CARTESIAN_POINT('Ctrl Pts',(-19.4166526981356,47.0063009403085,124.617657767281)) ;
#25265 = CARTESIAN_POINT('Ctrl Pts',(-19.4184961828357,46.8263118599456,124.91911890289)) ;
#25266 = CARTESIAN_POINT('Ctrl Pts',(-19.2079050762096,47.0162624500529,124.600964149911)) ;
#25267 = CARTESIAN_POINT('Ctrl Pts',(-19.1575612607115,46.83627336969,124.898251094209)) ;
#25268 = CARTESIAN_POINT('Ctrl Pts',(-19.0039009099091,47.0262918416617,124.54764239375)) ;
#25269 = CARTESIAN_POINT('Ctrl Pts',(-18.902556312997,46.8463027612989,124.831598304346)) ;
#25270 = CARTESIAN_POINT('Ctrl Pts',(-18.8145419924307,47.0361993372165,124.460883485285)) ;
#25271 = CARTESIAN_POINT('Ctrl Pts',(-18.6658571373904,46.8562102568536,124.723148671996)) ;
#25272 = CARTESIAN_POINT('Ctrl Pts',(-18.642246189298,47.0461447288795,124.342465094977)) ;
#25273 = CARTESIAN_POINT('Ctrl Pts',(-18.4504873824993,46.8661556485166,124.575124657286)) ;
#25274 = CARTESIAN_POINT('Ctrl Pts',(-18.4921614871914,47.0561466464769,124.1951532533)) ;
#25275 = CARTESIAN_POINT('Ctrl Pts',(-18.262882041295,46.876157566114,124.390984128)) ;
#25276 = CARTESIAN_POINT('Ctrl Pts',(-18.3698136381604,47.0661867140291,124.023179183361)) ;
#25277 = CARTESIAN_POINT('Ctrl Pts',(-18.1099479381027,46.8861976336662,124.176016249327)) ;
#25278 = CARTESIAN_POINT('Ctrl Pts',(-18.2806928887342,47.0760110254689,123.836839708192)) ;
#25279 = CARTESIAN_POINT('Ctrl Pts',(-17.998547175216,46.896021945106,123.943090129844)) ;
#25280 = CARTESIAN_POINT('Ctrl Pts',(-18.2237020979738,47.086067266625,123.633273731581)) ;
#25281 = CARTESIAN_POINT('Ctrl Pts',(-17.9273097685191,46.9060781862621,123.688632681324)) ;
#25282 = CARTESIAN_POINT('Ctrl Pts',(-18.203421628533,47.0959981883606,123.425458332389)) ;
#25283 = CARTESIAN_POINT('Ctrl Pts',(-17.9019600484687,46.9160091079977,123.4288626675)) ;
#25284 = CARTESIAN_POINT('Ctrl Pts',(-18.2191232760878,47.1059414244368,123.217037662918)) ;
#25285 = CARTESIAN_POINT('Ctrl Pts',(-17.9215882488076,46.925952344074,123.168336310537)) ;
#25286 = CARTESIAN_POINT('Ctrl Pts',(-18.2707913644975,47.1159227084493,123.013627488194)) ;
#25287 = CARTESIAN_POINT('Ctrl Pts',(-17.9861745623724,46.9359336280864,122.914073624315)) ;
#25288 = CARTESIAN_POINT('Ctrl Pts',(-18.3578456878256,47.125967010075,122.821273166394)) ;
#25289 = CARTESIAN_POINT('Ctrl Pts',(-18.0949933336756,46.9459779297121,122.673631325158)) ;
#25290 = CARTESIAN_POINT('Ctrl Pts',(-18.4740478321358,47.1357950912944,122.650390408871)) ;
#25291 = CARTESIAN_POINT('Ctrl Pts',(-18.2402478329783,46.9558060109315,122.460027367171)) ;
#25292 = CARTESIAN_POINT('Ctrl Pts',(-18.6216725538285,47.1458716941436,122.498517159224)) ;
#25293 = CARTESIAN_POINT('Ctrl Pts',(-18.4247793331419,46.9658826137807,122.270186990604)) ;
#25294 = CARTESIAN_POINT('Ctrl Pts',(-18.789608451275,47.1557237732621,122.377209771896)) ;
#25295 = CARTESIAN_POINT('Ctrl Pts',(-18.6347009617729,46.9757346928992,122.118553078034)) ;
#25296 = CARTESIAN_POINT('Ctrl Pts',(-18.980091407923,47.165797031571,122.284749398737)) ;
#25297 = CARTESIAN_POINT('Ctrl Pts',(-18.8728048873028,46.9858079512082,122.002979006205)) ;
#25298 = CARTESIAN_POINT('Ctrl Pts',(-19.1791102852178,47.1756384909513,122.228144087822)) ;
#25299 = CARTESIAN_POINT('Ctrl Pts',(-19.1215801045156,46.9956494105884,121.93222329205)) ;
#25300 = CARTESIAN_POINT('Ctrl Pts',(-19.3873332175923,47.1855995863637,122.205917819797)) ;
#25301 = CARTESIAN_POINT('Ctrl Pts',(-19.381859343394,47.0056105060008,121.904442012515)) ;
#25302 = CARTESIAN_POINT('Ctrl Pts',(-19.5978250311267,47.1956368707604,122.220705841968)) ;
#25303 = CARTESIAN_POINT('Ctrl Pts',(-19.6449738782894,47.0156477903975,121.922928491226)) ;
#25304 = CARTESIAN_POINT('Ctrl Pts',(-19.7993828425593,47.2055132094957,122.270652196407)) ;
#25305 = CARTESIAN_POINT('Ctrl Pts',(-19.8969217299239,47.0255241291328,121.985363214302)) ;
#25306 = CARTESIAN_POINT('Ctrl Pts',(-19.9927485786675,47.2155753356489,122.356364369119)) ;
#25307 = CARTESIAN_POINT('Ctrl Pts',(-20.1386279884017,47.0355862552861,122.092504779786)) ;
#25308 = CARTESIAN_POINT('Ctrl Pts',(-20.1649812697198,47.2254435096255,122.472061623222)) ;
#25309 = CARTESIAN_POINT('Ctrl Pts',(-20.3539188130597,47.0454544292626,122.237128270037)) ;
#25310 = CARTESIAN_POINT('Ctrl Pts',(-20.3168466409141,47.2354490581293,122.61756598711)) ;
#25311 = CARTESIAN_POINT('Ctrl Pts',(-20.5437493740665,47.0554599777664,122.419010050859)) ;
#25312 = CARTESIAN_POINT('Ctrl Pts',(-20.4408371920724,47.2454316900249,122.7869363998)) ;
#25313 = CARTESIAN_POINT('Ctrl Pts',(-20.6987362985448,47.065442609662,122.630724270001)) ;
#25314 = CARTESIAN_POINT('Ctrl Pts',(-20.5338834735868,47.2554756324466,122.976466219455)) ;
#25315 = CARTESIAN_POINT('Ctrl Pts',(-20.8150425909332,47.0754865520838,122.867637130232)) ;
#25316 = CARTESIAN_POINT('Ctrl Pts',(-20.5916167588128,47.2653037804738,123.17485450326)) ;
#25317 = CARTESIAN_POINT('Ctrl Pts',(-20.8872078791894,47.0853147001109,123.115624213289)) ;
#25318 = CARTESIAN_POINT('Ctrl Pts',(-20.6150653225155,47.2752936478482,123.383560571913)) ;
#25319 = CARTESIAN_POINT('Ctrl Pts',(-20.9165166534759,47.0953045674853,123.37650718992)) ;
#25320 = CARTESIAN_POINT('Ctrl Pts',(-20.601300740418,47.2853373868037,123.594262445601)) ;
#25321 = CARTESIAN_POINT('Ctrl Pts',(-20.8993091493922,47.1053483064408,123.639884268201)) ;
#25322 = CARTESIAN_POINT('Ctrl Pts',(-20.552687444503,47.2951591353416,123.794940800993)) ;
#25323 = CARTESIAN_POINT('Ctrl Pts',(-20.8385403650369,47.1151700549788,123.890732974447)) ;
#25324 = CARTESIAN_POINT('Ctrl Pts',(-20.4686462395042,47.3051941129514,123.988445576631)) ;
#25325 = CARTESIAN_POINT('Ctrl Pts',(-20.7334869965978,47.1252050325885,124.132613019297)) ;
#25326 = CARTESIAN_POINT('Ctrl Pts',(-20.3519069360569,47.3152190257091,124.163922378538)) ;
#25327 = CARTESIAN_POINT('Ctrl Pts',(-20.5875612969449,47.1352299453462,124.351957946675)) ;
#25328 = CARTESIAN_POINT('Ctrl Pts',(-20.2093112218679,47.3250709688029,124.314143088258)) ;
#25329 = CARTESIAN_POINT('Ctrl Pts',(-20.4093144805832,47.14508188844,124.539733165987)) ;
#25330 = CARTESIAN_POINT('Ctrl Pts',(-20.0406636984681,47.335061930132,124.439301449808)) ;
#25331 = CARTESIAN_POINT('Ctrl Pts',(-20.1985036701278,47.1550728497691,124.69617951058)) ;
#25332 = CARTESIAN_POINT('Ctrl Pts',(-19.8542359453285,47.3449798050004,124.532734343896)) ;
#25333 = CARTESIAN_POINT('Ctrl Pts',(-19.9654674976531,47.1649907246376,124.812968953075)) ;
#25334 = CARTESIAN_POINT('Ctrl Pts',(-19.6522424998238,47.3550083240017,124.593072966075)) ;
#25335 = CARTESIAN_POINT('Ctrl Pts',(-19.71297510293,47.1750192436388,124.88839013585)) ;
#25336 = CARTESIAN_POINT('Ctrl Pts',(-19.4458515602898,47.3648920027995,124.617180149755)) ;
#25337 = CARTESIAN_POINT('Ctrl Pts',(-19.4549854354218,47.1849029224366,124.918522015687)) ;
#25338 = CARTESIAN_POINT('Ctrl Pts',(-19.2360564520279,47.3748869462393,124.605411359256)) ;
#25339 = CARTESIAN_POINT('Ctrl Pts',(-19.1927415406444,47.1948978658764,124.903808702217)) ;
#25340 = CARTESIAN_POINT('Ctrl Pts',(-19.0309200127824,47.3849138000617,124.556888090555)) ;
#25341 = CARTESIAN_POINT('Ctrl Pts',(-18.9363215273581,47.2049247196988,124.843152452533)) ;
#25342 = CARTESIAN_POINT('Ctrl Pts',(-18.8399600132762,47.3947979644006,124.474930121574)) ;
#25343 = CARTESIAN_POINT('Ctrl Pts',(-18.6976217950589,47.2148088840377,124.740702605869)) ;
#25344 = CARTESIAN_POINT('Ctrl Pts',(-18.6641751096275,47.404786062443,124.360112233341)) ;
#25345 = CARTESIAN_POINT('Ctrl Pts',(-18.4778918251213,47.2247969820801,124.597178175501)) ;
#25346 = CARTESIAN_POINT('Ctrl Pts',(-18.5114500487226,47.4147371689001,124.217101265402)) ;
#25347 = CARTESIAN_POINT('Ctrl Pts',(-18.2869868870465,47.2347480885372,124.418412493407)) ;
#25348 = CARTESIAN_POINT('Ctrl Pts',(-18.3848081572941,47.4247822200682,124.048124629567)) ;
#25349 = CARTESIAN_POINT('Ctrl Pts',(-18.1286864683151,47.2447931397053,124.207190353518)) ;
#25350 = CARTESIAN_POINT('Ctrl Pts',(-18.2910618402465,47.4346439804265,123.86320370385)) ;
#25351 = CARTESIAN_POINT('Ctrl Pts',(-18.0115053675036,47.2546549000636,123.976037450219)) ;
#25352 = CARTESIAN_POINT('Ctrl Pts',(-18.2296126467464,47.4446067972569,123.662969790822)) ;
#25353 = CARTESIAN_POINT('Ctrl Pts',(-17.9346962187188,47.264617716894,123.725744078448)) ;
#25354 = CARTESIAN_POINT('Ctrl Pts',(-18.2040389740413,47.4546414785377,123.45357433271)) ;
#25355 = CARTESIAN_POINT('Ctrl Pts',(-17.9027315659369,47.2746523981748,123.463999492697)) ;
#25356 = CARTESIAN_POINT('Ctrl Pts',(-18.2146920724958,47.4645265083184,123.246004580245)) ;
#25357 = CARTESIAN_POINT('Ctrl Pts',(-17.9160504867167,47.2845374279556,123.204536864795)) ;
#25358 = CARTESIAN_POINT('Ctrl Pts',(-18.2621069746344,47.4745921017164,123.039809498366)) ;
#25359 = CARTESIAN_POINT('Ctrl Pts',(-17.9753215326006,47.2946030213536,122.946793722897)) ;
#25360 = CARTESIAN_POINT('Ctrl Pts',(-18.3425816794122,47.4844312700779,122.849220328905)) ;
#25361 = CARTESIAN_POINT('Ctrl Pts',(-18.0759175402315,47.3044421897151,122.708557598471)) ;
#25362 = CARTESIAN_POINT('Ctrl Pts',(-18.457201944164,47.4944938678194,122.671444955583)) ;
#25363 = CARTESIAN_POINT('Ctrl Pts',(-18.2191949884316,47.3145047874566,122.486339905974)) ;
#25364 = CARTESIAN_POINT('Ctrl Pts',(-18.5987718864396,47.5043908802264,122.518950167232)) ;
#25365 = CARTESIAN_POINT('Ctrl Pts',(-18.396159615514,47.3244017998635,122.295722821703)) ;
#25366 = CARTESIAN_POINT('Ctrl Pts',(-18.7648105631557,47.514322202052,122.392374159236)) ;
#25367 = CARTESIAN_POINT('Ctrl Pts',(-18.6037098264549,47.3343331216891,122.137504758704)) ;
#25368 = CARTESIAN_POINT('Ctrl Pts',(-18.9524743880465,47.5243639648065,122.295687498941)) ;
#25369 = CARTESIAN_POINT('Ctrl Pts',(-18.8382907890392,47.3443748844436,122.016648795488)) ;
#25370 = CARTESIAN_POINT('Ctrl Pts',(-19.1509626646768,47.5342521636972,122.233865751707)) ;
#25371 = CARTESIAN_POINT('Ctrl Pts',(-19.0864023365642,47.3542630833343,121.939374027969)) ;
#25372 = CARTESIAN_POINT('Ctrl Pts',(-19.3593042021687,47.544246102297,122.206837954189)) ;
#25373 = CARTESIAN_POINT('Ctrl Pts',(-19.3468297085847,47.3642570219342,121.905591956175)) ;
#25374 = CARTESIAN_POINT('Ctrl Pts',(-19.5680879347369,47.5541869233339,122.216359937286)) ;
#25375 = CARTESIAN_POINT('Ctrl Pts',(-19.6078094898697,47.374197842971,121.917497147633)) ;
#25376 = CARTESIAN_POINT('Ctrl Pts',(-19.7724614957895,47.5641463056221,122.26180879175)) ;
#25377 = CARTESIAN_POINT('Ctrl Pts',(-19.8632760200849,47.3841572252593,121.974310927408)) ;
#25378 = CARTESIAN_POINT('Ctrl Pts',(-19.966662779158,47.5741440652745,122.342257817906)) ;
#25379 = CARTESIAN_POINT('Ctrl Pts',(-20.1060266518377,47.3941549849116,122.074874782439)) ;
#25380 = CARTESIAN_POINT('Ctrl Pts',(-20.1444477349424,47.5841802014768,122.455869269298)) ;
#25381 = CARTESIAN_POINT('Ctrl Pts',(-20.3282563986287,47.4041911211139,122.216891398893)) ;
#25382 = CARTESIAN_POINT('Ctrl Pts',(-20.2971040279646,47.5940309989677,122.595810595244)) ;
#25383 = CARTESIAN_POINT('Ctrl Pts',(-20.5190751999569,47.4140419186048,122.391820347718)) ;
#25384 = CARTESIAN_POINT('Ctrl Pts',(-20.425042108738,47.603991864044,122.761583938118)) ;
#25385 = CARTESIAN_POINT('Ctrl Pts',(-20.6789956607079,47.4240027836811,122.599038839022)) ;
#25386 = CARTESIAN_POINT('Ctrl Pts',(-20.5226996631887,47.6140207316744,122.948455189612)) ;
#25387 = CARTESIAN_POINT('Ctrl Pts',(-20.8010651623618,47.4340316513115,122.832629226849)) ;
#25388 = CARTESIAN_POINT('Ctrl Pts',(-20.5857281504088,47.6239309678108,123.147028040722)) ;
#25389 = CARTESIAN_POINT('Ctrl Pts',(-20.8798481803655,47.4439418874479,123.080846336945)) ;
#25390 = CARTESIAN_POINT('Ctrl Pts',(-20.6139336283943,47.6338659211253,123.353984814139)) ;
#25391 = CARTESIAN_POINT('Ctrl Pts',(-20.9151022554273,47.4538768407624,123.339542816455)) ;
#25392 = CARTESIAN_POINT('Ctrl Pts',(-20.605496943485,47.6439068515349,123.564903134672)) ;
#25393 = CARTESIAN_POINT('Ctrl Pts',(-20.9045535939109,47.463917771172,123.603190649991)) ;
#25394 = CARTESIAN_POINT('Ctrl Pts',(-20.5613779871071,47.6537947483165,123.768050424334)) ;
#25395 = CARTESIAN_POINT('Ctrl Pts',(-20.849402115707,47.4738056679536,123.857124325427)) ;
#25396 = CARTESIAN_POINT('Ctrl Pts',(-20.4822143423052,47.6637841999752,123.962563095657)) ;
#25397 = CARTESIAN_POINT('Ctrl Pts',(-20.750444918412,47.4837951196123,124.1002641636)) ;
#25398 = CARTESIAN_POINT('Ctrl Pts',(-20.370678012507,47.6737432903405,124.139744915088)) ;
#25399 = CARTESIAN_POINT('Ctrl Pts',(-20.6110220669267,47.4937542099777,124.321740017003)) ;
#25400 = CARTESIAN_POINT('Ctrl Pts',(-20.2313246232406,47.6836406026468,124.294278132182)) ;
#25401 = CARTESIAN_POINT('Ctrl Pts',(-20.4368281965108,47.503651522284,124.514904688104)) ;
#25402 = CARTESIAN_POINT('Ctrl Pts',(-20.0645809253998,47.6936970285471,124.424226886793)) ;
#25403 = CARTESIAN_POINT('Ctrl Pts',(-20.2283967744204,47.5137079481842,124.677338457595)) ;
#25404 = CARTESIAN_POINT('Ctrl Pts',(-19.8812864921283,47.7035670311368,124.521524514142)) ;
#25405 = CARTESIAN_POINT('Ctrl Pts',(-19.9992773799533,47.523577950774,124.798958001509)) ;
#25406 = CARTESIAN_POINT('Ctrl Pts',(-19.6813729094116,47.7135709643141,124.586772503536)) ;
#25407 = CARTESIAN_POINT('Ctrl Pts',(-19.7493845402161,47.5335818839512,124.880515352736)) ;
#25408 = CARTESIAN_POINT('Ctrl Pts',(-19.4734437265146,47.723558224778,124.616166289177)) ;
#25409 = CARTESIAN_POINT('Ctrl Pts',(-19.4894723640348,47.5435691444151,124.917254732859)) ;
#25410 = CARTESIAN_POINT('Ctrl Pts',(-19.2627853496724,47.7335852763637,124.608859964159)) ;
#25411 = CARTESIAN_POINT('Ctrl Pts',(-19.2261503135035,47.5535961960008,124.908119289949)) ;
#25412 = CARTESIAN_POINT('Ctrl Pts',(-19.0593193011781,47.7434763661898,124.565875611357)) ;
#25413 = CARTESIAN_POINT('Ctrl Pts',(-18.9718149570964,47.5634872858269,124.854385043497)) ;
#25414 = CARTESIAN_POINT('Ctrl Pts',(-18.7998791514015,47.7567741209708,124.46180634869)) ;
#25415 = CARTESIAN_POINT('Ctrl Pts',(-18.6475331408761,47.576785040608,124.724300286802)) ;
#25416 = CARTESIAN_POINT('Ctrl Pts',(-18.5749055156603,47.769972180579,124.293953042302)) ;
#25417 = CARTESIAN_POINT('Ctrl Pts',(-18.3663382799237,47.5899831002161,124.51451143139)) ;
#25418 = CARTESIAN_POINT('Ctrl Pts',(-18.4005844763,47.7833689211482,124.072822952987)) ;
#25419 = CARTESIAN_POINT('Ctrl Pts',(-18.1483991888473,47.6033798407853,124.238054641967)) ;
#25420 = CARTESIAN_POINT('Ctrl Pts',(-18.3021342969201,47.7932398332216,123.890089252221)) ;
#25421 = CARTESIAN_POINT('Ctrl Pts',(-18.025347143704,47.6132507528587,124.009644853001)) ;
#25422 = CARTESIAN_POINT('Ctrl Pts',(-18.2356106700847,47.8033133949897,123.689082460906)) ;
#25423 = CARTESIAN_POINT('Ctrl Pts',(-17.9421929511721,47.6233243146269,123.758382877817)) ;
#25424 = CARTESIAN_POINT('Ctrl Pts',(-18.2055029737511,47.8131348075781,123.484761908509)) ;
#25425 = CARTESIAN_POINT('Ctrl Pts',(-17.9045616883877,47.6331457272152,123.502983370987)) ;
#25426 = CARTESIAN_POINT('Ctrl Pts',(-18.2112771538204,47.8232088248091,123.273106955294)) ;
#25427 = CARTESIAN_POINT('Ctrl Pts',(-17.911781843042,47.6432197444462,123.238412336144)) ;
#25428 = CARTESIAN_POINT('Ctrl Pts',(-18.2665340735366,47.8363676117737,123.001975829454)) ;
#25429 = CARTESIAN_POINT('Ctrl Pts',(-17.9808569614933,47.6563785314108,122.899509564629)) ;
#25430 = CARTESIAN_POINT('Ctrl Pts',(-18.3927847313785,47.8497337148678,122.747421002799)) ;
#25431 = CARTESIAN_POINT('Ctrl Pts',(-18.1386436633673,47.669744634505,122.581350825213)) ;
#25432 = CARTESIAN_POINT('Ctrl Pts',(-18.5783616406369,47.8630476497569,122.537834672679)) ;
#25433 = CARTESIAN_POINT('Ctrl Pts',(-18.370652315842,47.683058569394,122.319320691079)) ;
#25434 = CARTESIAN_POINT('Ctrl Pts',(-18.7409869953793,47.8729476892044,122.407978701696)) ;
#25435 = CARTESIAN_POINT('Ctrl Pts',(-18.5739282398627,47.6929586088415,122.157012936139)) ;
#25436 = CARTESIAN_POINT('Ctrl Pts',(-18.924736336014,47.8829120923389,122.307361857159)) ;
#25437 = CARTESIAN_POINT('Ctrl Pts',(-18.8036181717246,47.702923011976,122.031241515346)) ;
#25438 = CARTESIAN_POINT('Ctrl Pts',(-19.124525129965,47.89294205946,122.239917422604)) ;
#25439 = CARTESIAN_POINT('Ctrl Pts',(-19.0533535758895,47.7129529790972,121.946938831321)) ;
#25440 = CARTESIAN_POINT('Ctrl Pts',(-19.3303060797298,47.9028443360691,122.20850438304)) ;
#25441 = CARTESIAN_POINT('Ctrl Pts',(-19.3105838879911,47.7228552557062,121.907675661922)) ;
#25442 = CARTESIAN_POINT('Ctrl Pts',(-19.6091875472562,47.9161102652382,122.214220010693)) ;
#25443 = CARTESIAN_POINT('Ctrl Pts',(-19.6591650885652,47.7361211848754,121.914819682812)) ;
#25444 = CARTESIAN_POINT('Ctrl Pts',(-19.9485239198388,47.9327317963447,122.312705470027)) ;
#25445 = CARTESIAN_POINT('Ctrl Pts',(-20.0833550247634,47.7527427159818,122.037930509702)) ;
#25446 = CARTESIAN_POINT('Ctrl Pts',(-20.2902037781463,47.9526066249893,122.561462918073)) ;
#25447 = CARTESIAN_POINT('Ctrl Pts',(-20.510453729545,47.7726175446265,122.348898697034)) ;
#25448 = CARTESIAN_POINT('Ctrl Pts',(-20.4884640691053,47.9692798330912,122.855376240776)) ;
#25449 = CARTESIAN_POINT('Ctrl Pts',(-20.7582479358267,47.7892907527283,122.71623189636)) ;
#25450 = CARTESIAN_POINT('Ctrl Pts',(-20.5789910924744,47.9825309580725,123.118806998675)) ;
#25451 = CARTESIAN_POINT('Ctrl Pts',(-20.8714295868913,47.8025418777096,123.04557591284)) ;
#25452 = CARTESIAN_POINT('Ctrl Pts',(-20.6233964771784,47.9957732768933,123.393706926206)) ;
#25453 = CARTESIAN_POINT('Ctrl Pts',(-20.9269298434521,47.8157841965304,123.389178316211)) ;
#25454 = CARTESIAN_POINT('Ctrl Pts',(-20.5867718231029,48.0125065172328,123.747531507057)) ;
#25455 = CARTESIAN_POINT('Ctrl Pts',(-20.881145520325,47.8325174368699,123.831476120658)) ;
#25456 = CARTESIAN_POINT('Ctrl Pts',(-20.4028036698389,48.0323356654207,124.126994342041)) ;
#25457 = CARTESIAN_POINT('Ctrl Pts',(-20.6511822086368,47.8523465850579,124.305796219641)) ;
#25458 = CARTESIAN_POINT('Ctrl Pts',(-20.0997742547527,48.0522603605214,124.422927439283)) ;
#25459 = CARTESIAN_POINT('Ctrl Pts',(-20.2723934902227,47.8722712801585,124.675711001554)) ;
#25460 = CARTESIAN_POINT('Ctrl Pts',(-19.7138146747958,48.0721835891048,124.597703149849)) ;
#25461 = CARTESIAN_POINT('Ctrl Pts',(-19.7899432576281,47.8921945087419,124.89417687357)) ;
#25462 = CARTESIAN_POINT('Ctrl Pts',(-19.2914240334227,48.0921107282309,124.630406193651)) ;
#25463 = CARTESIAN_POINT('Ctrl Pts',(-19.2619554888101,47.912121647868,124.935052545408)) ;
#25464 = CARTESIAN_POINT('Ctrl Pts',(-18.8840463674362,48.1119871908466,124.517801066557)) ;
#25465 = CARTESIAN_POINT('Ctrl Pts',(-18.7527354696576,47.9319981104837,124.794293876189)) ;
#25466 = CARTESIAN_POINT('Ctrl Pts',(-18.5376979877752,48.1319644194519,124.271899046843)) ;
#25467 = CARTESIAN_POINT('Ctrl Pts',(-18.3198015893089,47.951975339089,124.486914551041)) ;
#25468 = CARTESIAN_POINT('Ctrl Pts',(-18.2968188645784,48.1518992774256,123.923081812922)) ;
#25469 = CARTESIAN_POINT('Ctrl Pts',(-18.0187050938315,47.9719101970627,124.050892286809)) ;
#25470 = CARTESIAN_POINT('Ctrl Pts',(-18.1892385120565,48.1717957263564,123.513969714441)) ;
#25471 = CARTESIAN_POINT('Ctrl Pts',(-17.8842318765923,47.9918066459935,123.539502996666)) ;
#25472 = CARTESIAN_POINT('Ctrl Pts',(-18.2273051805781,48.191717010423,123.092084857011)) ;
#25473 = CARTESIAN_POINT('Ctrl Pts',(-17.9318165298211,48.0117279300601,123.012148120241)) ;
#25474 = CARTESIAN_POINT('Ctrl Pts',(-18.4074959386059,48.2116736600939,122.707887148316)) ;
#25475 = CARTESIAN_POINT('Ctrl Pts',(-18.1570558911766,48.0316845797311,122.53190203543)) ;
#25476 = CARTESIAN_POINT('Ctrl Pts',(-18.7066336703321,48.2315509532055,122.409391624937)) ;
#25477 = CARTESIAN_POINT('Ctrl Pts',(-18.5309774065162,48.0515618728427,122.158784664484)) ;
#25478 = CARTESIAN_POINT('Ctrl Pts',(-19.0894690754,48.251437425434,122.229752123671)) ;
#25479 = CARTESIAN_POINT('Ctrl Pts',(-19.0095199143223,48.0714483450711,121.934235959805)) ;
#25480 = CARTESIAN_POINT('Ctrl Pts',(-19.5143590700572,48.271498991358,122.191844649005)) ;
#25481 = CARTESIAN_POINT('Ctrl Pts',(-19.540633493891,48.0915099109951,121.886851609452)) ;
#25482 = CARTESIAN_POINT('Ctrl Pts',(-19.9220000869853,48.2913393988987,122.300380775824)) ;
#25483 = CARTESIAN_POINT('Ctrl Pts',(-20.0501821768271,48.1113503185359,122.022521216227)) ;
#25484 = CARTESIAN_POINT('Ctrl Pts',(-20.2693591113835,48.3111907228717,122.540208509566)) ;
#25485 = CARTESIAN_POINT('Ctrl Pts',(-20.4843799802069,48.1312016425088,122.322303458234)) ;
#25486 = CARTESIAN_POINT('Ctrl Pts',(-20.515946924029,48.3312439928231,122.887990451022)) ;
#25487 = CARTESIAN_POINT('Ctrl Pts',(-20.7926161664346,48.1512549124602,122.757030819445)) ;
#25488 = CARTESIAN_POINT('Ctrl Pts',(-20.6278740447954,48.3510646502064,123.29441743572)) ;
#25489 = CARTESIAN_POINT('Ctrl Pts',(-20.93252583496,48.1710755698436,123.265061844735)) ;
#25490 = CARTESIAN_POINT('Ctrl Pts',(-20.594840913384,48.3710360715369,123.717637162342)) ;
#25491 = CARTESIAN_POINT('Ctrl Pts',(-20.8912365983079,48.1910469911741,123.794086280571)) ;
#25492 = CARTESIAN_POINT('Ctrl Pts',(-20.4200275936189,48.3909295639006,124.102979449163)) ;
#25493 = CARTESIAN_POINT('Ctrl Pts',(-20.6727225902505,48.2109404835378,124.275764014104)) ;
#25494 = CARTESIAN_POINT('Ctrl Pts',(-20.1222338289871,48.4109536501417,124.407148329069)) ;
#25495 = CARTESIAN_POINT('Ctrl Pts',(-20.3004819424767,48.2309645697788,124.655976968053)) ;
#25496 = CARTESIAN_POINT('Ctrl Pts',(-19.7426972067717,48.4307585292546,124.589684508702)) ;
#25497 = CARTESIAN_POINT('Ctrl Pts',(-19.8260643109497,48.2507694488917,124.884148701362)) ;
#25498 = CARTESIAN_POINT('Ctrl Pts',(-19.3205665484207,48.4507175449524,124.633213336041)) ;
#25499 = CARTESIAN_POINT('Ctrl Pts',(-19.298401689414,48.2707284645896,124.938563164576)) ;
#25500 = CARTESIAN_POINT('Ctrl Pts',(-18.9085978348677,48.4707035685815,124.528976750497)) ;
#25501 = CARTESIAN_POINT('Ctrl Pts',(-18.7834401752579,48.2907144882186,124.808270536172)) ;
#25502 = CARTESIAN_POINT('Ctrl Pts',(-18.5595521592662,48.490512064342,124.293192736646)) ;
#25503 = CARTESIAN_POINT('Ctrl Pts',(-18.3471324483424,48.3105229839791,124.513544556307)) ;
#25504 = CARTESIAN_POINT('Ctrl Pts',(-18.3093912570992,48.5104947034476,123.949871011709)) ;
#25505 = CARTESIAN_POINT('Ctrl Pts',(-18.0344280932835,48.3305056230847,124.084394876722)) ;
#25506 = CARTESIAN_POINT('Ctrl Pts',(-18.1920511017376,48.5303761512416,123.543638375906)) ;
#25507 = CARTESIAN_POINT('Ctrl Pts',(-17.8877491679608,48.3503870708787,123.576606049549)) ;
#25508 = CARTESIAN_POINT('Ctrl Pts',(-18.2201380169056,48.5503326179791,123.120331661826)) ;
#25509 = CARTESIAN_POINT('Ctrl Pts',(-17.9228534217252,48.3703435376163,123.047472668677)) ;
#25510 = CARTESIAN_POINT('Ctrl Pts',(-18.3901149333137,48.5702100149347,122.733295429989)) ;
#25511 = CARTESIAN_POINT('Ctrl Pts',(-18.1353200268485,48.3902209345718,122.563676201082)) ;
#25512 = CARTESIAN_POINT('Ctrl Pts',(-18.6832494392057,48.59019196111,122.425805232135)) ;
#25513 = CARTESIAN_POINT('Ctrl Pts',(-18.5017348375152,48.4102028807471,122.179310317759)) ;
#25514 = CARTESIAN_POINT('Ctrl Pts',(-19.0629244099466,48.6101210601467,122.237437305555)) ;
#25515 = CARTESIAN_POINT('Ctrl Pts',(-18.9763255338847,48.4301319797839,121.943845821942)) ;
#25516 = CARTESIAN_POINT('Ctrl Pts',(-19.483901793505,48.6300496833594,122.189890024133)) ;
#25517 = CARTESIAN_POINT('Ctrl Pts',(-19.5025485758174,48.4500606029965,121.8844085627)) ;
#25518 = CARTESIAN_POINT('Ctrl Pts',(-19.8941924839498,48.6498840074658,122.2876543526)) ;
#25519 = CARTESIAN_POINT('Ctrl Pts',(-20.0154041734413,48.4698949271029,122.006602474331)) ;
#25520 = CARTESIAN_POINT('Ctrl Pts',(-20.1900657132766,48.6665362948492,122.481970833508)) ;
#25521 = CARTESIAN_POINT('Ctrl Pts',(-20.3852740340378,48.4865472144863,122.249514009236)) ;
#25522 = CARTESIAN_POINT('Ctrl Pts',(-20.375507427574,48.6797967958714,122.690222552236)) ;
#25523 = CARTESIAN_POINT('Ctrl Pts',(-20.6170557319961,48.4998077155085,122.509808729621)) ;
#25524 = CARTESIAN_POINT('Ctrl Pts',(-20.4862754015006,48.6897982730727,122.868932780703)) ;
#25525 = CARTESIAN_POINT('Ctrl Pts',(-20.7555225669231,48.5098091927098,122.73319887295)) ;
#25526 = CARTESIAN_POINT('Ctrl Pts',(-20.5642475378503,48.6998302939322,123.064902655755)) ;
#25527 = CARTESIAN_POINT('Ctrl Pts',(-20.8529891978789,48.5198412135693,122.978158629166)) ;
#25528 = CARTESIAN_POINT('Ctrl Pts',(-20.6065360548538,48.7096938376577,123.267899186555)) ;
#25529 = CARTESIAN_POINT('Ctrl Pts',(-20.9058519382839,48.5297047572949,123.231906669117)) ;
#25530 = CARTESIAN_POINT('Ctrl Pts',(-20.6135560240591,48.7196625513279,123.477368148513)) ;
#25531 = CARTESIAN_POINT('Ctrl Pts',(-20.9146324101858,48.539673470965,123.493731289981)) ;
#25532 = CARTESIAN_POINT('Ctrl Pts',(-20.5737423786962,48.7330082987316,123.755033330118)) ;
#25533 = CARTESIAN_POINT('Ctrl Pts',(-20.8648547231583,48.5530192183687,123.840870176946)) ;
#25534 = CARTESIAN_POINT('Ctrl Pts',(-20.4644055794944,48.7461588538042,124.012444095883)) ;
#25535 = CARTESIAN_POINT('Ctrl Pts',(-20.7281894338226,48.5661697734414,124.16259745941)) ;
#25536 = CARTESIAN_POINT('Ctrl Pts',(-20.2913023971137,48.7595442343541,124.234297005858)) ;
#25537 = CARTESIAN_POINT('Ctrl Pts',(-20.5118249048892,48.5795551539912,124.439903596676)) ;
#25538 = CARTESIAN_POINT('Ctrl Pts',(-20.1368920609285,48.7694321703469,124.373504586034)) ;
#25539 = CARTESIAN_POINT('Ctrl Pts',(-20.3188115906214,48.5894430899841,124.613917552832)) ;
#25540 = CARTESIAN_POINT('Ctrl Pts',(-19.9590459239484,48.7794233601596,124.485212508452)) ;
#25541 = CARTESIAN_POINT('Ctrl Pts',(-20.0965059871697,48.5994342797967,124.753554193822)) ;
#25542 = CARTESIAN_POINT('Ctrl Pts',(-19.7652457599506,48.7893754586979,124.564139501548)) ;
#25543 = CARTESIAN_POINT('Ctrl Pts',(-19.8542566549361,48.609386378335,124.852215716831)) ;
#25544 = CARTESIAN_POINT('Ctrl Pts',(-19.5587662011907,48.7994217151483,124.608490141116)) ;
#25545 = CARTESIAN_POINT('Ctrl Pts',(-19.5961577410576,48.6194326347855,124.907656726796)) ;
#25546 = CARTESIAN_POINT('Ctrl Pts',(-19.3518437628438,48.8092711625425,124.616313912249)) ;
#25547 = CARTESIAN_POINT('Ctrl Pts',(-19.337504837007,48.6292820821796,124.917439257159)) ;
#25548 = CARTESIAN_POINT('Ctrl Pts',(-19.1442698754285,48.8192338150376,124.588420325865)) ;
#25549 = CARTESIAN_POINT('Ctrl Pts',(-19.078037022272,48.6392447346748,124.882575057759)) ;
#25550 = CARTESIAN_POINT('Ctrl Pts',(-18.9435612342431,48.8292569006798,124.52425240661)) ;
#25551 = CARTESIAN_POINT('Ctrl Pts',(-18.8271502999389,48.6492678203169,124.802367820736)) ;
#25552 = CARTESIAN_POINT('Ctrl Pts',(-18.7587343657275,48.8391820164367,124.427368142674)) ;
#25553 = CARTESIAN_POINT('Ctrl Pts',(-18.5961153422512,48.6591929360738,124.681264951306)) ;
#25554 = CARTESIAN_POINT('Ctrl Pts',(-18.5915035853904,48.8492344948365,124.298186724899)) ;
#25555 = CARTESIAN_POINT('Ctrl Pts',(-18.3870750955819,48.6692454144736,124.519790373217)) ;
#25556 = CARTESIAN_POINT('Ctrl Pts',(-18.4519608110317,48.8590859935392,124.14512278795)) ;
#25557 = CARTESIAN_POINT('Ctrl Pts',(-18.2126444694148,48.6790969131764,124.328462267053)) ;
#25558 = CARTESIAN_POINT('Ctrl Pts',(-18.3393227852187,48.8690577327418,123.968347894014)) ;
#25559 = CARTESIAN_POINT('Ctrl Pts',(-18.0718445075732,48.6890686523789,124.107495060904)) ;
#25560 = CARTESIAN_POINT('Ctrl Pts',(-18.2589016789919,48.8790529405074,123.774178747308)) ;
#25561 = CARTESIAN_POINT('Ctrl Pts',(-17.9713155069276,48.6990638601446,123.86478462589)) ;
#25562 = CARTESIAN_POINT('Ctrl Pts',(-18.2135023400313,48.8890869419765,123.568194672117)) ;
#25563 = CARTESIAN_POINT('Ctrl Pts',(-17.9145635742469,48.7090978616136,123.607305099869)) ;
#25564 = CARTESIAN_POINT('Ctrl Pts',(-18.2043860504649,48.8989423000689,123.361183900461)) ;
#25565 = CARTESIAN_POINT('Ctrl Pts',(-17.9031654069168,48.718953219706,123.348541528174)) ;
#25566 = CARTESIAN_POINT('Ctrl Pts',(-18.2314583491406,48.9089417756622,123.152751792762)) ;
#25567 = CARTESIAN_POINT('Ctrl Pts',(-17.937003026666,48.7289526952993,123.088000944887)) ;
#25568 = CARTESIAN_POINT('Ctrl Pts',(-18.2934466731116,48.9188362241573,122.954149298326)) ;
#25569 = CARTESIAN_POINT('Ctrl Pts',(-18.0144858731634,48.7388471437944,122.839746756377)) ;
#25570 = CARTESIAN_POINT('Ctrl Pts',(-18.3906263668652,48.928899348385,122.766272454152)) ;
#25571 = CARTESIAN_POINT('Ctrl Pts',(-18.1359580112243,48.7489102680221,122.604899456879)) ;
#25572 = CARTESIAN_POINT('Ctrl Pts',(-18.5159623132325,48.9387389747136,122.601663674346)) ;
#25573 = CARTESIAN_POINT('Ctrl Pts',(-18.2926260056632,48.7587498943507,122.399136493447)) ;
#25574 = CARTESIAN_POINT('Ctrl Pts',(-18.6712011618515,48.9488022097566,122.457974021879)) ;
#25575 = CARTESIAN_POINT('Ctrl Pts',(-18.4866726839865,48.7688131293937,122.219522458127)) ;
#25576 = CARTESIAN_POINT('Ctrl Pts',(-18.8461785268419,48.9586962149906,122.345468773217)) ;
#25577 = CARTESIAN_POINT('Ctrl Pts',(-18.7053931823134,48.7787071346277,122.078888414331)) ;
#25578 = CARTESIAN_POINT('Ctrl Pts',(-19.038712835581,48.9686389282064,122.264147456417)) ;
#25579 = CARTESIAN_POINT('Ctrl Pts',(-18.9460602718396,48.7886498478435,121.977234200229)) ;
#25580 = CARTESIAN_POINT('Ctrl Pts',(-19.2437694434536,48.9786446680046,122.217145600225)) ;
#25581 = CARTESIAN_POINT('Ctrl Pts',(-19.2023805082056,48.7986555876417,121.918479266341)) ;
#25582 = CARTESIAN_POINT('Ctrl Pts',(-19.4541758562915,48.988665570151,122.206684633886)) ;
#25583 = CARTESIAN_POINT('Ctrl Pts',(-19.4653884139487,48.8086764897881,121.905400360003)) ;
#25584 = CARTESIAN_POINT('Ctrl Pts',(-19.6605286713295,48.9985563401998,122.232339508242)) ;
#25585 = CARTESIAN_POINT('Ctrl Pts',(-19.7233301714243,48.818567259837,121.937466358609)) ;
#25586 = CARTESIAN_POINT('Ctrl Pts',(-19.8613941607014,49.0085477509796,122.29375208743)) ;
#25587 = CARTESIAN_POINT('Ctrl Pts',(-19.9744129235702,48.8285586706167,122.014229612701)) ;
#25588 = CARTESIAN_POINT('Ctrl Pts',(-20.0477097453618,49.0184960966441,122.388760410401)) ;
#25589 = CARTESIAN_POINT('Ctrl Pts',(-20.2073088426993,48.8385070162812,122.13298779378)) ;
#25590 = CARTESIAN_POINT('Ctrl Pts',(-20.2149235430791,49.0284409547052,122.514293134598)) ;
#25591 = CARTESIAN_POINT('Ctrl Pts',(-20.4163278633967,48.8484518743424,122.289901832939)) ;
#25592 = CARTESIAN_POINT('Ctrl Pts',(-20.3591274679965,49.0384957900982,122.668825290875)) ;
#25593 = CARTESIAN_POINT('Ctrl Pts',(-20.5965846062851,48.8585067097353,122.483065165235)) ;
#25594 = CARTESIAN_POINT('Ctrl Pts',(-20.4719672533018,49.0483181621996,122.841786669687)) ;
#25595 = CARTESIAN_POINT('Ctrl Pts',(-20.7376368968491,48.8683290818368,122.699266149593)) ;
#25596 = CARTESIAN_POINT('Ctrl Pts',(-20.5553257636715,49.0583740296434,123.036047834246)) ;
#25597 = CARTESIAN_POINT('Ctrl Pts',(-20.8418372689003,48.8783849492805,122.942091527948)) ;
#25598 = CARTESIAN_POINT('Ctrl Pts',(-20.6027766814193,49.0683147595013,123.239583217983)) ;
#25599 = CARTESIAN_POINT('Ctrl Pts',(-20.9011534756052,48.8883256791384,123.196510502706)) ;
#25600 = CARTESIAN_POINT('Ctrl Pts',(-20.6147759350692,49.0782190980524,123.447461236143)) ;
#25601 = CARTESIAN_POINT('Ctrl Pts',(-20.9161549876618,48.8982300176895,123.456358415646)) ;
#25602 = CARTESIAN_POINT('Ctrl Pts',(-20.5900184388483,49.0882657794809,123.657200174385)) ;
#25603 = CARTESIAN_POINT('Ctrl Pts',(-20.8852105592629,48.908276699118,123.718532273713)) ;
#25604 = CARTESIAN_POINT('Ctrl Pts',(-20.5303023151086,49.0981612869501,123.856515276786)) ;
#25605 = CARTESIAN_POINT('Ctrl Pts',(-20.810567540589,48.9181722065873,123.967677397249)) ;
#25606 = CARTESIAN_POINT('Ctrl Pts',(-20.4353377015861,49.1082235554488,124.045507278438)) ;
#25607 = CARTESIAN_POINT('Ctrl Pts',(-20.6918640066937,48.9282344750859,124.203918318717)) ;
#25608 = CARTESIAN_POINT('Ctrl Pts',(-20.3118353609742,49.1180655457194,124.211547456422)) ;
#25609 = CARTESIAN_POINT('Ctrl Pts',(-20.5374874732684,48.9380764653565,124.4114706526)) ;
#25610 = CARTESIAN_POINT('Ctrl Pts',(-20.1594306056428,49.1280589626003,124.356110189049)) ;
#25611 = CARTESIAN_POINT('Ctrl Pts',(-20.346982966348,48.9480698822375,124.59217583248)) ;
#25612 = CARTESIAN_POINT('Ctrl Pts',(-19.9854133922224,49.1379834504525,124.471260343078)) ;
#25613 = CARTESIAN_POINT('Ctrl Pts',(-20.1294622771985,48.9579943700896,124.736115686117)) ;
#25614 = CARTESIAN_POINT('Ctrl Pts',(-19.7927208813877,49.147983084361,124.555263507083)) ;
#25615 = CARTESIAN_POINT('Ctrl Pts',(-19.8885974147487,48.9679940039981,124.841121711921)) ;
#25616 = CARTESIAN_POINT('Ctrl Pts',(-19.5886002486788,49.1579691946177,124.604484612063)) ;
#25617 = CARTESIAN_POINT('Ctrl Pts',(-19.6334469697658,48.9779801142549,124.9026502756)) ;
#25618 = CARTESIAN_POINT('Ctrl Pts',(-19.3780258214189,49.1680051458049,124.617357030462)) ;
#25619 = CARTESIAN_POINT('Ctrl Pts',(-19.3702291570135,48.988016065442,124.918743054803)) ;
#25620 = CARTESIAN_POINT('Ctrl Pts',(-19.1720854488287,49.1778617841397,124.594203709604)) ;
#25621 = CARTESIAN_POINT('Ctrl Pts',(-19.1128025382839,48.9978727037768,124.889803469788)) ;
#25622 = CARTESIAN_POINT('Ctrl Pts',(-18.9703969120688,49.1878607442177,124.535088681931)) ;
#25623 = CARTESIAN_POINT('Ctrl Pts',(-18.8606911455665,49.0078716638548,124.815911669425)) ;
#25624 = CARTESIAN_POINT('Ctrl Pts',(-18.7838271969103,49.1977559745315,124.442990126703)) ;
#25625 = CARTESIAN_POINT('Ctrl Pts',(-18.6274774420179,49.0177668941686,124.700789980476)) ;
#25626 = CARTESIAN_POINT('Ctrl Pts',(-18.6133446048038,49.2078164870001,124.317858094273)) ;
#25627 = CARTESIAN_POINT('Ctrl Pts',(-18.4143731818113,49.0278274066372,124.544376734575)) ;
#25628 = CARTESIAN_POINT('Ctrl Pts',(-18.470133520923,49.2176657785463,124.168284568055)) ;
#25629 = CARTESIAN_POINT('Ctrl Pts',(-18.2353571530203,49.0376766981834,124.357410469631)) ;
#25630 = CARTESIAN_POINT('Ctrl Pts',(-18.3525585485733,49.2276929644785,123.993322107595)) ;
#25631 = CARTESIAN_POINT('Ctrl Pts',(-18.0883869155088,49.0477038841156,124.13870846236)) ;
#25632 = CARTESIAN_POINT('Ctrl Pts',(-18.2676375468135,49.2377215009378,123.800338049473)) ;
#25633 = CARTESIAN_POINT('Ctrl Pts',(-17.9822338382996,49.0577324205749,123.89747926818)) ;
#25634 = CARTESIAN_POINT('Ctrl Pts',(-18.2180547672955,49.2475667409028,123.599398819481)) ;
#25635 = CARTESIAN_POINT('Ctrl Pts',(-17.9202532459207,49.0675776605399,123.646304603655)) ;
#25636 = CARTESIAN_POINT('Ctrl Pts',(-18.2033462478986,49.257557435826,123.389873464327)) ;
#25637 = CARTESIAN_POINT('Ctrl Pts',(-17.9018658552473,49.0775683554631,123.384397836007)) ;
#25638 = CARTESIAN_POINT('Ctrl Pts',(-18.2258094823577,49.2675952565846,123.180046491113)) ;
#25639 = CARTESIAN_POINT('Ctrl Pts',(-17.9299430170255,49.0876061762217,123.122114050778)) ;
#25640 = CARTESIAN_POINT('Ctrl Pts',(-18.282899951332,49.2774398503615,122.981108060184)) ;
#25641 = CARTESIAN_POINT('Ctrl Pts',(-18.0013047262961,49.0974507699987,122.873439403411)) ;
#25642 = CARTESIAN_POINT('Ctrl Pts',(-18.3745381888825,49.2874238457376,122.792294663389)) ;
#25643 = CARTESIAN_POINT('Ctrl Pts',(-18.1158511804771,49.1074347653747,122.637421711162)) ;
#25644 = CARTESIAN_POINT('Ctrl Pts',(-18.4971732872616,49.297372894299,122.622845943854)) ;
#25645 = CARTESIAN_POINT('Ctrl Pts',(-18.2691440175312,49.1173838139361,122.425609469171)) ;
#25646 = CARTESIAN_POINT('Ctrl Pts',(-18.6480139790816,49.3073753332735,122.476322024514)) ;
#25647 = CARTESIAN_POINT('Ctrl Pts',(-18.4576938725769,49.1273862529106,122.242453382412)) ;
#25648 = CARTESIAN_POINT('Ctrl Pts',(-18.8224872342568,49.3173965745699,122.358233047741)) ;
#25649 = CARTESIAN_POINT('Ctrl Pts',(-18.6757844901155,49.137407494207,122.094840814009)) ;
#25650 = CARTESIAN_POINT('Ctrl Pts',(-19.0122435632454,49.3272892530094,122.273107300004)) ;
#25651 = CARTESIAN_POINT('Ctrl Pts',(-18.912980073684,49.1473001726465,121.988431832938)) ;
#25652 = CARTESIAN_POINT('Ctrl Pts',(-19.2157981994734,49.337279306957,122.221395750134)) ;
#25653 = CARTESIAN_POINT('Ctrl Pts',(-19.1674232251513,49.1572902265941,121.923790931797)) ;
#25654 = CARTESIAN_POINT('Ctrl Pts',(-19.4245809336143,49.3472376681055,122.206012139912)) ;
#25655 = CARTESIAN_POINT('Ctrl Pts',(-19.4284019621495,49.1672485877426,121.904559887262)) ;
#25656 = CARTESIAN_POINT('Ctrl Pts',(-19.6317061321161,49.3571372949903,122.226481358477)) ;
#25657 = CARTESIAN_POINT('Ctrl Pts',(-19.6873094646854,49.1771482146274,121.930145178779)) ;
#25658 = CARTESIAN_POINT('Ctrl Pts',(-19.8350793181158,49.3671851917937,122.283506518214)) ;
#25659 = CARTESIAN_POINT('Ctrl Pts',(-19.941526102593,49.1871961114308,122.001425268329)) ;
#25660 = CARTESIAN_POINT('Ctrl Pts',(-20.0226907344885,49.3770805494297,122.373464971147)) ;
#25661 = CARTESIAN_POINT('Ctrl Pts',(-20.1760417540059,49.1970914690668,122.113872563223)) ;
#25662 = CARTESIAN_POINT('Ctrl Pts',(-20.1946471925884,49.3871422018863,122.496611414451)) ;
#25663 = CARTESIAN_POINT('Ctrl Pts',(-20.3909878097268,49.2071531215235,122.267804384145)) ;
#25664 = CARTESIAN_POINT('Ctrl Pts',(-20.3394609229976,49.3969868061583,122.644483147191)) ;
#25665 = CARTESIAN_POINT('Ctrl Pts',(-20.5720068053571,49.2169977257954,122.452644101985)) ;
#25666 = CARTESIAN_POINT('Ctrl Pts',(-20.4583844624104,49.4069469278563,122.816823206098)) ;
#25667 = CARTESIAN_POINT('Ctrl Pts',(-20.7206623097227,49.2269578474934,122.668068984939)) ;
#25668 = CARTESIAN_POINT('Ctrl Pts',(-20.5458863827844,49.4169849622188,123.008849967238)) ;
#25669 = CARTESIAN_POINT('Ctrl Pts',(-20.8300406886576,49.2369958818559,122.90810181371)) ;
#25670 = CARTESIAN_POINT('Ctrl Pts',(-20.5982321140661,49.4268592748053,123.209757190274)) ;
#25671 = CARTESIAN_POINT('Ctrl Pts',(-20.895474107219,49.2468701944424,123.15923667191)) ;
#25672 = CARTESIAN_POINT('Ctrl Pts',(-20.6152137828225,49.436928755588,123.420738615319)) ;
#25673 = CARTESIAN_POINT('Ctrl Pts',(-20.9167021696326,49.2569396752251,123.422962968094)) ;
#25674 = CARTESIAN_POINT('Ctrl Pts',(-20.5958761668654,49.4467630916051,123.62659808383)) ;
#25675 = CARTESIAN_POINT('Ctrl Pts',(-20.8925309748415,49.2667740112422,123.680288852952)) ;
#25676 = CARTESIAN_POINT('Ctrl Pts',(-20.540545363407,49.4567960493333,123.83012921168)) ;
#25677 = CARTESIAN_POINT('Ctrl Pts',(-20.8233682239885,49.2768069689704,123.934702843844)) ;
#25678 = CARTESIAN_POINT('Ctrl Pts',(-20.4502978778667,49.4668164479085,124.020482337261)) ;
#25679 = CARTESIAN_POINT('Ctrl Pts',(-20.7105597644519,49.2868273675456,124.172644633411)) ;
#25680 = CARTESIAN_POINT('Ctrl Pts',(-20.3306741561224,49.4766820216797,124.189933002317)) ;
#25681 = CARTESIAN_POINT('Ctrl Pts',(-20.5610300420917,49.2966929413168,124.38445939655)) ;
#25682 = CARTESIAN_POINT('Ctrl Pts',(-20.1804401966572,49.4867508963358,124.339026315722)) ;
#25683 = CARTESIAN_POINT('Ctrl Pts',(-20.3732384290242,49.3067618159729,124.570826297004)) ;
#25684 = CARTESIAN_POINT('Ctrl Pts',(-20.0104505357021,49.4965963272413,124.45713399561)) ;
#25685 = CARTESIAN_POINT('Ctrl Pts',(-20.1607506292362,49.3166072468784,124.718462326025)) ;
#25686 = CARTESIAN_POINT('Ctrl Pts',(-19.8202741615974,49.506575952112,124.545721379773)) ;
#25687 = CARTESIAN_POINT('Ctrl Pts',(-19.9230300882037,49.3265868717491,124.829197136237)) ;
#25688 = CARTESIAN_POINT('Ctrl Pts',(-19.6167083846425,49.5165946350261,124.599768391812)) ;
#25689 = CARTESIAN_POINT('Ctrl Pts',(-19.6685730451368,49.3366055546632,124.896756529863)) ;
#25690 = CARTESIAN_POINT('Ctrl Pts',(-19.4096938931667,49.5264779002099,124.617848281754)) ;
#25691 = CARTESIAN_POINT('Ctrl Pts',(-19.4098038796016,49.346488819847,124.919356964503)) ;
#25692 = CARTESIAN_POINT('Ctrl Pts',(-19.198877107358,49.5365461943013,124.599282994167)) ;
#25693 = CARTESIAN_POINT('Ctrl Pts',(-19.1462832607712,49.3565571139384,124.89615090551)) ;
#25694 = CARTESIAN_POINT('Ctrl Pts',(-18.9991919639653,49.5463763244866,124.54591031217)) ;
#25695 = CARTESIAN_POINT('Ctrl Pts',(-18.8966752356581,49.3663872441237,124.829435060277)) ;
#25696 = CARTESIAN_POINT('Ctrl Pts',(-18.8072474578189,49.5564428727018,124.456856220617)) ;
#25697 = CARTESIAN_POINT('Ctrl Pts',(-18.656744831752,49.3764537923389,124.718117896912)) ;
#25698 = CARTESIAN_POINT('Ctrl Pts',(-18.6367469946914,49.5663331213904,124.337807634366)) ;
#25699 = CARTESIAN_POINT('Ctrl Pts',(-18.4436181844938,49.3863440410275,124.569306863408)) ;
#25700 = CARTESIAN_POINT('Ctrl Pts',(-18.4876920453678,49.5763253031664,124.189801919102)) ;
#25701 = CARTESIAN_POINT('Ctrl Pts',(-18.2572992166369,49.3963362228035,124.384299698902)) ;
#25702 = CARTESIAN_POINT('Ctrl Pts',(-18.3671123398386,49.5862880837942,124.018548544852)) ;
#25703 = CARTESIAN_POINT('Ctrl Pts',(-18.1065741069592,49.4062990034313,124.170232758712)) ;
#25704 = CARTESIAN_POINT('Ctrl Pts',(-18.2781412601889,49.5961924884679,123.830276313694)) ;
#25705 = CARTESIAN_POINT('Ctrl Pts',(-17.9953598077173,49.4162034081051,123.934891647468)) ;
#25706 = CARTESIAN_POINT('Ctrl Pts',(-18.222510202651,49.606252482947,123.626250710745)) ;
#25707 = CARTESIAN_POINT('Ctrl Pts',(-17.9258209627765,49.4262634025841,123.679859999836)) ;
#25708 = CARTESIAN_POINT('Ctrl Pts',(-18.203376410996,49.6161011049168,123.420072742586)) ;
#25709 = CARTESIAN_POINT('Ctrl Pts',(-17.9019035489539,49.4361120245539,123.422136143483)) ;
#25710 = CARTESIAN_POINT('Ctrl Pts',(-18.2201708403545,49.6261315443286,123.209883238116)) ;
#25711 = CARTESIAN_POINT('Ctrl Pts',(-17.9228967151139,49.4461424639657,123.159399391363)) ;
#25712 = CARTESIAN_POINT('Ctrl Pts',(-18.2735161472999,49.6361412599634,123.00629722832)) ;
#25713 = CARTESIAN_POINT('Ctrl Pts',(-17.9895783325629,49.4561521796005,122.90491683128)) ;
#25714 = CARTESIAN_POINT('Ctrl Pts',(-18.3603293584098,49.646052012656,122.816911028997)) ;
#25715 = CARTESIAN_POINT('Ctrl Pts',(-18.0980952655541,49.4660629322931,122.668183285469)) ;
#25716 = CARTESIAN_POINT('Ctrl Pts',(-18.4785136980993,49.6559812856024,122.644833121426)) ;
#25717 = CARTESIAN_POINT('Ctrl Pts',(-18.245826326081,49.4759922052395,122.453085432562)) ;
#25718 = CARTESIAN_POINT('Ctrl Pts',(-18.6265668723548,49.666023976995,122.494326841967)) ;
#25719 = CARTESIAN_POINT('Ctrl Pts',(-18.4308927790873,49.4860348966322,122.264952869192)) ;
#25720 = CARTESIAN_POINT('Ctrl Pts',(-18.7957677209067,49.6759105102126,122.373596637961)) ;
#25721 = CARTESIAN_POINT('Ctrl Pts',(-18.6423948660931,49.4959214298497,122.114039679069)) ;
#25722 = CARTESIAN_POINT('Ctrl Pts',(-18.985209711551,49.6859036551446,122.282802300609)) ;
#25723 = CARTESIAN_POINT('Ctrl Pts',(-18.8791977037883,49.5059145747817,122.000547015104)) ;
#25724 = CARTESIAN_POINT('Ctrl Pts',(-19.1866107318813,49.6958493359811,122.226622842635)) ;
#25725 = CARTESIAN_POINT('Ctrl Pts',(-19.1309496466814,49.5158602556182,121.930322869947)) ;
#25726 = CARTESIAN_POINT('Ctrl Pts',(-19.3947080629283,49.7057965931296,122.205836498686)) ;
#25727 = CARTESIAN_POINT('Ctrl Pts',(-19.3910719340289,49.5258075127667,121.904340399635)) ;
#25728 = CARTESIAN_POINT('Ctrl Pts',(-19.6053289184389,49.7158444970016,122.221892340969)) ;
#25729 = CARTESIAN_POINT('Ctrl Pts',(-19.6543477211243,49.5358554166387,121.924410607122)) ;
#25730 = CARTESIAN_POINT('Ctrl Pts',(-19.8059348665026,49.7256921960996,122.273064256038)) ;
#25731 = CARTESIAN_POINT('Ctrl Pts',(-19.9051063909627,49.5457031157367,121.988376325681)) ;
#25732 = CARTESIAN_POINT('Ctrl Pts',(-19.9970522744167,49.7356536870782,122.358669039494)) ;
#25733 = CARTESIAN_POINT('Ctrl Pts',(-20.1440032593785,49.5556646067154,122.095383178499)) ;
#25734 = CARTESIAN_POINT('Ctrl Pts',(-20.1714411232963,49.7456831494922,122.477202699067)) ;
#25735 = CARTESIAN_POINT('Ctrl Pts',(-20.3619888762732,49.5656940691293,122.243550726972)) ;
#25736 = CARTESIAN_POINT('Ctrl Pts',(-20.3208300958534,49.7555903805921,122.622336917083)) ;
#25737 = CARTESIAN_POINT('Ctrl Pts',(-20.5487252565727,49.5756013002292,122.424969613015)) ;
#25738 = CARTESIAN_POINT('Ctrl Pts',(-20.4435688894129,49.7655367592695,122.791613197818)) ;
#25739 = CARTESIAN_POINT('Ctrl Pts',(-20.7021484057419,49.5855476789066,122.636565942067)) ;
#25740 = CARTESIAN_POINT('Ctrl Pts',(-20.5356692060204,49.7755415280784,122.980728511161)) ;
#25741 = CARTESIAN_POINT('Ctrl Pts',(-20.817273052069,49.5955524477155,122.872960551607)) ;
#25742 = CARTESIAN_POINT('Ctrl Pts',(-20.5933907296624,49.7855626490986,123.183338291841)) ;
#25743 = CARTESIAN_POINT('Ctrl Pts',(-20.8894241945035,49.6055735687357,123.126222955828)) ;
#25744 = CARTESIAN_POINT('Ctrl Pts',(-20.615012812427,49.7954535149512,123.390155066676)) ;
#25745 = CARTESIAN_POINT('Ctrl Pts',(-20.9164510303163,49.6154644345883,123.384745011977)) ;
#25746 = CARTESIAN_POINT('Ctrl Pts',(-20.6005593145487,49.8054443237105,123.599683369761)) ;
#25747 = CARTESIAN_POINT('Ctrl Pts',(-20.8983831554368,49.6254552433476,123.64665553533)) ;
#25748 = CARTESIAN_POINT('Ctrl Pts',(-20.5501038609146,49.8153949818908,123.802712023402)) ;
#25749 = CARTESIAN_POINT('Ctrl Pts',(-20.8353127628865,49.6354059015279,123.900441641724)) ;
#25750 = CARTESIAN_POINT('Ctrl Pts',(-20.4655527395291,49.8253311915329,123.993707680392)) ;
#25751 = CARTESIAN_POINT('Ctrl Pts',(-20.7296226128942,49.64534211117,124.139186358957)) ;
#25752 = CARTESIAN_POINT('Ctrl Pts',(-20.3487747189752,49.8353143582578,124.168128009877)) ;
#25753 = CARTESIAN_POINT('Ctrl Pts',(-20.5836489640743,49.6553252778949,124.357211327668)) ;
#25754 = CARTESIAN_POINT('Ctrl Pts',(-20.2023558449378,49.8453581554681,124.320235724213)) ;
#25755 = CARTESIAN_POINT('Ctrl Pts',(-20.4006247563479,49.6653690751052,124.547345114736)) ;
#25756 = CARTESIAN_POINT('Ctrl Pts',(-20.0356569177011,49.8551863716364,124.442367095108)) ;
#25757 = CARTESIAN_POINT('Ctrl Pts',(-20.1922492122206,49.6751972912734,124.70000920038)) ;
#25758 = CARTESIAN_POINT('Ctrl Pts',(-19.8457113842319,49.8652629391056,124.536063834955)) ;
#25759 = CARTESIAN_POINT('Ctrl Pts',(-19.9548171286621,49.6852738587427,124.817128808093)) ;
#25760 = CARTESIAN_POINT('Ctrl Pts',(-19.6468577220022,49.875115024795,124.594160167334)) ;
#25761 = CARTESIAN_POINT('Ctrl Pts',(-19.706248503042,49.6951259444321,124.889748332412)) ;
#25762 = CARTESIAN_POINT('Ctrl Pts',(-19.4364134670954,49.8851882922004,124.617525881756)) ;
#25763 = CARTESIAN_POINT('Ctrl Pts',(-19.4431934347657,49.7051992118375,124.918954084388)) ;
#25764 = CARTESIAN_POINT('Ctrl Pts',(-19.2299283765432,49.895029708624,124.604248514442)) ;
#25765 = CARTESIAN_POINT('Ctrl Pts',(-19.1850858539182,49.7150406282611,124.902355961624)) ;
#25766 = CARTESIAN_POINT('Ctrl Pts',(-19.0262747705676,49.9049909667667,124.55549141664)) ;
#25767 = CARTESIAN_POINT('Ctrl Pts',(-18.93051882681,49.7250018864038,124.841407931651)) ;
#25768 = CARTESIAN_POINT('Ctrl Pts',(-18.8328848698317,49.9150276431986,124.471106946337)) ;
#25769 = CARTESIAN_POINT('Ctrl Pts',(-18.6887821551517,49.7350385628358,124.735926054212)) ;
#25770 = CARTESIAN_POINT('Ctrl Pts',(-18.6596380225063,49.9249062510625,124.35654118208)) ;
#25771 = CARTESIAN_POINT('Ctrl Pts',(-18.472223638631,49.7449171706996,124.592716974689)) ;
#25772 = CARTESIAN_POINT('Ctrl Pts',(-18.5061473019625,49.9349664797013,124.211075267504)) ;
#25773 = CARTESIAN_POINT('Ctrl Pts',(-18.2803615486336,49.7549773993384,124.410883615209)) ;
#25774 = CARTESIAN_POINT('Ctrl Pts',(-18.3825837811286,49.9448334638621,124.044425289918)) ;
#25775 = CARTESIAN_POINT('Ctrl Pts',(-18.1259078276829,49.7648443834992,124.2025693445)) ;
#25776 = CARTESIAN_POINT('Ctrl Pts',(-18.2881916231086,49.9548390301148,123.856476139896)) ;
#25777 = CARTESIAN_POINT('Ctrl Pts',(-18.007919160607,49.7748499497519,123.967632043592)) ;
#25778 = CARTESIAN_POINT('Ctrl Pts',(-18.2280312076151,49.9648228185294,123.655353475487)) ;
#25779 = CARTESIAN_POINT('Ctrl Pts',(-17.9327202356782,49.7848337381665,123.716228002346)) ;
#25780 = CARTESIAN_POINT('Ctrl Pts',(-18.2037899064989,49.974868675332,123.445570734123)) ;
#25781 = CARTESIAN_POINT('Ctrl Pts',(-17.9024202751919,49.7948795949691,123.453999545748)) ;
#25782 = CARTESIAN_POINT('Ctrl Pts',(-18.2157993043397,49.984694552548,123.239349234005)) ;
#25783 = CARTESIAN_POINT('Ctrl Pts',(-17.9174338428605,49.8047054721851,123.196221483282)) ;
#25784 = CARTESIAN_POINT('Ctrl Pts',(-18.2635625382729,49.9946850283893,123.034820965476)) ;
#25785 = CARTESIAN_POINT('Ctrl Pts',(-17.9771398351836,49.8146959480264,122.940561425494)) ;
#25786 = CARTESIAN_POINT('Ctrl Pts',(-18.3470621028792,50.0047286042881,122.840884623417)) ;
#25787 = CARTESIAN_POINT('Ctrl Pts',(-18.0815158765867,49.8247395239252,122.698141841169)) ;
#25788 = CARTESIAN_POINT('Ctrl Pts',(-18.4600443984035,50.0145503965861,122.668054220945)) ;
#25789 = CARTESIAN_POINT('Ctrl Pts',(-18.2227460406671,49.8345613162232,122.482103844544)) ;
#25790 = CARTESIAN_POINT('Ctrl Pts',(-18.604009794299,50.024585362212,122.513843576675)) ;
#25791 = CARTESIAN_POINT('Ctrl Pts',(-18.4027042307795,49.8445962818491,122.289342033901)) ;
#25792 = CARTESIAN_POINT('Ctrl Pts',(-18.7727524722638,50.034610279145,122.387565767662)) ;
#25793 = CARTESIAN_POINT('Ctrl Pts',(-18.6136336981396,49.8546211987822,122.131496311253)) ;
#25794 = CARTESIAN_POINT('Ctrl Pts',(-18.957405994649,50.0444622175212,122.293741975346)) ;
#25795 = CARTESIAN_POINT('Ctrl Pts',(-18.844452425863,49.8644731371583,122.014217927815)) ;
#25796 = CARTESIAN_POINT('Ctrl Pts',(-19.1582192780616,50.0544531935459,122.23225581094)) ;
#25797 = CARTESIAN_POINT('Ctrl Pts',(-19.0954698169911,49.8744641131831,121.937362207403)) ;
#25798 = CARTESIAN_POINT('Ctrl Pts',(-19.3651677350279,50.0643710143496,122.206614010036)) ;
#25799 = CARTESIAN_POINT('Ctrl Pts',(-19.3541562238253,49.8843819339867,121.905312031361)) ;
#25800 = CARTESIAN_POINT('Ctrl Pts',(-19.5757056924692,50.0743997349142,122.217377366657)) ;
#25801 = CARTESIAN_POINT('Ctrl Pts',(-19.6173285205986,49.8944106545513,121.918768394832)) ;
#25802 = CARTESIAN_POINT('Ctrl Pts',(-19.7782617157918,50.0842826615234,122.263718063625)) ;
#25803 = CARTESIAN_POINT('Ctrl Pts',(-19.8705237928236,49.9042935811605,121.976696588945)) ;
#25804 = CARTESIAN_POINT('Ctrl Pts',(-19.9721356284537,50.0942869466428,122.345192272109)) ;
#25805 = CARTESIAN_POINT('Ctrl Pts',(-20.1128653758692,49.91429786628,122.078541501099)) ;
#25806 = CARTESIAN_POINT('Ctrl Pts',(-20.1485909447356,50.1042706278507,122.458909425641)) ;
#25807 = CARTESIAN_POINT('Ctrl Pts',(-20.3334334359267,49.9242815474878,122.22068996082)) ;
#25808 = CARTESIAN_POINT('Ctrl Pts',(-20.3033028222086,50.1143116265806,122.602499485329)) ;
#25809 = CARTESIAN_POINT('Ctrl Pts',(-20.5268216963565,49.9343225462177,122.400179102875)) ;
#25810 = CARTESIAN_POINT('Ctrl Pts',(-20.4283285557546,50.1241440714477,122.767114268604)) ;
#25811 = CARTESIAN_POINT('Ctrl Pts',(-20.683102613612,49.9441549910849,122.605949735523)) ;
#25812 = CARTESIAN_POINT('Ctrl Pts',(-20.5249823851883,50.1341390698781,122.95368511086)) ;
#25813 = CARTESIAN_POINT('Ctrl Pts',(-20.8039177883312,49.9541499895152,122.839164524174)) ;
#25814 = CARTESIAN_POINT('Ctrl Pts',(-20.5875768112403,50.1441706186277,123.155088324659)) ;
#25815 = CARTESIAN_POINT('Ctrl Pts',(-20.8821585762413,49.9641815382648,123.090919199762)) ;
#25816 = CARTESIAN_POINT('Ctrl Pts',(-20.6140645488152,50.1540359969332,123.360779768465)) ;
#25817 = CARTESIAN_POINT('Ctrl Pts',(-20.9152659613685,49.9740469165703,123.348034537658)) ;
#25818 = CARTESIAN_POINT('Ctrl Pts',(-20.6049313505838,50.1639978443934,123.570016308224)) ;
#25819 = CARTESIAN_POINT('Ctrl Pts',(-20.9038469302478,49.9840087640306,123.609580354995)) ;
#25820 = CARTESIAN_POINT('Ctrl Pts',(-20.5589419047173,50.1740327852077,123.775896953256)) ;
#25821 = CARTESIAN_POINT('Ctrl Pts',(-20.8463577366402,49.9940437048448,123.8669305923)) ;
#25822 = CARTESIAN_POINT('Ctrl Pts',(-20.4794221936391,50.1839177462248,123.967925666986)) ;
#25823 = CARTESIAN_POINT('Ctrl Pts',(-20.7469555508652,50.003928665862,124.106966043971)) ;
#25824 = CARTESIAN_POINT('Ctrl Pts',(-20.3657227466916,50.1939833551437,124.146355086132)) ;
#25825 = CARTESIAN_POINT('Ctrl Pts',(-20.6048292012254,50.0139942747808,124.330001338928)) ;
#25826 = CARTESIAN_POINT('Ctrl Pts',(-20.2260937776423,50.2038225301854,124.299012275186)) ;
#25827 = CARTESIAN_POINT('Ctrl Pts',(-20.4302906277304,50.0238334498225,124.520821628096)) ;
#25828 = CARTESIAN_POINT('Ctrl Pts',(-20.0585794048684,50.2138850856853,124.428165424389)) ;
#25829 = CARTESIAN_POINT('Ctrl Pts',(-20.2208961768224,50.0338960053224,124.682260919657)) ;
#25830 = CARTESIAN_POINT('Ctrl Pts',(-19.8741279084005,50.2237822603782,124.524475108692)) ;
#25831 = CARTESIAN_POINT('Ctrl Pts',(-19.990330202873,50.0437931800154,124.802645968509)) ;
#25832 = CARTESIAN_POINT('Ctrl Pts',(-19.675310997847,50.2337129753016,124.588171794171)) ;
#25833 = CARTESIAN_POINT('Ctrl Pts',(-19.7418079589796,50.0537238949387,124.882264366511)) ;
#25834 = CARTESIAN_POINT('Ctrl Pts',(-19.4660617887297,50.2437570033792,124.616460712568)) ;
#25835 = CARTESIAN_POINT('Ctrl Pts',(-19.4802461248259,50.0637679230163,124.91762289268)) ;
#25836 = CARTESIAN_POINT('Ctrl Pts',(-19.2583695225843,50.2536432052325,124.608282274617)) ;
#25837 = CARTESIAN_POINT('Ctrl Pts',(-19.2206304688887,50.0736541248696,124.907397165842)) ;
#25838 = CARTESIAN_POINT('Ctrl Pts',(-19.0530229072309,50.2636363716993,124.564006896081)) ;
#25839 = CARTESIAN_POINT('Ctrl Pts',(-18.9639476699514,50.0836472913365,124.852050273482)) ;
#25840 = CARTESIAN_POINT('Ctrl Pts',(-18.8594602487142,50.2735758426865,124.485214042851)) ;
#25841 = CARTESIAN_POINT('Ctrl Pts',(-18.7219951492464,50.0935867623236,124.753556604735)) ;
#25842 = CARTESIAN_POINT('Ctrl Pts',(-18.6811659538875,50.2835923570407,124.373207861046)) ;
#25843 = CARTESIAN_POINT('Ctrl Pts',(-18.4991286839628,50.1036032766778,124.613546547454)) ;
#25844 = CARTESIAN_POINT('Ctrl Pts',(-18.5262199735624,50.2935223835175,124.233262173088)) ;
#25845 = CARTESIAN_POINT('Ctrl Pts',(-18.305447857855,50.1135333031546,124.438612238836)) ;
#25846 = CARTESIAN_POINT('Ctrl Pts',(-18.3964464306137,50.303574919027,124.066486390739)) ;
#25847 = CARTESIAN_POINT('Ctrl Pts',(-18.1432330982203,50.1235858386641,124.23014085339)) ;
#25848 = CARTESIAN_POINT('Ctrl Pts',(-18.2995125290276,50.3134213222466,123.883574583666)) ;
#25849 = CARTESIAN_POINT('Ctrl Pts',(-18.0220679537995,50.1334322418838,124.001499451881)) ;
#25850 = CARTESIAN_POINT('Ctrl Pts',(-18.2344247285052,50.3233833651007,123.684524259499)) ;
#25851 = CARTESIAN_POINT('Ctrl Pts',(-17.9407108291128,50.1433942847378,123.752685556883)) ;
#25852 = CARTESIAN_POINT('Ctrl Pts',(-18.204957703029,50.3334119158914,123.475747879046)) ;
#25853 = CARTESIAN_POINT('Ctrl Pts',(-17.903879790198,50.1534228355285,123.491714650898)) ;
#25854 = CARTESIAN_POINT('Ctrl Pts',(-18.2120324651509,50.343322241609,123.267531291762)) ;
#25855 = CARTESIAN_POINT('Ctrl Pts',(-17.9127260347505,50.1633331612461,123.23144379837)) ;
#25856 = CARTESIAN_POINT('Ctrl Pts',(-18.2547290771079,50.3532571534386,123.063072199955)) ;
#25857 = CARTESIAN_POINT('Ctrl Pts',(-17.9660995838745,50.1732680730757,122.975870378448)) ;
#25858 = CARTESIAN_POINT('Ctrl Pts',(-18.3332815125372,50.3632981602067,122.867144842082)) ;
#25859 = CARTESIAN_POINT('Ctrl Pts',(-18.0642927488552,50.1833090798438,122.730962183356)) ;
#25860 = CARTESIAN_POINT('Ctrl Pts',(-18.4428498626735,50.3731857930389,122.69048500063)) ;
#25861 = CARTESIAN_POINT('Ctrl Pts',(-18.201255664043,50.193196712676,122.510138724716)) ;
#25862 = CARTESIAN_POINT('Ctrl Pts',(-18.5825766741435,50.3831762241369,122.533689688026)) ;
#25863 = CARTESIAN_POINT('Ctrl Pts',(-18.3759163267486,50.203187143774,122.314146410369)) ;
#25864 = CARTESIAN_POINT('Ctrl Pts',(-18.7469116188207,50.3931316606941,122.404071107336)) ;
#25865 = CARTESIAN_POINT('Ctrl Pts',(-18.5813368510253,50.2131425803313,122.152125343484)) ;
#25866 = CARTESIAN_POINT('Ctrl Pts',(-18.930235657484,50.4030426087935,122.305070551018)) ;
#25867 = CARTESIAN_POINT('Ctrl Pts',(-18.8104932141694,50.2230535284306,122.028377092564)) ;
#25868 = CARTESIAN_POINT('Ctrl Pts',(-19.1299354241263,50.4130546848912,122.238492971298)) ;
#25869 = CARTESIAN_POINT('Ctrl Pts',(-19.0601191774314,50.2330656045283,121.945157820195)) ;
#25870 = CARTESIAN_POINT('Ctrl Pts',(-19.3385035067007,50.4230820069661,122.207980233689)) ;
#25871 = CARTESIAN_POINT('Ctrl Pts',(-19.3208286510922,50.2430929266033,121.907019503274)) ;
#25872 = CARTESIAN_POINT('Ctrl Pts',(-19.5457289876827,50.4329407819203,122.213520699819)) ;
#25873 = CARTESIAN_POINT('Ctrl Pts',(-19.5798646279409,50.2529517015574,121.913948569486)) ;
#25874 = CARTESIAN_POINT('Ctrl Pts',(-19.822185156653,50.4463669747327,122.270169175991)) ;
#25875 = CARTESIAN_POINT('Ctrl Pts',(-19.9254133373517,50.2663778943698,121.984759551957)) ;
#25876 = CARTESIAN_POINT('Ctrl Pts',(-20.0713938613618,50.4594509905141,122.394125106127)) ;
#25877 = CARTESIAN_POINT('Ctrl Pts',(-20.2369013110527,50.2794619101513,122.13968280904)) ;
#25878 = CARTESIAN_POINT('Ctrl Pts',(-20.2838339244026,50.4729244392694,122.581328585295)) ;
#25879 = CARTESIAN_POINT('Ctrl Pts',(-20.5024950621529,50.2929353589065,122.373723117195)) ;
#25880 = CARTESIAN_POINT('Ctrl Pts',(-20.4126445774875,50.4827573970752,122.743055891855)) ;
#25881 = CARTESIAN_POINT('Ctrl Pts',(-20.6634968410946,50.3027683167123,122.575877232274)) ;
#25882 = CARTESIAN_POINT('Ctrl Pts',(-20.5134783735398,50.4927206705259,122.926629074294)) ;
#25883 = CARTESIAN_POINT('Ctrl Pts',(-20.7895391335986,50.312731590163,122.805346777483)) ;
#25884 = CARTESIAN_POINT('Ctrl Pts',(-20.5809791036652,50.5027577443438,123.126549900042)) ;
#25885 = CARTESIAN_POINT('Ctrl Pts',(-20.8739118055342,50.322768663981,123.05524832364)) ;
#25886 = CARTESIAN_POINT('Ctrl Pts',(-20.6126206713393,50.5126327473555,123.331753130747)) ;
#25887 = CARTESIAN_POINT('Ctrl Pts',(-20.9134611751376,50.3326436669926,123.311752830501)) ;
#25888 = CARTESIAN_POINT('Ctrl Pts',(-20.608057270493,50.5227004269817,123.543329168377)) ;
#25889 = CARTESIAN_POINT('Ctrl Pts',(-20.9077542261225,50.3427113466188,123.576222416539)) ;
#25890 = CARTESIAN_POINT('Ctrl Pts',(-20.5678626540345,50.5325412771994,123.746296518726)) ;
#25891 = CARTESIAN_POINT('Ctrl Pts',(-20.857508009601,50.3525521968365,123.829932935511)) ;
#25892 = CARTESIAN_POINT('Ctrl Pts',(-20.4670213376231,50.5458774756753,124.007888589382)) ;
#25893 = CARTESIAN_POINT('Ctrl Pts',(-20.7314548291478,50.3658883953125,124.156910684336)) ;
#25894 = CARTESIAN_POINT('Ctrl Pts',(-20.3015547858526,50.5590949994898,124.235123685654)) ;
#25895 = CARTESIAN_POINT('Ctrl Pts',(-20.524653068368,50.3791059191269,124.440925618285)) ;
#25896 = CARTESIAN_POINT('Ctrl Pts',(-20.0837840031638,50.572429925981,124.411566237074)) ;
#25897 = CARTESIAN_POINT('Ctrl Pts',(-20.252395006723,50.3924408456182,124.66151880778)) ;
#25898 = CARTESIAN_POINT('Ctrl Pts',(-19.9002502528585,50.5824130265756,124.513455062962)) ;
#25899 = CARTESIAN_POINT('Ctrl Pts',(-20.0229851842833,50.4024239462128,124.788869046757)) ;
#25900 = CARTESIAN_POINT('Ctrl Pts',(-19.7005468923068,50.5924578024753,124.582032085012)) ;
#25901 = CARTESIAN_POINT('Ctrl Pts',(-19.7733522297728,50.4124687221124,124.874590001612)) ;
#25902 = CARTESIAN_POINT('Ctrl Pts',(-19.4967087425705,50.6022757256612,124.614562625887)) ;
#25903 = CARTESIAN_POINT('Ctrl Pts',(-19.5185568926512,50.4222866452983,124.915250650633)) ;
#25904 = CARTESIAN_POINT('Ctrl Pts',(-19.2854718592234,50.6123250396165,124.611560869832)) ;
#25905 = CARTESIAN_POINT('Ctrl Pts',(-19.2545052235582,50.4323359592536,124.911493375565)) ;
#25906 = CARTESIAN_POINT('Ctrl Pts',(-19.0108573397302,50.6256287802391,124.558525690301)) ;
#25907 = CARTESIAN_POINT('Ctrl Pts',(-18.9112636456039,50.4456396998762,124.845209773811)) ;
#25908 = CARTESIAN_POINT('Ctrl Pts',(-18.6949673472923,50.6421189757157,124.406294928456)) ;
#25909 = CARTESIAN_POINT('Ctrl Pts',(-18.5163636183236,50.4621298953529,124.654888417403)) ;
#25910 = CARTESIAN_POINT('Ctrl Pts',(-18.4467378433555,50.6588381406404,124.151872297138)) ;
#25911 = CARTESIAN_POINT('Ctrl Pts',(-18.2061311342259,50.4788490602775,124.336917792434)) ;
#25912 = CARTESIAN_POINT('Ctrl Pts',(-18.311368251597,50.6719991343105,123.910554451692)) ;
#25913 = CARTESIAN_POINT('Ctrl Pts',(-18.0368827272804,50.4920100539476,124.035219084609)) ;
#25914 = CARTESIAN_POINT('Ctrl Pts',(-18.2412163964924,50.6819953564158,123.7124638999)) ;
#25915 = CARTESIAN_POINT('Ctrl Pts',(-17.9492027072533,50.5020062760529,123.787616040863)) ;
#25916 = CARTESIAN_POINT('Ctrl Pts',(-18.2069016120642,50.6920191959495,123.504545752087)) ;
#25917 = CARTESIAN_POINT('Ctrl Pts',(-17.9063100733637,50.5120301155866,123.527712476807)) ;
#25918 = CARTESIAN_POINT('Ctrl Pts',(-18.209328291179,50.7052125179428,123.227157565911)) ;
#25919 = CARTESIAN_POINT('Ctrl Pts',(-17.9093431973629,50.5252234375799,123.180991999699)) ;
#25920 = CARTESIAN_POINT('Ctrl Pts',(-18.3035425854847,50.7218716897201,122.88574552881)) ;
#25921 = CARTESIAN_POINT('Ctrl Pts',(-18.027118283777,50.5418826093572,122.754212984447)) ;
#25922 = CARTESIAN_POINT('Ctrl Pts',(-18.5489966287471,50.7417818652058,122.540800163354)) ;
#25923 = CARTESIAN_POINT('Ctrl Pts',(-18.333937561739,50.5617927848429,122.323039035125)) ;
#25924 = CARTESIAN_POINT('Ctrl Pts',(-18.8965967981805,50.7616718530502,122.299823800529)) ;
#25925 = CARTESIAN_POINT('Ctrl Pts',(-18.7684393921744,50.5816827726873,122.021820822919)) ;
#25926 = CARTESIAN_POINT('Ctrl Pts',(-19.3079195621711,50.781677301065,122.191706071761)) ;
#25927 = CARTESIAN_POINT('Ctrl Pts',(-19.2825937715403,50.6016882207021,121.886677539595)) ;
#25928 = CARTESIAN_POINT('Ctrl Pts',(-19.728095167199,50.8015136950923,122.229696970735)) ;
#25929 = CARTESIAN_POINT('Ctrl Pts',(-19.8078113963263,50.6215246147294,121.934169205366)) ;
#25930 = CARTESIAN_POINT('Ctrl Pts',(-20.1132481010553,50.821521488989,122.410089592141)) ;
#25931 = CARTESIAN_POINT('Ctrl Pts',(-20.2892513212485,50.6415324086261,122.159662815759)) ;
#25932 = CARTESIAN_POINT('Ctrl Pts',(-20.4112416238867,50.8413481252829,122.708392112376)) ;
#25933 = CARTESIAN_POINT('Ctrl Pts',(-20.6617398847741,50.66135904492,122.532541564671)) ;
#25934 = CARTESIAN_POINT('Ctrl Pts',(-20.5915810372585,50.8613270682368,123.093001610394)) ;
#25935 = CARTESIAN_POINT('Ctrl Pts',(-20.8871620269531,50.6813379878739,123.013304098428)) ;
#25936 = CARTESIAN_POINT('Ctrl Pts',(-20.6290028587678,50.8812588701058,123.51509334654)) ;
#25937 = CARTESIAN_POINT('Ctrl Pts',(-20.9339369378857,50.701269789743,123.540918150504)) ;
#25938 = CARTESIAN_POINT('Ctrl Pts',(-20.5220534572003,50.9010831706034,123.922954659986)) ;
#25939 = CARTESIAN_POINT('Ctrl Pts',(-20.8002489892957,50.7210940902405,124.050742162796)) ;
#25940 = CARTESIAN_POINT('Ctrl Pts',(-20.2786120446289,50.9211791719433,124.273908281155)) ;
#25941 = CARTESIAN_POINT('Ctrl Pts',(-20.4959470937685,50.7411900915803,124.489434446394)) ;
#25942 = CARTESIAN_POINT('Ctrl Pts',(-19.9357982920383,50.9409375880472,124.517186763173)) ;
#25943 = CARTESIAN_POINT('Ctrl Pts',(-20.0674250455001,50.7609485076843,124.793529199864)) ;
#25944 = CARTESIAN_POINT('Ctrl Pts',(-19.5241716085477,50.9610312809313,124.630773509642)) ;
#25945 = CARTESIAN_POINT('Ctrl Pts',(-19.5529196248031,50.7810422005684,124.935512899744)) ;
#25946 = CARTESIAN_POINT('Ctrl Pts',(-19.2461442415946,50.9741422468379,124.608669218602)) ;
#25947 = CARTESIAN_POINT('Ctrl Pts',(-19.2053312341041,50.7941531664751,124.907880339345)) ;
#25948 = CARTESIAN_POINT('Ctrl Pts',(-19.1099467513572,50.9808556216258,124.573813086965)) ;
#25949 = CARTESIAN_POINT('Ctrl Pts',(-19.035117438896,50.8008665412629,124.864312062334)) ;
#25950 = CARTESIAN_POINT('',(-18.3453504609641,12.1170521379794,124.06799281052)) ;
#25951 = CARTESIAN_POINT('',(-18.1677493295881,12.0000000003486,124.153922006539)) ;
#25952 = CARTESIAN_POINT('Ctrl Pts',(-18.3453506846598,12.1170517297128,124.067992703577)) ;
#25953 = CARTESIAN_POINT('Ctrl Pts',(-18.3273547545627,12.1040527313448,124.079975178566)) ;
#25954 = CARTESIAN_POINT('Ctrl Pts',(-18.3083333684475,12.0907998558922,124.09127094444)) ;
#25955 = CARTESIAN_POINT('Ctrl Pts',(-18.2886731982766,12.0775160379758,124.101757360079)) ;
#25956 = CARTESIAN_POINT('Ctrl Pts',(-18.2692156830702,12.0643691482562,124.112135682849)) ;
#25957 = CARTESIAN_POINT('Ctrl Pts',(-18.2491324210418,12.0511919516622,124.121719977723)) ;
#25958 = CARTESIAN_POINT('Ctrl Pts',(-18.2288350990488,12.0382005709879,124.130431431038)) ;
#25959 = CARTESIAN_POINT('Ctrl Pts',(-18.2099998134723,12.0261449724652,124.138515389653)) ;
#25960 = CARTESIAN_POINT('Ctrl Pts',(-18.1909807008646,12.0142493854672,124.145847642283)) ;
#25961 = CARTESIAN_POINT('Ctrl Pts',(-18.1721346154261,12.0026865128952,124.152408160415)) ;
#25962 = CARTESIAN_POINT('Ctrl Pts',(-18.1706717407006,12.0017889772188,124.152917402304)) ;
#25963 = CARTESIAN_POINT('Ctrl Pts',(-18.1692099210947,12.0008934462135,124.153422017229)) ;
#25964 = CARTESIAN_POINT('Ctrl Pts',(-18.1677493297433,12.0000000006492,124.15392200753)) ;
#25965 = CARTESIAN_POINT('',(-20.4774766531755,11.9999999945496,124.060997935139)) ;
#25966 = CARTESIAN_POINT('Ctrl Pts',(-18.1677493286892,12.0000000000044,124.153922007891)) ;
#25967 = CARTESIAN_POINT('Ctrl Pts',(-18.1945949699472,12.0000000000052,124.192762375168)) ;
#25968 = CARTESIAN_POINT('Ctrl Pts',(-18.2231913450481,12.,124.230077351763)) ;
#25969 = CARTESIAN_POINT('Ctrl Pts',(-18.2533557201733,12.,124.265730705607)) ;
#25970 = CARTESIAN_POINT('Ctrl Pts',(-18.3070716273031,12.,124.329221238262)) ;
#25971 = CARTESIAN_POINT('Ctrl Pts',(-18.3658179607988,12.,124.387509039275)) ;
#25972 = CARTESIAN_POINT('Ctrl Pts',(-18.4293591975901,12.,124.440302750152)) ;
#25973 = CARTESIAN_POINT('Ctrl Pts',(-18.4721278246092,12.,124.475837383148)) ;
#25974 = CARTESIAN_POINT('Ctrl Pts',(-18.5170404532172,11.9999999780286,124.508860536102)) ;
#25975 = CARTESIAN_POINT('Ctrl Pts',(-18.5633173760341,11.9999999870879,124.538960478783)) ;
#25976 = CARTESIAN_POINT('Ctrl Pts',(-18.5859252873497,11.9999999915136,124.553665363925)) ;
#25977 = CARTESIAN_POINT('Ctrl Pts',(-18.6088594509681,12.,124.5676730489)) ;
#25978 = CARTESIAN_POINT('Ctrl Pts',(-18.6320326861663,12.,124.580938074486)) ;
#25979 = CARTESIAN_POINT('Ctrl Pts',(-18.6893271138161,12.,124.613735050922)) ;
#25980 = CARTESIAN_POINT('Ctrl Pts',(-18.7481011236149,12.0000000184731,124.642002547875)) ;
#25981 = CARTESIAN_POINT('Ctrl Pts',(-18.808591238206,12.0000000058446,124.665966773295)) ;
#25982 = CARTESIAN_POINT('Ctrl Pts',(-18.8228268816011,12.0000000028726,124.67160647442)) ;
#25983 = CARTESIAN_POINT('Ctrl Pts',(-18.8371573708013,12.,124.677007733495)) ;
#25984 = CARTESIAN_POINT('Ctrl Pts',(-18.8515854105586,12.,124.682173315896)) ;
#25985 = CARTESIAN_POINT('Ctrl Pts',(-18.9030665387764,12.,124.700604787836)) ;
#25986 = CARTESIAN_POINT('Ctrl Pts',(-18.9557905285045,11.9999999840944,124.716036106706)) ;
#25987 = CARTESIAN_POINT('Ctrl Pts',(-19.008882066701,11.9999999908829,124.72827599868)) ;
#25988 = CARTESIAN_POINT('Ctrl Pts',(-19.0340552814171,11.9999999941016,124.734079511617)) ;
#25989 = CARTESIAN_POINT('Ctrl Pts',(-19.0593118422177,12.,124.739165805691)) ;
#25990 = CARTESIAN_POINT('Ctrl Pts',(-19.0845623342861,12.,124.74351576159)) ;
#25991 = CARTESIAN_POINT('Ctrl Pts',(-19.1577583409821,12.,124.756125393127)) ;
#25992 = CARTESIAN_POINT('Ctrl Pts',(-19.230888238426,12.0000000080437,124.762545609574)) ;
#25993 = CARTESIAN_POINT('Ctrl Pts',(-19.3039949949029,12.000000000871,124.763034471808)) ;
#25994 = CARTESIAN_POINT('Ctrl Pts',(-19.3094679922311,12.0000000003341,124.763071069543)) ;
#25995 = CARTESIAN_POINT('Ctrl Pts',(-19.3149408364502,12.,124.763074419256)) ;
#25996 = CARTESIAN_POINT('Ctrl Pts',(-19.3204135341477,12.,124.763044626916)) ;
#25997 = CARTESIAN_POINT('Ctrl Pts',(-19.3794328487692,12.,124.762723336828)) ;
#25998 = CARTESIAN_POINT('Ctrl Pts',(-19.4384497074752,11.9999999923458,124.758547342743)) ;
#25999 = CARTESIAN_POINT('Ctrl Pts',(-19.4965921528861,11.9999999967179,124.750604967653)) ;
#26000 = CARTESIAN_POINT('Ctrl Pts',(-19.5160203292204,11.9999999981788,124.747951039654)) ;
#26001 = CARTESIAN_POINT('Ctrl Pts',(-19.5353513049696,12.,124.744876594293)) ;
#26002 = CARTESIAN_POINT('Ctrl Pts',(-19.5545538432223,12.,124.741384949252)) ;
#26003 = CARTESIAN_POINT('Ctrl Pts',(-19.6197198756548,12.,124.729535648341)) ;
#26004 = CARTESIAN_POINT('Ctrl Pts',(-19.6833426730566,11.9999999984792,124.712894770648)) ;
#26005 = CARTESIAN_POINT('Ctrl Pts',(-19.7447602360297,11.9999999996238,124.691979808156)) ;
#26006 = CARTESIAN_POINT('Ctrl Pts',(-19.7558013132351,11.9999999998296,124.688219911077)) ;
#26007 = CARTESIAN_POINT('Ctrl Pts',(-19.7667712412664,12.,124.684321819739)) ;
#26008 = CARTESIAN_POINT('Ctrl Pts',(-19.7776663287723,12.,124.680288453161)) ;
#26009 = CARTESIAN_POINT('Ctrl Pts',(-19.8493651138227,12.,124.653745528828)) ;
#26010 = CARTESIAN_POINT('Ctrl Pts',(-19.9179051001858,12.,124.621313026741)) ;
#26011 = CARTESIAN_POINT('Ctrl Pts',(-19.9832030943918,12.,124.583131212673)) ;
#26012 = CARTESIAN_POINT('Ctrl Pts',(-20.0330168871335,12.,124.554003503689)) ;
#26013 = CARTESIAN_POINT('Ctrl Pts',(-20.0809465543055,11.9999999945779,124.521528166539)) ;
#26014 = CARTESIAN_POINT('Ctrl Pts',(-20.1262764357416,11.9999999978038,124.486203412323)) ;
#26015 = CARTESIAN_POINT('Ctrl Pts',(-20.14045609981,11.9999999988129,124.475153457366)) ;
#26016 = CARTESIAN_POINT('Ctrl Pts',(-20.1543817184891,12.,124.463824515856)) ;
#26017 = CARTESIAN_POINT('Ctrl Pts',(-20.168032314776,12.,124.452231354919)) ;
#26018 = CARTESIAN_POINT('Ctrl Pts',(-20.2125408174554,12.,124.414431230746)) ;
#26019 = CARTESIAN_POINT('Ctrl Pts',(-20.2540726431959,11.9999999905181,124.373868567748)) ;
#26020 = CARTESIAN_POINT('Ctrl Pts',(-20.2922988408341,11.9999999963922,124.331241807081)) ;
#26021 = CARTESIAN_POINT('Ctrl Pts',(-20.3034097999745,11.9999999980996,124.318851765033)) ;
#26022 = CARTESIAN_POINT('Ctrl Pts',(-20.3142416754177,12.,124.306287061013)) ;
#26023 = CARTESIAN_POINT('Ctrl Pts',(-20.3247868528159,12.,124.293564166379)) ;
#26024 = CARTESIAN_POINT('Ctrl Pts',(-20.3674983751124,12.,124.242032155362)) ;
#26025 = CARTESIAN_POINT('Ctrl Pts',(-20.4055506162159,12.0000000087182,124.187851504183)) ;
#26026 = CARTESIAN_POINT('Ctrl Pts',(-20.43911209806,12.0000000012434,124.130991328396)) ;
#26027 = CARTESIAN_POINT('Ctrl Pts',(-20.4424600811825,12.0000000004977,124.125319144142)) ;
#26028 = CARTESIAN_POINT('Ctrl Pts',(-20.4457633499417,12.,124.119620329616)) ;
#26029 = CARTESIAN_POINT('Ctrl Pts',(-20.449022055999,12.,124.113894878083)) ;
#26030 = CARTESIAN_POINT('Ctrl Pts',(-20.4589227820742,12.,124.09649959103)) ;
#26031 = CARTESIAN_POINT('Ctrl Pts',(-20.4684137702848,11.999999998883,124.078855580405)) ;
#26032 = CARTESIAN_POINT('Ctrl Pts',(-20.4774766407636,11.9999999981016,124.06099792884)) ;
#26033 = CARTESIAN_POINT('Ctrl Pts',(-20.4774766589072,11.9999999855698,124.060997939105)) ;
#26034 = CARTESIAN_POINT('Ctrl Pts',(-20.4738210693409,12.0003235019738,124.067013058878)) ;
#26035 = CARTESIAN_POINT('Ctrl Pts',(-20.4701147454655,12.0006473274418,124.072997181455)) ;
#26036 = CARTESIAN_POINT('Ctrl Pts',(-20.4599245187432,12.0015264826127,124.089143747839)) ;
#26037 = CARTESIAN_POINT('Ctrl Pts',(-20.4533438467063,12.0020823228166,124.099244203208)) ;
#26038 = CARTESIAN_POINT('Ctrl Pts',(-20.4376630195742,12.0033791105184,124.122567490034)) ;
#26039 = CARTESIAN_POINT('Ctrl Pts',(-20.428452184928,12.00412012563,124.13571341996)) ;
#26040 = CARTESIAN_POINT('Ctrl Pts',(-20.4137874661628,12.0052668735873,124.155808361001)) ;
#26041 = CARTESIAN_POINT('Ctrl Pts',(-20.4085087918783,12.0056733952083,124.162883083463)) ;
#26042 = CARTESIAN_POINT('Ctrl Pts',(-20.3995692854148,12.0063514271215,124.174603146536)) ;
#26043 = CARTESIAN_POINT('Ctrl Pts',(-20.3959496291952,12.0066232068953,124.179279473883)) ;
#26044 = CARTESIAN_POINT('Ctrl Pts',(-20.389035901371,12.0071371506433,124.188081737764)) ;
#26045 = CARTESIAN_POINT('Ctrl Pts',(-20.3857486085966,12.0073793602748,124.192212832432)) ;
#26046 = CARTESIAN_POINT('Ctrl Pts',(-20.3788189177888,12.0078854994504,124.200808937747)) ;
#26047 = CARTESIAN_POINT('Ctrl Pts',(-20.3751716169832,12.0081493836918,124.205269839539)) ;
#26048 = CARTESIAN_POINT('Ctrl Pts',(-20.3655403449871,12.0088397827434,124.216884728752)) ;
#26049 = CARTESIAN_POINT('Ctrl Pts',(-20.3595069177169,12.0092658930284,124.223997249251)) ;
#26050 = CARTESIAN_POINT('Ctrl Pts',(-20.3387248785043,12.0107130376805,124.247947606164)) ;
#26051 = CARTESIAN_POINT('Ctrl Pts',(-20.3236038917401,12.0117313025691,124.2644565148)) ;
#26052 = CARTESIAN_POINT('Ctrl Pts',(-20.2970853611994,12.0134701087367,124.291892010138)) ;
#26053 = CARTESIAN_POINT('Ctrl Pts',(-20.285909288432,12.0141897642512,124.303024936002)) ;
#26054 = CARTESIAN_POINT('Ctrl Pts',(-20.2687677941853,12.0152756144541,124.319465750278)) ;
#26055 = CARTESIAN_POINT('Ctrl Pts',(-20.2629573020348,12.0156406853718,124.324932900176)) ;
#26056 = CARTESIAN_POINT('Ctrl Pts',(-20.251036665777,12.0163837308229,124.335935903857)) ;
#26057 = CARTESIAN_POINT('Ctrl Pts',(-20.2449232877602,12.0167617110627,124.341467683723)) ;
#26058 = CARTESIAN_POINT('Ctrl Pts',(-20.2220121681254,12.0181669907764,124.361790538748)) ;
#26059 = CARTESIAN_POINT('Ctrl Pts',(-20.2048728639287,12.0191962596192,124.376190102632)) ;
#26060 = CARTESIAN_POINT('Ctrl Pts',(-20.1805077183176,12.020627613373,124.395568605511)) ;
#26061 = CARTESIAN_POINT('Ctrl Pts',(-20.1736021343383,12.0210298357192,124.40094346769)) ;
#26062 = CARTESIAN_POINT('Ctrl Pts',(-20.1618123540089,12.0217104198955,124.409922680335)) ;
#26063 = CARTESIAN_POINT('Ctrl Pts',(-20.1569573042242,12.0219889590695,124.413564771728)) ;
#26064 = CARTESIAN_POINT('Ctrl Pts',(-20.1481685120957,12.0224899453031,124.42005833285)) ;
#26065 = CARTESIAN_POINT('Ctrl Pts',(-20.144244314968,12.0227124739396,124.422922494172)) ;
#26066 = CARTESIAN_POINT('Ctrl Pts',(-20.1318578952527,12.0234112809899,124.431852782512)) ;
#26067 = CARTESIAN_POINT('Ctrl Pts',(-20.12333651938,12.0238869104373,124.437836103776)) ;
#26068 = CARTESIAN_POINT('Ctrl Pts',(-20.0999049834915,12.0251830662214,124.453855348649)) ;
#26069 = CARTESIAN_POINT('Ctrl Pts',(-20.0848515943592,12.0260031798493,124.463677252077)) ;
#26070 = CARTESIAN_POINT('Ctrl Pts',(-20.0624930779402,12.0272072193321,124.477587525388)) ;
#26071 = CARTESIAN_POINT('Ctrl Pts',(-20.0553503676959,12.0275897944985,124.481932557054)) ;
#26072 = CARTESIAN_POINT('Ctrl Pts',(-20.0425338660351,12.0282728948922,124.489553957019)) ;
#26073 = CARTESIAN_POINT('Ctrl Pts',(-20.0368768872401,12.0285732479674,124.492857991191)) ;
#26074 = CARTESIAN_POINT('Ctrl Pts',(-20.0234686598769,12.029282547681,124.500548526906)) ;
#26075 = CARTESIAN_POINT('Ctrl Pts',(-20.0156959971541,12.0296917004838,124.504896952722)) ;
#26076 = CARTESIAN_POINT('Ctrl Pts',(-19.9832852508231,12.0313896109435,124.522577080194)) ;
#26077 = CARTESIAN_POINT('Ctrl Pts',(-19.9582490050827,12.0326821394932,124.535161706767)) ;
#26078 = CARTESIAN_POINT('Ctrl Pts',(-19.9230189690532,12.0344692748047,124.551411041485)) ;
#26079 = CARTESIAN_POINT('Ctrl Pts',(-19.9131686659644,12.0349656308202,124.55580067594)) ;
#26080 = CARTESIAN_POINT('Ctrl Pts',(-19.8963223391377,12.0358088084923,124.563048175201)) ;
#26081 = CARTESIAN_POINT('Ctrl Pts',(-19.8893549590441,12.0361558985472,124.565971056342)) ;
#26082 = CARTESIAN_POINT('Ctrl Pts',(-19.8789376232523,12.0366724659772,124.570230572808)) ;
#26083 = CARTESIAN_POINT('Ctrl Pts',(-19.8755075506304,12.0368421718385,124.57161534704)) ;
#26084 = CARTESIAN_POINT('Ctrl Pts',(-19.8648462191222,12.0373684864209,124.575864555093)) ;
#26085 = CARTESIAN_POINT('Ctrl Pts',(-19.8575943272026,12.0377248296873,124.578676739984)) ;
#26086 = CARTESIAN_POINT('Ctrl Pts',(-19.8378010135038,12.0386931774225,124.586140557026)) ;
#26087 = CARTESIAN_POINT('Ctrl Pts',(-19.8252104081584,12.0393045167842,124.590658865802)) ;
#26088 = CARTESIAN_POINT('Ctrl Pts',(-19.7956964157781,12.0407285350002,124.600718645363)) ;
#26089 = CARTESIAN_POINT('Ctrl Pts',(-19.7787223471021,12.0415406448223,124.606102290676)) ;
#26090 = CARTESIAN_POINT('Ctrl Pts',(-19.7516131399652,12.0428310586428,124.614067211164)) ;
#26091 = CARTESIAN_POINT('Ctrl Pts',(-19.7415506724082,12.0433086936194,124.616887076666)) ;
#26092 = CARTESIAN_POINT('Ctrl Pts',(-19.7206893896845,12.0442965319979,124.62245200034)) ;
#26093 = CARTESIAN_POINT('Ctrl Pts',(-19.7098868378585,12.0448067489102,124.625179515279)) ;
#26094 = CARTESIAN_POINT('Ctrl Pts',(-19.6757140325349,12.0464169892136,124.633323363431)) ;
#26095 = CARTESIAN_POINT('Ctrl Pts',(-19.6522235742641,12.0475184551027,124.638211570731)) ;
#26096 = CARTESIAN_POINT('Ctrl Pts',(-19.6171103822421,12.04915641197,124.64446990586)) ;
#26097 = CARTESIAN_POINT('Ctrl Pts',(-19.6055854942518,12.0496926476333,124.646357795818)) ;
#26098 = CARTESIAN_POINT('Ctrl Pts',(-19.5857186916462,12.0506143194798,124.649326939591)) ;
#26099 = CARTESIAN_POINT('Ctrl Pts',(-19.5773891963475,12.0509999315481,124.650485997081)) ;
#26100 = CARTESIAN_POINT('Ctrl Pts',(-19.5624628516343,12.0516892997172,124.652409678574)) ;
#26101 = CARTESIAN_POINT('Ctrl Pts',(-19.5558704031638,12.0519931973621,124.653205952913)) ;
#26102 = CARTESIAN_POINT('Ctrl Pts',(-19.5293790930094,12.0532118418825,124.656191758732)) ;
#26103 = CARTESIAN_POINT('Ctrl Pts',(-19.5094352662898,12.0541231886579,124.657955659061)) ;
#26104 = CARTESIAN_POINT('Ctrl Pts',(-19.4793903244375,12.0554955416909,124.659886970216)) ;
#26105 = CARTESIAN_POINT('Ctrl Pts',(-19.4693155323012,12.0559555993903,124.660412209013)) ;
#26106 = CARTESIAN_POINT('Ctrl Pts',(-19.4532847238482,12.056688238072,124.661053482769)) ;
#26107 = CARTESIAN_POINT('Ctrl Pts',(-19.4473323281987,12.0569604032001,124.661248997778)) ;
#26108 = CARTESIAN_POINT('Ctrl Pts',(-19.4411847351566,12.0572417066106,124.661406952228)) ;
#26109 = CARTESIAN_POINT('Ctrl Pts',(-19.4409906964236,12.0572505857107,124.661411892577)) ;
#26110 = CARTESIAN_POINT('Ctrl Pts',(-19.4406116208727,12.057267932418,124.661421455728)) ;
#26111 = CARTESIAN_POINT('Ctrl Pts',(-19.4404265840258,12.0572764000064,124.661426082631)) ;
#26112 = CARTESIAN_POINT('Ctrl Pts',(-19.4400644514001,12.0572929721822,124.661435057384)) ;
#26113 = CARTESIAN_POINT('Ctrl Pts',(-19.439887355894,12.05730107674,124.661439408682)) ;
#26114 = CARTESIAN_POINT('Ctrl Pts',(-19.4395401349731,12.0573169672439,124.661447866165)) ;
#26115 = CARTESIAN_POINT('Ctrl Pts',(-19.439370009467,12.0573247531797,124.661451975259)) ;
#26116 = CARTESIAN_POINT('Ctrl Pts',(-19.4390358319261,12.0573400474351,124.661459978471)) ;
#26117 = CARTESIAN_POINT('Ctrl Pts',(-19.438871779903,12.057347555742,124.661463875027)) ;
#26118 = CARTESIAN_POINT('Ctrl Pts',(-19.4385489143416,12.0573623329221,124.661471480101)) ;
#26119 = CARTESIAN_POINT('Ctrl Pts',(-19.4383901011446,12.0573696017696,124.661475190643)) ;
#26120 = CARTESIAN_POINT('Ctrl Pts',(-19.438076929371,12.0573839358809,124.661482447917)) ;
#26121 = CARTESIAN_POINT('Ctrl Pts',(-19.4379225708226,12.0573910011349,124.661485996324)) ;
#26122 = CARTESIAN_POINT('Ctrl Pts',(-19.437617563227,12.057404962142,124.661492951323)) ;
#26123 = CARTESIAN_POINT('Ctrl Pts',(-19.4374669140344,12.0574118578949,124.661496359277)) ;
#26124 = CARTESIAN_POINT('Ctrl Pts',(-19.4371686066429,12.0574255127705,124.661503053555)) ;
#26125 = CARTESIAN_POINT('Ctrl Pts',(-19.4370209486558,12.0574322718779,124.661506340945)) ;
#26126 = CARTESIAN_POINT('Ctrl Pts',(-19.436727922283,12.0574456855551,124.661512812793)) ;
#26127 = CARTESIAN_POINT('Ctrl Pts',(-19.4365825538598,12.0574523401223,124.661515998056)) ;
#26128 = CARTESIAN_POINT('Ctrl Pts',(-19.4362934092924,12.0574655766305,124.661522283219)) ;
#26129 = CARTESIAN_POINT('Ctrl Pts',(-19.4361496331152,12.0574721585701,124.661525383671)) ;
#26130 = CARTESIAN_POINT('Ctrl Pts',(-19.4358629669209,12.0574852821421,124.661531515974)) ;
#26131 = CARTESIAN_POINT('Ctrl Pts',(-19.4357200770283,12.0574918237673,124.661534548127)) ;
#26132 = CARTESIAN_POINT('Ctrl Pts',(-19.4354344547226,12.0575049000676,124.661540560083)) ;
#26133 = CARTESIAN_POINT('Ctrl Pts',(-19.4352917223177,12.0575114347421,124.66154353994)) ;
#26134 = CARTESIAN_POINT('Ctrl Pts',(-19.4350056466662,12.0575245323185,124.661549463377)) ;
#26135 = CARTESIAN_POINT('Ctrl Pts',(-19.434862303283,12.0575310952277,124.661552406749)) ;
#26136 = CARTESIAN_POINT('Ctrl Pts',(-19.4345741763691,12.0575442872488,124.661558273474)) ;
#26137 = CARTESIAN_POINT('Ctrl Pts',(-19.4344293929624,12.0575509163576,124.661561196325)) ;
#26138 = CARTESIAN_POINT('Ctrl Pts',(-19.4341374718464,12.0575642826441,124.661567038807)) ;
#26139 = CARTESIAN_POINT('Ctrl Pts',(-19.4339903339254,12.057571019836,124.661569957617)) ;
#26140 = CARTESIAN_POINT('Ctrl Pts',(-19.4336926702877,12.0575846496269,124.661575809852)) ;
#26141 = CARTESIAN_POINT('Ctrl Pts',(-19.4335421444777,12.0575915422368,124.66157874207)) ;
#26142 = CARTESIAN_POINT('Ctrl Pts',(-19.4332365079462,12.0576055377026,124.661584640579)) ;
#26143 = CARTESIAN_POINT('Ctrl Pts',(-19.4330813976021,12.0576126405504,124.661587605182)) ;
#26144 = CARTESIAN_POINT('Ctrl Pts',(-19.4327651732268,12.0576271214925,124.661593590244)) ;
#26145 = CARTESIAN_POINT('Ctrl Pts',(-19.4326040590737,12.0576344996049,124.661596608426)) ;
#26146 = CARTESIAN_POINT('Ctrl Pts',(-19.4322740989793,12.0576496102551,124.661602725804)) ;
#26147 = CARTESIAN_POINT('Ctrl Pts',(-19.4321052529801,12.0576573428126,124.661605821939)) ;
#26148 = CARTESIAN_POINT('Ctrl Pts',(-19.4317576680302,12.0576732613833,124.661612125155)) ;
#26149 = CARTESIAN_POINT('Ctrl Pts',(-19.4315789289088,12.0576814474273,124.661615328111)) ;
#26150 = CARTESIAN_POINT('Ctrl Pts',(-19.4312087741874,12.0576984005296,124.661621881751)) ;
#26151 = CARTESIAN_POINT('Ctrl Pts',(-19.4310173582948,12.0577071676329,124.661625226807)) ;
#26152 = CARTESIAN_POINT('Ctrl Pts',(-19.4306181438283,12.0577254527075,124.661632111472)) ;
#26153 = CARTESIAN_POINT('Ctrl Pts',(-19.430410345223,12.0577349707246,124.661635643229)) ;
#26154 = CARTESIAN_POINT('Ctrl Pts',(-19.4299732384347,12.0577549926066,124.66164296328)) ;
#26155 = CARTESIAN_POINT('Ctrl Pts',(-19.4297439301276,12.0577654965416,124.661646740289)) ;
#26156 = CARTESIAN_POINT('Ctrl Pts',(-19.4293241206059,12.0577847274385,124.661653539537)) ;
#26157 = CARTESIAN_POINT('Ctrl Pts',(-19.4291336196373,12.0577934542766,124.661656581331)) ;
#26158 = CARTESIAN_POINT('Ctrl Pts',(-19.4284938709738,12.0578227619729,124.661666650114)) ;
#26159 = CARTESIAN_POINT('Ctrl Pts',(-19.4280446201722,12.0578433441248,124.66167347844)) ;
#26160 = CARTESIAN_POINT('Ctrl Pts',(-19.4228496320521,12.0580813658386,124.661749637377)) ;
#26161 = CARTESIAN_POINT('Ctrl Pts',(-19.4181035494019,12.0582989796514,124.661792180226)) ;
#26162 = CARTESIAN_POINT('Ctrl Pts',(-19.4085663181077,12.0587366393522,124.661823348918)) ;
#26163 = CARTESIAN_POINT('Ctrl Pts',(-19.4037752472262,12.0589566851438,124.661811461456)) ;
#26164 = CARTESIAN_POINT('Ctrl Pts',(-19.3928182714876,12.0594603775997,124.661721279295)) ;
#26165 = CARTESIAN_POINT('Ctrl Pts',(-19.386652646881,12.059744143375,124.661624903119)) ;
#26166 = CARTESIAN_POINT('Ctrl Pts',(-19.3702485254162,12.0605000334054,124.661247058863)) ;
#26167 = CARTESIAN_POINT('Ctrl Pts',(-19.3600123721226,12.0609726605192,124.660885368162)) ;
#26168 = CARTESIAN_POINT('Ctrl Pts',(-19.3194505221568,12.0628488770994,124.658952746186)) ;
#26169 = CARTESIAN_POINT('Ctrl Pts',(-19.2891818541446,12.0642565609159,124.656402808202)) ;
#26170 = CARTESIAN_POINT('Ctrl Pts',(-19.2499488244313,12.0660792864179,124.651653000755)) ;
#26171 = CARTESIAN_POINT('Ctrl Pts',(-19.2408739165736,12.0665008166201,124.650453053011)) ;
#26172 = CARTESIAN_POINT('Ctrl Pts',(-19.2271113608395,12.0671398600002,124.648479226377)) ;
#26173 = CARTESIAN_POINT('Ctrl Pts',(-19.2224136208351,12.0673579534745,124.647778127388)) ;
#26174 = CARTESIAN_POINT('Ctrl Pts',(-19.2141602182459,12.0677410520105,124.646498244024)) ;
#26175 = CARTESIAN_POINT('Ctrl Pts',(-19.2106028531344,12.067906152505,124.645930833164)) ;
#26176 = CARTESIAN_POINT('Ctrl Pts',(-19.2033761632301,12.0682415114393,124.644746097007)) ;
#26177 = CARTESIAN_POINT('Ctrl Pts',(-19.199707041974,12.0684117591614,124.644127749704)) ;
#26178 = CARTESIAN_POINT('Ctrl Pts',(-19.1958534322709,12.0685905524619,124.643460602479)) ;
#26179 = CARTESIAN_POINT('Ctrl Pts',(-19.1956661421711,12.0685992419969,124.643428134312)) ;
#26180 = CARTESIAN_POINT('Ctrl Pts',(-19.195275631099,12.0686173601248,124.643360344485)) ;
#26181 = CARTESIAN_POINT('Ctrl Pts',(-19.1950724114504,12.0686267886501,124.643325015241)) ;
#26182 = CARTESIAN_POINT('Ctrl Pts',(-19.194648853637,12.0686464398438,124.643251272729)) ;
#26183 = CARTESIAN_POINT('Ctrl Pts',(-19.1944285169969,12.0686566624344,124.643212850616)) ;
#26184 = CARTESIAN_POINT('Ctrl Pts',(-19.1941166032895,12.0686711337091,124.643158373109)) ;
#26185 = CARTESIAN_POINT('Ctrl Pts',(-19.1940250176593,12.0686753828279,124.643142366626)) ;
#26186 = CARTESIAN_POINT('Ctrl Pts',(-19.1938174574849,12.0686850125726,124.643106067329)) ;
#26187 = CARTESIAN_POINT('Ctrl Pts',(-19.1937014843561,12.0686903931282,124.643085768406)) ;
#26188 = CARTESIAN_POINT('Ctrl Pts',(-19.1888127984142,12.0689172024584,124.642229383663)) ;
#26189 = CARTESIAN_POINT('Ctrl Pts',(-19.1840449741949,12.0691383833535,124.641365568702)) ;
#26190 = CARTESIAN_POINT('Ctrl Pts',(-19.1717441788884,12.0697090229041,124.639063011384)) ;
#26191 = CARTESIAN_POINT('Ctrl Pts',(-19.1642191986178,12.0700581093992,124.637582625163)) ;
#26192 = CARTESIAN_POINT('Ctrl Pts',(-19.1410204071488,12.0711346979073,124.632796570008)) ;
#26193 = CARTESIAN_POINT('Ctrl Pts',(-19.125396130456,12.0718602549915,124.629258799168)) ;
#26194 = CARTESIAN_POINT('Ctrl Pts',(-19.0835714685436,12.0738088310328,124.618939578824)) ;
#26195 = CARTESIAN_POINT('Ctrl Pts',(-19.0575162399829,12.0750312482448,124.611606008327)) ;
#26196 = CARTESIAN_POINT('Ctrl Pts',(-19.0268513532554,12.0764976026809,124.601890140989)) ;
#26197 = CARTESIAN_POINT('Ctrl Pts',(-19.0219924989272,12.0767307445927,124.600317831159)) ;
#26198 = CARTESIAN_POINT('Ctrl Pts',(-19.0145022832069,12.0770914495912,124.597843211721)) ;
#26199 = CARTESIAN_POINT('Ctrl Pts',(-19.0118640612916,12.0772187483851,124.596961817217)) ;
#26200 = CARTESIAN_POINT('Ctrl Pts',(-19.0066141860477,12.0774725732244,124.595188403482)) ;
#26201 = CARTESIAN_POINT('Ctrl Pts',(-19.0040025015199,12.0775990967851,124.594296526557)) ;
#26202 = CARTESIAN_POINT('Ctrl Pts',(-18.9988368058538,12.0778498558955,124.592513343906)) ;
#26203 = CARTESIAN_POINT('Ctrl Pts',(-18.9962826919722,12.0779740863863,124.591622382254)) ;
#26204 = CARTESIAN_POINT('Ctrl Pts',(-18.9917075901926,12.0781970608444,124.590009754347)) ;
#26205 = CARTESIAN_POINT('Ctrl Pts',(-18.9896855291606,12.0782957651326,124.589291160662)) ;
#26206 = CARTESIAN_POINT('Ctrl Pts',(-18.983382918585,12.0786039071758,124.587033062199)) ;
#26207 = CARTESIAN_POINT('Ctrl Pts',(-18.9791089268567,12.0788135723052,124.585475399608)) ;
#26208 = CARTESIAN_POINT('Ctrl Pts',(-18.9670217508405,12.0794085061267,124.580995316588)) ;
#26209 = CARTESIAN_POINT('Ctrl Pts',(-18.9592292173005,12.0797944240482,124.578017978943)) ;
#26210 = CARTESIAN_POINT('Ctrl Pts',(-18.9292645887745,12.0812870577032,124.566224161847)) ;
#26211 = CARTESIAN_POINT('Ctrl Pts',(-18.9073169515415,12.0823991197782,124.556851570734)) ;
#26212 = CARTESIAN_POINT('Ctrl Pts',(-18.8845552145466,12.083564050551,124.54635105798)) ;
#26213 = CARTESIAN_POINT('Ctrl Pts',(-18.8834600262495,12.0836201305224,124.545843897419)) ;
#26214 = CARTESIAN_POINT('Ctrl Pts',(-18.8657605416334,12.0845269026316,124.537616455553)) ;
#26215 = CARTESIAN_POINT('Ctrl Pts',(-18.8493269893566,12.0853751245775,124.529533758679)) ;
#26216 = CARTESIAN_POINT('Ctrl Pts',(-18.8286249753884,12.0864499439215,124.518780456604)) ;
#26217 = CARTESIAN_POINT('Ctrl Pts',(-18.8241871357782,12.0866807379356,124.516441268088)) ;
#26218 = CARTESIAN_POINT('Ctrl Pts',(-18.8172357565421,12.0870428640428,124.512723547234)) ;
#26219 = CARTESIAN_POINT('Ctrl Pts',(-18.8147126834728,12.0871744294068,124.511362981065)) ;
#26220 = CARTESIAN_POINT('Ctrl Pts',(-18.8096721717043,12.0874375275458,124.508622464916)) ;
#26221 = CARTESIAN_POINT('Ctrl Pts',(-18.8071547625425,12.0875690591694,124.507242497448)) ;
#26222 = CARTESIAN_POINT('Ctrl Pts',(-18.801501631591,12.0878647324247,124.504118247187)) ;
#26223 = CARTESIAN_POINT('Ctrl Pts',(-18.798368619582,12.0880288083069,124.502369109239)) ;
#26224 = CARTESIAN_POINT('Ctrl Pts',(-18.7888867428192,12.0885260484879,124.49702176359)) ;
#26225 = CARTESIAN_POINT('Ctrl Pts',(-18.782561801549,12.0888586530077,124.493381418098)) ;
#26226 = CARTESIAN_POINT('Ctrl Pts',(-18.7674488831082,12.0896559170703,124.484506032573)) ;
#26227 = CARTESIAN_POINT('Ctrl Pts',(-18.7586925736956,12.0901199194689,124.479218100648)) ;
#26228 = CARTESIAN_POINT('Ctrl Pts',(-18.7341723556921,12.0914267461618,124.463996526492)) ;
#26229 = CARTESIAN_POINT('Ctrl Pts',(-18.7185642720902,12.0922673334528,124.453817080138)) ;
#26230 = CARTESIAN_POINT('Ctrl Pts',(-18.686447694152,12.0940265539756,124.431832167163)) ;
#26231 = CARTESIAN_POINT('Ctrl Pts',(-18.6699874579514,12.0949456966258,124.419965960952)) ;
#26232 = CARTESIAN_POINT('Ctrl Pts',(-18.6498073608539,12.0961005888327,124.404658016493)) ;
#26233 = CARTESIAN_POINT('Ctrl Pts',(-18.6458097753173,12.0963307583701,124.401587310526)) ;
#26234 = CARTESIAN_POINT('Ctrl Pts',(-18.6395464583661,12.0966936287847,124.396715683008)) ;
#26235 = CARTESIAN_POINT('Ctrl Pts',(-18.6372682144919,12.0968260930661,124.394930924558)) ;
#26236 = CARTESIAN_POINT('Ctrl Pts',(-18.6327133843536,12.0970918813463,124.391337110293)) ;
#26237 = CARTESIAN_POINT('Ctrl Pts',(-18.6304368717348,12.0972252056011,124.389527990721)) ;
#26238 = CARTESIAN_POINT('Ctrl Pts',(-18.6258596232342,12.097494251951,124.385864370794)) ;
#26239 = CARTESIAN_POINT('Ctrl Pts',(-18.6235591099065,12.0976299769295,124.384009622674)) ;
#26240 = CARTESIAN_POINT('Ctrl Pts',(-18.6205214380454,12.0978098601505,124.381542728985)) ;
#26241 = CARTESIAN_POINT('Ctrl Pts',(-18.6197783720828,12.0978539157672,124.380937865914)) ;
#26242 = CARTESIAN_POINT('Ctrl Pts',(-18.6171912011342,12.0980074916404,124.378826932835)) ;
#26243 = CARTESIAN_POINT('Ctrl Pts',(-18.6153507066691,12.0981170728674,124.377316450639)) ;
#26244 = CARTESIAN_POINT('Ctrl Pts',(-18.6089361744421,12.0985001331964,124.372021341065)) ;
#26245 = CARTESIAN_POINT('Ctrl Pts',(-18.6043848064618,12.0987739753247,124.368209405571)) ;
#26246 = CARTESIAN_POINT('Ctrl Pts',(-18.5901353086799,12.0996376696245,124.356101173324)) ;
#26247 = CARTESIAN_POINT('Ctrl Pts',(-18.5805370220431,12.1002288535301,124.347688728406)) ;
#26248 = CARTESIAN_POINT('Ctrl Pts',(-18.5500842274618,12.1021322209924,124.320162394536)) ;
#26249 = CARTESIAN_POINT('Ctrl Pts',(-18.5297487021016,12.1034434568904,124.30048673222)) ;
#26250 = CARTESIAN_POINT('Ctrl Pts',(-18.5049979413526,12.1050847841069,124.274856604347)) ;
#26251 = CARTESIAN_POINT('Ctrl Pts',(-18.4999444178514,12.1054225466107,124.269530417417)) ;
#26252 = CARTESIAN_POINT('Ctrl Pts',(-18.4913785673575,12.105999728123,124.260341598713)) ;
#26253 = CARTESIAN_POINT('Ctrl Pts',(-18.4878429846463,12.1062393536411,124.256500927122)) ;
#26254 = CARTESIAN_POINT('Ctrl Pts',(-18.4807312329972,12.1067242527057,124.248677708956)) ;
#26255 = CARTESIAN_POINT('Ctrl Pts',(-18.4771563770096,12.1069695105611,124.24469411402)) ;
#26256 = CARTESIAN_POINT('Ctrl Pts',(-18.4698242084639,12.1074757731801,124.236417271705)) ;
#26257 = CARTESIAN_POINT('Ctrl Pts',(-18.4660704798358,12.1077367446997,124.232121013496)) ;
#26258 = CARTESIAN_POINT('Ctrl Pts',(-18.4441523147958,12.1092714977858,124.206685639786)) ;
#26259 = CARTESIAN_POINT('Ctrl Pts',(-18.4266695721527,12.1105399709451,124.184969470474)) ;
#26260 = CARTESIAN_POINT('Ctrl Pts',(-18.3980911222504,12.1127080177427,124.146934089148)) ;
#26261 = CARTESIAN_POINT('Ctrl Pts',(-18.3866290928262,12.1136070143731,124.130903545692)) ;
#26262 = CARTESIAN_POINT('Ctrl Pts',(-18.3701432296329,12.1149475624964,124.106654934539)) ;
#26263 = CARTESIAN_POINT('Ctrl Pts',(-18.3648276190754,12.115387648517,124.098638906238)) ;
#26264 = CARTESIAN_POINT('Ctrl Pts',(-18.3547732830454,12.1162356186954,124.083090121085)) ;
#26265 = CARTESIAN_POINT('Ctrl Pts',(-18.3500214397369,12.1166434238422,124.075566527033)) ;
#26266 = CARTESIAN_POINT('Ctrl Pts',(-18.3453503415257,12.1170515107657,124.067992850388)) ;
#26267 = CARTESIAN_POINT('Ctrl Pts',(-20.8283303706881,10.,122.926041870813)) ;
#26268 = CARTESIAN_POINT('Ctrl Pts',(-20.5445170967909,9.82001091963712,123.023196933748)) ;
#26269 = CARTESIAN_POINT('Ctrl Pts',(-20.8845408159969,10.0066268508181,123.090165629856)) ;
#26270 = CARTESIAN_POINT('Ctrl Pts',(-20.5894888524673,9.82663777045524,123.154521539138)) ;
#26271 = CARTESIAN_POINT('Ctrl Pts',(-20.9394617690737,10.0198574772991,123.437507823531)) ;
#26272 = CARTESIAN_POINT('Ctrl Pts',(-20.633420846741,9.83986839693625,123.432353293108)) ;
#26273 = CARTESIAN_POINT('Ctrl Pts',(-20.8387858493119,10.0398330985578,123.958797508285)) ;
#26274 = CARTESIAN_POINT('Ctrl Pts',(-20.5528814274113,9.85984401819488,123.849407562291)) ;
#26275 = CARTESIAN_POINT('Ctrl Pts',(-20.5666727975867,10.0597504334597,124.412849839357)) ;
#26276 = CARTESIAN_POINT('Ctrl Pts',(-20.3351890331055,9.87976135309682,124.212644574099)) ;
#26277 = CARTESIAN_POINT('Ctrl Pts',(-20.157556275784,10.0796237101757,124.747029739186)) ;
#26278 = CARTESIAN_POINT('Ctrl Pts',(-20.007894029438,9.89963462981282,124.479989709356)) ;
#26279 = CARTESIAN_POINT('Ctrl Pts',(-19.6551315118144,10.0996482003397,124.922482691163)) ;
#26280 = CARTESIAN_POINT('Ctrl Pts',(-19.6059539581694,9.91965911997678,124.6203502007)) ;
#26281 = CARTESIAN_POINT('Ctrl Pts',(-19.1270395366036,10.1195160414904,124.915890798164)) ;
#26282 = CARTESIAN_POINT('Ctrl Pts',(-19.183479078867,9.9395269611275,124.615075206311)) ;
#26283 = CARTESIAN_POINT('Ctrl Pts',(-18.6307952228403,10.1394616923699,124.72957580943)) ;
#26284 = CARTESIAN_POINT('Ctrl Pts',(-18.7864838467008,9.95947261200706,124.466021078065)) ;
#26285 = CARTESIAN_POINT('Ctrl Pts',(-18.2288224078826,10.1593670929869,124.385607616877)) ;
#26286 = CARTESIAN_POINT('Ctrl Pts',(-18.4649063275282,9.97937801262402,124.19084435197)) ;
#26287 = CARTESIAN_POINT('Ctrl Pts',(-17.9678535157127,10.1792413208033,123.926349000794)) ;
#26288 = CARTESIAN_POINT('Ctrl Pts',(-18.2561329793354,9.99925224044038,123.823435269459)) ;
#26289 = CARTESIAN_POINT('Ctrl Pts',(-17.878734209588,10.1992271116809,123.402675114316)) ;
#26290 = CARTESIAN_POINT('Ctrl Pts',(-18.1848402358937,10.019238031318,123.404495614569)) ;
#26291 = CARTESIAN_POINT('Ctrl Pts',(-17.973517700436,10.2191213543406,122.882519965019)) ;
#26292 = CARTESIAN_POINT('Ctrl Pts',(-18.2606699231879,10.0391322739778,122.988371207676)) ;
#26293 = CARTESIAN_POINT('Ctrl Pts',(-18.2387528910803,10.2390000704127,122.425502981447)) ;
#26294 = CARTESIAN_POINT('Ctrl Pts',(-18.4728612986517,10.0590109900498,122.62275860733)) ;
#26295 = CARTESIAN_POINT('Ctrl Pts',(-18.647614090005,10.2590395202573,122.084258749108)) ;
#26296 = CARTESIAN_POINT('Ctrl Pts',(-18.7999520972875,10.0790504398944,122.349765888777)) ;
#26297 = CARTESIAN_POINT('Ctrl Pts',(-19.1441721121047,10.2789026817952,121.90452088182)) ;
#26298 = CARTESIAN_POINT('Ctrl Pts',(-19.1972003931787,10.0989136014323,122.205978444044)) ;
#26299 = CARTESIAN_POINT('Ctrl Pts',(-19.6750232066901,10.2988820498094,121.904721686728)) ;
#26300 = CARTESIAN_POINT('Ctrl Pts',(-19.6218814079036,10.1188929694465,122.206142590273)) ;
#26301 = CARTESIAN_POINT('Ctrl Pts',(-20.1701799765179,10.3186926303322,122.084083785786)) ;
#26302 = CARTESIAN_POINT('Ctrl Pts',(-20.0180064135448,10.1387035499693,122.349636107043)) ;
#26303 = CARTESIAN_POINT('Ctrl Pts',(-20.578226084171,10.3386735586178,122.423812224567)) ;
#26304 = CARTESIAN_POINT('Ctrl Pts',(-20.3444408940403,10.1586844782549,122.621421767106)) ;
#26305 = CARTESIAN_POINT('Ctrl Pts',(-20.8444469588477,10.3585662304872,122.880680954098)) ;
#26306 = CARTESIAN_POINT('Ctrl Pts',(-20.5574140513056,10.1785771501243,122.986919611144)) ;
#26307 = CARTESIAN_POINT('Ctrl Pts',(-20.9398341757817,10.3784925607743,123.40162915944)) ;
#26308 = CARTESIAN_POINT('Ctrl Pts',(-20.6337210673662,10.1985034804115,123.403677177554)) ;
#26309 = CARTESIAN_POINT('Ctrl Pts',(-20.8510572230715,10.3984631148666,123.924927290891)) ;
#26310 = CARTESIAN_POINT('Ctrl Pts',(-20.5626906127405,10.2184740345037,123.822322291595)) ;
#26311 = CARTESIAN_POINT('Ctrl Pts',(-20.6345446351863,10.4149949539542,124.307272603886)) ;
#26312 = CARTESIAN_POINT('Ctrl Pts',(-20.3894922234183,10.2350058735914,124.128174543065)) ;
#26313 = CARTESIAN_POINT('Ctrl Pts',(-20.3891097552813,10.4283346927818,124.557601822174)) ;
#26314 = CARTESIAN_POINT('Ctrl Pts',(-20.1931290434829,10.2483456124189,124.328455837242)) ;
#26315 = CARTESIAN_POINT('Ctrl Pts',(-20.1744300570267,10.4383669350004,124.710615084593)) ;
#26316 = CARTESIAN_POINT('Ctrl Pts',(-20.0213869924123,10.2583778546375,124.450860682641)) ;
#26317 = CARTESIAN_POINT('Ctrl Pts',(-19.9407404802418,10.4482246356439,124.822421617883)) ;
#26318 = CARTESIAN_POINT('Ctrl Pts',(-19.8344327400403,10.268235555281,124.540305070127)) ;
#26319 = CARTESIAN_POINT('Ctrl Pts',(-19.6879423525307,10.4582165002831,124.893352629427)) ;
#26320 = CARTESIAN_POINT('Ctrl Pts',(-19.6321963403517,10.2782274199202,124.597047919264)) ;
#26321 = CARTESIAN_POINT('Ctrl Pts',(-19.4284710425139,10.4681390500432,124.919080315321)) ;
#26322 = CARTESIAN_POINT('Ctrl Pts',(-19.4246096943487,10.2881499696804,124.61762631767)) ;
#26323 = CARTESIAN_POINT('Ctrl Pts',(-19.0804105140851,10.4814168235367,124.893583985624)) ;
#26324 = CARTESIAN_POINT('Ctrl Pts',(-19.14620736525,10.3014277431738,124.597234554234)) ;
#26325 = CARTESIAN_POINT('Ctrl Pts',(-18.7455859092888,10.4947641624773,124.776616835755)) ;
#26326 = CARTESIAN_POINT('Ctrl Pts',(-18.8783191462352,10.3147750821144,124.503658407746)) ;
#26327 = CARTESIAN_POINT('Ctrl Pts',(-18.4584522382473,10.5079713942705,124.581549246914)) ;
#26328 = CARTESIAN_POINT('Ctrl Pts',(-18.648603078249,10.3279823139076,124.347593121025)) ;
#26329 = CARTESIAN_POINT('Ctrl Pts',(-18.269958838059,10.5179585103602,124.398989341533)) ;
#26330 = CARTESIAN_POINT('Ctrl Pts',(-18.497812104421,10.3379694299973,124.201545371492)) ;
#26331 = CARTESIAN_POINT('Ctrl Pts',(-18.1163933969716,10.52790941594,124.187269395838)) ;
#26332 = CARTESIAN_POINT('Ctrl Pts',(-18.3749610183035,10.3479203355771,124.032167599002)) ;
#26333 = CARTESIAN_POINT('Ctrl Pts',(-18.0010345813923,10.5379645179474,123.949583784548)) ;
#26334 = CARTESIAN_POINT('Ctrl Pts',(-18.2826761214566,10.3579754375845,123.842018479487)) ;
#26335 = CARTESIAN_POINT('Ctrl Pts',(-17.9299233421522,10.5477861912685,123.701439503961)) ;
#26336 = CARTESIAN_POINT('Ctrl Pts',(-18.2257894437957,10.3677971109056,123.643501792389)) ;
#26337 = CARTESIAN_POINT('Ctrl Pts',(-17.9019040586336,10.5578446623434,123.43862866708)) ;
#26338 = CARTESIAN_POINT('Ctrl Pts',(-18.2033755364028,10.3778555819805,123.43325511011)) ;
#26339 = CARTESIAN_POINT('Ctrl Pts',(-17.9200547531203,10.5677692735199,123.178437417212)) ;
#26340 = CARTESIAN_POINT('Ctrl Pts',(-18.2179011304931,10.387780193157,123.22509433493)) ;
#26341 = CARTESIAN_POINT('Ctrl Pts',(-18.0035329037317,10.5810466124203,122.839624585047)) ;
#26342 = CARTESIAN_POINT('Ctrl Pts',(-18.2846726619434,10.4010575320574,122.954084471608)) ;
#26343 = CARTESIAN_POINT('Ctrl Pts',(-18.174078890485,10.5943454916579,122.53009645584)) ;
#26344 = CARTESIAN_POINT('Ctrl Pts',(-18.4211116702471,10.414356411295,122.706442742821)) ;
#26345 = CARTESIAN_POINT('Ctrl Pts',(-18.4148290889509,10.6075843638286,122.278909287836)) ;
#26346 = CARTESIAN_POINT('Ctrl Pts',(-18.61372828438,10.4275952834657,122.505480269817)) ;
#26347 = CARTESIAN_POINT('Ctrl Pts',(-18.6267237904145,10.6175909819652,122.123170592624)) ;
#26348 = CARTESIAN_POINT('Ctrl Pts',(-18.7832424340302,10.4376019016023,122.380894154854)) ;
#26349 = CARTESIAN_POINT('Ctrl Pts',(-18.8632279358434,10.6276219270267,122.006771081612)) ;
#26350 = CARTESIAN_POINT('Ctrl Pts',(-18.9724474943499,10.4476328466638,122.287775782223)) ;
#26351 = CARTESIAN_POINT('Ctrl Pts',(-19.1118308518252,10.6374781003785,121.93402103227)) ;
#26352 = CARTESIAN_POINT('Ctrl Pts',(-19.1713300681509,10.4574890200157,122.229578162461)) ;
#26353 = CARTESIAN_POINT('Ctrl Pts',(-19.3729271808616,10.6474773713414,121.904805274484)) ;
#26354 = CARTESIAN_POINT('Ctrl Pts',(-19.3802073636504,10.4674882909785,122.206207726809)) ;
#26355 = CARTESIAN_POINT('Ctrl Pts',(-19.63249343999,10.6573718230987,121.920897070182)) ;
#26356 = CARTESIAN_POINT('Ctrl Pts',(-19.5878600087485,10.4773827427359,122.219083373213)) ;
#26357 = CARTESIAN_POINT('Ctrl Pts',(-19.8895240952696,10.6674351389081,121.982913347126)) ;
#26358 = CARTESIAN_POINT('Ctrl Pts',(-19.7934840442871,10.4874460585452,122.268698557826)) ;
#26359 = CARTESIAN_POINT('Ctrl Pts',(-20.1266813029374,10.6772739956477,122.086019825898)) ;
#26360 = CARTESIAN_POINT('Ctrl Pts',(-19.9832086272329,10.4972849152848,122.351185625972)) ;
#26361 = CARTESIAN_POINT('Ctrl Pts',(-20.3474018172676,10.6873401174653,122.231740902041)) ;
#26362 = CARTESIAN_POINT('Ctrl Pts',(-20.1597838722231,10.5073510371024,122.46776433411)) ;
#26363 = CARTESIAN_POINT('Ctrl Pts',(-20.5359503275351,10.6972233451896,122.410409425907)) ;
#26364 = CARTESIAN_POINT('Ctrl Pts',(-20.3106209609387,10.5172342648267,122.6107005406)) ;
#26365 = CARTESIAN_POINT('Ctrl Pts',(-20.6926994160287,10.7072128064683,122.620953380555)) ;
#26366 = CARTESIAN_POINT('Ctrl Pts',(-20.4360184466383,10.5272237261055,122.779136903454)) ;
#26367 = CARTESIAN_POINT('Ctrl Pts',(-20.8101391925705,10.7171765168948,122.854988704109)) ;
#26368 = CARTESIAN_POINT('Ctrl Pts',(-20.5299682760089,10.5371874365319,122.966365995585)) ;
#26369 = CARTESIAN_POINT('Ctrl Pts',(-20.8856615342042,10.7271715196257,123.106575647569)) ;
#26370 = CARTESIAN_POINT('Ctrl Pts',(-20.5903840854433,10.5471824392628,123.167636082224)) ;
#26371 = CARTESIAN_POINT('Ctrl Pts',(-20.9160649147156,10.737207850636,123.368548316933)) ;
#26372 = CARTESIAN_POINT('Ctrl Pts',(-20.6147046374483,10.5572187702731,123.377214485628)) ;
#26373 = CARTESIAN_POINT('Ctrl Pts',(-20.901237668564,10.7470540799783,123.626888226543)) ;
#26374 = CARTESIAN_POINT('Ctrl Pts',(-20.6028407406531,10.5670649996154,123.583885836904)) ;
#26375 = CARTESIAN_POINT('Ctrl Pts',(-20.8414280631531,10.7570395782535,123.88234711985)) ;
#26376 = CARTESIAN_POINT('Ctrl Pts',(-20.5549910573095,10.5770504978907,123.788252351213)) ;
#26377 = CARTESIAN_POINT('Ctrl Pts',(-20.7388329136923,10.7669744812365,124.122475498249)) ;
#26378 = CARTESIAN_POINT('Ctrl Pts',(-20.4729131488679,10.5869854008736,123.98035400456)) ;
#26379 = CARTESIAN_POINT('Ctrl Pts',(-20.5941893977946,10.7770319843317,124.343638489499)) ;
#26380 = CARTESIAN_POINT('Ctrl Pts',(-20.3571965368945,10.5970429039689,124.157283333151)) ;
#26381 = CARTESIAN_POINT('Ctrl Pts',(-20.4178270374552,10.7868536407023,124.532127444505)) ;
#26382 = CARTESIAN_POINT('Ctrl Pts',(-20.216105589301,10.6068645603394,124.308072644051)) ;
#26383 = CARTESIAN_POINT('Ctrl Pts',(-20.2068264505713,10.7969097033674,124.691194003415)) ;
#26384 = CARTESIAN_POINT('Ctrl Pts',(-20.0473038554878,10.6169206230045,124.435324362058)) ;
#26385 = CARTESIAN_POINT('Ctrl Pts',(-19.9738709151238,10.8068503680706,124.809425923824)) ;
#26386 = CARTESIAN_POINT('Ctrl Pts',(-19.8609387422743,10.6268612877077,124.529907956941)) ;
#26387 = CARTESIAN_POINT('Ctrl Pts',(-19.7250819168071,10.8167547720191,124.885913848072)) ;
#26388 = CARTESIAN_POINT('Ctrl Pts',(-19.6619073830525,10.6367656916563,124.591096321636)) ;
#26389 = CARTESIAN_POINT('Ctrl Pts',(-19.4630900672441,10.8268012570127,124.918337587752)) ;
#26390 = CARTESIAN_POINT('Ctrl Pts',(-19.4523135810077,10.6468121766498,124.617033381453)) ;
#26391 = CARTESIAN_POINT('Ctrl Pts',(-19.2033217042056,10.8366974848244,124.905200421478)) ;
#26392 = CARTESIAN_POINT('Ctrl Pts',(-19.2444994521855,10.6567084044615,124.606521750019)) ;
#26393 = CARTESIAN_POINT('Ctrl Pts',(-18.9456501548748,10.8467570683879,124.846258925075)) ;
#26394 = CARTESIAN_POINT('Ctrl Pts',(-19.0383625055845,10.666767988025,124.559366649145)) ;
#26395 = CARTESIAN_POINT('Ctrl Pts',(-18.7071032762899,10.8566090780567,124.745604613553)) ;
#26396 = CARTESIAN_POINT('Ctrl Pts',(-18.8475263594419,10.6766199976938,124.478841692918)) ;
#26397 = CARTESIAN_POINT('Ctrl Pts',(-18.4867618466311,10.8665716094963,124.604236201826)) ;
#26398 = CARTESIAN_POINT('Ctrl Pts',(-18.6712543942556,10.6865825291334,124.36574560245)) ;
#26399 = CARTESIAN_POINT('Ctrl Pts',(-18.2932415519936,10.8766031577357,124.425213596724)) ;
#26400 = CARTESIAN_POINT('Ctrl Pts',(-18.5164393722649,10.6966140773728,124.222526126703)) ;
#26401 = CARTESIAN_POINT('Ctrl Pts',(-18.1357799386366,10.8864945689487,124.218398117847)) ;
#26402 = CARTESIAN_POINT('Ctrl Pts',(-18.3904718496513,10.7065054885858,124.057073085295)) ;
#26403 = CARTESIAN_POINT('Ctrl Pts',(-18.0146891209222,10.8965108226567,123.984678099418)) ;
#26404 = CARTESIAN_POINT('Ctrl Pts',(-18.2936007418435,10.7165217422938,123.870096295635)) ;
#26405 = CARTESIAN_POINT('Ctrl Pts',(-17.9364599064937,10.9065409255014,123.732978598351)) ;
#26406 = CARTESIAN_POINT('Ctrl Pts',(-18.2310191023128,10.7265518451385,123.66873611636)) ;
#26407 = CARTESIAN_POINT('Ctrl Pts',(-17.9032046926023,10.9163973744551,123.476088297528)) ;
#26408 = CARTESIAN_POINT('Ctrl Pts',(-18.2044167490604,10.7364082940922,123.463224374815)) ;
#26409 = CARTESIAN_POINT('Ctrl Pts',(-17.9148974747618,10.9263963852274,123.213627004979)) ;
#26410 = CARTESIAN_POINT('Ctrl Pts',(-18.2137726540653,10.7464073048645,123.253255524932)) ;
#26411 = CARTESIAN_POINT('Ctrl Pts',(-17.9711291549323,10.9362916021454,122.959700121601)) ;
#26412 = CARTESIAN_POINT('Ctrl Pts',(-18.2587594621295,10.7563025217825,123.050114944414)) ;
#26413 = CARTESIAN_POINT('Ctrl Pts',(-18.0722565351528,10.9463521175027,122.715462501341)) ;
#26414 = CARTESIAN_POINT('Ctrl Pts',(-18.3396629540108,10.7663630371399,122.854725296797)) ;
#26415 = CARTESIAN_POINT('Ctrl Pts',(-18.2111793287984,10.9562014108898,122.497051143162)) ;
#26416 = CARTESIAN_POINT('Ctrl Pts',(-18.4508020993981,10.7762123305269,122.679997778405)) ;
#26417 = CARTESIAN_POINT('Ctrl Pts',(-18.388559678523,10.9662285865698,122.302199917963)) ;
#26418 = CARTESIAN_POINT('Ctrl Pts',(-18.5927074978848,10.7862395062069,122.524117774987)) ;
#26419 = CARTESIAN_POINT('Ctrl Pts',(-18.5975457775489,10.976257162197,122.141622604304)) ;
#26420 = CARTESIAN_POINT('Ctrl Pts',(-18.7598974069773,10.7962680818341,122.395657172665)) ;
#26421 = CARTESIAN_POINT('Ctrl Pts',(-18.8267122580128,10.9861022557429,122.021573575598)) ;
#26422 = CARTESIAN_POINT('Ctrl Pts',(-18.9432305035226,10.80611317538,122.299619713947)) ;
#26423 = CARTESIAN_POINT('Ctrl Pts',(-19.0767061726053,10.9960934971746,121.941311591283)) ;
#26424 = CARTESIAN_POINT('Ctrl Pts',(-19.1432259108285,10.8161044168118,122.235411491827)) ;
#26425 = CARTESIAN_POINT('Ctrl Pts',(-19.3380760888337,11.0061292783179,121.906059986019)) ;
#26426 = CARTESIAN_POINT('Ctrl Pts',(-19.3523221423469,10.826140197955,122.20721167611)) ;
#26427 = CARTESIAN_POINT('Ctrl Pts',(-19.5967752495355,11.0159814840476,121.916185579079)) ;
#26428 = CARTESIAN_POINT('Ctrl Pts',(-19.5592805072898,10.8359924036847,122.215313538143)) ;
#26429 = CARTESIAN_POINT('Ctrl Pts',(-19.8527735772293,11.0259435781646,121.970943280899)) ;
#26430 = CARTESIAN_POINT('Ctrl Pts',(-19.7640785909624,10.8459544978017,122.259120868789)) ;
#26431 = CARTESIAN_POINT('Ctrl Pts',(-20.0967309229679,11.0359661389917,122.070215768955)) ;
#26432 = CARTESIAN_POINT('Ctrl Pts',(-19.9592439949302,10.8559770586288,122.338540107306)) ;
#26433 = CARTESIAN_POINT('Ctrl Pts',(-20.3177943873502,11.0458939106433,122.208809071659)) ;
#26434 = CARTESIAN_POINT('Ctrl Pts',(-20.1360936655196,10.8659048302804,122.449415566975)) ;
#26435 = CARTESIAN_POINT('Ctrl Pts',(-20.513619210783,11.0559362947681,122.385690857822)) ;
#26436 = CARTESIAN_POINT('Ctrl Pts',(-20.2927527608326,10.8759472144052,122.590922041084)) ;
#26437 = CARTESIAN_POINT('Ctrl Pts',(-20.6733901753496,11.0658255188387,122.590674219405)) ;
#26438 = CARTESIAN_POINT('Ctrl Pts',(-20.4205680784334,10.8858364384758,122.754908921902)) ;
#26439 = CARTESIAN_POINT('Ctrl Pts',(-20.7967974985103,11.075814767006,122.822355021181)) ;
#26440 = CARTESIAN_POINT('Ctrl Pts',(-20.5192928376293,10.8958256866432,122.940253955908)) ;
#26441 = CARTESIAN_POINT('Ctrl Pts',(-20.8776639039544,11.085773344048,123.07124139589)) ;
#26442 = CARTESIAN_POINT('Ctrl Pts',(-20.5839847120867,10.9057842636851,123.139363096927)) ;
#26443 = CARTESIAN_POINT('Ctrl Pts',(-20.9145104547189,11.0956729131393,123.328785419539)) ;
#26444 = CARTESIAN_POINT('Ctrl Pts',(-20.6134608083522,10.9156838327764,123.34539776855)) ;
#26445 = CARTESIAN_POINT('Ctrl Pts',(-20.9058609614056,11.1057208252233,123.592665004876)) ;
#26446 = CARTESIAN_POINT('Ctrl Pts',(-20.6065401309608,10.9257317448604,123.556501576119)) ;
#26447 = CARTESIAN_POINT('Ctrl Pts',(-20.8525354819136,11.1156161795305,123.847220118537)) ;
#26448 = CARTESIAN_POINT('Ctrl Pts',(-20.5638788889721,10.9356270991676,123.760144740549)) ;
#26449 = CARTESIAN_POINT('Ctrl Pts',(-20.7542573598821,11.1256778300217,124.092654877015)) ;
#26450 = CARTESIAN_POINT('Ctrl Pts',(-20.485255344439,10.9456887496588,123.95649240933)) ;
#26451 = CARTESIAN_POINT('Ctrl Pts',(-20.6178768119318,11.1355224454842,124.31250491989)) ;
#26452 = CARTESIAN_POINT('Ctrl Pts',(-20.3761506014328,10.9555333651213,124.132371010177)) ;
#26453 = CARTESIAN_POINT('Ctrl Pts',(-20.4440816600714,11.1454825243856,124.508211665868)) ;
#26454 = CARTESIAN_POINT('Ctrl Pts',(-20.2371141294296,10.9654934440227,124.288935606726)) ;
#26455 = CARTESIAN_POINT('Ctrl Pts',(-20.2370227832588,11.1555207187439,124.671637321506)) ;
#26456 = CARTESIAN_POINT('Ctrl Pts',(-20.0714663599296,10.9755316383811,124.419675493237)) ;
#26457 = CARTESIAN_POINT('Ctrl Pts',(-20.0087297938616,11.1653944341435,124.795026404838)) ;
#26458 = CARTESIAN_POINT('Ctrl Pts',(-19.8888323768802,10.9854053537807,124.518385630322)) ;
#26459 = CARTESIAN_POINT('Ctrl Pts',(-19.7576006730884,11.1754661436778,124.87849507525)) ;
#26460 = CARTESIAN_POINT('Ctrl Pts',(-19.6879285180809,10.9954770633149,124.585159904661)) ;
#26461 = CARTESIAN_POINT('Ctrl Pts',(-19.5019775459593,11.1852985841303,124.916330182897)) ;
#26462 = CARTESIAN_POINT('Ctrl Pts',(-19.4834310649531,11.0053095037674,124.61542705853)) ;
#26463 = CARTESIAN_POINT('Ctrl Pts',(-19.2384391664689,11.1953304050557,124.909797495667)) ;
#26464 = CARTESIAN_POINT('Ctrl Pts',(-19.2726002800821,11.0153413246928,124.610200312681)) ;
#26465 = CARTESIAN_POINT('Ctrl Pts',(-18.9804733109709,11.2053507749413,124.856926970494)) ;
#26466 = CARTESIAN_POINT('Ctrl Pts',(-19.0662277209886,11.0253616945784,124.567903126728)) ;
#26467 = CARTESIAN_POINT('Ctrl Pts',(-18.7390964607104,11.215217546075,124.762178595596)) ;
#26468 = CARTESIAN_POINT('Ctrl Pts',(-18.8731273657641,11.0352284657122,124.492104212861)) ;
#26469 = CARTESIAN_POINT('Ctrl Pts',(-18.5133063352698,11.2252883172644,124.624178813688)) ;
#26470 = CARTESIAN_POINT('Ctrl Pts',(-18.6924953042277,11.0452992369015,124.381703691916)) ;
#26471 = CARTESIAN_POINT('Ctrl Pts',(-18.3193404016488,11.235131477786,124.453023478491)) ;
#26472 = CARTESIAN_POINT('Ctrl Pts',(-18.5373238034759,11.0551423974231,124.24477971788)) ;
#26473 = CARTESIAN_POINT('Ctrl Pts',(-18.1551353492722,11.2451117109724,124.248529269541)) ;
#26474 = CARTESIAN_POINT('Ctrl Pts',(-18.4059602224555,11.0651226306096,124.081184300254)) ;
#26475 = CARTESIAN_POINT('Ctrl Pts',(-18.028891195577,11.2551302310076,124.017503067163)) ;
#26476 = CARTESIAN_POINT('Ctrl Pts',(-18.3049653496854,11.0751411506447,123.896363082341)) ;
#26477 = CARTESIAN_POINT('Ctrl Pts',(-17.94527872475,11.2650135393913,123.771572840937)) ;
#26478 = CARTESIAN_POINT('Ctrl Pts',(-18.2380760136292,11.0850244590284,123.699619611155)) ;
#26479 = CARTESIAN_POINT('Ctrl Pts',(-17.9050223248742,11.2750818235621,123.510113552435)) ;
#26480 = CARTESIAN_POINT('Ctrl Pts',(-18.2058712472604,11.0950927431992,123.490451793453)) ;
#26481 = CARTESIAN_POINT('Ctrl Pts',(-17.9103370638304,11.2849119502298,123.251798025967)) ;
#26482 = CARTESIAN_POINT('Ctrl Pts',(-18.2101233434264,11.1049228698669,123.283800611474)) ;
#26483 = CARTESIAN_POINT('Ctrl Pts',(-17.9612752714376,11.2949785224363,122.992253063296)) ;
#26484 = CARTESIAN_POINT('Ctrl Pts',(-18.2508742115829,11.1149894420734,123.07616437634)) ;
#26485 = CARTESIAN_POINT('Ctrl Pts',(-18.0550114914209,11.304868678677,122.749806436418)) ;
#26486 = CARTESIAN_POINT('Ctrl Pts',(-18.3258631525923,11.1248795983141,122.882207960884)) ;
#26487 = CARTESIAN_POINT('Ctrl Pts',(-18.1902998279982,11.3148612062534,122.524765958901)) ;
#26488 = CARTESIAN_POINT('Ctrl Pts',(-18.4340938564837,11.1348721258905,122.702175798357)) ;
#26489 = CARTESIAN_POINT('Ctrl Pts',(-18.362252777776,11.3248226961277,122.327384835979)) ;
#26490 = CARTESIAN_POINT('Ctrl Pts',(-18.57165612635,11.1448336157648,122.544271311536)) ;
#26491 = CARTESIAN_POINT('Ctrl Pts',(-18.5644303505552,11.3347319180149,122.163249256382)) ;
#26492 = CARTESIAN_POINT('Ctrl Pts',(-18.7333976447445,11.154742837652,122.412963346025)) ;
#26493 = CARTESIAN_POINT('Ctrl Pts',(-18.7952595963488,11.3447804978252,122.035028175252)) ;
#26494 = CARTESIAN_POINT('Ctrl Pts',(-18.9180612583401,11.1647914174624,122.310386442191)) ;
#26495 = CARTESIAN_POINT('Ctrl Pts',(-19.0407305551564,11.3546634722953,121.950157334317)) ;
#26496 = CARTESIAN_POINT('Ctrl Pts',(-19.1144372025468,11.1746743919324,122.242490108327)) ;
#26497 = CARTESIAN_POINT('Ctrl Pts',(-19.3000011957523,11.364658383438,121.908176471057)) ;
#26498 = CARTESIAN_POINT('Ctrl Pts',(-19.3218535588989,11.1846693030751,122.208905345717)) ;
#26499 = CARTESIAN_POINT('Ctrl Pts',(-19.5633130308643,11.3746787700116,121.912223489131)) ;
#26500 = CARTESIAN_POINT('Ctrl Pts',(-19.532503054688,11.1946896896487,122.212142961274)) ;
#26501 = CARTESIAN_POINT('Ctrl Pts',(-19.8190707586081,11.3845888738687,121.961229817149)) ;
#26502 = CARTESIAN_POINT('Ctrl Pts',(-19.7371085224044,11.2045997935058,122.251347849191)) ;
#26503 = CARTESIAN_POINT('Ctrl Pts',(-20.0631345837218,11.3945165860786,122.053434027889)) ;
#26504 = CARTESIAN_POINT('Ctrl Pts',(-19.9323591038037,11.2145275057157,122.325110807346)) ;
#26505 = CARTESIAN_POINT('Ctrl Pts',(-20.2899581915959,11.4045596958458,122.18834359306)) ;
#26506 = CARTESIAN_POINT('Ctrl Pts',(-20.1138182163407,11.2245706154829,122.433038412383)) ;
#26507 = CARTESIAN_POINT('Ctrl Pts',(-20.4869200798739,11.4144461163014,122.357790944953)) ;
#26508 = CARTESIAN_POINT('Ctrl Pts',(-20.2713871970456,11.2344570359385,122.568595575828)) ;
#26509 = CARTESIAN_POINT('Ctrl Pts',(-20.653571934063,11.424439293907,122.560728657171)) ;
#26510 = CARTESIAN_POINT('Ctrl Pts',(-20.4047088177741,11.2444502135441,122.730945421941)) ;
#26511 = CARTESIAN_POINT('Ctrl Pts',(-20.7817631202176,11.4343849568109,122.788494689918)) ;
#26512 = CARTESIAN_POINT('Ctrl Pts',(-20.5072617816881,11.254395876448,122.913157693448)) ;
#26513 = CARTESIAN_POINT('Ctrl Pts',(-20.8689810112581,11.4443322530161,123.034933251578)) ;
#26514 = CARTESIAN_POINT('Ctrl Pts',(-20.5770363372179,11.2643431726532,123.11030796952)) ;
#26515 = CARTESIAN_POINT('Ctrl Pts',(-20.9122274632139,11.454380018594,123.295405142899)) ;
#26516 = CARTESIAN_POINT('Ctrl Pts',(-20.611633872492,11.2743909382311,123.318685623006)) ;
#26517 = CARTESIAN_POINT('Ctrl Pts',(-20.909847955661,11.4642282318116,123.554192250672)) ;
#26518 = CARTESIAN_POINT('Ctrl Pts',(-20.6097306740805,11.2842391514487,123.525714196094)) ;
#26519 = CARTESIAN_POINT('Ctrl Pts',(-20.8628861917845,11.4741878046057,123.811671085768)) ;
#26520 = CARTESIAN_POINT('Ctrl Pts',(-20.5721619350103,11.2941987242428,123.731697005072)) ;
#26521 = CARTESIAN_POINT('Ctrl Pts',(-20.7707963194684,11.4842244256382,124.058815012756)) ;
#26522 = CARTESIAN_POINT('Ctrl Pts',(-20.4984904591295,11.3042353452753,123.929412437981)) ;
#26523 = CARTESIAN_POINT('Ctrl Pts',(-20.6396015638057,11.4941049404486,124.282914554949)) ;
#26524 = CARTESIAN_POINT('Ctrl Pts',(-20.3935356247347,11.3141158600857,124.108691603462)) ;
#26525 = CARTESIAN_POINT('Ctrl Pts',(-20.4686789714687,11.5041575917556,124.484292270277)) ;
#26526 = CARTESIAN_POINT('Ctrl Pts',(-20.2567978844015,11.3241685113927,124.26979434849)) ;
#26527 = CARTESIAN_POINT('Ctrl Pts',(-20.2685707709031,11.5140529900356,124.650429772369)) ;
#26528 = CARTESIAN_POINT('Ctrl Pts',(-20.0967123281824,11.3340639096727,124.402704356806)) ;
#26529 = CARTESIAN_POINT('Ctrl Pts',(-20.0392516106828,11.5241031117417,124.781376915193)) ;
#26530 = CARTESIAN_POINT('Ctrl Pts',(-19.9132571537407,11.3441140313788,124.50746276443)) ;
#26531 = CARTESIAN_POINT('Ctrl Pts',(-19.794737934636,11.5339873912836,124.869107009898)) ;
#26532 = CARTESIAN_POINT('Ctrl Pts',(-19.7176472402292,11.3539983109207,124.577647198776)) ;
#26533 = CARTESIAN_POINT('Ctrl Pts',(-19.5359779545354,11.5439821725755,124.914016452958)) ;
#26534 = CARTESIAN_POINT('Ctrl Pts',(-19.5106395508264,11.3639930922127,124.613575518455)) ;
#26535 = CARTESIAN_POINT('Ctrl Pts',(-19.2745423776044,11.5539300177623,124.913217278818)) ;
#26536 = CARTESIAN_POINT('Ctrl Pts',(-19.3014915210338,11.3739409373994,124.612936961295)) ;
#26537 = CARTESIAN_POINT('Ctrl Pts',(-19.0174715357979,11.5638669811497,124.867467500935)) ;
#26538 = CARTESIAN_POINT('Ctrl Pts',(-19.0958351968564,11.3838779007868,124.576338085747)) ;
#26539 = CARTESIAN_POINT('Ctrl Pts',(-18.7709478903475,11.5738499458869,124.77765044511)) ;
#26540 = CARTESIAN_POINT('Ctrl Pts',(-18.8986161489032,11.3938608655241,124.504485401762)) ;
#26541 = CARTESIAN_POINT('Ctrl Pts',(-18.5426769439724,11.5838937973026,124.645205762056)) ;
#26542 = CARTESIAN_POINT('Ctrl Pts',(-18.7159988423959,11.4039047169397,124.398530300539)) ;
#26543 = CARTESIAN_POINT('Ctrl Pts',(-18.3447570490132,11.5937219986373,124.479210868658)) ;
#26544 = CARTESIAN_POINT('Ctrl Pts',(-18.5576631821431,11.4137329182744,124.265735876442)) ;
#26545 = CARTESIAN_POINT('Ctrl Pts',(-18.1744334770806,11.6037985712354,124.27652667465)) ;
#26546 = CARTESIAN_POINT('Ctrl Pts',(-18.4214033306732,11.4238094908725,124.103588905207)) ;
#26547 = CARTESIAN_POINT('Ctrl Pts',(-18.0446742700679,11.6136506512429,124.052422800966)) ;
#26548 = CARTESIAN_POINT('Ctrl Pts',(-18.3175955633479,11.43366157088,123.924307178956)) ;
#26549 = CARTESIAN_POINT('Ctrl Pts',(-17.9536271837052,11.623723936247,123.80390465869)) ;
#26550 = CARTESIAN_POINT('Ctrl Pts',(-18.2447567627859,11.4437348558841,123.725492737883)) ;
#26551 = CARTESIAN_POINT('Ctrl Pts',(-17.9082400349615,11.6335652879575,123.549277141686)) ;
#26552 = CARTESIAN_POINT('Ctrl Pts',(-18.2084461725825,11.4535762075946,123.521791939049)) ;
#26553 = CARTESIAN_POINT('Ctrl Pts',(-17.9067818389188,11.643526787354,123.287519099378)) ;
#26554 = CARTESIAN_POINT('Ctrl Pts',(-18.2072783316507,11.4635377069911,123.312385832505)) ;
#26555 = CARTESIAN_POINT('Ctrl Pts',(-17.951583816689,11.653562563484,123.027613430416)) ;
#26556 = CARTESIAN_POINT('Ctrl Pts',(-18.2431187615393,11.4735734831211,123.104461008452)) ;
#26557 = CARTESIAN_POINT('Ctrl Pts',(-18.0392630064654,11.6634509901216,122.782997517006)) ;
#26558 = CARTESIAN_POINT('Ctrl Pts',(-18.3132606925425,11.4834619097587,122.908768552732)) ;
#26559 = CARTESIAN_POINT('Ctrl Pts',(-18.169309686562,11.6734663121965,122.55416670281)) ;
#26560 = CARTESIAN_POINT('Ctrl Pts',(-18.4172968626864,11.4934772318336,122.72570323888)) ;
#26561 = CARTESIAN_POINT('Ctrl Pts',(-18.337832034103,11.6834966610967,122.351486710983)) ;
#26562 = CARTESIAN_POINT('Ctrl Pts',(-18.5521138475697,11.5035075807338,122.563558413002)) ;
#26563 = CARTESIAN_POINT('Ctrl Pts',(-18.5348954406339,11.6933400367034,122.18392868398)) ;
#26564 = CARTESIAN_POINT('Ctrl Pts',(-18.7097629733351,11.5133509563405,122.429511607795)) ;
#26565 = CARTESIAN_POINT('Ctrl Pts',(-18.7619871989816,11.7033694736005,122.05014873987)) ;
#26566 = CARTESIAN_POINT('Ctrl Pts',(-18.8914356924309,11.5233803932376,122.322486374189)) ;
#26567 = CARTESIAN_POINT('Ctrl Pts',(-19.0091747229,11.7134013515334,121.958483598159)) ;
#26568 = CARTESIAN_POINT('Ctrl Pts',(-19.0891853235092,11.5334122711706,122.24915301597)) ;
#26569 = CARTESIAN_POINT('Ctrl Pts',(-19.2631763810942,11.7232309746389,121.91157223852)) ;
#26570 = CARTESIAN_POINT('Ctrl Pts',(-19.2923853954677,11.543241894276,122.211622724481)) ;
#26571 = CARTESIAN_POINT('Ctrl Pts',(-19.5256800788775,11.733220445792,121.908654949481)) ;
#26572 = CARTESIAN_POINT('Ctrl Pts',(-19.5023881948005,11.5532313654291,122.209287326421)) ;
#26573 = CARTESIAN_POINT('Ctrl Pts',(-19.7859934259949,11.7432642945544,121.95225353693)) ;
#26574 = CARTESIAN_POINT('Ctrl Pts',(-19.7106392257516,11.5632752141915,122.244164799925)) ;
#26575 = CARTESIAN_POINT('Ctrl Pts',(-20.0294606191008,11.7530860000861,122.037936667196)) ;
#26576 = CARTESIAN_POINT('Ctrl Pts',(-19.9054125518466,11.5730969197232,122.312709519324)) ;
#26577 = CARTESIAN_POINT('Ctrl Pts',(-20.2595522204667,11.7631210399139,122.166778899388)) ;
#26578 = CARTESIAN_POINT('Ctrl Pts',(-20.0894867189853,11.583131959551,122.415781895507)) ;
#26579 = CARTESIAN_POINT('Ctrl Pts',(-20.4631137171743,11.7731457468054,122.334014058184)) ;
#26580 = CARTESIAN_POINT('Ctrl Pts',(-20.2523368993887,11.5931566664425,122.549568855976)) ;
#26581 = CARTESIAN_POINT('Ctrl Pts',(-20.6320140503155,11.7829984511461,122.530257519376)) ;
#26582 = CARTESIAN_POINT('Ctrl Pts',(-20.3874578756258,11.6030093707832,122.706561953202)) ;
#26583 = CARTESIAN_POINT('Ctrl Pts',(-20.7664764699797,11.7929865733538,122.755655719711)) ;
#26584 = CARTESIAN_POINT('Ctrl Pts',(-20.4950292060904,11.6129974929909,122.886879510142)) ;
#26585 = CARTESIAN_POINT('Ctrl Pts',(-20.8592244692304,11.8029150434611,122.999531121806)) ;
#26586 = CARTESIAN_POINT('Ctrl Pts',(-20.5692290568483,11.6229259630982,123.081978836487)) ;
#26587 = CARTESIAN_POINT('Ctrl Pts',(-20.9089464870837,11.8129040206283,123.257291767332)) ;
#26588 = CARTESIAN_POINT('Ctrl Pts',(-20.609008398413,11.6329149402654,123.288186875209)) ;
#26589 = CARTESIAN_POINT('Ctrl Pts',(-20.912726728438,11.822941827908,123.521040547069)) ;
#26590 = CARTESIAN_POINT('Ctrl Pts',(-20.6120343028068,11.6429527475451,123.499185942152)) ;
#26591 = CARTESIAN_POINT('Ctrl Pts',(-20.8718727620384,11.8327881287713,123.776548267499)) ;
#26592 = CARTESIAN_POINT('Ctrl Pts',(-20.5793530040237,11.6527990484084,123.703591663681)) ;
#26593 = CARTESIAN_POINT('Ctrl Pts',(-20.7862889531826,11.8428138721506,124.025729898005)) ;
#26594 = CARTESIAN_POINT('Ctrl Pts',(-20.5108877193562,11.6628247917877,123.902937607542)) ;
#26595 = CARTESIAN_POINT('Ctrl Pts',(-20.6580711492051,11.8528447385896,124.256054351195)) ;
#26596 = CARTESIAN_POINT('Ctrl Pts',(-20.4083150016841,11.6728556582267,124.087198055119)) ;
#26597 = CARTESIAN_POINT('Ctrl Pts',(-20.4954300469777,11.8626820973884,124.456984258248)) ;
#26598 = CARTESIAN_POINT('Ctrl Pts',(-20.2782040287213,11.6826930170255,124.24794255801)) ;
#26599 = CARTESIAN_POINT('Ctrl Pts',(-20.2977609080492,11.8726740583222,124.62982526479)) ;
#26600 = CARTESIAN_POINT('Ctrl Pts',(-20.1200700801293,11.6926849779593,124.386216765177)) ;
#26601 = CARTESIAN_POINT('Ctrl Pts',(-20.0718918884167,11.8827064208787,124.765820716401)) ;
#26602 = CARTESIAN_POINT('Ctrl Pts',(-19.9393758049619,11.7027173405158,124.495014745963)) ;
#26603 = CARTESIAN_POINT('Ctrl Pts',(-19.830074922632,11.8925715814531,124.859237594725)) ;
#26604 = CARTESIAN_POINT('Ctrl Pts',(-19.7459234677896,11.7125825010902,124.569749829709)) ;
#26605 = CARTESIAN_POINT('Ctrl Pts',(-19.5733413955139,11.9025334860308,124.910472534242)) ;
#26606 = CARTESIAN_POINT('Ctrl Pts',(-19.5405372387899,11.7225444056679,124.610739722214)) ;
#26607 = CARTESIAN_POINT('Ctrl Pts',(-19.3097054567228,11.9125684161065,124.915962853087)) ;
#26608 = CARTESIAN_POINT('Ctrl Pts',(-19.3296285015763,11.7325793357437,124.615133939698)) ;
#26609 = CARTESIAN_POINT('Ctrl Pts',(-19.0528979312036,11.9224533629601,124.876622619197)) ;
#26610 = CARTESIAN_POINT('Ctrl Pts',(-19.1241826214947,11.7424642825973,124.583663814499)) ;
#26611 = CARTESIAN_POINT('Ctrl Pts',(-18.8024198540435,11.9325190392716,124.791735612442)) ;
#26612 = CARTESIAN_POINT('Ctrl Pts',(-18.9237994015907,11.7525299589087,124.515756076817)) ;
#26613 = CARTESIAN_POINT('Ctrl Pts',(-18.5755065294971,11.9423579589065,124.667701912514)) ;
#26614 = CARTESIAN_POINT('Ctrl Pts',(-18.7422682586687,11.7623688785436,124.416531178168)) ;
#26615 = CARTESIAN_POINT('Ctrl Pts',(-18.3688173844643,11.9524214686409,124.502784044984)) ;
#26616 = CARTESIAN_POINT('Ctrl Pts',(-18.576915561043,11.7724323882781,124.284598445225)) ;
#26617 = CARTESIAN_POINT('Ctrl Pts',(-18.1969723593472,11.9623150818027,124.307637940785)) ;
#26618 = CARTESIAN_POINT('Ctrl Pts',(-18.4394382482953,11.7823260014398,124.128483203739)) ;
#26619 = CARTESIAN_POINT('Ctrl Pts',(-18.0603757685369,11.9722590886161,124.08490476088)) ;
#26620 = CARTESIAN_POINT('Ctrl Pts',(-18.3301592733883,11.7922700082532,123.950297959954)) ;
#26621 = CARTESIAN_POINT('Ctrl Pts',(-17.9638367967476,11.9822600429704,123.840420099808)) ;
#26622 = CARTESIAN_POINT('Ctrl Pts',(-18.2529261323973,11.8022709626075,123.754711076634)) ;
#26623 = CARTESIAN_POINT('Ctrl Pts',(-17.9114896578375,11.9922988006627,123.58188181945)) ;
#26624 = CARTESIAN_POINT('Ctrl Pts',(-18.2110463657214,11.8123097202998,123.547880858099)) ;
#26625 = CARTESIAN_POINT('Ctrl Pts',(-17.9044041219212,12.0021229848327,123.323787975382)) ;
#26626 = CARTESIAN_POINT('Ctrl Pts',(-18.2053758050296,11.8221339044698,123.341406308645)) ;
#26627 = CARTESIAN_POINT('Ctrl Pts',(-17.9427499485555,12.0121810504321,123.062292370625)) ;
#26628 = CARTESIAN_POINT('Ctrl Pts',(-18.2360503193674,11.8321919700692,123.132209452442)) ;
#26629 = CARTESIAN_POINT('Ctrl Pts',(-18.0251977237691,12.0221110972068,122.814691316201)) ;
#26630 = CARTESIAN_POINT('Ctrl Pts',(-18.3020064298566,11.8421220168439,122.934128140568)) ;
#26631 = CARTESIAN_POINT('Ctrl Pts',(-18.1490393731302,12.0320625395439,122.584356522223)) ;
#26632 = CARTESIAN_POINT('Ctrl Pts',(-18.4010777391838,11.8520734591811,122.749859395245)) ;
#26633 = CARTESIAN_POINT('Ctrl Pts',(-18.3128249788135,12.0421093367232,122.377284739554)) ;
#26634 = CARTESIAN_POINT('Ctrl Pts',(-18.5321045207289,11.8621202563603,122.584200615192)) ;
#26635 = CARTESIAN_POINT('Ctrl Pts',(-18.5060148098008,12.0519572774033,122.205087588693)) ;
#26636 = CARTESIAN_POINT('Ctrl Pts',(-18.6866546893362,11.8719681970404,122.446441468451)) ;
#26637 = CARTESIAN_POINT('Ctrl Pts',(-18.7282729224672,12.0619189087459,122.066794754727)) ;
#26638 = CARTESIAN_POINT('Ctrl Pts',(-18.8644599124411,11.881929828383,122.335805352937)) ;
#26639 = CARTESIAN_POINT('Ctrl Pts',(-18.9729503385559,12.0719475681218,121.968835081685)) ;
#26640 = CARTESIAN_POINT('Ctrl Pts',(-19.0602009883113,11.8919584877589,122.257435568384)) ;
#26641 = CARTESIAN_POINT('Ctrl Pts',(-19.227831787757,12.08185787101,121.915407496624)) ;
#26642 = CARTESIAN_POINT('Ctrl Pts',(-19.2641055266912,11.9018687906471,122.214691356274)) ;
#26643 = CARTESIAN_POINT('Ctrl Pts',(-19.4887612039821,12.0917927655722,121.906342273827)) ;
#26644 = CARTESIAN_POINT('Ctrl Pts',(-19.472848876618,11.9118036852093,122.207436933983)) ;
#26645 = CARTESIAN_POINT('Ctrl Pts',(-19.7500144690061,12.1018338642391,121.943349818059)) ;
#26646 = CARTESIAN_POINT('Ctrl Pts',(-19.6818517658866,11.9218447838762,122.23704074526)) ;
#26647 = CARTESIAN_POINT('Ctrl Pts',(-19.9971083719985,12.1117211467435,122.023739879768)) ;
#26648 = CARTESIAN_POINT('Ctrl Pts',(-19.8795274617952,11.9317320663806,122.301350619632)) ;
#26649 = CARTESIAN_POINT('Ctrl Pts',(-20.2290950029525,12.121712887254,122.146694306298)) ;
#26650 = CARTESIAN_POINT('Ctrl Pts',(-20.0651177734983,11.9417238068911,122.399712142644)) ;
#26651 = CARTESIAN_POINT('Ctrl Pts',(-20.4353231818005,12.1316634364894,122.307485013012)) ;
#26652 = CARTESIAN_POINT('Ctrl Pts',(-20.230101643679,11.9516743561265,122.528342886444)) ;
#26653 = CARTESIAN_POINT('Ctrl Pts',(-20.6105080303125,12.1415991141242,122.501068844292)) ;
#26654 = CARTESIAN_POINT('Ctrl Pts',(-20.3702511605467,11.9616100337613,122.683208400421)) ;
#26655 = CARTESIAN_POINT('Ctrl Pts',(-20.750371753253,12.151584531917,122.723117938316)) ;
#26656 = CARTESIAN_POINT('Ctrl Pts',(-20.4821440178031,11.9715954515541,122.860846434547)) ;
#26657 = CARTESIAN_POINT('Ctrl Pts',(-20.8496752814087,12.1616133247875,122.967237619846)) ;
#26658 = CARTESIAN_POINT('Ctrl Pts',(-20.5615889029913,11.9816242444246,123.056141266303)) ;
#26659 = CARTESIAN_POINT('Ctrl Pts',(-20.9045281450594,12.1714928360155,123.220996340645)) ;
#26660 = CARTESIAN_POINT('Ctrl Pts',(-20.6054733938422,11.9915037556526,123.259147756982)) ;
#26661 = CARTESIAN_POINT('Ctrl Pts',(-20.9152054113298,12.1814863726884,123.483408955597)) ;
#26662 = CARTESIAN_POINT('Ctrl Pts',(-20.6140174445098,12.0014972923255,123.469077721808)) ;
#26663 = CARTESIAN_POINT('Ctrl Pts',(-20.8794802827671,12.1915186409522,123.744603500789)) ;
#26664 = CARTESIAN_POINT('Ctrl Pts',(-20.5854395864625,12.0115295605894,123.678033578765)) ;
#26665 = CARTESIAN_POINT('Ctrl Pts',(-20.8008139737887,12.2013826029581,123.991621606298)) ;
#26666 = CARTESIAN_POINT('Ctrl Pts',(-20.522508650298,12.0213935225952,123.875648805063)) ;
#26667 = CARTESIAN_POINT('Ctrl Pts',(-20.678002189668,12.211452664303,124.225997440401)) ;
#26668 = CARTESIAN_POINT('Ctrl Pts',(-20.4242612619508,12.0314635839401,124.063150402527)) ;
#26669 = CARTESIAN_POINT('Ctrl Pts',(-20.5199833626838,12.2212950286517,124.430776031763)) ;
#26670 = CARTESIAN_POINT('Ctrl Pts',(-20.2978478905724,12.0413059482889,124.22697474946)) ;
#26671 = CARTESIAN_POINT('Ctrl Pts',(-20.327174746647,12.2312557011542,124.607803018266)) ;
#26672 = CARTESIAN_POINT('Ctrl Pts',(-20.1436024451247,12.0512666207913,124.368597976752)) ;
#26673 = CARTESIAN_POINT('Ctrl Pts',(-20.1045650508631,12.241293772222,124.749310160051)) ;
#26674 = CARTESIAN_POINT('Ctrl Pts',(-19.9655159909283,12.0613046918591,124.48180549562)) ;
#26675 = CARTESIAN_POINT('Ctrl Pts',(-19.8649051459857,12.2511673871824,124.84884392232)) ;
#26676 = CARTESIAN_POINT('Ctrl Pts',(-19.7737886892284,12.0711783068196,124.561434593888)) ;
#26677 = CARTESIAN_POINT('Ctrl Pts',(-19.6065797304044,12.2612396217637,124.906300997495)) ;
#26678 = CARTESIAN_POINT('Ctrl Pts',(-19.5671291439869,12.0812505414008,124.607402358508)) ;
#26679 = CARTESIAN_POINT('Ctrl Pts',(-19.3486297183306,12.2710636402125,124.918040759663)) ;
#26680 = CARTESIAN_POINT('Ctrl Pts',(-19.3607684323741,12.0910745598496,124.616796316392)) ;
#26681 = CARTESIAN_POINT('Ctrl Pts',(-19.0863456687476,12.2811285611885,124.884353810211)) ;
#26682 = CARTESIAN_POINT('Ctrl Pts',(-19.1509427633031,12.1011394808256,124.589849001883)) ;
#26683 = CARTESIAN_POINT('Ctrl Pts',(-18.7548496615759,12.2943388594833,124.781008020348)) ;
#26684 = CARTESIAN_POINT('Ctrl Pts',(-18.8857366261165,12.1143497791204,124.507174493907)) ;
#26685 = CARTESIAN_POINT('Ctrl Pts',(-18.4555083325038,12.3076543062152,124.592460114452)) ;
#26686 = CARTESIAN_POINT('Ctrl Pts',(-18.646238230641,12.1276652258523,124.356312323164)) ;
#26687 = CARTESIAN_POINT('Ctrl Pts',(-18.2182158984291,12.3209445514825,124.336043204847)) ;
#26688 = CARTESIAN_POINT('Ctrl Pts',(-18.4564387255934,12.1409554711196,124.15121228678)) ;
#26689 = CARTESIAN_POINT('Ctrl Pts',(-18.0753697674858,12.3309953010896,124.113946532571)) ;
#26690 = CARTESIAN_POINT('Ctrl Pts',(-18.3421528585355,12.1510062207267,123.973529844557)) ;
#26691 = CARTESIAN_POINT('Ctrl Pts',(-17.9751686262583,12.3408079080718,123.876303265546)) ;
#26692 = CARTESIAN_POINT('Ctrl Pts',(-18.261991656828,12.160818827709,123.783417405138)) ;
#26693 = CARTESIAN_POINT('Ctrl Pts',(-17.9159132713503,12.3508790060661,123.61839959421)) ;
#26694 = CARTESIAN_POINT('Ctrl Pts',(-18.2145854546591,12.1708899257032,123.577093729689)) ;
#26695 = CARTESIAN_POINT('Ctrl Pts',(-17.9028470180164,12.360768578841,123.358821518713)) ;
#26696 = CARTESIAN_POINT('Ctrl Pts',(-18.2041287543014,12.1807794984781,123.369434895776)) ;
#26697 = CARTESIAN_POINT('Ctrl Pts',(-17.9449900324593,12.3740386856443,123.012644489447)) ;
#26698 = CARTESIAN_POINT('Ctrl Pts',(-18.2378495546872,12.1940496052814,123.092473752692)) ;
#26699 = CARTESIAN_POINT('Ctrl Pts',(-18.1100382420715,12.3906553725668,122.603018959482)) ;
#26700 = CARTESIAN_POINT('Ctrl Pts',(-18.3698647094851,12.2106662922039,122.764802568865)) ;
#26701 = CARTESIAN_POINT('Ctrl Pts',(-18.403953809166,12.407229415883,122.274921978595)) ;
#26702 = CARTESIAN_POINT('Ctrl Pts',(-18.6050396625321,12.2272403355201,122.502279805884)) ;
#26703 = CARTESIAN_POINT('Ctrl Pts',(-18.6963080999561,12.4205259833148,122.083501484983)) ;
#26704 = CARTESIAN_POINT('Ctrl Pts',(-18.838884457567,12.2405369029519,122.349174750329)) ;
#26705 = CARTESIAN_POINT('Ctrl Pts',(-18.9385791929077,12.4305560468922,121.979673523522)) ;
#26706 = CARTESIAN_POINT('Ctrl Pts',(-19.0327084258361,12.2505669665293,122.266104229579)) ;
#26707 = CARTESIAN_POINT('Ctrl Pts',(-19.1916818709481,12.4404499387414,121.920281628208)) ;
#26708 = CARTESIAN_POINT('Ctrl Pts',(-19.2351869221464,12.2604608583786,122.218590195066)) ;
#26709 = CARTESIAN_POINT('Ctrl Pts',(-19.5394009792638,12.453702694527,121.899549493621)) ;
#26710 = CARTESIAN_POINT('Ctrl Pts',(-19.5133723354866,12.2737136141641,122.202003998467)) ;
#26711 = CARTESIAN_POINT('Ctrl Pts',(-19.9747293753154,12.4704307995194,121.989564308867)) ;
#26712 = CARTESIAN_POINT('Ctrl Pts',(-19.8616245760486,12.2904417191566,122.274010791926)) ;
#26713 = CARTESIAN_POINT('Ctrl Pts',(-20.423556659189,12.4902616359979,122.266069036656)) ;
#26714 = CARTESIAN_POINT('Ctrl Pts',(-20.2206924545975,12.3102725556351,122.495213082915)) ;
#26715 = CARTESIAN_POINT('Ctrl Pts',(-20.7535327226879,12.5101870278881,122.680135635484)) ;
#26716 = CARTESIAN_POINT('Ctrl Pts',(-20.4846749563749,12.3301979475252,122.826464874533)) ;
#26717 = CARTESIAN_POINT('Ctrl Pts',(-20.9224041261077,12.5301122412401,123.18215712058)) ;
#26718 = CARTESIAN_POINT('Ctrl Pts',(-20.6197750512931,12.3501231608772,123.228081791924)) ;
#26719 = CARTESIAN_POINT('Ctrl Pts',(-20.9099617273115,12.5500372547252,123.711523704258)) ;
#26720 = CARTESIAN_POINT('Ctrl Pts',(-20.6098235773023,12.3700481743623,123.651575730201)) ;
#26721 = CARTESIAN_POINT('Ctrl Pts',(-20.7187360422604,12.5699137264252,124.204018044716)) ;
#26722 = CARTESIAN_POINT('Ctrl Pts',(-20.4568446351546,12.3899246460623,124.045573021246)) ;
#26723 = CARTESIAN_POINT('Ctrl Pts',(-20.3693300643289,12.5898930443341,124.603877601687)) ;
#26724 = CARTESIAN_POINT('Ctrl Pts',(-20.1773211406971,12.4099039639712,124.365462064758)) ;
#26725 = CARTESIAN_POINT('Ctrl Pts',(-19.9052905888142,12.6098260479101,124.859582769263)) ;
#26726 = CARTESIAN_POINT('Ctrl Pts',(-19.8060899284359,12.4298369675472,124.570028153243)) ;
#26727 = CARTESIAN_POINT('Ctrl Pts',(-19.3829989743676,12.6297213179378,124.941977004567)) ;
#26728 = CARTESIAN_POINT('Ctrl Pts',(-19.388255790433,12.4497322375749,124.635945220169)) ;
#26729 = CARTESIAN_POINT('Ctrl Pts',(-18.8631060156455,12.6496426558436,124.841587523865)) ;
#26730 = CARTESIAN_POINT('Ctrl Pts',(-18.9723403696999,12.4696535754807,124.555634564112)) ;
#26731 = CARTESIAN_POINT('Ctrl Pts',(-18.4079042835162,12.6696002791098,124.569214868981)) ;
#26732 = CARTESIAN_POINT('Ctrl Pts',(-18.6081780879779,12.4896111987469,124.337737060207)) ;
#26733 = CARTESIAN_POINT('Ctrl Pts',(-18.0742532724176,12.689480111067,124.15962015315)) ;
#26734 = CARTESIAN_POINT('Ctrl Pts',(-18.3412557256098,12.5094910307041,124.010060596195)) ;
#26735 = CARTESIAN_POINT('Ctrl Pts',(-17.8989480657597,12.7093619623639,123.661012507451)) ;
#26736 = CARTESIAN_POINT('Ctrl Pts',(-18.2010112129469,12.529372882001,123.611173006021)) ;
#26737 = CARTESIAN_POINT('Ctrl Pts',(-17.9053743363839,12.7294329794677,123.127663535506)) ;
#26738 = CARTESIAN_POINT('Ctrl Pts',(-18.206152086956,12.5494438991048,123.184494766924)) ;
#26739 = CARTESIAN_POINT('Ctrl Pts',(-18.0909224032866,12.7492402032208,122.634900991628)) ;
#26740 = CARTESIAN_POINT('Ctrl Pts',(-18.3545915317239,12.5692511228579,122.79028245245)) ;
#26741 = CARTESIAN_POINT('Ctrl Pts',(-18.4354537167374,12.7692213387896,122.230824135122)) ;
#26742 = CARTESIAN_POINT('Ctrl Pts',(-18.630217413786,12.5892322584267,122.467021418923)) ;
#26743 = CARTESIAN_POINT('Ctrl Pts',(-18.8964641846084,12.7891488321288,121.970176160961)) ;
#26744 = CARTESIAN_POINT('Ctrl Pts',(-18.9990268654917,12.6091597517659,122.258503153768)) ;
#26745 = CARTESIAN_POINT('Ctrl Pts',(-19.415834432645,12.8089694934866,121.881151656097)) ;
#26746 = CARTESIAN_POINT('Ctrl Pts',(-19.4145251819836,12.6289804131237,122.187284802725)) ;
#26747 = CARTESIAN_POINT('Ctrl Pts',(-19.9411566590933,12.8290666827084,121.976780870031)) ;
#26748 = CARTESIAN_POINT('Ctrl Pts',(-19.8347817388246,12.6490776023455,122.26378939332)) ;
#26749 = CARTESIAN_POINT('Ctrl Pts',(-20.3952240684518,12.8488303617167,122.241384544964)) ;
#26750 = CARTESIAN_POINT('Ctrl Pts',(-20.1980368260556,12.6688412813539,122.475474968688)) ;
#26751 = CARTESIAN_POINT('Ctrl Pts',(-20.7368987004041,12.8688876403898,122.650278783027)) ;
#26752 = CARTESIAN_POINT('Ctrl Pts',(-20.471374567732,12.6888985600269,122.802591330888)) ;
#26753 = CARTESIAN_POINT('Ctrl Pts',(-20.915999998585,12.8886830641372,123.145136393717)) ;
#26754 = CARTESIAN_POINT('Ctrl Pts',(-20.6146542216816,12.7086939837743,123.198479843696)) ;
#26755 = CARTESIAN_POINT('Ctrl Pts',(-20.9171224626081,12.9086467088648,123.675675466344)) ;
#26756 = CARTESIAN_POINT('Ctrl Pts',(-20.6155493596477,12.7286576285019,123.62291137376)) ;
#26757 = CARTESIAN_POINT('Ctrl Pts',(-20.7357148689362,12.9286302001389,124.174870580485)) ;
#26758 = CARTESIAN_POINT('Ctrl Pts',(-20.4704208498852,12.748641119776,124.022266714748)) ;
#26759 = CARTESIAN_POINT('Ctrl Pts',(-20.3986521463145,12.9484376952882,124.579332558867)) ;
#26760 = CARTESIAN_POINT('Ctrl Pts',(-20.2007674929157,12.7684486149253,124.345835452123)) ;
#26761 = CARTESIAN_POINT('Ctrl Pts',(-19.9402235763069,12.9684202860083,124.847283742868)) ;
#26762 = CARTESIAN_POINT('Ctrl Pts',(-19.8340229155712,12.7884312056454,124.560193612836)) ;
#26763 = CARTESIAN_POINT('Ctrl Pts',(-19.4202416053834,12.9883029399995,124.942191223807)) ;
#26764 = CARTESIAN_POINT('Ctrl Pts',(-19.4180360713643,12.8083138596367,124.636116448561)) ;
#26765 = CARTESIAN_POINT('Ctrl Pts',(-18.8972653738817,13.0082611848626,124.854056149815)) ;
#26766 = CARTESIAN_POINT('Ctrl Pts',(-18.9996554343786,12.8282721044997,124.565604873839)) ;
#26767 = CARTESIAN_POINT('Ctrl Pts',(-18.4373467193133,13.0281367719042,124.594021898923)) ;
#26768 = CARTESIAN_POINT('Ctrl Pts',(-18.6317218256589,12.8481476915413,124.357573939608)) ;
#26769 = CARTESIAN_POINT('Ctrl Pts',(-18.0917408140289,13.0481176600395,124.190855292359)) ;
#26770 = CARTESIAN_POINT('Ctrl Pts',(-18.355239878661,12.8681285796766,124.035038248343)) ;
#26771 = CARTESIAN_POINT('Ctrl Pts',(-17.9052414355018,13.0680528011505,123.694844185524)) ;
#26772 = CARTESIAN_POINT('Ctrl Pts',(-18.2060442903282,12.8880637207876,123.63822733448)) ;
#26773 = CARTESIAN_POINT('Ctrl Pts',(-17.8988271166947,13.0879648191615,123.165702838927)) ;
#26774 = CARTESIAN_POINT('Ctrl Pts',(-18.200915253109,12.9079757387987,123.21491552465)) ;
#26775 = CARTESIAN_POINT('Ctrl Pts',(-18.072637630343,13.1078530374051,122.666485551976)) ;
#26776 = CARTESIAN_POINT('Ctrl Pts',(-18.3399734826579,12.9278639570422,122.815536572551)) ;
#26777 = CARTESIAN_POINT('Ctrl Pts',(-18.3508356377982,13.124451341252,122.324166060085)) ;
#26778 = CARTESIAN_POINT('Ctrl Pts',(-18.562516670019,12.9444622608891,122.54170220006)) ;
#26779 = CARTESIAN_POINT('Ctrl Pts',(-18.6332461345771,13.1377239311548,122.119417599801)) ;
#26780 = CARTESIAN_POINT('Ctrl Pts',(-18.7884633789187,12.957734850792,122.37788874013)) ;
#26781 = CARTESIAN_POINT('Ctrl Pts',(-18.8696106143661,13.1477313461057,122.004127651261)) ;
#26782 = CARTESIAN_POINT('Ctrl Pts',(-18.9775498041114,12.9677422657428,122.285661949653)) ;
#26783 = CARTESIAN_POINT('Ctrl Pts',(-19.1224757065835,13.1577386928383,121.931849416177)) ;
#26784 = CARTESIAN_POINT('Ctrl Pts',(-19.1798541601348,12.9777496124754,122.22784121804)) ;
#26785 = CARTESIAN_POINT('Ctrl Pts',(-19.4692111889447,13.1710050526399,121.895476582139)) ;
#26786 = CARTESIAN_POINT('Ctrl Pts',(-19.4571883101494,12.991015972277,122.198742524881)) ;
#26787 = CARTESIAN_POINT('Ctrl Pts',(-19.9027886653172,13.1875197102629,121.963391453896)) ;
#26788 = CARTESIAN_POINT('Ctrl Pts',(-19.8041192330616,13.0075306299,122.253086454829)) ;
#26789 = CARTESIAN_POINT('Ctrl Pts',(-20.2896179416635,13.2041171435055,122.175375538865)) ;
#26790 = CARTESIAN_POINT('Ctrl Pts',(-20.1135332169725,13.0241280631426,122.422657930658)) ;
#26791 = CARTESIAN_POINT('Ctrl Pts',(-20.5428541366256,13.2174651406505,122.418153018463)) ;
#26792 = CARTESIAN_POINT('Ctrl Pts',(-20.3161488901095,13.0374760602876,122.61689817093)) ;
#26793 = CARTESIAN_POINT('Ctrl Pts',(-20.6967627804406,13.2273608950021,122.62776755716)) ;
#26794 = CARTESIAN_POINT('Ctrl Pts',(-20.4392682594011,13.0473718146392,122.784587934019)) ;
#26795 = CARTESIAN_POINT('Ctrl Pts',(-20.8132896637095,13.2373488489335,122.862934128972)) ;
#26796 = CARTESIAN_POINT('Ctrl Pts',(-20.5324892841562,13.0573597685706,122.972723020215)) ;
#26797 = CARTESIAN_POINT('Ctrl Pts',(-20.887111769064,13.2473060726382,123.114002366625)) ;
#26798 = CARTESIAN_POINT('Ctrl Pts',(-20.591544390908,13.0673169922753,123.17357799442)) ;
#26799 = CARTESIAN_POINT('Ctrl Pts',(-20.9163194697392,13.2573416191949,123.376085199788)) ;
#26800 = CARTESIAN_POINT('Ctrl Pts',(-20.6149084219131,13.077352538832,123.383244498507)) ;
#26801 = CARTESIAN_POINT('Ctrl Pts',(-20.9000197111728,13.267228730471,123.635413520908)) ;
#26802 = CARTESIAN_POINT('Ctrl Pts',(-20.6018663387177,13.0872396501081,123.590707013406)) ;
#26803 = CARTESIAN_POINT('Ctrl Pts',(-20.8387093067046,13.2772201355718,123.890705618829)) ;
#26804 = CARTESIAN_POINT('Ctrl Pts',(-20.5528158398965,13.0972310552089,123.794940111806)) ;
#26805 = CARTESIAN_POINT('Ctrl Pts',(-20.7344045824693,13.2871657567866,124.130350209159)) ;
#26806 = CARTESIAN_POINT('Ctrl Pts',(-20.4693700045889,13.1071766764237,123.986654845543)) ;
#26807 = CARTESIAN_POINT('Ctrl Pts',(-20.5904556480587,13.2971150050549,124.348628887742)) ;
#26808 = CARTESIAN_POINT('Ctrl Pts',(-20.3542090074305,13.117125924692,124.161276491165)) ;
#26809 = CARTESIAN_POINT('Ctrl Pts',(-20.4088310489179,13.3071615002235,124.540222615066)) ;
#26810 = CARTESIAN_POINT('Ctrl Pts',(-20.208907719291,13.1271724198607,124.314549885357)) ;
#26811 = CARTESIAN_POINT('Ctrl Pts',(-20.2009526790891,13.3170128430151,124.69453910851)) ;
#26812 = CARTESIAN_POINT('Ctrl Pts',(-20.0426037537448,13.1370237626522,124.438001210113)) ;
#26813 = CARTESIAN_POINT('Ctrl Pts',(-19.9669434550335,13.3269846231424,124.812406349802)) ;
#26814 = CARTESIAN_POINT('Ctrl Pts',(-19.85539544562,13.1469955427795,124.532292952135)) ;
#26815 = CARTESIAN_POINT('Ctrl Pts',(-19.7153564891379,13.3369798231201,124.888022808457)) ;
#26816 = CARTESIAN_POINT('Ctrl Pts',(-19.6541252878157,13.1569907427572,124.592783951486)) ;
#26817 = CARTESIAN_POINT('Ctrl Pts',(-19.4534753611638,13.3470138148161,124.918598821052)) ;
#26818 = CARTESIAN_POINT('Ctrl Pts',(-19.4446201537456,13.1670247344533,124.617242515926)) ;
#26819 = CARTESIAN_POINT('Ctrl Pts',(-19.1948766730221,13.3568692197886,124.903920505576)) ;
#26820 = CARTESIAN_POINT('Ctrl Pts',(-19.2377415186523,13.1768801394258,124.605497635822)) ;
#26821 = CARTESIAN_POINT('Ctrl Pts',(-18.9390603846793,13.3668685176344,124.844062381727)) ;
#26822 = CARTESIAN_POINT('Ctrl Pts',(-19.0330890674642,13.1868794372715,124.557608978315)) ;
#26823 = CARTESIAN_POINT('Ctrl Pts',(-18.6998481883594,13.3767636302396,124.741995186928)) ;
#26824 = CARTESIAN_POINT('Ctrl Pts',(-18.8417203716604,13.1967745498767,124.475953269536)) ;
#26825 = CARTESIAN_POINT('Ctrl Pts',(-18.4784292945889,13.3868242757746,124.597585675323)) ;
#26826 = CARTESIAN_POINT('Ctrl Pts',(-18.6645864484423,13.2068351954117,124.360423788125)) ;
#26827 = CARTESIAN_POINT('Ctrl Pts',(-18.2893688821215,13.3966731527638,124.420799145494)) ;
#26828 = CARTESIAN_POINT('Ctrl Pts',(-18.5133398551408,13.2166840724009,124.218993165454)) ;
#26829 = CARTESIAN_POINT('Ctrl Pts',(-18.1305208053495,13.4067018638574,124.210511784196)) ;
#26830 = CARTESIAN_POINT('Ctrl Pts',(-18.3862631410708,13.2267127834945,124.050761997541)) ;
#26831 = CARTESIAN_POINT('Ctrl Pts',(-18.0112247910287,13.4167312651135,123.975488167396)) ;
#26832 = CARTESIAN_POINT('Ctrl Pts',(-18.2908283055355,13.2367421847506,123.862742104803)) ;
#26833 = CARTESIAN_POINT('Ctrl Pts',(-17.9354445009214,13.4265714569095,123.72824647118)) ;
#26834 = CARTESIAN_POINT('Ctrl Pts',(-18.2302062650651,13.2465823765466,123.664948483144)) ;
#26835 = CARTESIAN_POINT('Ctrl Pts',(-17.9027395319079,13.4365748861025,123.467435684465)) ;
#26836 = CARTESIAN_POINT('Ctrl Pts',(-18.2040444166883,13.2565858057396,123.456299663574)) ;
#26837 = CARTESIAN_POINT('Ctrl Pts',(-17.9158814573718,13.4465603985687,123.205311390375)) ;
#26838 = CARTESIAN_POINT('Ctrl Pts',(-18.2145600879431,13.2665713182058,123.24660043712)) ;
#26839 = CARTESIAN_POINT('Ctrl Pts',(-17.9749065837832,13.4566014949527,122.948155155583)) ;
#26840 = CARTESIAN_POINT('Ctrl Pts',(-18.2617823053095,13.2766124145898,123.040875912254)) ;
#26841 = CARTESIAN_POINT('Ctrl Pts',(-18.0753470360815,13.4664446909037,122.709757985454)) ;
#26842 = CARTESIAN_POINT('Ctrl Pts',(-18.3421364530239,13.2864556105408,122.850159423479)) ;
#26843 = CARTESIAN_POINT('Ctrl Pts',(-18.217218281521,13.4764310019581,122.489035231126)) ;
#26844 = CARTESIAN_POINT('Ctrl Pts',(-18.455635132101,13.2964419215952,122.673582454515)) ;
#26845 = CARTESIAN_POINT('Ctrl Pts',(-18.3942732512551,13.4863656872158,122.297106419642)) ;
#26846 = CARTESIAN_POINT('Ctrl Pts',(-18.5972804423146,13.3063766068529,122.520040993049)) ;
#26847 = CARTESIAN_POINT('Ctrl Pts',(-18.6046031877743,13.4964232484328,122.137116873894)) ;
#26848 = CARTESIAN_POINT('Ctrl Pts',(-18.7655457306992,13.31643416807,122.392050961701)) ;
#26849 = CARTESIAN_POINT('Ctrl Pts',(-18.8338850495127,13.5062448900414,122.018535713195)) ;
#26850 = CARTESIAN_POINT('Ctrl Pts',(-18.9489715980104,13.3262558096786,122.297188133943)) ;
#26851 = CARTESIAN_POINT('Ctrl Pts',(-19.0859583258846,13.5163009536324,121.939273611562)) ;
#26852 = CARTESIAN_POINT('Ctrl Pts',(-19.1506308986353,13.3363118732695,122.233780316748)) ;
#26853 = CARTESIAN_POINT('Ctrl Pts',(-19.3450516698222,13.5262416293942,121.905839973782)) ;
#26854 = CARTESIAN_POINT('Ctrl Pts',(-19.3579055692691,13.3462525490313,122.207035465221)) ;
#26855 = CARTESIAN_POINT('Ctrl Pts',(-19.6050909750196,13.5361459881825,121.917041144644)) ;
#26856 = CARTESIAN_POINT('Ctrl Pts',(-19.565936503742,13.3561569078197,122.215998316432)) ;
#26857 = CARTESIAN_POINT('Ctrl Pts',(-19.862825851585,13.5461926427583,121.97418792217)) ;
#26858 = CARTESIAN_POINT('Ctrl Pts',(-19.7721240620941,13.3662035623955,122.261717666906)) ;
#26859 = CARTESIAN_POINT('Ctrl Pts',(-20.1031997643857,13.5560882374012,122.073508487898)) ;
#26860 = CARTESIAN_POINT('Ctrl Pts',(-19.9644220277355,13.3760991570383,122.341175720192)) ;
#26861 = CARTESIAN_POINT('Ctrl Pts',(-20.3263218440362,13.5661501840581,122.215343672236)) ;
#26862 = CARTESIAN_POINT('Ctrl Pts',(-20.1429187779707,13.3861611036952,122.454645564345)) ;
#26863 = CARTESIAN_POINT('Ctrl Pts',(-20.5173749645332,13.5759998079902,122.38999462014)) ;
#26864 = CARTESIAN_POINT('Ctrl Pts',(-20.295759491306,13.3960107276274,122.594367286313)) ;
#26865 = CARTESIAN_POINT('Ctrl Pts',(-20.6776884554839,13.5859630470201,122.596980439567)) ;
#26866 = CARTESIAN_POINT('Ctrl Pts',(-20.4240087199095,13.4059739666572,122.759956837706)) ;
#26867 = CARTESIAN_POINT('Ctrl Pts',(-20.8000704181908,13.5959876217959,122.830280403309)) ;
#26868 = CARTESIAN_POINT('Ctrl Pts',(-20.5219126738478,13.415998541433,122.946597684399)) ;
#26869 = CARTESIAN_POINT('Ctrl Pts',(-20.8793920083737,13.6059061844836,123.07855998187)) ;
#26870 = CARTESIAN_POINT('Ctrl Pts',(-20.5853680842003,13.4259171041207,123.145221485307)) ;
#26871 = CARTESIAN_POINT('Ctrl Pts',(-20.9151199375489,13.6158983712076,123.338717822216)) ;
#26872 = CARTESIAN_POINT('Ctrl Pts',(-20.6139486858676,13.4359092908447,123.353347860863)) ;
#26873 = CARTESIAN_POINT('Ctrl Pts',(-20.9046168525977,13.6259331697918,123.6022019633)) ;
#26874 = CARTESIAN_POINT('Ctrl Pts',(-20.605544399225,13.4459440894289,123.564135168279)) ;
#26875 = CARTESIAN_POINT('Ctrl Pts',(-20.8499556627768,13.6357883604655,123.855372966742)) ;
#26876 = CARTESIAN_POINT('Ctrl Pts',(-20.5618138995585,13.4557992801026,123.766670884377)) ;
#26877 = CARTESIAN_POINT('Ctrl Pts',(-20.7510855573927,13.6457877086185,124.098788324435)) ;
#26878 = CARTESIAN_POINT('Ctrl Pts',(-20.4827162949927,13.4657986282556,123.961402436991)) ;
#26879 = CARTESIAN_POINT('Ctrl Pts',(-20.6130996723433,13.6556828342936,124.319242233489)) ;
#26880 = CARTESIAN_POINT('Ctrl Pts',(-20.3723265173656,13.4756937539307,124.137764200893)) ;
#26881 = CARTESIAN_POINT('Ctrl Pts',(-20.4360519660016,13.6657433772417,124.515540628893)) ;
#26882 = CARTESIAN_POINT('Ctrl Pts',(-20.2306870063593,13.4857542968788,124.294801963191)) ;
#26883 = CARTESIAN_POINT('Ctrl Pts',(-20.2320341456861,13.6755926515086,124.674850714962)) ;
#26884 = CARTESIAN_POINT('Ctrl Pts',(-20.0674724171004,13.4956035711457,124.422248249584)) ;
#26885 = CARTESIAN_POINT('Ctrl Pts',(-19.9996623311131,13.6856198760785,124.799086161189)) ;
#26886 = CARTESIAN_POINT('Ctrl Pts',(-19.8815742380617,13.5056307957156,124.521635311594)) ;
#26887 = CARTESIAN_POINT('Ctrl Pts',(-19.7489854254844,13.6956482752663,124.880448501815)) ;
#26888 = CARTESIAN_POINT('Ctrl Pts',(-19.6810321616281,13.5156591949034,124.586723663228)) ;
#26889 = CARTESIAN_POINT('Ctrl Pts',(-19.4928401900497,13.7054940256798,124.916853671087)) ;
#26890 = CARTESIAN_POINT('Ctrl Pts',(-19.4761166444092,13.5255049453169,124.615846163914)) ;
#26891 = CARTESIAN_POINT('Ctrl Pts',(-19.230454887784,13.7154828160805,124.908839488335)) ;
#26892 = CARTESIAN_POINT('Ctrl Pts',(-19.2662086080236,13.5354937357177,124.609433445062)) ;
#26893 = CARTESIAN_POINT('Ctrl Pts',(-18.9721627761797,13.7255277444802,124.854438840815)) ;
#26894 = CARTESIAN_POINT('Ctrl Pts',(-19.0595750986044,13.5455386641174,124.565911420256)) ;
#26895 = CARTESIAN_POINT('Ctrl Pts',(-18.7323658376547,13.7353522292692,124.758724681303)) ;
#26896 = CARTESIAN_POINT('Ctrl Pts',(-18.8677390346098,13.5553631489063,124.489339193207)) ;
#26897 = CARTESIAN_POINT('Ctrl Pts',(-18.507457139982,13.7454096268104,124.619951807237)) ;
#26898 = CARTESIAN_POINT('Ctrl Pts',(-18.6878125850875,13.5654205464475,124.378319667226)) ;
#26899 = CARTESIAN_POINT('Ctrl Pts',(-18.3128349524813,13.7553357183966,124.44624656969)) ;
#26900 = CARTESIAN_POINT('Ctrl Pts',(-18.5321161260099,13.5753466380337,124.239354778128)) ;
#26901 = CARTESIAN_POINT('Ctrl Pts',(-18.1503452309715,13.7652905035412,124.241231958245)) ;
#26902 = CARTESIAN_POINT('Ctrl Pts',(-18.4021255453027,13.5853014231783,124.075342601526)) ;
#26903 = CARTESIAN_POINT('Ctrl Pts',(-18.0251465109341,13.7753278731988,124.009068223143)) ;
#26904 = CARTESIAN_POINT('Ctrl Pts',(-18.3019676694534,13.5953387928359,123.889610906895)) ;
#26905 = CARTESIAN_POINT('Ctrl Pts',(-17.9431959784106,13.7852166833204,123.762452941019)) ;
#26906 = CARTESIAN_POINT('Ctrl Pts',(-18.2364086692508,13.6052276029575,123.692318981433)) ;
#26907 = CARTESIAN_POINT('Ctrl Pts',(-17.9044614031139,13.7952060423715,123.502822293364)) ;
#26908 = CARTESIAN_POINT('Ctrl Pts',(-18.2054221786113,13.6152169620086,123.484614462953)) ;
#26909 = CARTESIAN_POINT('Ctrl Pts',(-17.9115693386521,13.8051645898276,123.241226463732)) ;
#26910 = CARTESIAN_POINT('Ctrl Pts',(-18.2111097180374,13.6251755094647,123.275338178328)) ;
#26911 = CARTESIAN_POINT('Ctrl Pts',(-17.9630567197968,13.8150641663786,122.986205100608)) ;
#26912 = CARTESIAN_POINT('Ctrl Pts',(-18.2523005182494,13.6350750860157,123.071321986717)) ;
#26913 = CARTESIAN_POINT('Ctrl Pts',(-18.0595361492998,13.8251120782093,122.740443216478)) ;
#26914 = CARTESIAN_POINT('Ctrl Pts',(-18.329485128724,13.6451229978464,122.874712710548)) ;
#26915 = CARTESIAN_POINT('Ctrl Pts',(-18.1949930036132,13.8350074260699,122.518422190268)) ;
#26916 = CARTESIAN_POINT('Ctrl Pts',(-18.4378511109109,13.655018345707,122.697097049966)) ;
#26917 = CARTESIAN_POINT('Ctrl Pts',(-18.3697572977927,13.845069102601,122.320042659935)) ;
#26918 = CARTESIAN_POINT('Ctrl Pts',(-18.5776634866624,13.6650800222382,122.538393906198)) ;
#26919 = CARTESIAN_POINT('Ctrl Pts',(-18.5718588198519,13.8549136203502,122.158525512922)) ;
#26920 = CARTESIAN_POINT('Ctrl Pts',(-18.7393445112275,13.6749245399873,122.409181641225)) ;
#26921 = CARTESIAN_POINT('Ctrl Pts',(-18.8011469810602,13.864874064065,122.032284729829)) ;
#26922 = CARTESIAN_POINT('Ctrl Pts',(-18.9227751038679,13.6848849837021,122.308189886519)) ;
#26923 = CARTESIAN_POINT('Ctrl Pts',(-19.0509301231226,13.8749108968832,121.947590007007)) ;
#26924 = CARTESIAN_POINT('Ctrl Pts',(-19.1226020288338,13.6949218165203,122.240434931693)) ;
#26925 = CARTESIAN_POINT('Ctrl Pts',(-19.3074865101994,13.88478969363,121.907757156992)) ;
#26926 = CARTESIAN_POINT('Ctrl Pts',(-19.3278463927919,13.7048006132671,122.208569584531)) ;
#26927 = CARTESIAN_POINT('Ctrl Pts',(-19.5717537455678,13.8948490097584,121.91308802529)) ;
#26928 = CARTESIAN_POINT('Ctrl Pts',(-19.5392604248098,13.7148599293955,122.212835072421)) ;
#26929 = CARTESIAN_POINT('Ctrl Pts',(-19.8262549511952,13.9047194565116,121.963266910915)) ;
#26930 = CARTESIAN_POINT('Ctrl Pts',(-19.7428603300386,13.7247303761487,122.252978777756)) ;
#26931 = CARTESIAN_POINT('Ctrl Pts',(-20.0714142577279,13.9147120947696,122.057363864517)) ;
#26932 = CARTESIAN_POINT('Ctrl Pts',(-19.9389874113429,13.7347230144067,122.328256860103)) ;
#26933 = CARTESIAN_POINT('Ctrl Pts',(-20.2970965036502,13.9247441103175,122.193613633218)) ;
#26934 = CARTESIAN_POINT('Ctrl Pts',(-20.1195328981886,13.7447550299547,122.437257373362)) ;
#26935 = CARTESIAN_POINT('Ctrl Pts',(-20.4928009018349,13.9346099666241,122.363706237578)) ;
#26936 = CARTESIAN_POINT('Ctrl Pts',(-20.2760952675698,13.7546208862612,122.573331276944)) ;
#26937 = CARTESIAN_POINT('Ctrl Pts',(-20.6593476164435,13.9446792560932,122.569291069351)) ;
#26938 = CARTESIAN_POINT('Ctrl Pts',(-20.4093323747788,13.7646901757304,122.737799786026)) ;
#26939 = CARTESIAN_POINT('Ctrl Pts',(-20.7848399902421,13.9545228136445,122.795508554596)) ;
#26940 = CARTESIAN_POINT('Ctrl Pts',(-20.509725196703,13.7745337332817,122.91877307958)) ;
#26941 = CARTESIAN_POINT('Ctrl Pts',(-20.871120064522,13.9645029404324,123.043168459414)) ;
#26942 = CARTESIAN_POINT('Ctrl Pts',(-20.578748805291,13.7845138600695,123.116900896814)) ;
#26943 = CARTESIAN_POINT('Ctrl Pts',(-20.9127502836893,13.9745214890323,123.303126129535)) ;
#26944 = CARTESIAN_POINT('Ctrl Pts',(-20.6120524706176,13.7945324086694,123.324867123436)) ;
#26945 = CARTESIAN_POINT('Ctrl Pts',(-20.9092186327094,13.9844047895555,123.562857078074)) ;
#26946 = CARTESIAN_POINT('Ctrl Pts',(-20.609226783806,13.8044157091926,123.532650998994)) ;
#26947 = CARTESIAN_POINT('Ctrl Pts',(-20.8596340362664,13.9944730766036,123.822708783211)) ;
#26948 = CARTESIAN_POINT('Ctrl Pts',(-20.5695586439728,13.8144839962408,123.740532609343)) ;
#26949 = CARTESIAN_POINT('Ctrl Pts',(-20.7681595371697,14.0043031996223,124.064344085627)) ;
#26950 = CARTESIAN_POINT('Ctrl Pts',(-20.4963791721871,13.8243141192594,123.933839581481)) ;
#26951 = CARTESIAN_POINT('Ctrl Pts',(-20.6332814623007,14.0143697835476,124.291865630646)) ;
#26952 = CARTESIAN_POINT('Ctrl Pts',(-20.3884763385761,13.8343807031847,124.11585696606)) ;
#26953 = CARTESIAN_POINT('Ctrl Pts',(-20.4637992773007,14.0242598965621,124.488951781943)) ;
#26954 = CARTESIAN_POINT('Ctrl Pts',(-20.2528909214938,13.8442708161992,124.273525063999)) ;
#26955 = CARTESIAN_POINT('Ctrl Pts',(-20.2609821100153,14.0342525853247,124.655717889191)) ;
#26956 = CARTESIAN_POINT('Ctrl Pts',(-20.090637223389,13.8542635049618,124.406937730911)) ;
#26957 = CARTESIAN_POINT('Ctrl Pts',(-20.0328972096088,14.0442134736805,124.784181661414)) ;
#26958 = CARTESIAN_POINT('Ctrl Pts',(-19.9081695446619,13.8642243933176,124.509708392774)) ;
#26959 = CARTESIAN_POINT('Ctrl Pts',(-19.7872119388903,14.0541314185605,124.87112949854)) ;
#26960 = CARTESIAN_POINT('Ctrl Pts',(-19.7116219327022,13.8741423381976,124.579266367016)) ;
#26961 = CARTESIAN_POINT('Ctrl Pts',(-19.527842932523,14.0641391716567,124.914794637581)) ;
#26962 = CARTESIAN_POINT('Ctrl Pts',(-19.5041267743093,13.8841500912938,124.614198467582)) ;
#26963 = CARTESIAN_POINT('Ctrl Pts',(-19.2642632651857,14.0741702656157,124.912222739613)) ;
#26964 = CARTESIAN_POINT('Ctrl Pts',(-19.2932629428853,13.8941811852529,124.612140811124)) ;
#26965 = CARTESIAN_POINT('Ctrl Pts',(-19.0097259981526,14.0840182336437,124.865371406458)) ;
#26966 = CARTESIAN_POINT('Ctrl Pts',(-19.0896342385044,13.9040291532808,124.57465995883)) ;
#26967 = CARTESIAN_POINT('Ctrl Pts',(-18.7618772164016,14.0940801897696,124.773301901415)) ;
#26968 = CARTESIAN_POINT('Ctrl Pts',(-18.89135492329,13.9140911094067,124.501004319296)) ;
#26969 = CARTESIAN_POINT('Ctrl Pts',(-18.5376101429091,14.1039774013707,124.641559789166)) ;
#26970 = CARTESIAN_POINT('Ctrl Pts',(-18.7119419501136,13.9239883210078,124.395611039838)) ;
#26971 = CARTESIAN_POINT('Ctrl Pts',(-18.3384000135968,14.1139085680353,124.472965869001)) ;
#26972 = CARTESIAN_POINT('Ctrl Pts',(-18.5525741413936,13.9339194876725,124.26073644889)) ;
#26973 = CARTESIAN_POINT('Ctrl Pts',(-18.169843513441,14.1239507522395,124.269917095288)) ;
#26974 = CARTESIAN_POINT('Ctrl Pts',(-18.4177287173971,13.9439616718766,124.098297399059)) ;
#26975 = CARTESIAN_POINT('Ctrl Pts',(-18.0409566998773,14.1338374204927,124.044314253981)) ;
#26976 = CARTESIAN_POINT('Ctrl Pts',(-18.3146195241724,13.9538483401298,123.91781597991)) ;
#26977 = CARTESIAN_POINT('Ctrl Pts',(-17.9518498698231,14.1438305324709,123.797299870393)) ;
#26978 = CARTESIAN_POINT('Ctrl Pts',(-18.2433338227016,13.963841452108,123.720204732081)) ;
#26979 = CARTESIAN_POINT('Ctrl Pts',(-17.9072936184703,14.1537762100867,123.539763194409)) ;
#26980 = CARTESIAN_POINT('Ctrl Pts',(-18.2076886217236,13.9737871297239,123.514175908959)) ;
#26981 = CARTESIAN_POINT('Ctrl Pts',(-17.9075982211722,14.1637235130717,123.278346044345)) ;
#26982 = CARTESIAN_POINT('Ctrl Pts',(-18.2079318833263,13.9837344327088,123.305042647858)) ;
#26983 = CARTESIAN_POINT('Ctrl Pts',(-17.9540338467725,14.1737712368185,123.018424649771)) ;
#26984 = CARTESIAN_POINT('Ctrl Pts',(-18.245080078658,13.9937821564556,123.097105274778)) ;
#26985 = CARTESIAN_POINT('Ctrl Pts',(-18.0429036250617,14.183619610581,122.775359841272)) ;
#26986 = CARTESIAN_POINT('Ctrl Pts',(-18.3161751445601,14.0036305302181,122.90265434045)) ;
#26987 = CARTESIAN_POINT('Ctrl Pts',(-18.1733306008267,14.1935785830267,122.54846390798)) ;
#26988 = CARTESIAN_POINT('Ctrl Pts',(-18.4205160052355,14.0135895026638,122.721137613016)) ;
#26989 = CARTESIAN_POINT('Ctrl Pts',(-18.3428801887918,14.2036174449079,122.346364098552)) ;
#26990 = CARTESIAN_POINT('Ctrl Pts',(-18.5561553752817,14.023628364545,122.559457349719)) ;
#26991 = CARTESIAN_POINT('Ctrl Pts',(-18.5414813532127,14.2134960490797,122.179140432255)) ;
#26992 = CARTESIAN_POINT('Ctrl Pts',(-18.7150352359828,14.0335069687168,122.425678533261)) ;
#26993 = CARTESIAN_POINT('Ctrl Pts',(-18.7699215575239,14.223547590283,122.046595739492)) ;
#26994 = CARTESIAN_POINT('Ctrl Pts',(-18.8977872771299,14.0435585099201,122.319642127634)) ;
#26995 = CARTESIAN_POINT('Ctrl Pts',(-19.0141015690712,14.2334429882633,121.957035255779)) ;
#26996 = CARTESIAN_POINT('Ctrl Pts',(-19.0931303423171,14.0534539079004,122.247993398259)) ;
#26997 = CARTESIAN_POINT('Ctrl Pts',(-19.2740491001981,14.2434942208086,121.910385335695)) ;
#26998 = CARTESIAN_POINT('Ctrl Pts',(-19.3010884541272,14.0635051404457,122.210672757379)) ;
#26999 = CARTESIAN_POINT('Ctrl Pts',(-19.5338747027506,14.2533804114329,121.909562985904)) ;
#27000 = CARTESIAN_POINT('Ctrl Pts',(-19.5089480881137,14.07339133107,122.210014195614)) ;
#27001 = CARTESIAN_POINT('Ctrl Pts',(-19.7926811889532,14.2633729507487,121.953859464746)) ;
#27002 = CARTESIAN_POINT('Ctrl Pts',(-19.7159932556982,14.0833838703858,122.245450559124)) ;
#27003 = CARTESIAN_POINT('Ctrl Pts',(-20.0387837794866,14.2733213966434,122.042123340413)) ;
#27004 = CARTESIAN_POINT('Ctrl Pts',(-19.9128751830492,14.0933323162805,122.316060778059)) ;
#27005 = CARTESIAN_POINT('Ctrl Pts',(-20.2657069288235,14.2832581991753,122.171283774759)) ;
#27006 = CARTESIAN_POINT('Ctrl Pts',(-20.0944136903199,14.1032691188124,122.419388116494)) ;
#27007 = CARTESIAN_POINT('Ctrl Pts',(-20.4679459835233,14.2932412066266,122.338438899069)) ;
#27008 = CARTESIAN_POINT('Ctrl Pts',(-20.2562053796479,14.1132521262637,122.55311135473)) ;
#27009 = CARTESIAN_POINT('Ctrl Pts',(-20.6387149774407,14.3032850480414,122.539652891498)) ;
#27010 = CARTESIAN_POINT('Ctrl Pts',(-20.3928213084693,14.1232959676785,122.714082124582)) ;
#27011 = CARTESIAN_POINT('Ctrl Pts',(-20.7696539436816,14.3131132466653,122.762322078436)) ;
#27012 = CARTESIAN_POINT('Ctrl Pts',(-20.4975727394675,14.1331241663024,122.892215983891)) ;
#27013 = CARTESIAN_POINT('Ctrl Pts',(-20.8623069213888,14.3231898401075,123.010327296333)) ;
#27014 = CARTESIAN_POINT('Ctrl Pts',(-20.5716961867102,14.1432007597447,123.090620129128)) ;
#27015 = CARTESIAN_POINT('Ctrl Pts',(-20.909567306365,14.3330418394491,123.264936220785)) ;
#27016 = CARTESIAN_POINT('Ctrl Pts',(-20.6095053328595,14.1530527590862,123.294306109493)) ;
#27017 = CARTESIAN_POINT('Ctrl Pts',(-20.9121706248892,14.343115426273,123.529600919858)) ;
#27018 = CARTESIAN_POINT('Ctrl Pts',(-20.6115890777029,14.1631263459101,123.506038179509)) ;
#27019 = CARTESIAN_POINT('Ctrl Pts',(-20.8697248958235,14.3529556513705,123.784708643342)) ;
#27020 = CARTESIAN_POINT('Ctrl Pts',(-20.5776337239948,14.1729665710076,123.710123503099)) ;
#27021 = CARTESIAN_POINT('Ctrl Pts',(-20.7834156858806,14.3629213553991,124.031943418832)) ;
#27022 = CARTESIAN_POINT('Ctrl Pts',(-20.5085876682656,14.1829322750362,123.907911452828)) ;
#27023 = CARTESIAN_POINT('Ctrl Pts',(-20.6543560175008,14.3729479887057,124.26167893838)) ;
#27024 = CARTESIAN_POINT('Ctrl Pts',(-20.405340950833,14.1929589083428,124.091700497226)) ;
#27025 = CARTESIAN_POINT('Ctrl Pts',(-20.4893881315526,14.3828622844175,124.463327357308)) ;
#27026 = CARTESIAN_POINT('Ctrl Pts',(-20.273367967042,14.2028732040546,124.253019557366)) ;
#27027 = CARTESIAN_POINT('Ctrl Pts',(-20.29073289972,14.39285057311,124.634911409917)) ;
#27028 = CARTESIAN_POINT('Ctrl Pts',(-20.1144447718736,14.2128614927471,124.390287707971)) ;
#27029 = CARTESIAN_POINT('Ctrl Pts',(-20.0639385669575,14.4028893062683,124.769650931547)) ;
#27030 = CARTESIAN_POINT('Ctrl Pts',(-19.933009840498,14.2229002259054,124.498080437852)) ;
#27031 = CARTESIAN_POINT('Ctrl Pts',(-19.8221438934761,14.4127326380959,124.861560677325)) ;
#27032 = CARTESIAN_POINT('Ctrl Pts',(-19.7395754882741,14.232743557733,124.571609123733)) ;
#27033 = CARTESIAN_POINT('Ctrl Pts',(-19.5634174500474,14.4227603639755,124.911597480083)) ;
#27034 = CARTESIAN_POINT('Ctrl Pts',(-19.532594551231,14.2427712836126,124.611640002553)) ;
#27035 = CARTESIAN_POINT('Ctrl Pts',(-19.2997938732283,14.432792700364,124.915236180486)) ;
#27036 = CARTESIAN_POINT('Ctrl Pts',(-19.3216956393782,14.2528036200011,124.614552265305)) ;
#27037 = CARTESIAN_POINT('Ctrl Pts',(-19.0447452472327,14.4426222006646,124.874418148553)) ;
#27038 = CARTESIAN_POINT('Ctrl Pts',(-19.1176575176957,14.2626331203018,124.581899394182)) ;
#27039 = CARTESIAN_POINT('Ctrl Pts',(-18.796407103076,14.4526117045814,124.789299015739)) ;
#27040 = CARTESIAN_POINT('Ctrl Pts',(-18.9189866276755,14.2726226242185,124.513805617526)) ;
#27041 = CARTESIAN_POINT('Ctrl Pts',(-18.5657044122553,14.4626555450938,124.661080239922)) ;
#27042 = CARTESIAN_POINT('Ctrl Pts',(-18.734423674689,14.2826664647309,124.411231794536)) ;
#27043 = CARTESIAN_POINT('Ctrl Pts',(-18.3649628204512,14.4724772508619,124.498843726449)) ;
#27044 = CARTESIAN_POINT('Ctrl Pts',(-18.5738302074953,14.292488170499,124.281444409)) ;
#27045 = CARTESIAN_POINT('Ctrl Pts',(-18.1912720235427,14.4825122979942,124.300414746533)) ;
#27046 = CARTESIAN_POINT('Ctrl Pts',(-18.4348762631959,14.3025232176314,124.122702256751)) ;
#27047 = CARTESIAN_POINT('Ctrl Pts',(-18.055432254409,14.4925369754311,124.074689127998)) ;
#27048 = CARTESIAN_POINT('Ctrl Pts',(-18.3262031311123,14.3125478950683,123.942122532093)) ;
#27049 = CARTESIAN_POINT('Ctrl Pts',(-17.9619640242889,14.5023897902856,123.833226852752)) ;
#27050 = CARTESIAN_POINT('Ctrl Pts',(-18.2514273185047,14.3224007099227,123.748954049798)) ;
#27051 = CARTESIAN_POINT('Ctrl Pts',(-17.9107066774369,14.5123774998931,123.575833839664)) ;
#27052 = CARTESIAN_POINT('Ctrl Pts',(-18.210419791455,14.3323884195303,123.543040117254)) ;
#27053 = CARTESIAN_POINT('Ctrl Pts',(-17.9049402191342,14.5223075098872,123.314937805648)) ;
#27054 = CARTESIAN_POINT('Ctrl Pts',(-18.2058049219443,14.3423184295243,123.33432374461)) ;
#27055 = CARTESIAN_POINT('Ctrl Pts',(-17.9443990827381,14.5322972651064,123.055394867544)) ;
#27056 = CARTESIAN_POINT('Ctrl Pts',(-18.237370231834,14.3523081847435,123.126689256779)) ;
#27057 = CARTESIAN_POINT('Ctrl Pts',(-18.0289554645481,14.5423238737893,122.80583753216)) ;
#27058 = CARTESIAN_POINT('Ctrl Pts',(-18.3050137161035,14.3623347934264,122.927042810016)) ;
#27059 = CARTESIAN_POINT('Ctrl Pts',(-18.1535342537274,14.5522078138111,122.577928818094)) ;
#27060 = CARTESIAN_POINT('Ctrl Pts',(-18.4046749159261,14.3722187334482,122.744715509039)) ;
#27061 = CARTESIAN_POINT('Ctrl Pts',(-18.3170525414426,14.5621970413496,122.372560685954)) ;
#27062 = CARTESIAN_POINT('Ctrl Pts',(-18.5354880122314,14.3822079609867,122.580419941737)) ;
#27063 = CARTESIAN_POINT('Ctrl Pts',(-18.5151557257719,14.5722399118733,122.198188061704)) ;
#27064 = CARTESIAN_POINT('Ctrl Pts',(-18.6939694414926,14.3922508315104,122.440920462388)) ;
#27065 = CARTESIAN_POINT('Ctrl Pts',(-18.7355880780577,14.5820722986287,122.063388638443)) ;
#27066 = CARTESIAN_POINT('Ctrl Pts',(-18.8703137118598,14.4020832182658,122.333079750593)) ;
#27067 = CARTESIAN_POINT('Ctrl Pts',(-18.9797323076057,14.5920655918003,121.966658037112)) ;
#27068 = CARTESIAN_POINT('Ctrl Pts',(-19.0656282824221,14.4120765114374,122.255693489777)) ;
#27069 = CARTESIAN_POINT('Ctrl Pts',(-19.2380876823601,14.6020975974487,121.914120317295)) ;
#27070 = CARTESIAN_POINT('Ctrl Pts',(-19.2723122376113,14.4221085170859,122.213661473719)) ;
#27071 = CARTESIAN_POINT('Ctrl Pts',(-19.4972262784199,14.6119628534177,121.907034280981)) ;
#27072 = CARTESIAN_POINT('Ctrl Pts',(-19.479622479628,14.4319737730548,122.207990741055)) ;
#27073 = CARTESIAN_POINT('Ctrl Pts',(-19.7562992627137,14.6219247333252,121.944692330567)) ;
#27074 = CARTESIAN_POINT('Ctrl Pts',(-19.6868809582063,14.4419356529623,122.238115153452)) ;
#27075 = CARTESIAN_POINT('Ctrl Pts',(-20.0065648350329,14.6319596666871,122.027765848265)) ;
#27076 = CARTESIAN_POINT('Ctrl Pts',(-19.8870940599284,14.4519705863242,122.304572113767)) ;
#27077 = CARTESIAN_POINT('Ctrl Pts',(-20.2353895991265,14.6418446250664,122.150798715635)) ;
#27078 = CARTESIAN_POINT('Ctrl Pts',(-20.0701544291512,14.4618555447035,122.402996417728)) ;
#27079 = CARTESIAN_POINT('Ctrl Pts',(-20.4430039039663,14.6519102519891,122.314630587451)) ;
#27080 = CARTESIAN_POINT('Ctrl Pts',(-20.2362472126455,14.4719211716262,122.534060408975)) ;
#27081 = CARTESIAN_POINT('Ctrl Pts',(-20.6153099874822,14.6617493576534,122.507469086936)) ;
#27082 = CARTESIAN_POINT('Ctrl Pts',(-20.3740932248574,14.4817602772905,122.688329427988)) ;
#27083 = CARTESIAN_POINT('Ctrl Pts',(-20.7548702754188,14.6718121726588,122.732041086105)) ;
#27084 = CARTESIAN_POINT('Ctrl Pts',(-20.4857432796024,14.4918230922959,122.867986018619)) ;
#27085 = CARTESIAN_POINT('Ctrl Pts',(-20.8514895076296,14.6817083787074,122.973518167656)) ;
#27086 = CARTESIAN_POINT('Ctrl Pts',(-20.5630404332213,14.5017192983446,123.061166569921)) ;
#27087 = CARTESIAN_POINT('Ctrl Pts',(-20.905652298732,14.6916492017327,123.229045388477)) ;
#27088 = CARTESIAN_POINT('Ctrl Pts',(-20.6063727060311,14.5116601213698,123.265587688841)) ;
#27089 = CARTESIAN_POINT('Ctrl Pts',(-20.9147482972179,14.7016537847114,123.49182757385)) ;
#27090 = CARTESIAN_POINT('Ctrl Pts',(-20.6136516339194,14.5216647043485,123.475813306976)) ;
#27091 = CARTESIAN_POINT('Ctrl Pts',(-20.8777060565819,14.7116746791561,123.752541737872)) ;
#27092 = CARTESIAN_POINT('Ctrl Pts',(-20.584019929086,14.5316855987932,123.684384908824)) ;
#27093 = CARTESIAN_POINT('Ctrl Pts',(-20.7973137583484,14.7215665997455,123.999754867603)) ;
#27094 = CARTESIAN_POINT('Ctrl Pts',(-20.5197082201853,14.5415775193826,123.882155761826)) ;
#27095 = CARTESIAN_POINT('Ctrl Pts',(-20.6743041569518,14.7315600320909,124.231770792966)) ;
#27096 = CARTESIAN_POINT('Ctrl Pts',(-20.4213024934147,14.551570951728,124.067769440875)) ;
#27097 = CARTESIAN_POINT('Ctrl Pts',(-20.5135786631871,14.7415056369908,124.437867633095)) ;
#27098 = CARTESIAN_POINT('Ctrl Pts',(-20.2927239143119,14.5615165566279,124.232648095339)) ;
#27099 = CARTESIAN_POINT('Ctrl Pts',(-20.3198218573511,14.7514529104723,124.613360457444)) ;
#27100 = CARTESIAN_POINT('Ctrl Pts',(-20.137720063294,14.5714638301094,124.373043875978)) ;
#27101 = CARTESIAN_POINT('Ctrl Pts',(-20.0961599099383,14.7615008249487,124.753689774848)) ;
#27102 = CARTESIAN_POINT('Ctrl Pts',(-19.9587916558263,14.5815117445858,124.485309178269)) ;
#27103 = CARTESIAN_POINT('Ctrl Pts',(-19.8564776376663,14.771348465296,124.851279444888)) ;
#27104 = CARTESIAN_POINT('Ctrl Pts',(-19.7670469592938,14.5913593849331,124.563382825184)) ;
#27105 = CARTESIAN_POINT('Ctrl Pts',(-19.6007489896213,14.7813101806726,124.907199618394)) ;
#27106 = CARTESIAN_POINT('Ctrl Pts',(-19.5624646160184,14.6013211003097,124.608121129999)) ;
#27107 = CARTESIAN_POINT('Ctrl Pts',(-19.3373962978428,14.7913388042454,124.917606836282)) ;
#27108 = CARTESIAN_POINT('Ctrl Pts',(-19.3517825852773,14.6113497238825,124.616449119218)) ;
#27109 = CARTESIAN_POINT('Ctrl Pts',(-19.0793336231031,14.8012491663118,124.882634265756)) ;
#27110 = CARTESIAN_POINT('Ctrl Pts',(-19.1453323129572,14.6212600859489,124.58847329103)) ;
#27111 = CARTESIAN_POINT('Ctrl Pts',(-18.8304237660988,14.8111838599642,124.803839977348)) ;
#27112 = CARTESIAN_POINT('Ctrl Pts',(-18.9462038486766,14.6311947796013,124.52544003625)) ;
#27113 = CARTESIAN_POINT('Ctrl Pts',(-18.5966220485025,14.8212257030921,124.681499373881)) ;
#27114 = CARTESIAN_POINT('Ctrl Pts',(-18.7591614689245,14.6412366227292,124.427569556202)) ;
#27115 = CARTESIAN_POINT('Ctrl Pts',(-18.390716860511,14.8311102086625,124.523104155642)) ;
#27116 = CARTESIAN_POINT('Ctrl Pts',(-18.5944360498318,14.6511211282996,124.300855240205)) ;
#27117 = CARTESIAN_POINT('Ctrl Pts',(-18.2131739736385,14.8411123124477,124.329336878928)) ;
#27118 = CARTESIAN_POINT('Ctrl Pts',(-18.4524001167752,14.6611232320848,124.145842979682)) ;
#27119 = CARTESIAN_POINT('Ctrl Pts',(-18.0729290956816,14.8510306638627,124.109588770675)) ;
#27120 = CARTESIAN_POINT('Ctrl Pts',(-18.3402023497202,14.6710415834998,123.970045780687)) ;
#27121 = CARTESIAN_POINT('Ctrl Pts',(-17.9717628132547,14.8610783198836,123.865741080711)) ;
#27122 = CARTESIAN_POINT('Ctrl Pts',(-18.2592672790845,14.6810892395207,123.774968483768)) ;
#27123 = CARTESIAN_POINT('Ctrl Pts',(-17.9151745106479,14.8709495129118,123.612528140335)) ;
#27124 = CARTESIAN_POINT('Ctrl Pts',(-18.2139943885735,14.6909604325489,123.572398901037)) ;
#27125 = CARTESIAN_POINT('Ctrl Pts',(-17.9031429831484,14.8810152260553,123.34834743098)) ;
#27126 = CARTESIAN_POINT('Ctrl Pts',(-18.204367144922,14.7010261456924,123.361053634231)) ;
#27127 = CARTESIAN_POINT('Ctrl Pts',(-17.9361624249687,14.890867686628,123.091474379834)) ;
#27128 = CARTESIAN_POINT('Ctrl Pts',(-18.2307796125064,14.7108786062651,123.155558165158)) ;
#27129 = CARTESIAN_POINT('Ctrl Pts',(-18.0413449335706,14.9042961493505,122.754742299802)) ;
#27130 = CARTESIAN_POINT('Ctrl Pts',(-18.3149269800469,14.7243070689876,122.88615548597)) ;
#27131 = CARTESIAN_POINT('Ctrl Pts',(-18.2267874470069,14.9173770968676,122.460483907588)) ;
#27132 = CARTESIAN_POINT('Ctrl Pts',(-18.4633001749267,14.7373880165047,122.65073212564)) ;
#27133 = CARTESIAN_POINT('Ctrl Pts',(-18.4863543902938,14.9308515951022,122.219747666857)) ;
#27134 = CARTESIAN_POINT('Ctrl Pts',(-18.6709215324032,14.7508625147393,122.458175060593)) ;
#27135 = CARTESIAN_POINT('Ctrl Pts',(-18.7036544341988,14.9406836987116,122.079886991967)) ;
#27136 = CARTESIAN_POINT('Ctrl Pts',(-18.8447666073225,14.7606946183488,122.346277773026)) ;
#27137 = CARTESIAN_POINT('Ctrl Pts',(-18.9446987351203,14.9506496018383,121.977572951031)) ;
#27138 = CARTESIAN_POINT('Ctrl Pts',(-19.0375992137508,14.7706605214754,122.264426179784)) ;
#27139 = CARTESIAN_POINT('Ctrl Pts',(-19.2015765911018,14.9606770111485,121.918685704724)) ;
#27140 = CARTESIAN_POINT('Ctrl Pts',(-19.2431028113862,14.7806879307857,122.217314368209)) ;
#27141 = CARTESIAN_POINT('Ctrl Pts',(-19.4616556588049,14.9705880425151,121.905384721623)) ;
#27142 = CARTESIAN_POINT('Ctrl Pts',(-19.4511604538144,14.7905989621522,122.206669246989)) ;
#27143 = CARTESIAN_POINT('Ctrl Pts',(-19.8072618039374,14.9838323501362,121.947128778354)) ;
#27144 = CARTESIAN_POINT('Ctrl Pts',(-19.7276732696558,14.8038432697733,122.24007284524)) ;
#27145 = CARTESIAN_POINT('Ctrl Pts',(-20.2188550941679,15.0005328328073,122.113045312188)) ;
#27146 = CARTESIAN_POINT('Ctrl Pts',(-20.0569081396409,14.8205437524445,122.372778876184)) ;
#27147 = CARTESIAN_POINT('Ctrl Pts',(-20.5455679441702,15.0170396619631,122.405960959497)) ;
#27148 = CARTESIAN_POINT('Ctrl Pts',(-20.3183298372832,14.8370505816002,122.607156832751)) ;
#27149 = CARTESIAN_POINT('Ctrl Pts',(-20.7373262391937,15.0303502902007,122.698457845509)) ;
#27150 = CARTESIAN_POINT('Ctrl Pts',(-20.4717022185341,14.8503612098378,122.841112812095)) ;
#27151 = CARTESIAN_POINT('Ctrl Pts',(-20.8410482037776,15.0403428537408,122.939743261889)) ;
#27152 = CARTESIAN_POINT('Ctrl Pts',(-20.5546889224827,14.8603537733779,123.034149304461)) ;
#27153 = CARTESIAN_POINT('Ctrl Pts',(-20.9012011780977,15.0503729367423,123.196334518998)) ;
#27154 = CARTESIAN_POINT('Ctrl Pts',(-20.6028117682902,14.8703838563795,123.239415751326)) ;
#27155 = CARTESIAN_POINT('Ctrl Pts',(-20.9212136813736,15.0635465407401,123.542009444152)) ;
#27156 = CARTESIAN_POINT('Ctrl Pts',(-20.6188231356047,14.8835574603772,123.515975765134)) ;
#27157 = CARTESIAN_POINT('Ctrl Pts',(-20.8322977307926,15.0801842459715,123.97501211203)) ;
#27158 = CARTESIAN_POINT('Ctrl Pts',(-20.5476923868234,14.9001951656086,123.862358789437)) ;
#27159 = CARTESIAN_POINT('Ctrl Pts',(-20.5559470864143,15.1000660085389,124.425649304088)) ;
#27160 = CARTESIAN_POINT('Ctrl Pts',(-20.3266297541307,14.9200769281761,124.222868808078)) ;
#27161 = CARTESIAN_POINT('Ctrl Pts',(-20.2087222530336,15.1167623607554,124.70175262575)) ;
#27162 = CARTESIAN_POINT('Ctrl Pts',(-20.0488038623269,14.9367732803926,124.443780904704)) ;
#27163 = CARTESIAN_POINT('Ctrl Pts',(-19.8917080630513,15.1299193885445,124.839949683673)) ;
#27164 = CARTESIAN_POINT('Ctrl Pts',(-19.7952369425697,14.9499303081817,124.554316138444)) ;
#27165 = CARTESIAN_POINT('Ctrl Pts',(-19.5501536847632,15.1432967431881,124.92300774244)) ;
#27166 = CARTESIAN_POINT('Ctrl Pts',(-19.5219730467639,14.9633076628252,124.620769728734)) ;
#27167 = CARTESIAN_POINT('Ctrl Pts',(-19.1108554066313,15.1598275774469,124.912748434119)) ;
#27168 = CARTESIAN_POINT('Ctrl Pts',(-19.170551068665,14.979838497084,124.612563667479)) ;
#27169 = CARTESIAN_POINT('Ctrl Pts',(-18.616168502824,15.17979226719,124.720920100906)) ;
#27170 = CARTESIAN_POINT('Ctrl Pts',(-18.7747945577077,14.9998031868271,124.45910447757)) ;
#27171 = CARTESIAN_POINT('Ctrl Pts',(-18.2178819295255,15.1997087606136,124.372224270615)) ;
#27172 = CARTESIAN_POINT('Ctrl Pts',(-18.4561642627655,15.0197196802507,124.180149816018)) ;
#27173 = CARTESIAN_POINT('Ctrl Pts',(-17.9618943674429,15.2195984799632,123.909642300137)) ;
#27174 = CARTESIAN_POINT('Ctrl Pts',(-18.2513709039393,15.0396093996003,123.810084995758)) ;
#27175 = CARTESIAN_POINT('Ctrl Pts',(-17.8790867340295,15.239605209611,123.384461553137)) ;
#27176 = CARTESIAN_POINT('Ctrl Pts',(-18.1851220450662,15.0596161292481,123.389940905044)) ;
#27177 = CARTESIAN_POINT('Ctrl Pts',(-17.9792551414852,15.2594432632579,122.866690154571)) ;
#27178 = CARTESIAN_POINT('Ctrl Pts',(-18.2652543890131,15.079454182895,122.975722039237)) ;
#27179 = CARTESIAN_POINT('Ctrl Pts',(-18.2516493430185,15.2794366014715,122.410539526417)) ;
#27180 = CARTESIAN_POINT('Ctrl Pts',(-18.4831677681727,15.0994475211086,122.610800270065)) ;
#27181 = CARTESIAN_POINT('Ctrl Pts',(-18.661435692982,15.2993194008781,122.076711965965)) ;
#27182 = CARTESIAN_POINT('Ctrl Pts',(-18.8109961779416,15.1193303205152,122.34373578517)) ;
#27183 = CARTESIAN_POINT('Ctrl Pts',(-19.1602442446391,15.3192115817968,121.901912195536)) ;
#27184 = CARTESIAN_POINT('Ctrl Pts',(-19.2100434562284,15.1392225014339,122.203893842988)) ;
#27185 = CARTESIAN_POINT('Ctrl Pts',(-19.6893450348153,15.3391137602919,121.906937811211)) ;
#27186 = CARTESIAN_POINT('Ctrl Pts',(-19.6333250670439,15.159124679929,122.207913017499)) ;
#27187 = CARTESIAN_POINT('Ctrl Pts',(-20.1877316480936,15.3591510714956,122.094234259217)) ;
#27188 = CARTESIAN_POINT('Ctrl Pts',(-20.0320345164081,15.1791619911328,122.357748581197)) ;
#27189 = CARTESIAN_POINT('Ctrl Pts',(-20.5885091138174,15.3789635130365,122.4361550605)) ;
#27190 = CARTESIAN_POINT('Ctrl Pts',(-20.352658713179,15.1989744326736,122.631285748145)) ;
#27191 = CARTESIAN_POINT('Ctrl Pts',(-20.8514802727897,15.3990287537714,122.899819819407)) ;
#27192 = CARTESIAN_POINT('Ctrl Pts',(-20.5630361534512,15.2190396734085,123.002216473756)) ;
#27193 = CARTESIAN_POINT('Ctrl Pts',(-20.939569466923,15.4187859586272,123.417748054594)) ;
#27194 = CARTESIAN_POINT('Ctrl Pts',(-20.6335085384984,15.2387968782644,123.416561832562)) ;
#27195 = CARTESIAN_POINT('Ctrl Pts',(-20.8451846342489,15.4388192312729,123.941494843128)) ;
#27196 = CARTESIAN_POINT('Ctrl Pts',(-20.5580007277665,15.2588301509101,123.835558979513)) ;
#27197 = CARTESIAN_POINT('Ctrl Pts',(-20.5803681949361,15.4586321397268,124.396932991369)) ;
#27198 = CARTESIAN_POINT('Ctrl Pts',(-20.3461462373689,15.2786430593639,124.199911406604)) ;
#27199 = CARTESIAN_POINT('Ctrl Pts',(-20.1731096405733,15.4786282858542,124.738024765008)) ;
#27200 = CARTESIAN_POINT('Ctrl Pts',(-20.0203388220478,15.2986392054913,124.472784322776)) ;
#27201 = CARTESIAN_POINT('Ctrl Pts',(-19.6769061894164,15.4984900390767,124.918856330261)) ;
#27202 = CARTESIAN_POINT('Ctrl Pts',(-19.6233743087396,15.3185009587138,124.617449135294)) ;
#27203 = CARTESIAN_POINT('Ctrl Pts',(-19.1436360482035,15.5185585562048,124.919177517765)) ;
#27204 = CARTESIAN_POINT('Ctrl Pts',(-19.1967589767419,15.3385694758419,124.617705010039)) ;
#27205 = CARTESIAN_POINT('Ctrl Pts',(-18.6481039856445,15.5383894292016,124.739248841471)) ;
#27206 = CARTESIAN_POINT('Ctrl Pts',(-18.8003319653689,15.3584003488387,124.473760421146)) ;
#27207 = CARTESIAN_POINT('Ctrl Pts',(-18.2411262734598,15.5583113400183,124.400722475563)) ;
#27208 = CARTESIAN_POINT('Ctrl Pts',(-18.4747503480826,15.3783222596554,124.202937369334)) ;
#27209 = CARTESIAN_POINT('Ctrl Pts',(-17.9740267390617,15.5782407834536,123.943204335233)) ;
#27210 = CARTESIAN_POINT('Ctrl Pts',(-18.2610720716113,15.3982517030907,123.836921334488)) ;
#27211 = CARTESIAN_POINT('Ctrl Pts',(-17.8790194223619,15.59815045357,123.422718308582)) ;
#27212 = CARTESIAN_POINT('Ctrl Pts',(-18.1850681984714,15.4181613732071,123.42053129134)) ;
#27213 = CARTESIAN_POINT('Ctrl Pts',(-17.9662605748662,15.6180238108329,122.901708304058)) ;
#27214 = CARTESIAN_POINT('Ctrl Pts',(-18.254863873094,15.43803473047,123.00372270003)) ;
#27215 = CARTESIAN_POINT('Ctrl Pts',(-18.2276238439571,15.6380153454508,122.439173769157)) ;
#27216 = CARTESIAN_POINT('Ctrl Pts',(-18.4639568825122,15.4580262650879,122.633696362136)) ;
#27217 = CARTESIAN_POINT('Ctrl Pts',(-18.6285678009232,15.6578809628615,122.095505124988)) ;
#27218 = CARTESIAN_POINT('Ctrl Pts',(-18.7847146580216,15.4778918824987,122.358763014861)) ;
#27219 = CARTESIAN_POINT('Ctrl Pts',(-19.1253095706751,15.6778618926898,121.907746174012)) ;
#27220 = CARTESIAN_POINT('Ctrl Pts',(-19.1821092675839,15.4978728123269,122.208558782164)) ;
#27221 = CARTESIAN_POINT('Ctrl Pts',(-19.6552143908038,15.6978003547729,121.901373660419)) ;
#27222 = CARTESIAN_POINT('Ctrl Pts',(-19.6060335509028,15.51781127441,122.203463873449)) ;
#27223 = CARTESIAN_POINT('Ctrl Pts',(-20.1546433032014,15.7176925479946,122.075043824401)) ;
#27224 = CARTESIAN_POINT('Ctrl Pts',(-20.0055761682767,15.5377034676318,122.342403428384)) ;
#27225 = CARTESIAN_POINT('Ctrl Pts',(-20.5661496331982,15.73766326303,122.410119645807)) ;
#27226 = CARTESIAN_POINT('Ctrl Pts',(-20.3347791384015,15.5576741826671,122.610466906619)) ;
#27227 = CARTESIAN_POINT('Ctrl Pts',(-20.8373123753955,15.7574729346961,122.861577302707)) ;
#27228 = CARTESIAN_POINT('Ctrl Pts',(-20.5517067350592,15.5774838543332,122.97163565789)) ;
#27229 = CARTESIAN_POINT('Ctrl Pts',(-20.9393997364478,15.7774661513873,123.382866096592)) ;
#27230 = CARTESIAN_POINT('Ctrl Pts',(-20.6333723462591,15.5974770710244,123.388667788783)) ;
#27231 = CARTESIAN_POINT('Ctrl Pts',(-20.8584216081124,15.7973170635836,123.904440437728)) ;
#27232 = CARTESIAN_POINT('Ctrl Pts',(-20.5685874513888,15.6173279832208,123.805925914107)) ;
#27233 = CARTESIAN_POINT('Ctrl Pts',(-20.6013666268889,15.8173916699027,124.371819409561)) ;
#27234 = CARTESIAN_POINT('Ctrl Pts',(-20.3629338879566,15.6374025895398,124.17983155202)) ;
#27235 = CARTESIAN_POINT('Ctrl Pts',(-20.2709357008999,15.833908301786,124.661071335312)) ;
#27236 = CARTESIAN_POINT('Ctrl Pts',(-20.098605819619,15.6539192214231,124.411216220692)) ;
#27237 = CARTESIAN_POINT('Ctrl Pts',(-19.9567400193657,15.8472470094801,124.816295036982)) ;
#27238 = CARTESIAN_POINT('Ctrl Pts',(-19.8472304865429,15.6672579291172,124.535405548964)) ;
#27239 = CARTESIAN_POINT('Ctrl Pts',(-19.7085577801769,15.8570893837884,124.889269258747)) ;
#27240 = CARTESIAN_POINT('Ctrl Pts',(-19.6486898643955,15.6771003034255,124.593781066732)) ;
#27241 = CARTESIAN_POINT('Ctrl Pts',(-19.4460289923727,15.8671444037711,124.918903925048)) ;
#27242 = CARTESIAN_POINT('Ctrl Pts',(-19.438655254333,15.6871553234083,124.617484843905)) ;
#27243 = CARTESIAN_POINT('Ctrl Pts',(-19.0989283678214,15.8803765604287,124.897309206157)) ;
#27244 = CARTESIAN_POINT('Ctrl Pts',(-19.1610280086618,15.7003874800658,124.600218444694)) ;
#27245 = CARTESIAN_POINT('Ctrl Pts',(-18.680086550223,15.8969915277738,124.757481852894)) ;
#27246 = CARTESIAN_POINT('Ctrl Pts',(-18.8258890338263,15.717002447411,124.488333567479)) ;
#27247 = CARTESIAN_POINT('Ctrl Pts',(-18.3346327392559,15.913586114785,124.48329340641)) ;
#27248 = CARTESIAN_POINT('Ctrl Pts',(-18.549571248321,15.7335970344222,124.26900587412)) ;
#27249 = CARTESIAN_POINT('Ctrl Pts',(-18.1268897362054,15.9268196831404,124.204366870051)) ;
#27250 = CARTESIAN_POINT('Ctrl Pts',(-18.3833541247988,15.7468306027775,124.045842691326)) ;
#27251 = CARTESIAN_POINT('Ctrl Pts',(-18.0083439444997,15.9368633009491,123.968576154149)) ;
#27252 = CARTESIAN_POINT('Ctrl Pts',(-18.288524508184,15.7568742205862,123.857213407479)) ;
#27253 = CARTESIAN_POINT('Ctrl Pts',(-17.9336253681816,15.9467502251839,123.719711066793)) ;
#27254 = CARTESIAN_POINT('Ctrl Pts',(-18.228750615402,15.766761144821,123.658118921018)) ;
#27255 = CARTESIAN_POINT('Ctrl Pts',(-17.9024744065932,15.9567408796307,123.459039355824)) ;
#27256 = CARTESIAN_POINT('Ctrl Pts',(-18.2038316647778,15.7767517992678,123.44958390152)) ;
#27257 = CARTESIAN_POINT('Ctrl Pts',(-17.9170694041595,15.9667026380847,123.197660756749)) ;
#27258 = CARTESIAN_POINT('Ctrl Pts',(-18.2155127307376,15.7867135577218,123.240472575159)) ;
#27259 = CARTESIAN_POINT('Ctrl Pts',(-17.9967391763496,15.9800425031519,122.856207482281)) ;
#27260 = CARTESIAN_POINT('Ctrl Pts',(-18.2792369334935,15.800053422789,122.967353118238)) ;
#27261 = CARTESIAN_POINT('Ctrl Pts',(-18.1639736695918,15.9933512860652,122.544568270991)) ;
#27262 = CARTESIAN_POINT('Ctrl Pts',(-18.4130291807897,15.8133622057023,122.718017643817)) ;
#27263 = CARTESIAN_POINT('Ctrl Pts',(-18.4009205226991,16.0065470435093,122.291373958012)) ;
#27264 = CARTESIAN_POINT('Ctrl Pts',(-18.6026009981143,15.8265579631464,122.515452269556)) ;
#27265 = CARTESIAN_POINT('Ctrl Pts',(-18.6098352782094,16.0165089271858,122.133609050801)) ;
#27266 = CARTESIAN_POINT('Ctrl Pts',(-18.7697316665217,15.8365198468229,122.389244599765)) ;
#27267 = CARTESIAN_POINT('Ctrl Pts',(-18.8450601920169,16.0265520367004,122.013933523829)) ;
#27268 = CARTESIAN_POINT('Ctrl Pts',(-18.9579132372001,15.8465629563375,122.293505565848)) ;
#27269 = CARTESIAN_POINT('Ctrl Pts',(-19.0926161288735,16.0364042866996,121.938083702946)) ;
#27270 = CARTESIAN_POINT('Ctrl Pts',(-19.1559583816547,15.8564152063368,122.232828069619)) ;
#27271 = CARTESIAN_POINT('Ctrl Pts',(-19.3525761374353,16.0463758236501,121.90535120371)) ;
#27272 = CARTESIAN_POINT('Ctrl Pts',(-19.3639266242928,15.8663867432872,122.206644267402)) ;
#27273 = CARTESIAN_POINT('Ctrl Pts',(-19.6149622143192,16.0563710891276,121.918309627861)) ;
#27274 = CARTESIAN_POINT('Ctrl Pts',(-19.5738352989783,15.8763820087648,122.217013257549)) ;
#27275 = CARTESIAN_POINT('Ctrl Pts',(-19.8719707676213,16.0664050620013,121.977157725234)) ;
#27276 = CARTESIAN_POINT('Ctrl Pts',(-19.7794416116365,15.8864159816384,122.264093925763)) ;
#27277 = CARTESIAN_POINT('Ctrl Pts',(-20.1107386746183,16.0762604767636,122.077550542983)) ;
#27278 = CARTESIAN_POINT('Ctrl Pts',(-19.9704548934143,15.8962713964007,122.344410174474)) ;
#27279 = CARTESIAN_POINT('Ctrl Pts',(-20.3317609231274,16.0862597542724,122.219585083318)) ;
#27280 = CARTESIAN_POINT('Ctrl Pts',(-20.1472714239141,15.9062706739096,122.458039646496)) ;
#27281 = CARTESIAN_POINT('Ctrl Pts',(-20.5230102658078,16.0961549384354,122.395838020282)) ;
#27282 = CARTESIAN_POINT('Ctrl Pts',(-20.3002692442417,15.9161658580725,122.599043480994)) ;
#27283 = CARTESIAN_POINT('Ctrl Pts',(-20.6833117694189,16.1062153180762,122.606026601043)) ;
#27284 = CARTESIAN_POINT('Ctrl Pts',(-20.4285086974711,15.9262262377133,122.76719571147)) ;
#27285 = CARTESIAN_POINT('Ctrl Pts',(-20.8023123453152,16.1160651870843,122.835923343469)) ;
#27286 = CARTESIAN_POINT('Ctrl Pts',(-20.5237070533521,15.9360761067214,122.951113839647)) ;
#27287 = CARTESIAN_POINT('Ctrl Pts',(-20.8815749658397,16.1260967482922,123.087326542233)) ;
#27288 = CARTESIAN_POINT('Ctrl Pts',(-20.5871150742216,15.9461076679293,123.152237028848)) ;
#27289 = CARTESIAN_POINT('Ctrl Pts',(-20.9153886455586,16.1361071971745,123.3482327168)) ;
#27290 = CARTESIAN_POINT('Ctrl Pts',(-20.6141638267646,15.9561181168116,123.360962211071)) ;
#27291 = CARTESIAN_POINT('Ctrl Pts',(-20.9038000062041,16.1460139365915,123.608304860459)) ;
#27292 = CARTESIAN_POINT('Ctrl Pts',(-20.604890742972,15.9660248562286,123.569019582891)) ;
#27293 = CARTESIAN_POINT('Ctrl Pts',(-20.8475493442764,16.1559519526599,123.863320444448)) ;
#27294 = CARTESIAN_POINT('Ctrl Pts',(-20.5598881638927,15.9759628722971,123.773031376224)) ;
#27295 = CARTESIAN_POINT('Ctrl Pts',(-20.7473434745622,16.1659571991111,124.106434248665)) ;
#27296 = CARTESIAN_POINT('Ctrl Pts',(-20.4797215247247,15.9859681187482,123.967521547182)) ;
#27297 = CARTESIAN_POINT('Ctrl Pts',(-20.6056840713685,16.1759912601674,124.328819428175)) ;
#27298 = CARTESIAN_POINT('Ctrl Pts',(-20.3663921647497,15.9960021798045,124.145428536233)) ;
#27299 = CARTESIAN_POINT('Ctrl Pts',(-20.4312280688443,16.1858363412255,124.519891626386)) ;
#27300 = CARTESIAN_POINT('Ctrl Pts',(-20.2268260969221,16.0058472608626,124.298284524298)) ;
#27301 = CARTESIAN_POINT('Ctrl Pts',(-20.2236607634961,16.195822147179,124.680379963816)) ;
#27302 = CARTESIAN_POINT('Ctrl Pts',(-20.0607710803416,16.0158330668161,124.426673466983)) ;
#27303 = CARTESIAN_POINT('Ctrl Pts',(-19.9925740517516,16.2057569677332,124.801974564811)) ;
#27304 = CARTESIAN_POINT('Ctrl Pts',(-19.8759009849248,16.0257678873703,124.523947205164)) ;
#27305 = CARTESIAN_POINT('Ctrl Pts',(-19.7408239243177,16.2158144928654,124.88232980859)) ;
#27306 = CARTESIAN_POINT('Ctrl Pts',(-19.674500158399,16.0358254125025,124.588229439226)) ;
#27307 = CARTESIAN_POINT('Ctrl Pts',(-19.4850756391553,16.2256361435168,124.917322735119)) ;
#27308 = CARTESIAN_POINT('Ctrl Pts',(-19.4699018773493,16.0456470631539,124.616221674339)) ;
#27309 = CARTESIAN_POINT('Ctrl Pts',(-19.2210119356238,16.2356922070215,124.90763544783)) ;
#27310 = CARTESIAN_POINT('Ctrl Pts',(-19.258650898185,16.0557031266586,124.608469860502)) ;
#27311 = CARTESIAN_POINT('Ctrl Pts',(-18.965674000184,16.2456328740854,124.852413667813)) ;
#27312 = CARTESIAN_POINT('Ctrl Pts',(-19.0543812431617,16.0656437937226,124.564290497931)) ;
#27313 = CARTESIAN_POINT('Ctrl Pts',(-18.7243829673979,16.2555372677514,124.754815092852)) ;
#27314 = CARTESIAN_POINT('Ctrl Pts',(-18.8613495382106,16.0755481873885,124.486210004982)) ;
#27315 = CARTESIAN_POINT('Ctrl Pts',(-18.5006518515227,16.2655837915144,124.614693286642)) ;
#27316 = CARTESIAN_POINT('Ctrl Pts',(-18.6823656136091,16.0855947111516,124.374110855756)) ;
#27317 = CARTESIAN_POINT('Ctrl Pts',(-18.3073636533246,16.2754798745308,124.440639733717)) ;
#27318 = CARTESIAN_POINT('Ctrl Pts',(-18.5277366902723,16.0954907941679,124.234866901715)) ;
#27319 = CARTESIAN_POINT('Ctrl Pts',(-18.1445816442607,16.2855465737608,124.232170442766)) ;
#27320 = CARTESIAN_POINT('Ctrl Pts',(-18.3975125052179,16.105557493398,124.068090149545)) ;
#27321 = CARTESIAN_POINT('Ctrl Pts',(-18.0231616074987,16.2953701841619,124.004307681981)) ;
#27322 = CARTESIAN_POINT('Ctrl Pts',(-18.3003785015697,16.115381103799,123.885799728941)) ;
#27323 = CARTESIAN_POINT('Ctrl Pts',(-17.9408403240638,16.3054260443394,123.753235338654)) ;
#27324 = CARTESIAN_POINT('Ctrl Pts',(-18.2345231623342,16.1254369639765,123.684941163944)) ;
#27325 = CARTESIAN_POINT('Ctrl Pts',(-17.904145201317,16.3153591906443,123.494762458891)) ;
#27326 = CARTESIAN_POINT('Ctrl Pts',(-18.2051689666766,16.1353701102815,123.478162945526)) ;
#27327 = CARTESIAN_POINT('Ctrl Pts',(-17.9123613233359,16.3253044464149,123.233570994404)) ;
#27328 = CARTESIAN_POINT('Ctrl Pts',(-18.2117436421572,16.1453153660521,123.269210168122)) ;
#27329 = CARTESIAN_POINT('Ctrl Pts',(-17.9658149650056,16.3352877448534,122.976690048544)) ;
#27330 = CARTESIAN_POINT('Ctrl Pts',(-18.2545082370437,16.1552986644905,123.063705923525)) ;
#27331 = CARTESIAN_POINT('Ctrl Pts',(-18.0638986666255,16.345324925,122.731859880856)) ;
#27332 = CARTESIAN_POINT('Ctrl Pts',(-18.3329769087346,16.1653358446372,122.867842396204)) ;
#27333 = CARTESIAN_POINT('Ctrl Pts',(-18.2001537297579,16.3551794777095,122.511606700127)) ;
#27334 = CARTESIAN_POINT('Ctrl Pts',(-18.4419820544397,16.1751903973466,122.691641395589)) ;
#27335 = CARTESIAN_POINT('Ctrl Pts',(-18.3747984971053,16.3651789961568,122.315323705892)) ;
#27336 = CARTESIAN_POINT('Ctrl Pts',(-18.5816990552253,16.185189915794,122.534616199794)) ;
#27337 = CARTESIAN_POINT('Ctrl Pts',(-18.5786176379803,16.3750740786189,122.153776522294)) ;
#27338 = CARTESIAN_POINT('Ctrl Pts',(-18.7447549194951,16.195084998256,122.405380095778)) ;
#27339 = CARTESIAN_POINT('Ctrl Pts',(-18.8111591522696,16.385134624125,122.028064933009)) ;
#27340 = CARTESIAN_POINT('Ctrl Pts',(-18.9307890798417,16.2051455437621,122.304812173805)) ;
#27341 = CARTESIAN_POINT('Ctrl Pts',(-19.0567347651697,16.394983931373,121.946236873333)) ;
#27342 = CARTESIAN_POINT('Ctrl Pts',(-19.1272492874052,16.2149948510101,122.239351517279)) ;
#27343 = CARTESIAN_POINT('Ctrl Pts',(-19.3172847594668,16.4050110214604,121.906948036796)) ;
#27344 = CARTESIAN_POINT('Ctrl Pts',(-19.3356895344519,16.2250219410975,122.207921911425)) ;
#27345 = CARTESIAN_POINT('Ctrl Pts',(-19.5807454043777,16.4150399255973,121.91419747043)) ;
#27346 = CARTESIAN_POINT('Ctrl Pts',(-19.5464580626688,16.2350508452344,122.213723077586)) ;
#27347 = CARTESIAN_POINT('Ctrl Pts',(-19.8342636546748,16.4248837906966,121.965599859095)) ;
#27348 = CARTESIAN_POINT('Ctrl Pts',(-19.7492714785227,16.2448947103337,122.254846299181)) ;
#27349 = CARTESIAN_POINT('Ctrl Pts',(-20.0789676317228,16.434879617405,122.0611017389)) ;
#27350 = CARTESIAN_POINT('Ctrl Pts',(-19.9450340249279,16.2548905370421,122.331249046834)) ;
#27351 = CARTESIAN_POINT('Ctrl Pts',(-20.3037842341569,16.444904834054,122.198459857618)) ;
#27352 = CARTESIAN_POINT('Ctrl Pts',(-20.1248865660534,16.2649157536911,122.441136831011)) ;
#27353 = CARTESIAN_POINT('Ctrl Pts',(-20.4988993121104,16.4547946662116,122.370150559373)) ;
#27354 = CARTESIAN_POINT('Ctrl Pts',(-20.2809771772072,16.2748055858487,122.578490004565)) ;
#27355 = CARTESIAN_POINT('Ctrl Pts',(-20.6631697043296,16.4647855222963,122.574949866266)) ;
#27356 = CARTESIAN_POINT('Ctrl Pts',(-20.4123923501296,16.2847964419335,122.742330173249)) ;
#27357 = CARTESIAN_POINT('Ctrl Pts',(-20.7887677400445,16.4747306168892,122.804137700936)) ;
#27358 = CARTESIAN_POINT('Ctrl Pts',(-20.512869395449,16.2947415365263,122.925680738138)) ;
#27359 = CARTESIAN_POINT('Ctrl Pts',(-20.8731883104183,16.4846825206573,123.051673973059)) ;
#27360 = CARTESIAN_POINT('Ctrl Pts',(-20.5804045428109,16.3046934402944,123.123709795798)) ;
#27361 = CARTESIAN_POINT('Ctrl Pts',(-20.9134563188917,16.4947189201267,123.312320962728)) ;
#27362 = CARTESIAN_POINT('Ctrl Pts',(-20.612617681498,16.3147298397639,123.332227690102)) ;
#27363 = CARTESIAN_POINT('Ctrl Pts',(-20.9081282976239,16.5046079902154,123.572149884728)) ;
#27364 = CARTESIAN_POINT('Ctrl Pts',(-20.6083540200427,16.3246189098525,123.540090066167)) ;
#27365 = CARTESIAN_POINT('Ctrl Pts',(-20.8577220598271,16.5145972795863,123.829766727629)) ;
#27366 = CARTESIAN_POINT('Ctrl Pts',(-20.5680279279272,16.3346081992234,123.746183149683)) ;
#27367 = CARTESIAN_POINT('Ctrl Pts',(-20.76345961891,16.524555845796,124.073893348995)) ;
#27368 = CARTESIAN_POINT('Ctrl Pts',(-20.4926169796923,16.3445667654331,123.941483690802)) ;
#27369 = CARTESIAN_POINT('Ctrl Pts',(-20.6295786198911,16.5344554170128,124.296968784774)) ;
#27370 = CARTESIAN_POINT('Ctrl Pts',(-20.3855116377468,16.3544663366499,124.119942892736)) ;
#27371 = CARTESIAN_POINT('Ctrl Pts',(-20.4564004098396,16.5445033314271,124.49625876178)) ;
#27372 = CARTESIAN_POINT('Ctrl Pts',(-20.246968141716,16.3645142510642,124.279374299401)) ;
#27373 = CARTESIAN_POINT('Ctrl Pts',(-20.254440134761,16.5543986742876,124.660130610446)) ;
#27374 = CARTESIAN_POINT('Ctrl Pts',(-20.0853998401919,16.3744095939248,124.410470518004)) ;
#27375 = CARTESIAN_POINT('Ctrl Pts',(-20.0233532789183,16.5644603682351,124.788566418278)) ;
#27376 = CARTESIAN_POINT('Ctrl Pts',(-19.9005296298809,16.3844712878722,124.513218396484)) ;
#27377 = CARTESIAN_POINT('Ctrl Pts',(-19.7788459931032,16.5743048213192,124.873119039239)) ;
#27378 = CARTESIAN_POINT('Ctrl Pts',(-19.7049244705946,16.3943157409564,124.580859189868)) ;
#27379 = CARTESIAN_POINT('Ctrl Pts',(-19.5205255375102,16.5842655062777,124.915317433973)) ;
#27380 = CARTESIAN_POINT('Ctrl Pts',(-19.4982683335334,16.4042764259148,124.614617059786)) ;
#27381 = CARTESIAN_POINT('Ctrl Pts',(-19.2568102129339,16.5943014387862,124.911553126493)) ;
#27382 = CARTESIAN_POINT('Ctrl Pts',(-19.2872959783146,16.4143123584233,124.611604711671)) ;
#27383 = CARTESIAN_POINT('Ctrl Pts',(-19.0015211293968,16.6041900544743,124.863040443295)) ;
#27384 = CARTESIAN_POINT('Ctrl Pts',(-19.0830656658347,16.4242009741114,124.572793892405)) ;
#27385 = CARTESIAN_POINT('Ctrl Pts',(-18.7552356821971,16.6142044636167,124.770248444018)) ;
#27386 = CARTESIAN_POINT('Ctrl Pts',(-18.8860375696502,16.4342153832538,124.498559626099)) ;
#27387 = CARTESIAN_POINT('Ctrl Pts',(-18.5287435554736,16.6242382725745,124.635270964711)) ;
#27388 = CARTESIAN_POINT('Ctrl Pts',(-18.7048442231239,16.4442491922116,124.390576829673)) ;
#27389 = CARTESIAN_POINT('Ctrl Pts',(-18.3326680459431,16.6340687268307,124.467023867572)) ;
#27390 = CARTESIAN_POINT('Ctrl Pts',(-18.5479851753716,16.4540796464678,124.255979389229)) ;
#27391 = CARTESIAN_POINT('Ctrl Pts',(-18.164649593129,16.6441463944089,124.262383242805)) ;
#27392 = CARTESIAN_POINT('Ctrl Pts',(-18.4135707132439,16.464157314046,124.092266173035)) ;
#27393 = CARTESIAN_POINT('Ctrl Pts',(-18.037457177748,16.6539982625311,124.03681949593)) ;
#27394 = CARTESIAN_POINT('Ctrl Pts',(-18.3118178639604,16.4740091821683,123.911815773256)) ;
#27395 = CARTESIAN_POINT('Ctrl Pts',(-17.949256848314,16.6640713000965,123.787285292001)) ;
#27396 = CARTESIAN_POINT('Ctrl Pts',(-18.241258048914,16.4840822197336,123.712187880445)) ;
#27397 = CARTESIAN_POINT('Ctrl Pts',(-17.9067465102641,16.6739138534474,123.53212739955)) ;
#27398 = CARTESIAN_POINT('Ctrl Pts',(-18.2072505652693,16.4939247730845,123.508062584724)) ;
#27399 = CARTESIAN_POINT('Ctrl Pts',(-17.908337764321,16.6838942489408,123.269869124294)) ;
#27400 = CARTESIAN_POINT('Ctrl Pts',(-18.208523956492,16.5039051685779,123.29825621506)) ;
#27401 = CARTESIAN_POINT('Ctrl Pts',(-17.9561266808866,16.6939127269186,123.010973721011)) ;
#27402 = CARTESIAN_POINT('Ctrl Pts',(-18.2467556009483,16.5139236465557,123.091139978071)) ;
#27403 = CARTESIAN_POINT('Ctrl Pts',(-18.046394284067,16.7037960412247,122.767407615452)) ;
#27404 = CARTESIAN_POINT('Ctrl Pts',(-18.3189697326464,16.5238069608618,122.896288048403)) ;
#27405 = CARTESIAN_POINT('Ctrl Pts',(-18.1800998015951,16.7138643437634,122.539143460683)) ;
#27406 = CARTESIAN_POINT('Ctrl Pts',(-18.4259346651635,16.5338752634005,122.713676647449)) ;
#27407 = CARTESIAN_POINT('Ctrl Pts',(-18.3471784469217,16.7236943910368,122.342066798614)) ;
#27408 = CARTESIAN_POINT('Ctrl Pts',(-18.5595970360175,16.543705310674,122.556016471638)) ;
#27409 = CARTESIAN_POINT('Ctrl Pts',(-18.5504420735912,16.7337612624523,122.172817736648)) ;
#27410 = CARTESIAN_POINT('Ctrl Pts',(-18.7222083400755,16.5537721820895,122.420617207245)) ;
#27411 = CARTESIAN_POINT('Ctrl Pts',(-18.7760904676618,16.7436503012514,122.043833574538)) ;
#27412 = CARTESIAN_POINT('Ctrl Pts',(-18.9027264648716,16.5636612208885,122.317430542113)) ;
#27413 = CARTESIAN_POINT('Ctrl Pts',(-19.0231340623094,16.7536469993855,121.95457073187)) ;
#27414 = CARTESIAN_POINT('Ctrl Pts',(-19.1003612452814,16.5736579190226,122.246020463371)) ;
#27415 = CARTESIAN_POINT('Ctrl Pts',(-19.2808414151497,16.7635994250975,121.909859064209)) ;
#27416 = CARTESIAN_POINT('Ctrl Pts',(-19.306526737126,16.5836103447346,122.210251379847)) ;
#27417 = CARTESIAN_POINT('Ctrl Pts',(-19.5420687997964,16.7735407273304,121.910209653822)) ;
#27418 = CARTESIAN_POINT('Ctrl Pts',(-19.515508139504,16.5935516469676,122.210531942016)) ;
#27419 = CARTESIAN_POINT('Ctrl Pts',(-19.8004505578449,16.7835239664143,121.955836958364)) ;
#27420 = CARTESIAN_POINT('Ctrl Pts',(-19.7222133350524,16.6035348860515,122.247033765642)) ;
#27421 = CARTESIAN_POINT('Ctrl Pts',(-20.0481664431086,16.7935627679829,122.04650185724)) ;
#27422 = CARTESIAN_POINT('Ctrl Pts',(-19.9203861326362,16.6135736876201,122.319565851317)) ;
#27423 = CARTESIAN_POINT('Ctrl Pts',(-20.27233537467,16.8034108741046,122.175874106053)) ;
#27424 = CARTESIAN_POINT('Ctrl Pts',(-20.0997202925184,16.6234217937417,122.423063076114)) ;
#27425 = CARTESIAN_POINT('Ctrl Pts',(-20.4750293998556,16.8134710696799,122.345566817946)) ;
#27426 = CARTESIAN_POINT('Ctrl Pts',(-20.2618757772164,16.633481989317,122.55881737648)) ;
#27427 = CARTESIAN_POINT('Ctrl Pts',(-20.6422713390571,16.8233687529913,122.544786148084)) ;
#27428 = CARTESIAN_POINT('Ctrl Pts',(-20.3956688189713,16.6433796726285,122.718192224318)) ;
#27429 = CARTESIAN_POINT('Ctrl Pts',(-20.7735531876702,16.8332997933653,122.770334392659)) ;
#27430 = CARTESIAN_POINT('Ctrl Pts',(-20.5006942028639,16.6533107130024,122.898630207615)) ;
#27431 = CARTESIAN_POINT('Ctrl Pts',(-20.864420100794,16.8433420110219,123.018091751125)) ;
#27432 = CARTESIAN_POINT('Ctrl Pts',(-20.5733879339271,16.6633529306591,123.096836198398)) ;
#27433 = CARTESIAN_POINT('Ctrl Pts',(-20.9103551819919,16.8532286717559,123.273822728003)) ;
#27434 = CARTESIAN_POINT('Ctrl Pts',(-20.61013604196,16.673239591393,123.30142008903)) ;
#27435 = CARTESIAN_POINT('Ctrl Pts',(-20.9116383536201,16.8632217803584,123.536414570098)) ;
#27436 = CARTESIAN_POINT('Ctrl Pts',(-20.6111628897148,16.6832326999955,123.511493398078)) ;
#27437 = CARTESIAN_POINT('Ctrl Pts',(-20.8674180471858,16.8731674789966,123.794009449891)) ;
#27438 = CARTESIAN_POINT('Ctrl Pts',(-20.5757870061501,16.6931783986337,123.717568881039)) ;
#27439 = CARTESIAN_POINT('Ctrl Pts',(-20.7796283027966,16.8831147012677,124.04024353424)) ;
#27440 = CARTESIAN_POINT('Ctrl Pts',(-20.5055557607933,16.7031256209048,123.91455585675)) ;
#27441 = CARTESIAN_POINT('Ctrl Pts',(-20.6488602156385,16.8931627268478,124.269630633099)) ;
#27442 = CARTESIAN_POINT('Ctrl Pts',(-20.4009414915831,16.7131736464849,124.0980658808)) ;
#27443 = CARTESIAN_POINT('Ctrl Pts',(-20.4837823786232,16.9030099739907,124.468914512535)) ;
#27444 = CARTESIAN_POINT('Ctrl Pts',(-20.2688802436977,16.7230208936278,124.257492376889)) ;
#27445 = CARTESIAN_POINT('Ctrl Pts',(-20.2848296697992,16.9129731510814,124.639107596571)) ;
#27446 = CARTESIAN_POINT('Ctrl Pts',(-20.1097187494631,16.7329840707186,124.393647070472)) ;
#27447 = CARTESIAN_POINT('Ctrl Pts',(-20.0576375877666,16.9230028721148,124.772718133945)) ;
#27448 = CARTESIAN_POINT('Ctrl Pts',(-19.9279652726105,16.743013791752,124.500535980068)) ;
#27449 = CARTESIAN_POINT('Ctrl Pts',(-19.8138676646833,16.9329073396477,124.864008421836)) ;
#27450 = CARTESIAN_POINT('Ctrl Pts',(-19.7329502140236,16.7529182592849,124.573568505699)) ;
#27451 = CARTESIAN_POINT('Ctrl Pts',(-19.5549188176407,16.9429318254775,124.912240141092)) ;
#27452 = CARTESIAN_POINT('Ctrl Pts',(-19.5257912019944,16.7629427451146,124.612154489046)) ;
#27453 = CARTESIAN_POINT('Ctrl Pts',(-19.2946338276999,16.9528356606014,124.914963066489)) ;
#27454 = CARTESIAN_POINT('Ctrl Pts',(-19.3175639397184,16.7728465802385,124.614333480641)) ;
#27455 = CARTESIAN_POINT('Ctrl Pts',(-19.0340655773043,16.9628868513114,124.871886584455)) ;
#27456 = CARTESIAN_POINT('Ctrl Pts',(-19.1091090337395,16.7828977709485,124.579872926838)) ;
#27457 = CARTESIAN_POINT('Ctrl Pts',(-18.7889990253017,16.9727712939697,124.785703184415)) ;
#27458 = CARTESIAN_POINT('Ctrl Pts',(-18.9130563598052,16.7927822136068,124.510927134029)) ;
#27459 = CARTESIAN_POINT('Ctrl Pts',(-18.5599373549121,16.9827643018216,124.657327597577)) ;
#27460 = CARTESIAN_POINT('Ctrl Pts',(-18.7298067701624,16.8027752214587,124.408227443796)) ;
#27461 = CARTESIAN_POINT('Ctrl Pts',(-18.3575795915092,16.9927126215379,124.491777975001)) ;
#27462 = CARTESIAN_POINT('Ctrl Pts',(-18.5679204008152,16.812723541175,124.275788625095)) ;
#27463 = CARTESIAN_POINT('Ctrl Pts',(-18.186980138861,17.0026494602473,124.294109650112)) ;
#27464 = CARTESIAN_POINT('Ctrl Pts',(-18.4314405125063,16.8226603798844,124.117654920075)) ;
#27465 = CARTESIAN_POINT('Ctrl Pts',(-18.0523597654586,17.0126324491669,124.06890152174)) ;
#27466 = CARTESIAN_POINT('Ctrl Pts',(-18.3237435055854,16.832643368804,123.93748907981)) ;
#27467 = CARTESIAN_POINT('Ctrl Pts',(-17.9587951854769,17.022676328531,123.82213239202)) ;
#27468 = CARTESIAN_POINT('Ctrl Pts',(-18.2488910084418,16.8426872481681,123.740073929916)) ;
#27469 = CARTESIAN_POINT('Ctrl Pts',(-17.9099416408422,17.0325043938894,123.568481191394)) ;
#27470 = CARTESIAN_POINT('Ctrl Pts',(-18.2098074301906,16.8525153135265,123.537154287906)) ;
#27471 = CARTESIAN_POINT('Ctrl Pts',(-17.9056580144789,17.0425814824443,123.303759681484)) ;
#27472 = CARTESIAN_POINT('Ctrl Pts',(-18.2063795179285,16.8625924020815,123.325376748704)) ;
#27473 = CARTESIAN_POINT('Ctrl Pts',(-17.9463150166963,17.0524316346006,123.048052157451)) ;
#27474 = CARTESIAN_POINT('Ctrl Pts',(-18.2389039336585,16.8724425542378,123.120811549314)) ;
#27475 = CARTESIAN_POINT('Ctrl Pts',(-18.032582786432,17.062512115053,122.797658849589)) ;
#27476 = CARTESIAN_POINT('Ctrl Pts',(-18.3079172569512,16.8825230346901,122.920496215202)) ;
#27477 = CARTESIAN_POINT('Ctrl Pts',(-18.1574904407852,17.0723266128218,122.571941098829)) ;
#27478 = CARTESIAN_POINT('Ctrl Pts',(-18.4078418212507,16.8923375324589,122.739922521317)) ;
#27479 = CARTESIAN_POINT('Ctrl Pts',(-18.3234861663821,17.0823949088419,122.36598619016)) ;
#27480 = CARTESIAN_POINT('Ctrl Pts',(-18.5406376345855,16.9024058284791,122.575157613041)) ;
#27481 = CARTESIAN_POINT('Ctrl Pts',(-18.5195111943069,17.0922937413247,122.194881832912)) ;
#27482 = CARTESIAN_POINT('Ctrl Pts',(-18.697456370269,16.9123046609618,122.438273670192)) ;
#27483 = CARTESIAN_POINT('Ctrl Pts',(-18.7455842875903,17.1023466213392,122.058305557914)) ;
#27484 = CARTESIAN_POINT('Ctrl Pts',(-18.878314382243,16.9223575409764,122.329011510998)) ;
#27485 = CARTESIAN_POINT('Ctrl Pts',(-18.9874629412991,17.1122164368354,121.964526142813)) ;
#27486 = CARTESIAN_POINT('Ctrl Pts',(-19.0718160746585,16.9322273564725,122.253987102022)) ;
#27487 = CARTESIAN_POINT('Ctrl Pts',(-19.2470688770235,17.1222891179182,121.913081725806)) ;
#27488 = CARTESIAN_POINT('Ctrl Pts',(-19.2795008526622,16.9423000375553,122.212830257528)) ;
#27489 = CARTESIAN_POINT('Ctrl Pts',(-19.505422587486,17.1321215964892,121.907524515032)) ;
#27490 = CARTESIAN_POINT('Ctrl Pts',(-19.4861827690057,16.9521325161263,122.208383209402)) ;
#27491 = CARTESIAN_POINT('Ctrl Pts',(-19.7660419704814,17.1421522304753,121.946947546496)) ;
#27492 = CARTESIAN_POINT('Ctrl Pts',(-19.6946785626933,16.9621631501124,122.239920201912)) ;
#27493 = CARTESIAN_POINT('Ctrl Pts',(-20.0156574864725,17.1521837876944,122.031770159067)) ;
#27494 = CARTESIAN_POINT('Ctrl Pts',(-19.8943714558458,16.9721947073315,122.307777083162)) ;
#27495 = CARTESIAN_POINT('Ctrl Pts',(-20.2423350956265,17.1620134965661,122.155604235088)) ;
#27496 = CARTESIAN_POINT('Ctrl Pts',(-20.075713330144,16.9820244162032,122.406842617996)) ;
#27497 = CARTESIAN_POINT('Ctrl Pts',(-20.4478540416198,17.1720029453682,122.318940433098)) ;
#27498 = CARTESIAN_POINT('Ctrl Pts',(-20.2401293518006,16.9920138650053,122.537510260585)) ;
#27499 = CARTESIAN_POINT('Ctrl Pts',(-20.6223297569369,17.1820467977682,122.516986010216)) ;
#27500 = CARTESIAN_POINT('Ctrl Pts',(-20.379711079171,17.0020577174053,122.69594586157)) ;
#27501 = CARTESIAN_POINT('Ctrl Pts',(-20.7571853342976,17.1918685111003,122.737058592109)) ;
#27502 = CARTESIAN_POINT('Ctrl Pts',(-20.4875963345862,17.0118794307374,122.872002271996)) ;
#27503 = CARTESIAN_POINT('Ctrl Pts',(-20.8544363834582,17.201903516089,122.982179630652)) ;
#27504 = CARTESIAN_POINT('Ctrl Pts',(-20.5653987506376,17.0219144357261,123.068098568077)) ;
#27505 = CARTESIAN_POINT('Ctrl Pts',(-20.9068811373926,17.2119283545366,123.240357855693)) ;
#27506 = CARTESIAN_POINT('Ctrl Pts',(-20.6073560524299,17.0319392741737,123.274640863138)) ;
#27507 = CARTESIAN_POINT('Ctrl Pts',(-20.9141373279082,17.2217805674918,123.499162698651)) ;
#27508 = CARTESIAN_POINT('Ctrl Pts',(-20.6131626102164,17.0417914871289,123.481683887994)) ;
#27509 = CARTESIAN_POINT('Ctrl Pts',(-20.8762617532287,17.2317705236856,123.758921385039)) ;
#27510 = CARTESIAN_POINT('Ctrl Pts',(-20.5828638652605,17.0517814433227,123.689490938947)) ;
#27511 = CARTESIAN_POINT('Ctrl Pts',(-20.7943806135892,17.2416986339689,124.006649024893)) ;
#27512 = CARTESIAN_POINT('Ctrl Pts',(-20.5173607099962,17.061709553606,123.887673192447)) ;
#27513 = CARTESIAN_POINT('Ctrl Pts',(-20.670345385213,17.2516872340484,124.237992487124)) ;
#27514 = CARTESIAN_POINT('Ctrl Pts',(-20.4181341594561,17.0716981536855,124.07274868766)) ;
#27515 = CARTESIAN_POINT('Ctrl Pts',(-20.5071235397933,17.2617138259759,124.444842800166)) ;
#27516 = CARTESIAN_POINT('Ctrl Pts',(-20.2875580171586,17.081724745613,124.23823002585)) ;
#27517 = CARTESIAN_POINT('Ctrl Pts',(-20.3134293623449,17.2715989540401,124.617932746978)) ;
#27518 = CARTESIAN_POINT('Ctrl Pts',(-20.1326042907807,17.0916098736772,124.376702907249)) ;
#27519 = CARTESIAN_POINT('Ctrl Pts',(-20.0905573668405,17.2815900715136,124.756745161351)) ;
#27520 = CARTESIAN_POINT('Ctrl Pts',(-19.9543077846783,17.1016009911507,124.487754352768)) ;
#27521 = CARTESIAN_POINT('Ctrl Pts',(-19.8455645964301,17.2916306873654,124.854716110604)) ;
#27522 = CARTESIAN_POINT('Ctrl Pts',(-19.7583141598722,17.1116416070025,124.566132786485)) ;
#27523 = CARTESIAN_POINT('Ctrl Pts',(-19.5927130154484,17.3014636782191,124.907962066392)) ;
#27524 = CARTESIAN_POINT('Ctrl Pts',(-19.5560340209557,17.1214745978562,124.60873119612)) ;
#27525 = CARTESIAN_POINT('Ctrl Pts',(-19.330277450202,17.3114568096694,124.917387511024)) ;
#27526 = CARTESIAN_POINT('Ctrl Pts',(-19.3460857391731,17.1314677293065,124.616273501047)) ;
#27527 = CARTESIAN_POINT('Ctrl Pts',(-19.0692386893252,17.3214888581048,124.88041535309)) ;
#27528 = CARTESIAN_POINT('Ctrl Pts',(-19.1372544392363,17.1414997777419,124.58669762411)) ;
#27529 = CARTESIAN_POINT('Ctrl Pts',(-18.822677257513,17.3313541046472,124.800350459875)) ;
#27530 = CARTESIAN_POINT('Ctrl Pts',(-18.9400052547958,17.1513650242843,124.522647715831)) ;
#27531 = CARTESIAN_POINT('Ctrl Pts',(-18.5911545600622,17.341315979474,124.678145049276)) ;
#27532 = CARTESIAN_POINT('Ctrl Pts',(-18.7547863323555,17.1613268991111,124.424885267182)) ;
#27533 = CARTESIAN_POINT('Ctrl Pts',(-18.38313341919,17.3513509425853,124.516091097511)) ;
#27534 = CARTESIAN_POINT('Ctrl Pts',(-18.5883681924007,17.1713618622224,124.295243637103)) ;
#27535 = CARTESIAN_POINT('Ctrl Pts',(-18.2086914290502,17.3612357870477,124.323563591818)) ;
#27536 = CARTESIAN_POINT('Ctrl Pts',(-18.4488134084025,17.1812467066848,124.1412233211)) ;
#27537 = CARTESIAN_POINT('Ctrl Pts',(-18.0678947666769,17.3713018398884,124.099676485538)) ;
#27538 = CARTESIAN_POINT('Ctrl Pts',(-18.3361743120959,17.1913127595256,123.962114606341)) ;
#27539 = CARTESIAN_POINT('Ctrl Pts',(-17.9700726313909,17.3811393557974,123.860326944384)) ;
#27540 = CARTESIAN_POINT('Ctrl Pts',(-18.2579149281125,17.2011502754345,123.770636270255)) ;
#27541 = CARTESIAN_POINT('Ctrl Pts',(-17.9137531151006,17.3912081039063,123.601841075206)) ;
#27542 = CARTESIAN_POINT('Ctrl Pts',(-18.2128572598282,17.2112190235434,123.563847905866)) ;
#27543 = CARTESIAN_POINT('Ctrl Pts',(-17.9034613928053,17.4010886209373,123.342355402501)) ;
#27544 = CARTESIAN_POINT('Ctrl Pts',(-18.2046218361467,17.2210995405744,123.356259859083)) ;
#27545 = CARTESIAN_POINT('Ctrl Pts',(-17.9382344928248,17.4110798078718,123.082149155382)) ;
#27546 = CARTESIAN_POINT('Ctrl Pts',(-18.2324382019981,17.2310907275089,123.148094673223)) ;
#27547 = CARTESIAN_POINT('Ctrl Pts',(-18.0173408799565,17.4210328741467,122.832800782693)) ;
#27548 = CARTESIAN_POINT('Ctrl Pts',(-18.2957212338474,17.2410437937838,122.948615510215)) ;
#27549 = CARTESIAN_POINT('Ctrl Pts',(-18.1395964065383,17.4310687116793,122.599142062341)) ;
#27550 = CARTESIAN_POINT('Ctrl Pts',(-18.3935237856952,17.2510796313164,122.761687546562)) ;
#27551 = CARTESIAN_POINT('Ctrl Pts',(-18.2981116221672,17.4409588378907,122.393154239559)) ;
#27552 = CARTESIAN_POINT('Ctrl Pts',(-18.5203340659042,17.2609697575279,122.596896255148)) ;
#27553 = CARTESIAN_POINT('Ctrl Pts',(-18.4916578231572,17.4509510197987,122.215719190812)) ;
#27554 = CARTESIAN_POINT('Ctrl Pts',(-18.6751695002837,17.2709619394358,122.454946675199)) ;
#27555 = CARTESIAN_POINT('Ctrl Pts',(-18.7121069676179,17.4608969597373,122.075305569039)) ;
#27556 = CARTESIAN_POINT('Ctrl Pts',(-18.8515275002128,17.2809078793744,122.342614056364)) ;
#27557 = CARTESIAN_POINT('Ctrl Pts',(-18.9534274542707,17.4708441435014,121.974794440461)) ;
#27558 = CARTESIAN_POINT('Ctrl Pts',(-19.0445828970662,17.2908550631385,122.262203186491)) ;
#27559 = CARTESIAN_POINT('Ctrl Pts',(-19.211160386698,17.4808920818088,121.917426601221)) ;
#27560 = CARTESIAN_POINT('Ctrl Pts',(-19.2507687776007,17.300903001446,122.216306788302)) ;
#27561 = CARTESIAN_POINT('Ctrl Pts',(-19.4696824314095,17.4907397165491,121.905695967141)) ;
#27562 = CARTESIAN_POINT('Ctrl Pts',(-19.4575859964064,17.3107506361862,122.206920105047)) ;
#27563 = CARTESIAN_POINT('Ctrl Pts',(-19.7293772423961,17.5007014305229,121.938602055784)) ;
#27564 = CARTESIAN_POINT('Ctrl Pts',(-19.6653420282454,17.3207123501601,122.233242742379)) ;
#27565 = CARTESIAN_POINT('Ctrl Pts',(-19.9810217545707,17.5107300653138,122.016948020053)) ;
#27566 = CARTESIAN_POINT('Ctrl Pts',(-19.8666582637803,17.3307409849509,122.295917385593)) ;
#27567 = CARTESIAN_POINT('Ctrl Pts',(-20.2124907996332,17.5206403839109,122.136283881726)) ;
#27568 = CARTESIAN_POINT('Ctrl Pts',(-20.0518343705786,17.340651303548,122.391384019584)) ;
#27569 = CARTESIAN_POINT('Ctrl Pts',(-20.4206686080383,17.5305752402224,122.293854796919)) ;
#27570 = CARTESIAN_POINT('Ctrl Pts',(-20.2183778909395,17.3505861598595,122.517438895075)) ;
#27571 = CARTESIAN_POINT('Ctrl Pts',(-20.6000255828736,17.5406164761831,122.487384162176)) ;
#27572 = CARTESIAN_POINT('Ctrl Pts',(-20.3618650889074,17.3606273958202,122.672260836499)) ;
#27573 = CARTESIAN_POINT('Ctrl Pts',(-20.7410561133952,17.5505032477631,122.70562002418)) ;
#27574 = CARTESIAN_POINT('Ctrl Pts',(-20.4746913307344,17.3705141674002,122.846848200213)) ;
#27575 = CARTESIAN_POINT('Ctrl Pts',(-20.8434772707178,17.5605034264693,122.947591960567)) ;
#27576 = CARTESIAN_POINT('Ctrl Pts',(-20.5566303111727,17.3805143461064,123.040424818321)) ;
#27577 = CARTESIAN_POINT('Ctrl Pts',(-20.9020786278622,17.5704207046789,123.201578349681)) ;
#27578 = CARTESIAN_POINT('Ctrl Pts',(-20.6035135750036,17.390431624316,123.24361335474)) ;
#27579 = CARTESIAN_POINT('Ctrl Pts',(-20.91578288945,17.5804679510926,123.465216930615)) ;
#27580 = CARTESIAN_POINT('Ctrl Pts',(-20.6144792336198,17.4004788707297,123.454524044763)) ;
#27581 = CARTESIAN_POINT('Ctrl Pts',(-20.8843256015444,17.5903418400739,123.722819361991)) ;
#27582 = CARTESIAN_POINT('Ctrl Pts',(-20.5893156441907,17.410352759711,123.660606216813)) ;
#27583 = CARTESIAN_POINT('Ctrl Pts',(-20.8073356878369,17.6004038576544,123.975747950634)) ;
#27584 = CARTESIAN_POINT('Ctrl Pts',(-20.527725890698,17.4204147772915,123.862949679042)) ;
#27585 = CARTESIAN_POINT('Ctrl Pts',(-20.6898154915697,17.6102749193887,124.207021563565)) ;
#27586 = CARTESIAN_POINT('Ctrl Pts',(-20.4337117468578,17.4302858390258,124.047969580495)) ;
#27587 = CARTESIAN_POINT('Ctrl Pts',(-20.5325789116341,17.620268982749,124.417385133982)) ;
#27588 = CARTESIAN_POINT('Ctrl Pts',(-20.307924299848,17.4402799023861,124.216261749645)) ;
#27589 = CARTESIAN_POINT('Ctrl Pts',(-20.3400800616733,17.6303011407824,124.597505830153)) ;
#27590 = CARTESIAN_POINT('Ctrl Pts',(-20.1539268192864,17.4503120604195,124.360359893607)) ;
#27591 = CARTESIAN_POINT('Ctrl Pts',(-20.1232165512678,17.6401650170226,124.739545873156)) ;
#27592 = CARTESIAN_POINT('Ctrl Pts',(-19.9804371926355,17.4601759366597,124.473993837202)) ;
#27593 = CARTESIAN_POINT('Ctrl Pts',(-19.8800594521067,17.6502355316608,124.843920027478)) ;
#27594 = CARTESIAN_POINT('Ctrl Pts',(-19.7859124646786,17.470246451298,124.557495161762)) ;
#27595 = CARTESIAN_POINT('Ctrl Pts',(-19.6283095577294,17.6600761686018,124.90314183829)) ;
#27596 = CARTESIAN_POINT('Ctrl Pts',(-19.5845130945949,17.4800870882389,124.60487484599)) ;
#27597 = CARTESIAN_POINT('Ctrl Pts',(-19.366875274711,17.670043297442,124.918801259543)) ;
#27598 = CARTESIAN_POINT('Ctrl Pts',(-19.375365146763,17.4900542170791,124.61740447096)) ;
#27599 = CARTESIAN_POINT('Ctrl Pts',(-19.1054626465016,17.6800572705665,124.888408905222)) ;
#27600 = CARTESIAN_POINT('Ctrl Pts',(-19.1662371963715,17.5000681902037,124.593093168698)) ;
#27601 = CARTESIAN_POINT('Ctrl Pts',(-18.7709105569482,17.6933420044298,124.788587304081)) ;
#27602 = CARTESIAN_POINT('Ctrl Pts',(-18.8985830635496,17.5133529240669,124.513236786793)) ;
#27603 = CARTESIAN_POINT('Ctrl Pts',(-18.4713115759659,17.7065672691446,124.604860086354)) ;
#27604 = CARTESIAN_POINT('Ctrl Pts',(-18.6588815387832,17.5265781887817,124.36623312436)) ;
#27605 = CARTESIAN_POINT('Ctrl Pts',(-18.23024753484,17.7198777916994,124.351352544017)) ;
#27606 = CARTESIAN_POINT('Ctrl Pts',(-18.4660643742217,17.5398887113366,124.163459835131)) ;
#27607 = CARTESIAN_POINT('Ctrl Pts',(-18.0847456433107,17.7299064366016,124.131627885447)) ;
#27608 = CARTESIAN_POINT('Ctrl Pts',(-18.3496538990184,17.5499173562387,123.987675132136)) ;
#27609 = CARTESIAN_POINT('Ctrl Pts',(-17.9809344252587,17.7397874689555,123.893612632043)) ;
#27610 = CARTESIAN_POINT('Ctrl Pts',(-18.2666046634578,17.5597983885926,123.797265517451)) ;
#27611 = CARTESIAN_POINT('Ctrl Pts',(-17.9188829813947,17.7497684416356,123.638771587196)) ;
#27612 = CARTESIAN_POINT('Ctrl Pts',(-18.2169614863476,17.5697793612727,123.593391459913)) ;
#27613 = CARTESIAN_POINT('Ctrl Pts',(-17.9022490540845,17.7597495692216,123.377020959202)) ;
#27614 = CARTESIAN_POINT('Ctrl Pts',(-18.2036504220169,17.5797604888587,123.383995815664)) ;
#27615 = CARTESIAN_POINT('Ctrl Pts',(-17.940086062115,17.772992759483,123.030998917188)) ;
#27616 = CARTESIAN_POINT('Ctrl Pts',(-18.233927074126,17.5930036791201,123.10715455913)) ;
#27617 = CARTESIAN_POINT('Ctrl Pts',(-18.1006895820262,17.7896607548438,122.618237447441)) ;
#27618 = CARTESIAN_POINT('Ctrl Pts',(-18.3623849444853,17.6096716744809,122.776980015619)) ;
#27619 = CARTESIAN_POINT('Ctrl Pts',(-18.3897812209932,17.8061812548558,122.28765824502)) ;
#27620 = CARTESIAN_POINT('Ctrl Pts',(-18.5937018866241,17.626192174493,122.512467686169)) ;
#27621 = CARTESIAN_POINT('Ctrl Pts',(-18.6800705190158,17.8194942711718,122.092466331838)) ;
#27622 = CARTESIAN_POINT('Ctrl Pts',(-18.8258934626634,17.639505190809,122.356347530936)) ;
#27623 = CARTESIAN_POINT('Ctrl Pts',(-18.9181973224567,17.8294108294048,121.986503440751)) ;
#27624 = CARTESIAN_POINT('Ctrl Pts',(-19.016402860702,17.649421749042,122.271568344734)) ;
#27625 = CARTESIAN_POINT('Ctrl Pts',(-19.1738622433935,17.8394384977077,121.92290647105)) ;
#27626 = CARTESIAN_POINT('Ctrl Pts',(-19.2209295533305,17.6594494173448,122.220690413991)) ;
#27627 = CARTESIAN_POINT('Ctrl Pts',(-19.5194723945054,17.8526190874524,121.898080551952)) ;
#27628 = CARTESIAN_POINT('Ctrl Pts',(-19.4974317792493,17.6726300070895,122.200829004453)) ;
#27629 = CARTESIAN_POINT('Ctrl Pts',(-19.9563231936178,17.8693672265717,121.982455382444)) ;
#27630 = CARTESIAN_POINT('Ctrl Pts',(-19.8468977311799,17.6893781462089,122.268323444308)) ;
#27631 = CARTESIAN_POINT('Ctrl Pts',(-20.4081951552472,17.8891619690823,122.252387033747)) ;
#27632 = CARTESIAN_POINT('Ctrl Pts',(-20.2084028189433,17.7091728887194,122.484267129473)) ;
#27633 = CARTESIAN_POINT('Ctrl Pts',(-20.7451718132866,17.9092063618911,122.66478304066)) ;
#27634 = CARTESIAN_POINT('Ctrl Pts',(-20.4779852136411,17.7292172815282,122.814181443718)) ;
#27635 = CARTESIAN_POINT('Ctrl Pts',(-20.9190608630453,17.9290455441898,123.162728597956)) ;
#27636 = CARTESIAN_POINT('Ctrl Pts',(-20.6171002151294,17.7490564638269,123.212537829593)) ;
#27637 = CARTESIAN_POINT('Ctrl Pts',(-20.9138698455996,17.9489708678827,123.692157121899)) ;
#27638 = CARTESIAN_POINT('Ctrl Pts',(-20.6129501230136,17.7689817875198,123.636081264938)) ;
#27639 = CARTESIAN_POINT('Ctrl Pts',(-20.7282004987486,17.9688945059342,124.188169695646)) ;
#27640 = CARTESIAN_POINT('Ctrl Pts',(-20.4644169876035,17.7889054255713,124.032892793635)) ;
#27641 = CARTESIAN_POINT('Ctrl Pts',(-20.3846133570625,17.9888193793997,124.591069561661)) ;
#27642 = CARTESIAN_POINT('Ctrl Pts',(-20.1895487840061,17.8088302990368,124.355214802049)) ;
#27643 = CARTESIAN_POINT('Ctrl Pts',(-19.9254924402877,18.0086979864787,124.852574068712)) ;
#27644 = CARTESIAN_POINT('Ctrl Pts',(-19.8222521396401,17.8287089061158,124.564420818094)) ;
#27645 = CARTESIAN_POINT('Ctrl Pts',(-19.4021887856867,18.0286754293106,124.94239921452)) ;
#27646 = CARTESIAN_POINT('Ctrl Pts',(-19.403609335955,17.8486863489478,124.636282835405)) ;
#27647 = CARTESIAN_POINT('Ctrl Pts',(-18.8808448567372,18.0486072773953,124.848094480769)) ;
#27648 = CARTESIAN_POINT('Ctrl Pts',(-18.9865332449473,17.8686181970324,124.560840796153)) ;
#27649 = CARTESIAN_POINT('Ctrl Pts',(-18.4236271458194,18.0685025457379,124.582520931676)) ;
#27650 = CARTESIAN_POINT('Ctrl Pts',(-18.620757360624,17.888513465375,124.348382725567)) ;
#27651 = CARTESIAN_POINT('Ctrl Pts',(-18.083533966346,18.08842504415,124.176653707817)) ;
#27652 = CARTESIAN_POINT('Ctrl Pts',(-18.3486814135184,17.9084359637871,124.023689002201)) ;
#27653 = CARTESIAN_POINT('Ctrl Pts',(-17.9021445000866,18.108384526026,123.678105539859)) ;
#27654 = CARTESIAN_POINT('Ctrl Pts',(-18.2035687540983,17.9283954456631,123.624850383669)) ;
#27655 = CARTESIAN_POINT('Ctrl Pts',(-17.901677043034,18.1282622784854,123.149870596743)) ;
#27656 = CARTESIAN_POINT('Ctrl Pts',(-18.2031940192158,17.9482731981225,123.202260912629)) ;
#27657 = CARTESIAN_POINT('Ctrl Pts',(-18.0801792550787,18.1481440692199,122.65239779122)) ;
#27658 = CARTESIAN_POINT('Ctrl Pts',(-18.3459964494123,17.9681549888571,122.804281306169)) ;
#27659 = CARTESIAN_POINT('Ctrl Pts',(-18.4216843162061,18.1682174080709,122.242598944837)) ;
#27660 = CARTESIAN_POINT('Ctrl Pts',(-18.6191997939776,17.988228327708,122.476442865587)) ;
#27661 = CARTESIAN_POINT('Ctrl Pts',(-18.8764446818162,18.1880218753067,121.977323375824)) ;
#27662 = CARTESIAN_POINT('Ctrl Pts',(-18.983010300815,18.0080327949438,122.26422127326)) ;
#27663 = CARTESIAN_POINT('Ctrl Pts',(-19.3987200282656,18.2080052157145,121.881178045719)) ;
#27664 = CARTESIAN_POINT('Ctrl Pts',(-19.4008309101687,18.0280161353516,122.187305861256)) ;
#27665 = CARTESIAN_POINT('Ctrl Pts',(-19.9205934708167,18.2279201803125,121.969578565073)) ;
#27666 = CARTESIAN_POINT('Ctrl Pts',(-19.8183305317221,18.0479310999496,122.258027130134)) ;
#27667 = CARTESIAN_POINT('Ctrl Pts',(-20.3807158505364,18.2477887150289,122.228912632756)) ;
#27668 = CARTESIAN_POINT('Ctrl Pts',(-20.1864289023512,18.067799634666,122.465496375139)) ;
#27669 = CARTESIAN_POINT('Ctrl Pts',(-20.7270809482803,18.2678410992406,122.6337729235)) ;
#27670 = CARTESIAN_POINT('Ctrl Pts',(-20.4635196475679,18.0878520188777,122.789385098956)) ;
#27671 = CARTESIAN_POINT('Ctrl Pts',(-20.9126860426018,18.2876150630298,123.125692137824)) ;
#27672 = CARTESIAN_POINT('Ctrl Pts',(-20.6120028561782,18.1076259826669,123.182923161825)) ;
#27673 = CARTESIAN_POINT('Ctrl Pts',(-20.919787056096,18.3076694420512,123.658444810698)) ;
#27674 = CARTESIAN_POINT('Ctrl Pts',(-20.6176815610967,18.1276803616883,123.609124837985)) ;
#27675 = CARTESIAN_POINT('Ctrl Pts',(-20.7465962162573,18.3274661796244,124.155452562203)) ;
#27676 = CARTESIAN_POINT('Ctrl Pts',(-20.4791262659657,18.1474770992615,124.006732040671)) ;
#27677 = CARTESIAN_POINT('Ctrl Pts',(-20.4126446942546,18.3474339919759,124.567768827108)) ;
#27678 = CARTESIAN_POINT('Ctrl Pts',(-20.2119627251939,18.167444911613,124.336583477204)) ;
#27679 = CARTESIAN_POINT('Ctrl Pts',(-19.9576212451287,18.3673929680409,124.840656736435)) ;
#27680 = CARTESIAN_POINT('Ctrl Pts',(-19.8479423832508,18.187403887678,124.554891689415)) ;
#27681 = CARTESIAN_POINT('Ctrl Pts',(-19.4386451944303,18.3872878863183,124.941871042673)) ;
#27682 = CARTESIAN_POINT('Ctrl Pts',(-19.4327602304496,18.2072988059554,124.635860461353)) ;
#27683 = CARTESIAN_POINT('Ctrl Pts',(-18.9161726453232,18.4071841987686,124.860555263088)) ;
#27684 = CARTESIAN_POINT('Ctrl Pts',(-19.0147819951874,18.2271951184057,124.570804600373)) ;
#27685 = CARTESIAN_POINT('Ctrl Pts',(-18.4521815633956,18.4270921321427,124.606153931591)) ;
#27686 = CARTESIAN_POINT('Ctrl Pts',(-18.6435902854391,18.2471030517799,124.367280294003)) ;
#27687 = CARTESIAN_POINT('Ctrl Pts',(-18.1022181077,18.4470420224312,124.207874213592)) ;
#27688 = CARTESIAN_POINT('Ctrl Pts',(-18.3636220163142,18.2670529420683,124.048653992795)) ;
#27689 = CARTESIAN_POINT('Ctrl Pts',(-17.9093397630461,18.4669192529325,123.715982843254)) ;
#27690 = CARTESIAN_POINT('Ctrl Pts',(-18.2093224069639,18.2869301725696,123.655139058645)) ;
#27691 = CARTESIAN_POINT('Ctrl Pts',(-17.8955552161801,18.4869019218035,123.185081472576)) ;
#27692 = CARTESIAN_POINT('Ctrl Pts',(-18.1982991666636,18.3069128414406,123.230417568849)) ;
#27693 = CARTESIAN_POINT('Ctrl Pts',(-18.0637189576036,18.5068348083839,122.682625101242)) ;
#27694 = CARTESIAN_POINT('Ctrl Pts',(-18.3328317622398,18.326845728021,122.82845440733)) ;
#27695 = CARTESIAN_POINT('Ctrl Pts',(-18.3925705510188,18.5267475544018,122.267998602716)) ;
#27696 = CARTESIAN_POINT('Ctrl Pts',(-18.5959242479568,18.3467584740389,122.496751834392)) ;
#27697 = CARTESIAN_POINT('Ctrl Pts',(-18.767281881698,18.5433172757436,122.036622749478)) ;
#27698 = CARTESIAN_POINT('Ctrl Pts',(-18.8956708387233,18.3633281953808,122.311665074245)) ;
#27699 = CARTESIAN_POINT('Ctrl Pts',(-19.1020056145289,18.5566172870486,121.936011376313)) ;
#27700 = CARTESIAN_POINT('Ctrl Pts',(-19.1634797346767,18.3766282066857,122.231169157369)) ;
#27701 = CARTESIAN_POINT('Ctrl Pts',(-19.4482877506077,18.5698874747985,121.89465138511)) ;
#27702 = CARTESIAN_POINT('Ctrl Pts',(-19.4404490281102,18.3898983944356,122.198083477283)) ;
#27703 = CARTESIAN_POINT('Ctrl Pts',(-19.8857560482088,18.5865148571639,121.957313792384)) ;
#27704 = CARTESIAN_POINT('Ctrl Pts',(-19.7904920476466,18.406525776801,122.248222840253)) ;
#27705 = CARTESIAN_POINT('Ctrl Pts',(-20.2753787251303,18.6031371469091,122.165595250357)) ;
#27706 = CARTESIAN_POINT('Ctrl Pts',(-20.1021439506729,18.4231480665462,122.414835475618)) ;
#27707 = CARTESIAN_POINT('Ctrl Pts',(-20.5295847929134,18.6163823613036,122.403352527217)) ;
#27708 = CARTESIAN_POINT('Ctrl Pts',(-20.3055329796882,18.4363932809408,122.60505706455)) ;
#27709 = CARTESIAN_POINT('Ctrl Pts',(-20.6866624263127,18.6262943262643,122.611158628173)) ;
#27710 = CARTESIAN_POINT('Ctrl Pts',(-20.4311881581819,18.4463052459014,122.771300643665)) ;
#27711 = CARTESIAN_POINT('Ctrl Pts',(-20.8067318368115,18.6363529494288,122.846612050245)) ;
#27712 = CARTESIAN_POINT('Ctrl Pts',(-20.5272430699789,18.4563638690659,122.959664983458)) ;
#27713 = CARTESIAN_POINT('Ctrl Pts',(-20.882799746978,18.6461930635446,123.093798587262)) ;
#27714 = CARTESIAN_POINT('Ctrl Pts',(-20.5880949652043,18.4662039831817,123.157414861851)) ;
#27715 = CARTESIAN_POINT('Ctrl Pts',(-20.9157793856879,18.6562588485022,123.356213554678)) ;
#27716 = CARTESIAN_POINT('Ctrl Pts',(-20.6144765429298,18.4762697681393,123.367347025587)) ;
#27717 = CARTESIAN_POINT('Ctrl Pts',(-20.9028157443252,18.6661421662901,123.615646798569)) ;
#27718 = CARTESIAN_POINT('Ctrl Pts',(-20.6041033763825,18.4861530859272,123.574893593804)) ;
#27719 = CARTESIAN_POINT('Ctrl Pts',(-20.8449533316139,18.6761316041487,123.871675964814)) ;
#27720 = CARTESIAN_POINT('Ctrl Pts',(-20.5578112681338,18.4961425237858,123.779716386074)) ;
#27721 = CARTESIAN_POINT('Ctrl Pts',(-20.7436744284095,18.6860953182014,124.113145006398)) ;
#27722 = CARTESIAN_POINT('Ctrl Pts',(-20.4767860825283,18.5061062378385,123.972890731368)) ;
#27723 = CARTESIAN_POINT('Ctrl Pts',(-20.6017905558508,18.6960903298606,124.334207674781)) ;
#27724 = CARTESIAN_POINT('Ctrl Pts',(-20.3632771185327,18.5161012494978,124.149739604004)) ;
#27725 = CARTESIAN_POINT('Ctrl Pts',(-20.4226612590053,18.7061266215549,124.527770408748)) ;
#27726 = CARTESIAN_POINT('Ctrl Pts',(-20.2199720814813,18.526137541192,124.304588217699)) ;
#27727 = CARTESIAN_POINT('Ctrl Pts',(-20.2168518529892,18.7159729992483,124.684624557531)) ;
#27728 = CARTESIAN_POINT('Ctrl Pts',(-20.0553231661172,18.5359839188854,124.430069764472)) ;
#27729 = CARTESIAN_POINT('Ctrl Pts',(-19.9839760536042,18.725957943399,124.805452933041)) ;
#27730 = CARTESIAN_POINT('Ctrl Pts',(-19.8690215418316,18.5459688630361,124.526730426201)) ;
#27731 = CARTESIAN_POINT('Ctrl Pts',(-19.7348307743134,18.735894914529,124.883803103654)) ;
#27732 = CARTESIAN_POINT('Ctrl Pts',(-19.6697046968684,18.5559058341661,124.589408393291)) ;
#27733 = CARTESIAN_POINT('Ctrl Pts',(-19.4729748038764,18.7459446991607,124.917940423187)) ;
#27734 = CARTESIAN_POINT('Ctrl Pts',(-19.4602196750584,18.5659556187978,124.616716001048)) ;
#27735 = CARTESIAN_POINT('Ctrl Pts',(-19.21434799551,18.7557951612382,124.906522324717)) ;
#27736 = CARTESIAN_POINT('Ctrl Pts',(-19.2533184225446,18.5758060808753,124.607579270633)) ;
#27737 = CARTESIAN_POINT('Ctrl Pts',(-18.9584174462669,18.7657671747586,124.850357148989)) ;
#27738 = CARTESIAN_POINT('Ctrl Pts',(-19.0485745563845,18.5857780943957,124.562644952603)) ;
#27739 = CARTESIAN_POINT('Ctrl Pts',(-18.7155078312172,18.775762321878,124.750315034863)) ;
#27740 = CARTESIAN_POINT('Ctrl Pts',(-18.8542477777451,18.5957732415151,124.48260921036)) ;
#27741 = CARTESIAN_POINT('Ctrl Pts',(-18.493022848757,18.7857962916141,124.608834245128)) ;
#27742 = CARTESIAN_POINT('Ctrl Pts',(-18.6762610286674,18.6058072112512,124.369422690082)) ;
#27743 = CARTESIAN_POINT('Ctrl Pts',(-18.3016334315015,18.7956518372847,124.434305714712)) ;
#27744 = CARTESIAN_POINT('Ctrl Pts',(-18.5231511449158,18.6156627569218,124.229798335907)) ;
#27745 = CARTESIAN_POINT('Ctrl Pts',(-18.140904940295,18.8056505942979,124.226495189743)) ;
#27746 = CARTESIAN_POINT('Ctrl Pts',(-18.394570163324,18.6256615139351,124.063548607924)) ;
#27747 = CARTESIAN_POINT('Ctrl Pts',(-18.019684455447,18.8155477295351,123.99634137885)) ;
#27748 = CARTESIAN_POINT('Ctrl Pts',(-18.2975958304662,18.6355586491722,123.87942470902)) ;
#27749 = CARTESIAN_POINT('Ctrl Pts',(-17.93899129175,18.8256008253747,123.744810345997)) ;
#27750 = CARTESIAN_POINT('Ctrl Pts',(-18.2330434068114,18.6456117450119,123.678199198287)) ;
#27751 = CARTESIAN_POINT('Ctrl Pts',(-17.9037702162779,18.8354843341053,123.487463211661)) ;
#27752 = CARTESIAN_POINT('Ctrl Pts',(-18.2048687720169,18.6554952537425,123.472321440138)) ;
#27753 = CARTESIAN_POINT('Ctrl Pts',(-17.9132654845491,18.8454792067514,123.224988077224)) ;
#27754 = CARTESIAN_POINT('Ctrl Pts',(-18.2124671563329,18.6654901263886,123.262341496769)) ;
#27755 = CARTESIAN_POINT('Ctrl Pts',(-17.9687343278623,18.8554991683871,122.967567757792)) ;
#27756 = CARTESIAN_POINT('Ctrl Pts',(-18.2568443761274,18.6755100880243,123.056405729243)) ;
#27757 = CARTESIAN_POINT('Ctrl Pts',(-18.0667115840973,18.865404532187,122.726412358638)) ;
#27758 = CARTESIAN_POINT('Ctrl Pts',(-18.3352281137652,18.6854154518241,122.863482464888)) ;
#27759 = CARTESIAN_POINT('Ctrl Pts',(-18.2051056278125,18.8753451197945,122.504876382137)) ;
#27760 = CARTESIAN_POINT('Ctrl Pts',(-18.4459450547457,18.6953560394316,122.68625500378)) ;
#27761 = CARTESIAN_POINT('Ctrl Pts',(-18.3808775940096,18.8853479378952,122.309383985207)) ;
#27762 = CARTESIAN_POINT('Ctrl Pts',(-18.5865641665979,18.7053588575323,122.529862558861)) ;
#27763 = CARTESIAN_POINT('Ctrl Pts',(-18.5888129419843,18.8953826496193,122.147230647452)) ;
#27764 = CARTESIAN_POINT('Ctrl Pts',(-18.7529137900349,18.7153935692564,122.40014159165)) ;
#27765 = CARTESIAN_POINT('Ctrl Pts',(-18.8171608789422,18.9052275563566,122.025580674038)) ;
#27766 = CARTESIAN_POINT('Ctrl Pts',(-18.9355927397188,18.7252384759937,122.302823704996)) ;
#27767 = CARTESIAN_POINT('Ctrl Pts',(-19.066475495053,18.9152134089256,121.943828689904)) ;
#27768 = CARTESIAN_POINT('Ctrl Pts',(-19.1350449591221,18.7352243285627,122.237424137714)) ;
#27769 = CARTESIAN_POINT('Ctrl Pts',(-19.3249330398174,18.9251482173387,121.906600838846)) ;
#27770 = CARTESIAN_POINT('Ctrl Pts',(-19.3418110288155,18.7451591369758,122.207643930442)) ;
#27771 = CARTESIAN_POINT('Ctrl Pts',(-19.5890580305708,18.9352057444197,121.915149697282)) ;
#27772 = CARTESIAN_POINT('Ctrl Pts',(-19.5531110478041,18.7552166640568,122.214485107576)) ;
#27773 = CARTESIAN_POINT('Ctrl Pts',(-19.8417664438443,18.9450273994168,121.967782613312)) ;
#27774 = CARTESIAN_POINT('Ctrl Pts',(-19.7552767463782,18.7650383190539,122.256593308813)) ;
#27775 = CARTESIAN_POINT('Ctrl Pts',(-20.0873540689241,18.9550834435898,122.065301218056)) ;
#27776 = CARTESIAN_POINT('Ctrl Pts',(-19.9517461977428,18.775094363227,122.334610067724)) ;
#27777 = CARTESIAN_POINT('Ctrl Pts',(-20.3094798342934,18.965024183635,122.20280861514)) ;
#27778 = CARTESIAN_POINT('Ctrl Pts',(-20.1294455077566,18.7850351032721,122.444617579698)) ;
#27779 = CARTESIAN_POINT('Ctrl Pts',(-20.5041752042223,18.9749283047079,122.375539516404)) ;
#27780 = CARTESIAN_POINT('Ctrl Pts',(-20.2852002006892,18.794939224345,122.582803465436)) ;
#27781 = CARTESIAN_POINT('Ctrl Pts',(-20.6681231446912,18.9849758458621,122.58248803559)) ;
#27782 = CARTESIAN_POINT('Ctrl Pts',(-20.416357069613,18.8049867654992,122.748363557921)) ;
#27783 = CARTESIAN_POINT('Ctrl Pts',(-20.7919825435621,18.9948745974625,122.811275811282)) ;
#27784 = CARTESIAN_POINT('Ctrl Pts',(-20.5154426771701,18.8148855170996,122.931394296776)) ;
#27785 = CARTESIAN_POINT('Ctrl Pts',(-20.8755683816824,19.0049230764283,123.061730492506)) ;
#27786 = CARTESIAN_POINT('Ctrl Pts',(-20.5823095619046,18.8249339960654,123.131758740942)) ;
#27787 = CARTESIAN_POINT('Ctrl Pts',(-20.9138033739238,19.014810573512,123.318762800787)) ;
#27788 = CARTESIAN_POINT('Ctrl Pts',(-20.612895591588,18.8348214931492,123.33738436397)) ;
#27789 = CARTESIAN_POINT('Ctrl Pts',(-20.9072423074913,19.0248036638101,123.581265757207)) ;
#27790 = CARTESIAN_POINT('Ctrl Pts',(-20.6076449012029,18.8448145834472,123.547386559869)) ;
#27791 = CARTESIAN_POINT('Ctrl Pts',(-20.8553184944048,19.0347558338704,123.837608299615)) ;
#27792 = CARTESIAN_POINT('Ctrl Pts',(-20.5661040904152,18.8547667535075,123.752459944652)) ;
#27793 = CARTESIAN_POINT('Ctrl Pts',(-20.7601517684657,19.0446942537849,124.080804362951)) ;
#27794 = CARTESIAN_POINT('Ctrl Pts',(-20.4899691655713,18.864705173422,123.947015810628)) ;
#27795 = CARTESIAN_POINT('Ctrl Pts',(-20.6237942335491,19.0546793838705,124.305021774752)) ;
#27796 = CARTESIAN_POINT('Ctrl Pts',(-20.3808817246997,18.8746903035076,124.126388699509)) ;
#27797 = CARTESIAN_POINT('Ctrl Pts',(-20.4494165139908,19.0647160732846,124.502884010772)) ;
#27798 = CARTESIAN_POINT('Ctrl Pts',(-20.2413781403973,18.8847269929217,124.284677342677)) ;
#27799 = CARTESIAN_POINT('Ctrl Pts',(-20.2472957009717,19.0745707572771,124.664826057112)) ;
#27800 = CARTESIAN_POINT('Ctrl Pts',(-20.0796809747905,18.8945816769142,124.414229158598)) ;
#27801 = CARTESIAN_POINT('Ctrl Pts',(-20.0170234288064,19.0845702413249,124.791326058903)) ;
#27802 = CARTESIAN_POINT('Ctrl Pts',(-19.8954624401579,18.9045811609621,124.515427632247)) ;
#27803 = CARTESIAN_POINT('Ctrl Pts',(-19.7708869846679,19.0944653301018,124.875329679388)) ;
#27804 = CARTESIAN_POINT('Ctrl Pts',(-19.6985533150144,18.914476249739,124.582628795942)) ;
#27805 = CARTESIAN_POINT('Ctrl Pts',(-19.5096800897201,19.104525884748,124.915950078661)) ;
#27806 = CARTESIAN_POINT('Ctrl Pts',(-19.4895873565871,18.9245368043851,124.61512352611)) ;
#27807 = CARTESIAN_POINT('Ctrl Pts',(-19.2508813050788,19.1143751491209,124.910856545189)) ;
#27808 = CARTESIAN_POINT('Ctrl Pts',(-19.2825491948916,18.934386068758,124.611047106101)) ;
#27809 = CARTESIAN_POINT('Ctrl Pts',(-18.99220707569,19.1244024015687,124.86066175785)) ;
#27810 = CARTESIAN_POINT('Ctrl Pts',(-19.0756100641405,18.9444133212059,124.570889813033)) ;
#27811 = CARTESIAN_POINT('Ctrl Pts',(-18.7463833099064,19.1344306991389,124.765652294078)) ;
#27812 = CARTESIAN_POINT('Ctrl Pts',(-18.8789515818906,18.954441618776,124.49488071212)) ;
#27813 = CARTESIAN_POINT('Ctrl Pts',(-18.5246504442198,19.1442768281449,124.632315524006)) ;
#27814 = CARTESIAN_POINT('Ctrl Pts',(-18.7015668443456,18.964287747782,124.388210457223)) ;
#27815 = CARTESIAN_POINT('Ctrl Pts',(-18.3260692253604,19.154270733507,124.460445802928)) ;
#27816 = CARTESIAN_POINT('Ctrl Pts',(-18.54270288402,18.9742816531441,124.250713721188)) ;
#27817 = CARTESIAN_POINT('Ctrl Pts',(-18.1602075359614,19.16429483119,124.255787351941)) ;
#27818 = CARTESIAN_POINT('Ctrl Pts',(-18.4100146618778,18.9843057508271,124.0869859934)) ;
#27819 = CARTESIAN_POINT('Ctrl Pts',(-18.0338280399953,19.174184659044,124.028684394348)) ;
#27820 = CARTESIAN_POINT('Ctrl Pts',(-18.3089126375273,18.9941955786812,123.905303536338)) ;
#27821 = CARTESIAN_POINT('Ctrl Pts',(-17.947565914458,19.1841766404745,123.780690475578)) ;
#27822 = CARTESIAN_POINT('Ctrl Pts',(-18.2399042544237,19.0041875601116,123.706908101772)) ;
#27823 = CARTESIAN_POINT('Ctrl Pts',(-17.9059220811503,19.1941236452403,123.522631607328)) ;
#27824 = CARTESIAN_POINT('Ctrl Pts',(-18.2065905909474,19.0141345648774,123.500461190172)) ;
#27825 = CARTESIAN_POINT('Ctrl Pts',(-17.9092390395663,19.2040732966301,123.261175270493)) ;
#27826 = CARTESIAN_POINT('Ctrl Pts',(-18.2092454041741,19.0240842162672,123.291296521161)) ;
#27827 = CARTESIAN_POINT('Ctrl Pts',(-17.958538306793,19.2141102996075,123.002069408009)) ;
#27828 = CARTESIAN_POINT('Ctrl Pts',(-18.2486861142578,19.0341212192446,123.084011970538)) ;
#27829 = CARTESIAN_POINT('Ctrl Pts',(-18.0505326598567,19.2239992080425,122.759016798404)) ;
#27830 = CARTESIAN_POINT('Ctrl Pts',(-18.3222825144302,19.0440101276797,122.88957101701)) ;
#27831 = CARTESIAN_POINT('Ctrl Pts',(-18.1842635126106,19.23398854052,122.533132432072)) ;
#27832 = CARTESIAN_POINT('Ctrl Pts',(-18.429268104139,19.0539994601571,122.708864261039)) ;
#27833 = CARTESIAN_POINT('Ctrl Pts',(-18.3548053010277,19.2439470959571,122.334641591459)) ;
#27834 = CARTESIAN_POINT('Ctrl Pts',(-18.5657022198966,19.0639580155942,122.550072634139)) ;
#27835 = CARTESIAN_POINT('Ctrl Pts',(-18.5556335270977,19.2538466671576,122.169248739393)) ;
#27836 = CARTESIAN_POINT('Ctrl Pts',(-18.7263649283418,19.0738575867947,122.417759614696)) ;
#27837 = CARTESIAN_POINT('Ctrl Pts',(-18.7855306745994,19.2638945924096,122.039423510114)) ;
#27838 = CARTESIAN_POINT('Ctrl Pts',(-18.910283328349,19.0839055120467,122.313900283675)) ;
#27839 = CARTESIAN_POINT('Ctrl Pts',(-19.0306926009335,19.2737898919356,121.952607002251)) ;
#27840 = CARTESIAN_POINT('Ctrl Pts',(-19.1064125243075,19.0938008115727,122.244448292274)) ;
#27841 = CARTESIAN_POINT('Ctrl Pts',(-19.2914444276105,19.2838517483836,121.908933829335)) ;
#27842 = CARTESIAN_POINT('Ctrl Pts',(-19.3150144124183,19.1038626680207,122.209510720343)) ;
#27843 = CARTESIAN_POINT('Ctrl Pts',(-19.5501343610573,19.2936955948002,121.911097613413)) ;
#27844 = CARTESIAN_POINT('Ctrl Pts',(-19.5219652921603,19.1137065144373,122.211242751695)) ;
#27845 = CARTESIAN_POINT('Ctrl Pts',(-19.8077343935755,19.3036585439283,121.957822195286)) ;
#27846 = CARTESIAN_POINT('Ctrl Pts',(-19.7280448206616,19.1236694635654,122.248623138328)) ;
#27847 = CARTESIAN_POINT('Ctrl Pts',(-20.0549291177178,19.3136925803563,122.049626315006)) ;
#27848 = CARTESIAN_POINT('Ctrl Pts',(-19.9258003882064,19.1337034999934,122.322067316074)) ;
#27849 = CARTESIAN_POINT('Ctrl Pts',(-20.2792335465816,19.3235800073143,122.18076820435)) ;
#27850 = CARTESIAN_POINT('Ctrl Pts',(-20.1052428067102,19.1435909269514,122.426981141854)) ;
#27851 = CARTESIAN_POINT('Ctrl Pts',(-20.4802444747173,19.3335944416507,122.350655841088)) ;
#27852 = CARTESIAN_POINT('Ctrl Pts',(-20.2660510795986,19.1536053612878,122.562891792175)) ;
#27853 = CARTESIAN_POINT('Ctrl Pts',(-20.6485175407954,19.3436293862856,122.553674509814)) ;
#27854 = CARTESIAN_POINT('Ctrl Pts',(-20.4006689258585,19.1636403059227,122.725307374417)) ;
#27855 = CARTESIAN_POINT('Ctrl Pts',(-20.7769890298325,19.3534617363166,122.777893029322)) ;
#27856 = CARTESIAN_POINT('Ctrl Pts',(-20.5034449148929,19.1734726559537,122.904681511226)) ;
#27857 = CARTESIAN_POINT('Ctrl Pts',(-20.8667862746344,19.3635371754338,123.026918659849)) ;
#27858 = CARTESIAN_POINT('Ctrl Pts',(-20.5752821883899,19.183548095071,123.103902590368)) ;
#27859 = CARTESIAN_POINT('Ctrl Pts',(-20.9111458115105,19.3733896406684,123.282059452494)) ;
#27860 = CARTESIAN_POINT('Ctrl Pts',(-20.6107689973514,19.1934005603056,123.308014298688)) ;
#27861 = CARTESIAN_POINT('Ctrl Pts',(-20.9107290324318,19.3834625182453,123.546718673386)) ;
#27862 = CARTESIAN_POINT('Ctrl Pts',(-20.6104349741825,19.2034734378824,123.519742024396)) ;
#27863 = CARTESIAN_POINT('Ctrl Pts',(-20.8653781808651,19.3933051144378,123.801387925564)) ;
#27864 = CARTESIAN_POINT('Ctrl Pts',(-20.5741538923526,19.2133160340749,123.723476203268)) ;
#27865 = CARTESIAN_POINT('Ctrl Pts',(-20.7760923678515,19.4032854985531,124.047984519831)) ;
#27866 = CARTESIAN_POINT('Ctrl Pts',(-20.5027249602154,19.2232964181902,123.920753112728)) ;
#27867 = CARTESIAN_POINT('Ctrl Pts',(-20.6443997501556,19.4133039792019,124.275948701137)) ;
#27868 = CARTESIAN_POINT('Ctrl Pts',(-20.3973704129932,19.233314898839,124.103124205952)) ;
#27869 = CARTESIAN_POINT('Ctrl Pts',(-20.4778099653252,19.4231872942023,124.475248963833)) ;
#27870 = CARTESIAN_POINT('Ctrl Pts',(-20.2640988584677,19.2431982138394,124.262563499982)) ;
#27871 = CARTESIAN_POINT('Ctrl Pts',(-20.2754104277972,19.4332555912927,124.645589428262)) ;
#27872 = CARTESIAN_POINT('Ctrl Pts',(-20.1021787138093,19.2532665109298,124.398835770553)) ;
#27873 = CARTESIAN_POINT('Ctrl Pts',(-20.0520012191522,19.443085659665,124.775372441285)) ;
#27874 = CARTESIAN_POINT('Ctrl Pts',(-19.9234522479264,19.2630965793021,124.502661276645)) ;
#27875 = CARTESIAN_POINT('Ctrl Pts',(-19.8038135625138,19.4531524521334,124.86681341649)) ;
#27876 = CARTESIAN_POINT('Ctrl Pts',(-19.7249017349538,19.2731633717705,124.575813934512)) ;
#27877 = CARTESIAN_POINT('Ctrl Pts',(-19.5479941097252,19.4630417856219,124.912847154411)) ;
#27878 = CARTESIAN_POINT('Ctrl Pts',(-19.5202469635521,19.2830527052591,124.612640501714)) ;
#27879 = CARTESIAN_POINT('Ctrl Pts',(-19.2851987471319,19.473043917038,124.914186378401)) ;
#27880 = CARTESIAN_POINT('Ctrl Pts',(-19.3100107840446,19.2930548366751,124.613711708274)) ;
#27881 = CARTESIAN_POINT('Ctrl Pts',(-19.0280693627692,19.482967786659,124.870372052193)) ;
#27882 = CARTESIAN_POINT('Ctrl Pts',(-19.1043078948215,19.3029787062961,124.578660218181)) ;
#27883 = CARTESIAN_POINT('Ctrl Pts',(-18.7796000674895,19.4930113021762,124.781474531052)) ;
#27884 = CARTESIAN_POINT('Ctrl Pts',(-18.9055323440351,19.3130222218133,124.507542000366)) ;
#27885 = CARTESIAN_POINT('Ctrl Pts',(-18.5537969176444,19.5028935150645,124.653102676941)) ;
#27886 = CARTESIAN_POINT('Ctrl Pts',(-18.7248906370469,19.3229044347016,124.404844891224)) ;
#27887 = CARTESIAN_POINT('Ctrl Pts',(-18.3500292628219,19.5129615922839,124.484417808806)) ;
#27888 = CARTESIAN_POINT('Ctrl Pts',(-18.5618763184921,19.332972511921,124.269896733581)) ;
#27889 = CARTESIAN_POINT('Ctrl Pts',(-18.1823173295114,19.5228000970181,124.287590469283)) ;
#27890 = CARTESIAN_POINT('Ctrl Pts',(-18.4277075526952,19.3428110166552,124.112435753387)) ;
#27891 = CARTESIAN_POINT('Ctrl Pts',(-18.04805852035,19.5328628654475,124.059806889975)) ;
#27892 = CARTESIAN_POINT('Ctrl Pts',(-18.3203002879426,19.3528737850846,123.930208672601)) ;
#27893 = CARTESIAN_POINT('Ctrl Pts',(-17.9571650618813,19.5427598587302,123.816107138229)) ;
#27894 = CARTESIAN_POINT('Ctrl Pts',(-18.247585798284,19.3627707783674,123.735249623978)) ;
#27895 = CARTESIAN_POINT('Ctrl Pts',(-17.9089504191746,19.552691086365,123.559623490826)) ;
#27896 = CARTESIAN_POINT('Ctrl Pts',(-18.2090139678198,19.3727020060021,123.530063314493)) ;
#27897 = CARTESIAN_POINT('Ctrl Pts',(-17.9062584823097,19.5627332450072,123.295743025407)) ;
#27898 = CARTESIAN_POINT('Ctrl Pts',(-18.2068602643135,19.3827441646443,123.318958777135)) ;
#27899 = CARTESIAN_POINT('Ctrl Pts',(-17.9485751372052,19.5726199545382,123.039387974114)) ;
#27900 = CARTESIAN_POINT('Ctrl Pts',(-18.240713249619,19.3926308741753,123.113875561071)) ;
#27901 = CARTESIAN_POINT('Ctrl Pts',(-18.035260566707,19.5826129269668,122.791515506251)) ;
#27902 = CARTESIAN_POINT('Ctrl Pts',(-18.3100612446795,19.4026238466039,122.915577638234)) ;
#27903 = CARTESIAN_POINT('Ctrl Pts',(-18.1631676695922,19.5925591215034,122.563579250553)) ;
#27904 = CARTESIAN_POINT('Ctrl Pts',(-18.4123864487675,19.4125700411405,122.733228908367)) ;
#27905 = CARTESIAN_POINT('Ctrl Pts',(-18.3282687771438,19.6025044963549,122.360947075224)) ;
#27906 = CARTESIAN_POINT('Ctrl Pts',(-18.5444667060827,19.422515415992,122.571123262125)) ;
#27907 = CARTESIAN_POINT('Ctrl Pts',(-18.5284509193618,19.6125594157148,122.188521930226)) ;
#27908 = CARTESIAN_POINT('Ctrl Pts',(-18.7046123935706,19.4325703353519,122.433182741857)) ;
#27909 = CARTESIAN_POINT('Ctrl Pts',(-18.750061582201,19.6223809351583,122.056150769602)) ;
#27910 = CARTESIAN_POINT('Ctrl Pts',(-18.8818995815922,19.4423918547954,122.327286088883)) ;
#27911 = CARTESIAN_POINT('Ctrl Pts',(-18.9970975872,19.6324467039252,121.961712899097)) ;
#27912 = CARTESIAN_POINT('Ctrl Pts',(-19.0795284847268,19.4524576235623,122.251735185212)) ;
#27913 = CARTESIAN_POINT('Ctrl Pts',(-19.2526602063055,19.6423486255803,121.912488218236)) ;
#27914 = CARTESIAN_POINT('Ctrl Pts',(-19.2839777620693,19.4623595452174,122.212355084193)) ;
#27915 = CARTESIAN_POINT('Ctrl Pts',(-19.5165208729935,19.6523916844013,121.908094752818)) ;
#27916 = CARTESIAN_POINT('Ctrl Pts',(-19.4950664570593,19.4724026040384,122.208839744185)) ;
#27917 = CARTESIAN_POINT('Ctrl Pts',(-19.7735886685139,19.662297678444,121.949158051718)) ;
#27918 = CARTESIAN_POINT('Ctrl Pts',(-19.7007200621191,19.4823085980811,122.241689749395)) ;
#27919 = CARTESIAN_POINT('Ctrl Pts',(-20.0206528799151,19.6722354515258,122.033777229908)) ;
#27920 = CARTESIAN_POINT('Ctrl Pts',(-19.8983711686072,19.4922463711629,122.30938424429)) ;
#27921 = CARTESIAN_POINT('Ctrl Pts',(-20.2514911587077,19.6822758152581,122.161558568198)) ;
#27922 = CARTESIAN_POINT('Ctrl Pts',(-20.0830422357934,19.5022867348952,122.411608819251)) ;
#27923 = CARTESIAN_POINT('Ctrl Pts',(-20.4536472526372,19.6921631589816,122.324810150255)) ;
#27924 = CARTESIAN_POINT('Ctrl Pts',(-20.2447669012231,19.5121740786187,122.542209021845)) ;
#27925 = CARTESIAN_POINT('Ctrl Pts',(-20.6265036649569,19.7021553895503,122.522452222942)) ;
#27926 = CARTESIAN_POINT('Ctrl Pts',(-20.3830525266567,19.5221663091874,122.700322030319)) ;
#27927 = CARTESIAN_POINT('Ctrl Pts',(-20.7617787531808,19.7121039173339,122.746188030278)) ;
#27928 = CARTESIAN_POINT('Ctrl Pts',(-20.4912730421252,19.532114836971,122.879309900702)) ;
#27929 = CARTESIAN_POINT('Ctrl Pts',(-20.856369565108,19.7220407010572,122.989558473137)) ;
#27930 = CARTESIAN_POINT('Ctrl Pts',(-20.5669463183877,19.5420516206943,123.074005464355)) ;
#27931 = CARTESIAN_POINT('Ctrl Pts',(-20.9078402627332,19.7320237018542,123.246836830907)) ;
#27932 = CARTESIAN_POINT('Ctrl Pts',(-20.6081237656465,19.5520346214913,123.279827763413)) ;
#27933 = CARTESIAN_POINT('Ctrl Pts',(-20.9134056044351,19.7420675886949,123.510689929292)) ;
#27934 = CARTESIAN_POINT('Ctrl Pts',(-20.6125768755946,19.562078508332,123.490910375999)) ;
#27935 = CARTESIAN_POINT('Ctrl Pts',(-20.8745366916682,19.7518956122695,123.766060949729)) ;
#27936 = CARTESIAN_POINT('Ctrl Pts',(-20.5814828864297,19.5719065319066,123.69520619847)) ;
#27937 = CARTESIAN_POINT('Ctrl Pts',(-20.7899593277774,19.7619728604831,124.016948250578)) ;
#27938 = CARTESIAN_POINT('Ctrl Pts',(-20.513821837292,19.5819837801202,123.895916689788)) ;
#27939 = CARTESIAN_POINT('Ctrl Pts',(-20.6660660069028,19.7718224157884,124.244285226899)) ;
#27940 = CARTESIAN_POINT('Ctrl Pts',(-20.4147085725534,19.5918333354255,124.077785895298)) ;
#27941 = CARTESIAN_POINT('Ctrl Pts',(-20.5009161893016,19.7819051239861,124.451396677659)) ;
#27942 = CARTESIAN_POINT('Ctrl Pts',(-20.2825893295826,19.6019160436232,124.243476002834)) ;
#27943 = CARTESIAN_POINT('Ctrl Pts',(-20.307696830118,19.7917177169126,124.622248846254)) ;
#27944 = CARTESIAN_POINT('Ctrl Pts',(-20.1280154809097,19.6117286365497,124.380157782015)) ;
#27945 = CARTESIAN_POINT('Ctrl Pts',(-20.0823669714035,19.8017849091705,124.760755273323)) ;
#27946 = CARTESIAN_POINT('Ctrl Pts',(-19.9477519880674,19.6217958288076,124.490964105197)) ;
#27947 = CARTESIAN_POINT('Ctrl Pts',(-19.8403718039497,19.8116837386331,124.856362880226)) ;
#27948 = CARTESIAN_POINT('Ctrl Pts',(-19.7541569135087,19.6316946582702,124.567451052078)) ;
#27949 = CARTESIAN_POINT('Ctrl Pts',(-19.581599257843,19.8217377298233,124.90940442077)) ;
#27950 = CARTESIAN_POINT('Ctrl Pts',(-19.5471389315843,19.6417486494604,124.609885512907)) ;
#27951 = CARTESIAN_POINT('Ctrl Pts',(-19.3222318233483,19.8316094546065,124.916810422138)) ;
#27952 = CARTESIAN_POINT('Ctrl Pts',(-19.339645850064,19.6516203742436,124.615811552476)) ;
#27953 = CARTESIAN_POINT('Ctrl Pts',(-19.0604406240858,19.8416798967367,124.878387276188)) ;
#27954 = CARTESIAN_POINT('Ctrl Pts',(-19.1302124239704,19.6616908163738,124.585074260848)) ;
#27955 = CARTESIAN_POINT('Ctrl Pts',(-18.8151144576531,19.851512975167,124.797145106877)) ;
#27956 = CARTESIAN_POINT('Ctrl Pts',(-18.9339520539141,19.6715238948041,124.52008208332)) ;
#27957 = CARTESIAN_POINT('Ctrl Pts',(-18.5827297027157,19.8615434486684,124.672758530689)) ;
#27958 = CARTESIAN_POINT('Ctrl Pts',(-18.7480434996773,19.6815543683055,124.420574076199)) ;
#27959 = CARTESIAN_POINT('Ctrl Pts',(-18.3759053294246,19.8715750479671,124.509274829673)) ;
#27960 = CARTESIAN_POINT('Ctrl Pts',(-18.5825831437698,19.6915859676042,124.289788093677)) ;
#27961 = CARTESIAN_POINT('Ctrl Pts',(-18.2037555511074,19.8814047490052,124.31670801897)) ;
#27962 = CARTESIAN_POINT('Ctrl Pts',(-18.4448629441187,19.7014156686424,124.135736342827)) ;
#27963 = CARTESIAN_POINT('Ctrl Pts',(-18.0647658072952,19.8913941870617,124.094000670336)) ;
#27964 = CARTESIAN_POINT('Ctrl Pts',(-18.3336698936195,19.7114051066988,123.957571414372)) ;
#27965 = CARTESIAN_POINT('Ctrl Pts',(-17.9666480383149,19.9014380902778,123.848976044792)) ;
#27966 = CARTESIAN_POINT('Ctrl Pts',(-18.2551743019667,19.7214490099149,123.761552138209)) ;
#27967 = CARTESIAN_POINT('Ctrl Pts',(-17.9132339251412,19.9112596110913,123.596462120658)) ;
#27968 = CARTESIAN_POINT('Ctrl Pts',(-18.212441709217,19.7312705307284,123.559542293389)) ;
#27969 = CARTESIAN_POINT('Ctrl Pts',(-17.9036546813369,19.9212953353384,123.332913768264)) ;
#27970 = CARTESIAN_POINT('Ctrl Pts',(-18.2047766510836,19.7413062549755,123.348703585753)) ;
#27971 = CARTESIAN_POINT('Ctrl Pts',(-17.9406113337571,19.9313174892709,123.072128085455)) ;
#27972 = CARTESIAN_POINT('Ctrl Pts',(-18.2343404591825,19.751328408908,123.140074813286)) ;
#27973 = CARTESIAN_POINT('Ctrl Pts',(-18.0205697573143,19.9411797210282,122.825622198603)) ;
#27974 = CARTESIAN_POINT('Ctrl Pts',(-18.2983054242486,19.7611906406653,122.942870341222)) ;
#27975 = CARTESIAN_POINT('Ctrl Pts',(-18.1426708877126,19.9511387914861,122.594127929803)) ;
#27976 = CARTESIAN_POINT('Ctrl Pts',(-18.3959846585781,19.7711497111232,122.757674351822)) ;
#27977 = CARTESIAN_POINT('Ctrl Pts',(-18.3046496822276,19.9611739638623,122.386036391047)) ;
#27978 = CARTESIAN_POINT('Ctrl Pts',(-18.525566417151,19.7811848834994,122.591200043048)) ;
#27979 = CARTESIAN_POINT('Ctrl Pts',(-18.4970491714254,19.9710543490205,122.211642765681)) ;
#27980 = CARTESIAN_POINT('Ctrl Pts',(-18.6794843828221,19.7910652686577,122.451684269361)) ;
#27981 = CARTESIAN_POINT('Ctrl Pts',(-18.720627652709,19.9811110636145,122.070778322321)) ;
#27982 = CARTESIAN_POINT('Ctrl Pts',(-18.8583463631659,19.8011219832516,122.338991147531)) ;
#27983 = CARTESIAN_POINT('Ctrl Pts',(-18.960996130641,19.9909903321865,121.972639347132)) ;
#27984 = CARTESIAN_POINT('Ctrl Pts',(-19.0506399085198,19.8110012518237,122.260478581221)) ;
#27985 = CARTESIAN_POINT('Ctrl Pts',(-19.2174586026876,20.0009812896722,121.916419162101)) ;
#27986 = CARTESIAN_POINT('Ctrl Pts',(-19.2558093721547,19.8209922093093,122.21550063503)) ;
#27987 = CARTESIAN_POINT('Ctrl Pts',(-19.4811173295918,20.0110219483074,121.906111456795)) ;
#27988 = CARTESIAN_POINT('Ctrl Pts',(-19.4667363549532,19.8310328679445,122.207252696804)) ;
#27989 = CARTESIAN_POINT('Ctrl Pts',(-19.7372046092749,20.0208549280154,121.940573290861)) ;
#27990 = CARTESIAN_POINT('Ctrl Pts',(-19.6716056688886,19.8408658476525,122.234820236614)) ;
#27991 = CARTESIAN_POINT('Ctrl Pts',(-19.9876565139675,20.0308480612651,122.019537420732)) ;
#27992 = CARTESIAN_POINT('Ctrl Pts',(-19.871967684399,19.8508589809022,122.297989646812)) ;
#27993 = CARTESIAN_POINT('Ctrl Pts',(-20.2212609501245,20.0408801136485,122.141754795336)) ;
#27994 = CARTESIAN_POINT('Ctrl Pts',(-20.0588521268464,19.8608910332856,122.395761901234)) ;
#27995 = CARTESIAN_POINT('Ctrl Pts',(-20.4267990069944,20.0507453425998,122.29973257063)) ;
#27996 = CARTESIAN_POINT('Ctrl Pts',(-20.2232832806594,19.8707562622369,122.522142243935)) ;
#27997 = CARTESIAN_POINT('Ctrl Pts',(-20.6040593213488,20.060707283843,122.492388017739)) ;
#27998 = CARTESIAN_POINT('Ctrl Pts',(-20.3650928817087,19.8807182034801,122.676265086268)) ;
#27999 = CARTESIAN_POINT('Ctrl Pts',(-20.7458379853386,20.0707419988798,122.71471883926)) ;
#28000 = CARTESIAN_POINT('Ctrl Pts',(-20.4785174821517,19.8907529185169,122.854128710767)) ;
#28001 = CARTESIAN_POINT('Ctrl Pts',(-20.8457638320152,20.0806277692238,122.954554133205)) ;
#28002 = CARTESIAN_POINT('Ctrl Pts',(-20.5584598470704,19.9006386888609,123.045995755698)) ;
#28003 = CARTESIAN_POINT('Ctrl Pts',(-20.9035264743855,20.0906903666126,123.212570178599)) ;
#28004 = CARTESIAN_POINT('Ctrl Pts',(-20.6046719531102,19.9107012862497,123.252408261689)) ;
#28005 = CARTESIAN_POINT('Ctrl Pts',(-20.9154749497781,20.1005407784478,123.471173528851)) ;
#28006 = CARTESIAN_POINT('Ctrl Pts',(-20.6142327359483,19.9205516980849,123.459290308044)) ;
#28007 = CARTESIAN_POINT('Ctrl Pts',(-20.8824212203225,20.1105679477337,123.732588303383)) ;
#28008 = CARTESIAN_POINT('Ctrl Pts',(-20.5877918409855,19.9305788673709,123.668422402238)) ;
#28009 = CARTESIAN_POINT('Ctrl Pts',(-20.8038130480593,20.1205954284479,123.984115444725)) ;
#28010 = CARTESIAN_POINT('Ctrl Pts',(-20.5249072402036,19.940606348085,123.86964471591)) ;
#28011 = CARTESIAN_POINT('Ctrl Pts',(-20.6854052876472,20.1304384810272,124.214077225316)) ;
#28012 = CARTESIAN_POINT('Ctrl Pts',(-20.4301831161523,19.9504494006643,124.053614646428)) ;
#28013 = CARTESIAN_POINT('Ctrl Pts',(-20.5269966913248,20.1404323844658,124.423553915828)) ;
#28014 = CARTESIAN_POINT('Ctrl Pts',(-20.3034580001774,19.9604433041029,124.221197233981)) ;
#28015 = CARTESIAN_POINT('Ctrl Pts',(-20.3336481312429,20.1504595072422,124.602587618317)) ;
#28016 = CARTESIAN_POINT('Ctrl Pts',(-20.1487805945953,19.9704704268793,124.364425725248)) ;
#28017 = CARTESIAN_POINT('Ctrl Pts',(-20.1153421998912,20.1603502121343,124.743661057522)) ;
#28018 = CARTESIAN_POINT('Ctrl Pts',(-19.9741372834993,19.9803611317714,124.477286090543)) ;
#28019 = CARTESIAN_POINT('Ctrl Pts',(-19.873563628878,20.1703422389846,124.846066786522)) ;
#28020 = CARTESIAN_POINT('Ctrl Pts',(-19.7807153501285,19.9903531586217,124.559212634884)) ;
#28021 = CARTESIAN_POINT('Ctrl Pts',(-19.618831660715,20.1802882204731,124.904591118333)) ;
#28022 = CARTESIAN_POINT('Ctrl Pts',(-19.5769304388928,20.0002991401102,124.60603416333)) ;
#28023 = CARTESIAN_POINT('Ctrl Pts',(-19.3577875500338,20.190235393095,124.918525903528)) ;
#28024 = CARTESIAN_POINT('Ctrl Pts',(-19.3680954272052,20.0102463127322,124.61718417711)) ;
#28025 = CARTESIAN_POINT('Ctrl Pts',(-19.0957195762214,20.2002833344212,124.886313111744)) ;
#28026 = CARTESIAN_POINT('Ctrl Pts',(-19.1584407747982,20.0202942540583,124.591416103589)) ;
#28027 = CARTESIAN_POINT('Ctrl Pts',(-18.8481841830687,20.210130968229,124.810831448379)) ;
#28028 = CARTESIAN_POINT('Ctrl Pts',(-18.9604121247911,20.0301418878661,124.531032963021)) ;
#28029 = CARTESIAN_POINT('Ctrl Pts',(-18.6144848557031,20.220092682914,124.692895466025)) ;
#28030 = CARTESIAN_POINT('Ctrl Pts',(-18.7734517428529,20.0401036025511,124.436686220242)) ;
#28031 = CARTESIAN_POINT('Ctrl Pts',(-18.4035822760522,20.2301213157925,124.534835645106)) ;
#28032 = CARTESIAN_POINT('Ctrl Pts',(-18.6047283766993,20.0501322354297,124.310240160807)) ;
#28033 = CARTESIAN_POINT('Ctrl Pts',(-18.2254094105789,20.2400316413277,124.34490354003)) ;
#28034 = CARTESIAN_POINT('Ctrl Pts',(-18.4621885771613,20.0600425609648,124.158296117052)) ;
#28035 = CARTESIAN_POINT('Ctrl Pts',(-18.0819921054121,20.2499664717994,124.126739575367)) ;
#28036 = CARTESIAN_POINT('Ctrl Pts',(-18.347452906344,20.0699773914365,123.983766287248)) ;
#28037 = CARTESIAN_POINT('Ctrl Pts',(-17.9777343205273,20.2600078041814,123.884334153632)) ;
#28038 = CARTESIAN_POINT('Ctrl Pts',(-18.2640446533727,20.0800187238185,123.789842799783)) ;
#28039 = CARTESIAN_POINT('Ctrl Pts',(-17.9179543452334,20.2699006776202,123.631328380915)) ;
#28040 = CARTESIAN_POINT('Ctrl Pts',(-18.2162184451713,20.0899115972573,123.587439083643)) ;
#28041 = CARTESIAN_POINT('Ctrl Pts',(-17.9022315156781,20.2798698434381,123.369810686241)) ;
#28042 = CARTESIAN_POINT('Ctrl Pts',(-18.2036382029103,20.0998807630752,123.37822414266)) ;
#28043 = CARTESIAN_POINT('Ctrl Pts',(-17.9327660607719,20.2898985771546,123.108061591331)) ;
#28044 = CARTESIAN_POINT('Ctrl Pts',(-18.2280625915591,20.1099094967917,123.168828314924)) ;
#28045 = CARTESIAN_POINT('Ctrl Pts',(-18.0314212956118,20.3030910959258,122.775637805959)) ;
#28046 = CARTESIAN_POINT('Ctrl Pts',(-18.3069888734284,20.1231020155629,122.902870362102)) ;
#28047 = CARTESIAN_POINT('Ctrl Pts',(-18.2167817772954,20.3164509639684,122.472918789065)) ;
#28048 = CARTESIAN_POINT('Ctrl Pts',(-18.455294322149,20.1364618836056,122.660681237817)) ;
#28049 = CARTESIAN_POINT('Ctrl Pts',(-18.4689719567282,20.3296763011173,122.233665328807)) ;
#28050 = CARTESIAN_POINT('Ctrl Pts',(-18.657015967816,20.1496872207544,122.469309185131)) ;
#28051 = CARTESIAN_POINT('Ctrl Pts',(-18.6872891439649,20.3396575269579,122.0882957323)) ;
#28052 = CARTESIAN_POINT('Ctrl Pts',(-18.8316741569079,20.1596684465951,122.353005054526)) ;
#28053 = CARTESIAN_POINT('Ctrl Pts',(-18.9290457583576,20.3496930939408,121.982939786469)) ;
#28054 = CARTESIAN_POINT('Ctrl Pts',(-19.0250769393784,20.1697040135779,122.268720036234)) ;
#28055 = CARTESIAN_POINT('Ctrl Pts',(-19.1809279027677,20.3595561719029,121.921703115503)) ;
#28056 = CARTESIAN_POINT('Ctrl Pts',(-19.2265826009953,20.17956709154,122.219728036107)) ;
#28057 = CARTESIAN_POINT('Ctrl Pts',(-19.4449915418395,20.369626470704,121.904729894139)) ;
#28058 = CARTESIAN_POINT('Ctrl Pts',(-19.4378331366122,20.1896373903411,122.206147360686)) ;
#28059 = CARTESIAN_POINT('Ctrl Pts',(-19.7020745055463,20.3794687692718,121.933224576347)) ;
#28060 = CARTESIAN_POINT('Ctrl Pts',(-19.6434999173445,20.1994796889089,122.228940862857)) ;
#28061 = CARTESIAN_POINT('Ctrl Pts',(-19.9535442296739,20.3894294674416,122.005865433082)) ;
#28062 = CARTESIAN_POINT('Ctrl Pts',(-19.844676334268,20.2094403870787,122.287051467107)) ;
#28063 = CARTESIAN_POINT('Ctrl Pts',(-20.1901714045228,20.3994675016211,122.122429978516)) ;
#28064 = CARTESIAN_POINT('Ctrl Pts',(-20.0339789452335,20.2194784212582,122.380301057783)) ;
#28065 = CARTESIAN_POINT('Ctrl Pts',(-20.3998046709007,20.4093412384676,122.275390622965)) ;
#28066 = CARTESIAN_POINT('Ctrl Pts',(-20.2016870029984,20.2293521581047,122.502667926402)) ;
#28067 = CARTESIAN_POINT('Ctrl Pts',(-20.5832300951106,20.4194130223928,122.466148916955)) ;
#28068 = CARTESIAN_POINT('Ctrl Pts',(-20.3484287872655,20.2394239420299,122.655272907251)) ;
#28069 = CARTESIAN_POINT('Ctrl Pts',(-20.7274022481108,20.429245143594,122.680593266604)) ;
#28070 = CARTESIAN_POINT('Ctrl Pts',(-20.4637684999712,20.2492560632311,122.826827448914)) ;
#28071 = CARTESIAN_POINT('Ctrl Pts',(-20.83492227229,20.4392781676194,122.921317142792)) ;
#28072 = CARTESIAN_POINT('Ctrl Pts',(-20.549786401994,20.2592890872566,123.019405611083)) ;
#28073 = CARTESIAN_POINT('Ctrl Pts',(-20.8982551027824,20.4492940478161,123.176808341218)) ;
#28074 = CARTESIAN_POINT('Ctrl Pts',(-20.6004547451558,20.2693049674532,123.223797857408)) ;
#28075 = CARTESIAN_POINT('Ctrl Pts',(-20.9165069215087,20.4591775669103,123.435894221683)) ;
#28076 = CARTESIAN_POINT('Ctrl Pts',(-20.615058364723,20.2791884865474,123.43106704069)) ;
#28077 = CARTESIAN_POINT('Ctrl Pts',(-20.8895420040221,20.469167979274,123.697025786576)) ;
#28078 = CARTESIAN_POINT('Ctrl Pts',(-20.5934884233315,20.2891788989111,123.639971206989)) ;
#28079 = CARTESIAN_POINT('Ctrl Pts',(-20.7941934591565,20.4824311424774,124.032297261989)) ;
#28080 = CARTESIAN_POINT('Ctrl Pts',(-20.5172126368922,20.3024420621145,123.908195802062)) ;
#28081 = CARTESIAN_POINT('Ctrl Pts',(-20.61364497499,20.4957087127286,124.335469275498)) ;
#28082 = CARTESIAN_POINT('Ctrl Pts',(-20.3727498733357,20.3157196323657,124.15076100523)) ;
#28083 = CARTESIAN_POINT('Ctrl Pts',(-20.3624251620307,20.5090390152352,124.579659196355)) ;
#28084 = CARTESIAN_POINT('Ctrl Pts',(-20.1718067039307,20.3290499348723,124.346077405116)) ;
#28085 = CARTESIAN_POINT('Ctrl Pts',(-20.1474678125217,20.5189376970516,124.726143222167)) ;
#28086 = CARTESIAN_POINT('Ctrl Pts',(-19.9998354017675,20.3389486166887,124.463273991554)) ;
#28087 = CARTESIAN_POINT('Ctrl Pts',(-19.9082988338251,20.5289272120991,124.834343756603)) ;
#28088 = CARTESIAN_POINT('Ctrl Pts',(-19.8085028501753,20.3489381317363,124.549834241605)) ;
#28089 = CARTESIAN_POINT('Ctrl Pts',(-19.6550087594271,20.5388752638742,124.899096739163)) ;
#28090 = CARTESIAN_POINT('Ctrl Pts',(-19.6058699022926,20.3588861835113,124.601638844772)) ;
#28091 = CARTESIAN_POINT('Ctrl Pts',(-19.3945515389815,20.5488166671527,124.919199688652)) ;
#28092 = CARTESIAN_POINT('Ctrl Pts',(-19.3975068666403,20.3688275867898,124.617723886778)) ;
#28093 = CARTESIAN_POINT('Ctrl Pts',(-19.0469745337114,20.5621033319336,124.885630332357)) ;
#28094 = CARTESIAN_POINT('Ctrl Pts',(-19.1194311731786,20.3821142515707,124.590866211464)) ;
#28095 = CARTESIAN_POINT('Ctrl Pts',(-18.6334863377988,20.5787137535884,124.731039345078)) ;
#28096 = CARTESIAN_POINT('Ctrl Pts',(-18.788654663985,20.3987246732255,124.467201404259)) ;
#28097 = CARTESIAN_POINT('Ctrl Pts',(-18.2305106418667,20.5986250158392,124.387975748647)) ;
#28098 = CARTESIAN_POINT('Ctrl Pts',(-18.4662665446094,20.4186359354763,124.192751186382)) ;
#28099 = CARTESIAN_POINT('Ctrl Pts',(-17.9681790722083,20.6185691450041,123.927324296484)) ;
#28100 = CARTESIAN_POINT('Ctrl Pts',(-18.2563995729899,20.4385800646412,123.824231859657)) ;
#28101 = CARTESIAN_POINT('Ctrl Pts',(-17.8789643904274,20.6384923076093,123.405418987404)) ;
#28102 = CARTESIAN_POINT('Ctrl Pts',(-18.1850241788991,20.4585032272464,123.406707562409)) ;
#28103 = CARTESIAN_POINT('Ctrl Pts',(-17.9722011638597,20.6583824300158,122.884976490813)) ;
#28104 = CARTESIAN_POINT('Ctrl Pts',(-18.2596109762183,20.4783933496529,122.990352318436)) ;
#28105 = CARTESIAN_POINT('Ctrl Pts',(-18.2392413285999,20.6783873836159,122.425297035635)) ;
#28106 = CARTESIAN_POINT('Ctrl Pts',(-18.4732405399828,20.498398303253,122.622607344408)) ;
#28107 = CARTESIAN_POINT('Ctrl Pts',(-18.6435876221089,20.6982256406315,122.086739272797)) ;
#28108 = CARTESIAN_POINT('Ctrl Pts',(-18.7967168578306,20.5182365602686,122.35175829032)) ;
#28109 = CARTESIAN_POINT('Ctrl Pts',(-19.1427514572152,20.718219941418,121.904613931299)) ;
#28110 = CARTESIAN_POINT('Ctrl Pts',(-19.1960471830647,20.5382308610552,122.206055793577)) ;
#28111 = CARTESIAN_POINT('Ctrl Pts',(-19.6712810445263,20.7381051834625,121.904239572849)) ;
#28112 = CARTESIAN_POINT('Ctrl Pts',(-19.6188718571092,20.5581161030996,122.205753939832)) ;
#28113 = CARTESIAN_POINT('Ctrl Pts',(-20.168447470455,20.7579801299384,122.082748587511)) ;
#28114 = CARTESIAN_POINT('Ctrl Pts',(-20.0166067329943,20.5779910495756,122.348559983418)) ;
#28115 = CARTESIAN_POINT('Ctrl Pts',(-20.5778609764888,20.7780131998795,122.423240113376)) ;
#28116 = CARTESIAN_POINT('Ctrl Pts',(-20.3441382911306,20.5980241195166,122.620951670167)) ;
#28117 = CARTESIAN_POINT('Ctrl Pts',(-20.8439482662448,20.7979017067799,122.879935963145)) ;
#28118 = CARTESIAN_POINT('Ctrl Pts',(-20.5570102575303,20.617912626417,122.986308438082)) ;
#28119 = CARTESIAN_POINT('Ctrl Pts',(-20.9398845189848,20.8177565665612,123.398932664504)) ;
#28120 = CARTESIAN_POINT('Ctrl Pts',(-20.6337603893495,20.6377674861983,123.401507281384)) ;
#28121 = CARTESIAN_POINT('Ctrl Pts',(-20.8512719992327,20.8378074003489,123.924305207163)) ;
#28122 = CARTESIAN_POINT('Ctrl Pts',(-20.5628715067338,20.657818319986,123.821804891128)) ;
#28123 = CARTESIAN_POINT('Ctrl Pts',(-20.5928049104702,20.8575733422382,124.381835472892)) ;
#28124 = CARTESIAN_POINT('Ctrl Pts',(-20.3560969395519,20.6775842618753,124.187831867116)) ;
#28125 = CARTESIAN_POINT('Ctrl Pts',(-20.1896580437569,20.8775860736975,124.728578782344)) ;
#28126 = CARTESIAN_POINT('Ctrl Pts',(-20.0335794046623,20.6975969933346,124.465226382195)) ;
#28127 = CARTESIAN_POINT('Ctrl Pts',(-19.6948360554275,20.8974789086411,124.915243821142)) ;
#28128 = CARTESIAN_POINT('Ctrl Pts',(-19.6377205723978,20.7174898282782,124.61455887421)) ;
#28129 = CARTESIAN_POINT('Ctrl Pts',(-19.1659236264529,20.9173859319806,124.922728039924)) ;
#28130 = CARTESIAN_POINT('Ctrl Pts',(-19.2145894369091,20.7373968516177,124.620545637084)) ;
#28131 = CARTESIAN_POINT('Ctrl Pts',(-18.6655619227043,20.9373011968813,124.749682544139)) ;
#28132 = CARTESIAN_POINT('Ctrl Pts',(-18.8142995780805,20.7573121165184,124.482107923995)) ;
#28133 = CARTESIAN_POINT('Ctrl Pts',(-18.2524397020174,20.957332889041,124.413908184194)) ;
#28134 = CARTESIAN_POINT('Ctrl Pts',(-18.4838026915331,20.7773438086781,124.21348792732)) ;
#28135 = CARTESIAN_POINT('Ctrl Pts',(-17.9811972981208,20.977175935614,123.961546540794)) ;
#28136 = CARTESIAN_POINT('Ctrl Pts',(-18.2668088563855,20.7971868552511,123.8515965203)) ;
#28137 = CARTESIAN_POINT('Ctrl Pts',(-17.8790621516814,20.9970924835138,123.442223784006)) ;
#28138 = CARTESIAN_POINT('Ctrl Pts',(-18.1851023793624,20.8171034031509,123.436137129649)) ;
#28139 = CARTESIAN_POINT('Ctrl Pts',(-17.9604499278885,21.0170247265051,122.918699625149)) ;
#28140 = CARTESIAN_POINT('Ctrl Pts',(-18.2502146020831,20.8370356461422,123.017317483767)) ;
#28141 = CARTESIAN_POINT('Ctrl Pts',(-18.2149540834011,21.0369285613144,122.454965536719)) ;
#28142 = CARTESIAN_POINT('Ctrl Pts',(-18.4538202863488,20.8569394809515,122.646330486718)) ;
#28143 = CARTESIAN_POINT('Ctrl Pts',(-18.6119399166127,21.0568289615019,122.105461255144)) ;
#28144 = CARTESIAN_POINT('Ctrl Pts',(-18.7714112568372,20.876839881139,122.366728442058)) ;
#28145 = CARTESIAN_POINT('Ctrl Pts',(-19.1055245267092,21.0767786378812,121.91171422936)) ;
#28146 = CARTESIAN_POINT('Ctrl Pts',(-19.1662802778635,20.8967895575183,122.211733244875)) ;
#28147 = CARTESIAN_POINT('Ctrl Pts',(-19.6351319246211,21.0967111621016,121.898157078062)) ;
#28148 = CARTESIAN_POINT('Ctrl Pts',(-19.5899667460685,20.9167220817387,122.200890351572)) ;
#28149 = CARTESIAN_POINT('Ctrl Pts',(-20.1374331359232,21.1166311710878,122.065615887878)) ;
#28150 = CARTESIAN_POINT('Ctrl Pts',(-19.9918072525265,20.9366420907249,122.334860475937)) ;
#28151 = CARTESIAN_POINT('Ctrl Pts',(-20.5530840765956,21.136588077264,122.395047352195)) ;
#28152 = CARTESIAN_POINT('Ctrl Pts',(-20.3243262285862,20.9565989969011,122.598408332127)) ;
#28153 = CARTESIAN_POINT('Ctrl Pts',(-20.8308668599276,21.1564739167655,122.844813593085)) ;
#28154 = CARTESIAN_POINT('Ctrl Pts',(-20.5465500430235,20.9764848364026,122.958223574526)) ;
#28155 = CARTESIAN_POINT('Ctrl Pts',(-20.9388483133597,21.1764450889013,123.364394953387)) ;
#28156 = CARTESIAN_POINT('Ctrl Pts',(-20.6329313716892,20.9964560085384,123.373889855656)) ;
#28157 = CARTESIAN_POINT('Ctrl Pts',(-20.8643333248033,21.1962592858857,123.885809151916)) ;
#28158 = CARTESIAN_POINT('Ctrl Pts',(-20.5733172829464,21.0162702055228,123.791020397466)) ;
#28159 = CARTESIAN_POINT('Ctrl Pts',(-20.6149914724651,21.2162404718539,124.35458992427)) ;
#28160 = CARTESIAN_POINT('Ctrl Pts',(-20.3738339226301,21.0362513914911,124.166047707023)) ;
#28161 = CARTESIAN_POINT('Ctrl Pts',(-20.2875771231592,21.2328159772432,124.649450004713)) ;
#28162 = CARTESIAN_POINT('Ctrl Pts',(-20.1119198605758,21.0528268968803,124.401919518092)) ;
#28163 = CARTESIAN_POINT('Ctrl Pts',(-19.976190695121,21.2461254251068,124.808734121278)) ;
#28164 = CARTESIAN_POINT('Ctrl Pts',(-19.8627850672793,21.0661363447439,124.529357922434)) ;
#28165 = CARTESIAN_POINT('Ctrl Pts',(-19.6403422561752,21.2594931228834,124.911767929916)) ;
#28166 = CARTESIAN_POINT('Ctrl Pts',(-19.5941577979202,21.0795040425205,124.611771756262)) ;
#28167 = CARTESIAN_POINT('Ctrl Pts',(-19.2023540010426,21.2759836945493,124.927912591737)) ;
#28168 = CARTESIAN_POINT('Ctrl Pts',(-19.2437108124987,21.0959946141864,124.62469560568)) ;
#28169 = CARTESIAN_POINT('Ctrl Pts',(-18.6980130161789,21.2959039668821,124.76705541604)) ;
#28170 = CARTESIAN_POINT('Ctrl Pts',(-18.8402511097492,21.1159148865192,124.495996295646)) ;
#28171 = CARTESIAN_POINT('Ctrl Pts',(-18.3484015779916,21.3125210026031,124.497134075246)) ;
#28172 = CARTESIAN_POINT('Ctrl Pts',(-18.5605800541927,21.1325319222402,124.280076149471)) ;
#28173 = CARTESIAN_POINT('Ctrl Pts',(-18.1364098503999,21.3258118528842,124.219524949621)) ;
#28174 = CARTESIAN_POINT('Ctrl Pts',(-18.3909714359101,21.1458227725213,124.057970053224)) ;
#28175 = CARTESIAN_POINT('Ctrl Pts',(-18.0158871388316,21.3357808980387,123.986950081581)) ;
#28176 = CARTESIAN_POINT('Ctrl Pts',(-18.2945586408566,21.1557918176758,123.871912706625)) ;
#28177 = CARTESIAN_POINT('Ctrl Pts',(-17.9375848219816,21.3456842886722,123.7387264045)) ;
#28178 = CARTESIAN_POINT('Ctrl Pts',(-18.2319181148261,21.1656952083094,123.673331434388)) ;
#28179 = CARTESIAN_POINT('Ctrl Pts',(-17.9031917373362,21.355742074785,123.476694986446)) ;
#28180 = CARTESIAN_POINT('Ctrl Pts',(-18.2044053250832,21.1757529944221,123.463708741263)) ;
#28181 = CARTESIAN_POINT('Ctrl Pts',(-17.9143537185253,21.3655941114347,123.218009520766)) ;
#28182 = CARTESIAN_POINT('Ctrl Pts',(-18.2133399425486,21.1856050310718,123.256751469431)) ;
#28183 = CARTESIAN_POINT('Ctrl Pts',(-17.9896212280947,21.3789592355779,122.874956968011)) ;
#28184 = CARTESIAN_POINT('Ctrl Pts',(-18.2735425071571,21.198970155215,122.982353715324)) ;
#28185 = CARTESIAN_POINT('Ctrl Pts',(-18.1513956643206,21.3921852985409,122.562838107837)) ;
#28186 = CARTESIAN_POINT('Ctrl Pts',(-18.4029674268594,21.2121962181781,122.732632497982)) ;
#28187 = CARTESIAN_POINT('Ctrl Pts',(-18.3866109363659,21.4054889468232,122.304222180962)) ;
#28188 = CARTESIAN_POINT('Ctrl Pts',(-18.5911529954546,21.2254998664603,122.525730915353)) ;
#28189 = CARTESIAN_POINT('Ctrl Pts',(-18.5942688365872,21.4154804779862,122.143483381919)) ;
#28190 = CARTESIAN_POINT('Ctrl Pts',(-18.7572784100833,21.2354913976233,122.397143875669)) ;
#28191 = CARTESIAN_POINT('Ctrl Pts',(-18.8279161165822,21.4255199257855,122.020995347853)) ;
#28192 = CARTESIAN_POINT('Ctrl Pts',(-18.9441978151252,21.2455308454226,122.299154881713)) ;
#28193 = CARTESIAN_POINT('Ctrl Pts',(-19.0743002770801,21.4353637012994,121.942115783865)) ;
#28194 = CARTESIAN_POINT('Ctrl Pts',(-19.1413056995706,21.2553746209365,122.236053522357)) ;
#28195 = CARTESIAN_POINT('Ctrl Pts',(-19.3342026170286,21.445349342687,121.90619908811)) ;
#28196 = CARTESIAN_POINT('Ctrl Pts',(-19.3492278602432,21.2653602623241,122.207322374569)) ;
#28197 = CARTESIAN_POINT('Ctrl Pts',(-19.5951977714836,21.4552861270488,121.915768063468)) ;
#28198 = CARTESIAN_POINT('Ctrl Pts',(-19.5580238317526,21.2752970466859,122.214979818382)) ;
#28199 = CARTESIAN_POINT('Ctrl Pts',(-19.8533761099886,21.4653359615162,121.971250859302)) ;
#28200 = CARTESIAN_POINT('Ctrl Pts',(-19.7645659845222,21.2853468811533,122.259368252402)) ;
#28201 = CARTESIAN_POINT('Ctrl Pts',(-20.0932613278945,21.4751864110193,122.068581121297)) ;
#28202 = CARTESIAN_POINT('Ctrl Pts',(-19.9564732213435,21.2951973306564,122.337234519556)) ;
#28203 = CARTESIAN_POINT('Ctrl Pts',(-20.3156279272745,21.4851584250014,122.207174295959)) ;
#28204 = CARTESIAN_POINT('Ctrl Pts',(-20.1343652320431,21.3051693446385,122.448110919028)) ;
#28205 = CARTESIAN_POINT('Ctrl Pts',(-20.5110376061981,21.4951535828485,122.382755229701)) ;
#28206 = CARTESIAN_POINT('Ctrl Pts',(-20.290691427895,21.3151645024856,122.588577292965)) ;
#28207 = CARTESIAN_POINT('Ctrl Pts',(-20.6733301023097,21.5051875092122,122.590546133602)) ;
#28208 = CARTESIAN_POINT('Ctrl Pts',(-20.4205236271332,21.3251984288494,122.754811381595)) ;
#28209 = CARTESIAN_POINT('Ctrl Pts',(-20.7952585397872,21.5150432176446,122.819075138393)) ;
#28210 = CARTESIAN_POINT('Ctrl Pts',(-20.5180643101211,21.3350541372817,122.937635474695)) ;
#28211 = CARTESIAN_POINT('Ctrl Pts',(-20.8771547988309,21.5250413669833,123.068682710145)) ;
#28212 = CARTESIAN_POINT('Ctrl Pts',(-20.5835791727783,21.3450522866204,123.13732215833)) ;
#28213 = CARTESIAN_POINT('Ctrl Pts',(-20.9143410126104,21.5349407701568,123.326195883179)) ;
#28214 = CARTESIAN_POINT('Ctrl Pts',(-20.6133259222408,21.354951689794,123.343332810001)) ;
#28215 = CARTESIAN_POINT('Ctrl Pts',(-20.9061846999684,21.5449919670453,123.590176807784)) ;
#28216 = CARTESIAN_POINT('Ctrl Pts',(-20.6067986577069,21.3650028866824,123.554517489311)) ;
#28217 = CARTESIAN_POINT('Ctrl Pts',(-20.853249823519,21.5548742908582,123.844441837906)) ;
#28218 = CARTESIAN_POINT('Ctrl Pts',(-20.5644486425954,21.3748852104953,123.7579288163)) ;
#28219 = CARTESIAN_POINT('Ctrl Pts',(-20.7564330306425,21.5648691865148,124.088593766656)) ;
#28220 = CARTESIAN_POINT('Ctrl Pts',(-20.4869932187418,21.3848801061519,123.953249478274)) ;
#28221 = CARTESIAN_POINT('Ctrl Pts',(-20.6179931768872,21.5748902858973,124.312627761359)) ;
#28222 = CARTESIAN_POINT('Ctrl Pts',(-20.3762394774589,21.3949012055344,124.132475496053)) ;
#28223 = CARTESIAN_POINT('Ctrl Pts',(-20.4449112034606,21.5847975537594,124.507113190861)) ;
#28224 = CARTESIAN_POINT('Ctrl Pts',(-20.2377724303908,21.4048084733965,124.288062198318)) ;
#28225 = CARTESIAN_POINT('Ctrl Pts',(-20.2403849662515,21.5947358975846,124.669500522451)) ;
#28226 = CARTESIAN_POINT('Ctrl Pts',(-20.0741502752422,21.4147468172218,124.417970248963)) ;
#28227 = CARTESIAN_POINT('Ctrl Pts',(-20.0093045735368,21.6047393168851,124.79489097273)) ;
#28228 = CARTESIAN_POINT('Ctrl Pts',(-19.8892850037941,21.4247502365222,124.518280706296)) ;
#28229 = CARTESIAN_POINT('Ctrl Pts',(-19.7590892507398,21.6147738675922,124.878084487071)) ;
#28230 = CARTESIAN_POINT('Ctrl Pts',(-19.6891120481609,21.4347847872293,124.584833462809)) ;
#28231 = CARTESIAN_POINT('Ctrl Pts',(-19.5031930456652,21.6246188171978,124.916282417656)) ;
#28232 = CARTESIAN_POINT('Ctrl Pts',(-19.4843952188806,21.4446297368349,124.615389634999)) ;
#28233 = CARTESIAN_POINT('Ctrl Pts',(-19.2408957415365,21.6346046593107,124.909864611199)) ;
#28234 = CARTESIAN_POINT('Ctrl Pts',(-19.274557555605,21.4546155789478,124.610253310096)) ;
#28235 = CARTESIAN_POINT('Ctrl Pts',(-18.9848863453834,21.6445394666798,124.858431106566)) ;
#28236 = CARTESIAN_POINT('Ctrl Pts',(-19.0697507008442,21.4645503863169,124.569104541095)) ;
#28237 = CARTESIAN_POINT('Ctrl Pts',(-18.738859338082,21.6545970083931,124.761963952245)) ;
#28238 = CARTESIAN_POINT('Ctrl Pts',(-18.8729297698642,21.4746079280302,124.491928838993)) ;
#28239 = CARTESIAN_POINT('Ctrl Pts',(-18.5183469904694,21.6644186059052,124.627779140097)) ;
#28240 = CARTESIAN_POINT('Ctrl Pts',(-18.696521489678,21.4844295255424,124.384579574157)) ;
#28241 = CARTESIAN_POINT('Ctrl Pts',(-18.3195680415686,21.6744748653857,124.453674665829)) ;
#28242 = CARTESIAN_POINT('Ctrl Pts',(-18.5374995695825,21.4944857850228,124.245294444731)) ;
#28243 = CARTESIAN_POINT('Ctrl Pts',(-18.1562878546674,21.6844148016861,124.249767117428)) ;
#28244 = CARTESIAN_POINT('Ctrl Pts',(-18.4068771805631,21.5044257213232,124.082167340354)) ;
#28245 = CARTESIAN_POINT('Ctrl Pts',(-18.0306281552504,21.6943219224305,124.021754765608)) ;
#28246 = CARTESIAN_POINT('Ctrl Pts',(-18.3063513226383,21.5143328420676,123.899756895081)) ;
#28247 = CARTESIAN_POINT('Ctrl Pts',(-17.9454073048491,21.7043648283558,123.771982422679)) ;
#28248 = CARTESIAN_POINT('Ctrl Pts',(-18.2381764644056,21.5243757479929,123.699938324042)) ;
#28249 = CARTESIAN_POINT('Ctrl Pts',(-17.9053416812303,21.714272609455,123.51470692144)) ;
#28250 = CARTESIAN_POINT('Ctrl Pts',(-18.2061259509787,21.5342835290921,123.494118036696)) ;
#28251 = CARTESIAN_POINT('Ctrl Pts',(-17.9101476585179,21.7242829784574,123.251680239082)) ;
#28252 = CARTESIAN_POINT('Ctrl Pts',(-18.2099726089032,21.5442938980945,123.283696771005)) ;
#28253 = CARTESIAN_POINT('Ctrl Pts',(-17.9611784249865,21.7343138170262,122.993069233019)) ;
#28254 = CARTESIAN_POINT('Ctrl Pts',(-18.25079914997,21.5543247366633,123.076808307396)) ;
#28255 = CARTESIAN_POINT('Ctrl Pts',(-18.0542181019441,21.7441666566659,122.751434398998)) ;
#28256 = CARTESIAN_POINT('Ctrl Pts',(-18.3252324147839,21.564177576303,122.883501741555)) ;
#28257 = CARTESIAN_POINT('Ctrl Pts',(-18.1892070598107,21.7541546578309,122.526357242308)) ;
#28258 = CARTESIAN_POINT('Ctrl Pts',(-18.433225062823,21.574165577468,122.703441075812)) ;
#28259 = CARTESIAN_POINT('Ctrl Pts',(-18.3602212353183,21.76408347681,122.32928753721)) ;
#28260 = CARTESIAN_POINT('Ctrl Pts',(-18.5700375178516,21.5840943964472,122.545786794347)) ;
#28261 = CARTESIAN_POINT('Ctrl Pts',(-18.5637837492857,21.7740711795323,122.163582862095)) ;
#28262 = CARTESIAN_POINT('Ctrl Pts',(-18.7328885150387,21.5940820991695,122.413224497597)) ;
#28263 = CARTESIAN_POINT('Ctrl Pts',(-18.7943281092038,21.784107179335,122.035521757821)) ;
#28264 = CARTESIAN_POINT('Ctrl Pts',(-18.9173249461088,21.6041180989721,122.310777167978)) ;
#28265 = CARTESIAN_POINT('Ctrl Pts',(-19.038997751584,21.7939620491364,121.950573239043)) ;
#28266 = CARTESIAN_POINT('Ctrl Pts',(-19.1130605360951,21.6139729687736,122.242820240775)) ;
#28267 = CARTESIAN_POINT('Ctrl Pts',(-19.2983295791008,21.80396147956,121.908451210414)) ;
#28268 = CARTESIAN_POINT('Ctrl Pts',(-19.3205261622003,21.6239723991971,122.209124297681)) ;
#28269 = CARTESIAN_POINT('Ctrl Pts',(-19.5583862373949,21.8138565970253,121.911683181411)) ;
#28270 = CARTESIAN_POINT('Ctrl Pts',(-19.5285708804354,21.6338675166624,122.21171149709)) ;
#28271 = CARTESIAN_POINT('Ctrl Pts',(-19.8181211650492,21.8239170905422,121.96083913654)) ;
#28272 = CARTESIAN_POINT('Ctrl Pts',(-19.7363587075279,21.6439280101794,122.251037906807)) ;
#28273 = CARTESIAN_POINT('Ctrl Pts',(-20.0602885784198,21.8337665707434,122.052271697296)) ;
#28274 = CARTESIAN_POINT('Ctrl Pts',(-19.930091288856,21.6537774903805,122.324185167146)) ;
#28275 = CARTESIAN_POINT('Ctrl Pts',(-20.2872285089844,21.8437930210072,122.186139952124)) ;
#28276 = CARTESIAN_POINT('Ctrl Pts',(-20.1116425053652,21.6638039406443,122.431281064082)) ;
#28277 = CARTESIAN_POINT('Ctrl Pts',(-20.4871079315352,21.8538243114853,122.35801891506)) ;
#28278 = CARTESIAN_POINT('Ctrl Pts',(-20.2715450314613,21.6738352311224,122.568785502684)) ;
#28279 = CARTESIAN_POINT('Ctrl Pts',(-20.6513791646752,21.8636656991371,122.557772038563)) ;
#28280 = CARTESIAN_POINT('Ctrl Pts',(-20.4029602709634,21.6836766187742,122.728588256116)) ;
#28281 = CARTESIAN_POINT('Ctrl Pts',(-20.7809938111829,21.8736691000283,122.786445434062)) ;
#28282 = CARTESIAN_POINT('Ctrl Pts',(-20.5066507156167,21.6936800196655,122.91152759353)) ;
#28283 = CARTESIAN_POINT('Ctrl Pts',(-20.8686887483206,21.8836534828195,123.033784325657)) ;
#28284 = CARTESIAN_POINT('Ctrl Pts',(-20.5768052604981,21.7036644024566,123.109399027828)) ;
#28285 = CARTESIAN_POINT('Ctrl Pts',(-20.9120839655183,21.8936925728329,123.293981074003)) ;
#28286 = CARTESIAN_POINT('Ctrl Pts',(-20.6115199849103,21.71370349247,123.317556776986)) ;
#28287 = CARTESIAN_POINT('Ctrl Pts',(-20.9100499298834,21.9035383817421,123.552730180815)) ;
#28288 = CARTESIAN_POINT('Ctrl Pts',(-20.609891351577,21.7235493013792,123.524555112863)) ;
#28289 = CARTESIAN_POINT('Ctrl Pts',(-20.8629939222876,21.9135228045611,123.810817924676)) ;
#28290 = CARTESIAN_POINT('Ctrl Pts',(-20.5722453017055,21.7335337241982,123.73102487777)) ;
#28291 = CARTESIAN_POINT('Ctrl Pts',(-20.7723283116897,21.9234624298023,124.05581995963)) ;
#28292 = CARTESIAN_POINT('Ctrl Pts',(-20.4997117680828,21.7434733494394,123.927025654345)) ;
#28293 = CARTESIAN_POINT('Ctrl Pts',(-20.6391479210158,21.9335021193209,124.283546922036)) ;
#28294 = CARTESIAN_POINT('Ctrl Pts',(-20.3931662819036,21.7535130389581,124.109206674248)) ;
#28295 = CARTESIAN_POINT('Ctrl Pts',(-20.4711013650952,21.9433903077395,124.481766445994)) ;
#28296 = CARTESIAN_POINT('Ctrl Pts',(-20.2587285516933,21.7634012273766,124.267780913417)) ;
#28297 = CARTESIAN_POINT('Ctrl Pts',(-20.2694747065142,21.9533798337416,124.649861363959)) ;
#28298 = CARTESIAN_POINT('Ctrl Pts',(-20.097426616492,21.7733907533787,124.402255850537)) ;
#28299 = CARTESIAN_POINT('Ctrl Pts',(-20.0423296292845,21.9633383350968,124.779814856002)) ;
#28300 = CARTESIAN_POINT('Ctrl Pts',(-19.915710259167,21.7833492547339,124.506217429302)) ;
#28301 = CARTESIAN_POINT('Ctrl Pts',(-19.7977240449736,21.9732379291004,124.868443422786)) ;
#28302 = CARTESIAN_POINT('Ctrl Pts',(-19.7200260940079,21.7932488487375,124.577119050715)) ;
#28303 = CARTESIAN_POINT('Ctrl Pts',(-19.5376330731142,21.9832858172217,124.913825837491)) ;
#28304 = CARTESIAN_POINT('Ctrl Pts',(-19.5119529591425,21.8032967368588,124.61342395089)) ;
#28305 = CARTESIAN_POINT('Ctrl Pts',(-19.2775503015537,21.9931812424672,124.913569399124)) ;
#28306 = CARTESIAN_POINT('Ctrl Pts',(-19.3038874739033,21.8131921621044,124.613217771097)) ;
#28307 = CARTESIAN_POINT('Ctrl Pts',(-19.017233305932,22.0032426331678,124.86744619023)) ;
#28308 = CARTESIAN_POINT('Ctrl Pts',(-19.0956337981961,21.8232535528049,124.576318149791)) ;
#28309 = CARTESIAN_POINT('Ctrl Pts',(-18.7741467328486,22.0130882168545,124.778797095436)) ;
#28310 = CARTESIAN_POINT('Ctrl Pts',(-18.9011658833268,21.8330991364916,124.505398287498)) ;
#28311 = CARTESIAN_POINT('Ctrl Pts',(-18.5470623486079,22.0230511901637,124.648524437436)) ;
#28312 = CARTESIAN_POINT('Ctrl Pts',(-18.7194990790042,21.8430621098008,124.401179638259)) ;
#28313 = CARTESIAN_POINT('Ctrl Pts',(-18.3449798305692,22.0330768569895,124.479454619294)) ;
#28314 = CARTESIAN_POINT('Ctrl Pts',(-18.5578335854537,21.8530877766266,124.265923060778)) ;
#28315 = CARTESIAN_POINT('Ctrl Pts',(-18.1771126653133,22.0429913348558,124.28020996493)) ;
#28316 = CARTESIAN_POINT('Ctrl Pts',(-18.4235409199083,21.8630022544929,124.106527278134)) ;
#28317 = CARTESIAN_POINT('Ctrl Pts',(-18.0449474119808,22.0529798495308,124.053398711337)) ;
#28318 = CARTESIAN_POINT('Ctrl Pts',(-18.317809439298,21.8729907691679,123.925078062203)) ;
#28319 = CARTESIAN_POINT('Ctrl Pts',(-17.954211848732,22.0630239604462,123.805561752125)) ;
#28320 = CARTESIAN_POINT('Ctrl Pts',(-18.2452217507632,21.8830348800833,123.726808050528)) ;
#28321 = CARTESIAN_POINT('Ctrl Pts',(-17.9082542485454,22.0728520980408,123.551371969022)) ;
#28322 = CARTESIAN_POINT('Ctrl Pts',(-18.2084565831269,21.8928630176779,123.523457276199)) ;
#28323 = CARTESIAN_POINT('Ctrl Pts',(-17.9069805912369,22.0829286660997,123.286627562761)) ;
#28324 = CARTESIAN_POINT('Ctrl Pts',(-18.2074383400266,21.9029395857368,123.311661381763)) ;
#28325 = CARTESIAN_POINT('Ctrl Pts',(-17.9505873022016,22.0927808280039,123.031363437666)) ;
#28326 = CARTESIAN_POINT('Ctrl Pts',(-18.2423241725982,21.912791747641,123.107451229462)) ;
#28327 = CARTESIAN_POINT('Ctrl Pts',(-18.0395690380517,22.1028537899607,122.782109150564)) ;
#28328 = CARTESIAN_POINT('Ctrl Pts',(-18.3135102432881,21.9228647095978,122.908047671536)) ;
#28329 = CARTESIAN_POINT('Ctrl Pts',(-18.1675496052933,22.1126963519636,122.557311692099)) ;
#28330 = CARTESIAN_POINT('Ctrl Pts',(-18.4158946651662,21.9327072716007,122.728210991207)) ;
#28331 = CARTESIAN_POINT('Ctrl Pts',(-18.3342296705409,22.1226767884574,122.354827390352)) ;
#28332 = CARTESIAN_POINT('Ctrl Pts',(-18.5492388606532,21.9426877080945,122.566223989023)) ;
#28333 = CARTESIAN_POINT('Ctrl Pts',(-18.5346278830778,22.1326950937818,122.184094281001)) ;
#28334 = CARTESIAN_POINT('Ctrl Pts',(-18.7095577721264,21.9527060134189,122.429637890191)) ;
#28335 = CARTESIAN_POINT('Ctrl Pts',(-18.7583362356547,22.1425790577013,122.052058163512)) ;
#28336 = CARTESIAN_POINT('Ctrl Pts',(-18.8885238944235,21.9625899773384,122.32400976912)) ;
#28337 = CARTESIAN_POINT('Ctrl Pts',(-19.0060171333251,22.1526449344398,121.959277593487)) ;
#28338 = CARTESIAN_POINT('Ctrl Pts',(-19.0866690470502,21.9726558540769,122.249785576266)) ;
#28339 = CARTESIAN_POINT('Ctrl Pts',(-19.2602098520566,22.1624840353007,121.911823353389)) ;
#28340 = CARTESIAN_POINT('Ctrl Pts',(-19.2900221324471,21.9824949549378,122.211822750592)) ;
#28341 = CARTESIAN_POINT('Ctrl Pts',(-19.5238350449174,22.1725171181664,121.908510218283)) ;
#28342 = CARTESIAN_POINT('Ctrl Pts',(-19.5009223790608,21.9925280378036,122.209172428358)) ;
#28343 = CARTESIAN_POINT('Ctrl Pts',(-19.7836614016497,22.1825388034419,121.951624796669)) ;
#28344 = CARTESIAN_POINT('Ctrl Pts',(-19.7087834435619,22.002549723079,122.243664446075)) ;
#28345 = CARTESIAN_POINT('Ctrl Pts',(-20.0283161574298,22.1924054985404,122.037437936202)) ;
#28346 = CARTESIAN_POINT('Ctrl Pts',(-19.9045062201637,22.0124164181775,122.312314862293)) ;
#28347 = CARTESIAN_POINT('Ctrl Pts',(-20.2568547840646,22.2023653882749,122.165037255751)) ;
#28348 = CARTESIAN_POINT('Ctrl Pts',(-20.0873367614171,22.0223763079121,122.414394197747)) ;
#28349 = CARTESIAN_POINT('Ctrl Pts',(-20.4610185638516,22.2124003761004,122.331922477437)) ;
#28350 = CARTESIAN_POINT('Ctrl Pts',(-20.2506677635409,22.0324112957375,122.547902586744)) ;
#28351 = CARTESIAN_POINT('Ctrl Pts',(-20.6309241388541,22.2222870801747,122.528528183517)) ;
#28352 = CARTESIAN_POINT('Ctrl Pts',(-20.3865915994159,22.0422979998118,122.705186531169)) ;
#28353 = CARTESIAN_POINT('Ctrl Pts',(-20.766416856272,22.2323522244076,122.755640405164)) ;
#28354 = CARTESIAN_POINT('Ctrl Pts',(-20.4949858643928,22.0523631440447,122.88687662059)) ;
#28355 = CARTESIAN_POINT('Ctrl Pts',(-20.8585847061565,22.2421915151362,122.997265190441)) ;
#28356 = CARTESIAN_POINT('Ctrl Pts',(-20.5687197080449,22.0622024347733,123.080175347708)) ;
#28357 = CARTESIAN_POINT('Ctrl Pts',(-20.9088481489483,22.2522540725746,123.256845872699)) ;
#28358 = CARTESIAN_POINT('Ctrl Pts',(-20.6089305940997,22.0722649922117,123.287840171023)) ;
#28359 = CARTESIAN_POINT('Ctrl Pts',(-20.9129252441028,22.2621511238267,123.516913308371)) ;
#28360 = CARTESIAN_POINT('Ctrl Pts',(-20.6121922611426,22.0821620434638,123.495893317472)) ;
#28361 = CARTESIAN_POINT('Ctrl Pts',(-20.8725051637196,22.272082330575,123.774739999813)) ;
#28362 = CARTESIAN_POINT('Ctrl Pts',(-20.5798565101102,22.0920932502121,123.702154136205)) ;
#28363 = CARTESIAN_POINT('Ctrl Pts',(-20.786712131682,22.2821245147938,124.024299304319)) ;
#28364 = CARTESIAN_POINT('Ctrl Pts',(-20.5112221742166,22.1021354344309,123.901801786887)) ;
#28365 = CARTESIAN_POINT('Ctrl Pts',(-20.6610284500015,22.2920111429047,124.25170115506)) ;
#28366 = CARTESIAN_POINT('Ctrl Pts',(-20.4106758246915,22.1120220625418,124.083722603376)) ;
#28367 = CARTESIAN_POINT('Ctrl Pts',(-20.4963649928319,22.3020044154371,124.45625910245)) ;
#28368 = CARTESIAN_POINT('Ctrl Pts',(-20.2789454023778,22.1220153350742,124.247369029717)) ;
#28369 = CARTESIAN_POINT('Ctrl Pts',(-20.2995680280399,22.3119494909786,124.628229064092)) ;
#28370 = CARTESIAN_POINT('Ctrl Pts',(-20.1215083814713,22.1319604106157,124.384944899341)) ;
#28371 = CARTESIAN_POINT('Ctrl Pts',(-20.0760548364874,22.3218990417068,124.763918115327)) ;
#28372 = CARTESIAN_POINT('Ctrl Pts',(-19.9426984210111,22.141909961344,124.493496265617)) ;
#28373 = CARTESIAN_POINT('Ctrl Pts',(-19.8301102215282,22.3319383765548,124.859349625922)) ;
#28374 = CARTESIAN_POINT('Ctrl Pts',(-19.7459427347351,22.1519492961919,124.569841851037)) ;
#28375 = CARTESIAN_POINT('Ctrl Pts',(-19.5752934234394,22.3418245154987,124.910085821145)) ;
#28376 = CARTESIAN_POINT('Ctrl Pts',(-19.5420902200881,22.1618354351359,124.610431044817)) ;
#28377 = CARTESIAN_POINT('Ctrl Pts',(-19.3126560173104,22.3518226284724,124.916205138615)) ;
#28378 = CARTESIAN_POINT('Ctrl Pts',(-19.3319804315117,22.1718335481096,124.615326989773)) ;
#28379 = CARTESIAN_POINT('Ctrl Pts',(-19.0548963059002,22.3617423908249,124.877085616116)) ;
#28380 = CARTESIAN_POINT('Ctrl Pts',(-19.1257731976824,22.181753310462,124.584031994196)) ;
#28381 = CARTESIAN_POINT('Ctrl Pts',(-18.8048804750818,22.3717817864375,124.792892259255)) ;
#28382 = CARTESIAN_POINT('Ctrl Pts',(-18.9257602220697,22.1917927060747,124.51667778619)) ;
#28383 = CARTESIAN_POINT('Ctrl Pts',(-18.5763093840162,22.3816909722258,124.668127742339)) ;
#28384 = CARTESIAN_POINT('Ctrl Pts',(-18.7429037235827,22.2017018918629,124.41686698238)) ;
#28385 = CARTESIAN_POINT('Ctrl Pts',(-18.3718830460784,22.3916261563833,124.505717216813)) ;
#28386 = CARTESIAN_POINT('Ctrl Pts',(-18.5793626191556,22.2116370760204,124.286939448208)) ;
#28387 = CARTESIAN_POINT('Ctrl Pts',(-18.1971172156532,22.4016672137692,124.308030847448)) ;
#28388 = CARTESIAN_POINT('Ctrl Pts',(-18.4395493697844,22.2216781334063,124.128790671233)) ;
#28389 = CARTESIAN_POINT('Ctrl Pts',(-18.0612726927552,22.4115543718025,124.086530580778)) ;
#28390 = CARTESIAN_POINT('Ctrl Pts',(-18.330873593402,22.2315652914396,123.951591529793)) ;
#28391 = CARTESIAN_POINT('Ctrl Pts',(-17.9645436848904,22.4215466514784,123.842428732897)) ;
#28392 = CARTESIAN_POINT('Ctrl Pts',(-18.2534897026088,22.2415575711155,123.756310497809)) ;
#28393 = CARTESIAN_POINT('Ctrl Pts',(-17.9119640315032,22.4314951685235,123.586318714181)) ;
#28394 = CARTESIAN_POINT('Ctrl Pts',(-18.211425301115,22.2515060881606,123.551423064664)) ;
#28395 = CARTESIAN_POINT('Ctrl Pts',(-17.9042933598069,22.4414319460939,123.325324977717)) ;
#28396 = CARTESIAN_POINT('Ctrl Pts',(-18.2052879085007,22.261442865731,123.342628610746)) ;
#28397 = CARTESIAN_POINT('Ctrl Pts',(-17.9419119920911,22.4514149822408,123.065658904093)) ;
#28398 = CARTESIAN_POINT('Ctrl Pts',(-18.235381847005,22.2714259018779,123.134895818999)) ;
#28399 = CARTESIAN_POINT('Ctrl Pts',(-18.0249844510094,22.4614587338345,122.815165001349)) ;
#28400 = CARTESIAN_POINT('Ctrl Pts',(-18.3018390701171,22.2814696534717,122.934500290776)) ;
#28401 = CARTESIAN_POINT('Ctrl Pts',(-18.1471041894676,22.4712872630471,122.587531223368)) ;
#28402 = CARTESIAN_POINT('Ctrl Pts',(-18.3995334548748,22.2912981826842,122.752393822393)) ;
#28403 = CARTESIAN_POINT('Ctrl Pts',(-18.310736925562,22.4813626239558,122.379445782567)) ;
#28404 = CARTESIAN_POINT('Ctrl Pts',(-18.5304390610458,22.3013735435929,122.585924577045)) ;
#28405 = CARTESIAN_POINT('Ctrl Pts',(-18.5037504475988,22.491219222843,122.2066258693)) ;
#28406 = CARTESIAN_POINT('Ctrl Pts',(-18.684848467763,22.3112301424801,122.447668526044)) ;
#28407 = CARTESIAN_POINT('Ctrl Pts',(-18.7282113464719,22.5012822168609,122.066906399844)) ;
#28408 = CARTESIAN_POINT('Ctrl Pts',(-18.8644168289928,22.321293136498,122.335891884029)) ;
#28409 = CARTESIAN_POINT('Ctrl Pts',(-18.9691081441337,22.5111601511503,121.970077874885)) ;
#28410 = CARTESIAN_POINT('Ctrl Pts',(-19.0571331080001,22.3311710707875,122.258428360996)) ;
#28411 = CARTESIAN_POINT('Ctrl Pts',(-19.2261379991879,22.5211607987084,121.915505689096)) ;
#28412 = CARTESIAN_POINT('Ctrl Pts',(-19.2627566457403,22.3411717183456,122.214769480072)) ;
#28413 = CARTESIAN_POINT('Ctrl Pts',(-19.4866516087189,22.5310786451465,121.906267040837)) ;
#28414 = CARTESIAN_POINT('Ctrl Pts',(-19.4711669227681,22.3510895647836,122.207377364757)) ;
#28415 = CARTESIAN_POINT('Ctrl Pts',(-19.7481817747748,22.5411297621521,121.942948938101)) ;
#28416 = CARTESIAN_POINT('Ctrl Pts',(-19.6803913883822,22.3611406817893,122.236721714525)) ;
#28417 = CARTESIAN_POINT('Ctrl Pts',(-19.9950390178656,22.5510004974627,122.022770439589)) ;
#28418 = CARTESIAN_POINT('Ctrl Pts',(-19.8778767883679,22.3710114170999,122.300577456873)) ;
#28419 = CARTESIAN_POINT('Ctrl Pts',(-20.2288742155722,22.5610712047057,122.146611832965)) ;
#28420 = CARTESIAN_POINT('Ctrl Pts',(-20.0649457944915,22.3810821243429,122.399649573841)) ;
#28421 = CARTESIAN_POINT('Ctrl Pts',(-20.432852059648,22.5709042121576,122.305284591667)) ;
#28422 = CARTESIAN_POINT('Ctrl Pts',(-20.2281280611383,22.3909151317947,122.526586124132)) ;
#28423 = CARTESIAN_POINT('Ctrl Pts',(-20.6101957114275,22.5809347044599,122.50028265826)) ;
#28424 = CARTESIAN_POINT('Ctrl Pts',(-20.3700041091279,22.400945624097,122.682583647088)) ;
#28425 = CARTESIAN_POINT('Ctrl Pts',(-20.7503657377508,22.5909662995333,122.723566173364)) ;
#28426 = CARTESIAN_POINT('Ctrl Pts',(-20.4821412655094,22.4109772191704,122.861209824262)) ;
#28427 = CARTESIAN_POINT('Ctrl Pts',(-20.848126630718,22.6007959986715,122.962648437251)) ;
#28428 = CARTESIAN_POINT('Ctrl Pts',(-20.5603509034017,22.4208069183087,123.052474161789)) ;
#28429 = CARTESIAN_POINT('Ctrl Pts',(-20.904551077241,22.6107854485531,123.219033095629)) ;
#28430 = CARTESIAN_POINT('Ctrl Pts',(-20.6054919617955,22.4307963681902,123.257581413107)) ;
#28431 = CARTESIAN_POINT('Ctrl Pts',(-20.9149919746047,22.6208293063688,123.482765312887)) ;
#28432 = CARTESIAN_POINT('Ctrl Pts',(-20.6138461187708,22.4408402260059,123.46856724786)) ;
#28433 = CARTESIAN_POINT('Ctrl Pts',(-20.8807975538298,22.630650996959,123.738595413769)) ;
#28434 = CARTESIAN_POINT('Ctrl Pts',(-20.5864922425363,22.4506619165961,123.673230544663)) ;
#28435 = CARTESIAN_POINT('Ctrl Pts',(-20.8016166335874,22.6406860874994,123.990134218036)) ;
#28436 = CARTESIAN_POINT('Ctrl Pts',(-20.5231490649285,22.4606970071365,123.874462168931)) ;
#28437 = CARTESIAN_POINT('Ctrl Pts',(-20.6794595798729,22.6507106064821,124.223553358068)) ;
#28438 = CARTESIAN_POINT('Ctrl Pts',(-20.4254247725794,22.4707215261192,124.061198201126)) ;
#28439 = CARTESIAN_POINT('Ctrl Pts',(-20.5216428899484,22.6605704518923,124.429030130044)) ;
#28440 = CARTESIAN_POINT('Ctrl Pts',(-20.2991731733227,22.4805813715294,124.22557998796)) ;
#28441 = CARTESIAN_POINT('Ctrl Pts',(-20.3290800370369,22.670530228208,124.606303874563)) ;
#28442 = CARTESIAN_POINT('Ctrl Pts',(-20.1451242645067,22.4905411478451,124.367400086112)) ;
#28443 = CARTESIAN_POINT('Ctrl Pts',(-20.1069583810948,22.6805584255226,124.748107125882)) ;
#28444 = CARTESIAN_POINT('Ctrl Pts',(-19.9674278116215,22.5005693451597,124.480844120942)) ;
#28445 = CARTESIAN_POINT('Ctrl Pts',(-19.8666123895492,22.6904659678129,124.848267265594)) ;
#28446 = CARTESIAN_POINT('Ctrl Pts',(-19.7751521487821,22.51047688745,124.5609736348)) ;
#28447 = CARTESIAN_POINT('Ctrl Pts',(-19.6093776535577,22.7004986183768,124.905971284957)) ;
#28448 = CARTESIAN_POINT('Ctrl Pts',(-19.569364702959,22.5205095380139,124.607138561972)) ;
#28449 = CARTESIAN_POINT('Ctrl Pts',(-19.349909838197,22.7103825748034,124.918032249207)) ;
#28450 = CARTESIAN_POINT('Ctrl Pts',(-19.3617911229907,22.5303934944406,124.616789062543)) ;
#28451 = CARTESIAN_POINT('Ctrl Pts',(-19.0894539708058,22.7203722761653,124.88515179817)) ;
#28452 = CARTESIAN_POINT('Ctrl Pts',(-19.1534263193822,22.5403831958024,124.590486565815)) ;
#28453 = CARTESIAN_POINT('Ctrl Pts',(-18.8375462307077,22.7304132714413,124.806612946757)) ;
#28454 = CARTESIAN_POINT('Ctrl Pts',(-18.9518995301889,22.5504241910784,124.527657156544)) ;
#28455 = CARTESIAN_POINT('Ctrl Pts',(-18.6077694357356,22.7402461607097,124.68841772116)) ;
#28456 = CARTESIAN_POINT('Ctrl Pts',(-18.7680779300007,22.5602570803468,124.4331029628)) ;
#28457 = CARTESIAN_POINT('Ctrl Pts',(-18.3981964690907,22.7502393190771,124.530174726569)) ;
#28458 = CARTESIAN_POINT('Ctrl Pts',(-18.6004184592641,22.5702502387142,124.306510187023)) ;
#28459 = CARTESIAN_POINT('Ctrl Pts',(-18.2189780474116,22.7602713614292,124.336812835409)) ;
#28460 = CARTESIAN_POINT('Ctrl Pts',(-18.457042329262,22.5802822810663,124.151821925346)) ;
#28461 = CARTESIAN_POINT('Ctrl Pts',(-18.078177052041,22.7701366053876,124.11914781899)) ;
#28462 = CARTESIAN_POINT('Ctrl Pts',(-18.3444002370286,22.5901475250248,123.97769144434)) ;
#28463 = CARTESIAN_POINT('Ctrl Pts',(-17.9756297430813,22.7800984966336,123.878272519234)) ;
#28464 = CARTESIAN_POINT('Ctrl Pts',(-18.262360610908,22.6001094162708,123.784992180742)) ;
#28465 = CARTESIAN_POINT('Ctrl Pts',(-17.9164527324428,22.7901333966521,123.621304920688)) ;
#28466 = CARTESIAN_POINT('Ctrl Pts',(-18.2150170837711,22.6101443162892,123.579418516256)) ;
#28467 = CARTESIAN_POINT('Ctrl Pts',(-17.9025653496462,22.8000184770667,123.361873137659)) ;
#28468 = CARTESIAN_POINT('Ctrl Pts',(-18.2039051888414,22.6200293967038,123.371873646667)) ;
#28469 = CARTESIAN_POINT('Ctrl Pts',(-17.9345250196897,22.8100836491915,123.099344214703)) ;
#28470 = CARTESIAN_POINT('Ctrl Pts',(-18.229470937305,22.6300945688287,123.161850152158)) ;
#28471 = CARTESIAN_POINT('Ctrl Pts',(-18.0097882001565,22.819930883915,122.851728714304)) ;
#28472 = CARTESIAN_POINT('Ctrl Pts',(-18.2896793803027,22.6399418035521,122.963757680924)) ;
#28473 = CARTESIAN_POINT('Ctrl Pts',(-18.1285132437623,22.8299616952328,122.616400101498)) ;
#28474 = CARTESIAN_POINT('Ctrl Pts',(-18.3846575488646,22.6499726148699,122.775493825297)) ;
#28475 = CARTESIAN_POINT('Ctrl Pts',(-18.2864226563192,22.8399713111463,122.40599165732)) ;
#28476 = CARTESIAN_POINT('Ctrl Pts',(-18.5109834183892,22.6599822307834,122.607165884196)) ;
#28477 = CARTESIAN_POINT('Ctrl Pts',(-18.4763564295643,22.84988209055,122.227822802769)) ;
#28478 = CARTESIAN_POINT('Ctrl Pts',(-18.6629287774965,22.6698930101871,122.464629519222)) ;
#28479 = CARTESIAN_POINT('Ctrl Pts',(-18.6944202111758,22.859811356339,122.084505529354)) ;
#28480 = CARTESIAN_POINT('Ctrl Pts',(-18.8373784211579,22.6798222759761,122.349974053439)) ;
#28481 = CARTESIAN_POINT('Ctrl Pts',(-18.9368601501301,22.8698540496516,121.980263237278)) ;
#28482 = CARTESIAN_POINT('Ctrl Pts',(-19.0313295614933,22.6898649692887,122.266578267691)) ;
#28483 = CARTESIAN_POINT('Ctrl Pts',(-19.1897096706424,22.8797405823464,121.920470478153)) ;
#28484 = CARTESIAN_POINT('Ctrl Pts',(-19.2336083570812,22.6997515019835,122.218742067114)) ;
#28485 = CARTESIAN_POINT('Ctrl Pts',(-19.4518420605083,22.8897337274496,121.904884777647)) ;
#28486 = CARTESIAN_POINT('Ctrl Pts',(-19.4433140578841,22.7097446470868,122.206271347572)) ;
#28487 = CARTESIAN_POINT('Ctrl Pts',(-19.7114632832621,22.8996794081237,121.935008316747)) ;
#28488 = CARTESIAN_POINT('Ctrl Pts',(-19.6510111009045,22.7196903277608,122.230368013377)) ;
#28489 = CARTESIAN_POINT('Ctrl Pts',(-19.9621146837926,22.9096266657504,122.009255961602)) ;
#28490 = CARTESIAN_POINT('Ctrl Pts',(-19.8515326922247,22.7296375853876,122.289763976907)) ;
#28491 = CARTESIAN_POINT('Ctrl Pts',(-20.1982818352397,22.9196745678719,122.127332902665)) ;
#28492 = CARTESIAN_POINT('Ctrl Pts',(-20.0404673939253,22.739685487509,122.38422358596)) ;
#28493 = CARTESIAN_POINT('Ctrl Pts',(-20.4062715090379,22.9295222734936,122.281319880695)) ;
#28494 = CARTESIAN_POINT('Ctrl Pts',(-20.2068601821527,22.7495331931307,122.507411217)) ;
#28495 = CARTESIAN_POINT('Ctrl Pts',(-20.5870134936696,22.9394837401277,122.470672801482)) ;
#28496 = CARTESIAN_POINT('Ctrl Pts',(-20.3514553209462,22.7594946597648,122.658891935936)) ;
#28497 = CARTESIAN_POINT('Ctrl Pts',(-20.7328386955894,22.9495132933959,122.690234279952)) ;
#28498 = CARTESIAN_POINT('Ctrl Pts',(-20.4681173105457,22.769524213033,122.834539862625)) ;
#28499 = CARTESIAN_POINT('Ctrl Pts',(-20.8371700436695,22.9594201854233,122.928761227148)) ;
#28500 = CARTESIAN_POINT('Ctrl Pts',(-20.5515843614637,22.7794311050604,123.025360373342)) ;
#28501 = CARTESIAN_POINT('Ctrl Pts',(-20.8992391770811,22.9693678295363,123.182677656175)) ;
#28502 = CARTESIAN_POINT('Ctrl Pts',(-20.6012418268376,22.7893787491735,123.228492885336)) ;
#28503 = CARTESIAN_POINT('Ctrl Pts',(-20.9165341377211,22.9793678725652,123.444932969306)) ;
#28504 = CARTESIAN_POINT('Ctrl Pts',(-20.6150800337761,22.7993787922023,123.438296931167)) ;
#28505 = CARTESIAN_POINT('Ctrl Pts',(-20.8874593437994,22.9894066385592,123.707113721901)) ;
#28506 = CARTESIAN_POINT('Ctrl Pts',(-20.5918224275554,22.8094175581963,123.648041733911)) ;
#28507 = CARTESIAN_POINT('Ctrl Pts',(-20.8153966815368,22.9992317005814,123.955064177239)) ;
#28508 = CARTESIAN_POINT('Ctrl Pts',(-20.5341744977842,22.8192426202186,123.846402585896)) ;
#28509 = CARTESIAN_POINT('Ctrl Pts',(-20.6991206973961,23.0092862479078,124.192308936938)) ;
#28510 = CARTESIAN_POINT('Ctrl Pts',(-20.4411557498176,22.8292971675449,124.036199358367)) ;
#28511 = CARTESIAN_POINT('Ctrl Pts',(-20.5447615013441,23.019229491357,124.403151003466)) ;
#28512 = CARTESIAN_POINT('Ctrl Pts',(-20.3176702602204,22.8392404109942,124.204874274932)) ;
#28513 = CARTESIAN_POINT('Ctrl Pts',(-20.357481348229,23.0291316629649,124.583821375332)) ;
#28514 = CARTESIAN_POINT('Ctrl Pts',(-20.1678477266094,22.849142582602,124.349412166951)) ;
#28515 = CARTESIAN_POINT('Ctrl Pts',(-20.1383129462667,23.0391844985751,124.731298547748)) ;
#28516 = CARTESIAN_POINT('Ctrl Pts',(-19.9925143364415,22.8591954182122,124.4673957384)) ;
#28517 = CARTESIAN_POINT('Ctrl Pts',(-19.9012076725115,23.0490575562606,124.836667408501)) ;
#28518 = CARTESIAN_POINT('Ctrl Pts',(-19.8028309876301,22.8690684758978,124.551692871464)) ;
#28519 = CARTESIAN_POINT('Ctrl Pts',(-19.6464624451115,23.0590528177863,124.90066823185)) ;
#28520 = CARTESIAN_POINT('Ctrl Pts',(-19.5990355883761,22.8790637374234,124.602895734181)) ;
#28521 = CARTESIAN_POINT('Ctrl Pts',(-19.3836439744441,23.0690781872068,124.919051527796)) ;
#28522 = CARTESIAN_POINT('Ctrl Pts',(-19.3887803013881,22.8890891068439,124.617604464544)) ;
#28523 = CARTESIAN_POINT('Ctrl Pts',(-19.1251242692714,23.0789680197334,124.892233416081)) ;
#28524 = CARTESIAN_POINT('Ctrl Pts',(-19.1819670497776,22.8989789393705,124.59615274981)) ;
#28525 = CARTESIAN_POINT('Ctrl Pts',(-18.7890035337137,23.0922659905428,124.796782825436)) ;
#28526 = CARTESIAN_POINT('Ctrl Pts',(-18.9130558291102,22.9122769101799,124.519792421691)) ;
#28527 = CARTESIAN_POINT('Ctrl Pts',(-18.4874072190834,23.105464385652,124.617549791502)) ;
#28528 = CARTESIAN_POINT('Ctrl Pts',(-18.6717586476981,22.9254753052891,124.376385659626)) ;
#28529 = CARTESIAN_POINT('Ctrl Pts',(-18.2417519026231,23.1188598279314,124.365440342986)) ;
#28530 = CARTESIAN_POINT('Ctrl Pts',(-18.4752682092803,22.9388707475686,124.1747301264)) ;
#28531 = CARTESIAN_POINT('Ctrl Pts',(-18.0954516814504,23.1287356661704,124.151032241541)) ;
#28532 = CARTESIAN_POINT('Ctrl Pts',(-18.3582189589316,22.9487465858075,124.003198627306)) ;
#28533 = CARTESIAN_POINT('Ctrl Pts',(-17.9865146772214,23.1387970687681,123.910158781384)) ;
#28534 = CARTESIAN_POINT('Ctrl Pts',(-18.2710692167074,22.9588079884053,123.810502898505)) ;
#28535 = CARTESIAN_POINT('Ctrl Pts',(-17.922240462111,23.1486621257033,123.658970587668)) ;
#28536 = CARTESIAN_POINT('Ctrl Pts',(-18.2196477108387,22.9686730453404,123.60955078964)) ;
#28537 = CARTESIAN_POINT('Ctrl Pts',(-17.9018022904604,23.1586742216521,123.396691351192)) ;
#28538 = CARTESIAN_POINT('Ctrl Pts',(-18.2032931318325,22.9786851412892,123.399733036954)) ;
#28539 = CARTESIAN_POINT('Ctrl Pts',(-17.9355630207714,23.1719515307975,123.049376976604)) ;
#28540 = CARTESIAN_POINT('Ctrl Pts',(-18.230309065925,22.9919624504346,123.121854826151)) ;
#28541 = CARTESIAN_POINT('Ctrl Pts',(-18.0899419028751,23.1885505563048,122.636110521846)) ;
#28542 = CARTESIAN_POINT('Ctrl Pts',(-18.3537865821073,23.0085614759419,122.791280237995)) ;
#28543 = CARTESIAN_POINT('Ctrl Pts',(-18.3760258329839,23.2051496043378,122.300311520429)) ;
#28544 = CARTESIAN_POINT('Ctrl Pts',(-18.5826974346445,23.025160523975,122.522589580736)) ;
#28545 = CARTESIAN_POINT('Ctrl Pts',(-18.6623130734036,23.2183930163688,122.102367993719)) ;
#28546 = CARTESIAN_POINT('Ctrl Pts',(-18.8116871062911,23.0384039360059,122.364269513183)) ;
#28547 = CARTESIAN_POINT('Ctrl Pts',(-18.9019676656497,23.2284304440572,121.992209381467)) ;
#28548 = CARTESIAN_POINT('Ctrl Pts',(-19.0034183798067,23.0484413636943,122.27613348672)) ;
#28549 = CARTESIAN_POINT('Ctrl Pts',(-19.1537511180854,23.2383347460128,121.926257438649)) ;
#28550 = CARTESIAN_POINT('Ctrl Pts',(-19.2048396762017,23.0583456656499,122.223371601155)) ;
#28551 = CARTESIAN_POINT('Ctrl Pts',(-19.5011668383559,23.251601585988,121.896906683047)) ;
#28552 = CARTESIAN_POINT('Ctrl Pts',(-19.4827890606653,23.0716125056251,122.199889201105)) ;
#28553 = CARTESIAN_POINT('Ctrl Pts',(-19.9361152832958,23.2682277840779,121.974875772965)) ;
#28554 = CARTESIAN_POINT('Ctrl Pts',(-19.8307319806188,23.088238703715,122.262263124349)) ;
#28555 = CARTESIAN_POINT('Ctrl Pts',(-20.394142712814,23.2881468994613,122.240416456631)) ;
#28556 = CARTESIAN_POINT('Ctrl Pts',(-20.1971528580598,23.1081578190985,122.474678337376)) ;
#28557 = CARTESIAN_POINT('Ctrl Pts',(-20.6777956763041,23.3047533225956,122.578559316856)) ;
#28558 = CARTESIAN_POINT('Ctrl Pts',(-20.4241051196912,23.1247642422327,122.745236815236)) ;
#28559 = CARTESIAN_POINT('Ctrl Pts',(-20.8254141685684,23.3180495430913,122.895260367424)) ;
#28560 = CARTESIAN_POINT('Ctrl Pts',(-20.5421769247472,23.1380604627284,122.998554989249)) ;
#28561 = CARTESIAN_POINT('Ctrl Pts',(-20.9163840285696,23.3313183754327,123.231954203337)) ;
#28562 = CARTESIAN_POINT('Ctrl Pts',(-20.614959974584,23.1513292950698,123.26792816828)) ;
#28563 = CARTESIAN_POINT('Ctrl Pts',(-20.9167633041339,23.3480096234658,123.675476169135)) ;
#28564 = CARTESIAN_POINT('Ctrl Pts',(-20.6152647077734,23.1680205431029,123.622731052057)) ;
#28565 = CARTESIAN_POINT('Ctrl Pts',(-20.7380527826187,23.3678193551386,124.170798980292)) ;
#28566 = CARTESIAN_POINT('Ctrl Pts',(-20.4722993945024,23.1878302747757,124.018996228655)) ;
#28567 = CARTESIAN_POINT('Ctrl Pts',(-20.3990487800684,23.3877969624672,124.579436972735)) ;
#28568 = CARTESIAN_POINT('Ctrl Pts',(-20.2010981192601,23.2078078821043,124.345907297091)) ;
#28569 = CARTESIAN_POINT('Ctrl Pts',(-19.9416700356385,23.407723271525,124.846309372867)) ;
#28570 = CARTESIAN_POINT('Ctrl Pts',(-19.8351962131263,23.2277341911621,124.559408404364)) ;
#28571 = CARTESIAN_POINT('Ctrl Pts',(-19.423672280542,23.4275401316897,124.942420637845)) ;
#28572 = CARTESIAN_POINT('Ctrl Pts',(-19.4207968852883,23.2475510513268,124.636299832249)) ;
#28573 = CARTESIAN_POINT('Ctrl Pts',(-18.897005210854,23.4476399472837,124.853997620555)) ;
#28574 = CARTESIAN_POINT('Ctrl Pts',(-18.9994637104009,23.2676508669208,124.565563970077)) ;
#28575 = CARTESIAN_POINT('Ctrl Pts',(-18.4395858732156,23.4673969111663,124.595670036021)) ;
#28576 = CARTESIAN_POINT('Ctrl Pts',(-18.6335252687433,23.2874078308034,124.358902707329)) ;
#28577 = CARTESIAN_POINT('Ctrl Pts',(-18.0924014778527,23.4874338372357,124.192088863914)) ;
#28578 = CARTESIAN_POINT('Ctrl Pts',(-18.3557767077419,23.3074447568728,124.036039090244)) ;
#28579 = CARTESIAN_POINT('Ctrl Pts',(-17.9060208621862,23.5073034196172,123.697826439083)) ;
#28580 = CARTESIAN_POINT('Ctrl Pts',(-18.206670079505,23.3273143392544,123.64062860021)) ;
#28581 = CARTESIAN_POINT('Ctrl Pts',(-17.8981510516399,23.5272079913704,123.168957382108)) ;
#28582 = CARTESIAN_POINT('Ctrl Pts',(-18.2003731028714,23.3472189110075,123.217532238313)) ;
#28583 = CARTESIAN_POINT('Ctrl Pts',(-18.0717585757874,23.5471605935689,122.667777463739)) ;
#28584 = CARTESIAN_POINT('Ctrl Pts',(-18.3392584148753,23.367171513206,122.816587536918)) ;
#28585 = CARTESIAN_POINT('Ctrl Pts',(-18.4052588840874,23.5670700845392,122.257079257931)) ;
#28586 = CARTESIAN_POINT('Ctrl Pts',(-18.6060587086755,23.3870810041763,122.488027567399)) ;
#28587 = CARTESIAN_POINT('Ctrl Pts',(-18.8570010753677,23.5869214532386,121.984239388305)) ;
#28588 = CARTESIAN_POINT('Ctrl Pts',(-18.9674541463767,23.4069323728757,122.269754763327)) ;
#28589 = CARTESIAN_POINT('Ctrl Pts',(-19.3806182677798,23.6070016493746,121.881570519937)) ;
#28590 = CARTESIAN_POINT('Ctrl Pts',(-19.3863468682687,23.4270125690117,122.187619790065)) ;
#28591 = CARTESIAN_POINT('Ctrl Pts',(-19.9007519851589,23.62680259295,121.962636023239)) ;
#28592 = CARTESIAN_POINT('Ctrl Pts',(-19.8024563004733,23.4468135125871,122.252472687978)) ;
#28593 = CARTESIAN_POINT('Ctrl Pts',(-20.366645013507,23.6467865694595,122.217519363045)) ;
#28594 = CARTESIAN_POINT('Ctrl Pts',(-20.1751704371761,23.4667974890966,122.456380235725)) ;
#28595 = CARTESIAN_POINT('Ctrl Pts',(-20.7158350928187,23.6667025324351,122.615335633075)) ;
#28596 = CARTESIAN_POINT('Ctrl Pts',(-20.4545226369622,23.4867134520722,122.774634459819)) ;
#28597 = CARTESIAN_POINT('Ctrl Pts',(-20.909269753505,23.686572967257,123.106869748193)) ;
#28598 = CARTESIAN_POINT('Ctrl Pts',(-20.6092694713509,23.5065838868942,123.167863591692)) ;
#28599 = CARTESIAN_POINT('Ctrl Pts',(-20.922587690353,23.7066232524901,123.639453176953)) ;
#28600 = CARTESIAN_POINT('Ctrl Pts',(-20.6199224768603,23.5266341721272,123.593929874628)) ;
#28601 = CARTESIAN_POINT('Ctrl Pts',(-20.7562955195823,23.7263972212494,124.138232320058)) ;
#28602 = CARTESIAN_POINT('Ctrl Pts',(-20.4868863698106,23.5464081408865,123.992954730668)) ;
#28603 = CARTESIAN_POINT('Ctrl Pts',(-20.4256681461167,23.746453679369,124.556107455173)) ;
#28604 = CARTESIAN_POINT('Ctrl Pts',(-20.2223831283312,23.5664645990061,124.327253151564)) ;
#28605 = CARTESIAN_POINT('Ctrl Pts',(-19.9777988611578,23.76624856236,124.832456311627)) ;
#28606 = CARTESIAN_POINT('Ctrl Pts',(-19.8640850333811,23.5862594819971,124.548331359068)) ;
#28607 = CARTESIAN_POINT('Ctrl Pts',(-19.4586032621524,23.7862152176623,124.941723989977)) ;
#28608 = CARTESIAN_POINT('Ctrl Pts',(-19.4487277454471,23.6062261372994,124.635742813942)) ;
#28609 = CARTESIAN_POINT('Ctrl Pts',(-18.9333997951415,23.8061741877388,124.86638911577)) ;
#28610 = CARTESIAN_POINT('Ctrl Pts',(-19.0285650781102,23.6261851073759,124.575472274884)) ;
#28611 = CARTESIAN_POINT('Ctrl Pts',(-18.466838553606,23.8260702753289,124.617539311619)) ;
#28612 = CARTESIAN_POINT('Ctrl Pts',(-18.6553167537536,23.6460811949661,124.376389529742)) ;
#28613 = CARTESIAN_POINT('Ctrl Pts',(-18.1127087822637,23.8459684452405,124.224807490326)) ;
#28614 = CARTESIAN_POINT('Ctrl Pts',(-18.3720148240515,23.6659793648776,124.062201436306)) ;
#28615 = CARTESIAN_POINT('Ctrl Pts',(-17.9132245363324,23.8658742806076,123.734750368409)) ;
#28616 = CARTESIAN_POINT('Ctrl Pts',(-18.2124303796564,23.6858852002447,123.670153955737)) ;
#28617 = CARTESIAN_POINT('Ctrl Pts',(-17.8929172316979,23.8858242055455,123.204950398228)) ;
#28618 = CARTESIAN_POINT('Ctrl Pts',(-18.1961880248625,23.7058351251827,123.246313584245)) ;
#28619 = CARTESIAN_POINT('Ctrl Pts',(-18.0536055022471,23.9057033954559,122.701563671004)) ;
#28620 = CARTESIAN_POINT('Ctrl Pts',(-18.3247423344152,23.725714315093,122.843604744158)) ;
#28621 = CARTESIAN_POINT('Ctrl Pts',(-18.3778029519875,23.9256847197365,122.280987362701)) ;
#28622 = CARTESIAN_POINT('Ctrl Pts',(-18.584103378577,23.7456956393736,122.507146042841)) ;
#28623 = CARTESIAN_POINT('Ctrl Pts',(-18.8251843464588,23.9456145039448,121.997171158723)) ;
#28624 = CARTESIAN_POINT('Ctrl Pts',(-18.9420106639801,23.765625423582,122.280096052287)) ;
#28625 = CARTESIAN_POINT('Ctrl Pts',(-19.3420527237489,23.9655344933356,121.8830575886)) ;
#28626 = CARTESIAN_POINT('Ctrl Pts',(-19.3555069146509,23.7855454129728,122.188809484294)) ;
#28627 = CARTESIAN_POINT('Ctrl Pts',(-19.8655341729859,23.9853896886896,121.950798016933)) ;
#28628 = CARTESIAN_POINT('Ctrl Pts',(-19.7742905208817,23.8054006083268,122.243004187493)) ;
#28629 = CARTESIAN_POINT('Ctrl Pts',(-20.3385180584329,24.005435690349,122.195770834828)) ;
#28630 = CARTESIAN_POINT('Ctrl Pts',(-20.1526809568724,23.8254466099861,122.438992919313)) ;
#28631 = CARTESIAN_POINT('Ctrl Pts',(-20.6359495242104,24.0219354375588,122.518207743344)) ;
#28632 = CARTESIAN_POINT('Ctrl Pts',(-20.3906069626951,23.8419463571959,122.696923825608)) ;
#28633 = CARTESIAN_POINT('Ctrl Pts',(-20.7997715920691,24.0353240420069,122.829526935845)) ;
#28634 = CARTESIAN_POINT('Ctrl Pts',(-20.5216768386143,23.855334961644,122.945999782161)) ;
#28635 = CARTESIAN_POINT('Ctrl Pts',(-20.8788004514205,24.0451858703418,123.076353832387)) ;
#28636 = CARTESIAN_POINT('Ctrl Pts',(-20.5848955788943,23.8651967899789,123.143455681254)) ;
#28637 = CARTESIAN_POINT('Ctrl Pts',(-20.9149604443776,24.0551520130994,123.335751428972)) ;
#28638 = CARTESIAN_POINT('Ctrl Pts',(-20.6138199293417,23.8751629327365,123.350985772304)) ;
#28639 = CARTESIAN_POINT('Ctrl Pts',(-20.9016757192965,24.0685137592243,123.68657640661)) ;
#28640 = CARTESIAN_POINT('Ctrl Pts',(-20.6032002770534,23.8885246788614,123.631591920217)) ;
#28641 = CARTESIAN_POINT('Ctrl Pts',(-20.7738010339285,24.0849680881794,124.104947280262)) ;
#28642 = CARTESIAN_POINT('Ctrl Pts',(-20.5008787101127,23.9049790078165,123.966355119094)) ;
#28643 = CARTESIAN_POINT('Ctrl Pts',(-20.506074005893,24.1017353332277,124.460989068715)) ;
#28644 = CARTESIAN_POINT('Ctrl Pts',(-20.2867199296873,23.9217462528648,124.251141688073)) ;
#28645 = CARTESIAN_POINT('Ctrl Pts',(-20.2328267963323,24.1149218985017,124.674311881725)) ;
#28646 = CARTESIAN_POINT('Ctrl Pts',(-20.0681001136612,23.9349328181389,124.421823903416)) ;
#28647 = CARTESIAN_POINT('Ctrl Pts',(-20.0014355866622,24.1249113572463,124.798149275947)) ;
#28648 = CARTESIAN_POINT('Ctrl Pts',(-19.8829901714832,23.9449222768835,124.520886542304)) ;
#28649 = CARTESIAN_POINT('Ctrl Pts',(-19.7528479925732,24.1348651297274,124.879719694348)) ;
#28650 = CARTESIAN_POINT('Ctrl Pts',(-19.6841183272593,23.9548760493646,124.586142147501)) ;
#28651 = CARTESIAN_POINT('Ctrl Pts',(-19.4914820582763,24.1449129462601,124.917021763208)) ;
#28652 = CARTESIAN_POINT('Ctrl Pts',(-19.4750256307248,23.9649238658972,124.615981190194)) ;
#28653 = CARTESIAN_POINT('Ctrl Pts',(-19.2329600579686,24.1547544793826,124.90885452434)) ;
#28654 = CARTESIAN_POINT('Ctrl Pts',(-19.268207989371,23.9747653990197,124.609445249634)) ;
#28655 = CARTESIAN_POINT('Ctrl Pts',(-18.9760140363379,24.1647407216023,124.855708116863)) ;
#28656 = CARTESIAN_POINT('Ctrl Pts',(-19.0626517155432,23.9847516412394,124.566925893019)) ;
#28657 = CARTESIAN_POINT('Ctrl Pts',(-18.7332816198796,24.1746773450272,124.759326036302)) ;
#28658 = CARTESIAN_POINT('Ctrl Pts',(-18.8684666629235,23.9946882646643,124.489818160608)) ;
#28659 = CARTESIAN_POINT('Ctrl Pts',(-18.5085675410313,24.1847272224102,124.620623799681)) ;
#28660 = CARTESIAN_POINT('Ctrl Pts',(-18.6886966289881,24.0047381420473,124.378854470344)) ;
#28661 = CARTESIAN_POINT('Ctrl Pts',(-18.3151003354371,24.1945776611878,124.448610838)) ;
#28662 = CARTESIAN_POINT('Ctrl Pts',(-18.5339244352023,24.0145885808249,124.241242476954)) ;
#28663 = CARTESIAN_POINT('Ctrl Pts',(-18.1519526133633,24.2045496751565,124.243579488805)) ;
#28664 = CARTESIAN_POINT('Ctrl Pts',(-18.4034080760509,24.0245605947936,124.077216069596)) ;
#28665 = CARTESIAN_POINT('Ctrl Pts',(-18.0265886284109,24.2145448437826,124.012717326557)) ;
#28666 = CARTESIAN_POINT('Ctrl Pts',(-18.303118890646,24.0345557634197,123.892525324631)) ;
#28667 = CARTESIAN_POINT('Ctrl Pts',(-17.9432101173695,24.2245787270438,123.762588848226)) ;
#28668 = CARTESIAN_POINT('Ctrl Pts',(-18.2364182327103,24.0445896466809,123.692421857217)) ;
#28669 = CARTESIAN_POINT('Ctrl Pts',(-17.9048199953682,24.2344345971071,123.506429025599)) ;
#28670 = CARTESIAN_POINT('Ctrl Pts',(-18.2057083811246,24.0544455167443,123.487493852008)) ;
#28671 = CARTESIAN_POINT('Ctrl Pts',(-17.9111670277577,24.2444321430243,123.243809194865)) ;
#28672 = CARTESIAN_POINT('Ctrl Pts',(-18.2107882352827,24.0644430626614,123.277398119021)) ;
#28673 = CARTESIAN_POINT('Ctrl Pts',(-17.9624791058961,24.2543402699236,122.988529382377)) ;
#28674 = CARTESIAN_POINT('Ctrl Pts',(-18.2518400388648,24.0743511895607,123.073174891986)) ;
#28675 = CARTESIAN_POINT('Ctrl Pts',(-18.0578908532251,24.2643506414457,122.743365948088)) ;
#28676 = CARTESIAN_POINT('Ctrl Pts',(-18.3281714650137,24.0843615610829,122.877044994232)) ;
#28677 = CARTESIAN_POINT('Ctrl Pts',(-18.1951870356825,24.2743810841931,122.518367543358)) ;
#28678 = CARTESIAN_POINT('Ctrl Pts',(-18.4380103114372,24.0943920038303,122.697047441839)) ;
#28679 = CARTESIAN_POINT('Ctrl Pts',(-18.3658593160879,24.2842290367464,122.323803295538)) ;
#28680 = CARTESIAN_POINT('Ctrl Pts',(-18.574549574067,24.1042399563836,122.541397733003)) ;
#28681 = CARTESIAN_POINT('Ctrl Pts',(-18.5719589574334,24.2942917057674,122.158164871478)) ;
#28682 = CARTESIAN_POINT('Ctrl Pts',(-18.7394306821448,24.1143026254045,122.408888674427)) ;
#28683 = CARTESIAN_POINT('Ctrl Pts',(-18.7999455381362,24.3041860812313,122.033096218261)) ;
#28684 = CARTESIAN_POINT('Ctrl Pts',(-18.9218207704429,24.1241970008685,122.308835803467)) ;
#28685 = CARTESIAN_POINT('Ctrl Pts',(-19.0470862012802,24.3141278795495,121.948467825779)) ;
#28686 = CARTESIAN_POINT('Ctrl Pts',(-19.1195337945076,24.1341387991866,122.24113518591)) ;
#28687 = CARTESIAN_POINT('Ctrl Pts',(-19.306793360523,24.3241303732768,121.9076794678)) ;
#28688 = CARTESIAN_POINT('Ctrl Pts',(-19.3272997862454,24.1441412929139,122.208506614045)) ;
#28689 = CARTESIAN_POINT('Ctrl Pts',(-19.5704262020177,24.3341651717837,121.913035104117)) ;
#28690 = CARTESIAN_POINT('Ctrl Pts',(-19.5382060289476,24.1541760914208,122.212793292696)) ;
#28691 = CARTESIAN_POINT('Ctrl Pts',(-19.8243456090835,24.3440100557631,121.962698662003)) ;
#28692 = CARTESIAN_POINT('Ctrl Pts',(-19.7413407004111,24.1640209754002,122.252526140925)) ;
#28693 = CARTESIAN_POINT('Ctrl Pts',(-20.069363913774,24.3539959125811,122.056545067836)) ;
#28694 = CARTESIAN_POINT('Ctrl Pts',(-19.937354478382,24.1740068322182,122.327605165077)) ;
#28695 = CARTESIAN_POINT('Ctrl Pts',(-20.2933885436929,24.3639307267559,122.190706447143)) ;
#28696 = CARTESIAN_POINT('Ctrl Pts',(-20.1165729005004,24.183941646393,122.434935898804)) ;
#28697 = CARTESIAN_POINT('Ctrl Pts',(-20.4929322997301,24.3739882265412,122.363960667453)) ;
#28698 = CARTESIAN_POINT('Ctrl Pts',(-20.2762066070936,24.1939991461783,122.573540913657)) ;
#28699 = CARTESIAN_POINT('Ctrl Pts',(-20.6558088061112,24.3838099849595,122.564221525997)) ;
#28700 = CARTESIAN_POINT('Ctrl Pts',(-20.4065058327547,24.2038209045966,122.733750399107)) ;
#28701 = CARTESIAN_POINT('Ctrl Pts',(-20.7848399620391,24.3938656427435,122.794804496023)) ;
#28702 = CARTESIAN_POINT('Ctrl Pts',(-20.5097290712294,24.2138765623806,122.918217820985)) ;
#28703 = CARTESIAN_POINT('Ctrl Pts',(-20.8704564403244,24.4038078249235,123.041662828752)) ;
#28704 = CARTESIAN_POINT('Ctrl Pts',(-20.5782202377542,24.2238187445607,123.11570490205)) ;
#28705 = CARTESIAN_POINT('Ctrl Pts',(-20.9125354801232,24.4137130336182,123.298533938)) ;
#28706 = CARTESIAN_POINT('Ctrl Pts',(-20.6118814893409,24.2337239532553,123.321201684156)) ;
#28707 = CARTESIAN_POINT('Ctrl Pts',(-20.909246248355,24.4237548245807,123.562396507273)) ;
#28708 = CARTESIAN_POINT('Ctrl Pts',(-20.6092481539301,24.2437657442178,123.532291786414)) ;
#28709 = CARTESIAN_POINT('Ctrl Pts',(-20.8608714359243,24.4336625990529,123.818239689833)) ;
#28710 = CARTESIAN_POINT('Ctrl Pts',(-20.5705464711203,24.25367351869,123.736965560673)) ;
#28711 = CARTESIAN_POINT('Ctrl Pts',(-20.7683009426795,24.4436740992805,124.064515066611)) ;
#28712 = CARTESIAN_POINT('Ctrl Pts',(-20.496488335269,24.2636850189176,123.933985158452)) ;
#28713 = CARTESIAN_POINT('Ctrl Pts',(-20.6336219825576,24.4537068596732,124.291169915681)) ;
#28714 = CARTESIAN_POINT('Ctrl Pts',(-20.388743464398,24.2737177793103,124.115308070656)) ;
#28715 = CARTESIAN_POINT('Ctrl Pts',(-20.4650972755638,24.4635574288081,124.487670909562)) ;
#28716 = CARTESIAN_POINT('Ctrl Pts',(-20.2539226994214,24.2835683484452,124.272507129792)) ;
#28717 = CARTESIAN_POINT('Ctrl Pts',(-20.262546647733,24.473546038338,124.654592807145)) ;
#28718 = CARTESIAN_POINT('Ctrl Pts',(-20.0918811554699,24.2935569579751,124.40604315333)) ;
#28719 = CARTESIAN_POINT('Ctrl Pts',(-20.035434390892,24.4834746943621,124.783046651201)) ;
#28720 = CARTESIAN_POINT('Ctrl Pts',(-19.910190795979,24.3034856139992,124.508804458404)) ;
#28721 = CARTESIAN_POINT('Ctrl Pts',(-19.788147480938,24.4934624405399,124.871054527459)) ;
#28722 = CARTESIAN_POINT('Ctrl Pts',(-19.7123608220074,24.313473360177,124.579209069275)) ;
#28723 = CARTESIAN_POINT('Ctrl Pts',(-19.5280364525962,24.5034984294756,124.914557400059)) ;
#28724 = CARTESIAN_POINT('Ctrl Pts',(-19.5042716307132,24.3235093491128,124.614009587492)) ;
#28725 = CARTESIAN_POINT('Ctrl Pts',(-19.2690459880752,24.5133532992892,124.912706949231)) ;
#28726 = CARTESIAN_POINT('Ctrl Pts',(-19.2970800077781,24.3333642189264,124.612527489391)) ;
#28727 = CARTESIAN_POINT('Ctrl Pts',(-19.0105743992336,24.523352740531,124.865592193593)) ;
#28728 = CARTESIAN_POINT('Ctrl Pts',(-19.0903031443664,24.3433636601681,124.574834047047)) ;
#28729 = CARTESIAN_POINT('Ctrl Pts',(-18.7666019329129,24.5332478147111,124.775498416424)) ;
#28730 = CARTESIAN_POINT('Ctrl Pts',(-18.8951262877469,24.3532587343482,124.502757699957)) ;
#28731 = CARTESIAN_POINT('Ctrl Pts',(-18.5383021509909,24.5433084705508,124.642232833805)) ;
#28732 = CARTESIAN_POINT('Ctrl Pts',(-18.7124871214675,24.3633193901879,124.39614372167)) ;
#28733 = CARTESIAN_POINT('Ctrl Pts',(-18.3407179161461,24.5531573447464,124.475027408876)) ;
#28734 = CARTESIAN_POINT('Ctrl Pts',(-18.5544214106381,24.3731682643835,124.262378691614)) ;
#28735 = CARTESIAN_POINT('Ctrl Pts',(-18.1716495641239,24.5631860567097,124.272865839476)) ;
#28736 = CARTESIAN_POINT('Ctrl Pts',(-18.4191678481287,24.3831969763468,124.100648461118)) ;
#28737 = CARTESIAN_POINT('Ctrl Pts',(-18.0408595712216,24.5732154572928,124.044039432676)) ;
#28738 = CARTESIAN_POINT('Ctrl Pts',(-18.3145372315862,24.3932263769299,123.917586479356)) ;
#28739 = CARTESIAN_POINT('Ctrl Pts',(-17.9529267054046,24.5830556509096,123.80085466428)) ;
#28740 = CARTESIAN_POINT('Ctrl Pts',(-18.2441926703123,24.4030665705467,123.723039009644)) ;
#28741 = CARTESIAN_POINT('Ctrl Pts',(-17.9073440510645,24.5930590734848,123.541984051105)) ;
#28742 = CARTESIAN_POINT('Ctrl Pts',(-18.2077279538104,24.4130699931219,123.515942359835)) ;
#28743 = CARTESIAN_POINT('Ctrl Pts',(-17.9074876720707,24.6030446105779,123.279530447817)) ;
#28744 = CARTESIAN_POINT('Ctrl Pts',(-18.2078442820345,24.423055530215,123.305979644887)) ;
#28745 = CARTESIAN_POINT('Ctrl Pts',(-17.953701474388,24.6130856150647,123.019767558698)) ;
#28746 = CARTESIAN_POINT('Ctrl Pts',(-18.2448168072216,24.4330965347018,123.098169488521)) ;
#28747 = CARTESIAN_POINT('Ctrl Pts',(-18.0422190940517,24.6229291540059,122.776684574555)) ;
#28748 = CARTESIAN_POINT('Ctrl Pts',(-18.3156319085525,24.442940073643,122.903704466201)) ;
#28749 = CARTESIAN_POINT('Ctrl Pts',(-18.1729536422505,24.6329141849967,122.549220386111)) ;
#28750 = CARTESIAN_POINT('Ctrl Pts',(-18.42022057525,24.4529251046338,122.72173393716)) ;
#28751 = CARTESIAN_POINT('Ctrl Pts',(-18.3403982888488,24.6428536475187,122.348704583029)) ;
#28752 = CARTESIAN_POINT('Ctrl Pts',(-18.5541769923721,24.4628645671558,122.56132244681)) ;
#28753 = CARTESIAN_POINT('Ctrl Pts',(-18.5421236161833,24.6528933797425,122.178692975382)) ;
#28754 = CARTESIAN_POINT('Ctrl Pts',(-18.7155581760706,24.4729042993796,122.425314071837)) ;
#28755 = CARTESIAN_POINT('Ctrl Pts',(-18.766826532383,24.6627815600597,122.048158969798)) ;
#28756 = CARTESIAN_POINT('Ctrl Pts',(-18.8953205045771,24.4827924796968,122.320888330278)) ;
#28757 = CARTESIAN_POINT('Ctrl Pts',(-19.0130885634454,24.6727710757622,121.957251380598)) ;
#28758 = CARTESIAN_POINT('Ctrl Pts',(-19.0923303688238,24.4927819953993,122.248163402219)) ;
#28759 = CARTESIAN_POINT('Ctrl Pts',(-19.2706307855915,24.6827296264169,121.910828202634)) ;
#28760 = CARTESIAN_POINT('Ctrl Pts',(-19.2983640185096,24.502740546054,122.211026103761)) ;
#28761 = CARTESIAN_POINT('Ctrl Pts',(-19.5307897392351,24.6926290335219,121.909185754216)) ;
#28762 = CARTESIAN_POINT('Ctrl Pts',(-19.5064904836855,24.5126399531591,122.209713204043)) ;
#28763 = CARTESIAN_POINT('Ctrl Pts',(-19.7910790035536,24.7026776199382,121.953496342207)) ;
#28764 = CARTESIAN_POINT('Ctrl Pts',(-19.7147218884372,24.5226885395753,122.245162768907)) ;
#28765 = CARTESIAN_POINT('Ctrl Pts',(-20.0360311856884,24.7125704389027,122.040742561825)) ;
#28766 = CARTESIAN_POINT('Ctrl Pts',(-19.9106825930213,24.5325813585398,122.31496045899)) ;
#28767 = CARTESIAN_POINT('Ctrl Pts',(-20.2660472328048,24.7226415564325,122.171540812148)) ;
#28768 = CARTESIAN_POINT('Ctrl Pts',(-20.0946951781208,24.5426524760696,122.419600117649)) ;
#28769 = CARTESIAN_POINT('Ctrl Pts',(-20.4649896868534,24.7324572503985,122.33580820644)) ;
#28770 = CARTESIAN_POINT('Ctrl Pts',(-20.2538475822672,24.5524681700357,122.55101399222)) ;
#28771 = CARTESIAN_POINT('Ctrl Pts',(-20.6368834830163,24.7425236278958,122.536807653796)) ;
#28772 = CARTESIAN_POINT('Ctrl Pts',(-20.3913621437234,24.562534547533,122.711814344018)) ;
#28773 = CARTESIAN_POINT('Ctrl Pts',(-20.7690258159267,24.7524226139777,122.760956322212)) ;
#28774 = CARTESIAN_POINT('Ctrl Pts',(-20.4970748780025,24.5724335336148,122.891133115402)) ;
#28775 = CARTESIAN_POINT('Ctrl Pts',(-20.8617232642626,24.7624767939712,123.008312860307)) ;
#28776 = CARTESIAN_POINT('Ctrl Pts',(-20.5712320948138,24.5824877136083,123.089018856006)) ;
#28777 = CARTESIAN_POINT('Ctrl Pts',(-20.9094544648808,24.7723476069039,123.263341038962)) ;
#28778 = CARTESIAN_POINT('Ctrl Pts',(-20.6094160886339,24.592358526541,123.293040642391)) ;
#28779 = CARTESIAN_POINT('Ctrl Pts',(-20.9122265609454,24.7824215077577,123.527995577717)) ;
#28780 = CARTESIAN_POINT('Ctrl Pts',(-20.6116329563875,24.6024324273948,123.504764628738)) ;
#28781 = CARTESIAN_POINT('Ctrl Pts',(-20.8703860648763,24.7922416631444,123.782706579754)) ;
#28782 = CARTESIAN_POINT('Ctrl Pts',(-20.5781600363798,24.6122525827815,123.708532082081)) ;
#28783 = CARTESIAN_POINT('Ctrl Pts',(-20.7829843523247,24.8023203700966,124.032658419494)) ;
#28784 = CARTESIAN_POINT('Ctrl Pts',(-20.5082379034631,24.6223312897337,123.90849368722)) ;
#28785 = CARTESIAN_POINT('Ctrl Pts',(-20.6564437174401,24.8121719586354,124.258586397133)) ;
#28786 = CARTESIAN_POINT('Ctrl Pts',(-20.4070053415969,24.6321828782725,124.08923482883)) ;
#28787 = CARTESIAN_POINT('Ctrl Pts',(-20.4891628443996,24.8222450751604,124.463680852311)) ;
#28788 = CARTESIAN_POINT('Ctrl Pts',(-20.2731799578671,24.6422559947975,124.253310286516)) ;
#28789 = CARTESIAN_POINT('Ctrl Pts',(-20.2933179390205,24.8320875922562,124.632670356776)) ;
#28790 = CARTESIAN_POINT('Ctrl Pts',(-20.116504494174,24.6520985118933,124.388500688278)) ;
#28791 = CARTESIAN_POINT('Ctrl Pts',(-20.0684748873038,24.8420680538102,124.767681031673)) ;
#28792 = CARTESIAN_POINT('Ctrl Pts',(-19.9366300648084,24.6620789734473,124.496508766413)) ;
#28793 = CARTESIAN_POINT('Ctrl Pts',(-19.8224883546883,24.8520863038009,124.861485946865)) ;
#28794 = CARTESIAN_POINT('Ctrl Pts',(-19.7398406470911,24.6720972234381,124.571552218075)) ;
#28795 = CARTESIAN_POINT('Ctrl Pts',(-19.5674837085229,24.8619704639947,124.911020996683)) ;
#28796 = CARTESIAN_POINT('Ctrl Pts',(-19.535837716226,24.6819813836318,124.611179716792)) ;
#28797 = CARTESIAN_POINT('Ctrl Pts',(-19.3030511330044,24.8720356109697,124.915550386411)) ;
#28798 = CARTESIAN_POINT('Ctrl Pts',(-19.3242913349557,24.6920465306068,124.614802835819)) ;
#28799 = CARTESIAN_POINT('Ctrl Pts',(-19.0475737608601,24.8818774346105,124.875152002711)) ;
#28800 = CARTESIAN_POINT('Ctrl Pts',(-19.1199106517723,24.7018883542476,124.582483957355)) ;
#28801 = CARTESIAN_POINT('Ctrl Pts',(-18.7981220481967,24.8919069070713,124.790082006543)) ;
#28802 = CARTESIAN_POINT('Ctrl Pts',(-18.9203492635413,24.7119178267085,124.514427763563)) ;
#28803 = CARTESIAN_POINT('Ctrl Pts',(-18.5676370265376,24.9019337623334,124.662373648599)) ;
#28804 = CARTESIAN_POINT('Ctrl Pts',(-18.7359613597194,24.7219446819705,124.41226071562)) ;
#28805 = CARTESIAN_POINT('Ctrl Pts',(-18.3661893963596,24.9117770124439,124.500103756191)) ;
#28806 = CARTESIAN_POINT('Ctrl Pts',(-18.5748042848117,24.731787932081,124.282445362066)) ;
#28807 = CARTESIAN_POINT('Ctrl Pts',(-18.1921666070184,24.9218254520271,124.30150622892)) ;
#28808 = CARTESIAN_POINT('Ctrl Pts',(-18.4355860078039,24.7418363716642,124.123567103051)) ;
#28809 = CARTESIAN_POINT('Ctrl Pts',(-18.056967678217,24.931774946275,124.077710500125)) ;
#28810 = CARTESIAN_POINT('Ctrl Pts',(-18.3274273007974,24.7517858659121,123.944530798796)) ;
#28811 = CARTESIAN_POINT('Ctrl Pts',(-17.9623422828139,24.941682802001,123.835129981)) ;
#28812 = CARTESIAN_POINT('Ctrl Pts',(-18.25172727253,24.7616937216381,123.750467050901)) ;
#28813 = CARTESIAN_POINT('Ctrl Pts',(-17.9107761380726,24.9517422786509,123.575884197323)) ;
#28814 = CARTESIAN_POINT('Ctrl Pts',(-18.2104744001724,24.771753198288,123.543070133189)) ;
#28815 = CARTESIAN_POINT('Ctrl Pts',(-17.9047808645182,24.9615830880596,123.317314560702)) ;
#28816 = CARTESIAN_POINT('Ctrl Pts',(-18.2056782172109,24.7815940076967,123.336215598447)) ;
#28817 = CARTESIAN_POINT('Ctrl Pts',(-17.9443132377084,24.9716452383604,123.055891956674)) ;
#28818 = CARTESIAN_POINT('Ctrl Pts',(-18.237304086214,24.7916561579975,123.127077212028)) ;
#28819 = CARTESIAN_POINT('Ctrl Pts',(-18.027522505227,24.981542399483,122.809459900675)) ;
#28820 = CARTESIAN_POINT('Ctrl Pts',(-18.3038712398251,24.8015533191201,122.929932325436)) ;
#28821 = CARTESIAN_POINT('Ctrl Pts',(-18.15191407074,24.991473573887,122.580036852208)) ;
#28822 = CARTESIAN_POINT('Ctrl Pts',(-18.4033840182732,24.8114844935241,122.746394285566)) ;
#28823 = CARTESIAN_POINT('Ctrl Pts',(-18.3162936300384,25.001515777612,122.373591256392)) ;
#28824 = CARTESIAN_POINT('Ctrl Pts',(-18.5348876504328,24.8215266972492,122.581237583697)) ;
#28825 = CARTESIAN_POINT('Ctrl Pts',(-18.5108445770742,25.0114023600425,122.201377852405)) ;
#28826 = CARTESIAN_POINT('Ctrl Pts',(-18.6905276243258,24.8314132796796,122.443467286876)) ;
#28827 = CARTESIAN_POINT('Ctrl Pts',(-18.7344855027603,25.0213957957908,122.063738108185)) ;
#28828 = CARTESIAN_POINT('Ctrl Pts',(-18.8694400641659,24.8414067154279,122.333355312054)) ;
#28829 = CARTESIAN_POINT('Ctrl Pts',(-18.9774777481212,25.031340264149,121.967563232072)) ;
#28830 = CARTESIAN_POINT('Ctrl Pts',(-19.0638333079419,24.8513511837861,122.256415320713)) ;
#28831 = CARTESIAN_POINT('Ctrl Pts',(-19.2335763972328,25.0412920803945,121.914516693683)) ;
#28832 = CARTESIAN_POINT('Ctrl Pts',(-19.2687117105756,24.8613030000317,122.213977773435)) ;
#28833 = CARTESIAN_POINT('Ctrl Pts',(-19.4972265998584,25.051329516509,121.906917954592)) ;
#28834 = CARTESIAN_POINT('Ctrl Pts',(-19.4796319935927,24.8713404361461,122.207898425137)) ;
#28835 = CARTESIAN_POINT('Ctrl Pts',(-19.7542997604475,25.0612144756854,121.944387345544)) ;
#28836 = CARTESIAN_POINT('Ctrl Pts',(-19.6852897308738,24.8812253953225,122.237873404825)) ;
#28837 = CARTESIAN_POINT('Ctrl Pts',(-20.0038315528282,25.0712125938973,122.026544562977)) ;
#28838 = CARTESIAN_POINT('Ctrl Pts',(-19.8849152007323,24.8912235135344,122.303598670447)) ;
#28839 = CARTESIAN_POINT('Ctrl Pts',(-20.2336588620757,25.0811335264093,122.149690526495)) ;
#28840 = CARTESIAN_POINT('Ctrl Pts',(-20.0687767521282,24.9011444460464,122.402114675573)) ;
#28841 = CARTESIAN_POINT('Ctrl Pts',(-20.4411095234431,25.0911748266313,122.31274727971)) ;
#28842 = CARTESIAN_POINT('Ctrl Pts',(-20.2347377340864,24.9111857462685,122.532559732178)) ;
#28843 = CARTESIAN_POINT('Ctrl Pts',(-20.6146855652456,25.1010817450213,122.506787487702)) ;
#28844 = CARTESIAN_POINT('Ctrl Pts',(-20.3735984857151,24.9210926646584,122.687791010339)) ;
#28845 = CARTESIAN_POINT('Ctrl Pts',(-20.7529678400047,25.1110175367304,122.728267052382)) ;
#28846 = CARTESIAN_POINT('Ctrl Pts',(-20.4842246343113,24.9310284563675,122.86497383834)) ;
#28847 = CARTESIAN_POINT('Ctrl Pts',(-20.8514767358832,25.1210584313083,122.973046599286)) ;
#28848 = CARTESIAN_POINT('Ctrl Pts',(-20.5630324089093,24.9410693509454,123.060797371555)) ;
#28849 = CARTESIAN_POINT('Ctrl Pts',(-20.9053425589782,25.1309456330221,123.227241473632)) ;
#28850 = CARTESIAN_POINT('Ctrl Pts',(-20.6061255751286,24.9509565526592,123.264152313877)) ;
#28851 = CARTESIAN_POINT('Ctrl Pts',(-20.9147827032288,25.1409379007837,123.489640019812)) ;
#28852 = CARTESIAN_POINT('Ctrl Pts',(-20.6136784849478,24.9609488204208,123.474070959372)) ;
#28853 = CARTESIAN_POINT('Ctrl Pts',(-20.8786010725189,25.1508864218055,123.748576028363)) ;
#28854 = CARTESIAN_POINT('Ctrl Pts',(-20.5847340147397,24.9708973414426,123.681219445159)) ;
#28855 = CARTESIAN_POINT('Ctrl Pts',(-20.7984664179347,25.1608231953832,123.997081667606)) ;
#28856 = CARTESIAN_POINT('Ctrl Pts',(-20.5206272762469,24.9808341150203,123.880023738464)) ;
#28857 = CARTESIAN_POINT('Ctrl Pts',(-20.6760989906385,25.1708062435242,124.229175844446)) ;
#28858 = CARTESIAN_POINT('Ctrl Pts',(-20.4227342680816,24.9908171631614,124.065699340434)) ;
#28859 = CARTESIAN_POINT('Ctrl Pts',(-20.5139718407011,25.1808499511343,124.437414474404)) ;
#28860 = CARTESIAN_POINT('Ctrl Pts',(-20.2930331145472,25.0008608707714,124.232290876119)) ;
#28861 = CARTESIAN_POINT('Ctrl Pts',(-20.3226951495202,25.1906786442876,124.611032523133)) ;
#28862 = CARTESIAN_POINT('Ctrl Pts',(-20.1400132673799,25.0106895639247,124.371185263449)) ;
#28863 = CARTESIAN_POINT('Ctrl Pts',(-20.098868954127,25.200753393417,124.752367074633)) ;
#28864 = CARTESIAN_POINT('Ctrl Pts',(-19.9609525783771,25.0207643130542,124.484253941825)) ;
#28865 = CARTESIAN_POINT('Ctrl Pts',(-19.858910190644,25.2106187192126,124.850577176108)) ;
#28866 = CARTESIAN_POINT('Ctrl Pts',(-19.7689867940253,25.0306296388497,124.562822605687)) ;
#28867 = CARTESIAN_POINT('Ctrl Pts',(-19.6016970937392,25.2206408935695,124.907156637884)) ;
#28868 = CARTESIAN_POINT('Ctrl Pts',(-19.5632165305531,25.0406518132067,124.608087310509)) ;
#28869 = CARTESIAN_POINT('Ctrl Pts',(-19.33841109203,25.2306669467765,124.91757426496)) ;
#28870 = CARTESIAN_POINT('Ctrl Pts',(-19.3525877130776,25.0506778664136,124.616422422536)) ;
#28871 = CARTESIAN_POINT('Ctrl Pts',(-19.0817846505437,25.2405206436227,124.883149004069)) ;
#28872 = CARTESIAN_POINT('Ctrl Pts',(-19.1472873801373,25.0605315632599,124.588883436946)) ;
#28873 = CARTESIAN_POINT('Ctrl Pts',(-18.8321213569949,25.2504800483757,124.804588928289)) ;
#28874 = CARTESIAN_POINT('Ctrl Pts',(-18.9475566863649,25.0704909680128,124.526036697892)) ;
#28875 = CARTESIAN_POINT('Ctrl Pts',(-18.5982908950502,25.2605182940806,124.68251138002)) ;
#28876 = CARTESIAN_POINT('Ctrl Pts',(-18.7604916748522,25.0805292137177,124.428375651128)) ;
#28877 = CARTESIAN_POINT('Ctrl Pts',(-18.3923032184799,25.2703924782426,124.52465527997)) ;
#28878 = CARTESIAN_POINT('Ctrl Pts',(-18.5957014002325,25.0904033978798,124.302092277131)) ;
#28879 = CARTESIAN_POINT('Ctrl Pts',(-18.2134348354326,25.2804622613806,124.32968799242)) ;
#28880 = CARTESIAN_POINT('Ctrl Pts',(-18.4526055652732,25.1004731810177,124.146119103615)) ;
#28881 = CARTESIAN_POINT('Ctrl Pts',(-18.0743301698985,25.2902955164013,124.111890050986)) ;
#28882 = CARTESIAN_POINT('Ctrl Pts',(-18.341321285219,25.1103064360384,123.971882314404)) ;
#28883 = CARTESIAN_POINT('Ctrl Pts',(-17.9724906536207,25.300325942533,123.868778335182)) ;
#28884 = CARTESIAN_POINT('Ctrl Pts',(-18.2598482995309,25.1203368621701,123.777393441329)) ;
#28885 = CARTESIAN_POINT('Ctrl Pts',(-17.9151462002579,25.31035755472,123.611455902983)) ;
#28886 = CARTESIAN_POINT('Ctrl Pts',(-18.213971454411,25.1303684743571,123.571535713818)) ;
#28887 = CARTESIAN_POINT('Ctrl Pts',(-17.9030533678709,25.3201872515746,123.353441667699)) ;
#28888 = CARTESIAN_POINT('Ctrl Pts',(-18.2042958249843,25.1401981712117,123.365125405049)) ;
#28889 = CARTESIAN_POINT('Ctrl Pts',(-17.935703946638,25.3301766934771,123.092960405583)) ;
#28890 = CARTESIAN_POINT('Ctrl Pts',(-18.2304147144429,25.1501876131142,123.156740340782)) ;
#28891 = CARTESIAN_POINT('Ctrl Pts',(-18.01414488107,25.3402205854928,122.840945210804)) ;
#28892 = CARTESIAN_POINT('Ctrl Pts',(-18.293166125743,25.1602315051299,122.955127645986)) ;
#28893 = CARTESIAN_POINT('Ctrl Pts',(-18.1320014123289,25.350042147262,122.611326074322)) ;
#28894 = CARTESIAN_POINT('Ctrl Pts',(-18.3874495259112,25.1700530668991,122.771432519081)) ;
#28895 = CARTESIAN_POINT('Ctrl Pts',(-18.290812004256,25.3600777188862,122.400775785575)) ;
#28896 = CARTESIAN_POINT('Ctrl Pts',(-18.5144967171378,25.1800886385233,122.602991221329)) ;
#28897 = CARTESIAN_POINT('Ctrl Pts',(-18.4841839838092,25.370106993168,122.221692735608)) ;
#28898 = CARTESIAN_POINT('Ctrl Pts',(-18.6691932985931,25.1901179128051,122.459723641306)) ;
#28899 = CARTESIAN_POINT('Ctrl Pts',(-18.7010269361118,25.3799408302867,122.081101987193)) ;
#28900 = CARTESIAN_POINT('Ctrl Pts',(-18.8426660234848,25.1999517499238,122.347250143643)) ;
#28901 = CARTESIAN_POINT('Ctrl Pts',(-18.9441309444256,25.3899932263748,121.977771975232)) ;
#28902 = CARTESIAN_POINT('Ctrl Pts',(-19.037148711284,25.2100041460119,122.264584503233)) ;
#28903 = CARTESIAN_POINT('Ctrl Pts',(-19.1986250893084,25.3999299933253,121.919230643914)) ;
#28904 = CARTESIAN_POINT('Ctrl Pts',(-19.2407432792532,25.2199409129625,122.21774992714)) ;
#28905 = CARTESIAN_POINT('Ctrl Pts',(-19.459301128586,25.4098642283046,121.905097168243)) ;
#28906 = CARTESIAN_POINT('Ctrl Pts',(-19.4492836234959,25.2298751479417,122.206441411335)) ;
#28907 = CARTESIAN_POINT('Ctrl Pts',(-19.72078773703,25.4198879916314,121.936883279556)) ;
#28908 = CARTESIAN_POINT('Ctrl Pts',(-19.6584731310004,25.2398989112685,122.231868582496)) ;
#28909 = CARTESIAN_POINT('Ctrl Pts',(-19.9693851432808,25.429774333016,122.012355109386)) ;
#28910 = CARTESIAN_POINT('Ctrl Pts',(-19.8573510090563,25.2497852526532,122.292244189265)) ;
#28911 = CARTESIAN_POINT('Ctrl Pts',(-20.2037937296493,25.439763381783,122.130525368287)) ;
#28912 = CARTESIAN_POINT('Ctrl Pts',(-20.0448786033805,25.2597743014202,122.38677867719)) ;
#28913 = CARTESIAN_POINT('Ctrl Pts',(-20.4148854638875,25.4498046024804,122.288855457116)) ;
#28914 = CARTESIAN_POINT('Ctrl Pts',(-20.213753113731,25.2698155221175,122.513441372726)) ;
#28915 = CARTESIAN_POINT('Ctrl Pts',(-20.5918392755866,25.4596372426583,122.477141002139)) ;
#28916 = CARTESIAN_POINT('Ctrl Pts',(-20.3553169822991,25.2796481622954,122.664067990868)) ;
#28917 = CARTESIAN_POINT('Ctrl Pts',(-20.7363655379612,25.4696311719663,122.696425976588)) ;
#28918 = CARTESIAN_POINT('Ctrl Pts',(-20.4709395700862,25.2896420916034,122.839494814172)) ;
#28919 = CARTESIAN_POINT('Ctrl Pts',(-20.8404780632738,25.4796603796468,122.93854969465)) ;
#28920 = CARTESIAN_POINT('Ctrl Pts',(-20.5542313158732,25.2996712992839,123.033193065027)) ;
#28921 = CARTESIAN_POINT('Ctrl Pts',(-20.9004575630717,25.4895361913509,123.191064817286)) ;
#28922 = CARTESIAN_POINT('Ctrl Pts',(-20.6022166706708,25.309547110988,123.235204193094)) ;
#28923 = CARTESIAN_POINT('Ctrl Pts',(-20.9161564441938,25.4995354183223,123.453329386861)) ;
#28924 = CARTESIAN_POINT('Ctrl Pts',(-20.6147777399727,25.3195463379594,123.445015642034)) ;
#28925 = CARTESIAN_POINT('Ctrl Pts',(-20.8865881009697,25.509444899478,123.712094698215)) ;
#28926 = CARTESIAN_POINT('Ctrl Pts',(-20.5911250962336,25.3294558191151,123.65202774278)) ;
#28927 = CARTESIAN_POINT('Ctrl Pts',(-20.81145089258,25.5194981297789,123.965343699702)) ;
#28928 = CARTESIAN_POINT('Ctrl Pts',(-20.5310172244404,25.339509049416,123.854627590473)) ;
#28929 = CARTESIAN_POINT('Ctrl Pts',(-20.6957175422055,25.52936874633,124.197502953534)) ;
#28930 = CARTESIAN_POINT('Ctrl Pts',(-20.438432564313,25.3493796659671,124.040355455078)) ;
#28931 = CARTESIAN_POINT('Ctrl Pts',(-20.5395534186836,25.539390408062,124.409561109384)) ;
#28932 = CARTESIAN_POINT('Ctrl Pts',(-20.3135029430388,25.3594013276991,124.210003211742)) ;
#28933 = CARTESIAN_POINT('Ctrl Pts',(-20.3484908449209,25.5494132212431,124.590878299816)) ;
#28934 = CARTESIAN_POINT('Ctrl Pts',(-20.1606542784881,25.3694241408802,124.355058414572)) ;
#28935 = CARTESIAN_POINT('Ctrl Pts',(-20.1325195803171,25.5592803857031,124.734357216796)) ;
#28936 = CARTESIAN_POINT('Ctrl Pts',(-19.987878794653,25.3792913053402,124.469843008238)) ;
#28937 = CARTESIAN_POINT('Ctrl Pts',(-19.8920996177146,25.569273827923,124.840044812153)) ;
#28938 = CARTESIAN_POINT('Ctrl Pts',(-19.7955437603287,25.3892847475601,124.554394994497)) ;
#28939 = CARTESIAN_POINT('Ctrl Pts',(-19.6358915111173,25.5793055015233,124.902119378316)) ;
#28940 = CARTESIAN_POINT('Ctrl Pts',(-19.5905777624909,25.3993164211604,124.604056661626)) ;
#28941 = CARTESIAN_POINT('Ctrl Pts',(-19.377143513442,25.5891719366363,124.918889100785)) ;
#28942 = CARTESIAN_POINT('Ctrl Pts',(-19.3835799123551,25.4091828562734,124.617474520486)) ;
#28943 = CARTESIAN_POINT('Ctrl Pts',(-19.1162493958071,25.5991593871694,124.890557819024)) ;
#28944 = CARTESIAN_POINT('Ctrl Pts',(-19.1748644832375,25.4191703068065,124.594811646345)) ;
#28945 = CARTESIAN_POINT('Ctrl Pts',(-18.8652039002789,25.6091043169973,124.817783333034)) ;
#28946 = CARTESIAN_POINT('Ctrl Pts',(-18.9740276649419,25.4291152366345,124.536594184406)) ;
#28947 = CARTESIAN_POINT('Ctrl Pts',(-18.6283721225821,25.6191492120525,124.701260743701)) ;
#28948 = CARTESIAN_POINT('Ctrl Pts',(-18.784561279619,25.4391601316896,124.443378036371)) ;
#28949 = CARTESIAN_POINT('Ctrl Pts',(-18.419077049514,25.6290112737383,124.548382059341)) ;
#28950 = CARTESIAN_POINT('Ctrl Pts',(-18.6171242178969,25.4490221933754,124.321077040016)) ;
#28951 = CARTESIAN_POINT('Ctrl Pts',(-18.2367942709095,25.6390029965252,124.359421375143)) ;
#28952 = CARTESIAN_POINT('Ctrl Pts',(-18.4712964601253,25.4590139161623,124.169910079133)) ;
#28953 = CARTESIAN_POINT('Ctrl Pts',(-18.091029495205,25.6489352107651,124.142904444548)) ;
#28954 = CARTESIAN_POINT('Ctrl Pts',(-18.3546829152542,25.4689461304023,123.996697908865)) ;
#28955 = CARTESIAN_POINT('Ctrl Pts',(-17.9844458363519,25.6588745293309,123.904437503963)) ;
#28956 = CARTESIAN_POINT('Ctrl Pts',(-18.2694140074215,25.478885448968,123.805925391818)) ;
#28957 = CARTESIAN_POINT('Ctrl Pts',(-17.9204539831751,25.6689187041067,123.648365609469)) ;
#28958 = CARTESIAN_POINT('Ctrl Pts',(-18.2182183772246,25.4889296237439,123.60106842999)) ;
#28959 = CARTESIAN_POINT('Ctrl Pts',(-17.9020768058315,25.6787892581717,123.389630116784)) ;
#28960 = CARTESIAN_POINT('Ctrl Pts',(-18.2035144291742,25.4988001778088,123.394080402049)) ;
#28961 = CARTESIAN_POINT('Ctrl Pts',(-17.9284060681277,25.6887542405259,123.1290873224)) ;
#28962 = CARTESIAN_POINT('Ctrl Pts',(-18.2245755901221,25.508765160163,123.185646014976)) ;
#28963 = CARTESIAN_POINT('Ctrl Pts',(-18.000430199717,25.6987849434157,122.875529417126)) ;
#28964 = CARTESIAN_POINT('Ctrl Pts',(-18.2821927290592,25.5187958630528,122.98279912396)) ;
#28965 = CARTESIAN_POINT('Ctrl Pts',(-18.1134771988756,25.7086772834409,122.641401239108)) ;
#28966 = CARTESIAN_POINT('Ctrl Pts',(-18.3726282522614,25.528688203078,122.795495711768)) ;
#28967 = CARTESIAN_POINT('Ctrl Pts',(-18.2678679863379,25.7187305166009,122.427066576845)) ;
#28968 = CARTESIAN_POINT('Ctrl Pts',(-18.4961390336313,25.538741436238,122.624026697012)) ;
#28969 = CARTESIAN_POINT('Ctrl Pts',(-18.4538393268546,25.7286117610776,122.245777047898)) ;
#28970 = CARTESIAN_POINT('Ctrl Pts',(-18.6449144658524,25.5486226807147,122.478993530744)) ;
#28971 = CARTESIAN_POINT('Ctrl Pts',(-18.6715752593228,25.7386448819486,122.097176077592)) ;
#28972 = CARTESIAN_POINT('Ctrl Pts',(-18.8191018953641,25.5586558015858,122.360110920692)) ;
#28973 = CARTESIAN_POINT('Ctrl Pts',(-18.9081608033064,25.7485260922237,121.990030737852)) ;
#28974 = CARTESIAN_POINT('Ctrl Pts',(-19.0083693555972,25.5685370118608,122.274392619025)) ;
#28975 = CARTESIAN_POINT('Ctrl Pts',(-19.1642552672847,25.758588167993,121.924365385186)) ;
#28976 = CARTESIAN_POINT('Ctrl Pts',(-19.2132442996693,25.5785990876302,122.2218581685)) ;
#28977 = CARTESIAN_POINT('Ctrl Pts',(-19.4225607860531,25.7684452263748,121.904478285387)) ;
#28978 = CARTESIAN_POINT('Ctrl Pts',(-19.4198885350739,25.5884561460119,122.205946244612)) ;
#28979 = CARTESIAN_POINT('Ctrl Pts',(-19.6839642883553,25.7784397816638,121.929561151871)) ;
#28980 = CARTESIAN_POINT('Ctrl Pts',(-19.6290115124918,25.5984507013009,122.226010297302)) ;
#28981 = CARTESIAN_POINT('Ctrl Pts',(-19.9354025958823,25.7883656691993,121.999101330404)) ;
#28982 = CARTESIAN_POINT('Ctrl Pts',(-19.8301627662093,25.6083765888364,122.281640286907)) ;
#28983 = CARTESIAN_POINT('Ctrl Pts',(-20.1732821454297,25.7983906891946,122.112270545144)) ;
#28984 = CARTESIAN_POINT('Ctrl Pts',(-20.020467298116,25.6184016088317,122.372173604384)) ;
#28985 = CARTESIAN_POINT('Ctrl Pts',(-20.3852412939983,25.8082880662982,122.26301982624)) ;
#28986 = CARTESIAN_POINT('Ctrl Pts',(-20.1900359672413,25.6282989859354,122.49277124775)) ;
#28987 = CARTESIAN_POINT('Ctrl Pts',(-20.5699265939808,25.8182783033791,122.449617357553)) ;
#28988 = CARTESIAN_POINT('Ctrl Pts',(-20.3377857573925,25.6382892230162,122.64204770688)) ;
#28989 = CARTESIAN_POINT('Ctrl Pts',(-20.7196773404664,25.8283149161879,122.666729559919)) ;
#28990 = CARTESIAN_POINT('Ctrl Pts',(-20.4575881296598,25.648325835825,122.815736096847)) ;
#28991 = CARTESIAN_POINT('Ctrl Pts',(-20.8278012350198,25.8381647996059,122.901920140004)) ;
#28992 = CARTESIAN_POINT('Ctrl Pts',(-20.5440893331541,25.658175719243,123.003887861845)) ;
#28993 = CARTESIAN_POINT('Ctrl Pts',(-20.8949727103039,25.8481684165084,123.156051177432)) ;
#28994 = CARTESIAN_POINT('Ctrl Pts',(-20.5978286197024,25.6681793361455,123.207191954639)) ;
#28995 = CARTESIAN_POINT('Ctrl Pts',(-20.9168297433397,25.8581578282735,123.417692998704)) ;
#28996 = CARTESIAN_POINT('Ctrl Pts',(-20.6153163642316,25.6781687479106,123.416505743654)) ;
#28997 = CARTESIAN_POINT('Ctrl Pts',(-20.8926982525151,25.8681765896183,123.67984195633)) ;
#28998 = CARTESIAN_POINT('Ctrl Pts',(-20.5960135622755,25.6881875092555,123.626222991465)) ;
#28999 = CARTESIAN_POINT('Ctrl Pts',(-20.8017581311539,25.8813952649994,124.015153473732)) ;
#29000 = CARTESIAN_POINT('Ctrl Pts',(-20.5232632286193,25.7014061846365,123.894483244612)) ;
#29001 = CARTESIAN_POINT('Ctrl Pts',(-20.6243920028856,25.8947055722441,124.321133430442)) ;
#29002 = CARTESIAN_POINT('Ctrl Pts',(-20.3813483028792,25.7147164918812,124.139291566757)) ;
#29003 = CARTESIAN_POINT('Ctrl Pts',(-20.3779377392562,25.9079432384701,124.566705392269)) ;
#29004 = CARTESIAN_POINT('Ctrl Pts',(-20.1842168620273,25.7279541581072,124.335714004042)) ;
#29005 = CARTESIAN_POINT('Ctrl Pts',(-20.1646098417396,25.9178629338808,124.716521317829)) ;
#29006 = CARTESIAN_POINT('Ctrl Pts',(-20.0135493900519,25.7378738535179,124.455576016923)) ;
#29007 = CARTESIAN_POINT('Ctrl Pts',(-19.9252257840937,25.9279158008794,124.828226044214)) ;
#29008 = CARTESIAN_POINT('Ctrl Pts',(-19.8220451597961,25.7479267205165,124.544939701704)) ;
#29009 = CARTESIAN_POINT('Ctrl Pts',(-19.6751350635831,25.9377712092086,124.895616007158)) ;
#29010 = CARTESIAN_POINT('Ctrl Pts',(-19.6219710432747,25.7577821288458,124.598853833472)) ;
#29011 = CARTESIAN_POINT('Ctrl Pts',(-19.4124225556355,25.9478098408852,124.919414322609)) ;
#29012 = CARTESIAN_POINT('Ctrl Pts',(-19.4118058300607,25.7678207605223,124.617896055851)) ;
#29013 = CARTESIAN_POINT('Ctrl Pts',(-19.0641152659986,25.9611120231522,124.889602889987)) ;
#29014 = CARTESIAN_POINT('Ctrl Pts',(-19.1331381422336,25.7811229427894,124.594040874612)) ;
#29015 = CARTESIAN_POINT('Ctrl Pts',(-18.6502847526992,25.9776570362351,124.740819809691)) ;
#29016 = CARTESIAN_POINT('Ctrl Pts',(-18.8021063710032,25.7976679558722,124.475037523198)) ;
#29017 = CARTESIAN_POINT('Ctrl Pts',(-18.3098802866931,25.9943090523113,124.458074394266)) ;
#29018 = CARTESIAN_POINT('Ctrl Pts',(-18.5297345562069,25.8143199719484,124.248799717003)) ;
#29019 = CARTESIAN_POINT('Ctrl Pts',(-18.1090436808664,26.0075321432166,124.174455573223)) ;
#29020 = CARTESIAN_POINT('Ctrl Pts',(-18.369098690815,25.8275430628537,124.021942719457)) ;
#29021 = CARTESIAN_POINT('Ctrl Pts',(-17.9965176539852,26.0174931027759,123.938117510176)) ;
#29022 = CARTESIAN_POINT('Ctrl Pts',(-18.2790691278245,25.837504022413,123.832864843426)) ;
#29023 = CARTESIAN_POINT('Ctrl Pts',(-17.9266031351628,26.027517899527,123.684128674994)) ;
#29024 = CARTESIAN_POINT('Ctrl Pts',(-18.223137350365,25.8475288191641,123.629678646653)) ;
#29025 = CARTESIAN_POINT('Ctrl Pts',(-17.8934600554389,26.0407423469228,123.338151922398)) ;
#29026 = CARTESIAN_POINT('Ctrl Pts',(-18.1966218500974,25.8607532665599,123.352885080339)) ;
#29027 = CARTESIAN_POINT('Ctrl Pts',(-17.9661098980233,26.0573761316219,122.902122581917)) ;
#29028 = CARTESIAN_POINT('Ctrl Pts',(-18.2547370849816,25.877387051259,123.004073841914)) ;
#29029 = CARTESIAN_POINT('Ctrl Pts',(-18.2260016702492,26.0772787983468,122.441338078492)) ;
#29030 = CARTESIAN_POINT('Ctrl Pts',(-18.4626485568475,25.897289717984,122.6354399701)) ;
#29031 = CARTESIAN_POINT('Ctrl Pts',(-18.6269689740633,26.0971790261287,122.096464789941)) ;
#29032 = CARTESIAN_POINT('Ctrl Pts',(-18.7834208261286,25.9171899457658,122.359539719814)) ;
#29033 = CARTESIAN_POINT('Ctrl Pts',(-19.1218834344603,26.1170965136602,121.908606135804)) ;
#29034 = CARTESIAN_POINT('Ctrl Pts',(-19.1793520415274,25.9371074332973,122.209249695182)) ;
#29035 = CARTESIAN_POINT('Ctrl Pts',(-19.6515421009118,26.1370260394771,121.900579250022)) ;
#29036 = CARTESIAN_POINT('Ctrl Pts',(-19.6030795010678,25.9570369591142,122.202825735213)) ;
#29037 = CARTESIAN_POINT('Ctrl Pts',(-20.1529386123422,26.1569883073634,122.074158377623)) ;
#29038 = CARTESIAN_POINT('Ctrl Pts',(-20.0041977734396,25.9769992270005,122.341686821222)) ;
#29039 = CARTESIAN_POINT('Ctrl Pts',(-20.5634651727886,26.1768785023156,122.407118082729)) ;
#29040 = CARTESIAN_POINT('Ctrl Pts',(-20.3326212396169,25.9968894219527,122.608053440236)) ;
#29041 = CARTESIAN_POINT('Ctrl Pts',(-20.8369695350651,26.1967687470618,122.859653772299)) ;
#29042 = CARTESIAN_POINT('Ctrl Pts',(-20.5514266616668,26.016779666699,122.970082039285)) ;
#29043 = CARTESIAN_POINT('Ctrl Pts',(-20.9394612388346,26.2168431196243,123.383189522101)) ;
#29044 = CARTESIAN_POINT('Ctrl Pts',(-20.6334217424483,26.0368540392614,123.388909499368)) ;
#29045 = CARTESIAN_POINT('Ctrl Pts',(-20.858478621002,26.2366284969846,123.902848054689)) ;
#29046 = CARTESIAN_POINT('Ctrl Pts',(-20.5686369629156,26.0566394166217,123.80463880822)) ;
#29047 = CARTESIAN_POINT('Ctrl Pts',(-20.604272042101,26.2565903710517,124.368482650199)) ;
#29048 = CARTESIAN_POINT('Ctrl Pts',(-20.3652721856668,26.0766012906889,124.177147290224)) ;
#29049 = CARTESIAN_POINT('Ctrl Pts',(-20.2051802401964,26.2765703465422,124.718824795122)) ;
#29050 = CARTESIAN_POINT('Ctrl Pts',(-20.0459994054117,26.0965812661794,124.457422009913)) ;
#29051 = CARTESIAN_POINT('Ctrl Pts',(-19.7149987089246,26.2963827764202,124.911292999828)) ;
#29052 = CARTESIAN_POINT('Ctrl Pts',(-19.6538521960381,26.1163936960573,124.611397916623)) ;
#29053 = CARTESIAN_POINT('Ctrl Pts',(-19.1842547999823,26.3163628845105,124.925735636618)) ;
#29054 = CARTESIAN_POINT('Ctrl Pts',(-19.2292567523326,26.1363738041476,124.622952026166)) ;
#29055 = CARTESIAN_POINT('Ctrl Pts',(-18.6824717518944,26.3362572681077,124.758627144309)) ;
#29056 = CARTESIAN_POINT('Ctrl Pts',(-18.8278291137582,26.1562681877448,124.489264722442)) ;
#29057 = CARTESIAN_POINT('Ctrl Pts',(-18.2670439988586,26.3561841960849,124.430303289928)) ;
#29058 = CARTESIAN_POINT('Ctrl Pts',(-18.4954865238769,26.1761951157221,124.226604620263)) ;
#29059 = CARTESIAN_POINT('Ctrl Pts',(-17.9883141683562,26.3760790533862,123.980817223551)) ;
#29060 = CARTESIAN_POINT('Ctrl Pts',(-18.2725029335029,26.1960899730233,123.867014230406)) ;
#29061 = CARTESIAN_POINT('Ctrl Pts',(-17.8794749235701,26.3961182469898,123.459500138785)) ;
#29062 = CARTESIAN_POINT('Ctrl Pts',(-18.1854325963948,26.2161291666269,123.449960783738)) ;
#29063 = CARTESIAN_POINT('Ctrl Pts',(-17.9544430376458,26.4159582149006,122.937489228161)) ;
#29064 = CARTESIAN_POINT('Ctrl Pts',(-18.2454084587968,26.2359691345377,123.032350471907)) ;
#29065 = CARTESIAN_POINT('Ctrl Pts',(-18.2027276437108,26.4358730318646,122.470081707864)) ;
#29066 = CARTESIAN_POINT('Ctrl Pts',(-18.4440381844851,26.2558839515018,122.658424577818)) ;
#29067 = CARTESIAN_POINT('Ctrl Pts',(-18.596400995126,26.4558152772609,122.115240379138)) ;
#29068 = CARTESIAN_POINT('Ctrl Pts',(-18.7589785547177,26.275826196898,122.374552517246)) ;
#29069 = CARTESIAN_POINT('Ctrl Pts',(-19.0856111707764,26.4756873253754,121.915849802114)) ;
#29070 = CARTESIAN_POINT('Ctrl Pts',(-19.1503485944393,26.2956982450125,122.215041802279)) ;
#29071 = CARTESIAN_POINT('Ctrl Pts',(-19.6169161682822,26.4956983903295,121.895626311636)) ;
#29072 = CARTESIAN_POINT('Ctrl Pts',(-19.57539261041,26.3157093099666,122.198865364486)) ;
#29073 = CARTESIAN_POINT('Ctrl Pts',(-20.118823655691,26.5155099146331,122.055636433992)) ;
#29074 = CARTESIAN_POINT('Ctrl Pts',(-19.9769191395575,26.3355208342703,122.326876501952)) ;
#29075 = CARTESIAN_POINT('Ctrl Pts',(-20.5414187886625,26.5356051265965,122.381904092641)) ;
#29076 = CARTESIAN_POINT('Ctrl Pts',(-20.3149929725486,26.3556160462336,122.587892382152)) ;
#29077 = CARTESIAN_POINT('Ctrl Pts',(-20.8229786362358,26.5553858505163,122.826139617815)) ;
#29078 = CARTESIAN_POINT('Ctrl Pts',(-20.5402392941985,26.3753967701534,122.943283661868)) ;
#29079 = CARTESIAN_POINT('Ctrl Pts',(-20.9383530388371,26.5753769261591,123.344589665565)) ;
#29080 = CARTESIAN_POINT('Ctrl Pts',(-20.6325355740105,26.3953878457962,123.358044462546)) ;
#29081 = CARTESIAN_POINT('Ctrl Pts',(-20.86985320622,26.5952588652021,123.868710610695)) ;
#29082 = CARTESIAN_POINT('Ctrl Pts',(-20.577732355409,26.4152697848392,123.777341477282)) ;
#29083 = CARTESIAN_POINT('Ctrl Pts',(-20.6263804833536,26.6152114697054,124.339726432393)) ;
#29084 = CARTESIAN_POINT('Ctrl Pts',(-20.3829508664611,26.4352223893425,124.154152702177)) ;
#29085 = CARTESIAN_POINT('Ctrl Pts',(-20.2377323609478,26.635110338436,124.698507478413)) ;
#29086 = CARTESIAN_POINT('Ctrl Pts',(-20.0720296498314,26.4551212580731,124.441175303376)) ;
#29087 = CARTESIAN_POINT('Ctrl Pts',(-19.750506384729,26.6550037382456,124.903616092832)) ;
#29088 = CARTESIAN_POINT('Ctrl Pts',(-19.6822465171285,26.4750146578827,124.605258460819)) ;
#29089 = CARTESIAN_POINT('Ctrl Pts',(-19.2219548120851,26.6749128690856,124.930993209538)) ;
#29090 = CARTESIAN_POINT('Ctrl Pts',(-19.2594063325904,26.4949237887228,124.627157492375)) ;
#29091 = CARTESIAN_POINT('Ctrl Pts',(-18.7130356342311,26.6949449688492,124.774763267432)) ;
#29092 = CARTESIAN_POINT('Ctrl Pts',(-18.8522664567341,26.5149558884863,124.502164665301)) ;
#29093 = CARTESIAN_POINT('Ctrl Pts',(-18.3620528555376,26.7114770420187,124.510268121194)) ;
#29094 = CARTESIAN_POINT('Ctrl Pts',(-18.5715001976287,26.5314879616558,124.290581423656)) ;
#29095 = CARTESIAN_POINT('Ctrl Pts',(-18.1460617747501,26.7248123826246,124.234367496516)) ;
#29096 = CARTESIAN_POINT('Ctrl Pts',(-18.3986933386626,26.5448233022617,124.069844646193)) ;
#29097 = CARTESIAN_POINT('Ctrl Pts',(-18.0239800547126,26.7346549411643,124.006303612785)) ;
#29098 = CARTESIAN_POINT('Ctrl Pts',(-18.3010327997462,26.5546658608015,123.887397815469)) ;
#29099 = CARTESIAN_POINT('Ctrl Pts',(-17.9413973813911,26.7447068480142,123.755428033597)) ;
#29100 = CARTESIAN_POINT('Ctrl Pts',(-18.2349681691499,26.5647177676514,123.686685201408)) ;
#29101 = CARTESIAN_POINT('Ctrl Pts',(-17.891686149238,26.7579553624051,123.410787353362)) ;
#29102 = CARTESIAN_POINT('Ctrl Pts',(-18.1952008751101,26.5779662820423,123.411026738166)) ;
#29103 = CARTESIAN_POINT('Ctrl Pts',(-17.9431815127596,26.7745545373529,122.972680824458)) ;
#29104 = CARTESIAN_POINT('Ctrl Pts',(-18.2364062949001,26.59456545699,123.060472645166)) ;
#29105 = CARTESIAN_POINT('Ctrl Pts',(-18.1408483242503,26.7911433231479,122.578566000262)) ;
#29106 = CARTESIAN_POINT('Ctrl Pts',(-18.3945264353871,26.6111542427851,122.745229800877)) ;
#29107 = CARTESIAN_POINT('Ctrl Pts',(-18.3723926843041,26.8044191394899,122.317598644227)) ;
#29108 = CARTESIAN_POINT('Ctrl Pts',(-18.5797786876683,26.624430059127,122.536429224287)) ;
#29109 = CARTESIAN_POINT('Ctrl Pts',(-18.5775216542846,26.8143929902837,122.15442033865)) ;
#29110 = CARTESIAN_POINT('Ctrl Pts',(-18.7438803146688,26.6344039099208,122.405894095803)) ;
#29111 = CARTESIAN_POINT('Ctrl Pts',(-18.8092589677791,26.8244220223761,122.028905565457)) ;
#29112 = CARTESIAN_POINT('Ctrl Pts',(-18.9292719326846,26.6444329420132,122.305482723991)) ;
#29113 = CARTESIAN_POINT('Ctrl Pts',(-19.0557421895212,26.834312147878,121.946421302957)) ;
#29114 = CARTESIAN_POINT('Ctrl Pts',(-19.1264590870646,26.6543230675151,122.239497816618)) ;
#29115 = CARTESIAN_POINT('Ctrl Pts',(-19.3153650354541,26.8443046261495,121.907247691411)) ;
#29116 = CARTESIAN_POINT('Ctrl Pts',(-19.3341577092669,26.6643155457866,122.208161046948)) ;
#29117 = CARTESIAN_POINT('Ctrl Pts',(-19.5768371046668,26.8542558412469,121.913582155201)) ;
#29118 = CARTESIAN_POINT('Ctrl Pts',(-19.5433352791444,26.674266760884,122.213230894477)) ;
#29119 = CARTESIAN_POINT('Ctrl Pts',(-19.8356332457282,26.8643043430019,121.965922317603)) ;
#29120 = CARTESIAN_POINT('Ctrl Pts',(-19.7503716736977,26.6843152626391,122.255105201927)) ;
#29121 = CARTESIAN_POINT('Ctrl Pts',(-20.0765024472187,26.8741456926187,122.060153190044)) ;
#29122 = CARTESIAN_POINT('Ctrl Pts',(-19.9430662458474,26.6941566122558,122.330492010687)) ;
#29123 = CARTESIAN_POINT('Ctrl Pts',(-20.3008378724975,26.8841319836389,122.196241980051)) ;
#29124 = CARTESIAN_POINT('Ctrl Pts',(-20.1225333562957,26.7041429032761,122.439364943551)) ;
#29125 = CARTESIAN_POINT('Ctrl Pts',(-20.4973053062689,26.8940685953675,122.368314358404)) ;
#29126 = CARTESIAN_POINT('Ctrl Pts',(-20.2797057735737,26.7140795150047,122.577024505294)) ;
#29127 = CARTESIAN_POINT('Ctrl Pts',(-20.662628518743,26.9041184707351,122.574234184223)) ;
#29128 = CARTESIAN_POINT('Ctrl Pts',(-20.4119625510863,26.7241293903722,122.741761744443)) ;
#29129 = CARTESIAN_POINT('Ctrl Pts',(-20.7873567686691,26.9139689292705,122.801084418396)) ;
#29130 = CARTESIAN_POINT('Ctrl Pts',(-20.5117431267573,26.7339798489077,122.92324293676)) ;
#29131 = CARTESIAN_POINT('Ctrl Pts',(-20.8724634669083,26.9239408662233,123.048897162386)) ;
#29132 = CARTESIAN_POINT('Ctrl Pts',(-20.5798263274072,26.7439517858604,123.121493774499)) ;
#29133 = CARTESIAN_POINT('Ctrl Pts',(-20.9133152577875,26.9339363231554,123.308411671272)) ;
#29134 = CARTESIAN_POINT('Ctrl Pts',(-20.6125055330845,26.7539472427925,123.329105668054)) ;
#29135 = CARTESIAN_POINT('Ctrl Pts',(-20.9081708679061,26.9439691302085,123.571995622508)) ;
#29136 = CARTESIAN_POINT('Ctrl Pts',(-20.6083877656907,26.7639800498456,123.539972753807)) ;
#29137 = CARTESIAN_POINT('Ctrl Pts',(-20.8585534427238,26.9538290167985,123.826321841959)) ;
#29138 = CARTESIAN_POINT('Ctrl Pts',(-20.5686916578816,26.7738399364356,123.743433118056)) ;
#29139 = CARTESIAN_POINT('Ctrl Pts',(-20.7647835915375,26.9638180973637,124.071480590036)) ;
#29140 = CARTESIAN_POINT('Ctrl Pts',(-20.4936737272855,26.7838290170008,123.939559239062)) ;
#29141 = CARTESIAN_POINT('Ctrl Pts',(-20.6306305349959,26.9737495765729,124.29536007837)) ;
#29142 = CARTESIAN_POINT('Ctrl Pts',(-20.3863494522034,26.79376049621,124.118661555198)) ;
#29143 = CARTESIAN_POINT('Ctrl Pts',(-20.4590264458182,26.9837354360188,124.493916247248)) ;
#29144 = CARTESIAN_POINT('Ctrl Pts',(-20.2490645750113,26.8037463556559,124.277504981672)) ;
#29145 = CARTESIAN_POINT('Ctrl Pts',(-20.254221659418,26.993773586666,124.66014484481)) ;
#29146 = CARTESIAN_POINT('Ctrl Pts',(-20.0852193413478,26.8137845063031,124.410486127387)) ;
#29147 = CARTESIAN_POINT('Ctrl Pts',(-20.0282504284219,27.0036216771704,124.786342691733)) ;
#29148 = CARTESIAN_POINT('Ctrl Pts',(-19.9044415680484,26.8236325968075,124.511442329042)) ;
#29149 = CARTESIAN_POINT('Ctrl Pts',(-19.7786397745395,27.0136825856884,124.873419336829)) ;
#29150 = CARTESIAN_POINT('Ctrl Pts',(-19.7047522927702,26.8336935053255,124.581101595474)) ;
#29151 = CARTESIAN_POINT('Ctrl Pts',(-19.5219286374244,27.0235774328464,124.914963808306)) ;
#29152 = CARTESIAN_POINT('Ctrl Pts',(-19.4993832936596,26.8435883524835,124.614334963387)) ;
#29153 = CARTESIAN_POINT('Ctrl Pts',(-19.2607200330095,27.0335191048914,124.911983091372)) ;
#29154 = CARTESIAN_POINT('Ctrl Pts',(-19.2904166467755,26.8535300245285,124.611948249213)) ;
#29155 = CARTESIAN_POINT('Ctrl Pts',(-19.002340474553,27.0435216320169,124.863486618766)) ;
#29156 = CARTESIAN_POINT('Ctrl Pts',(-19.0837134587159,26.863532551654,124.573148990088)) ;
#29157 = CARTESIAN_POINT('Ctrl Pts',(-18.755708647713,27.0535564232043,124.770193481186)) ;
#29158 = CARTESIAN_POINT('Ctrl Pts',(-18.8864087522121,26.8735673428414,124.498512445791)) ;
#29159 = CARTESIAN_POINT('Ctrl Pts',(-18.53306086531,27.0634013030634,124.63840012197)) ;
#29160 = CARTESIAN_POINT('Ctrl Pts',(-18.7082920013057,26.8834122227005,124.393076157916)) ;
#29161 = CARTESIAN_POINT('Ctrl Pts',(-18.3335903392706,27.0733871836819,124.467951336687)) ;
#29162 = CARTESIAN_POINT('Ctrl Pts',(-18.5487170321478,26.893398103319,124.256715629541)) ;
#29163 = CARTESIAN_POINT('Ctrl Pts',(-18.1673965821684,27.0833219067751,124.266543402248)) ;
#29164 = CARTESIAN_POINT('Ctrl Pts',(-18.4157637799795,26.9033328264122,124.095588174979)) ;
#29165 = CARTESIAN_POINT('Ctrl Pts',(-18.0373591121067,27.0933797470863,124.03648134582)) ;
#29166 = CARTESIAN_POINT('Ctrl Pts',(-18.3117355760186,26.9133906667234,123.911537419721)) ;
#29167 = CARTESIAN_POINT('Ctrl Pts',(-17.9509061764655,27.1032002344828,123.793285094069)) ;
#29168 = CARTESIAN_POINT('Ctrl Pts',(-18.242575359153,26.9232111541199,123.716980330585)) ;
#29169 = CARTESIAN_POINT('Ctrl Pts',(-17.9065238901742,27.1132606358279,123.532692664086)) ;
#29170 = CARTESIAN_POINT('Ctrl Pts',(-18.2070714726686,26.9332715554651,123.508505957209)) ;
#29171 = CARTESIAN_POINT('Ctrl Pts',(-17.9083966530251,27.1231916013808,123.271694164607)) ;
#29172 = CARTESIAN_POINT('Ctrl Pts',(-18.2085717099821,26.943202521018,123.299707472759)) ;
#29173 = CARTESIAN_POINT('Ctrl Pts',(-17.9550143490479,27.1331304637173,123.014732779571)) ;
#29174 = CARTESIAN_POINT('Ctrl Pts',(-18.2458677394245,26.9531413833544,123.094139009809)) ;
#29175 = CARTESIAN_POINT('Ctrl Pts',(-18.0458227293772,27.1431161946435,122.768499870868)) ;
#29176 = CARTESIAN_POINT('Ctrl Pts',(-18.3185162096812,26.9631271142806,122.897153472277)) ;
#29177 = CARTESIAN_POINT('Ctrl Pts',(-18.1787338062467,27.1531405800709,122.54108010085)) ;
#29178 = CARTESIAN_POINT('Ctrl Pts',(-18.4248467768607,26.9731514997081,122.715218646662)) ;
#29179 = CARTESIAN_POINT('Ctrl Pts',(-18.3467863406668,27.1630438644242,122.342321573022)) ;
#29180 = CARTESIAN_POINT('Ctrl Pts',(-18.5592899783311,26.9830547840613,122.556213402555)) ;
#29181 = CARTESIAN_POINT('Ctrl Pts',(-18.5499675318017,27.1731038690022,122.173235543931)) ;
#29182 = CARTESIAN_POINT('Ctrl Pts',(-18.7218362738242,26.9931147886393,122.420945971278)) ;
#29183 = CARTESIAN_POINT('Ctrl Pts',(-18.7744378365037,27.1829471380713,122.044638016558)) ;
#29184 = CARTESIAN_POINT('Ctrl Pts',(-18.9014128616889,27.0029580577084,122.318069943643)) ;
#29185 = CARTESIAN_POINT('Ctrl Pts',(-19.0212070083882,27.192937703679,121.955103241881)) ;
#29186 = CARTESIAN_POINT('Ctrl Pts',(-19.0988286849585,27.0129486233161,122.246443874494)) ;
#29187 = CARTESIAN_POINT('Ctrl Pts',(-19.2782077784814,27.2028658354578,121.910092465526)) ;
#29188 = CARTESIAN_POINT('Ctrl Pts',(-19.3044292293712,27.022876755095,122.210437108631)) ;
#29189 = CARTESIAN_POINT('Ctrl Pts',(-19.5406906769413,27.2128537225387,121.909933250644)) ;
#29190 = CARTESIAN_POINT('Ctrl Pts',(-19.5144154029953,27.0328646421759,122.210311478194)) ;
#29191 = CARTESIAN_POINT('Ctrl Pts',(-19.8003580009036,27.2228896721074,121.956008127035)) ;
#29192 = CARTESIAN_POINT('Ctrl Pts',(-19.7221490136593,27.0429005917445,122.247173180015)) ;
#29193 = CARTESIAN_POINT('Ctrl Pts',(-20.0437890490973,27.2327445584862,122.044444124203)) ;
#29194 = CARTESIAN_POINT('Ctrl Pts',(-19.9168925651677,27.0527554781234,122.317923364294)) ;
#29195 = CARTESIAN_POINT('Ctrl Pts',(-20.2715790260407,27.2427439728341,122.175359156114)) ;
#29196 = CARTESIAN_POINT('Ctrl Pts',(-20.0991236143385,27.0627548924712,122.422656796826)) ;
#29197 = CARTESIAN_POINT('Ctrl Pts',(-20.47132188163,27.2526391380246,122.341923187153)) ;
#29198 = CARTESIAN_POINT('Ctrl Pts',(-20.2589164031302,27.0726500576617,122.555908896478)) ;
#29199 = CARTESIAN_POINT('Ctrl Pts',(-20.6418377253297,27.2626994567166,122.543912452748)) ;
#29200 = CARTESIAN_POINT('Ctrl Pts',(-20.3953279507184,27.0827103763537,122.717501514616)) ;
#29201 = CARTESIAN_POINT('Ctrl Pts',(-20.7720769168341,27.2725495884926,122.767639569015)) ;
#29202 = CARTESIAN_POINT('Ctrl Pts',(-20.4995174924838,27.0925605081298,122.89648329143)) ;
#29203 = CARTESIAN_POINT('Ctrl Pts',(-20.8637005068752,27.2825801589429,123.014783157539)) ;
#29204 = CARTESIAN_POINT('Ctrl Pts',(-20.5728149832003,27.10259107858,123.094198725936)) ;
#29205 = CARTESIAN_POINT('Ctrl Pts',(-20.9103706252309,27.2925943096157,123.273787983254)) ;
#29206 = CARTESIAN_POINT('Ctrl Pts',(-20.6101494956889,27.1126052292528,123.301402858841)) ;
#29207 = CARTESIAN_POINT('Ctrl Pts',(-20.911768495837,27.3024872431611,123.533764947733)) ;
#29208 = CARTESIAN_POINT('Ctrl Pts',(-20.6112662665047,27.1224981627982,123.509383800559)) ;
#29209 = CARTESIAN_POINT('Ctrl Pts',(-20.8678776029836,27.3124767571514,123.792558185261)) ;
#29210 = CARTESIAN_POINT('Ctrl Pts',(-20.5761521325388,27.1324876767885,123.716417986733)) ;
#29211 = CARTESIAN_POINT('Ctrl Pts',(-20.7801754400193,27.3224305278038,124.03903194835)) ;
#29212 = CARTESIAN_POINT('Ctrl Pts',(-20.505989170069,27.1424414474409,123.913596190151)) ;
#29213 = CARTESIAN_POINT('Ctrl Pts',(-20.6496157399914,27.3324782964644,124.26850963764)) ;
#29214 = CARTESIAN_POINT('Ctrl Pts',(-20.4015400481253,27.1524892161015,124.097177744708)) ;
#29215 = CARTESIAN_POINT('Ctrl Pts',(-20.4848531000536,27.3423200229042,124.467895083723)) ;
#29216 = CARTESIAN_POINT('Ctrl Pts',(-20.2697294497831,27.1623309425413,124.256684466489)) ;
#29217 = CARTESIAN_POINT('Ctrl Pts',(-20.2855162962699,27.3523055397269,124.638488743857)) ;
#29218 = CARTESIAN_POINT('Ctrl Pts',(-20.1102593118314,27.172316459364,124.393158279408)) ;
#29219 = CARTESIAN_POINT('Ctrl Pts',(-20.0606131128351,27.3622448714225,124.771385186807)) ;
#29220 = CARTESIAN_POINT('Ctrl Pts',(-19.9303364915707,27.1822557910596,124.499474112979)) ;
#29221 = CARTESIAN_POINT('Ctrl Pts',(-19.8136159800649,27.37228464112,124.864066326302)) ;
#29222 = CARTESIAN_POINT('Ctrl Pts',(-19.7327382216027,27.1922955607571,124.57361785765)) ;
#29223 = CARTESIAN_POINT('Ctrl Pts',(-19.5581817302825,27.3821728023688,124.911855032732)) ;
#29224 = CARTESIAN_POINT('Ctrl Pts',(-19.5283913156951,27.2021837220059,124.61184744574)) ;
#29225 = CARTESIAN_POINT('Ctrl Pts',(-19.2956955404914,27.3921623568712,124.915085978907)) ;
#29226 = CARTESIAN_POINT('Ctrl Pts',(-19.318402520903,27.2121732765083,124.614431045079)) ;
#29227 = CARTESIAN_POINT('Ctrl Pts',(-19.0374725439821,27.4021207713948,124.872626590807)) ;
#29228 = CARTESIAN_POINT('Ctrl Pts',(-19.1118246609645,27.222131691032,124.580462405806)) ;
#29229 = CARTESIAN_POINT('Ctrl Pts',(-18.7917647458714,27.4120206842242,124.787079499337)) ;
#29230 = CARTESIAN_POINT('Ctrl Pts',(-18.9152594335383,27.2320316038613,124.51202396635)) ;
#29231 = CARTESIAN_POINT('Ctrl Pts',(-18.5613480077617,27.4220673838741,124.658240132733)) ;
#29232 = CARTESIAN_POINT('Ctrl Pts',(-18.7309264191264,27.2420783035112,124.40895145111)) ;
#29233 = CARTESIAN_POINT('Ctrl Pts',(-18.3596364546277,27.4319672441797,124.493876043428)) ;
#29234 = CARTESIAN_POINT('Ctrl Pts',(-18.5695583841052,27.2519781638168,124.277459828361)) ;
#29235 = CARTESIAN_POINT('Ctrl Pts',(-18.186909253097,27.4420186483852,124.294086730336)) ;
#29236 = CARTESIAN_POINT('Ctrl Pts',(-18.4313772630263,27.2620295680223,124.117627563925)) ;
#29237 = CARTESIAN_POINT('Ctrl Pts',(-18.0536713291326,27.4518996853063,124.071168267617)) ;
#29238 = CARTESIAN_POINT('Ctrl Pts',(-18.3247881999234,27.2719106049434,123.939292985394)) ;
#29239 = CARTESIAN_POINT('Ctrl Pts',(-17.9597465513536,27.4618995174838,123.825788262627)) ;
#29240 = CARTESIAN_POINT('Ctrl Pts',(-18.24964927092,27.2819104371209,123.742988761484)) ;
#29241 = CARTESIAN_POINT('Ctrl Pts',(-17.9100347106082,27.4718175204687,123.56989145949)) ;
#29242 = CARTESIAN_POINT('Ctrl Pts',(-18.2098807623671,27.2918284401058,123.538271752722)) ;
#29243 = CARTESIAN_POINT('Ctrl Pts',(-17.9055372820663,27.4818688263432,123.305836914717)) ;
#29244 = CARTESIAN_POINT('Ctrl Pts',(-18.2062837024167,27.3018797459804,123.327027911082)) ;
#29245 = CARTESIAN_POINT('Ctrl Pts',(-17.9459117765369,27.4917386497348,123.049572996332)) ;
#29246 = CARTESIAN_POINT('Ctrl Pts',(-18.2385839520129,27.3117495693719,123.122017805772)) ;
#29247 = CARTESIAN_POINT('Ctrl Pts',(-18.0318915985893,27.5018128157851,122.799249602971)) ;
#29248 = CARTESIAN_POINT('Ctrl Pts',(-18.3073686920026,27.3218237354222,122.921759028966)) ;
#29249 = CARTESIAN_POINT('Ctrl Pts',(-18.1565773494833,27.5116328999267,122.573239483822)) ;
#29250 = CARTESIAN_POINT('Ctrl Pts',(-18.4071173341134,27.3316438195639,122.740952378761)) ;
#29251 = CARTESIAN_POINT('Ctrl Pts',(-18.3226042808018,27.5217116266626,122.366962086733)) ;
#29252 = CARTESIAN_POINT('Ctrl Pts',(-18.5399396427468,27.3417225462997,122.575930590935)) ;
#29253 = CARTESIAN_POINT('Ctrl Pts',(-18.5174703780383,27.5315632073121,122.196424414338)) ;
#29254 = CARTESIAN_POINT('Ctrl Pts',(-18.6958321561076,27.3515741269492,122.439501639971)) ;
#29255 = CARTESIAN_POINT('Ctrl Pts',(-18.7437532834736,27.5416363356105,122.05915550415)) ;
#29256 = CARTESIAN_POINT('Ctrl Pts',(-18.8768590906674,27.3616472552476,122.329686841586)) ;
#29257 = CARTESIAN_POINT('Ctrl Pts',(-18.9848658829686,27.5514788135019,121.965469396346)) ;
#29258 = CARTESIAN_POINT('Ctrl Pts',(-19.0697483336544,27.3714897331391,122.25473893346)) ;
#29259 = CARTESIAN_POINT('Ctrl Pts',(-19.2419340497948,27.5614594201,121.913511275121)) ;
#29260 = CARTESIAN_POINT('Ctrl Pts',(-19.2754027022882,27.3814703397371,122.213172868281)) ;
#29261 = CARTESIAN_POINT('Ctrl Pts',(-19.505118136635,27.5714771291188,121.907449255122)) ;
#29262 = CARTESIAN_POINT('Ctrl Pts',(-19.4859499875362,27.3914880487559,122.208323766678)) ;
#29263 = CARTESIAN_POINT('Ctrl Pts',(-19.7620374996728,27.5813633081562,121.946159440311)) ;
#29264 = CARTESIAN_POINT('Ctrl Pts',(-19.6914845708838,27.4013742277934,122.239292171034)) ;
#29265 = CARTESIAN_POINT('Ctrl Pts',(-20.0125674013974,27.5914209207286,122.030295059284)) ;
#29266 = CARTESIAN_POINT('Ctrl Pts',(-19.8919086080025,27.4114318403657,122.306601108605)) ;
#29267 = CARTESIAN_POINT('Ctrl Pts',(-20.2405477178494,27.6012973141007,122.154372035112)) ;
#29268 = CARTESIAN_POINT('Ctrl Pts',(-20.0742918644194,27.4213082337378,122.405862575282)) ;
#29269 = CARTESIAN_POINT('Ctrl Pts',(-20.4463485472987,27.6112923422511,122.317564461287)) ;
#29270 = CARTESIAN_POINT('Ctrl Pts',(-20.2389322836839,27.4313032618883,122.53641659574)) ;
#29271 = CARTESIAN_POINT('Ctrl Pts',(-20.6208115759906,27.6213130890971,122.51483046535)) ;
#29272 = CARTESIAN_POINT('Ctrl Pts',(-20.3785024861279,27.4413240087343,122.694229642115)) ;
#29273 = CARTESIAN_POINT('Ctrl Pts',(-20.7569960330264,27.6312151577635,122.736562250952)) ;
#29274 = CARTESIAN_POINT('Ctrl Pts',(-20.4874494348297,27.4512260774006,122.871614548114)) ;
#29275 = CARTESIAN_POINT('Ctrl Pts',(-20.8538296011518,27.6412058975832,122.980600241119)) ;
#29276 = CARTESIAN_POINT('Ctrl Pts',(-20.5649160765477,27.4612168172203,123.066844821881)) ;
#29277 = CARTESIAN_POINT('Ctrl Pts',(-20.9064812123952,27.6511690937935,123.237061229662)) ;
#29278 = CARTESIAN_POINT('Ctrl Pts',(-20.6070370952218,27.4711800134306,123.272013299712)) ;
#29279 = CARTESIAN_POINT('Ctrl Pts',(-20.9144047817725,27.6610732780936,123.497236530681)) ;
#29280 = CARTESIAN_POINT('Ctrl Pts',(-20.6133758900281,27.4810841977308,123.480152789572)) ;
#29281 = CARTESIAN_POINT('Ctrl Pts',(-20.8762301626549,27.6711337384845,123.758811110914)) ;
#29282 = CARTESIAN_POINT('Ctrl Pts',(-20.5828360598664,27.4911446581216,123.689412720083)) ;
#29283 = CARTESIAN_POINT('Ctrl Pts',(-20.7953249519176,27.6809742843553,124.004465402187)) ;
#29284 = CARTESIAN_POINT('Ctrl Pts',(-20.5181122497151,27.5009852039924,123.88593503245)) ;
#29285 = CARTESIAN_POINT('Ctrl Pts',(-20.6705674371017,27.6910365050671,124.237576347375)) ;
#29286 = CARTESIAN_POINT('Ctrl Pts',(-20.4183061644665,27.5110474247042,124.072424084696)) ;
#29287 = CARTESIAN_POINT('Ctrl Pts',(-20.5096693378974,27.7009336480836,124.441939302609)) ;
#29288 = CARTESIAN_POINT('Ctrl Pts',(-20.2895881841943,27.5209445677207,124.235913821433)) ;
#29289 = CARTESIAN_POINT('Ctrl Pts',(-20.315658373556,27.7108648245008,124.61649018712)) ;
#29290 = CARTESIAN_POINT('Ctrl Pts',(-20.1343799929666,27.5308757441379,124.375554311888)) ;
#29291 = CARTESIAN_POINT('Ctrl Pts',(-20.091657303987,27.7209070382794,124.756002912722)) ;
#29292 = CARTESIAN_POINT('Ctrl Pts',(-19.9551790760134,27.5409179579165,124.487164709501)) ;
#29293 = CARTESIAN_POINT('Ctrl Pts',(-19.8506842942627,27.7307935784821,124.85316185408)) ;
#29294 = CARTESIAN_POINT('Ctrl Pts',(-19.7624015506141,27.5508044981193,124.564891723896)) ;
#29295 = CARTESIAN_POINT('Ctrl Pts',(-19.5938710456304,27.7407871730876,124.907993194414)) ;
#29296 = CARTESIAN_POINT('Ctrl Pts',(-19.5569511707671,27.5607980927247,124.608757063164)) ;
#29297 = CARTESIAN_POINT('Ctrl Pts',(-19.3327071093546,27.7507310482451,124.917315275339)) ;
#29298 = CARTESIAN_POINT('Ctrl Pts',(-19.3480205279212,27.5707419678822,124.616215008341)) ;
#29299 = CARTESIAN_POINT('Ctrl Pts',(-19.0734423500519,27.7606915843599,124.881432829596)) ;
#29300 = CARTESIAN_POINT('Ctrl Pts',(-19.1406090425669,27.5807025039971,124.587509484983)) ;
#29301 = CARTESIAN_POINT('Ctrl Pts',(-18.823353749831,27.7706881876827,124.800925220385)) ;
#29302 = CARTESIAN_POINT('Ctrl Pts',(-18.9405381483672,27.5906991073198,124.523103835156)) ;
#29303 = CARTESIAN_POINT('Ctrl Pts',(-18.5903995182117,27.7807212706372,124.677453935382)) ;
#29304 = CARTESIAN_POINT('Ctrl Pts',(-18.7541745110723,27.6007321902743,124.424327045669)) ;
#29305 = CARTESIAN_POINT('Ctrl Pts',(-18.3859904696139,27.7905724393387,124.518604840361)) ;
#29306 = CARTESIAN_POINT('Ctrl Pts',(-18.5906478871506,27.6105833589758,124.297248765221)) ;
#29307 = CARTESIAN_POINT('Ctrl Pts',(-18.2097360022858,27.8005349300376,124.325031213336)) ;
#29308 = CARTESIAN_POINT('Ctrl Pts',(-18.4496441165959,27.6205458496747,124.142390542805)) ;
#29309 = CARTESIAN_POINT('Ctrl Pts',(-18.0691061956658,27.8105633584554,124.102135115778)) ;
#29310 = CARTESIAN_POINT('Ctrl Pts',(-18.3371397875157,27.6305742780925,123.964073876923)) ;
#29311 = CARTESIAN_POINT('Ctrl Pts',(-17.9704213296521,27.8204737258199,123.861134793012)) ;
#29312 = CARTESIAN_POINT('Ctrl Pts',(-18.2581916587335,27.640484645457,123.771274472976)) ;
#29313 = CARTESIAN_POINT('Ctrl Pts',(-17.9142719852206,27.830408593435,123.606158130962)) ;
#29314 = CARTESIAN_POINT('Ctrl Pts',(-18.2132716018524,27.6504195130721,123.567293812213)) ;
#29315 = CARTESIAN_POINT('Ctrl Pts',(-17.9033759753097,27.840449735414,123.342521266579)) ;
#29316 = CARTESIAN_POINT('Ctrl Pts',(-18.2045541379343,27.6604606550512,123.356384198053)) ;
#29317 = CARTESIAN_POINT('Ctrl Pts',(-17.9377060396121,27.8503368716172,123.084960416994)) ;
#29318 = CARTESIAN_POINT('Ctrl Pts',(-18.2320173908359,27.6703477912543,123.150336250561)) ;
#29319 = CARTESIAN_POINT('Ctrl Pts',(-18.0166431581778,27.8603291540206,122.834538577221)) ;
#29320 = CARTESIAN_POINT('Ctrl Pts',(-18.2951662729315,27.6803400736577,122.94999869318)) ;
#29321 = CARTESIAN_POINT('Ctrl Pts',(-18.137412126526,27.8702776819858,122.602650848213)) ;
#29322 = CARTESIAN_POINT('Ctrl Pts',(-18.3917805539364,27.6902886016229,122.764488533233)) ;
#29323 = CARTESIAN_POINT('Ctrl Pts',(-18.2961056898845,27.8802144131479,122.395304507949)) ;
#29324 = CARTESIAN_POINT('Ctrl Pts',(-18.5187344032728,27.7002253327851,122.598611336762)) ;
#29325 = CARTESIAN_POINT('Ctrl Pts',(-18.4891076721817,27.8901976240079,122.217558370946)) ;
#29326 = CARTESIAN_POINT('Ctrl Pts',(-18.6731351964962,27.710208543645,122.456413869143)) ;
#29327 = CARTESIAN_POINT('Ctrl Pts',(-18.7115707177152,27.9002407231578,122.075605016214)) ;
#29328 = CARTESIAN_POINT('Ctrl Pts',(-18.8511053106445,27.7202516427949,122.342850400546)) ;
#29329 = CARTESIAN_POINT('Ctrl Pts',(-18.9499871891245,27.9100716874327,121.976015433695)) ;
#29330 = CARTESIAN_POINT('Ctrl Pts',(-19.041837051544,27.7300826070698,122.263178278936)) ;
#29331 = CARTESIAN_POINT('Ctrl Pts',(-19.2081615249894,27.9201445398186,121.917767583989)) ;
#29332 = CARTESIAN_POINT('Ctrl Pts',(-19.2483766156714,27.7401554594558,122.216578932533)) ;
#29333 = CARTESIAN_POINT('Ctrl Pts',(-19.4671216625185,27.9300086675304,121.905533740892)) ;
#29334 = CARTESIAN_POINT('Ctrl Pts',(-19.4555437647533,27.7500195871675,122.206790898622)) ;
#29335 = CARTESIAN_POINT('Ctrl Pts',(-19.7284352632182,27.9400308696653,121.938326646805)) ;
#29336 = CARTESIAN_POINT('Ctrl Pts',(-19.6645948238701,27.7600417893024,122.233024081806)) ;
#29337 = CARTESIAN_POINT('Ctrl Pts',(-19.980050984628,27.9500580626337,122.016636385366)) ;
#29338 = CARTESIAN_POINT('Ctrl Pts',(-19.8658877542819,27.7700689822708,122.295670925777)) ;
#29339 = CARTESIAN_POINT('Ctrl Pts',(-20.2103950643466,27.9599136566007,122.135000592785)) ;
#29340 = CARTESIAN_POINT('Ctrl Pts',(-20.0501626545512,27.7799245762378,122.39036086436)) ;
#29341 = CARTESIAN_POINT('Ctrl Pts',(-20.4193072748828,27.969870828466,122.29257198083)) ;
#29342 = CARTESIAN_POINT('Ctrl Pts',(-20.2172929209471,27.7898817481031,122.5164167495)) ;
#29343 = CARTESIAN_POINT('Ctrl Pts',(-20.5987996284151,27.9799096724644,122.485885053549)) ;
#29344 = CARTESIAN_POINT('Ctrl Pts',(-20.3608877406853,27.7999205921015,122.67106648784)) ;
#29345 = CARTESIAN_POINT('Ctrl Pts',(-20.7400613604965,27.98978369634,122.703583668428)) ;
#29346 = CARTESIAN_POINT('Ctrl Pts',(-20.4738977561458,27.8097946159771,122.845224005242)) ;
#29347 = CARTESIAN_POINT('Ctrl Pts',(-20.8433506853364,27.9998535223304,122.947177423952)) ;
#29348 = CARTESIAN_POINT('Ctrl Pts',(-20.5565304991962,27.8198644419675,123.040098768756)) ;
#29349 = CARTESIAN_POINT('Ctrl Pts',(-20.9015266940339,28.0096867662276,123.198973980949)) ;
#29350 = CARTESIAN_POINT('Ctrl Pts',(-20.6030723456922,27.8296976858648,123.241534723945)) ;
#29351 = CARTESIAN_POINT('Ctrl Pts',(-20.9161142994382,28.0197171940007,123.462150342134)) ;
#29352 = CARTESIAN_POINT('Ctrl Pts',(-20.6147438907103,27.8397281136378,123.452075801618)) ;
#29353 = CARTESIAN_POINT('Ctrl Pts',(-20.8840166201033,28.0297488107458,123.72382387547)) ;
#29354 = CARTESIAN_POINT('Ctrl Pts',(-20.5890670287782,27.8497597303829,123.661414851897)) ;
#29355 = CARTESIAN_POINT('Ctrl Pts',(-20.80904662986,28.0395784877265,123.971001465148)) ;
#29356 = CARTESIAN_POINT('Ctrl Pts',(-20.5290926826595,27.8595894073637,123.859156362875)) ;
#29357 = CARTESIAN_POINT('Ctrl Pts',(-20.6910868706554,28.0495680045665,124.205529304447)) ;
#29358 = CARTESIAN_POINT('Ctrl Pts',(-20.4347263402333,27.8695789242036,124.046779212421)) ;
#29359 = CARTESIAN_POINT('Ctrl Pts',(-20.5328182779669,28.0596116167062,124.416742316167)) ;
#29360 = CARTESIAN_POINT('Ctrl Pts',(-20.308112543254,27.8796225363434,124.215750577102)) ;
#29361 = CARTESIAN_POINT('Ctrl Pts',(-20.3448814894554,28.0694342230415,124.593693576125)) ;
#29362 = CARTESIAN_POINT('Ctrl Pts',(-20.1577648989237,27.8894451426787,124.357312023611)) ;
#29363 = CARTESIAN_POINT('Ctrl Pts',(-20.124678185504,28.0794724529408,124.73892784558)) ;
#29364 = CARTESIAN_POINT('Ctrl Pts',(-19.9816030855766,27.8994833725779,124.473500876513)) ;
#29365 = CARTESIAN_POINT('Ctrl Pts',(-19.8829899980489,28.0894834877327,124.842887131756)) ;
#29366 = CARTESIAN_POINT('Ctrl Pts',(-19.7882531778609,27.9094944073698,124.556669703237)) ;
#29367 = CARTESIAN_POINT('Ctrl Pts',(-19.6299384968335,28.0993812186998,124.903017471924)) ;
#29368 = CARTESIAN_POINT('Ctrl Pts',(-19.5858129211223,27.919392138337,124.60477541441)) ;
#29369 = CARTESIAN_POINT('Ctrl Pts',(-19.3678981582499,28.1093708465503,124.918781274721)) ;
#29370 = CARTESIAN_POINT('Ctrl Pts',(-19.3761808908369,27.9293817661874,124.617388123224)) ;
#29371 = CARTESIAN_POINT('Ctrl Pts',(-19.1079954571358,28.1193266369963,124.888817431813)) ;
#29372 = CARTESIAN_POINT('Ctrl Pts',(-19.1682588492881,27.9393375566334,124.593418735249)) ;
#29373 = CARTESIAN_POINT('Ctrl Pts',(-18.8578037171305,28.1292540355584,124.814868421456)) ;
#29374 = CARTESIAN_POINT('Ctrl Pts',(-18.968105356819,27.9492649551955,124.534261321663)) ;
#29375 = CARTESIAN_POINT('Ctrl Pts',(-18.6219935808609,28.1392796306682,124.697390886151)) ;
#29376 = CARTESIAN_POINT('Ctrl Pts',(-18.7794564590463,27.9592905503054,124.440280839266)) ;
#29377 = CARTESIAN_POINT('Ctrl Pts',(-18.413012495007,28.1491654813378,124.543058534145)) ;
#29378 = CARTESIAN_POINT('Ctrl Pts',(-18.612271014501,27.9691764009749,124.316816723086)) ;
#29379 = CARTESIAN_POINT('Ctrl Pts',(-18.2316780606301,28.159154661182,124.353241304876)) ;
#29380 = CARTESIAN_POINT('Ctrl Pts',(-18.4672022077259,27.9791655808191,124.164964317004)) ;
#29381 = CARTESIAN_POINT('Ctrl Pts',(-18.085762555499,28.1691958482856,124.133385523761)) ;
#29382 = CARTESIAN_POINT('Ctrl Pts',(-18.3504682851199,27.9892067679227,123.989080612378)) ;
#29383 = CARTESIAN_POINT('Ctrl Pts',(-17.9820414176768,28.1790284917615,123.896729581303)) ;
#29384 = CARTESIAN_POINT('Ctrl Pts',(-18.2674899943736,27.9990394113987,123.799757297218)) ;
#29385 = CARTESIAN_POINT('Ctrl Pts',(-17.9192545217861,28.189022441471,123.641716424028)) ;
#29386 = CARTESIAN_POINT('Ctrl Pts',(-18.2172586037933,28.0090333611081,123.595747332759)) ;
#29387 = CARTESIAN_POINT('Ctrl Pts',(-17.9021928664862,28.1990515642475,123.378711840277)) ;
#29388 = CARTESIAN_POINT('Ctrl Pts',(-18.2036074112526,28.0190624838847,123.385343770105)) ;
#29389 = CARTESIAN_POINT('Ctrl Pts',(-17.9302039422221,28.2089276951662,123.120680343544)) ;
#29390 = CARTESIAN_POINT('Ctrl Pts',(-18.2260142937599,28.0289386148033,123.178918899042)) ;
#29391 = CARTESIAN_POINT('Ctrl Pts',(-18.0031776926144,28.2189257301832,122.86831261201)) ;
#29392 = CARTESIAN_POINT('Ctrl Pts',(-18.2843913725109,28.0389366498204,122.977024252251)) ;
#29393 = CARTESIAN_POINT('Ctrl Pts',(-18.117736776842,28.2288396599419,122.634287677194)) ;
#29394 = CARTESIAN_POINT('Ctrl Pts',(-18.376036681339,28.0488505795791,122.789803759949)) ;
#29395 = CARTESIAN_POINT('Ctrl Pts',(-18.2731150794606,28.2388828476797,122.420974122389)) ;
#29396 = CARTESIAN_POINT('Ctrl Pts',(-18.5003377353294,28.0588937673169,122.619151688384)) ;
#29397 = CARTESIAN_POINT('Ctrl Pts',(-18.4604722427515,28.2487826898201,122.24045743561)) ;
#29398 = CARTESIAN_POINT('Ctrl Pts',(-18.6502217887544,28.0687936094572,122.474737169911)) ;
#29399 = CARTESIAN_POINT('Ctrl Pts',(-18.6779981948743,28.2587739566281,122.093415286291)) ;
#29400 = CARTESIAN_POINT('Ctrl Pts',(-18.8242413102653,28.0787848762652,122.357101786154)) ;
#29401 = CARTESIAN_POINT('Ctrl Pts',(-18.918918044841,28.2688060587601,121.986355077235)) ;
#29402 = CARTESIAN_POINT('Ctrl Pts',(-19.0169763807828,28.0888169783972,122.271451769572)) ;
#29403 = CARTESIAN_POINT('Ctrl Pts',(-19.1704626082505,28.2786729397148,121.923469734543)) ;
#29404 = CARTESIAN_POINT('Ctrl Pts',(-19.2182110752363,28.098683859352,122.221141611949)) ;
#29405 = CARTESIAN_POINT('Ctrl Pts',(-19.432345213223,28.288664731003,121.904359612356)) ;
#29406 = CARTESIAN_POINT('Ctrl Pts',(-19.4277169183523,28.1086756506401,122.20585140049)) ;
#29407 = CARTESIAN_POINT('Ctrl Pts',(-19.694564039776,28.2986968469145,121.93162572317)) ;
#29408 = CARTESIAN_POINT('Ctrl Pts',(-19.6374921940647,28.1187077665516,122.227662228157)) ;
#29409 = CARTESIAN_POINT('Ctrl Pts',(-19.943995852301,28.3085631637145,122.002434913296)) ;
#29410 = CARTESIAN_POINT('Ctrl Pts',(-19.8370378243453,28.1285740833517,122.284307435928)) ;
#29411 = CARTESIAN_POINT('Ctrl Pts',(-20.1803573809643,28.3185506451881,122.116461326157)) ;
#29412 = CARTESIAN_POINT('Ctrl Pts',(-20.0261278945652,28.1385615648253,122.375526584252)) ;
#29413 = CARTESIAN_POINT('Ctrl Pts',(-20.3925607131235,28.328495569567,122.269070719418)) ;
#29414 = CARTESIAN_POINT('Ctrl Pts',(-20.1958916697619,28.1485064892042,122.497612235911)) ;
#29415 = CARTESIAN_POINT('Ctrl Pts',(-20.5767268496923,28.3385404554777,122.458146387094)) ;
#29416 = CARTESIAN_POINT('Ctrl Pts',(-20.343226130455,28.1585513751149,122.648871279974)) ;
#29417 = CARTESIAN_POINT('Ctrl Pts',(-20.7227745276264,28.3484025591903,122.672264744843)) ;
#29418 = CARTESIAN_POINT('Ctrl Pts',(-20.4600658712918,28.1684134788274,122.820164463442)) ;
#29419 = CARTESIAN_POINT('Ctrl Pts',(-20.8312927348308,28.3583941230148,122.911337082898)) ;
#29420 = CARTESIAN_POINT('Ctrl Pts',(-20.5468824144814,28.1784050426519,123.011421352625)) ;
#29421 = CARTESIAN_POINT('Ctrl Pts',(-20.8961668071842,28.3683269310777,123.164169825498)) ;
#29422 = CARTESIAN_POINT('Ctrl Pts',(-20.5987837570556,28.1883378507148,123.213686829248)) ;
#29423 = CARTESIAN_POINT('Ctrl Pts',(-20.9168053566465,28.378264033314,123.424505796562)) ;
#29424 = CARTESIAN_POINT('Ctrl Pts',(-20.615296810215,28.1982749529511,123.421955292323)) ;
#29425 = CARTESIAN_POINT('Ctrl Pts',(-20.8912939664117,28.3883164795844,123.687418366482)) ;
#29426 = CARTESIAN_POINT('Ctrl Pts',(-20.5948899052389,28.2083273992215,123.632285549448)) ;
#29427 = CARTESIAN_POINT('Ctrl Pts',(-20.8223185569164,28.398162595166,123.936824298385)) ;
#29428 = CARTESIAN_POINT('Ctrl Pts',(-20.5397117877283,28.2181735148031,123.831810673226)) ;
#29429 = CARTESIAN_POINT('Ctrl Pts',(-20.709193147176,28.4082106148809,124.175395051952)) ;
#29430 = CARTESIAN_POINT('Ctrl Pts',(-20.4492134944853,28.228221534518,124.022668227718)) ;
#29431 = CARTESIAN_POINT('Ctrl Pts',(-20.5576594223878,28.4181525665098,124.388243230741)) ;
#29432 = CARTESIAN_POINT('Ctrl Pts',(-20.3279884025434,28.238163486147,124.192947972631)) ;
#29433 = CARTESIAN_POINT('Ctrl Pts',(-20.3719920554206,28.4280913475089,124.571940487482)) ;
#29434 = CARTESIAN_POINT('Ctrl Pts',(-20.1794561524199,28.248102267146,124.339907313728)) ;
#29435 = CARTESIAN_POINT('Ctrl Pts',(-20.155266255181,28.438117396235,124.721739105602)) ;
#29436 = CARTESIAN_POINT('Ctrl Pts',(-20.0060768524774,28.2581283158721,124.45974803094)) ;
#29437 = CARTESIAN_POINT('Ctrl Pts',(-19.9192398618305,28.4480042566432,124.830426395165)) ;
#29438 = CARTESIAN_POINT('Ctrl Pts',(-19.8172566995611,28.2680151762803,124.546699853667)) ;
#29439 = CARTESIAN_POINT('Ctrl Pts',(-19.6643603212813,28.458035531775,124.897541005947)) ;
#29440 = CARTESIAN_POINT('Ctrl Pts',(-19.6133539336829,28.2780464514121,124.600393764835)) ;
#29441 = CARTESIAN_POINT('Ctrl Pts',(-19.405507635062,28.4679185090754,124.919330220156)) ;
#29442 = CARTESIAN_POINT('Ctrl Pts',(-19.4062711317406,28.2879294287125,124.617827171934)) ;
#29443 = CARTESIAN_POINT('Ctrl Pts',(-19.14236864725,28.4779753624826,124.895445755536)) ;
#29444 = CARTESIAN_POINT('Ctrl Pts',(-19.1957631355811,28.2979862821197,124.598722613177)) ;
#29445 = CARTESIAN_POINT('Ctrl Pts',(-18.8081529113529,28.4911436035585,124.80533200887)) ;
#29446 = CARTESIAN_POINT('Ctrl Pts',(-18.9283732060215,28.3111545231956,124.526630734819)) ;
#29447 = CARTESIAN_POINT('Ctrl Pts',(-18.4999549682012,28.504544632785,124.627092881207)) ;
#29448 = CARTESIAN_POINT('Ctrl Pts',(-18.681798248427,28.3245555524222,124.384021484789)) ;
#29449 = CARTESIAN_POINT('Ctrl Pts',(-18.2548346129752,28.5177575495159,124.381018273064)) ;
#29450 = CARTESIAN_POINT('Ctrl Pts',(-18.4857344323844,28.337768469153,124.187192189279)) ;
#29451 = CARTESIAN_POINT('Ctrl Pts',(-18.1049098192041,28.5276859439691,124.167554176501)) ;
#29452 = CARTESIAN_POINT('Ctrl Pts',(-18.3657857952432,28.3476968636062,124.016416466804)) ;
#29453 = CARTESIAN_POINT('Ctrl Pts',(-17.9935167509591,28.5376674440972,123.930036177092)) ;
#29454 = CARTESIAN_POINT('Ctrl Pts',(-18.2766712098695,28.3576783637344,123.826404555807)) ;
#29455 = CARTESIAN_POINT('Ctrl Pts',(-17.9250194853092,28.5477079873673,123.675241990111)) ;
#29456 = CARTESIAN_POINT('Ctrl Pts',(-18.2218707823498,28.3677189070045,123.622569449493)) ;
#29457 = CARTESIAN_POINT('Ctrl Pts',(-17.9019033242933,28.5575573191504,123.417442838969)) ;
#29458 = CARTESIAN_POINT('Ctrl Pts',(-18.2033757289784,28.3775682387876,123.416330378134)) ;
#29459 = CARTESIAN_POINT('Ctrl Pts',(-17.9235537436292,28.5675527236221,123.155670875178)) ;
#29460 = CARTESIAN_POINT('Ctrl Pts',(-18.2206940100474,28.3875636432592,123.206912092977)) ;
#29461 = CARTESIAN_POINT('Ctrl Pts',(-17.990923682755,28.5775690510707,122.901217359065)) ;
#29462 = CARTESIAN_POINT('Ctrl Pts',(-18.2745872927144,28.3975799707078,123.003350782383)) ;
#29463 = CARTESIAN_POINT('Ctrl Pts',(-18.1363563321866,28.5907927082372,122.585573838039)) ;
#29464 = CARTESIAN_POINT('Ctrl Pts',(-18.3909334946143,28.4108036278744,122.750824793006)) ;
#29465 = CARTESIAN_POINT('Ctrl Pts',(-18.361738888197,28.6040869996266,122.313564150216)) ;
#29466 = CARTESIAN_POINT('Ctrl Pts',(-18.5712653371683,28.4240979192637,122.533196651324)) ;
#29467 = CARTESIAN_POINT('Ctrl Pts',(-18.6465253994931,28.6173713505581,122.111531614028)) ;
#29468 = CARTESIAN_POINT('Ctrl Pts',(-18.7990570818657,28.4373822701952,122.371600047551)) ;
#29469 = CARTESIAN_POINT('Ctrl Pts',(-18.8832307222806,28.6273437316199,121.999158080089)) ;
#29470 = CARTESIAN_POINT('Ctrl Pts',(-18.9884277554392,28.447354651257,122.281692950129)) ;
#29471 = CARTESIAN_POINT('Ctrl Pts',(-19.1341788049863,28.6372521112455,121.929579826141)) ;
#29472 = CARTESIAN_POINT('Ctrl Pts',(-19.1891837168037,28.4572630308826,122.22602983351)) ;
#29473 = CARTESIAN_POINT('Ctrl Pts',(-19.3971551455222,28.6473061099936,121.904389073441)) ;
#29474 = CARTESIAN_POINT('Ctrl Pts',(-19.3995659464143,28.4673170296307,122.205875390456)) ;
#29475 = CARTESIAN_POINT('Ctrl Pts',(-19.6555567772795,28.6571683071099,121.924649710965)) ;
#29476 = CARTESIAN_POINT('Ctrl Pts',(-19.6062837665613,28.477179226747,122.222079569028)) ;
#29477 = CARTESIAN_POINT('Ctrl Pts',(-19.9952798306344,28.670515433484,122.011813758423)) ;
#29478 = CARTESIAN_POINT('Ctrl Pts',(-19.8780825920856,28.4905263531211,122.291820399844)) ;
#29479 = CARTESIAN_POINT('Ctrl Pts',(-20.3783371558031,28.6870523991254,122.227433848027)) ;
#29480 = CARTESIAN_POINT('Ctrl Pts',(-20.1845001448543,28.5070633187626,122.464288220489)) ;
#29481 = CARTESIAN_POINT('Ctrl Pts',(-20.6669572705968,28.7036870032994,122.562229846375)) ;
#29482 = CARTESIAN_POINT('Ctrl Pts',(-20.4154369512327,28.5236979229365,122.73217404382)) ;
#29483 = CARTESIAN_POINT('Ctrl Pts',(-20.818619503667,28.716976796542,122.876897221786)) ;
#29484 = CARTESIAN_POINT('Ctrl Pts',(-20.536739963039,28.5369877161791,122.983864515057)) ;
#29485 = CARTESIAN_POINT('Ctrl Pts',(-20.8898646071741,28.7269294278014,123.12852052043)) ;
#29486 = CARTESIAN_POINT('Ctrl Pts',(-20.5937435077852,28.5469403474385,123.185172022197)) ;
#29487 = CARTESIAN_POINT('Ctrl Pts',(-20.916646989976,28.7368813951061,123.388702342932)) ;
#29488 = CARTESIAN_POINT('Ctrl Pts',(-20.6151704550531,28.5568923147432,123.393312774312)) ;
#29489 = CARTESIAN_POINT('Ctrl Pts',(-20.891192739327,28.7502486535699,123.739016958567)) ;
#29490 = CARTESIAN_POINT('Ctrl Pts',(-20.5948058393565,28.570259573207,123.673577519016)) ;
#29491 = CARTESIAN_POINT('Ctrl Pts',(-20.7477418810432,28.7667654655191,124.154036877155)) ;
#29492 = CARTESIAN_POINT('Ctrl Pts',(-20.4800520421779,28.5867763851562,124.005580886931)) ;
#29493 = CARTESIAN_POINT('Ctrl Pts',(-20.4126932064644,28.7867913605254,124.567418944492)) ;
#29494 = CARTESIAN_POINT('Ctrl Pts',(-20.2120144196254,28.6068022801626,124.336293127083)) ;
#29495 = CARTESIAN_POINT('Ctrl Pts',(-19.9614615275447,28.8066020906556,124.838970603354)) ;
#29496 = CARTESIAN_POINT('Ctrl Pts',(-19.8510300684342,28.6266130102927,124.553536623259)) ;
#29497 = CARTESIAN_POINT('Ctrl Pts',(-19.4406750274565,28.8265793067854,124.942183198345)) ;
#29498 = CARTESIAN_POINT('Ctrl Pts',(-19.4344011473137,28.6465902264226,124.636109825958)) ;
#29499 = CARTESIAN_POINT('Ctrl Pts',(-18.9173848458449,28.8465061821807,124.860730356123)) ;
#29500 = CARTESIAN_POINT('Ctrl Pts',(-19.015768045154,28.6665171018178,124.570950325204)) ;
#29501 = CARTESIAN_POINT('Ctrl Pts',(-18.4548495376105,28.866327643657,124.608386572972)) ;
#29502 = CARTESIAN_POINT('Ctrl Pts',(-18.6457373585372,28.6863385632941,124.36907662557)) ;
#29503 = CARTESIAN_POINT('Ctrl Pts',(-18.1021082199431,28.8864019614663,124.20819190284)) ;
#29504 = CARTESIAN_POINT('Ctrl Pts',(-18.3635430360855,28.7064128811034,124.048922914079)) ;
#29505 = CARTESIAN_POINT('Ctrl Pts',(-17.9097030414757,28.9062499304742,123.716849978485)) ;
#29506 = CARTESIAN_POINT('Ctrl Pts',(-18.2096162521416,28.7262608501113,123.655848998423)) ;
#29507 = CARTESIAN_POINT('Ctrl Pts',(-17.8953659112392,28.9261969645374,123.187000088179)) ;
#29508 = CARTESIAN_POINT('Ctrl Pts',(-18.1981447291151,28.7462078841745,123.231968583052)) ;
#29509 = CARTESIAN_POINT('Ctrl Pts',(-18.0624463345147,28.9460929155096,122.685244684184)) ;
#29510 = CARTESIAN_POINT('Ctrl Pts',(-18.3318078029622,28.7661038351467,122.830562717796)) ;
#29511 = CARTESIAN_POINT('Ctrl Pts',(-18.3899816868081,28.9659883951278,122.270147568337)) ;
#29512 = CARTESIAN_POINT('Ctrl Pts',(-18.5938359071739,28.7859993147649,122.498483387)) ;
#29513 = CARTESIAN_POINT('Ctrl Pts',(-18.8408757372252,28.9859445060926,121.990748528834)) ;
#29514 = CARTESIAN_POINT('Ctrl Pts',(-18.9545510633946,28.8059554257297,122.274963123727)) ;
#29515 = CARTESIAN_POINT('Ctrl Pts',(-19.3586261760562,29.0058490541326,121.882442313881)) ;
#29516 = CARTESIAN_POINT('Ctrl Pts',(-19.3687524196573,28.8258599737697,122.188317114002)) ;
#29517 = CARTESIAN_POINT('Ctrl Pts',(-19.8818129365437,29.0257231784517,121.95590917428)) ;
#29518 = CARTESIAN_POINT('Ctrl Pts',(-19.7873033983275,28.8457340980888,122.24709086078)) ;
#29519 = CARTESIAN_POINT('Ctrl Pts',(-20.3522418344828,29.0457777084507,122.206339109689)) ;
#29520 = CARTESIAN_POINT('Ctrl Pts',(-20.1636459491141,28.8657886280878,122.447434352417)) ;
#29521 = CARTESIAN_POINT('Ctrl Pts',(-20.7048254925126,29.0655852222107,122.597429836113)) ;
#29522 = CARTESIAN_POINT('Ctrl Pts',(-20.4457143874069,28.8855961418478,122.760308841788)) ;
#29523 = CARTESIAN_POINT('Ctrl Pts',(-20.9055115949536,29.0855685779784,123.089100356984)) ;
#29524 = CARTESIAN_POINT('Ctrl Pts',(-20.6062625174432,28.9055794976156,123.153645765125)) ;
#29525 = CARTESIAN_POINT('Ctrl Pts',(-20.9255057422183,29.1054868805624,123.618111697477)) ;
#29526 = CARTESIAN_POINT('Ctrl Pts',(-20.622257172822,28.9254978001995,123.576855858986)) ;
#29527 = CARTESIAN_POINT('Ctrl Pts',(-20.7655021762044,29.1253550960081,124.121463964361)) ;
#29528 = CARTESIAN_POINT('Ctrl Pts',(-20.4942524673024,28.9453660156452,123.979538536319)) ;
#29529 = CARTESIAN_POINT('Ctrl Pts',(-20.4398756731327,29.1454054128044,124.543114839599)) ;
#29530 = CARTESIAN_POINT('Ctrl Pts',(-20.2337505118372,28.9654163324415,124.316858031653)) ;
#29531 = CARTESIAN_POINT('Ctrl Pts',(-19.9961359923068,29.1651814746869,124.82522657557)) ;
#29532 = CARTESIAN_POINT('Ctrl Pts',(-19.878755955537,28.985192394324,124.542547120948)) ;
#29533 = CARTESIAN_POINT('Ctrl Pts',(-19.4760372478541,29.1852360803793,124.9408742549)) ;
#29534 = CARTESIAN_POINT('Ctrl Pts',(-19.4626769826316,29.0052470000165,124.63506310846)) ;
#29535 = CARTESIAN_POINT('Ctrl Pts',(-18.9542188864203,29.2050297695352,124.872787108227)) ;
#29536 = CARTESIAN_POINT('Ctrl Pts',(-19.0452207775086,29.0250406891723,124.580591027841)) ;
#29537 = CARTESIAN_POINT('Ctrl Pts',(-18.4824497195716,29.2249964611296,124.630017164074)) ;
#29538 = CARTESIAN_POINT('Ctrl Pts',(-18.667806512202,29.0450073807667,124.386372476876)) ;
#29539 = CARTESIAN_POINT('Ctrl Pts',(-18.1224282621344,29.2449565068806,124.240242601981)) ;
#29540 = CARTESIAN_POINT('Ctrl Pts',(-18.3797910944419,29.0649674265177,124.074550845858)) ;
#29541 = CARTESIAN_POINT('Ctrl Pts',(-17.9173907834527,29.2648547670308,123.752777846934)) ;
#29542 = CARTESIAN_POINT('Ctrl Pts',(-18.2157634593431,29.084865686668,123.68457721216)) ;
#29543 = CARTESIAN_POINT('Ctrl Pts',(-17.8903701259974,29.28474968258,123.224718223152)) ;
#29544 = CARTESIAN_POINT('Ctrl Pts',(-18.1941500680826,29.1047606022171,123.262128658022)) ;
#29545 = CARTESIAN_POINT('Ctrl Pts',(-18.0448227791641,29.3046598629936,122.718584462674)) ;
#29546 = CARTESIAN_POINT('Ctrl Pts',(-18.3177155786987,29.1246707826307,122.857222129875)) ;
#29547 = CARTESIAN_POINT('Ctrl Pts',(-18.3629508949474,29.3245956621079,122.294833096222)) ;
#29548 = CARTESIAN_POINT('Ctrl Pts',(-18.5722211306576,29.144606581745,122.518222926126)) ;
#29549 = CARTESIAN_POINT('Ctrl Pts',(-18.8065966645385,29.344533523762,122.005031573975)) ;
#29550 = CARTESIAN_POINT('Ctrl Pts',(-18.9271398869184,29.1645444433991,122.28638447727)) ;
#29551 = CARTESIAN_POINT('Ctrl Pts',(-19.3219781329333,29.3644525703997,121.88380547982)) ;
#29552 = CARTESIAN_POINT('Ctrl Pts',(-19.339446619592,29.1844634900368,122.189407632627)) ;
#29553 = CARTESIAN_POINT('Ctrl Pts',(-19.8485530096058,29.3844014684538,121.945745518254)) ;
#29554 = CARTESIAN_POINT('Ctrl Pts',(-19.7607049211448,29.2044123880909,122.238961921839)) ;
#29555 = CARTESIAN_POINT('Ctrl Pts',(-20.3214474198052,29.4043072958969,122.18303123303)) ;
#29556 = CARTESIAN_POINT('Ctrl Pts',(-20.1390239324075,29.224318215534,122.428800199034)) ;
#29557 = CARTESIAN_POINT('Ctrl Pts',(-20.6245684184595,29.4208899912622,122.502888255951)) ;
#29558 = CARTESIAN_POINT('Ctrl Pts',(-20.381503037069,29.2409009108993,122.684669703668)) ;
#29559 = CARTESIAN_POINT('Ctrl Pts',(-20.791234180934,29.4341642049858,122.809390920718)) ;
#29560 = CARTESIAN_POINT('Ctrl Pts',(-20.5148468140483,29.2541751246229,122.929890379545)) ;
#29561 = CARTESIAN_POINT('Ctrl Pts',(-20.8750220852076,29.4442109241851,123.05973121324)) ;
#29562 = CARTESIAN_POINT('Ctrl Pts',(-20.5818729237177,29.2642218438223,123.13015699649)) ;
#29563 = CARTESIAN_POINT('Ctrl Pts',(-20.9135737768039,29.4540549588308,123.315549607641)) ;
#29564 = CARTESIAN_POINT('Ctrl Pts',(-20.6127109316255,29.2740658784679,123.334824035889)) ;
#29565 = CARTESIAN_POINT('Ctrl Pts',(-20.9056110532671,29.4673893437353,123.665862635849)) ;
#29566 = CARTESIAN_POINT('Ctrl Pts',(-20.6063479581414,29.2874002633725,123.615020710436)) ;
#29567 = CARTESIAN_POINT('Ctrl Pts',(-20.7817183691016,29.4839765610351,124.089008121444)) ;
#29568 = CARTESIAN_POINT('Ctrl Pts',(-20.5072137252115,29.3039874806722,123.953603177572)) ;
#29569 = CARTESIAN_POINT('Ctrl Pts',(-20.5204871039959,29.500609773073,124.445591168462)) ;
#29570 = CARTESIAN_POINT('Ctrl Pts',(-20.2982490932776,29.3206206927101,124.238824480431)) ;
#29571 = CARTESIAN_POINT('Ctrl Pts',(-20.2482786094575,29.5138922153452,124.664142759317)) ;
#29572 = CARTESIAN_POINT('Ctrl Pts',(-20.0804621387608,29.3339031349823,124.413688421931)) ;
#29573 = CARTESIAN_POINT('Ctrl Pts',(-20.0203496111071,29.5237981032594,124.789853895898)) ;
#29574 = CARTESIAN_POINT('Ctrl Pts',(-19.8981216151747,29.3438090228965,124.514250475789)) ;
#29575 = CARTESIAN_POINT('Ctrl Pts',(-19.7720804977814,29.5337865213645,124.875101645455)) ;
#29576 = CARTESIAN_POINT('Ctrl Pts',(-19.699504035617,29.3537974410017,124.582447706781)) ;
#29577 = CARTESIAN_POINT('Ctrl Pts',(-19.5118312861888,29.5438099486033,124.9158105401)) ;
#29578 = CARTESIAN_POINT('Ctrl Pts',(-19.4913069695219,29.3638208682404,124.615012953148)) ;
#29579 = CARTESIAN_POINT('Ctrl Pts',(-19.2516162816116,29.5537143797203,124.910922144998)) ;
#29580 = CARTESIAN_POINT('Ctrl Pts',(-19.2831262502567,29.3737252993574,124.611097513249)) ;
#29581 = CARTESIAN_POINT('Ctrl Pts',(-18.9093488133413,29.5669775323307,124.844857601197)) ;
#29582 = CARTESIAN_POINT('Ctrl Pts',(-19.0093557497466,29.3869884519678,124.558255787372)) ;
#29583 = CARTESIAN_POINT('Ctrl Pts',(-18.5909285364746,29.5803024302346,124.689972489664)) ;
#29584 = CARTESIAN_POINT('Ctrl Pts',(-18.7545953313426,29.4003133498717,124.434343999134)) ;
#29585 = CARTESIAN_POINT('Ctrl Pts',(-18.3276416499704,29.5935581738502,124.461801734779)) ;
#29586 = CARTESIAN_POINT('Ctrl Pts',(-18.5439553434392,29.4135690934873,124.251793461498)) ;
#29587 = CARTESIAN_POINT('Ctrl Pts',(-18.1623453454126,29.6035175472975,124.258928464813)) ;
#29588 = CARTESIAN_POINT('Ctrl Pts',(-18.4117225892705,29.4235284669346,124.089495803923)) ;
#29589 = CARTESIAN_POINT('Ctrl Pts',(-18.0346636089127,29.6134613712245,124.030895956569)) ;
#29590 = CARTESIAN_POINT('Ctrl Pts',(-18.3095785285436,29.4334722908616,123.907068119568)) ;
#29591 = CARTESIAN_POINT('Ctrl Pts',(-17.9478442966657,29.6235093153718,123.781548712612)) ;
#29592 = CARTESIAN_POINT('Ctrl Pts',(-18.2401254083158,29.4435202350089,123.707589793291)) ;
#29593 = CARTESIAN_POINT('Ctrl Pts',(-17.906234953778,29.6333602865899,123.526025793516)) ;
#29594 = CARTESIAN_POINT('Ctrl Pts',(-18.2068401299479,29.4533712062271,123.503171143586)) ;
#29595 = CARTESIAN_POINT('Ctrl Pts',(-17.9089904954044,29.643332104032,123.264021399714)) ;
#29596 = CARTESIAN_POINT('Ctrl Pts',(-18.2090468245195,29.4633430236691,123.293567757575)) ;
#29597 = CARTESIAN_POINT('Ctrl Pts',(-17.9573656877064,29.6533275263241,123.005808163303)) ;
#29598 = CARTESIAN_POINT('Ctrl Pts',(-18.2477491698236,29.4733384459612,123.086997640274)) ;
#29599 = CARTESIAN_POINT('Ctrl Pts',(-18.0504309097234,29.6633605914478,122.75912999775)) ;
#29600 = CARTESIAN_POINT('Ctrl Pts',(-18.3222034468051,29.4833715110849,122.88965593636)) ;
#29601 = CARTESIAN_POINT('Ctrl Pts',(-18.1824501820335,29.673225924113,122.536018472183)) ;
#29602 = CARTESIAN_POINT('Ctrl Pts',(-18.4278207101303,29.4932368437501,122.711168011498)) ;
#29603 = CARTESIAN_POINT('Ctrl Pts',(-18.352254460823,29.6831864667106,122.336809734032)) ;
#29604 = CARTESIAN_POINT('Ctrl Pts',(-18.5636657405991,29.5031973863477,122.551802554504)) ;
#29605 = CARTESIAN_POINT('Ctrl Pts',(-18.5558196647205,29.6932201522123,122.169242143868)) ;
#29606 = CARTESIAN_POINT('Ctrl Pts',(-18.7265193140521,29.5132310718494,122.417750218351)) ;
#29607 = CARTESIAN_POINT('Ctrl Pts',(-18.7818025397086,29.7031049842026,122.041072921772)) ;
#29608 = CARTESIAN_POINT('Ctrl Pts',(-18.9073065097523,29.5231159038397,122.315216877536)) ;
#29609 = CARTESIAN_POINT('Ctrl Pts',(-19.0310733364163,29.7131724109624,121.952565569517)) ;
#29610 = CARTESIAN_POINT('Ctrl Pts',(-19.1067239210886,29.5331833305995,122.24441307792)) ;
#29611 = CARTESIAN_POINT('Ctrl Pts',(-19.286036901977,29.7230109001213,121.909416064618)) ;
#29612 = CARTESIAN_POINT('Ctrl Pts',(-19.3106948134357,29.5430218197584,122.209895699158)) ;
#29613 = CARTESIAN_POINT('Ctrl Pts',(-19.550453199473,29.7330743813114,121.910880737687)) ;
#29614 = CARTESIAN_POINT('Ctrl Pts',(-19.5222278763447,29.5530853009485,122.211069619433)) ;
#29615 = CARTESIAN_POINT('Ctrl Pts',(-19.8062464008285,29.7429685391265,121.957671456219)) ;
#29616 = CARTESIAN_POINT('Ctrl Pts',(-19.7268617815842,29.5629794587636,122.248504306379)) ;
#29617 = CARTESIAN_POINT('Ctrl Pts',(-20.0513931602021,29.7529103958708,122.047912589705)) ;
#29618 = CARTESIAN_POINT('Ctrl Pts',(-19.9229782497092,29.5729213155079,122.320699150998)) ;
#29619 = CARTESIAN_POINT('Ctrl Pts',(-20.27863327422,29.7629128735422,122.180100002924)) ;
#29620 = CARTESIAN_POINT('Ctrl Pts',(-20.1047692120472,29.5829237931793,122.426450889047)) ;
#29621 = CARTESIAN_POINT('Ctrl Pts',(-20.4798098359431,29.7729476778465,122.350566712122)) ;
#29622 = CARTESIAN_POINT('Ctrl Pts',(-20.265709069093,29.5929585974836,122.562825920578)) ;
#29623 = CARTESIAN_POINT('Ctrl Pts',(-20.64549843004,29.7827925546922,122.549284780308)) ;
#29624 = CARTESIAN_POINT('Ctrl Pts',(-20.3982580187208,29.6028034743293,122.721801389537)) ;
#29625 = CARTESIAN_POINT('Ctrl Pts',(-20.7764071388104,29.7927784342477,122.776669844146)) ;
#29626 = CARTESIAN_POINT('Ctrl Pts',(-20.5029831155846,29.6127893538848,122.903710368416)) ;
#29627 = CARTESIAN_POINT('Ctrl Pts',(-20.8655976909384,29.8027131646062,123.022090489185)) ;
#29628 = CARTESIAN_POINT('Ctrl Pts',(-20.5743335346531,29.6227240842433,123.100047340193)) ;
#29629 = CARTESIAN_POINT('Ctrl Pts',(-20.911118673284,29.8127709769191,123.2824053866)) ;
#29630 = CARTESIAN_POINT('Ctrl Pts',(-20.6107482780399,29.6327818965562,123.308299712704)) ;
#29631 = CARTESIAN_POINT('Ctrl Pts',(-20.9112011989042,29.8225915690435,123.540523528446)) ;
#29632 = CARTESIAN_POINT('Ctrl Pts',(-20.610812264355,29.6426024886806,123.514793589066)) ;
#29633 = CARTESIAN_POINT('Ctrl Pts',(-20.8656816934186,29.8326581546532,123.801062971402)) ;
#29634 = CARTESIAN_POINT('Ctrl Pts',(-20.5743946700159,29.6526690742904,123.723224921033)) ;
#29635 = CARTESIAN_POINT('Ctrl Pts',(-20.7770260888292,29.8425577352351,124.045706385067)) ;
#29636 = CARTESIAN_POINT('Ctrl Pts',(-20.503468442044,29.6625686548722,123.918938590259)) ;
#29637 = CARTESIAN_POINT('Ctrl Pts',(-20.6453879764234,29.8526093349133,124.274656477308)) ;
#29638 = CARTESIAN_POINT('Ctrl Pts',(-20.398156179075,29.6726202545505,124.102097751505)) ;
#29639 = CARTESIAN_POINT('Ctrl Pts',(-20.4790736605817,29.8624835213303,124.473897491922)) ;
#29640 = CARTESIAN_POINT('Ctrl Pts',(-20.2651035506588,29.6824944409674,124.261488905988)) ;
#29641 = CARTESIAN_POINT('Ctrl Pts',(-20.2772141277769,29.8725399972112,124.644389380226)) ;
#29642 = CARTESIAN_POINT('Ctrl Pts',(-20.1036145883348,29.6925509168483,124.39788099837)) ;
#29643 = CARTESIAN_POINT('Ctrl Pts',(-20.0524919644059,29.8824329285138,124.775217544899)) ;
#29644 = CARTESIAN_POINT('Ctrl Pts',(-19.9238362960661,29.7024438481509,124.502541627271)) ;
#29645 = CARTESIAN_POINT('Ctrl Pts',(-19.8043884253136,29.8924957072264,124.866595201475)) ;
#29646 = CARTESIAN_POINT('Ctrl Pts',(-19.7253526612113,29.7125066268636,124.57564199753)) ;
#29647 = CARTESIAN_POINT('Ctrl Pts',(-19.5498333322758,29.9023382328076,124.91262179111)) ;
#29648 = CARTESIAN_POINT('Ctrl Pts',(-19.5217089312482,29.7223491524447,124.612461273201)) ;
#29649 = CARTESIAN_POINT('Ctrl Pts',(-19.2873260771025,29.9123289982325,124.914394172825)) ;
#29650 = CARTESIAN_POINT('Ctrl Pts',(-19.3117032550328,29.7323399178696,124.613877366799)) ;
#29651 = CARTESIAN_POINT('Ctrl Pts',(-19.0300851291776,29.9222570742305,124.870781057726)) ;
#29652 = CARTESIAN_POINT('Ctrl Pts',(-19.1059111853094,29.7422679938676,124.578985150407)) ;
#29653 = CARTESIAN_POINT('Ctrl Pts',(-18.7826904157509,29.9322449846175,124.783069756764)) ;
#29654 = CARTESIAN_POINT('Ctrl Pts',(-18.9079961342318,29.7522559042547,124.508814517184)) ;
#29655 = CARTESIAN_POINT('Ctrl Pts',(-18.5534253143983,29.9422808967425,124.652734665094)) ;
#29656 = CARTESIAN_POINT('Ctrl Pts',(-18.7245848901154,29.7622918163796,124.404544830416)) ;
#29657 = CARTESIAN_POINT('Ctrl Pts',(-18.3536388771245,29.9521359095901,124.487912827377)) ;
#29658 = CARTESIAN_POINT('Ctrl Pts',(-18.5647574170873,29.7721468292273,124.272686483657)) ;
#29659 = CARTESIAN_POINT('Ctrl Pts',(-18.1828123336801,29.9621348555064,124.288313606199)) ;
#29660 = CARTESIAN_POINT('Ctrl Pts',(-18.4280975323811,29.7821457751435,124.113006096126)) ;
#29661 = CARTESIAN_POINT('Ctrl Pts',(-18.0503403718914,29.9720317679544,124.064451745925)) ;
#29662 = CARTESIAN_POINT('Ctrl Pts',(-18.3221216633801,29.7920426875915,123.933916272445)) ;
#29663 = CARTESIAN_POINT('Ctrl Pts',(-17.9572951648542,29.9820855660479,123.817209301492)) ;
#29664 = CARTESIAN_POINT('Ctrl Pts',(-18.2476869703767,29.802096485685,123.736121602035)) ;
#29665 = CARTESIAN_POINT('Ctrl Pts',(-17.9093444927588,29.9919664868746,123.56198502385)) ;
#29666 = CARTESIAN_POINT('Ctrl Pts',(-18.2093281437484,29.8119774065117,123.53194254377)) ;
#29667 = CARTESIAN_POINT('Ctrl Pts',(-17.9059278138796,30.0019710128723,123.299129283876)) ;
#29668 = CARTESIAN_POINT('Ctrl Pts',(-18.2065963307077,29.8219819325095,123.321658010208)) ;
#29669 = CARTESIAN_POINT('Ctrl Pts',(-17.9482064112771,30.0119549764898,123.040145215749)) ;
#29670 = CARTESIAN_POINT('Ctrl Pts',(-18.2404207028938,29.8319658961269,123.114471165854)) ;
#29671 = CARTESIAN_POINT('Ctrl Pts',(-18.035508186737,30.0219946170411,122.791197498885)) ;
#29672 = CARTESIAN_POINT('Ctrl Pts',(-18.3102636613557,29.8420055366782,122.915313421293)) ;
#29673 = CARTESIAN_POINT('Ctrl Pts',(-18.161925212928,30.0318386426558,122.565497657734)) ;
#29674 = CARTESIAN_POINT('Ctrl Pts',(-18.411398175043,29.8518495622929,122.734755088774)) ;
#29675 = CARTESIAN_POINT('Ctrl Pts',(-18.3274685805744,30.0418296484732,122.361708399386)) ;
#29676 = CARTESIAN_POINT('Ctrl Pts',(-18.5438338428557,29.8618405681103,122.571724671418)) ;
#29677 = CARTESIAN_POINT('Ctrl Pts',(-18.5272036340267,30.0518674400053,122.189409573137)) ;
#29678 = CARTESIAN_POINT('Ctrl Pts',(-18.7036229469901,29.8718783596425,122.433886677935)) ;
#29679 = CARTESIAN_POINT('Ctrl Pts',(-18.749230903998,30.0617118397937,122.056613364073)) ;
#29680 = CARTESIAN_POINT('Ctrl Pts',(-18.8812446799317,29.8817227594309,122.327651401076)) ;
#29681 = CARTESIAN_POINT('Ctrl Pts',(-18.994164126273,30.0716966403505,121.962602178295)) ;
#29682 = CARTESIAN_POINT('Ctrl Pts',(-19.0771915377067,29.8917075599876,122.252443739457)) ;
#29683 = CARTESIAN_POINT('Ctrl Pts',(-19.2505801464928,30.0816361637616,121.912649736868)) ;
#29684 = CARTESIAN_POINT('Ctrl Pts',(-19.2823241699332,29.9016470833988,122.212483121513)) ;
#29685 = CARTESIAN_POINT('Ctrl Pts',(-19.5143516088782,30.0916758828626,121.907994125418)) ;
#29686 = CARTESIAN_POINT('Ctrl Pts',(-19.4933414803542,29.9116868024998,122.208759920945)) ;
#29687 = CARTESIAN_POINT('Ctrl Pts',(-19.7710473972636,30.1015640547819,121.948463714533)) ;
#29688 = CARTESIAN_POINT('Ctrl Pts',(-19.6986971847122,29.921574974419,122.241136724367)) ;
#29689 = CARTESIAN_POINT('Ctrl Pts',(-20.0194726827981,30.1115536171989,122.033282181041)) ;
#29690 = CARTESIAN_POINT('Ctrl Pts',(-19.897436877706,29.931564536836,122.30899253618)) ;
#29691 = CARTESIAN_POINT('Ctrl Pts',(-20.2485888048623,30.1215119893936,122.159725978258)) ;
#29692 = CARTESIAN_POINT('Ctrl Pts',(-20.0807288910839,29.9415229090307,122.410148456545)) ;
#29693 = CARTESIAN_POINT('Ctrl Pts',(-20.451481155513,30.1314120636243,122.322590700227)) ;
#29694 = CARTESIAN_POINT('Ctrl Pts',(-20.2430415629541,29.9514229832614,122.540440622386)) ;
#29695 = CARTESIAN_POINT('Ctrl Pts',(-20.6255019413428,30.1414581599979,122.521102011054)) ;
#29696 = CARTESIAN_POINT('Ctrl Pts',(-20.3822574929672,29.961469079635,122.699250490915)) ;
#29697 = CARTESIAN_POINT('Ctrl Pts',(-20.7605632740528,30.151366743995,122.743737177707)) ;
#29698 = CARTESIAN_POINT('Ctrl Pts',(-20.4903053110624,29.9713776636321,122.877358615472)) ;
#29699 = CARTESIAN_POINT('Ctrl Pts',(-20.8563375787038,30.1613773225859,122.988755129718)) ;
#29700 = CARTESIAN_POINT('Ctrl Pts',(-20.5669238525766,29.981388242223,123.073373289288)) ;
#29701 = CARTESIAN_POINT('Ctrl Pts',(-20.9076881587369,30.1714064806987,123.247269528944)) ;
#29702 = CARTESIAN_POINT('Ctrl Pts',(-20.6080032779403,29.9914174003359,123.28018509895)) ;
#29703 = CARTESIAN_POINT('Ctrl Pts',(-20.913643859901,30.1812593625368,123.506108579083)) ;
#29704 = CARTESIAN_POINT('Ctrl Pts',(-20.6127668237937,30.0012702821739,123.4872553494)) ;
#29705 = CARTESIAN_POINT('Ctrl Pts',(-20.8749374874299,30.1912189236878,123.764965708006)) ;
#29706 = CARTESIAN_POINT('Ctrl Pts',(-20.5818009891085,30.0112298433249,123.694340561445)) ;
#29707 = CARTESIAN_POINT('Ctrl Pts',(-20.7907663164554,30.2012573582769,124.014958246547)) ;
#29708 = CARTESIAN_POINT('Ctrl Pts',(-20.5144631445051,30.021268277914,123.89433442643)) ;
#29709 = CARTESIAN_POINT('Ctrl Pts',(-20.6669470046296,30.211130630504,124.243014320118)) ;
#29710 = CARTESIAN_POINT('Ctrl Pts',(-20.4154074251945,30.0311415501411,124.07677811357)) ;
#29711 = CARTESIAN_POINT('Ctrl Pts',(-20.5021342923516,30.2212038724976,124.450093173102)) ;
#29712 = CARTESIAN_POINT('Ctrl Pts',(-20.2835564026306,30.0412147921347,124.242440954527)) ;
#29713 = CARTESIAN_POINT('Ctrl Pts',(-20.3089888716899,30.2310242040306,124.621335698669)) ;
#29714 = CARTESIAN_POINT('Ctrl Pts',(-20.1290405109537,30.0510351236678,124.379433600609)) ;
#29715 = CARTESIAN_POINT('Ctrl Pts',(-20.0834917211719,30.2411028652574,124.760137415769)) ;
#29716 = CARTESIAN_POINT('Ctrl Pts',(-19.9486421144359,30.0611137848945,124.49047459601)) ;
#29717 = CARTESIAN_POINT('Ctrl Pts',(-19.8427824861803,30.2509544605516,124.855609977345)) ;
#29718 = CARTESIAN_POINT('Ctrl Pts',(-19.7560754671688,30.0709653801888,124.566851648864)) ;
#29719 = CARTESIAN_POINT('Ctrl Pts',(-19.5836045391597,30.2610275957804,124.909215904106)) ;
#29720 = CARTESIAN_POINT('Ctrl Pts',(-19.5487326449223,30.0810385154176,124.609735875249)) ;
#29721 = CARTESIAN_POINT('Ctrl Pts',(-19.3250420856673,30.2708700313055,124.916790254833)) ;
#29722 = CARTESIAN_POINT('Ctrl Pts',(-19.3418837978834,30.0908809509426,124.615794714185)) ;
#29723 = CARTESIAN_POINT('Ctrl Pts',(-19.0654078751379,30.2808508004389,124.879699535808)) ;
#29724 = CARTESIAN_POINT('Ctrl Pts',(-19.1341767293187,30.100861720076,124.58612178724)) ;
#29725 = CARTESIAN_POINT('Ctrl Pts',(-18.8153894691253,30.2908679016827,124.797325621791)) ;
#29726 = CARTESIAN_POINT('Ctrl Pts',(-18.9341621618172,30.1108788213199,124.520222166044)) ;
#29727 = CARTESIAN_POINT('Ctrl Pts',(-18.5862012535222,30.3007563492846,124.674812609811)) ;
#29728 = CARTESIAN_POINT('Ctrl Pts',(-18.75081252989,30.1207672689217,124.422211818588)) ;
#29729 = CARTESIAN_POINT('Ctrl Pts',(-18.378326748722,30.3108120634654,124.511700910524)) ;
#29730 = CARTESIAN_POINT('Ctrl Pts',(-18.5845129649496,30.1308229831026,124.29172200353)) ;
#29731 = CARTESIAN_POINT('Ctrl Pts',(-18.2050407985295,30.3206872698793,124.31849941652)) ;
#29732 = CARTESIAN_POINT('Ctrl Pts',(-18.4458851060229,30.1406981895164,124.137161249517)) ;
#29733 = CARTESIAN_POINT('Ctrl Pts',(-18.065746667546,30.330682322352,124.095826539079)) ;
#29734 = CARTESIAN_POINT('Ctrl Pts',(-18.3344500579577,30.1506932419891,123.959022954298)) ;
#29735 = CARTESIAN_POINT('Ctrl Pts',(-17.9673568014916,30.3407042063141,123.851520456621)) ;
#29736 = CARTESIAN_POINT('Ctrl Pts',(-18.2557384543419,30.1607151259512,123.763577933142)) ;
#29737 = CARTESIAN_POINT('Ctrl Pts',(-17.9132391133063,30.3506081788434,123.596944459868)) ;
#29738 = CARTESIAN_POINT('Ctrl Pts',(-18.2124447103049,30.1706190984805,123.559917834642)) ;
#29739 = CARTESIAN_POINT('Ctrl Pts',(-17.9036909635563,30.3605966755043,123.334628818861)) ;
#29740 = CARTESIAN_POINT('Ctrl Pts',(-18.2048063513031,30.1806075951414,123.350065504462)) ;
#29741 = CARTESIAN_POINT('Ctrl Pts',(-17.9399190541115,30.3705604727523,123.075322497842)) ;
#29742 = CARTESIAN_POINT('Ctrl Pts',(-18.2337889737254,30.1905713923894,123.142620833117)) ;
#29743 = CARTESIAN_POINT('Ctrl Pts',(-18.019542401481,30.3804644960603,122.827507706759)) ;
#29744 = CARTESIAN_POINT('Ctrl Pts',(-18.2974874574404,30.2004754156974,122.944369728192)) ;
#29745 = CARTESIAN_POINT('Ctrl Pts',(-18.1430719623568,30.3905249993819,122.593799613876)) ;
#29746 = CARTESIAN_POINT('Ctrl Pts',(-18.3963113223776,30.2105359190191,122.757403048071)) ;
#29747 = CARTESIAN_POINT('Ctrl Pts',(-18.3015384279696,30.4003655345218,122.38939813401)) ;
#29748 = CARTESIAN_POINT('Ctrl Pts',(-18.5230837819883,30.2203764541589,122.593882800201)) ;
#29749 = CARTESIAN_POINT('Ctrl Pts',(-18.4971286724099,30.4104277552264,122.211494771059)) ;
#29750 = CARTESIAN_POINT('Ctrl Pts',(-18.6795561458151,30.2304386748635,122.451559855394)) ;
#29751 = CARTESIAN_POINT('Ctrl Pts',(-18.7171521979687,30.4203249090026,122.072778646605)) ;
#29752 = CARTESIAN_POINT('Ctrl Pts',(-18.8555742859337,30.2403358286398,122.340587380024)) ;
#29753 = CARTESIAN_POINT('Ctrl Pts',(-18.9583979844501,30.4302560423881,121.973238309069)) ;
#29754 = CARTESIAN_POINT('Ctrl Pts',(-19.0485702956595,30.2502669620252,122.260955120397)) ;
#29755 = CARTESIAN_POINT('Ctrl Pts',(-19.216180617271,30.4402984175338,121.916755158295)) ;
#29756 = CARTESIAN_POINT('Ctrl Pts',(-19.2547965323524,30.260309337171,122.215768415683)) ;
#29757 = CARTESIAN_POINT('Ctrl Pts',(-19.4757597411927,30.4501843553,121.905857590778)) ;
#29758 = CARTESIAN_POINT('Ctrl Pts',(-19.4624589536106,30.2701952749371,122.207050197027)) ;
#29759 = CARTESIAN_POINT('Ctrl Pts',(-19.7361687240311,30.4601801982848,121.940170527014)) ;
#29760 = CARTESIAN_POINT('Ctrl Pts',(-19.6707860227431,30.2801911179219,122.234500220989)) ;
#29761 = CARTESIAN_POINT('Ctrl Pts',(-19.9853388632678,30.4701221761634,122.018791502423)) ;
#29762 = CARTESIAN_POINT('Ctrl Pts',(-19.8701217511132,30.2901330958005,122.297396567724)) ;
#29763 = CARTESIAN_POINT('Ctrl Pts',(-20.2176167858868,30.4800815506444,122.139363771227)) ;
#29764 = CARTESIAN_POINT('Ctrl Pts',(-20.0559439306465,30.3000924702815,122.393853866718)) ;
#29765 = CARTESIAN_POINT('Ctrl Pts',(-20.4263236161457,30.4900781664782,122.298948878856)) ;
#29766 = CARTESIAN_POINT('Ctrl Pts',(-20.2229095545966,30.3100890861153,122.521521545282)) ;
#29767 = CARTESIAN_POINT('Ctrl Pts',(-20.6045380695498,30.5001123850517,122.493286837832)) ;
#29768 = CARTESIAN_POINT('Ctrl Pts',(-20.3654814345688,30.3201233046888,122.676991771903)) ;
#29769 = CARTESIAN_POINT('Ctrl Pts',(-20.7440103711108,30.5099654522623,122.711437778196)) ;
#29770 = CARTESIAN_POINT('Ctrl Pts',(-20.477059029593,30.3299763718994,122.851511380086)) ;
#29771 = CARTESIAN_POINT('Ctrl Pts',(-20.8452704862501,30.5199257101399,122.952793072304)) ;
#29772 = CARTESIAN_POINT('Ctrl Pts',(-20.5580675344423,30.339936629777,123.044595041422)) ;
#29773 = CARTESIAN_POINT('Ctrl Pts',(-20.9031858777252,30.5299547368455,123.209917654151)) ;
#29774 = CARTESIAN_POINT('Ctrl Pts',(-20.604400374506,30.3499656564826,123.250294668849)) ;
#29775 = CARTESIAN_POINT('Ctrl Pts',(-20.9155052003231,30.5398649438799,123.470044892547)) ;
#29776 = CARTESIAN_POINT('Ctrl Pts',(-20.6142563408965,30.3598758635171,123.458395733584)) ;
#29777 = CARTESIAN_POINT('Ctrl Pts',(-20.8830672767706,30.5497998545275,123.729108750999)) ;
#29778 = CARTESIAN_POINT('Ctrl Pts',(-20.5883067737471,30.3698107741647,123.665646384641)) ;
#29779 = CARTESIAN_POINT('Ctrl Pts',(-20.8050869196827,30.5598409847068,123.981184304442)) ;
#29780 = CARTESIAN_POINT('Ctrl Pts',(-20.5259230651749,30.3798519043439,123.867307162557)) ;
#29781 = CARTESIAN_POINT('Ctrl Pts',(-20.6865234424483,30.5697281250767,124.212396007676)) ;
#29782 = CARTESIAN_POINT('Ctrl Pts',(-20.4310732809217,30.3897390447139,124.052276102492)) ;
#29783 = CARTESIAN_POINT('Ctrl Pts',(-20.5283158328247,30.5797204026127,124.421949250781)) ;
#29784 = CARTESIAN_POINT('Ctrl Pts',(-20.3045079305415,30.3997313222498,124.219919049695)) ;
#29785 = CARTESIAN_POINT('Ctrl Pts',(-20.336893127493,30.589668945881,124.600034325977)) ;
#29786 = CARTESIAN_POINT('Ctrl Pts',(-20.1513706158548,30.4096798655181,124.362387386942)) ;
#29787 = CARTESIAN_POINT('Ctrl Pts',(-20.117949669728,30.5996056206982,124.742302120517)) ;
#29788 = CARTESIAN_POINT('Ctrl Pts',(-19.9762167528585,30.4196165403353,124.476202075347)) ;
#29789 = CARTESIAN_POINT('Ctrl Pts',(-19.8765801266705,30.6095890416346,124.845182022236)) ;
#29790 = CARTESIAN_POINT('Ctrl Pts',(-19.7831216739518,30.4295999612717,124.558506786004)) ;
#29791 = CARTESIAN_POINT('Ctrl Pts',(-19.619448424608,30.6196313568238,124.904513792509)) ;
#29792 = CARTESIAN_POINT('Ctrl Pts',(-19.577416370328,30.4396422764609,124.605973056573)) ;
#29793 = CARTESIAN_POINT('Ctrl Pts',(-19.3612267210301,30.629471674263,124.918439915204)) ;
#29794 = CARTESIAN_POINT('Ctrl Pts',(-19.3708401454886,30.4494825939001,124.617114839488)) ;
#29795 = CARTESIAN_POINT('Ctrl Pts',(-19.0994956244019,30.6395013783205,124.887333257162)) ;
#29796 = CARTESIAN_POINT('Ctrl Pts',(-19.1614550554373,30.4595122979576,124.592230579924)) ;
#29797 = CARTESIAN_POINT('Ctrl Pts',(-18.84757050077,30.649522335043,124.810642476183)) ;
#29798 = CARTESIAN_POINT('Ctrl Pts',(-18.9599146662731,30.4695332546801,124.530878830767)) ;
#29799 = CARTESIAN_POINT('Ctrl Pts',(-18.6160882477537,30.6593888773466,124.69379526334)) ;
#29800 = CARTESIAN_POINT('Ctrl Pts',(-18.7747291880007,30.4793997969837,124.437402426566)) ;
#29801 = CARTESIAN_POINT('Ctrl Pts',(-18.4041389450964,30.6694599772918,124.535339469786)) ;
#29802 = CARTESIAN_POINT('Ctrl Pts',(-18.6051688617141,30.4894708969289,124.310638472156)) ;
#29803 = CARTESIAN_POINT('Ctrl Pts',(-18.2270241518516,30.6793020514693,124.346845255088)) ;
#29804 = CARTESIAN_POINT('Ctrl Pts',(-18.4634769547701,30.4993129711065,124.159844592022)) ;
#29805 = CARTESIAN_POINT('Ctrl Pts',(-18.0828214570917,30.6892628460564,124.128395071014)) ;
#29806 = CARTESIAN_POINT('Ctrl Pts',(-18.3481139027231,30.5092737656935,123.98508542601)) ;
#29807 = CARTESIAN_POINT('Ctrl Pts',(-17.9784145006715,30.6993007189572,123.886162207482)) ;
#29808 = CARTESIAN_POINT('Ctrl Pts',(-18.2645872182837,30.5193116385943,123.791299501671)) ;
#29809 = CARTESIAN_POINT('Ctrl Pts',(-17.9181661940265,30.7091750045013,123.63373426702)) ;
#29810 = CARTESIAN_POINT('Ctrl Pts',(-18.216387518212,30.5291859241384,123.589358233217)) ;
#29811 = CARTESIAN_POINT('Ctrl Pts',(-17.9023753757216,30.7192447549152,123.369619175597)) ;
#29812 = CARTESIAN_POINT('Ctrl Pts',(-18.203753574066,30.5392556745523,123.378065957705)) ;
#29813 = CARTESIAN_POINT('Ctrl Pts',(-17.9318397718058,30.7290780394499,123.112874144442)) ;
#29814 = CARTESIAN_POINT('Ctrl Pts',(-18.2273236794525,30.549088959087,123.172670800708)) ;
#29815 = CARTESIAN_POINT('Ctrl Pts',(-18.0061852690051,30.7391083802499,122.859997359419)) ;
#29816 = CARTESIAN_POINT('Ctrl Pts',(-18.2867986965905,30.559119299887,122.970368894539)) ;
#29817 = CARTESIAN_POINT('Ctrl Pts',(-18.1240293775023,30.7491403042495,122.624160309324)) ;
#29818 = CARTESIAN_POINT('Ctrl Pts',(-18.381072852259,30.5691512238866,122.781698614195)) ;
#29819 = CARTESIAN_POINT('Ctrl Pts',(-18.2773844645063,30.7589688391854,122.416346355351)) ;
#29820 = CARTESIAN_POINT('Ctrl Pts',(-18.5037551769327,30.5789797588226,122.615447430621)) ;
#29821 = CARTESIAN_POINT('Ctrl Pts',(-18.4671493140597,30.7689626169501,122.234795344671)) ;
#29822 = CARTESIAN_POINT('Ctrl Pts',(-18.6555658924433,30.5889735365872,122.470205578814)) ;
#29823 = CARTESIAN_POINT('Ctrl Pts',(-18.6865926220814,30.7789903274356,122.088882738916)) ;
#29824 = CARTESIAN_POINT('Ctrl Pts',(-18.8311197585545,30.5990012470728,122.353474263841)) ;
#29825 = CARTESIAN_POINT('Ctrl Pts',(-18.924548918543,30.7888787382696,121.984461740876)) ;
#29826 = CARTESIAN_POINT('Ctrl Pts',(-19.0214835756871,30.6088896579067,122.269936340011)) ;
#29827 = CARTESIAN_POINT('Ctrl Pts',(-19.1791493957345,30.7988555888051,121.921954029357)) ;
#29828 = CARTESIAN_POINT('Ctrl Pts',(-19.2251633755617,30.6188665084423,122.219928660186)) ;
#29829 = CARTESIAN_POINT('Ctrl Pts',(-19.4411836962534,30.8088473853556,121.904551040875)) ;
#29830 = CARTESIAN_POINT('Ctrl Pts',(-19.4347905867356,30.6288583049927,122.206004671625)) ;
#29831 = CARTESIAN_POINT('Ctrl Pts',(-19.7033209422536,30.8188833914493,121.933349289194)) ;
#29832 = CARTESIAN_POINT('Ctrl Pts',(-19.6445006241245,30.6388943110864,122.229041739031)) ;
#29833 = CARTESIAN_POINT('Ctrl Pts',(-19.9519531581678,30.8287341257121,122.005489324719)) ;
#29834 = CARTESIAN_POINT('Ctrl Pts',(-19.84340606214,30.6487450453492,122.286751981054)) ;
#29835 = CARTESIAN_POINT('Ctrl Pts',(-20.1877451626918,30.8387253842403,122.12090221111)) ;
#29836 = CARTESIAN_POINT('Ctrl Pts',(-20.0320402961377,30.6587363038774,122.379080697725)) ;
#29837 = CARTESIAN_POINT('Ctrl Pts',(-20.3985067246429,30.8486432791435,122.274284311981)) ;
#29838 = CARTESIAN_POINT('Ctrl Pts',(-20.2006501933195,30.6686541987806,122.50178471108)) ;
#29839 = CARTESIAN_POINT('Ctrl Pts',(-20.5814557895788,30.8586714208065,122.463931047394)) ;
#29840 = CARTESIAN_POINT('Ctrl Pts',(-20.3470107187746,30.6786823404437,122.653500909386)) ;
#29841 = CARTESIAN_POINT('Ctrl Pts',(-20.726703975958,30.8685565889224,122.679309656422)) ;
#29842 = CARTESIAN_POINT('Ctrl Pts',(-20.4632103980333,30.6885675085595,122.82580232508)) ;
#29843 = CARTESIAN_POINT('Ctrl Pts',(-20.8340446604117,30.8785459524284,122.918876333056)) ;
#29844 = CARTESIAN_POINT('Ctrl Pts',(-20.5490845941834,30.6985568720655,123.017454790216)) ;
#29845 = CARTESIAN_POINT('Ctrl Pts',(-20.8979488651774,30.8885870874385,123.174891648262)) ;
#29846 = CARTESIAN_POINT('Ctrl Pts',(-20.6002096966955,30.7085980070756,123.222266683441)) ;
#29847 = CARTESIAN_POINT('Ctrl Pts',(-20.916470523059,30.8984197556265,123.432614768819)) ;
#29848 = CARTESIAN_POINT('Ctrl Pts',(-20.6150288055355,30.7184306752636,123.42844428619)) ;
#29849 = CARTESIAN_POINT('Ctrl Pts',(-20.8902751541959,30.908413658581,123.693933046635)) ;
#29850 = CARTESIAN_POINT('Ctrl Pts',(-20.5940744640968,30.7284245782181,123.637499006698)) ;
#29851 = CARTESIAN_POINT('Ctrl Pts',(-20.8183135578191,30.9184429436655,123.947479863912)) ;
#29852 = CARTESIAN_POINT('Ctrl Pts',(-20.5365069824791,30.7384538633026,123.840336987593)) ;
#29853 = CARTESIAN_POINT('Ctrl Pts',(-20.705558307434,30.9283184721074,124.181239071671)) ;
#29854 = CARTESIAN_POINT('Ctrl Pts',(-20.4463047552757,30.7483293917445,124.027344708354)) ;
#29855 = CARTESIAN_POINT('Ctrl Pts',(-20.55227636311,30.9383187547235,124.394663488926)) ;
#29856 = CARTESIAN_POINT('Ctrl Pts',(-20.3236808563954,30.7583296743606,124.198085320578)) ;
#29857 = CARTESIAN_POINT('Ctrl Pts',(-20.3660263502005,30.9482307707805,124.576805636963)) ;
#29858 = CARTESIAN_POINT('Ctrl Pts',(-20.1746825091219,30.7682416904176,124.343800207381)) ;
#29859 = CARTESIAN_POINT('Ctrl Pts',(-20.148238159027,30.9582728461195,124.725798531691)) ;
#29860 = CARTESIAN_POINT('Ctrl Pts',(-20.0004530415488,30.7782837657566,124.462996211481)) ;
#29861 = CARTESIAN_POINT('Ctrl Pts',(-19.9112599341149,30.9681726787756,124.833177229003)) ;
#29862 = CARTESIAN_POINT('Ctrl Pts',(-19.8108716507074,30.7881835984127,124.548900832387)) ;
#29863 = CARTESIAN_POINT('Ctrl Pts',(-19.6570385216495,30.9781650793536,124.898943043692)) ;
#29864 = CARTESIAN_POINT('Ctrl Pts',(-19.6074951324964,30.7981759989908,124.601515467701)) ;
#29865 = CARTESIAN_POINT('Ctrl Pts',(-19.3941289164041,30.988199101113,124.91918719167)) ;
#29866 = CARTESIAN_POINT('Ctrl Pts',(-19.3971675920454,30.8082100207501,124.617712800097)) ;
#29867 = CARTESIAN_POINT('Ctrl Pts',(-19.1361050769742,30.9980637119542,124.894240456014)) ;
#29868 = CARTESIAN_POINT('Ctrl Pts',(-19.1907487911247,30.8180746315913,124.597757506025)) ;
#29869 = CARTESIAN_POINT('Ctrl Pts',(-18.8829168166101,31.0080561114154,124.824588928341)) ;
#29870 = CARTESIAN_POINT('Ctrl Pts',(-18.9881977022827,30.8280670310525,124.542038356411)) ;
#29871 = CARTESIAN_POINT('Ctrl Pts',(-18.6449556256928,31.0180880647483,124.711122383822)) ;
#29872 = CARTESIAN_POINT('Ctrl Pts',(-18.7978278575721,30.8380989843854,124.451266991065)) ;
#29873 = CARTESIAN_POINT('Ctrl Pts',(-18.433613598993,31.0279544236899,124.56090527812)) ;
#29874 = CARTESIAN_POINT('Ctrl Pts',(-18.6287533485745,30.8479653433271,124.331095266806)) ;
#29875 = CARTESIAN_POINT('Ctrl Pts',(-18.2490556295149,31.0379418991757,124.374338785496)) ;
#29876 = CARTESIAN_POINT('Ctrl Pts',(-18.4811055111565,30.8579528188129,124.181843656717)) ;
#29877 = CARTESIAN_POINT('Ctrl Pts',(-18.1001763827017,31.0478868053642,124.159502137119)) ;
#29878 = CARTESIAN_POINT('Ctrl Pts',(-18.3620004446378,30.8678977250013,124.009975722139)) ;
#29879 = CARTESIAN_POINT('Ctrl Pts',(-17.9899251037199,31.0579317700244,123.919685682728)) ;
#29880 = CARTESIAN_POINT('Ctrl Pts',(-18.2737974607781,30.8779426896616,123.818123443375)) ;
#29881 = CARTESIAN_POINT('Ctrl Pts',(-17.9239698947395,31.0677935769293,123.669038395262)) ;
#29882 = CARTESIAN_POINT('Ctrl Pts',(-18.221031284142,30.8878044965664,123.617606494588)) ;
#29883 = CARTESIAN_POINT('Ctrl Pts',(-17.9017545884407,31.0777862492351,123.407409964502)) ;
#29884 = CARTESIAN_POINT('Ctrl Pts',(-18.2032568478911,30.8977971688722,123.408304011957)) ;
#29885 = CARTESIAN_POINT('Ctrl Pts',(-17.9251878868137,31.0877149201804,123.147532162219)) ;
#29886 = CARTESIAN_POINT('Ctrl Pts',(-18.2220012797528,30.9077258398175,123.200401751263)) ;
#29887 = CARTESIAN_POINT('Ctrl Pts',(-17.9931295756622,31.0976674624057,122.894987346514)) ;
#29888 = CARTESIAN_POINT('Ctrl Pts',(-18.2763524482962,30.9176783820428,122.998365442682)) ;
#29889 = CARTESIAN_POINT('Ctrl Pts',(-18.1043255909368,31.1076688184016,122.656813330348)) ;
#29890 = CARTESIAN_POINT('Ctrl Pts',(-18.3653072153254,30.9276797380387,122.807825340817)) ;
#29891 = CARTESIAN_POINT('Ctrl Pts',(-18.2558710625769,31.1176974306763,122.441217023634)) ;
#29892 = CARTESIAN_POINT('Ctrl Pts',(-18.486541760213,30.9377083503134,122.63534705266)) ;
#29893 = CARTESIAN_POINT('Ctrl Pts',(-18.4392436560099,31.1275617652258,122.257966085798)) ;
#29894 = CARTESIAN_POINT('Ctrl Pts',(-18.6332381127442,30.9475726848629,122.488744871235)) ;
#29895 = CARTESIAN_POINT('Ctrl Pts',(-18.6541277020736,31.1375540893024,122.107106052772)) ;
#29896 = CARTESIAN_POINT('Ctrl Pts',(-18.805144006808,30.9575650089395,122.368055041523)) ;
#29897 = CARTESIAN_POINT('Ctrl Pts',(-18.8903979931826,31.1474815816683,121.99639777191)) ;
#29898 = CARTESIAN_POINT('Ctrl Pts',(-18.9941591920697,30.9674925013054,122.279486427225)) ;
#29899 = CARTESIAN_POINT('Ctrl Pts',(-19.1447705223875,31.1575089402191,121.927739862365)) ;
#29900 = CARTESIAN_POINT('Ctrl Pts',(-19.1976565800842,30.9775198598562,122.224557940461)) ;
#29901 = CARTESIAN_POINT('Ctrl Pts',(-19.403557785468,31.1673953582702,121.904339822956)) ;
#29902 = CARTESIAN_POINT('Ctrl Pts',(-19.40468609459,30.9874062779074,122.205835676203)) ;
#29903 = CARTESIAN_POINT('Ctrl Pts',(-19.6662117593913,31.1774270930056,121.926411212978)) ;
#29904 = CARTESIAN_POINT('Ctrl Pts',(-19.6148094082564,30.9974380126427,122.223490535075)) ;
#29905 = CARTESIAN_POINT('Ctrl Pts',(-19.9173816828502,31.1873086742489,121.992520931665)) ;
#29906 = CARTESIAN_POINT('Ctrl Pts',(-19.815745871323,31.007319593886,122.276376119868)) ;
#29907 = CARTESIAN_POINT('Ctrl Pts',(-20.1575099536661,31.1973706522812,122.103127502672)) ;
#29908 = CARTESIAN_POINT('Ctrl Pts',(-20.0078493692217,31.0173815719183,122.364859298836)) ;
#29909 = CARTESIAN_POINT('Ctrl Pts',(-20.3704779128565,31.2072277306429,122.250647114545)) ;
#29910 = CARTESIAN_POINT('Ctrl Pts',(-20.1782250129861,31.02723865028,122.482873132973)) ;
#29911 = CARTESIAN_POINT('Ctrl Pts',(-20.557479635411,31.2172223037489,122.435014859895)) ;
#29912 = CARTESIAN_POINT('Ctrl Pts',(-20.3278279402508,31.037233223386,122.630365704853)) ;
#29913 = CARTESIAN_POINT('Ctrl Pts',(-20.7087042530508,31.2271481000365,122.647587798087)) ;
#29914 = CARTESIAN_POINT('Ctrl Pts',(-20.4488094657624,31.0471590196736,122.8004227559)) ;
#29915 = CARTESIAN_POINT('Ctrl Pts',(-20.8218837391766,31.2371734672062,122.885470873075)) ;
#29916 = CARTESIAN_POINT('Ctrl Pts',(-20.539355037212,31.0571843868434,122.99072823021)) ;
#29917 = CARTESIAN_POINT('Ctrl Pts',(-20.8912500206041,31.2470695468601,123.136118325641)) ;
#29918 = CARTESIAN_POINT('Ctrl Pts',(-20.594850255258,31.0670804664972,123.191245492355)) ;
#29919 = CARTESIAN_POINT('Ctrl Pts',(-20.916817797818,31.2570646265657,123.397534145115)) ;
#29920 = CARTESIAN_POINT('Ctrl Pts',(-20.6153065879517,31.0770755462028,123.400378543151)) ;
#29921 = CARTESIAN_POINT('Ctrl Pts',(-20.8960973227342,31.2670897143815,123.660166672547)) ;
#29922 = CARTESIAN_POINT('Ctrl Pts',(-20.5987327498281,31.0871006340186,123.610482259063)) ;
#29923 = CARTESIAN_POINT('Ctrl Pts',(-20.809893476644,31.2802735367488,123.995726533553)) ;
#29924 = CARTESIAN_POINT('Ctrl Pts',(-20.5297709305419,31.1002844563859,123.87894293253)) ;
#29925 = CARTESIAN_POINT('Ctrl Pts',(-20.6369390480152,31.2935956548947,124.30466223955)) ;
#29926 = CARTESIAN_POINT('Ctrl Pts',(-20.3913865526123,31.1136065745318,124.126114241275)) ;
#29927 = CARTESIAN_POINT('Ctrl Pts',(-20.3908148582284,31.3069748645223,124.555818133117)) ;
#29928 = CARTESIAN_POINT('Ctrl Pts',(-20.1945187656795,31.1269857841594,124.327003669048)) ;
#29929 = CARTESIAN_POINT('Ctrl Pts',(-20.1809438414753,31.3168131017665,124.706820601801)) ;
#29930 = CARTESIAN_POINT('Ctrl Pts',(-20.0266169655379,31.1368240214036,124.447815030813)) ;
#29931 = CARTESIAN_POINT('Ctrl Pts',(-19.9425721439745,31.3268860250252,124.821852782534)) ;
#29932 = CARTESIAN_POINT('Ctrl Pts',(-19.8359226633174,31.1468969446624,124.539840740485)) ;
#29933 = CARTESIAN_POINT('Ctrl Pts',(-19.6932575438715,31.3367426664803,124.89218888602)) ;
#29934 = CARTESIAN_POINT('Ctrl Pts',(-19.6364695236485,31.1567535861175,124.596111832383)) ;
#29935 = CARTESIAN_POINT('Ctrl Pts',(-19.4322556852193,31.3467280419864,124.919201640466)) ;
#29936 = CARTESIAN_POINT('Ctrl Pts',(-19.4276731793723,31.1667389616235,124.617725775355)) ;
#29937 = CARTESIAN_POINT('Ctrl Pts',(-19.0841345592013,31.3600120734468,124.893999424143)) ;
#29938 = CARTESIAN_POINT('Ctrl Pts',(-19.1491518620383,31.180022993084,124.597557799836)) ;
#29939 = CARTESIAN_POINT('Ctrl Pts',(-18.6686831095259,31.3765308653172,124.751522351196)) ;
#29940 = CARTESIAN_POINT('Ctrl Pts',(-18.8168267270378,31.1965417849543,124.483599784169)) ;
#29941 = CARTESIAN_POINT('Ctrl Pts',(-18.3221176258635,31.3933165823238,124.470780414967)) ;
#29942 = CARTESIAN_POINT('Ctrl Pts',(-18.5395236640967,31.2133275019609,124.258964588696)) ;
#29943 = CARTESIAN_POINT('Ctrl Pts',(-18.1195171640873,31.4064297308328,124.19192546978)) ;
#29944 = CARTESIAN_POINT('Ctrl Pts',(-18.3774781924197,31.2264406504699,124.035919165873)) ;
#29945 = CARTESIAN_POINT('Ctrl Pts',(-18.0029767278721,31.416465279913,123.955390640417)) ;
#29946 = CARTESIAN_POINT('Ctrl Pts',(-18.2842367998029,31.2364761995501,123.846683979849)) ;
#29947 = CARTESIAN_POINT('Ctrl Pts',(-17.930131161295,31.4264813360924,123.702427282653)) ;
#29948 = CARTESIAN_POINT('Ctrl Pts',(-18.2259601153952,31.2464922557295,123.644318871564)) ;
#29949 = CARTESIAN_POINT('Ctrl Pts',(-17.8927981854828,31.4396593719584,123.358188928687)) ;
#29950 = CARTESIAN_POINT('Ctrl Pts',(-18.1960923899022,31.2596702915955,123.368912638922)) ;
#29951 = CARTESIAN_POINT('Ctrl Pts',(-17.9589427761027,31.4562612491455,122.921846253614)) ;
#29952 = CARTESIAN_POINT('Ctrl Pts',(-18.2490034305915,31.2762721687826,123.019854359994)) ;
#29953 = CARTESIAN_POINT('Ctrl Pts',(-18.2153452936868,31.4763243937614,122.454312103361)) ;
#29954 = CARTESIAN_POINT('Ctrl Pts',(-18.4541225899952,31.2963353133985,122.645820297505)) ;
#29955 = CARTESIAN_POINT('Ctrl Pts',(-18.6105119795525,31.4961252838451,122.106643007625)) ;
#29956 = CARTESIAN_POINT('Ctrl Pts',(-18.7702543020853,31.3161362034822,122.36768303858)) ;
#29957 = CARTESIAN_POINT('Ctrl Pts',(-19.1034924936999,31.5160684091238,121.912133008607)) ;
#29958 = CARTESIAN_POINT('Ctrl Pts',(-19.164637971874,31.3360793287609,122.212071605184)) ;
#29959 = CARTESIAN_POINT('Ctrl Pts',(-19.6321465341764,31.5359664542434,121.89791137193)) ;
#29960 = CARTESIAN_POINT('Ctrl Pts',(-19.5875618065476,31.3559773738805,122.200691277358)) ;
#29961 = CARTESIAN_POINT('Ctrl Pts',(-20.1341066883384,31.5558522138702,122.063616102464)) ;
#29962 = CARTESIAN_POINT('Ctrl Pts',(-19.9891315918773,31.3758631335073,122.333252851735)) ;
#29963 = CARTESIAN_POINT('Ctrl Pts',(-20.5525283110554,31.57591738905,122.394200252169)) ;
#29964 = CARTESIAN_POINT('Ctrl Pts',(-20.3238701259959,31.3959283086872,122.597717694145)) ;
#29965 = CARTESIAN_POINT('Ctrl Pts',(-20.8296000415882,31.5957440321528,122.84254361497)) ;
#29966 = CARTESIAN_POINT('Ctrl Pts',(-20.5455305086285,31.41575495179,122.95639217086)) ;
#29967 = CARTESIAN_POINT('Ctrl Pts',(-20.9388687495492,31.6156527416012,123.360136077141)) ;
#29968 = CARTESIAN_POINT('Ctrl Pts',(-20.6329476561718,31.4356636612383,123.370466593898)) ;
#29969 = CARTESIAN_POINT('Ctrl Pts',(-20.8648791195812,31.635604578633,123.885385533411)) ;
#29970 = CARTESIAN_POINT('Ctrl Pts',(-20.573757693884,31.4556154982701,123.790666808917)) ;
#29971 = CARTESIAN_POINT('Ctrl Pts',(-20.6147262487971,31.6556130533361,124.354604940983)) ;
#29972 = CARTESIAN_POINT('Ctrl Pts',(-20.3736372170781,31.4756239729733,124.166043186308)) ;
#29973 = CARTESIAN_POINT('Ctrl Pts',(-20.2239265792252,31.6754145120976,124.70712499995)) ;
#29974 = CARTESIAN_POINT('Ctrl Pts',(-20.0609969972757,31.4954254317348,124.448061814946)) ;
#29975 = CARTESIAN_POINT('Ctrl Pts',(-19.7329944592127,31.6953714003336,124.907950846951)) ;
#29976 = CARTESIAN_POINT('Ctrl Pts',(-19.6682511534378,31.5153823199707,124.608723469387)) ;
#29977 = CARTESIAN_POINT('Ctrl Pts',(-19.2022559885623,31.7153552377477,124.928017723692)) ;
#29978 = CARTESIAN_POINT('Ctrl Pts',(-19.2436602612597,31.5353661573848,124.624778160052)) ;
#29979 = CARTESIAN_POINT('Ctrl Pts',(-18.7005580952729,31.7351636769686,124.768181953029)) ;
#29980 = CARTESIAN_POINT('Ctrl Pts',(-18.8422995577168,31.5551745966057,124.496909315192)) ;
#29981 = CARTESIAN_POINT('Ctrl Pts',(-18.2796327533169,31.7551493863488,124.444432947283)) ;
#29982 = CARTESIAN_POINT('Ctrl Pts',(-18.505559042595,31.5751603059859,124.237909991823)) ;
#29983 = CARTESIAN_POINT('Ctrl Pts',(-17.9957625956122,31.7750189093641,123.998861683797)) ;
#29984 = CARTESIAN_POINT('Ctrl Pts',(-18.2784622930544,31.5950298290012,123.881451524151)) ;
#29985 = CARTESIAN_POINT('Ctrl Pts',(-17.8804111930879,31.7950396484813,123.479601508631)) ;
#29986 = CARTESIAN_POINT('Ctrl Pts',(-18.1861815644187,31.6150505681184,123.466043484708)) ;
#29987 = CARTESIAN_POINT('Ctrl Pts',(-17.947813732566,31.8148437134583,122.957375358431)) ;
#29988 = CARTESIAN_POINT('Ctrl Pts',(-18.240104726759,31.6348546330954,123.048260409413)) ;
#29989 = CARTESIAN_POINT('Ctrl Pts',(-18.1922019497661,31.834905677189,122.483631625261)) ;
#29990 = CARTESIAN_POINT('Ctrl Pts',(-18.4356159960294,31.6549165968261,122.669266566499)) ;
#29991 = CARTESIAN_POINT('Ctrl Pts',(-18.579670503548,31.8547388574775,122.126047237428)) ;
#29992 = CARTESIAN_POINT('Ctrl Pts',(-18.7455928985157,31.6747497771146,122.383198612062)) ;
#29993 = CARTESIAN_POINT('Ctrl Pts',(-19.0672415407129,31.8746580548036,121.919977102834)) ;
#29994 = CARTESIAN_POINT('Ctrl Pts',(-19.1356512341748,31.6946689744407,122.218343904972)) ;
#29995 = CARTESIAN_POINT('Ctrl Pts',(-19.596473798273,31.8945960799169,121.892968380712)) ;
#29996 = CARTESIAN_POINT('Ctrl Pts',(-19.559037724007,31.714606999554,122.196738778409)) ;
#29997 = CARTESIAN_POINT('Ctrl Pts',(-20.1018977424829,31.914474125973,122.047010861552)) ;
#29998 = CARTESIAN_POINT('Ctrl Pts',(-19.9633772292207,31.7344850456101,122.319975266152)) ;
#29999 = CARTESIAN_POINT('Ctrl Pts',(-20.5266155989396,31.934458860261,122.365876034326)) ;
#30000 = CARTESIAN_POINT('Ctrl Pts',(-20.3031501256687,31.7544697798982,122.575069435507)) ;
#30001 = CARTESIAN_POINT('Ctrl Pts',(-20.8161540516341,31.9543696769395,122.809022005469)) ;
#30002 = CARTESIAN_POINT('Ctrl Pts',(-20.5347790794781,31.7743805965766,122.92958819007)) ;
#30003 = CARTESIAN_POINT('Ctrl Pts',(-20.9372264313366,31.9743686524582,123.326459903439)) ;
#30004 = CARTESIAN_POINT('Ctrl Pts',(-20.6316344224308,31.7943795720954,123.343539156427)) ;
#30005 = CARTESIAN_POINT('Ctrl Pts',(-20.8757007542274,31.9941735731034,123.849340834267)) ;
#30006 = CARTESIAN_POINT('Ctrl Pts',(-20.5824107852335,31.8141844927406,123.761844941543)) ;
#30007 = CARTESIAN_POINT('Ctrl Pts',(-20.6381061492539,32.0141575333947,124.324236585198)) ;
#30008 = CARTESIAN_POINT('Ctrl Pts',(-20.3923321320177,31.8341684530318,124.141760152678)) ;
#30009 = CARTESIAN_POINT('Ctrl Pts',(-20.254277484515,32.0340437371186,124.687750970673)) ;
#30010 = CARTESIAN_POINT('Ctrl Pts',(-20.085266409861,31.8540546567557,124.432569686706)) ;
#30011 = CARTESIAN_POINT('Ctrl Pts',(-19.7682819396191,32.0539929154418,124.89962239012)) ;
#30012 = CARTESIAN_POINT('Ctrl Pts',(-19.696468384716,31.8740038350789,124.60206379762)) ;
#30013 = CARTESIAN_POINT('Ctrl Pts',(-19.2403770539516,32.0738947146813,124.932732853793)) ;
#30014 = CARTESIAN_POINT('Ctrl Pts',(-19.2741434998259,31.8939056343185,124.628548078608)) ;
#30015 = CARTESIAN_POINT('Ctrl Pts',(-18.7330993587673,32.0937733197337,124.784941725984)) ;
#30016 = CARTESIAN_POINT('Ctrl Pts',(-18.868322906955,31.9137842393708,124.510313181707)) ;
#30017 = CARTESIAN_POINT('Ctrl Pts',(-18.3035498467669,32.1138056794594,124.470304693559)) ;
#30018 = CARTESIAN_POINT('Ctrl Pts',(-18.5246822315973,31.9338165990965,124.258593399843)) ;
#30019 = CARTESIAN_POINT('Ctrl Pts',(-18.0587930611329,32.1303874054155,124.103782576889)) ;
#30020 = CARTESIAN_POINT('Ctrl Pts',(-18.3288903810443,31.9503983250526,123.965395758089)) ;
#30021 = CARTESIAN_POINT('Ctrl Pts',(-17.9464384610694,32.1435815757134,123.775785395635)) ;
#30022 = CARTESIAN_POINT('Ctrl Pts',(-18.2389994529127,31.9635924953505,123.702969740174)) ;
#30023 = CARTESIAN_POINT('Ctrl Pts',(-17.8916962164165,32.1568937538066,123.430264324837)) ;
#30024 = CARTESIAN_POINT('Ctrl Pts',(-18.1952099799321,31.9769046734437,123.426608864667)) ;
#30025 = CARTESIAN_POINT('Ctrl Pts',(-17.9374894753685,32.1734599333999,122.99232521224)) ;
#30026 = CARTESIAN_POINT('Ctrl Pts',(-18.2318514252023,31.9934708530371,123.076188915836)) ;
#30027 = CARTESIAN_POINT('Ctrl Pts',(-18.1302718088824,32.1900881282601,122.594703559392)) ;
#30028 = CARTESIAN_POINT('Ctrl Pts',(-18.3860665483606,32.0100990478972,122.758138239794)) ;
#30029 = CARTESIAN_POINT('Ctrl Pts',(-18.3588141057148,32.2033767099699,122.330591540781)) ;
#30030 = CARTESIAN_POINT('Ctrl Pts',(-18.5689151874287,32.023387629607,122.546823962737)) ;
#30031 = CARTESIAN_POINT('Ctrl Pts',(-18.5618539277949,32.2133449580735,122.165112713871)) ;
#30032 = CARTESIAN_POINT('Ctrl Pts',(-18.7313457221629,32.0333558777106,122.414447852175)) ;
#30033 = CARTESIAN_POINT('Ctrl Pts',(-18.7891790717996,32.2232597143296,122.037790376024)) ;
#30034 = CARTESIAN_POINT('Ctrl Pts',(-18.9132084602232,32.0432706339667,122.312590559703)) ;
#30035 = CARTESIAN_POINT('Ctrl Pts',(-19.037513591275,32.2332728649808,121.95074327932)) ;
#30036 = CARTESIAN_POINT('Ctrl Pts',(-19.1118736703297,32.0532837846179,122.242954838167)) ;
#30037 = CARTESIAN_POINT('Ctrl Pts',(-19.2972230251791,32.2432855721828,121.908553873528)) ;
#30038 = CARTESIAN_POINT('Ctrl Pts',(-19.3196523089538,32.0632964918199,122.209207408094)) ;
#30039 = CARTESIAN_POINT('Ctrl Pts',(-19.6446403660395,32.2565048608741,121.9125795524)) ;
#30040 = CARTESIAN_POINT('Ctrl Pts',(-19.5975327596128,32.0765157805112,122.212420869537)) ;
#30041 = CARTESIAN_POINT('Ctrl Pts',(-20.0699198327109,32.2731235418722,122.031411460383)) ;
#30042 = CARTESIAN_POINT('Ctrl Pts',(-19.937823277613,32.0931344615093,122.307507212326)) ;
#30043 = CARTESIAN_POINT('Ctrl Pts',(-20.4284615240151,32.2896884496456,122.28707638829)) ;
#30044 = CARTESIAN_POINT('Ctrl Pts',(-20.224607600475,32.1096993692827,122.512015776509)) ;
#30045 = CARTESIAN_POINT('Ctrl Pts',(-20.6522321703216,32.3030869212564,122.55890721292)) ;
#30046 = CARTESIAN_POINT('Ctrl Pts',(-20.4036500863331,32.1230978408936,122.729503326657)) ;
#30047 = CARTESIAN_POINT('Ctrl Pts',(-20.7796679108865,32.3129281767434,122.783972393412)) ;
#30048 = CARTESIAN_POINT('Ctrl Pts',(-20.5055910403937,32.1329390963805,122.909552376083)) ;
#30049 = CARTESIAN_POINT('Ctrl Pts',(-20.8678841148157,32.3229144923316,123.031085830974)) ;
#30050 = CARTESIAN_POINT('Ctrl Pts',(-20.576163376053,32.1429254119687,123.107244959995)) ;
#30051 = CARTESIAN_POINT('Ctrl Pts',(-20.9117732133019,32.332851099918,123.288538866815)) ;
#30052 = CARTESIAN_POINT('Ctrl Pts',(-20.6112720124456,32.1528620195551,123.313207406856)) ;
#30053 = CARTESIAN_POINT('Ctrl Pts',(-20.910145815352,32.3429009672863,123.552606824038)) ;
#30054 = CARTESIAN_POINT('Ctrl Pts',(-20.6099679432151,32.1629118869234,123.524461792942)) ;
#30055 = CARTESIAN_POINT('Ctrl Pts',(-20.8638163142715,32.3527514619611,123.807307622436)) ;
#30056 = CARTESIAN_POINT('Ctrl Pts',(-20.5729021084178,32.1727623815982,123.72822191254)) ;
#30057 = CARTESIAN_POINT('Ctrl Pts',(-20.773519983493,32.3627232623556,124.053271401024)) ;
#30058 = CARTESIAN_POINT('Ctrl Pts',(-20.5006629717372,32.1827341819927,123.924992078725)) ;
#30059 = CARTESIAN_POINT('Ctrl Pts',(-20.6415042015941,32.3727192293814,124.280422776241)) ;
#30060 = CARTESIAN_POINT('Ctrl Pts',(-20.3950484362192,32.1927301490186,124.106711993813)) ;
#30061 = CARTESIAN_POINT('Ctrl Pts',(-20.4711197706811,32.3827566887626,124.481749462152)) ;
#30062 = CARTESIAN_POINT('Ctrl Pts',(-20.2587391854302,32.2027676083997,124.267771863989)) ;
#30063 = CARTESIAN_POINT('Ctrl Pts',(-20.2726207381904,32.3925973896634,124.6475312724)) ;
#30064 = CARTESIAN_POINT('Ctrl Pts',(-20.0999386785007,32.2126083093005,124.400395461972)) ;
#30065 = CARTESIAN_POINT('Ctrl Pts',(-20.0438481628859,32.4026454109307,124.779365277945)) ;
#30066 = CARTESIAN_POINT('Ctrl Pts',(-19.9169195251314,32.2226563305678,124.50586072606)) ;
#30067 = CARTESIAN_POINT('Ctrl Pts',(-19.7979892008617,32.4125928040134,124.868183348147)) ;
#30068 = CARTESIAN_POINT('Ctrl Pts',(-19.7202316993048,32.2326037236505,124.576913031386)) ;
#30069 = CARTESIAN_POINT('Ctrl Pts',(-19.5415342218403,32.4225029500598,124.913581797367)) ;
#30070 = CARTESIAN_POINT('Ctrl Pts',(-19.515067529213,32.2425138696969,124.613229582587)) ;
#30071 = CARTESIAN_POINT('Ctrl Pts',(-19.277223918375,32.4325618639094,124.913465271175)) ;
#30072 = CARTESIAN_POINT('Ctrl Pts',(-19.3036192607228,32.2525727835465,124.613134137926)) ;
#30073 = CARTESIAN_POINT('Ctrl Pts',(-19.022469311543,32.4424026341987,124.868802452506)) ;
#30074 = CARTESIAN_POINT('Ctrl Pts',(-19.099816280715,32.2624135538358,124.577401773527)) ;
#30075 = CARTESIAN_POINT('Ctrl Pts',(-18.7738114256327,32.4524655037773,124.778908029314)) ;
#30076 = CARTESIAN_POINT('Ctrl Pts',(-18.9008906793119,32.2724764234145,124.505484170492)) ;
#30077 = CARTESIAN_POINT('Ctrl Pts',(-18.5484324346786,32.4623598269078,124.649195864268)) ;
#30078 = CARTESIAN_POINT('Ctrl Pts',(-18.7205888114285,32.2823707465449,124.401712667753)) ;
#30079 = CARTESIAN_POINT('Ctrl Pts',(-18.3476349380033,32.4723016340023,124.482101731582)) ;
#30080 = CARTESIAN_POINT('Ctrl Pts',(-18.5599523479521,32.2923125536394,124.268035850005)) ;
#30081 = CARTESIAN_POINT('Ctrl Pts',(-18.1777508202333,32.4823041449576,124.281474853431)) ;
#30082 = CARTESIAN_POINT('Ctrl Pts',(-18.4240467225334,32.3023150645948,124.10753302208)) ;
#30083 = CARTESIAN_POINT('Ctrl Pts',(-18.0452392633268,32.492338865776,124.053503454134)) ;
#30084 = CARTESIAN_POINT('Ctrl Pts',(-18.3180393459561,32.3123497854131,123.925154800795)) ;
#30085 = CARTESIAN_POINT('Ctrl Pts',(-17.9556292696089,32.5021840432817,123.810780412352)) ;
#30086 = CARTESIAN_POINT('Ctrl Pts',(-18.24635350555,32.3221949629189,123.73097605505)) ;
#30087 = CARTESIAN_POINT('Ctrl Pts',(-17.9083727783839,32.5121688036828,123.552719582534)) ;
#30088 = CARTESIAN_POINT('Ctrl Pts',(-18.2085503837353,32.3321797233199,123.524527146658)) ;
#30089 = CARTESIAN_POINT('Ctrl Pts',(-17.9065240318847,32.5221077099992,123.291502653985)) ;
#30090 = CARTESIAN_POINT('Ctrl Pts',(-18.2070734512826,32.3421186296363,123.315553837412)) ;
#30091 = CARTESIAN_POINT('Ctrl Pts',(-17.9505907657664,32.5321499376349,123.031335993592)) ;
#30092 = CARTESIAN_POINT('Ctrl Pts',(-18.242328891931,32.3521608572721,123.107420816645)) ;
#30093 = CARTESIAN_POINT('Ctrl Pts',(-18.0376192936705,32.5420351492193,122.786543593569)) ;
#30094 = CARTESIAN_POINT('Ctrl Pts',(-18.3119535058972,32.3620460688564,122.911587983726)) ;
#30095 = CARTESIAN_POINT('Ctrl Pts',(-18.1669767556182,32.5520340794212,122.557873550048)) ;
#30096 = CARTESIAN_POINT('Ctrl Pts',(-18.4154411876375,32.3720449990584,122.728653018332)) ;
#30097 = CARTESIAN_POINT('Ctrl Pts',(-18.3326104946629,32.5619515023317,122.356600741746)) ;
#30098 = CARTESIAN_POINT('Ctrl Pts',(-18.5479494908398,32.3819624219688,122.567636304059)) ;
#30099 = CARTESIAN_POINT('Ctrl Pts',(-18.5332526173871,32.5719994344104,122.185007966984)) ;
#30100 = CARTESIAN_POINT('Ctrl Pts',(-18.7084645480787,32.3920103540475,122.430363551794)) ;
#30101 = CARTESIAN_POINT('Ctrl Pts',(-18.7567232187338,32.5818768102198,122.052875232647)) ;
#30102 = CARTESIAN_POINT('Ctrl Pts',(-18.8872415842206,32.4018877298569,122.324659316094)) ;
#30103 = CARTESIAN_POINT('Ctrl Pts',(-19.0039525695959,32.5919307033877,121.95982536141)) ;
#30104 = CARTESIAN_POINT('Ctrl Pts',(-19.0850258485824,32.4119416230248,122.250221203348)) ;
#30105 = CARTESIAN_POINT('Ctrl Pts',(-19.2595182815849,32.601824326641,121.911755678648)) ;
#30106 = CARTESIAN_POINT('Ctrl Pts',(-19.2894783105699,32.4218352462781,122.211767438031)) ;
#30107 = CARTESIAN_POINT('Ctrl Pts',(-19.5238926627054,32.611886920264,121.908700188409)) ;
#30108 = CARTESIAN_POINT('Ctrl Pts',(-19.5009779851935,32.4318978399011,122.209324968628)) ;
#30109 = CARTESIAN_POINT('Ctrl Pts',(-19.7791709674073,32.6217294942531,121.950535647314)) ;
#30110 = CARTESIAN_POINT('Ctrl Pts',(-19.7051996362344,32.4417404138902,122.242795101324)) ;
#30111 = CARTESIAN_POINT('Ctrl Pts',(-20.0271280441419,32.631720251136,122.036735366636)) ;
#30112 = CARTESIAN_POINT('Ctrl Pts',(-19.9035645706121,32.4517311707731,122.311756541242)) ;
#30113 = CARTESIAN_POINT('Ctrl Pts',(-20.2549311093635,32.6416483128939,122.163938821337)) ;
#30114 = CARTESIAN_POINT('Ctrl Pts',(-20.0858057967329,32.4616592325311,122.413520699274)) ;
#30115 = CARTESIAN_POINT('Ctrl Pts',(-20.4586943445291,32.6516362887831,122.329402962598)) ;
#30116 = CARTESIAN_POINT('Ctrl Pts',(-20.2488151736051,32.4716472084202,122.545893272239)) ;
#30117 = CARTESIAN_POINT('Ctrl Pts',(-20.6311078851739,32.6616719531395,122.528955452347)) ;
#30118 = CARTESIAN_POINT('Ctrl Pts',(-20.3867446776176,32.4816828727767,122.705536503265)) ;
#30119 = CARTESIAN_POINT('Ctrl Pts',(-20.76419350534,32.6715278915592,122.751167847475)) ;
#30120 = CARTESIAN_POINT('Ctrl Pts',(-20.4932112993434,32.4915388111963,122.88330668774)) ;
#30121 = CARTESIAN_POINT('Ctrl Pts',(-20.8583709770248,32.6815233829561,122.99634558384)) ;
#30122 = CARTESIAN_POINT('Ctrl Pts',(-20.5685516696912,32.5015343025932,123.079449363677)) ;
#30123 = CARTESIAN_POINT('Ctrl Pts',(-20.9082019158921,32.6914331879096,123.251966021349)) ;
#30124 = CARTESIAN_POINT('Ctrl Pts',(-20.6084146932958,32.5114441075467,123.283945511149)) ;
#30125 = CARTESIAN_POINT('Ctrl Pts',(-20.913367466307,32.7014454101763,123.515032024856)) ;
#30126 = CARTESIAN_POINT('Ctrl Pts',(-20.6125455536325,32.5214563298134,123.494398306009)) ;
#30127 = CARTESIAN_POINT('Ctrl Pts',(-20.8722060909322,32.7114732908691,123.775321815842)) ;
#30128 = CARTESIAN_POINT('Ctrl Pts',(-20.5796147887184,32.5314842105063,123.702629927723)) ;
#30129 = CARTESIAN_POINT('Ctrl Pts',(-20.7883600167789,32.7213296868517,124.02038977865)) ;
#30130 = CARTESIAN_POINT('Ctrl Pts',(-20.5125366813953,32.5413406064889,123.898683026209)) ;
#30131 = CARTESIAN_POINT('Ctrl Pts',(-20.6615779007813,32.7313544840317,124.25132140461)) ;
#30132 = CARTESIAN_POINT('Ctrl Pts',(-20.4111096709629,32.5513654036688,124.083427628986)) ;
#30133 = CARTESIAN_POINT('Ctrl Pts',(-20.4960157375153,32.7413854140155,124.456454889738)) ;
#30134 = CARTESIAN_POINT('Ctrl Pts',(-20.2786586468199,32.5613963336526,124.247533447329)) ;
#30135 = CARTESIAN_POINT('Ctrl Pts',(-20.3013621684409,32.7512300165242,124.626844922445)) ;
#30136 = CARTESIAN_POINT('Ctrl Pts',(-20.1229354628895,32.5712409361613,124.38384373688)) ;
#30137 = CARTESIAN_POINT('Ctrl Pts',(-20.0771483650704,32.7612208677483,124.763458712167)) ;
#30138 = CARTESIAN_POINT('Ctrl Pts',(-19.9435638346434,32.5812317873854,124.493133506793)) ;
#30139 = CARTESIAN_POINT('Ctrl Pts',(-19.8312628601083,32.7712587007595,124.858962378708)) ;
#30140 = CARTESIAN_POINT('Ctrl Pts',(-19.7468547876405,32.5912696203966,124.569535079804)) ;
#30141 = CARTESIAN_POINT('Ctrl Pts',(-19.5775920832475,32.7811030892249,124.909777937782)) ;
#30142 = CARTESIAN_POINT('Ctrl Pts',(-19.5439188102841,32.6011140088621,124.610185961714)) ;
#30143 = CARTESIAN_POINT('Ctrl Pts',(-19.3153197757331,32.7910878935945,124.916379101424)) ;
#30144 = CARTESIAN_POINT('Ctrl Pts',(-19.3341011312526,32.6110988132316,124.615465586228)) ;
#30145 = CARTESIAN_POINT('Ctrl Pts',(-19.0569748481772,32.8010274130773,124.877619388893)) ;
#30146 = CARTESIAN_POINT('Ctrl Pts',(-19.1274258094831,32.6210383327145,124.584456619583)) ;
#30147 = CARTESIAN_POINT('Ctrl Pts',(-18.8068609697535,32.8110671440787,124.793713447214)) ;
#30148 = CARTESIAN_POINT('Ctrl Pts',(-18.9273350056697,32.6310780637158,124.517330604952)) ;
#30149 = CARTESIAN_POINT('Ctrl Pts',(-18.5785199696836,32.820955272325,124.669655218426)) ;
#30150 = CARTESIAN_POINT('Ctrl Pts',(-18.7446634574821,32.6409661919621,124.418083265181)) ;
#30151 = CARTESIAN_POINT('Ctrl Pts',(-18.3728153330768,32.8309449975335,124.506569798915)) ;
#30152 = CARTESIAN_POINT('Ctrl Pts',(-18.5801006004135,32.6509559171706,124.287614130099)) ;
#30153 = CARTESIAN_POINT('Ctrl Pts',(-18.1992468678326,32.840902762235,124.310742518053)) ;
#30154 = CARTESIAN_POINT('Ctrl Pts',(-18.4412469568537,32.6609136818721,124.130951769751)) ;
#30155 = CARTESIAN_POINT('Ctrl Pts',(-18.0625524288157,32.850805103647,124.089302873787)) ;
#30156 = CARTESIAN_POINT('Ctrl Pts',(-18.3318926747522,32.6708160232841,123.95380009295)) ;
#30157 = CARTESIAN_POINT('Ctrl Pts',(-17.9650377613778,32.8608492993534,123.844039624706)) ;
#30158 = CARTESIAN_POINT('Ctrl Pts',(-18.2538818733743,32.6808602189905,123.757588954974)) ;
#30159 = CARTESIAN_POINT('Ctrl Pts',(-17.9122844842802,32.8707567001127,123.58906943826)) ;
#30160 = CARTESIAN_POINT('Ctrl Pts',(-18.2116804247751,32.6907676197498,123.553613231978)) ;
#30161 = CARTESIAN_POINT('Ctrl Pts',(-17.9040614841339,32.880767299987,123.326126151249)) ;
#30162 = CARTESIAN_POINT('Ctrl Pts',(-18.2051029793148,32.7007782196241,123.34325861009)) ;
#30163 = CARTESIAN_POINT('Ctrl Pts',(-17.9421976273555,32.8907975958992,123.065306227518)) ;
#30164 = CARTESIAN_POINT('Ctrl Pts',(-18.2356129698765,32.7108085155363,123.134602745316)) ;
#30165 = CARTESIAN_POINT('Ctrl Pts',(-18.0232436735507,32.9006523755489,122.819357208247)) ;
#30166 = CARTESIAN_POINT('Ctrl Pts',(-18.3004504322419,32.720663295186,122.937844802407)) ;
#30167 = CARTESIAN_POINT('Ctrl Pts',(-18.1463463293519,32.9106097037664,122.588444800357)) ;
#30168 = CARTESIAN_POINT('Ctrl Pts',(-18.3989330865564,32.7306206234035,122.753115585193)) ;
#30169 = CARTESIAN_POINT('Ctrl Pts',(-18.3093474042476,32.9206487366733,122.381033273986)) ;
#30170 = CARTESIAN_POINT('Ctrl Pts',(-18.5293347464535,32.7406596563104,122.587186824327)) ;
#30171 = CARTESIAN_POINT('Ctrl Pts',(-18.5023603004912,32.9305218485626,122.207583253798)) ;
#30172 = CARTESIAN_POINT('Ctrl Pts',(-18.6837449255098,32.7505327681997,122.448428002608)) ;
#30173 = CARTESIAN_POINT('Ctrl Pts',(-18.7269817759468,32.9405951335897,122.067617063673)) ;
#30174 = CARTESIAN_POINT('Ctrl Pts',(-18.8634428286131,32.7606060532268,122.336455563458)) ;
#30175 = CARTESIAN_POINT('Ctrl Pts',(-18.9663055363985,32.9504154533265,121.970905134139)) ;
#30176 = CARTESIAN_POINT('Ctrl Pts',(-19.0549009577353,32.7704263729636,122.259087166004)) ;
#30177 = CARTESIAN_POINT('Ctrl Pts',(-19.2252558871534,32.9604941187049,121.915591458617)) ;
#30178 = CARTESIAN_POINT('Ctrl Pts',(-19.262061748827,32.780505038342,122.214836808385)) ;
#30179 = CARTESIAN_POINT('Ctrl Pts',(-19.4840372151867,32.9703457091887,121.906199287805)) ;
#30180 = CARTESIAN_POINT('Ctrl Pts',(-19.4690857796967,32.7903566288258,122.207323762619)) ;
#30181 = CARTESIAN_POINT('Ctrl Pts',(-19.7462073716882,32.9804188595076,121.942441422299)) ;
#30182 = CARTESIAN_POINT('Ctrl Pts',(-19.6788221704482,32.8004297791447,122.236318111422)) ;
#30183 = CARTESIAN_POINT('Ctrl Pts',(-19.9923907933803,32.9902612394826,122.021850824201)) ;
#30184 = CARTESIAN_POINT('Ctrl Pts',(-19.8757676411912,32.8102721591198,122.299845862724)) ;
#30185 = CARTESIAN_POINT('Ctrl Pts',(-20.2246277641436,33.0002422157257,122.143718242006)) ;
#30186 = CARTESIAN_POINT('Ctrl Pts',(-20.0615568191512,32.8202531353628,122.397340033153)) ;
#30187 = CARTESIAN_POINT('Ctrl Pts',(-20.4326666594073,33.010258544081,122.304997705767)) ;
#30188 = CARTESIAN_POINT('Ctrl Pts',(-20.2279876169795,32.8302694637181,122.52636399411)) ;
#30189 = CARTESIAN_POINT('Ctrl Pts',(-20.6076780088902,33.0201563410721,122.497403957948)) ;
#30190 = CARTESIAN_POINT('Ctrl Pts',(-20.3679958534134,32.8401672607093,122.680288693608)) ;
#30191 = CARTESIAN_POINT('Ctrl Pts',(-20.7486295700232,33.0301688978042,122.719608055138)) ;
#30192 = CARTESIAN_POINT('Ctrl Pts',(-20.4807568301996,32.8501798174413,122.858052122149)) ;
#30193 = CARTESIAN_POINT('Ctrl Pts',(-20.8484637130917,33.0402009326507,122.96359161389)) ;
#30194 = CARTESIAN_POINT('Ctrl Pts',(-20.5606237531606,32.8602118522878,123.053239243088)) ;
#30195 = CARTESIAN_POINT('Ctrl Pts',(-20.9039796443904,33.0500403334661,123.216152649294)) ;
#30196 = CARTESIAN_POINT('Ctrl Pts',(-20.6050359484339,32.8700512531033,123.255286987946)) ;
#30197 = CARTESIAN_POINT('Ctrl Pts',(-20.9152463774755,33.0601061191177,123.480399984258)) ;
#30198 = CARTESIAN_POINT('Ctrl Pts',(-20.6140490933859,32.8801170387548,123.466685170754)) ;
#30199 = CARTESIAN_POINT('Ctrl Pts',(-20.8809372575507,33.0699965742323,123.738064421165)) ;
#30200 = CARTESIAN_POINT('Ctrl Pts',(-20.5866016261539,32.8900074938694,123.672815854496)) ;
#30201 = CARTESIAN_POINT('Ctrl Pts',(-20.8021533889854,33.0799886928681,123.98853537261)) ;
#30202 = CARTESIAN_POINT('Ctrl Pts',(-20.523574446852,32.8999996125052,123.873192408795)) ;
#30203 = CARTESIAN_POINT('Ctrl Pts',(-20.6812106073249,33.0899515196311,124.220732031348)) ;
#30204 = CARTESIAN_POINT('Ctrl Pts',(-20.4268202076342,32.9099624392683,124.058949317243)) ;
#30205 = CARTESIAN_POINT('Ctrl Pts',(-20.5232306933288,33.099855802904,124.427605321835)) ;
#30206 = CARTESIAN_POINT('Ctrl Pts',(-20.3004367035077,32.9198667225411,124.22444733005)) ;
#30207 = CARTESIAN_POINT('Ctrl Pts',(-20.3285971107455,33.1099162368511,124.606480559927)) ;
#30208 = CARTESIAN_POINT('Ctrl Pts',(-20.1447295646736,32.9299271564882,124.36754764172)) ;
#30209 = CARTESIAN_POINT('Ctrl Pts',(-20.1108525131507,33.1197567895243,124.746047511506)) ;
#30210 = CARTESIAN_POINT('Ctrl Pts',(-19.970534871693,32.9397677091614,124.479200559667)) ;
#30211 = CARTESIAN_POINT('Ctrl Pts',(-19.8669950901314,33.12981900947,124.84821784105)) ;
#30212 = CARTESIAN_POINT('Ctrl Pts',(-19.7754486895611,32.9498299291071,124.560937006756)) ;
#30213 = CARTESIAN_POINT('Ctrl Pts',(-19.6132318493154,33.1397161487486,124.905283007203)) ;
#30214 = CARTESIAN_POINT('Ctrl Pts',(-19.5724388798712,32.9597270683857,124.606588967545)) ;
#30215 = CARTESIAN_POINT('Ctrl Pts',(-19.3525812289575,33.1496473408836,124.918328736674)) ;
#30216 = CARTESIAN_POINT('Ctrl Pts',(-19.3639189712111,32.9696582605208,124.617025749215)) ;
#30217 = CARTESIAN_POINT('Ctrl Pts',(-19.090770522027,33.1596894955287,124.885264797401)) ;
#30218 = CARTESIAN_POINT('Ctrl Pts',(-19.1544702195643,32.9797004151658,124.590574725584)) ;
#30219 = CARTESIAN_POINT('Ctrl Pts',(-18.842487870914,33.169576256548,124.808646986439)) ;
#30220 = CARTESIAN_POINT('Ctrl Pts',(-18.9558448766533,32.9895871761851,124.529280933374)) ;
#30221 = CARTESIAN_POINT('Ctrl Pts',(-18.6085457635101,33.1795755582652,124.689058201042)) ;
#30222 = CARTESIAN_POINT('Ctrl Pts',(-18.7686911704573,32.9995864779024,124.433610222531)) ;
#30223 = CARTESIAN_POINT('Ctrl Pts',(-18.4004044124469,33.189496356432,124.532007686267)) ;
#30224 = CARTESIAN_POINT('Ctrl Pts',(-18.6021783869313,33.0095072760691,124.307970451747)) ;
#30225 = CARTESIAN_POINT('Ctrl Pts',(-18.2206897370185,33.1995304100287,124.339091714962)) ;
#30226 = CARTESIAN_POINT('Ctrl Pts',(-18.4584063193687,33.0195413296658,124.153637825087)) ;
#30227 = CARTESIAN_POINT('Ctrl Pts',(-18.0786177880743,33.2094535275951,124.120374761366)) ;
#30228 = CARTESIAN_POINT('Ctrl Pts',(-18.344748777028,33.0294644472322,123.978664981646)) ;
#30229 = CARTESIAN_POINT('Ctrl Pts',(-17.9753934550452,33.2195096510942,123.87713368977)) ;
#30230 = CARTESIAN_POINT('Ctrl Pts',(-18.2621688831962,33.0395205707314,123.784072046529)) ;
#30231 = CARTESIAN_POINT('Ctrl Pts',(-17.9170984303965,33.2293550927491,123.625046988953)) ;
#30232 = CARTESIAN_POINT('Ctrl Pts',(-18.2155327344032,33.0493660123862,123.582403874291)) ;
#30233 = CARTESIAN_POINT('Ctrl Pts',(-17.9024396209619,33.2393173938732,123.363675275733)) ;
#30234 = CARTESIAN_POINT('Ctrl Pts',(-18.2038050999464,33.0593283135103,123.373306898927)) ;
#30235 = CARTESIAN_POINT('Ctrl Pts',(-17.9339408232565,33.2493458731483,123.102009100134)) ;
#30236 = CARTESIAN_POINT('Ctrl Pts',(-18.2290055541262,33.0693567927855,123.163973819942)) ;
#30237 = CARTESIAN_POINT('Ctrl Pts',(-18.009402919707,33.259256226658,122.852760854094)) ;
#30238 = CARTESIAN_POINT('Ctrl Pts',(-18.2893745088673,33.0792671462951,122.964575736527)) ;
#30239 = CARTESIAN_POINT('Ctrl Pts',(-18.1266871223674,33.2691910988352,122.61950036567)) ;
#30240 = CARTESIAN_POINT('Ctrl Pts',(-18.3832009980876,33.0892020184723,122.777967498192)) ;
#30241 = CARTESIAN_POINT('Ctrl Pts',(-18.2845465433898,33.2792322364209,122.40806845954)) ;
#30242 = CARTESIAN_POINT('Ctrl Pts',(-18.5094881032574,33.099243156058,122.608821464249)) ;
#30243 = CARTESIAN_POINT('Ctrl Pts',(-18.4736647676083,33.2891193856355,122.229881635933)) ;
#30244 = CARTESIAN_POINT('Ctrl Pts',(-18.6607816011752,33.1091303052726,122.466272069737)) ;
#30245 = CARTESIAN_POINT('Ctrl Pts',(-18.6928889148738,33.2991116203865,122.085373784708)) ;
#30246 = CARTESIAN_POINT('Ctrl Pts',(-18.8361603422665,33.1191225400237,122.350665209582)) ;
#30247 = CARTESIAN_POINT('Ctrl Pts',(-18.9328841091275,33.3090603259495,121.981637584403)) ;
#30248 = CARTESIAN_POINT('Ctrl Pts',(-19.0281557898517,33.1290712455866,122.267675703838)) ;
#30249 = CARTESIAN_POINT('Ctrl Pts',(-19.1868031331839,33.3189963943732,121.920862306553)) ;
#30250 = CARTESIAN_POINT('Ctrl Pts',(-19.2312903095408,33.1390073140103,122.219054752622)) ;
#30251 = CARTESIAN_POINT('Ctrl Pts',(-19.4487454010854,33.328982078589,121.90471788781)) ;
#30252 = CARTESIAN_POINT('Ctrl Pts',(-19.4408438645719,33.1489929982261,122.20613828772)) ;
#30253 = CARTESIAN_POINT('Ctrl Pts',(-19.7108540776556,33.3390225051576,121.934873930191)) ;
#30254 = CARTESIAN_POINT('Ctrl Pts',(-19.6505310372627,33.1590334247948,122.230262297346)) ;
#30255 = CARTESIAN_POINT('Ctrl Pts',(-19.9588162424853,33.3488616186214,122.008165761205)) ;
#30256 = CARTESIAN_POINT('Ctrl Pts',(-19.8488999925423,33.1688725382585,122.288894547529)) ;
#30257 = CARTESIAN_POINT('Ctrl Pts',(-20.1950323307625,33.3588913527972,122.125097981869)) ;
#30258 = CARTESIAN_POINT('Ctrl Pts',(-20.0378734209598,33.1789022724343,122.38243939003)) ;
#30259 = CARTESIAN_POINT('Ctrl Pts',(-20.406784218548,33.3689134523031,122.281698617158)) ;
#30260 = CARTESIAN_POINT('Ctrl Pts',(-20.2072754977896,33.1889243719402,122.507719170111)) ;
#30261 = CARTESIAN_POINT('Ctrl Pts',(-20.5858350552601,33.3787818921965,122.469326974363)) ;
#30262 = CARTESIAN_POINT('Ctrl Pts',(-20.350516319059,33.1987928118337,122.657820459907)) ;
#30263 = CARTESIAN_POINT('Ctrl Pts',(-20.732476955186,33.3888507568821,122.68954538537)) ;
#30264 = CARTESIAN_POINT('Ctrl Pts',(-20.4678308998726,33.2088616765193,122.833994843785)) ;
#30265 = CARTESIAN_POINT('Ctrl Pts',(-20.8362904559934,33.3986934299808,122.926463443138)) ;
#30266 = CARTESIAN_POINT('Ctrl Pts',(-20.5508822680002,33.2187043496179,123.023527908559)) ;
#30267 = CARTESIAN_POINT('Ctrl Pts',(-20.8990494415645,33.4086540641432,123.180578146984)) ;
#30268 = CARTESIAN_POINT('Ctrl Pts',(-20.6010906294462,33.2286649837803,123.226819047015)) ;
#30269 = CARTESIAN_POINT('Ctrl Pts',(-20.916351249052,33.4186919798213,123.443786581483)) ;
#30270 = CARTESIAN_POINT('Ctrl Pts',(-20.6149332528463,33.2387028994585,123.43738582393)) ;
#30271 = CARTESIAN_POINT('Ctrl Pts',(-20.8886281343362,33.4285662546808,123.701819630219)) ;
#30272 = CARTESIAN_POINT('Ctrl Pts',(-20.592756117805,33.2485771743179,123.643811594593)) ;
#30273 = CARTESIAN_POINT('Ctrl Pts',(-20.8151004364326,33.4386360050559,123.95598455471)) ;
#30274 = CARTESIAN_POINT('Ctrl Pts',(-20.5339351068565,33.258646924693,123.84714415652)) ;
#30275 = CARTESIAN_POINT('Ctrl Pts',(-20.7013946872375,33.4484693004304,124.188056231771)) ;
#30276 = CARTESIAN_POINT('Ctrl Pts',(-20.442972128081,33.2684802200675,124.03280115278)) ;
#30277 = CARTESIAN_POINT('Ctrl Pts',(-20.5466931297227,33.45849959791,124.401459336272)) ;
#30278 = CARTESIAN_POINT('Ctrl Pts',(-20.3192120229929,33.2785105175472,124.20352454908)) ;
#30279 = CARTESIAN_POINT('Ctrl Pts',(-20.3567007162318,33.4685316843515,124.58424663072)) ;
#30280 = CARTESIAN_POINT('Ctrl Pts',(-20.1672189437675,33.2885426039886,124.34975536662)) ;
#30281 = CARTESIAN_POINT('Ctrl Pts',(-20.1426457143214,33.4783596128404,124.728735741513)) ;
#30282 = CARTESIAN_POINT('Ctrl Pts',(-19.9959765796565,33.2983705324775,124.465347258471)) ;
#30283 = CARTESIAN_POINT('Ctrl Pts',(-19.9029989792466,33.4883556539512,124.836308043002)) ;
#30284 = CARTESIAN_POINT('Ctrl Pts',(-19.8042599394586,33.3083665735883,124.551406472735)) ;
#30285 = CARTESIAN_POINT('Ctrl Pts',(-19.6474220237301,33.4983814660524,124.900335793291)) ;
#30286 = CARTESIAN_POINT('Ctrl Pts',(-19.5997986983396,33.3183923856895,124.602630093288)) ;
#30287 = CARTESIAN_POINT('Ctrl Pts',(-19.3882695560054,33.5082687009472,124.919091810044)) ;
#30288 = CARTESIAN_POINT('Ctrl Pts',(-19.3924774972755,33.3282796205843,124.617636375343)) ;
#30289 = CARTESIAN_POINT('Ctrl Pts',(-19.1274334857693,33.5182455671582,124.892759807624)) ;
#30290 = CARTESIAN_POINT('Ctrl Pts',(-19.1838086836,33.3382564867954,124.596572391666)) ;
#30291 = CARTESIAN_POINT('Ctrl Pts',(-18.8746590268341,33.52823851103,124.821451907867)) ;
#30292 = CARTESIAN_POINT('Ctrl Pts',(-18.9815887977188,33.3482494306672,124.539527654376)) ;
#30293 = CARTESIAN_POINT('Ctrl Pts',(-18.6372374521722,33.5382764337014,124.706546424498)) ;
#30294 = CARTESIAN_POINT('Ctrl Pts',(-18.7916507985739,33.3582873533385,124.447604630339)) ;
#30295 = CARTESIAN_POINT('Ctrl Pts',(-18.4271493677989,33.5481248979631,124.555368999614)) ;
#30296 = CARTESIAN_POINT('Ctrl Pts',(-18.6235800486874,33.3681358176002,124.326664485506)) ;
#30297 = CARTESIAN_POINT('Ctrl Pts',(-18.2435773439465,33.5581167647071,124.367679767415)) ;
#30298 = CARTESIAN_POINT('Ctrl Pts',(-18.4767213025052,33.3781276843442,124.176514389402)) ;
#30299 = CARTESIAN_POINT('Ctrl Pts',(-18.096319636919,33.5680344967483,124.152599028164)) ;
#30300 = CARTESIAN_POINT('Ctrl Pts',(-18.3589139685211,33.3880454163854,124.004451152358)) ;
#30301 = CARTESIAN_POINT('Ctrl Pts',(-17.9874040348388,33.5780626816436,123.912652984584)) ;
#30302 = CARTESIAN_POINT('Ctrl Pts',(-18.271779888472,33.3980736012807,123.812495012593)) ;
#30303 = CARTESIAN_POINT('Ctrl Pts',(-17.9226291155959,33.5879478396924,123.661079753393)) ;
#30304 = CARTESIAN_POINT('Ctrl Pts',(-18.2199583955529,33.4079587593295,123.611237435979)) ;
#30305 = CARTESIAN_POINT('Ctrl Pts',(-17.9016709287819,33.5979372002341,123.399402541443)) ;
#30306 = CARTESIAN_POINT('Ctrl Pts',(-18.2031899993243,33.4179481198712,123.401895940217)) ;
#30307 = CARTESIAN_POINT('Ctrl Pts',(-17.9271501704679,33.6079783571685,123.1367648659)) ;
#30308 = CARTESIAN_POINT('Ctrl Pts',(-18.2235716341578,33.4279892768056,123.191785556007)) ;
#30309 = CARTESIAN_POINT('Ctrl Pts',(-17.9959631146861,33.6178109406236,122.887710030823)) ;
#30310 = CARTESIAN_POINT('Ctrl Pts',(-18.2786200105537,33.4378218602607,122.992541933455)) ;
#30311 = CARTESIAN_POINT('Ctrl Pts',(-18.1081263093149,33.6278051605856,122.650231330554)) ;
#30312 = CARTESIAN_POINT('Ctrl Pts',(-18.3683487586546,33.4478160802227,122.802558226559)) ;
#30313 = CARTESIAN_POINT('Ctrl Pts',(-18.2607792875272,33.6378332623729,122.435411305488)) ;
#30314 = CARTESIAN_POINT('Ctrl Pts',(-18.4904696240239,33.45784418201,122.630701109372)) ;
#30315 = CARTESIAN_POINT('Ctrl Pts',(-18.4453797141511,33.647713206996,122.252832221367)) ;
#30316 = CARTESIAN_POINT('Ctrl Pts',(-18.6381482311407,33.4677241266331,122.484636845497)) ;
#30317 = CARTESIAN_POINT('Ctrl Pts',(-18.6610157891126,33.657703533553,122.10310705135)) ;
#30318 = CARTESIAN_POINT('Ctrl Pts',(-18.8106558663145,33.4777144531901,122.364855145268)) ;
#30319 = CARTESIAN_POINT('Ctrl Pts',(-18.8982140305105,33.6676444652073,121.993631136502)) ;
#30320 = CARTESIAN_POINT('Ctrl Pts',(-19.0004133768427,33.4876553848444,122.277272732784)) ;
#30321 = CARTESIAN_POINT('Ctrl Pts',(-19.1519080089799,33.6776315837102,121.92632833614)) ;
#30322 = CARTESIAN_POINT('Ctrl Pts',(-19.2033679299254,33.4976425033473,122.223428561246)) ;
#30323 = CARTESIAN_POINT('Ctrl Pts',(-19.4146423301779,33.6876649166074,121.904411969349)) ;
#30324 = CARTESIAN_POINT('Ctrl Pts',(-19.4135552411739,33.5076758362445,122.20589349727)) ;
#30325 = CARTESIAN_POINT('Ctrl Pts',(-19.6729091690056,33.6975310210521,121.927545767156)) ;
#30326 = CARTESIAN_POINT('Ctrl Pts',(-19.6201683942856,33.5175419406893,122.224398461816)) ;
#30327 = CARTESIAN_POINT('Ctrl Pts',(-19.9282681240009,33.7075971349325,121.996466980296)) ;
#30328 = CARTESIAN_POINT('Ctrl Pts',(-19.8244562056054,33.5276080545696,122.279533486686)) ;
#30329 = CARTESIAN_POINT('Ctrl Pts',(-20.1628320829574,33.7174531467009,122.10634520991)) ;
#30330 = CARTESIAN_POINT('Ctrl Pts',(-20.0121077897334,33.537464066338,122.367434006079)) ;
#30331 = CARTESIAN_POINT('Ctrl Pts',(-20.3781604555604,33.7274478503322,122.256728476995)) ;
#30332 = CARTESIAN_POINT('Ctrl Pts',(-20.184371642184,33.5474587699693,122.487738827655)) ;
#30333 = CARTESIAN_POINT('Ctrl Pts',(-20.5643974693118,33.7374791860571,122.443302838799)) ;
#30334 = CARTESIAN_POINT('Ctrl Pts',(-20.3333627176559,33.5574901056942,122.636996853287)) ;
#30335 = CARTESIAN_POINT('Ctrl Pts',(-20.713269761922,33.7473457112607,122.655597325724)) ;
#30336 = CARTESIAN_POINT('Ctrl Pts',(-20.4524620449125,33.5673566308979,122.806830892729)) ;
#30337 = CARTESIAN_POINT('Ctrl Pts',(-20.8247303532555,33.7573331393065,122.893178808627)) ;
#30338 = CARTESIAN_POINT('Ctrl Pts',(-20.5416324255552,33.5773440589437,122.99689507574)) ;
#30339 = CARTESIAN_POINT('Ctrl Pts',(-20.8931087336896,33.767278068993,123.145457142139)) ;
#30340 = CARTESIAN_POINT('Ctrl Pts',(-20.5963371660383,33.5872889886301,123.198716996963)) ;
#30341 = CARTESIAN_POINT('Ctrl Pts',(-20.9167263518425,33.7773229871015,123.408343079754)) ;
#30342 = CARTESIAN_POINT('Ctrl Pts',(-20.6152334042726,33.5973339067386,123.409025569641)) ;
#30343 = CARTESIAN_POINT('Ctrl Pts',(-20.8949748056446,33.7871849567154,123.666612207482)) ;
#30344 = CARTESIAN_POINT('Ctrl Pts',(-20.5978343558141,33.6071958763525,123.61564071411)) ;
#30345 = CARTESIAN_POINT('Ctrl Pts',(-20.8283422293108,33.7971770247366,123.920571241178)) ;
#30346 = CARTESIAN_POINT('Ctrl Pts',(-20.5445304472365,33.6171879443737,123.818808427627)) ;
#30347 = CARTESIAN_POINT('Ctrl Pts',(-20.7192376865205,33.8071079501112,124.157662672187)) ;
#30348 = CARTESIAN_POINT('Ctrl Pts',(-20.4572488862588,33.6271188697483,124.008482329076)) ;
#30349 = CARTESIAN_POINT('Ctrl Pts',(-20.5707091129721,33.8170585783346,124.372854625881)) ;
#30350 = CARTESIAN_POINT('Ctrl Pts',(-20.3384279325118,33.6370694979717,124.180637052448)) ;
#30351 = CARTESIAN_POINT('Ctrl Pts',(-20.3862313186414,33.8270588173937,124.560056609312)) ;
#30352 = CARTESIAN_POINT('Ctrl Pts',(-20.1908473210986,33.6470697370308,124.330400159823)) ;
#30353 = CARTESIAN_POINT('Ctrl Pts',(-20.1712584195521,33.8370872727629,124.71248063517)) ;
#30354 = CARTESIAN_POINT('Ctrl Pts',(-20.0188703330059,33.6570981924,124.45234117015)) ;
#30355 = CARTESIAN_POINT('Ctrl Pts',(-19.9370901885251,33.8469533073462,124.823799494521)) ;
#30356 = CARTESIAN_POINT('Ctrl Pts',(-19.8315368156364,33.6669642269833,124.541398163761)) ;
#30357 = CARTESIAN_POINT('Ctrl Pts',(-19.6841021964421,33.8569456290936,124.894057284954)) ;
#30358 = CARTESIAN_POINT('Ctrl Pts',(-19.6291473694453,33.6769565487307,124.597606616661)) ;
#30359 = CARTESIAN_POINT('Ctrl Pts',(-19.424287490384,33.8668779187706,124.9192160717)) ;
#30360 = CARTESIAN_POINT('Ctrl Pts',(-19.4212948596349,33.6868888384077,124.617735604572)) ;
#30361 = CARTESIAN_POINT('Ctrl Pts',(-19.1622401128872,33.8768795637414,124.898995670993)) ;
#30362 = CARTESIAN_POINT('Ctrl Pts',(-19.2116608120875,33.6968904833785,124.60156252601)) ;
#30363 = CARTESIAN_POINT('Ctrl Pts',(-18.823429392135,33.8901921971574,124.811777112252)) ;
#30364 = CARTESIAN_POINT('Ctrl Pts',(-18.9405918138416,33.7102031167945,124.531785666973)) ;
#30365 = CARTESIAN_POINT('Ctrl Pts',(-18.5168908225473,33.903423946539,124.639429121269)) ;
#30366 = CARTESIAN_POINT('Ctrl Pts',(-18.6953483850143,33.7234348661761,124.393891756695)) ;
#30367 = CARTESIAN_POINT('Ctrl Pts',(-18.266416953034,33.916747211356,124.394788919274)) ;
#30368 = CARTESIAN_POINT('Ctrl Pts',(-18.4950002778242,33.7367581309931,124.198208384198)) ;
#30369 = CARTESIAN_POINT('Ctrl Pts',(-18.1147393757088,33.9266229175737,124.184190734435)) ;
#30370 = CARTESIAN_POINT('Ctrl Pts',(-18.3736497561591,33.7466338372108,124.029725816734)) ;
#30371 = CARTESIAN_POINT('Ctrl Pts',(-18.0003398463956,33.9366125086737,123.947943873737)) ;
#30372 = CARTESIAN_POINT('Ctrl Pts',(-18.2821299057794,33.7566234283109,123.840730774139)) ;
#30373 = CARTESIAN_POINT('Ctrl Pts',(-17.9289645288639,33.9465396051291,123.69699206503)) ;
#30374 = CARTESIAN_POINT('Ctrl Pts',(-18.2250270203462,33.7665505247663,123.639969543988)) ;
#30375 = CARTESIAN_POINT('Ctrl Pts',(-17.9019571311773,33.9565647536337,123.434953214904)) ;
#30376 = CARTESIAN_POINT('Ctrl Pts',(-18.2034190100901,33.7765756732709,123.430338874046)) ;
#30377 = CARTESIAN_POINT('Ctrl Pts',(-17.920456867938,33.9664604077804,123.175542057052)) ;
#30378 = CARTESIAN_POINT('Ctrl Pts',(-18.2182165454262,33.7864713274175,123.222809688118)) ;
#30379 = CARTESIAN_POINT('Ctrl Pts',(-17.9840343132116,33.9764639421586,122.920489516577)) ;
#30380 = CARTESIAN_POINT('Ctrl Pts',(-18.2690763509193,33.7964748617957,123.018767172028)) ;
#30381 = CARTESIAN_POINT('Ctrl Pts',(-18.0907856147797,33.9864490805987,122.680743142477)) ;
#30382 = CARTESIAN_POINT('Ctrl Pts',(-18.3544753559251,33.8064600002358,122.826969197833)) ;
#30383 = CARTESIAN_POINT('Ctrl Pts',(-18.2384789185145,33.996485005194,122.462260358717)) ;
#30384 = CARTESIAN_POINT('Ctrl Pts',(-18.4726280899805,33.8164959248312,122.652181813698)) ;
#30385 = CARTESIAN_POINT('Ctrl Pts',(-18.4182776203018,34.0063362806217,122.276005602402)) ;
#30386 = CARTESIAN_POINT('Ctrl Pts',(-18.6164655966101,33.8263472002588,122.503176330571)) ;
#30387 = CARTESIAN_POINT('Ctrl Pts',(-18.6302489538193,34.0163285417831,122.121008187001)) ;
#30388 = CARTESIAN_POINT('Ctrl Pts',(-18.7860413729788,33.8363394614202,122.379176658812)) ;
#30389 = CARTESIAN_POINT('Ctrl Pts',(-18.8673098715377,34.0263684258007,122.00522798075)) ;
#30390 = CARTESIAN_POINT('Ctrl Pts',(-18.9756890388998,33.8463793454378,122.2865505691)) ;
#30391 = CARTESIAN_POINT('Ctrl Pts',(-19.1155543481873,34.0362032003031,121.933213929773)) ;
#30392 = CARTESIAN_POINT('Ctrl Pts',(-19.1742842270233,33.8562141199402,122.228937167852)) ;
#30393 = CARTESIAN_POINT('Ctrl Pts',(-19.3787606441446,34.0462795813234,121.904625237353)) ;
#30394 = CARTESIAN_POINT('Ctrl Pts',(-19.3848492266586,33.8662905009605,122.20606409206)) ;
#30395 = CARTESIAN_POINT('Ctrl Pts',(-19.636979964933,34.056125854474,121.921704730838)) ;
#30396 = CARTESIAN_POINT('Ctrl Pts',(-19.591423616235,33.8761367741112,122.219725605663)) ;
#30397 = CARTESIAN_POINT('Ctrl Pts',(-19.9782262367002,34.0694903757593,122.004738916925)) ;
#30398 = CARTESIAN_POINT('Ctrl Pts',(-19.8644290060011,33.8895012953964,122.286150073343)) ;
#30399 = CARTESIAN_POINT('Ctrl Pts',(-20.2860725515586,34.0826966201937,122.173341752895)) ;
#30400 = CARTESIAN_POINT('Ctrl Pts',(-20.1107333615667,33.9027075398308,122.421054696917)) ;
#30401 = CARTESIAN_POINT('Ctrl Pts',(-20.5388137926812,34.0959615748709,122.413398914322)) ;
#30402 = CARTESIAN_POINT('Ctrl Pts',(-20.3128900569695,33.9159724945081,122.613069455434)) ;
#30403 = CARTESIAN_POINT('Ctrl Pts',(-20.6954462284396,34.1059938554226,122.625471146507)) ;
#30404 = CARTESIAN_POINT('Ctrl Pts',(-20.4382052101993,33.9260047750597,122.782731831385)) ;
#30405 = CARTESIAN_POINT('Ctrl Pts',(-20.8114438350329,34.1159025889405,122.858591933872)) ;
#30406 = CARTESIAN_POINT('Ctrl Pts',(-20.5310032327312,33.9359135085776,122.969226073235)) ;
#30407 = CARTESIAN_POINT('Ctrl Pts',(-20.8860726329882,34.125840139808,123.108858926557)) ;
#30408 = CARTESIAN_POINT('Ctrl Pts',(-20.5907085395253,33.9458510594451,123.169440598116)) ;
#30409 = CARTESIAN_POINT('Ctrl Pts',(-20.9161696354576,34.1358699874019,123.370684085346)) ;
#30410 = CARTESIAN_POINT('Ctrl Pts',(-20.6147885800743,33.9558809070391,123.37889723275)) ;
#30411 = CARTESIAN_POINT('Ctrl Pts',(-20.8957675550664,34.1491051273224,123.717974610671)) ;
#30412 = CARTESIAN_POINT('Ctrl Pts',(-20.5984660541345,33.9691160469595,123.656745092967)) ;
#30413 = CARTESIAN_POINT('Ctrl Pts',(-20.7562726268257,34.1657735916935,124.138314956001)) ;
#30414 = CARTESIAN_POINT('Ctrl Pts',(-20.4868736501461,33.9857845113307,123.993003032338)) ;
#30415 = CARTESIAN_POINT('Ctrl Pts',(-20.4290861791078,34.1856446035674,124.553127465598)) ;
#30416 = CARTESIAN_POINT('Ctrl Pts',(-20.2251415375173,34.0056555232046,124.32485414861)) ;
#30417 = CARTESIAN_POINT('Ctrl Pts',(-20.0516612997823,34.2023516879504,124.786832185012)) ;
#30418 = CARTESIAN_POINT('Ctrl Pts',(-19.9231542599151,34.0223626075875,124.511841034845)) ;
#30419 = CARTESIAN_POINT('Ctrl Pts',(-19.7200431655426,34.215528969261,124.88675620924)) ;
#30420 = CARTESIAN_POINT('Ctrl Pts',(-19.6579040689418,34.0355398888981,124.591763773494)) ;
#30421 = CARTESIAN_POINT('Ctrl Pts',(-19.3739840223207,34.2287964297751,124.92908813568)) ;
#30422 = CARTESIAN_POINT('Ctrl Pts',(-19.3810402452549,34.0488073494122,124.625633782971)) ;
#30423 = CARTESIAN_POINT('Ctrl Pts',(-18.936720024018,34.2454103204623,124.86755517988)) ;
#30424 = CARTESIAN_POINT('Ctrl Pts',(-19.0312400607427,34.0654212400994,124.576410349906)) ;
#30425 = CARTESIAN_POINT('Ctrl Pts',(-18.4683529488932,34.2653591198897,124.618947214226)) ;
#30426 = CARTESIAN_POINT('Ctrl Pts',(-18.6565409486287,34.0853700395268,124.377526283527)) ;
#30427 = CARTESIAN_POINT('Ctrl Pts',(-18.1135823385577,34.2852802314206,124.226010700003)) ;
#30428 = CARTESIAN_POINT('Ctrl Pts',(-18.3727229363681,34.1052911510577,124.063178594994)) ;
#30429 = CARTESIAN_POINT('Ctrl Pts',(-17.9136663305497,34.3051466795934,123.737213595555)) ;
#30430 = CARTESIAN_POINT('Ctrl Pts',(-18.2127872251194,34.1251575992306,123.672140797996)) ;
#30431 = CARTESIAN_POINT('Ctrl Pts',(-17.8927069831386,34.3251730262106,123.205416904764)) ;
#30432 = CARTESIAN_POINT('Ctrl Pts',(-18.1960174659992,34.1451839458477,123.246703802556)) ;
#30433 = CARTESIAN_POINT('Ctrl Pts',(-18.0532950837359,34.3450350706001,122.702439446676)) ;
#30434 = CARTESIAN_POINT('Ctrl Pts',(-18.3244861394055,34.1650459902372,122.844319988715)) ;
#30435 = CARTESIAN_POINT('Ctrl Pts',(-18.3764719974847,34.3649803732812,122.282323158732)) ;
#30436 = CARTESIAN_POINT('Ctrl Pts',(-18.5830265759983,34.1849912929184,122.50822539218)) ;
#30437 = CARTESIAN_POINT('Ctrl Pts',(-18.8226102498659,34.3848756803401,121.998446004947)) ;
#30438 = CARTESIAN_POINT('Ctrl Pts',(-18.9399371661432,34.2048865999772,122.281121677154)) ;
#30439 = CARTESIAN_POINT('Ctrl Pts',(-19.3385786404572,34.4047689505077,121.882935209767)) ;
#30440 = CARTESIAN_POINT('Ctrl Pts',(-19.3527127879478,34.2247798701449,122.188711677315)) ;
#30441 = CARTESIAN_POINT('Ctrl Pts',(-19.864843872694,34.4247345431882,121.950781567567)) ;
#30442 = CARTESIAN_POINT('Ctrl Pts',(-19.773725507496,34.2447454628253,122.242987830082)) ;
#30443 = CARTESIAN_POINT('Ctrl Pts',(-20.3344600160615,34.444609866873,122.192739799094)) ;
#30444 = CARTESIAN_POINT('Ctrl Pts',(-20.149420050782,34.2646207865101,122.436554544585)) ;
#30445 = CARTESIAN_POINT('Ctrl Pts',(-20.6955112754201,34.464584929448,122.582004291072)) ;
#30446 = CARTESIAN_POINT('Ctrl Pts',(-20.4382613889304,34.2845958490851,122.74796620737)) ;
#30447 = CARTESIAN_POINT('Ctrl Pts',(-20.9010681970121,34.4845373390791,123.070845431308)) ;
#30448 = CARTESIAN_POINT('Ctrl Pts',(-20.6027074986626,34.3045482587162,123.139039529433)) ;
#30449 = CARTESIAN_POINT('Ctrl Pts',(-20.9283379623324,34.5043733933152,123.597346656962)) ;
#30450 = CARTESIAN_POINT('Ctrl Pts',(-20.6245230859658,34.3243843129523,123.560242643287)) ;
#30451 = CARTESIAN_POINT('Ctrl Pts',(-20.7737648833637,34.5243513047327,124.105329355223)) ;
#30452 = CARTESIAN_POINT('Ctrl Pts',(-20.5008637718727,34.3443622243698,123.966628801619)) ;
#30453 = CARTESIAN_POINT('Ctrl Pts',(-20.4555977349369,34.5442693542362,124.528394482397)) ;
#30454 = CARTESIAN_POINT('Ctrl Pts',(-20.2463288803223,34.3642802738733,124.305081255519)) ;
#30455 = CARTESIAN_POINT('Ctrl Pts',(-20.0139097341758,34.5641374980043,124.818008765311)) ;
#30456 = CARTESIAN_POINT('Ctrl Pts',(-19.8929765031619,34.3841484176414,124.536772192443)) ;
#30457 = CARTESIAN_POINT('Ctrl Pts',(-19.4952245290992,34.5841883545916,124.939780508264)) ;
#30458 = CARTESIAN_POINT('Ctrl Pts',(-19.4780285056584,34.4041992742287,124.634188162972)) ;
#30459 = CARTESIAN_POINT('Ctrl Pts',(-18.9729159061863,34.6039687910475,124.878612004196)) ;
#30460 = CARTESIAN_POINT('Ctrl Pts',(-19.0601796451305,34.4239797106846,124.585251399659)) ;
#30461 = CARTESIAN_POINT('Ctrl Pts',(-18.496759486199,34.6239988467253,124.640786108479)) ;
#30462 = CARTESIAN_POINT('Ctrl Pts',(-18.6792557743103,34.4440097663624,124.394988854983)) ;
#30463 = CARTESIAN_POINT('Ctrl Pts',(-18.1335792137849,34.6438799519001,124.256847057463)) ;
#30464 = CARTESIAN_POINT('Ctrl Pts',(-18.3887122909116,34.4638908715372,124.087835457315)) ;
#30465 = CARTESIAN_POINT('Ctrl Pts',(-17.9219139096296,34.6637604142679,123.772762991353)) ;
#30466 = CARTESIAN_POINT('Ctrl Pts',(-18.2193820937176,34.483771333905,123.700566231009)) ;
#30467 = CARTESIAN_POINT('Ctrl Pts',(-17.8881094855176,34.6837455614122,123.242649910961)) ;
#30468 = CARTESIAN_POINT('Ctrl Pts',(-18.1923412744921,34.5037564810494,123.276475501805)) ;
#30469 = CARTESIAN_POINT('Ctrl Pts',(-18.0366497415648,34.7036361399486,122.735276316463)) ;
#30470 = CARTESIAN_POINT('Ctrl Pts',(-18.3111764212583,34.5236470595857,122.87057664201)) ;
#30471 = CARTESIAN_POINT('Ctrl Pts',(-18.3487015779653,34.723530159823,122.308436690887)) ;
#30472 = CARTESIAN_POINT('Ctrl Pts',(-18.5608208835814,34.5435410794601,122.529106268789)) ;
#30473 = CARTESIAN_POINT('Ctrl Pts',(-18.7881430602527,34.7434516045494,122.013226846896)) ;
#30474 = CARTESIAN_POINT('Ctrl Pts',(-18.9123763432651,34.5634625241865,122.292940896369)) ;
#30475 = CARTESIAN_POINT('Ctrl Pts',(-19.3013427498124,34.7633497426048,121.884875817397)) ;
#30476 = CARTESIAN_POINT('Ctrl Pts',(-19.3229374638322,34.583360662242,122.190263485441)) ;
#30477 = CARTESIAN_POINT('Ctrl Pts',(-19.8317538659919,34.7834204978209,121.940822959894)) ;
#30478 = CARTESIAN_POINT('Ctrl Pts',(-19.7472655742941,34.603431417458,122.235024637541)) ;
#30479 = CARTESIAN_POINT('Ctrl Pts',(-20.3047188071783,34.8032060478722,122.170959918835)) ;
#30480 = CARTESIAN_POINT('Ctrl Pts',(-20.1256368670043,34.6232169675093,122.419137989732)) ;
#30481 = CARTESIAN_POINT('Ctrl Pts',(-20.6751904640124,34.8231891227495,122.55139832022)) ;
#30482 = CARTESIAN_POINT('Ctrl Pts',(-20.4220114541107,34.6432000423866,122.72349136495)) ;
#30483 = CARTESIAN_POINT('Ctrl Pts',(-20.8920819873269,34.8430982053954,123.034062768714)) ;
#30484 = CARTESIAN_POINT('Ctrl Pts',(-20.5955208682009,34.6631091250326,123.109625335908)) ;
#30485 = CARTESIAN_POINT('Ctrl Pts',(-20.9326680570592,34.8629567645182,123.560377307948)) ;
#30486 = CARTESIAN_POINT('Ctrl Pts',(-20.6279870568241,34.6829676841553,123.53067592304)) ;
#30487 = CARTESIAN_POINT('Ctrl Pts',(-20.7893451366516,34.8830002083569,124.073345382285)) ;
#30488 = CARTESIAN_POINT('Ctrl Pts',(-20.5133192229244,34.703011127994,123.941055778839)) ;
#30489 = CARTESIAN_POINT('Ctrl Pts',(-20.5344079580577,34.8995002730861,124.43033347796)) ;
#30490 = CARTESIAN_POINT('Ctrl Pts',(-20.309383562949,34.7195111927232,124.226623694968)) ;
#30491 = CARTESIAN_POINT('Ctrl Pts',(-20.2630356079764,34.912890012935,124.654232063007)) ;
#30492 = CARTESIAN_POINT('Ctrl Pts',(-20.0922687245513,34.7329009325721,124.405758721467)) ;
#30493 = CARTESIAN_POINT('Ctrl Pts',(-20.0376601532639,34.9227469141434,124.781982024209)) ;
#30494 = CARTESIAN_POINT('Ctrl Pts',(-19.911970256192,34.7427578337805,124.507953327853)) ;
#30495 = CARTESIAN_POINT('Ctrl Pts',(-19.7904462531825,34.9327384399899,124.870322609915)) ;
#30496 = CARTESIAN_POINT('Ctrl Pts',(-19.7141969621559,34.752749359627,124.578624529211)) ;
#30497 = CARTESIAN_POINT('Ctrl Pts',(-19.5333148830126,34.9426631204409,124.914209741491)) ;
#30498 = CARTESIAN_POINT('Ctrl Pts',(-19.5084940323309,34.762674040078,124.613732529277)) ;
#30499 = CARTESIAN_POINT('Ctrl Pts',(-19.2702905171994,34.9526737104853,124.912873328828)) ;
#30500 = CARTESIAN_POINT('Ctrl Pts',(-19.2980655576572,34.7726846301224,124.61265864524)) ;
#30501 = CARTESIAN_POINT('Ctrl Pts',(-18.9272936377873,34.9659329711889,124.851006430555)) ;
#30502 = CARTESIAN_POINT('Ctrl Pts',(-19.0237133047444,34.7859438908261,124.563175229187)) ;
#30503 = CARTESIAN_POINT('Ctrl Pts',(-18.606436005865,34.9792840463392,124.69972105366)) ;
#30504 = CARTESIAN_POINT('Ctrl Pts',(-18.7669990812473,34.7992949659763,124.442141522519)) ;
#30505 = CARTESIAN_POINT('Ctrl Pts',(-18.3413122765646,34.992490355574,124.475665673841)) ;
#30506 = CARTESIAN_POINT('Ctrl Pts',(-18.5548921869106,34.8125012752111,124.262885113938)) ;
#30507 = CARTESIAN_POINT('Ctrl Pts',(-18.1729444100433,35.0024771891643,124.274406568228)) ;
#30508 = CARTESIAN_POINT('Ctrl Pts',(-18.4202016064083,34.8224881088014,124.101878384377)) ;
#30509 = CARTESIAN_POINT('Ctrl Pts',(-18.0423683362087,35.0124299166604,124.047733829672)) ;
#30510 = CARTESIAN_POINT('Ctrl Pts',(-18.3157421784876,34.8324408362975,123.920538559733)) ;
#30511 = CARTESIAN_POINT('Ctrl Pts',(-17.9525123755645,35.022478013502,123.799470169266)) ;
#30512 = CARTESIAN_POINT('Ctrl Pts',(-18.2438596889398,34.8424889331391,123.721927081998)) ;
#30513 = CARTESIAN_POINT('Ctrl Pts',(-17.9077516294115,35.0323194703738,123.544724476242)) ;
#30514 = CARTESIAN_POINT('Ctrl Pts',(-18.208053265257,34.8523303900109,123.518130066413)) ;
#30515 = CARTESIAN_POINT('Ctrl Pts',(-17.9073445683786,35.0423057372873,123.282339109367)) ;
#30516 = CARTESIAN_POINT('Ctrl Pts',(-18.2077298902901,34.8623166569244,123.308221845002)) ;
#30517 = CARTESIAN_POINT('Ctrl Pts',(-17.9521637827218,35.0522423381877,123.025046666914)) ;
#30518 = CARTESIAN_POINT('Ctrl Pts',(-18.2435874714704,34.8722532578248,123.10238833231)) ;
#30519 = CARTESIAN_POINT('Ctrl Pts',(-18.0420906679866,35.0622922809748,122.776754559742)) ;
#30520 = CARTESIAN_POINT('Ctrl Pts',(-18.3155310899466,34.8823032006119,122.903755461618)) ;
#30521 = CARTESIAN_POINT('Ctrl Pts',(-18.1709996406622,35.0721424806605,122.552262724124)) ;
#30522 = CARTESIAN_POINT('Ctrl Pts',(-18.4186601790438,34.8921534002976,122.724163199285)) ;
#30523 = CARTESIAN_POINT('Ctrl Pts',(-18.3384352196694,35.0821153855926,122.350682137594)) ;
#30524 = CARTESIAN_POINT('Ctrl Pts',(-18.5526103127129,34.9021263052297,122.562900239816)) ;
#30525 = CARTESIAN_POINT('Ctrl Pts',(-18.5389407429953,35.0921137600722,122.180827804113)) ;
#30526 = CARTESIAN_POINT('Ctrl Pts',(-18.7130161369838,34.9121246797094,122.427018525397)) ;
#30527 = CARTESIAN_POINT('Ctrl Pts',(-18.7664484679922,35.1021339339422,122.048263316574)) ;
#30528 = CARTESIAN_POINT('Ctrl Pts',(-18.8950234142683,34.9221448535794,122.320968904354)) ;
#30529 = CARTESIAN_POINT('Ctrl Pts',(-19.0105165623716,35.1120349778842,121.958081319082)) ;
#30530 = CARTESIAN_POINT('Ctrl Pts',(-19.0902785364057,34.9320458975213,122.24882546228)) ;
#30531 = CARTESIAN_POINT('Ctrl Pts',(-19.2687227454526,35.1220237816085,121.910830619248)) ;
#30532 = CARTESIAN_POINT('Ctrl Pts',(-19.2968438044793,34.9420347012456,122.211027113215)) ;
#30533 = CARTESIAN_POINT('Ctrl Pts',(-19.5305882706686,35.1319892484403,121.909321300949)) ;
#30534 = CARTESIAN_POINT('Ctrl Pts',(-19.5063361388599,34.9520001680775,122.209821901071)) ;
#30535 = CARTESIAN_POINT('Ctrl Pts',(-19.7872767838356,35.1418928107133,121.952415553993)) ;
#30536 = CARTESIAN_POINT('Ctrl Pts',(-19.7116863821234,34.9619037303504,122.244299447509)) ;
#30537 = CARTESIAN_POINT('Ctrl Pts',(-20.0363461469721,35.1519534885913,122.040990349835)) ;
#30538 = CARTESIAN_POINT('Ctrl Pts',(-19.9109411536517,34.9719644082284,122.315161388044)) ;
#30539 = CARTESIAN_POINT('Ctrl Pts',(-20.2614426416287,35.1617937865408,122.168353377903)) ;
#30540 = CARTESIAN_POINT('Ctrl Pts',(-20.0910169782063,34.9818047061779,122.417053562184)) ;
#30541 = CARTESIAN_POINT('Ctrl Pts',(-20.4656690482286,35.1718567814502,122.33629520841)) ;
#30542 = CARTESIAN_POINT('Ctrl Pts',(-20.2543967460004,34.9918677010873,122.551408735198)) ;
#30543 = CARTESIAN_POINT('Ctrl Pts',(-20.6346269466373,35.1817510755973,122.533966500745)) ;
#30544 = CARTESIAN_POINT('Ctrl Pts',(-20.389561223534,35.0017619952345,122.709546994155)) ;
#30545 = CARTESIAN_POINT('Ctrl Pts',(-20.7679099510609,35.1916928732942,122.758634465352)) ;
#30546 = CARTESIAN_POINT('Ctrl Pts',(-20.4961856757514,35.0117037929313,122.889282276775)) ;
#30547 = CARTESIAN_POINT('Ctrl Pts',(-20.8608365588192,35.2016954508233,123.004554830575)) ;
#30548 = CARTESIAN_POINT('Ctrl Pts',(-20.5705249456458,35.0217063704604,123.086019259422)) ;
#30549 = CARTESIAN_POINT('Ctrl Pts',(-20.9093992123313,35.2117299147444,123.263726218813)) ;
#30550 = CARTESIAN_POINT('Ctrl Pts',(-20.6093729389667,35.0317408343815,123.293356782246)) ;
#30551 = CARTESIAN_POINT('Ctrl Pts',(-20.912575954229,35.2215760532655,123.522461220006)) ;
#30552 = CARTESIAN_POINT('Ctrl Pts',(-20.6119121959131,35.0415869729026,123.500344358)) ;
#30553 = CARTESIAN_POINT('Ctrl Pts',(-20.8707879748683,35.2315572265025,123.781384610257)) ;
#30554 = CARTESIAN_POINT('Ctrl Pts',(-20.5784797854132,35.0515681461396,123.707482601004)) ;
#30555 = CARTESIAN_POINT('Ctrl Pts',(-20.7848581741263,35.2415095204597,124.028409346698)) ;
#30556 = CARTESIAN_POINT('Ctrl Pts',(-20.5097340530019,35.0615204400968,123.905101502577)) ;
#30557 = CARTESIAN_POINT('Ctrl Pts',(-20.6570382603351,35.2515083155943,124.258005618651)) ;
#30558 = CARTESIAN_POINT('Ctrl Pts',(-20.4074763796465,35.0715192352314,124.088777453895)) ;
#30559 = CARTESIAN_POINT('Ctrl Pts',(-20.4902556612724,35.2615474238551,124.462394870675)) ;
#30560 = CARTESIAN_POINT('Ctrl Pts',(-20.2740486420064,35.0815583434922,124.252287564926)) ;
#30561 = CARTESIAN_POINT('Ctrl Pts',(-20.2951179160963,35.2713723652943,124.631484396849)) ;
#30562 = CARTESIAN_POINT('Ctrl Pts',(-20.117937581225,35.0913832849314,124.387557244038)) ;
#30563 = CARTESIAN_POINT('Ctrl Pts',(-20.0686559821828,35.2814270523687,124.767580615175)) ;
#30564 = CARTESIAN_POINT('Ctrl Pts',(-19.9367669380912,35.1014379720058,124.496432562579)) ;
#30565 = CARTESIAN_POINT('Ctrl Pts',(-19.8245654449264,35.2913698573088,124.860825828368)) ;
#30566 = CARTESIAN_POINT('Ctrl Pts',(-19.74149402968,35.1113807769459,124.571026731217)) ;
#30567 = CARTESIAN_POINT('Ctrl Pts',(-19.5691531625667,35.3012736433053,124.910862029586)) ;
#30568 = CARTESIAN_POINT('Ctrl Pts',(-19.5371642509211,35.1212845629424,124.61105371151)) ;
#30569 = CARTESIAN_POINT('Ctrl Pts',(-19.3052006854437,35.3113204598701,124.915700617854)) ;
#30570 = CARTESIAN_POINT('Ctrl Pts',(-19.3260021502799,35.1313313795072,124.614922626619)) ;
#30571 = CARTESIAN_POINT('Ctrl Pts',(-19.0482438728121,35.3212159793488,124.875474923149)) ;
#30572 = CARTESIAN_POINT('Ctrl Pts',(-19.1204374586696,35.1412268989859,124.582740243431)) ;
#30573 = CARTESIAN_POINT('Ctrl Pts',(-18.7981091918514,35.3312780646732,124.789853312718)) ;
#30574 = CARTESIAN_POINT('Ctrl Pts',(-18.9203301991824,35.1512889843104,124.514241085553)) ;
#30575 = CARTESIAN_POINT('Ctrl Pts',(-18.571557569673,35.3411207756312,124.664983089902)) ;
#30576 = CARTESIAN_POINT('Ctrl Pts',(-18.7390904274587,35.1611316952683,124.4143435761)) ;
#30577 = CARTESIAN_POINT('Ctrl Pts',(-18.3667589020139,35.3511114929372,124.500756432804)) ;
#30578 = CARTESIAN_POINT('Ctrl Pts',(-18.5752527356648,35.1711224125743,124.282960925271)) ;
#30579 = CARTESIAN_POINT('Ctrl Pts',(-18.1946758847601,35.3610395760338,124.304637787655)) ;
#30580 = CARTESIAN_POINT('Ctrl Pts',(-18.4375879438694,35.1810504956709,124.126065105729)) ;
#30581 = CARTESIAN_POINT('Ctrl Pts',(-18.0580530664321,35.3710275061455,124.080513754998)) ;
#30582 = CARTESIAN_POINT('Ctrl Pts',(-18.3282912523427,35.1910384257827,123.946765097769)) ;
#30583 = CARTESIAN_POINT('Ctrl Pts',(-17.9623826480587,35.3810633322728,123.83475626619)) ;
#30584 = CARTESIAN_POINT('Ctrl Pts',(-18.2517565843422,35.20107425191,123.750158383688)) ;
#30585 = CARTESIAN_POINT('Ctrl Pts',(-17.9113535514333,35.3909186693864,123.580830234499)) ;
#30586 = CARTESIAN_POINT('Ctrl Pts',(-18.2109351630595,35.2109295890236,123.547017932825)) ;
#30587 = CARTESIAN_POINT('Ctrl Pts',(-17.9046862415223,35.4009164042366,123.318213209581)) ;
#30588 = CARTESIAN_POINT('Ctrl Pts',(-18.205602992744,35.2209273238737,123.336924392206)) ;
#30589 = CARTESIAN_POINT('Ctrl Pts',(-17.9432873405184,35.4108243082211,123.060708970242)) ;
#30590 = CARTESIAN_POINT('Ctrl Pts',(-18.2364854316828,35.2308352278582,123.130921769729)) ;
#30591 = CARTESIAN_POINT('Ctrl Pts',(-18.0264553068263,35.4208353827695,122.811112169827)) ;
#30592 = CARTESIAN_POINT('Ctrl Pts',(-18.3030212907696,35.2408463024066,122.931244865584)) ;
#30593 = CARTESIAN_POINT('Ctrl Pts',(-18.1523789389796,35.4308632383051,122.579621476818)) ;
#30594 = CARTESIAN_POINT('Ctrl Pts',(-18.403761694324,35.2508741579423,122.746053067434)) ;
#30595 = CARTESIAN_POINT('Ctrl Pts',(-18.3134289650525,35.4407208322104,122.376725539727)) ;
#30596 = CARTESIAN_POINT('Ctrl Pts',(-18.5326024658146,35.2607317518475,122.583737933796)) ;
#30597 = CARTESIAN_POINT('Ctrl Pts',(-18.5102358433116,35.4507475190485,122.201520587918)) ;
#30598 = CARTESIAN_POINT('Ctrl Pts',(-18.6900489765213,35.2707584386856,122.443575071446)) ;
#30599 = CARTESIAN_POINT('Ctrl Pts',(-18.7348673255698,35.4607761882022,122.063678979707)) ;
#30600 = CARTESIAN_POINT('Ctrl Pts',(-18.8697550564223,35.2807871078393,122.333303131403)) ;
#30601 = CARTESIAN_POINT('Ctrl Pts',(-18.9753389392073,35.4706213964836,121.968264330612)) ;
#30602 = CARTESIAN_POINT('Ctrl Pts',(-19.0621320757983,35.2906323161207,122.256973158654)) ;
#30603 = CARTESIAN_POINT('Ctrl Pts',(-19.232344395239,35.4806120854467,121.914585662056)) ;
#30604 = CARTESIAN_POINT('Ctrl Pts',(-19.2677365699942,35.3006230050839,122.214031608862)) ;
#30605 = CARTESIAN_POINT('Ctrl Pts',(-19.4960145845419,35.490649961729,121.906896220203)) ;
#30606 = CARTESIAN_POINT('Ctrl Pts',(-19.4786728720695,35.3106608813661,122.207881552385)) ;
#30607 = CARTESIAN_POINT('Ctrl Pts',(-19.7520613231325,35.5004943393712,121.943923950967)) ;
#30608 = CARTESIAN_POINT('Ctrl Pts',(-19.6835091319941,35.3205052590084,122.237504996433)) ;
#30609 = CARTESIAN_POINT('Ctrl Pts',(-20.0014137029836,35.5104791437627,122.025494346825)) ;
#30610 = CARTESIAN_POINT('Ctrl Pts',(-19.8829904412346,35.3304900633998,122.302762488264)) ;
#30611 = CARTESIAN_POINT('Ctrl Pts',(-20.2318815338735,35.5204186739812,122.148494733348)) ;
#30612 = CARTESIAN_POINT('Ctrl Pts',(-20.0673637209045,35.3404295936183,122.401163717447)) ;
#30613 = CARTESIAN_POINT('Ctrl Pts',(-20.4394809697131,35.5304583620181,122.311280393352)) ;
#30614 = CARTESIAN_POINT('Ctrl Pts',(-20.2334425657068,35.3504692816552,122.53139333392)) ;
#30615 = CARTESIAN_POINT('Ctrl Pts',(-20.6131244207075,35.5403466513864,122.504619288811)) ;
#30616 = CARTESIAN_POINT('Ctrl Pts',(-20.3723558935254,35.3603575710235,122.686064744329)) ;
#30617 = CARTESIAN_POINT('Ctrl Pts',(-20.7523694041922,35.5503357750712,122.72713725888)) ;
#30618 = CARTESIAN_POINT('Ctrl Pts',(-20.4837508097204,35.3703466947083,122.864079588493)) ;
#30619 = CARTESIAN_POINT('Ctrl Pts',(-20.8503882560538,35.5602957847458,122.969824688647)) ;
#30620 = CARTESIAN_POINT('Ctrl Pts',(-20.5621646481119,35.3803067043829,123.058229659203)) ;
#30621 = CARTESIAN_POINT('Ctrl Pts',(-20.9050630989688,35.57019621445,123.224196430447)) ;
#30622 = CARTESIAN_POINT('Ctrl Pts',(-20.6059033396929,35.3902071340872,123.261726591413)) ;
#30623 = CARTESIAN_POINT('Ctrl Pts',(-20.9148664709882,35.5802392958568,123.487924566708)) ;
#30624 = CARTESIAN_POINT('Ctrl Pts',(-20.6137449783066,35.4002502154939,123.472709296187)) ;
#30625 = CARTESIAN_POINT('Ctrl Pts',(-20.8792189654738,35.5901466897644,123.74584291802)) ;
#30626 = CARTESIAN_POINT('Ctrl Pts',(-20.5852260111583,35.4101576094016,123.679043182914)) ;
#30627 = CARTESIAN_POINT('Ctrl Pts',(-20.7989552795368,35.6001584207536,123.996400804876)) ;
#30628 = CARTESIAN_POINT('Ctrl Pts',(-20.5210141652758,35.4201693403907,123.879489165425)) ;
#30629 = CARTESIAN_POINT('Ctrl Pts',(-20.6756899073301,35.6101906384684,124.229454654533)) ;
#30630 = CARTESIAN_POINT('Ctrl Pts',(-20.4224008782605,35.4302015581055,124.065931815006)) ;
#30631 = CARTESIAN_POINT('Ctrl Pts',(-20.5170202759795,35.6200431477146,124.434034154075)) ;
#30632 = CARTESIAN_POINT('Ctrl Pts',(-20.2954650100176,35.4400540673517,124.229594006282)) ;
#30633 = CARTESIAN_POINT('Ctrl Pts',(-20.3237177193579,35.6300010842576,124.610433802406)) ;
#30634 = CARTESIAN_POINT('Ctrl Pts',(-20.1408227029007,35.4500120038947,124.370712879431)) ;
#30635 = CARTESIAN_POINT('Ctrl Pts',(-20.1006943914862,35.6400399542659,124.751315017522)) ;
#30636 = CARTESIAN_POINT('Ctrl Pts',(-19.9624034408403,35.460050873903,124.483417150071)) ;
#30637 = CARTESIAN_POINT('Ctrl Pts',(-19.8607559657353,35.6499131094241,124.850152762012)) ;
#30638 = CARTESIAN_POINT('Ctrl Pts',(-19.7704532300316,35.4699240290612,124.562486266306)) ;
#30639 = CARTESIAN_POINT('Ctrl Pts',(-19.6022411196816,35.6599863842738,124.906856510779)) ;
#30640 = CARTESIAN_POINT('Ctrl Pts',(-19.5636408438425,35.4799973039109,124.607848540031)) ;
#30641 = CARTESIAN_POINT('Ctrl Pts',(-19.3443505908473,35.6698067014512,124.917880380727)) ;
#30642 = CARTESIAN_POINT('Ctrl Pts',(-19.3573296329594,35.4898176210883,124.616666850261)) ;
#30643 = CARTESIAN_POINT('Ctrl Pts',(-19.0818227174019,35.6798853872447,124.883323751729)) ;
#30644 = CARTESIAN_POINT('Ctrl Pts',(-19.147307048226,35.4998963068818,124.589020826947)) ;
#30645 = CARTESIAN_POINT('Ctrl Pts',(-18.8348266453424,35.6897368986278,124.805553629414)) ;
#30646 = CARTESIAN_POINT('Ctrl Pts',(-18.9497113939592,35.5097478182649,124.526804423587)) ;
#30647 = CARTESIAN_POINT('Ctrl Pts',(-18.5999081950905,35.6998103449344,124.683638544709)) ;
#30648 = CARTESIAN_POINT('Ctrl Pts',(-18.7617765978972,35.5198212645716,124.429271661873)) ;
#30649 = CARTESIAN_POINT('Ctrl Pts',(-18.3945197612094,35.7096516200591,124.526430434708)) ;
#30650 = CARTESIAN_POINT('Ctrl Pts',(-18.5974671222276,35.5296625396963,124.303505384468)) ;
#30651 = CARTESIAN_POINT('Ctrl Pts',(-18.2164254320828,35.7196367197159,124.333759479541)) ;
#30652 = CARTESIAN_POINT('Ctrl Pts',(-18.4549921099954,35.539647639353,124.149368519473)) ;
#30653 = CARTESIAN_POINT('Ctrl Pts',(-18.0744564633631,35.7296441958502,124.112362113073)) ;
#30654 = CARTESIAN_POINT('Ctrl Pts',(-18.3414173794509,35.5496551154873,123.972250409102)) ;
#30655 = CARTESIAN_POINT('Ctrl Pts',(-17.9737377684653,35.7395667835592,123.871857563518)) ;
#30656 = CARTESIAN_POINT('Ctrl Pts',(-18.2608430645821,35.5595777031963,123.779847173338)) ;
#30657 = CARTESIAN_POINT('Ctrl Pts',(-17.915514233427,35.7495533878325,123.61593526692)) ;
#30658 = CARTESIAN_POINT('Ctrl Pts',(-18.2142645957526,35.5695643074696,123.575109448264)) ;
#30659 = CARTESIAN_POINT('Ctrl Pts',(-17.9030386020177,35.7595935161666,123.352407710946)) ;
#30660 = CARTESIAN_POINT('Ctrl Pts',(-18.2042845372192,35.5796044358037,123.364287232758)) ;
#30661 = CARTESIAN_POINT('Ctrl Pts',(-17.9352873093838,35.7694329507,123.095829361004)) ;
#30662 = CARTESIAN_POINT('Ctrl Pts',(-18.2300836623065,35.5894438703371,123.159025769629)) ;
#30663 = CARTESIAN_POINT('Ctrl Pts',(-18.0131110083021,35.779497005191,122.843100123072)) ;
#30664 = CARTESIAN_POINT('Ctrl Pts',(-18.2923429533616,35.5995079248281,122.956842160068)) ;
#30665 = CARTESIAN_POINT('Ctrl Pts',(-18.1316925352344,35.7893879244282,122.611771524711)) ;
#30666 = CARTESIAN_POINT('Ctrl Pts',(-18.3872080467958,35.6093988440653,122.771780155463)) ;
#30667 = CARTESIAN_POINT('Ctrl Pts',(-18.2897713917017,35.7993799177342,122.402124132987)) ;
#30668 = CARTESIAN_POINT('Ctrl Pts',(-18.5136711422251,35.6193908373713,122.604062465028)) ;
#30669 = CARTESIAN_POINT('Ctrl Pts',(-18.4814613118421,35.8093427816935,122.223804692162)) ;
#30670 = CARTESIAN_POINT('Ctrl Pts',(-18.6670229513666,35.6293537013306,122.461407311499)) ;
#30671 = CARTESIAN_POINT('Ctrl Pts',(-18.6995746479886,35.8192470415113,122.081746101379)) ;
#30672 = CARTESIAN_POINT('Ctrl Pts',(-18.8415130103748,35.6392579611484,122.347760879673)) ;
#30673 = CARTESIAN_POINT('Ctrl Pts',(-18.9428567780933,35.8293075320827,121.978340523878)) ;
#30674 = CARTESIAN_POINT('Ctrl Pts',(-19.0361390123414,35.6493184517198,122.265036395034)) ;
#30675 = CARTESIAN_POINT('Ctrl Pts',(-19.1947540652062,35.8391478817137,121.919707183759)) ;
#30676 = CARTESIAN_POINT('Ctrl Pts',(-19.2376556973774,35.6591588013508,122.218129998438)) ;
#30677 = CARTESIAN_POINT('Ctrl Pts',(-19.4587582959314,35.8492108572037,121.905070980687)) ;
#30678 = CARTESIAN_POINT('Ctrl Pts',(-19.448859376931,35.6692217768408,122.206420948279)) ;
#30679 = CARTESIAN_POINT('Ctrl Pts',(-19.716930430725,35.8591051773471,121.936190237955)) ;
#30680 = CARTESIAN_POINT('Ctrl Pts',(-19.6553962747645,35.6791160969842,122.231316240817)) ;
#30681 = CARTESIAN_POINT('Ctrl Pts',(-19.9671129941824,35.8690468904787,122.011332156098)) ;
#30682 = CARTESIAN_POINT('Ctrl Pts',(-19.8555418925478,35.6890578101158,122.291429441969)) ;
#30683 = CARTESIAN_POINT('Ctrl Pts',(-20.2020024297301,35.8790497802728,122.129427167199)) ;
#30684 = CARTESIAN_POINT('Ctrl Pts',(-20.0434534559638,35.69906069991,122.385905206129)) ;
#30685 = CARTESIAN_POINT('Ctrl Pts',(-20.4132559197395,35.8890896374333,122.28744132461)) ;
#30686 = CARTESIAN_POINT('Ctrl Pts',(-20.2124564260292,35.7091005570704,122.512316537818)) ;
#30687 = CARTESIAN_POINT('Ctrl Pts',(-20.5904446049363,35.8989138182709,122.475235422024)) ;
#30688 = CARTESIAN_POINT('Ctrl Pts',(-20.3542066813593,35.7189247379081,122.662550716544)) ;
#30689 = CARTESIAN_POINT('Ctrl Pts',(-20.7359772784035,35.9089707917741,122.695816923843)) ;
#30690 = CARTESIAN_POINT('Ctrl Pts',(-20.4706332561571,35.7289817114113,122.839015952767)) ;
#30691 = CARTESIAN_POINT('Ctrl Pts',(-20.8393638309279,35.9188989159612,122.935375322683)) ;
#30692 = CARTESIAN_POINT('Ctrl Pts',(-20.5533424999389,35.7389098355983,123.030662030176)) ;
#30693 = CARTESIAN_POINT('Ctrl Pts',(-20.9004170383969,35.9288526110346,123.189725205683)) ;
#30694 = CARTESIAN_POINT('Ctrl Pts',(-20.602185386523,35.7488635306717,123.234141416124)) ;
#30695 = CARTESIAN_POINT('Ctrl Pts',(-20.9161514803797,35.9388988046099,123.453256665995)) ;
#30696 = CARTESIAN_POINT('Ctrl Pts',(-20.6147732911417,35.758909724247,123.444966757205)) ;
#30697 = CARTESIAN_POINT('Ctrl Pts',(-20.8867329496708,35.9487469069698,123.710376268567)) ;
#30698 = CARTESIAN_POINT('Ctrl Pts',(-20.5912389928801,35.7687578266069,123.650661374287)) ;
#30699 = CARTESIAN_POINT('Ctrl Pts',(-20.813048468652,35.9587084951974,123.961560575043)) ;
#30700 = CARTESIAN_POINT('Ctrl Pts',(-20.5322920915651,35.7787194148345,123.851608640381)) ;
#30701 = CARTESIAN_POINT('Ctrl Pts',(-20.6957786698797,35.9687371653537,124.19759210035)) ;
#30702 = CARTESIAN_POINT('Ctrl Pts',(-20.4384766850489,35.7887480849908,124.04043416191)) ;
#30703 = CARTESIAN_POINT('Ctrl Pts',(-20.5412377893036,35.9786474682354,124.407201312219)) ;
#30704 = CARTESIAN_POINT('Ctrl Pts',(-20.3148448330596,35.7986583878725,124.208121289199)) ;
#30705 = CARTESIAN_POINT('Ctrl Pts',(-20.3526398125085,35.9885823520433,124.587747365873)) ;
#30706 = CARTESIAN_POINT('Ctrl Pts',(-20.1639673252218,35.8085932716804,124.352558280755)) ;
#30707 = CARTESIAN_POINT('Ctrl Pts',(-20.1331135059456,35.9986234937339,124.734141809642)) ;
#30708 = CARTESIAN_POINT('Ctrl Pts',(-19.9883465163358,35.8186344133711,124.469674459931)) ;
#30709 = CARTESIAN_POINT('Ctrl Pts',(-19.8952608881985,36.0085106148979,124.838745840386)) ;
#30710 = CARTESIAN_POINT('Ctrl Pts',(-19.7980654626942,35.828521534535,124.553357985807)) ;
#30711 = CARTESIAN_POINT('Ctrl Pts',(-19.6403085962477,36.0185029577464,124.901535971408)) ;
#30712 = CARTESIAN_POINT('Ctrl Pts',(-19.5941039789621,35.8385138773836,124.603590829665)) ;
#30713 = CARTESIAN_POINT('Ctrl Pts',(-19.3794454821469,36.0284512589704,124.918954868183)) ;
#30714 = CARTESIAN_POINT('Ctrl Pts',(-19.3854139711554,35.8484621786075,124.617526697189)) ;
#30715 = CARTESIAN_POINT('Ctrl Pts',(-19.1197882532334,36.0383888366525,124.8912260194)) ;
#30716 = CARTESIAN_POINT('Ctrl Pts',(-19.1776886066464,35.8583997562896,124.595344542413)) ;
#30717 = CARTESIAN_POINT('Ctrl Pts',(-18.8675463523897,36.0483754111031,124.818724120264)) ;
#30718 = CARTESIAN_POINT('Ctrl Pts',(-18.9758950062236,35.8683863307402,124.537343974835)) ;
#30719 = CARTESIAN_POINT('Ctrl Pts',(-18.6308789216368,36.0584042210115,124.702775017872)) ;
#30720 = CARTESIAN_POINT('Ctrl Pts',(-18.7865606156517,35.8784151406487,124.444585433762)) ;
#30721 = CARTESIAN_POINT('Ctrl Pts',(-18.4209855121877,36.0682825423183,124.550028242115)) ;
#30722 = CARTESIAN_POINT('Ctrl Pts',(-18.6186460335251,35.8882934619554,124.322389261554)) ;
#30723 = CARTESIAN_POINT('Ctrl Pts',(-18.2382837456184,36.0782741896657,124.361434085726)) ;
#30724 = CARTESIAN_POINT('Ctrl Pts',(-18.4724839618908,35.8982851093029,124.17151478619)) ;
#30725 = CARTESIAN_POINT('Ctrl Pts',(-18.0909304837619,36.0883087131035,124.142763989122)) ;
#30726 = CARTESIAN_POINT('Ctrl Pts',(-18.3546005264068,35.9083196327406,123.996579163665)) ;
#30727 = CARTESIAN_POINT('Ctrl Pts',(-17.9851026047473,36.0981720699821,123.906123266323)) ;
#30728 = CARTESIAN_POINT('Ctrl Pts',(-18.2699376258738,35.9181829896192,123.807267861114)) ;
#30729 = CARTESIAN_POINT('Ctrl Pts',(-17.9206102595099,36.1082422966624,123.649496524002)) ;
#30730 = CARTESIAN_POINT('Ctrl Pts',(-18.2183426310434,35.9282532162995,123.601966434206)) ;
#30731 = CARTESIAN_POINT('Ctrl Pts',(-17.9020958099089,36.1180846047971,123.391502808904)) ;
#30732 = CARTESIAN_POINT('Ctrl Pts',(-18.2035300751442,35.9380955244342,123.39557257472)) ;
#30733 = CARTESIAN_POINT('Ctrl Pts',(-17.9280157514707,36.1280453368205,123.131037798645)) ;
#30734 = CARTESIAN_POINT('Ctrl Pts',(-18.2242647137395,35.9480562564576,123.187200762251)) ;
#30735 = CARTESIAN_POINT('Ctrl Pts',(-17.999816726095,36.1380832260186,122.877221984986)) ;
#30736 = CARTESIAN_POINT('Ctrl Pts',(-18.2817043938246,35.9580941456557,122.984147689638)) ;
#30737 = CARTESIAN_POINT('Ctrl Pts',(-18.1123123668843,36.1479575089374,122.643353698666)) ;
#30738 = CARTESIAN_POINT('Ctrl Pts',(-18.3716994042814,35.9679684285746,122.797053236207)) ;
#30739 = CARTESIAN_POINT('Ctrl Pts',(-18.2666755578384,36.1580272535549,122.428462610188)) ;
#30740 = CARTESIAN_POINT('Ctrl Pts',(-18.4951890841048,35.978038173192,122.625139394901)) ;
#30741 = CARTESIAN_POINT('Ctrl Pts',(-18.4515040641022,36.1678605639005,122.247839904849)) ;
#30742 = CARTESIAN_POINT('Ctrl Pts',(-18.6430502466827,35.9878714835377,122.480641013743)) ;
#30743 = CARTESIAN_POINT('Ctrl Pts',(-18.6687131962433,36.1778908072532,122.098528505516)) ;
#30744 = CARTESIAN_POINT('Ctrl Pts',(-18.8168167817684,35.9979017268903,122.361190651918)) ;
#30745 = CARTESIAN_POINT('Ctrl Pts',(-18.9089342117129,36.1879230952316,121.98989079608)) ;
#30746 = CARTESIAN_POINT('Ctrl Pts',(-19.0089931242432,36.0079340148687,122.274279275505)) ;
#30747 = CARTESIAN_POINT('Ctrl Pts',(-19.1589917224903,36.1977502716997,121.925355327248)) ;
#30748 = CARTESIAN_POINT('Ctrl Pts',(-19.2090377774814,36.0177611913368,122.222649778263)) ;
#30749 = CARTESIAN_POINT('Ctrl Pts',(-19.4210472098018,36.2077556545666,121.904313326992)) ;
#30750 = CARTESIAN_POINT('Ctrl Pts',(-19.4186819756106,36.0277665742037,122.205814653997)) ;
#30751 = CARTESIAN_POINT('Ctrl Pts',(-19.6822546897857,36.2177382935593,121.929130110005)) ;
#30752 = CARTESIAN_POINT('Ctrl Pts',(-19.6276479311042,36.0377492131964,122.225666559862)) ;
#30753 = CARTESIAN_POINT('Ctrl Pts',(-19.9365810271852,36.2277823606959,121.999644910744)) ;
#30754 = CARTESIAN_POINT('Ctrl Pts',(-19.8311095076827,36.047793280333,122.282077034315)) ;
#30755 = CARTESIAN_POINT('Ctrl Pts',(-20.1697398906336,36.2376035794999,122.110337795579)) ;
#30756 = CARTESIAN_POINT('Ctrl Pts',(-20.0176363566891,36.057614499137,122.370629526365)) ;
#30757 = CARTESIAN_POINT('Ctrl Pts',(-20.3851350977547,36.247640418438,122.262557053081)) ;
#30758 = CARTESIAN_POINT('Ctrl Pts',(-20.1899535516625,36.0676513380751,122.492403621598)) ;
#30759 = CARTESIAN_POINT('Ctrl Pts',(-20.5700735002195,36.2576648305357,122.450169309994)) ;
#30760 = CARTESIAN_POINT('Ctrl Pts',(-20.3379053729967,36.0776757501728,122.64249237106)) ;
#30761 = CARTESIAN_POINT('Ctrl Pts',(-20.7175254012894,36.267516914941,122.662985785925)) ;
#30762 = CARTESIAN_POINT('Ctrl Pts',(-20.4558677751605,36.0875278345781,122.812743960038)) ;
#30763 = CARTESIAN_POINT('Ctrl Pts',(-20.827658912847,36.2775078116842,122.901285416374)) ;
#30764 = CARTESIAN_POINT('Ctrl Pts',(-20.5439760743343,36.0975187313213,123.003382825012)) ;
#30765 = CARTESIAN_POINT('Ctrl Pts',(-20.894433698142,36.2874258035851,123.153253367672)) ;
#30766 = CARTESIAN_POINT('Ctrl Pts',(-20.597397457909,36.1074367232222,123.204956301286)) ;
#30767 = CARTESIAN_POINT('Ctrl Pts',(-20.9167470714456,36.2974539190421,123.415814568147)) ;
#30768 = CARTESIAN_POINT('Ctrl Pts',(-20.6152498951296,36.1174648386792,123.415005141595)) ;
#30769 = CARTESIAN_POINT('Ctrl Pts',(-20.8935762347595,36.3073390949842,123.674557784478)) ;
#30770 = CARTESIAN_POINT('Ctrl Pts',(-20.5967150310461,36.1273500146213,123.621999285867)) ;
#30771 = CARTESIAN_POINT('Ctrl Pts',(-20.8257335492576,36.3173284533911,123.928155184694)) ;
#30772 = CARTESIAN_POINT('Ctrl Pts',(-20.5424427145472,36.1373393730282,123.824877566207)) ;
#30773 = CARTESIAN_POINT('Ctrl Pts',(-20.7138111338408,36.3273696009714,124.167113009814)) ;
#30774 = CARTESIAN_POINT('Ctrl Pts',(-20.4529063575782,36.1473805206085,124.016044644643)) ;
#30775 = CARTESIAN_POINT('Ctrl Pts',(-20.5656005075822,36.3372022239778,124.378768633685)) ;
#30776 = CARTESIAN_POINT('Ctrl Pts',(-20.334339803994,36.157213143615,124.185369574841)) ;
#30777 = CARTESIAN_POINT('Ctrl Pts',(-20.3804184420739,36.3471962950886,124.564996698335)) ;
#30778 = CARTESIAN_POINT('Ctrl Pts',(-20.1861956033881,36.1672072147257,124.334353335145)) ;
#30779 = CARTESIAN_POINT('Ctrl Pts',(-20.1646550508293,36.3572249527295,124.716351716207)) ;
#30780 = CARTESIAN_POINT('Ctrl Pts',(-20.013585958757,36.1772358723666,124.455438891468)) ;
#30781 = CARTESIAN_POINT('Ctrl Pts',(-19.9294697798766,36.3671092789223,124.82658534845)) ;
#30782 = CARTESIAN_POINT('Ctrl Pts',(-19.8254390212486,36.1871201985594,124.543627316612)) ;
#30783 = CARTESIAN_POINT('Ctrl Pts',(-19.6767994745705,36.3770750224129,124.895495364823)) ;
#30784 = CARTESIAN_POINT('Ctrl Pts',(-19.6233034862338,36.19708594205,124.598757213134)) ;
#30785 = CARTESIAN_POINT('Ctrl Pts',(-19.4143489319624,36.3871034015441,124.91925636217)) ;
#30786 = CARTESIAN_POINT('Ctrl Pts',(-19.4133432160735,36.2071143211812,124.617767958243)) ;
#30787 = CARTESIAN_POINT('Ctrl Pts',(-19.1550206095445,36.397004247751,124.897758003346)) ;
#30788 = CARTESIAN_POINT('Ctrl Pts',(-19.2058807986506,36.2170151673881,124.600571300824)) ;
#30789 = CARTESIAN_POINT('Ctrl Pts',(-18.8994442732755,36.4070629051681,124.830453416065)) ;
#30790 = CARTESIAN_POINT('Ctrl Pts',(-19.0014191286445,36.2270738248052,124.546729537339)) ;
#30791 = CARTESIAN_POINT('Ctrl Pts',(-18.6640416210879,36.41692046795,124.722218749263)) ;
#30792 = CARTESIAN_POINT('Ctrl Pts',(-18.8130966335472,36.2369313875871,124.460143863879)) ;
#30793 = CARTESIAN_POINT('Ctrl Pts',(-18.4464240794683,36.4269888705032,124.571792635111)) ;
#30794 = CARTESIAN_POINT('Ctrl Pts',(-18.6390013333269,36.2469997901403,124.339804589422)) ;
#30795 = CARTESIAN_POINT('Ctrl Pts',(-18.2621870024575,36.4368442692428,124.389737932051)) ;
#30796 = CARTESIAN_POINT('Ctrl Pts',(-18.4916105893428,36.2568551888799,124.194162632583)) ;
#30797 = CARTESIAN_POINT('Ctrl Pts',(-18.1096139658518,36.4468391363167,124.175952224907)) ;
#30798 = CARTESIAN_POINT('Ctrl Pts',(-18.3695504720034,36.2668500559538,124.023135369185)) ;
#30799 = CARTESIAN_POINT('Ctrl Pts',(-17.9965739248701,36.4568704313002,123.937801266144)) ;
#30800 = CARTESIAN_POINT('Ctrl Pts',(-18.2791165693549,36.2768813509373,123.832615491336)) ;
#30801 = CARTESIAN_POINT('Ctrl Pts',(-17.9273507223424,36.4667369560267,123.68792118455)) ;
#30802 = CARTESIAN_POINT('Ctrl Pts',(-18.2237360813941,36.2867478756638,123.632712386933)) ;
#30803 = CARTESIAN_POINT('Ctrl Pts',(-17.9018470654154,36.4767244267224,123.426734881173)) ;
#30804 = CARTESIAN_POINT('Ctrl Pts',(-18.2033310225224,36.2967353463596,123.423763651116)) ;
#30805 = CARTESIAN_POINT('Ctrl Pts',(-17.9218551058738,36.4866691862863,123.166123729046)) ;
#30806 = CARTESIAN_POINT('Ctrl Pts',(-18.2193352864995,36.3066801059234,123.215274750521)) ;
#30807 = CARTESIAN_POINT('Ctrl Pts',(-17.9876098911621,36.4967147422351,122.910487765929)) ;
#30808 = CARTESIAN_POINT('Ctrl Pts',(-18.2719370358106,36.3167256618723,123.010765429301)) ;
#30809 = CARTESIAN_POINT('Ctrl Pts',(-18.0945065089563,36.5065743306102,122.674433491217)) ;
#30810 = CARTESIAN_POINT('Ctrl Pts',(-18.3574522130804,36.3265852502474,122.821921426848)) ;
#30811 = CARTESIAN_POINT('Ctrl Pts',(-18.2424940102238,36.5165752857463,122.457296954355)) ;
#30812 = CARTESIAN_POINT('Ctrl Pts',(-18.4758403558108,36.3365862053834,122.648211013651)) ;
#30813 = CARTESIAN_POINT('Ctrl Pts',(-18.4240741922966,36.5264795130239,122.270772500049)) ;
#30814 = CARTESIAN_POINT('Ctrl Pts',(-18.6211027732019,36.346490432661,122.498990059894)) ;
#30815 = CARTESIAN_POINT('Ctrl Pts',(-18.6381179777294,36.536521589919,122.116476705951)) ;
#30816 = CARTESIAN_POINT('Ctrl Pts',(-18.7923365002083,36.3565325095561,122.375551632485)) ;
#30817 = CARTESIAN_POINT('Ctrl Pts',(-18.8725385168482,36.5464292026052,122.003075302597)) ;
#30818 = CARTESIAN_POINT('Ctrl Pts',(-18.979871801407,36.3664401222423,122.284828592145)) ;
#30819 = CARTESIAN_POINT('Ctrl Pts',(-19.1267156102874,36.5564837332209,121.931052177972)) ;
#30820 = CARTESIAN_POINT('Ctrl Pts',(-19.1832128661274,36.376494652858,122.227207955336)) ;
#30821 = CARTESIAN_POINT('Ctrl Pts',(-19.3845283469667,36.5663445197698,121.904614760594)) ;
#30822 = CARTESIAN_POINT('Ctrl Pts',(-19.3894626144026,36.3863554394069,122.206055828326)) ;
#30823 = CARTESIAN_POINT('Ctrl Pts',(-19.646459660601,36.5763382748409,121.923105823683)) ;
#30824 = CARTESIAN_POINT('Ctrl Pts',(-19.5990077631151,36.396349194478,122.220846431411)) ;
#30825 = CARTESIAN_POINT('Ctrl Pts',(-19.8995693751158,36.5862636350808,121.986256533974)) ;
#30826 = CARTESIAN_POINT('Ctrl Pts',(-19.8014959764349,36.406274554718,122.271364795615)) ;
#30827 = CARTESIAN_POINT('Ctrl Pts',(-20.1402663825485,36.5962915644761,122.093453651258)) ;
#30828 = CARTESIAN_POINT('Ctrl Pts',(-19.9940544515842,36.4163024841132,122.357120413461)) ;
#30829 = CARTESIAN_POINT('Ctrl Pts',(-20.3558196617263,36.6061778312754,122.23855197328)) ;
#30830 = CARTESIAN_POINT('Ctrl Pts',(-20.1664982539507,36.4261887509125,122.473197150911)) ;
#30831 = CARTESIAN_POINT('Ctrl Pts',(-20.5456928031172,36.6162096001737,122.421371062193)) ;
#30832 = CARTESIAN_POINT('Ctrl Pts',(-20.3183982921077,36.4362205198108,122.619450762827)) ;
#30833 = CARTESIAN_POINT('Ctrl Pts',(-20.6988722845905,36.6260911960173,122.631115950227)) ;
#30834 = CARTESIAN_POINT('Ctrl Pts',(-20.4409436684768,36.4461021156544,122.787245289088)) ;
#30835 = CARTESIAN_POINT('Ctrl Pts',(-20.815415738362,36.6361530814852,122.868418182703)) ;
#30836 = CARTESIAN_POINT('Ctrl Pts',(-20.5341804158425,36.4561640011224,122.97708607685)) ;
#30837 = CARTESIAN_POINT('Ctrl Pts',(-20.8875930298801,36.6460105155041,123.11723735423)) ;
#30838 = CARTESIAN_POINT('Ctrl Pts',(-20.5919244479909,36.4660214351412,123.176140562993)) ;
#30839 = CARTESIAN_POINT('Ctrl Pts',(-20.9163988743177,36.6560037585461,123.37823043788)) ;
#30840 = CARTESIAN_POINT('Ctrl Pts',(-20.6149712081136,36.4760146781832,123.384935555596)) ;
#30841 = CARTESIAN_POINT('Ctrl Pts',(-20.8995719078508,36.6659345194324,123.638673612031)) ;
#30842 = CARTESIAN_POINT('Ctrl Pts',(-20.6015124065235,36.4859454390695,123.593287223642)) ;
#30843 = CARTESIAN_POINT('Ctrl Pts',(-20.8168446966216,36.6792835116296,123.979609103864)) ;
#30844 = CARTESIAN_POINT('Ctrl Pts',(-20.535330876497,36.4992944312667,123.866051291918)) ;
#30845 = CARTESIAN_POINT('Ctrl Pts',(-20.6476556408436,36.692551884446,124.288994177467)) ;
#30846 = CARTESIAN_POINT('Ctrl Pts',(-20.3999608846557,36.5125628040832,124.113578703363)) ;
#30847 = CARTESIAN_POINT('Ctrl Pts',(-20.4070652076398,36.7058348258304,124.541941671544)) ;
#30848 = CARTESIAN_POINT('Ctrl Pts',(-20.2075187930554,36.5258457454675,124.31590241707)) ;
#30849 = CARTESIAN_POINT('Ctrl Pts',(-20.1946380684897,36.7158776116726,124.698516250031)) ;
#30850 = CARTESIAN_POINT('Ctrl Pts',(-20.0375727496872,36.5358885313097,124.441171067068)) ;
#30851 = CARTESIAN_POINT('Ctrl Pts',(-19.9628921814832,36.7257275542247,124.813842499232)) ;
#30852 = CARTESIAN_POINT('Ctrl Pts',(-19.8521787603597,36.5457384738618,124.53343231864)) ;
#30853 = CARTESIAN_POINT('Ctrl Pts',(-19.7111366687982,36.7357247871437,124.888900023742)) ;
#30854 = CARTESIAN_POINT('Ctrl Pts',(-19.6507730800588,36.5557357067808,124.593480421543)) ;
#30855 = CARTESIAN_POINT('Ctrl Pts',(-19.4496388355441,36.7457396824782,124.918754107173)) ;
#30856 = CARTESIAN_POINT('Ctrl Pts',(-19.4415808798337,36.5657506021153,124.617367625246)) ;
#30857 = CARTESIAN_POINT('Ctrl Pts',(-19.1023419164485,36.7589793591164,124.897941856105)) ;
#30858 = CARTESIAN_POINT('Ctrl Pts',(-19.163714991499,36.5789902787535,124.600711280948)) ;
#30859 = CARTESIAN_POINT('Ctrl Pts',(-18.6847931249913,36.7755265835217,124.759912521952)) ;
#30860 = CARTESIAN_POINT('Ctrl Pts',(-18.8297169408902,36.5955375031589,124.490312244877)) ;
#30861 = CARTESIAN_POINT('Ctrl Pts',(-18.3371603330514,36.7921740206528,124.486198909286)) ;
#30862 = CARTESIAN_POINT('Ctrl Pts',(-18.5515569759396,36.6121849402899,124.27129948126)) ;
#30863 = CARTESIAN_POINT('Ctrl Pts',(-18.1282776888068,36.805463518131,124.206288377136)) ;
#30864 = CARTESIAN_POINT('Ctrl Pts',(-18.3844875071243,36.6254744377682,124.047410080626)) ;
#30865 = CARTESIAN_POINT('Ctrl Pts',(-18.0108710102114,36.8153369259534,123.974907927257)) ;
#30866 = CARTESIAN_POINT('Ctrl Pts',(-18.2905523869042,36.6353478455905,123.86229865506)) ;
#30867 = CARTESIAN_POINT('Ctrl Pts',(-17.9340138084422,36.8253893035461,123.722181735766)) ;
#30868 = CARTESIAN_POINT('Ctrl Pts',(-18.2290667220401,36.6454002231832,123.660120782758)) ;
#30869 = CARTESIAN_POINT('Ctrl Pts',(-17.9027830695279,36.835292957087,123.463785283055)) ;
#30870 = CARTESIAN_POINT('Ctrl Pts',(-18.2040801107792,36.6553038767241,123.453402008484)) ;
#30871 = CARTESIAN_POINT('Ctrl Pts',(-17.9163185741068,36.8452372260823,123.20284412538)) ;
#30872 = CARTESIAN_POINT('Ctrl Pts',(-18.2149045717325,36.6652481457194,123.244652494399)) ;
#30873 = CARTESIAN_POINT('Ctrl Pts',(-17.9947816309639,36.858568234415,122.86134409118)) ;
#30874 = CARTESIAN_POINT('Ctrl Pts',(-18.2776833949051,36.6785791540521,122.971434015951)) ;
#30875 = CARTESIAN_POINT('Ctrl Pts',(-18.2021201495934,36.8751898149393,122.471324046481)) ;
#30876 = CARTESIAN_POINT('Ctrl Pts',(-18.4435276248863,36.6952007345764,122.65944458022)) ;
#30877 = CARTESIAN_POINT('Ctrl Pts',(-18.5280140338344,36.8917324856377,122.176159129624)) ;
#30878 = CARTESIAN_POINT('Ctrl Pts',(-18.7042903718315,36.7117434052748,122.423272175924)) ;
#30879 = CARTESIAN_POINT('Ctrl Pts',(-18.8400831149496,36.9050816452006,122.015936356967)) ;
#30880 = CARTESIAN_POINT('Ctrl Pts',(-18.9539021452591,36.7250925648377,122.295120890868)) ;
#30881 = CARTESIAN_POINT('Ctrl Pts',(-19.1721122727388,36.9183097953601,121.912858361427)) ;
#30882 = CARTESIAN_POINT('Ctrl Pts',(-19.2195445013812,36.7383207149972,122.212649893044)) ;
#30883 = CARTESIAN_POINT('Ctrl Pts',(-19.6137036972869,36.9349404724976,121.895030598863)) ;
#30884 = CARTESIAN_POINT('Ctrl Pts',(-19.5728023332913,36.7549513921347,122.198387296976)) ;
#30885 = CARTESIAN_POINT('Ctrl Pts',(-20.1178689307979,36.9548434117857,122.055389405996)) ;
#30886 = CARTESIAN_POINT('Ctrl Pts',(-19.9761410205625,36.7748543314228,122.326670629609)) ;
#30887 = CARTESIAN_POINT('Ctrl Pts',(-20.5372508618261,36.974746278389,122.377628584719)) ;
#30888 = CARTESIAN_POINT('Ctrl Pts',(-20.3116476493232,36.7947571980261,122.584460225814)) ;
#30889 = CARTESIAN_POINT('Ctrl Pts',(-20.8224429652518,36.9946594434938,122.823616943194)) ;
#30890 = CARTESIAN_POINT('Ctrl Pts',(-20.5398042577158,36.8146703631309,122.941249965246)) ;
#30891 = CARTESIAN_POINT('Ctrl Pts',(-20.9381837029395,37.0146952726351,123.343330198138)) ;
#30892 = CARTESIAN_POINT('Ctrl Pts',(-20.6323994047383,36.8347061922723,123.357019653058)) ;
#30893 = CARTESIAN_POINT('Ctrl Pts',(-20.870660430698,37.0345138475132,123.865857791706)) ;
#30894 = CARTESIAN_POINT('Ctrl Pts',(-20.5783831490658,36.8545247671503,123.775043510851)) ;
#30895 = CARTESIAN_POINT('Ctrl Pts',(-20.6279168053025,37.0544841485552,124.337676429547)) ;
#30896 = CARTESIAN_POINT('Ctrl Pts',(-20.3841900155139,36.8744950681923,124.152499694084)) ;
#30897 = CARTESIAN_POINT('Ctrl Pts',(-20.2401177850533,37.0743756809197,124.697290350133)) ;
#30898 = CARTESIAN_POINT('Ctrl Pts',(-20.0739513811675,36.8943866005569,124.440192902116)) ;
#30899 = CARTESIAN_POINT('Ctrl Pts',(-19.7497910668488,37.0943987787363,124.90385539926)) ;
#30900 = CARTESIAN_POINT('Ctrl Pts',(-19.6816909775682,36.9144096983734,124.60544662509)) ;
#30901 = CARTESIAN_POINT('Ctrl Pts',(-19.2242516782472,37.1141955316562,124.930779156354)) ;
#30902 = CARTESIAN_POINT('Ctrl Pts',(-19.2612574376801,36.9342064512933,124.626987358956)) ;
#30903 = CARTESIAN_POINT('Ctrl Pts',(-18.7165851062784,37.134156620145,124.77686253658)) ;
#30904 = CARTESIAN_POINT('Ctrl Pts',(-18.8551234525687,36.9541675397821,124.503854730213)) ;
#30905 = CARTESIAN_POINT('Ctrl Pts',(-18.2921431805836,37.1541348890772,124.457730120068)) ;
#30906 = CARTESIAN_POINT('Ctrl Pts',(-18.5155690830116,36.9741458087143,124.24854960687)) ;
#30907 = CARTESIAN_POINT('Ctrl Pts',(-18.0037890981737,37.1739549038682,124.016935959716)) ;
#30908 = CARTESIAN_POINT('Ctrl Pts',(-18.2848840606162,36.9939658235053,123.89591275192)) ;
#30909 = CARTESIAN_POINT('Ctrl Pts',(-17.8810922820256,37.19389331312,123.50137832524)) ;
#30910 = CARTESIAN_POINT('Ctrl Pts',(-18.1867266714987,37.0139042327571,123.483465809288)) ;
#30911 = CARTESIAN_POINT('Ctrl Pts',(-17.9432206011059,37.2139404305124,122.97212475137)) ;
#30912 = CARTESIAN_POINT('Ctrl Pts',(-18.2364291043745,37.0339513501496,123.06006363056)) ;
#30913 = CARTESIAN_POINT('Ctrl Pts',(-18.1799938362226,37.2337866763463,122.500836491877)) ;
#30914 = CARTESIAN_POINT('Ctrl Pts',(-18.4258485917207,37.0537975959834,122.683031144881)) ;
#30915 = CARTESIAN_POINT('Ctrl Pts',(-18.5620635941251,37.2536356448583,122.137020325925)) ;
#30916 = CARTESIAN_POINT('Ctrl Pts',(-18.7315064596815,37.0736465644954,122.391977845995)) ;
#30917 = CARTESIAN_POINT('Ctrl Pts',(-19.0504528465872,37.2736859471696,121.923931865139)) ;
#30918 = CARTESIAN_POINT('Ctrl Pts',(-19.1222177233639,37.0936968668067,122.221508236812)) ;
#30919 = CARTESIAN_POINT('Ctrl Pts',(-19.5767155011093,37.2935208696008,121.890757346003)) ;
#30920 = CARTESIAN_POINT('Ctrl Pts',(-19.5432297263916,37.113531789238,122.194969649968)) ;
#30921 = CARTESIAN_POINT('Ctrl Pts',(-20.08511494409,37.3134512708267,122.038788804448)) ;
#30922 = CARTESIAN_POINT('Ctrl Pts',(-19.9499495172448,37.1334621904638,122.313396725135)) ;
#30923 = CARTESIAN_POINT('Ctrl Pts',(-20.5122328950149,37.3333362161856,122.35040788788)) ;
#30924 = CARTESIAN_POINT('Ctrl Pts',(-20.2916434333738,37.1533471358227,122.562694298399)) ;
#30925 = CARTESIAN_POINT('Ctrl Pts',(-20.8092661802658,37.353408824337,122.793446550335)) ;
#30926 = CARTESIAN_POINT('Ctrl Pts',(-20.5292680326244,37.1734197439741,122.917125764005)) ;
#30927 = CARTESIAN_POINT('Ctrl Pts',(-20.9356180404718,37.3732001406651,123.304147384377)) ;
#30928 = CARTESIAN_POINT('Ctrl Pts',(-20.6303478832511,37.1932110603022,123.325688757585)) ;
#30929 = CARTESIAN_POINT('Ctrl Pts',(-20.8812658706226,37.3931649304323,123.8319433124)) ;
#30930 = CARTESIAN_POINT('Ctrl Pts',(-20.5868633031295,37.2131758500695,123.747925458238)) ;
#30931 = CARTESIAN_POINT('Ctrl Pts',(-20.6486375255731,37.4131478861826,124.309410738548)) ;
#30932 = CARTESIAN_POINT('Ctrl Pts',(-20.4007582836289,37.2331588058198,124.129898402551)) ;
#30933 = CARTESIAN_POINT('Ctrl Pts',(-20.2710983170399,37.4329564081588,124.676413569009)) ;
#30934 = CARTESIAN_POINT('Ctrl Pts',(-20.0987238439308,37.2529673277959,124.423499492388)) ;
#30935 = CARTESIAN_POINT('Ctrl Pts',(-19.7870846025984,37.4529419828946,124.894968051368)) ;
#30936 = CARTESIAN_POINT('Ctrl Pts',(-19.7115114515686,37.2729529025317,124.598340127017)) ;
#30937 = CARTESIAN_POINT('Ctrl Pts',(-19.2600251516879,37.472824622963,124.934935958172)) ;
#30938 = CARTESIAN_POINT('Ctrl Pts',(-19.2898629599609,37.2928355426001,124.630311187914)) ;
#30939 = CARTESIAN_POINT('Ctrl Pts',(-18.7492134555832,37.4927799350949,124.792594096249)) ;
#30940 = CARTESIAN_POINT('Ctrl Pts',(-18.8812143169606,37.312790854732,124.516434239319)) ;
#30941 = CARTESIAN_POINT('Ctrl Pts',(-18.319033254551,37.5126542917027,124.485894779788)) ;
#30942 = CARTESIAN_POINT('Ctrl Pts',(-18.5370718339478,37.3326652113398,124.27107140888)) ;
#30943 = CARTESIAN_POINT('Ctrl Pts',(-18.0175106060064,37.5326364985638,124.048765115388)) ;
#30944 = CARTESIAN_POINT('Ctrl Pts',(-18.2958567266438,37.3526474182009,123.921365577981)) ;
#30945 = CARTESIAN_POINT('Ctrl Pts',(-17.8838308617942,37.5525675765137,123.536059048149)) ;
#30946 = CARTESIAN_POINT('Ctrl Pts',(-18.1889170443655,37.3725784961509,123.5111991052)) ;
#30947 = CARTESIAN_POINT('Ctrl Pts',(-17.9330320754365,37.5724945513687,123.008830582015)) ;
#30948 = CARTESIAN_POINT('Ctrl Pts',(-18.2282802580598,37.3925054710058,123.089417886411)) ;
#30949 = CARTESIAN_POINT('Ctrl Pts',(-18.157254622848,37.5923270103176,122.531709623646)) ;
#30950 = CARTESIAN_POINT('Ctrl Pts',(-18.4076687041876,37.4123379299547,122.707716901662)) ;
#30951 = CARTESIAN_POINT('Ctrl Pts',(-18.4706659458096,37.6089846944928,122.219158784054)) ;
#30952 = CARTESIAN_POINT('Ctrl Pts',(-18.658380296989,37.4289956141299,122.457695891381)) ;
#30953 = CARTESIAN_POINT('Ctrl Pts',(-18.7724796762074,37.6222339183999,122.045392670349)) ;
#30954 = CARTESIAN_POINT('Ctrl Pts',(-18.8998510804845,37.442244838037,122.318670265349)) ;
#30955 = CARTESIAN_POINT('Ctrl Pts',(-19.0206690089167,37.6322829398511,121.955269929733)) ;
#30956 = CARTESIAN_POINT('Ctrl Pts',(-19.0983967704762,37.4522938594882,122.246576695617)) ;
#30957 = CARTESIAN_POINT('Ctrl Pts',(-19.2758657649021,37.6421429480816,121.910397904174)) ;
#30958 = CARTESIAN_POINT('Ctrl Pts',(-19.3025665790804,37.4621538677187,122.210682152963)) ;
#30959 = CARTESIAN_POINT('Ctrl Pts',(-19.6249794284296,37.6554264613062,121.909413584284)) ;
#30960 = CARTESIAN_POINT('Ctrl Pts',(-19.5818035064809,37.4754373809433,122.20988869481)) ;
#30961 = CARTESIAN_POINT('Ctrl Pts',(-20.0524638778648,37.672072380307,122.023188295616)) ;
#30962 = CARTESIAN_POINT('Ctrl Pts',(-19.9238581002366,37.4920832999442,122.300927565958)) ;
#30963 = CARTESIAN_POINT('Ctrl Pts',(-20.413880776944,37.6886263581231,122.274169668414)) ;
#30964 = CARTESIAN_POINT('Ctrl Pts',(-20.2129442060005,37.5086372777602,122.501691816295)) ;
#30965 = CARTESIAN_POINT('Ctrl Pts',(-20.6406243713132,37.7019860870947,122.542201540504)) ;
#30966 = CARTESIAN_POINT('Ctrl Pts',(-20.3943637147157,37.5219970067318,122.716138256514)) ;
#30967 = CARTESIAN_POINT('Ctrl Pts',(-20.771703979078,37.7118791388914,122.766737576687)) ;
#30968 = CARTESIAN_POINT('Ctrl Pts',(-20.4992200975137,37.5318900585285,122.895764440336)) ;
#30969 = CARTESIAN_POINT('Ctrl Pts',(-20.8630031282262,37.7218691041725,123.012844193469)) ;
#30970 = CARTESIAN_POINT('Ctrl Pts',(-20.5722587448008,37.5418800238096,123.092651501254)) ;
#30971 = CARTESIAN_POINT('Ctrl Pts',(-20.9101691765086,37.7318209850333,123.270122215449)) ;
#30972 = CARTESIAN_POINT('Ctrl Pts',(-20.609988980369,37.5518319046704,123.298474032624)) ;
#30973 = CARTESIAN_POINT('Ctrl Pts',(-20.9117400295103,37.7418693367251,123.534149528085)) ;
#30974 = CARTESIAN_POINT('Ctrl Pts',(-20.6112435209441,37.5618802563622,123.509695891286)) ;
#30975 = CARTESIAN_POINT('Ctrl Pts',(-20.8686496157947,37.7517106208313,123.789179451331)) ;
#30976 = CARTESIAN_POINT('Ctrl Pts',(-20.576768936994,37.5717215404684,123.713719468987)) ;
#30977 = CARTESIAN_POINT('Ctrl Pts',(-20.7811945958756,37.761697323957,124.0365703206)) ;
#30978 = CARTESIAN_POINT('Ctrl Pts',(-20.5068028158722,37.5817082435941,123.911631353683)) ;
#30979 = CARTESIAN_POINT('Ctrl Pts',(-20.6528738763807,37.7716323527744,124.263999794878)) ;
#30980 = CARTESIAN_POINT('Ctrl Pts',(-20.4041443030014,37.5916432724115,124.093573772257)) ;
#30981 = CARTESIAN_POINT('Ctrl Pts',(-20.4848851322175,37.7816881476813,124.467934944113)) ;
#30982 = CARTESIAN_POINT('Ctrl Pts',(-20.2697515895762,37.6016990673184,124.256720420404)) ;
#30983 = CARTESIAN_POINT('Ctrl Pts',(-20.2887835292672,37.7915165109706,124.636074676787)) ;
#30984 = CARTESIAN_POINT('Ctrl Pts',(-20.1128689225267,37.6115274306077,124.391230423038)) ;
#30985 = CARTESIAN_POINT('Ctrl Pts',(-20.0614584855971,37.8015774808685,124.771009318032)) ;
#30986 = CARTESIAN_POINT('Ctrl Pts',(-19.931007771351,37.6215884005056,124.49917617883)) ;
#30987 = CARTESIAN_POINT('Ctrl Pts',(-19.8176275658583,37.8114917597583,124.862882128275)) ;
#30988 = CARTESIAN_POINT('Ctrl Pts',(-19.735942339562,37.6315026793954,124.572672280903)) ;
#30989 = CARTESIAN_POINT('Ctrl Pts',(-19.5592226441299,37.8215007542265,124.911986102219)) ;
#30990 = CARTESIAN_POINT('Ctrl Pts',(-19.5292180435957,37.6415116738637,124.611953245993)) ;
#30991 = CARTESIAN_POINT('Ctrl Pts',(-19.2956698137528,37.8315305887903,124.914944725245)) ;
#30992 = CARTESIAN_POINT('Ctrl Pts',(-19.3183757846655,37.6515415084274,124.614317886194)) ;
#30993 = CARTESIAN_POINT('Ctrl Pts',(-19.0399553923332,37.8413888188625,124.873312424771)) ;
#30994 = CARTESIAN_POINT('Ctrl Pts',(-19.113804794043,37.6613997384997,124.581009863178)) ;
#30995 = CARTESIAN_POINT('Ctrl Pts',(-18.7918216048471,37.8513875246049,124.787014243601)) ;
#30996 = CARTESIAN_POINT('Ctrl Pts',(-18.915298566103,37.6713984442421,124.511969231989)) ;
#30997 = CARTESIAN_POINT('Ctrl Pts',(-18.5645984860679,37.8612821805237,124.660501733372)) ;
#30998 = CARTESIAN_POINT('Ctrl Pts',(-18.7335213311777,37.6812931001609,124.410757393858)) ;
#30999 = CARTESIAN_POINT('Ctrl Pts',(-18.3594834848053,37.8713452449077,124.493660346681)) ;
#31000 = CARTESIAN_POINT('Ctrl Pts',(-18.5694307097895,37.6913561645448,124.277282542542)) ;
#31001 = CARTESIAN_POINT('Ctrl Pts',(-18.1900212161876,37.8811849031876,124.298298757576)) ;
#31002 = CARTESIAN_POINT('Ctrl Pts',(-18.4338627738789,37.7011958228247,124.120992079632)) ;
#31003 = CARTESIAN_POINT('Ctrl Pts',(-18.0537869453756,37.8912480702694,124.071683477115)) ;
#31004 = CARTESIAN_POINT('Ctrl Pts',(-18.3248772081804,37.7112589899066,123.939698699603)) ;
#31005 = CARTESIAN_POINT('Ctrl Pts',(-17.9607436771395,37.9011423153965,123.828859729569)) ;
#31006 = CARTESIAN_POINT('Ctrl Pts',(-18.2504447386895,37.7211532350337,123.745439163456)) ;
#31007 = CARTESIAN_POINT('Ctrl Pts',(-17.9103527062584,37.9110841370011,123.572537760102)) ;
#31008 = CARTESIAN_POINT('Ctrl Pts',(-18.2101341056503,37.7310950566383,123.540381382668)) ;
#31009 = CARTESIAN_POINT('Ctrl Pts',(-17.9051034699468,37.9210866679192,123.309699103469)) ;
#31010 = CARTESIAN_POINT('Ctrl Pts',(-18.2059368477175,37.7410975875563,123.330110481641)) ;
#31011 = CARTESIAN_POINT('Ctrl Pts',(-17.946097783474,37.9311212943767,123.049219622139)) ;
#31012 = CARTESIAN_POINT('Ctrl Pts',(-18.238734443196,37.7511322140138,123.121727220956)) ;
#31013 = CARTESIAN_POINT('Ctrl Pts',(-18.0297012300919,37.9409668293631,122.804359246479)) ;
#31014 = CARTESIAN_POINT('Ctrl Pts',(-18.3056190713924,37.7609777490003,122.925840036189)) ;
#31015 = CARTESIAN_POINT('Ctrl Pts',(-18.1557855280744,37.9509502542022,122.574313582137)) ;
#31016 = CARTESIAN_POINT('Ctrl Pts',(-18.4064882631411,37.7709611738393,122.741804625682)) ;
#31017 = CARTESIAN_POINT('Ctrl Pts',(-18.3194140988036,37.9609006445672,122.370342409505)) ;
#31018 = CARTESIAN_POINT('Ctrl Pts',(-18.5373926050169,37.7809115642044,122.578629156935)) ;
#31019 = CARTESIAN_POINT('Ctrl Pts',(-18.5166838775539,37.9708982848643,122.196785487703)) ;
#31020 = CARTESIAN_POINT('Ctrl Pts',(-18.6952097128482,37.7909092045014,122.439785207195)) ;
#31021 = CARTESIAN_POINT('Ctrl Pts',(-18.7422660732146,37.9809373654275,122.060023983283)) ;
#31022 = CARTESIAN_POINT('Ctrl Pts',(-18.8756765999443,37.8009482850646,122.330377774988)) ;
#31023 = CARTESIAN_POINT('Ctrl Pts',(-18.9827700674646,37.9907635161966,121.965984935098)) ;
#31024 = CARTESIAN_POINT('Ctrl Pts',(-19.068079960445,37.8107744358337,122.255148655797)) ;
#31025 = CARTESIAN_POINT('Ctrl Pts',(-19.2417735141306,38.0008200911257,121.913534414804)) ;
#31026 = CARTESIAN_POINT('Ctrl Pts',(-19.2752831961908,37.8208310107629,122.213190167423)) ;
#31027 = CARTESIAN_POINT('Ctrl Pts',(-19.5029368385389,38.010760630506,121.907384733562)) ;
#31028 = CARTESIAN_POINT('Ctrl Pts',(-19.4842136365279,37.8307715501431,122.20827246862)) ;
#31029 = CARTESIAN_POINT('Ctrl Pts',(-19.7603796758828,38.0206650234824,121.94572645087)) ;
#31030 = CARTESIAN_POINT('Ctrl Pts',(-19.6901671990176,37.8406759431195,122.238947693233)) ;
#31031 = CARTESIAN_POINT('Ctrl Pts',(-20.0107210558662,38.0307116776873,122.029521129623)) ;
#31032 = CARTESIAN_POINT('Ctrl Pts',(-19.8904397605092,37.8507225973244,122.305985318718)) ;
#31033 = CARTESIAN_POINT('Ctrl Pts',(-20.2393912303446,38.0406072396257,122.153437722029)) ;
#31034 = CARTESIAN_POINT('Ctrl Pts',(-20.0733745736591,37.8606181592628,122.405120060761)) ;
#31035 = CARTESIAN_POINT('Ctrl Pts',(-20.4464358604614,38.0506693174713,122.317848314889)) ;
#31036 = CARTESIAN_POINT('Ctrl Pts',(-20.2390091946635,37.8706802371084,122.536650134307)) ;
#31037 = CARTESIAN_POINT('Ctrl Pts',(-20.6181207395519,38.060512015885,122.511348876402)) ;
#31038 = CARTESIAN_POINT('Ctrl Pts',(-20.3763552143861,37.8805229355222,122.691451327068)) ;
#31039 = CARTESIAN_POINT('Ctrl Pts',(-20.7561325943481,38.0705027908465,122.734655821582)) ;
#31040 = CARTESIAN_POINT('Ctrl Pts',(-20.4867630838622,37.8905137104836,122.870097716257)) ;
#31041 = CARTESIAN_POINT('Ctrl Pts',(-20.8526444302202,38.0804306558656,122.977057792993)) ;
#31042 = CARTESIAN_POINT('Ctrl Pts',(-20.5639707221755,37.9004415755027,123.064019601063)) ;
#31043 = CARTESIAN_POINT('Ctrl Pts',(-20.9063538531691,38.0904194006318,123.234003272381)) ;
#31044 = CARTESIAN_POINT('Ctrl Pts',(-20.6069365241512,37.9104303202689,123.269576200659)) ;
#31045 = CARTESIAN_POINT('Ctrl Pts',(-20.9142822162603,38.1004521862187,123.497539173054)) ;
#31046 = CARTESIAN_POINT('Ctrl Pts',(-20.6132774084487,37.9204631058559,123.480405034982)) ;
#31047 = CARTESIAN_POINT('Ctrl Pts',(-20.8772223147212,38.1103188708394,123.754154223928)) ;
#31048 = CARTESIAN_POINT('Ctrl Pts',(-20.5836278397377,37.9303297904765,123.685696137519)) ;
#31049 = CARTESIAN_POINT('Ctrl Pts',(-20.7960987290107,38.1202807630025,124.00306041153)) ;
#31050 = CARTESIAN_POINT('Ctrl Pts',(-20.5187275050565,37.9402916826396,123.884820316478)) ;
#31051 = CARTESIAN_POINT('Ctrl Pts',(-20.6717436692743,38.1303142399151,124.235550043403)) ;
#31052 = CARTESIAN_POINT('Ctrl Pts',(-20.4192419168591,37.9503251595522,124.070811279402)) ;
#31053 = CARTESIAN_POINT('Ctrl Pts',(-20.5116269403932,38.1401985811634,124.440122137364)) ;
#31054 = CARTESIAN_POINT('Ctrl Pts',(-20.291147641117,37.9602095008005,124.2344674478)) ;
#31055 = CARTESIAN_POINT('Ctrl Pts',(-20.3149827227567,38.1502615232845,124.616881340023)) ;
#31056 = CARTESIAN_POINT('Ctrl Pts',(-20.1338310207247,37.9702724429217,124.37587373082)) ;
#31057 = CARTESIAN_POINT('Ctrl Pts',(-20.0953938752767,38.1601119249041,124.75399118927)) ;
#31058 = CARTESIAN_POINT('Ctrl Pts',(-19.9581597997883,37.9801228445412,124.48555979968)) ;
#31059 = CARTESIAN_POINT('Ctrl Pts',(-19.8513087068426,38.1701388136938,124.853234002042)) ;
#31060 = CARTESIAN_POINT('Ctrl Pts',(-19.7628910767466,37.9901497333309,124.564952686841)) ;
#31061 = CARTESIAN_POINT('Ctrl Pts',(-19.593491376287,38.18016742865,124.907926696643)) ;
#31062 = CARTESIAN_POINT('Ctrl Pts',(-19.5566368221853,38.0001783482871,124.60870527169)) ;
#31063 = CARTESIAN_POINT('Ctrl Pts',(-19.3349545228551,38.19001265177,124.917345289566)) ;
#31064 = CARTESIAN_POINT('Ctrl Pts',(-19.3498081794795,38.0100235714072,124.616238591865)) ;
#31065 = CARTESIAN_POINT('Ctrl Pts',(-19.0748065717966,38.200003335576,124.88189910921)) ;
#31066 = CARTESIAN_POINT('Ctrl Pts',(-19.1416901604654,38.0200142552131,124.587880298934)) ;
#31067 = CARTESIAN_POINT('Ctrl Pts',(-18.8237728136893,38.2100412176484,124.80088615643)) ;
#31068 = CARTESIAN_POINT('Ctrl Pts',(-18.9408635131046,38.0300521372856,124.52306847567)) ;
#31069 = CARTESIAN_POINT('Ctrl Pts',(-18.5948907896328,38.2198855772873,124.680287851483)) ;
#31070 = CARTESIAN_POINT('Ctrl Pts',(-18.7577593811284,38.0398964969244,124.426589023562)) ;
#31071 = CARTESIAN_POINT('Ctrl Pts',(-18.3872272286847,38.229870447902,124.519955106578)) ;
#31072 = CARTESIAN_POINT('Ctrl Pts',(-18.5916294861403,38.0498813675391,124.298321919019)) ;
#31073 = CARTESIAN_POINT('Ctrl Pts',(-18.2112252563883,38.2398097312307,124.326911572828)) ;
#31074 = CARTESIAN_POINT('Ctrl Pts',(-18.4508291441772,38.0598206508678,124.143886556018)) ;
#31075 = CARTESIAN_POINT('Ctrl Pts',(-18.0700954992362,38.2498503406038,124.104002776353)) ;
#31076 = CARTESIAN_POINT('Ctrl Pts',(-18.3379263671355,38.0698612602409,123.9655587244)) ;
#31077 = CARTESIAN_POINT('Ctrl Pts',(-17.9711690914586,38.259735191517,123.863780801288)) ;
#31078 = CARTESIAN_POINT('Ctrl Pts',(-18.2587866856612,38.0797461111542,123.773381363225)) ;
#31079 = CARTESIAN_POINT('Ctrl Pts',(-17.9145022539865,38.2697371476858,123.607161518794)) ;
#31080 = CARTESIAN_POINT('Ctrl Pts',(-18.2134543961033,38.089748067323,123.568085793676)) ;
#31081 = CARTESIAN_POINT('Ctrl Pts',(-17.9031351939843,38.2796557444063,123.34671741945)) ;
#31082 = CARTESIAN_POINT('Ctrl Pts',(-18.2043619071338,38.0996666640434,123.359731038019)) ;
#31083 = CARTESIAN_POINT('Ctrl Pts',(-17.9376431227796,38.2897025664821,123.084999919376)) ;
#31084 = CARTESIAN_POINT('Ctrl Pts',(-18.2319694141101,38.1097134861192,123.150357019419)) ;
#31085 = CARTESIAN_POINT('Ctrl Pts',(-18.0154975116536,38.2995768475948,122.837421943665)) ;
#31086 = CARTESIAN_POINT('Ctrl Pts',(-18.2942537162335,38.1195877672319,122.95229576589)) ;
#31087 = CARTESIAN_POINT('Ctrl Pts',(-18.1371535108144,38.3096310476394,122.602934129142)) ;
#31088 = CARTESIAN_POINT('Ctrl Pts',(-18.391579553754,38.1296419672765,122.764705818433)) ;
#31089 = CARTESIAN_POINT('Ctrl Pts',(-18.2951140075871,38.3195264772746,122.396304412918)) ;
#31090 = CARTESIAN_POINT('Ctrl Pts',(-18.5179483256354,38.1395373969118,122.599403261707)) ;
#31091 = CARTESIAN_POINT('Ctrl Pts',(-18.489664634007,38.329588105592,122.217293421697)) ;
#31092 = CARTESIAN_POINT('Ctrl Pts',(-18.6735897116982,38.1495990252291,122.456195042217)) ;
#31093 = CARTESIAN_POINT('Ctrl Pts',(-18.7075571482892,38.3394327344219,122.077804596519)) ;
#31094 = CARTESIAN_POINT('Ctrl Pts',(-18.8479033795345,38.159443654059,122.344605407475)) ;
#31095 = CARTESIAN_POINT('Ctrl Pts',(-18.9487829946581,38.3493927820275,121.976237815657)) ;
#31096 = CARTESIAN_POINT('Ctrl Pts',(-19.0408840272685,38.1694037016646,122.26335285546)) ;
#31097 = CARTESIAN_POINT('Ctrl Pts',(-19.2060908983608,38.3594310882016,121.918149353435)) ;
#31098 = CARTESIAN_POINT('Ctrl Pts',(-19.2467306787397,38.1794420078387,122.216882950581)) ;
#31099 = CARTESIAN_POINT('Ctrl Pts',(-19.4652741750424,38.3693043876342,121.905324657195)) ;
#31100 = CARTESIAN_POINT('Ctrl Pts',(-19.4540764400432,38.1893153072714,122.206624032452)) ;
#31101 = CARTESIAN_POINT('Ctrl Pts',(-19.7278563927704,38.3793776492205,121.938426707961)) ;
#31102 = CARTESIAN_POINT('Ctrl Pts',(-19.6641424513348,38.1993885688576,122.233106527423)) ;
#31103 = CARTESIAN_POINT('Ctrl Pts',(-19.9745595742938,38.3891978751772,122.014360134831)) ;
#31104 = CARTESIAN_POINT('Ctrl Pts',(-19.8615035911148,38.2092087948143,122.293853602793)) ;
#31105 = CARTESIAN_POINT('Ctrl Pts',(-20.2103785146625,38.3992769391167,122.134809378916)) ;
#31106 = CARTESIAN_POINT('Ctrl Pts',(-20.0501587726125,38.2192878587538,122.390213775036)) ;
#31107 = CARTESIAN_POINT('Ctrl Pts',(-20.4170842341087,38.4091270291365,122.29073495999)) ;
#31108 = CARTESIAN_POINT('Ctrl Pts',(-20.2155221090438,38.2291379487737,122.514954115043)) ;
#31109 = CARTESIAN_POINT('Ctrl Pts',(-20.5976790049717,38.4192057827503,122.484385049267)) ;
#31110 = CARTESIAN_POINT('Ctrl Pts',(-20.359997738072,38.2392167023874,122.669874889421)) ;
#31111 = CARTESIAN_POINT('Ctrl Pts',(-20.7384592821363,38.4290272500098,122.700777392782)) ;
#31112 = CARTESIAN_POINT('Ctrl Pts',(-20.4726207917741,38.2490381696469,122.842988001983)) ;
#31113 = CARTESIAN_POINT('Ctrl Pts',(-20.8423676549778,38.4390928483674,122.943961403778)) ;
#31114 = CARTESIAN_POINT('Ctrl Pts',(-20.5557471819317,38.2591037680045,123.037535670951)) ;
#31115 = CARTESIAN_POINT('Ctrl Pts',(-20.9014598751906,38.4489955041421,123.197461404665)) ;
#31116 = CARTESIAN_POINT('Ctrl Pts',(-20.6030203204311,38.2690064237792,123.240335071546)) ;
#31117 = CARTESIAN_POINT('Ctrl Pts',(-20.9159258761711,38.4590463299717,123.461136272486)) ;
#31118 = CARTESIAN_POINT('Ctrl Pts',(-20.6145926705631,38.2790572496089,123.451275207691)) ;
#31119 = CARTESIAN_POINT('Ctrl Pts',(-20.8851806308957,38.4689205343106,123.718849938155)) ;
#31120 = CARTESIAN_POINT('Ctrl Pts',(-20.5899961850183,38.2889314539477,123.657445168674)) ;
#31121 = CARTESIAN_POINT('Ctrl Pts',(-20.808697747039,38.4789929843497,123.972194060034)) ;
#31122 = CARTESIAN_POINT('Ctrl Pts',(-20.5288093967578,38.2990039039868,123.860120677196)) ;
#31123 = CARTESIAN_POINT('Ctrl Pts',(-20.6924452330028,38.4888220011232,124.202906653744)) ;
#31124 = CARTESIAN_POINT('Ctrl Pts',(-20.4358076437675,38.3088329207603,124.044689498754)) ;
#31125 = CARTESIAN_POINT('Ctrl Pts',(-20.5345088117265,38.498888847038,124.415079071641)) ;
#31126 = CARTESIAN_POINT('Ctrl Pts',(-20.3094581203434,38.3188997666751,124.214427542869)) ;
#31127 = CARTESIAN_POINT('Ctrl Pts',(-20.3453362910282,38.5087790183398,124.593350718177)) ;
#31128 = CARTESIAN_POINT('Ctrl Pts',(-20.1581205171573,38.3287899379769,124.35704407548)) ;
#31129 = CARTESIAN_POINT('Ctrl Pts',(-20.1262004053155,38.5187712119636,124.737995435515)) ;
#31130 = CARTESIAN_POINT('Ctrl Pts',(-19.9828118735316,38.3387821316008,124.472759636862)) ;
#31131 = CARTESIAN_POINT('Ctrl Pts',(-19.8858793197356,38.5287340225871,124.841862120209)) ;
#31132 = CARTESIAN_POINT('Ctrl Pts',(-19.7905552583215,38.3487449422242,124.55585265074)) ;
#31133 = CARTESIAN_POINT('Ctrl Pts',(-19.6327966736522,38.5386382954305,124.9027167446)) ;
#31134 = CARTESIAN_POINT('Ctrl Pts',(-19.5880898637253,38.3586492150676,124.604536139099)) ;
#31135 = CARTESIAN_POINT('Ctrl Pts',(-19.3689353661875,38.5486987872351,124.918722771456)) ;
#31136 = CARTESIAN_POINT('Ctrl Pts',(-19.3770005294909,38.3687097068723,124.617340882227)) ;
#31137 = CARTESIAN_POINT('Ctrl Pts',(-19.1119433120646,38.5585391189074,124.8896559552)) ;
#31138 = CARTESIAN_POINT('Ctrl Pts',(-19.1714080569819,38.3785500385446,124.594087552618)) ;
#31139 = CARTESIAN_POINT('Ctrl Pts',(-18.858267179598,38.5686021649992,124.815076395297)) ;
#31140 = CARTESIAN_POINT('Ctrl Pts',(-18.9684668438895,38.3886130846363,124.534423889178)) ;
#31141 = CARTESIAN_POINT('Ctrl Pts',(-18.6254129262552,38.5784962206943,124.699336919331)) ;
#31142 = CARTESIAN_POINT('Ctrl Pts',(-18.782184165847,38.3985071403314,124.441832684119)) ;
#31143 = CARTESIAN_POINT('Ctrl Pts',(-18.4147842988255,38.5884389210173,124.544774213898)) ;
#31144 = CARTESIAN_POINT('Ctrl Pts',(-18.6136815630311,38.4084498406544,124.318182986908)) ;
#31145 = CARTESIAN_POINT('Ctrl Pts',(-18.2329705623296,38.5984446619449,124.354785151136)) ;
#31146 = CARTESIAN_POINT('Ctrl Pts',(-18.4682304676226,38.418455581582,124.166191932299)) ;
#31147 = CARTESIAN_POINT('Ctrl Pts',(-18.086951476104,38.6084655724604,124.135644682199)) ;
#31148 = CARTESIAN_POINT('Ctrl Pts',(-18.3514150709044,38.4284764920975,123.990879603999)) ;
#31149 = CARTESIAN_POINT('Ctrl Pts',(-17.9822934308915,38.6183563079104,123.897719206915)) ;
#31150 = CARTESIAN_POINT('Ctrl Pts',(-18.2676887771091,38.4383672275475,123.800540072914)) ;
#31151 = CARTESIAN_POINT('Ctrl Pts',(-17.9195346698227,38.6283478486392,123.642773296593)) ;
#31152 = CARTESIAN_POINT('Ctrl Pts',(-18.2174815116301,38.4483587682763,123.596583584727)) ;
#31153 = CARTESIAN_POINT('Ctrl Pts',(-17.9021467020347,38.6382957090609,123.381934725884)) ;
#31154 = CARTESIAN_POINT('Ctrl Pts',(-18.2035708827029,38.458306628698,123.387913220143)) ;
#31155 = CARTESIAN_POINT('Ctrl Pts',(-17.9297985346469,38.6482423782472,123.121998548221)) ;
#31156 = CARTESIAN_POINT('Ctrl Pts',(-18.225691882754,38.4682532978843,123.179964691049)) ;
#31157 = CARTESIAN_POINT('Ctrl Pts',(-18.0031723206151,38.6582904543828,122.868354913034)) ;
#31158 = CARTESIAN_POINT('Ctrl Pts',(-18.2843906358415,38.4783013740199,122.977049494518)) ;
#31159 = CARTESIAN_POINT('Ctrl Pts',(-18.1169630845849,38.6681380523884,122.635927730738)) ;
#31160 = CARTESIAN_POINT('Ctrl Pts',(-18.3754223953298,38.4881489720256,122.791108578199)) ;
#31161 = CARTESIAN_POINT('Ctrl Pts',(-18.2704754939803,38.6780997754729,122.423894509235)) ;
#31162 = CARTESIAN_POINT('Ctrl Pts',(-18.498231618631,38.49811069511,122.621481940386)) ;
#31163 = CARTESIAN_POINT('Ctrl Pts',(-18.459987920288,38.6881284105559,122.240733703719)) ;
#31164 = CARTESIAN_POINT('Ctrl Pts',(-18.6498412530283,38.508139330193,122.474952867454)) ;
#31165 = CARTESIAN_POINT('Ctrl Pts',(-18.6757765964958,38.6980387188739,122.094945578105)) ;
#31166 = CARTESIAN_POINT('Ctrl Pts',(-18.822471309607,38.5180496385111,122.358322309801)) ;
#31167 = CARTESIAN_POINT('Ctrl Pts',(-18.9139298646634,38.7079736160098,121.987944654687)) ;
#31168 = CARTESIAN_POINT('Ctrl Pts',(-19.0129931507068,38.5279845356469,122.272721138619)) ;
#31169 = CARTESIAN_POINT('Ctrl Pts',(-19.1697940908906,38.7180146989524,121.92347677505)) ;
#31170 = CARTESIAN_POINT('Ctrl Pts',(-19.2176845178362,38.5380256185895,122.221146167551)) ;
#31171 = CARTESIAN_POINT('Ctrl Pts',(-19.4289447281885,38.7279020417806,121.904527054462)) ;
#31172 = CARTESIAN_POINT('Ctrl Pts',(-19.4250041481742,38.5479129614178,122.20598575918)) ;
#31173 = CARTESIAN_POINT('Ctrl Pts',(-19.6901903067169,38.73789355672,121.930687744959)) ;
#31174 = CARTESIAN_POINT('Ctrl Pts',(-19.634000528053,38.5579044763571,122.226913496927)) ;
#31175 = CARTESIAN_POINT('Ctrl Pts',(-19.9419001392369,38.7478449479164,122.001637581168)) ;
#31176 = CARTESIAN_POINT('Ctrl Pts',(-19.8353681920912,38.5678558675536,122.283672501495)) ;
#31177 = CARTESIAN_POINT('Ctrl Pts',(-20.1772104092053,38.7577774812491,122.114589337141)) ;
#31178 = CARTESIAN_POINT('Ctrl Pts',(-20.0236163134936,38.5777884008862,122.374032878613)) ;
#31179 = CARTESIAN_POINT('Ctrl Pts',(-20.3907677132585,38.7677746391485,122.267583026891)) ;
#31180 = CARTESIAN_POINT('Ctrl Pts',(-20.1944625857522,38.5877855587856,122.496427023054)) ;
#31181 = CARTESIAN_POINT('Ctrl Pts',(-20.5743995160923,38.777759649312,122.455072551218)) ;
#31182 = CARTESIAN_POINT('Ctrl Pts',(-20.3413685642757,38.5977705689491,122.646417859673)) ;
#31183 = CARTESIAN_POINT('Ctrl Pts',(-20.7231828307075,38.7878024758818,122.673007430821)) ;
#31184 = CARTESIAN_POINT('Ctrl Pts',(-20.4603959891244,38.6078133955189,122.82076541107)) ;
#31185 = CARTESIAN_POINT('Ctrl Pts',(-20.8301369986688,38.7976327101868,122.908200598567)) ;
#31186 = CARTESIAN_POINT('Ctrl Pts',(-20.5459597363222,38.6176436298239,123.008918492089)) ;
#31187 = CARTESIAN_POINT('Ctrl Pts',(-20.8963322764258,38.8077087354214,123.164523836751)) ;
#31188 = CARTESIAN_POINT('Ctrl Pts',(-20.5989170207742,38.6277196550586,123.213977164575)) ;
#31189 = CARTESIAN_POINT('Ctrl Pts',(-20.9166999184839,38.8175609719123,123.422684680524)) ;
#31190 = CARTESIAN_POINT('Ctrl Pts',(-20.6152120890159,38.6375718915494,123.420504774744)) ;
#31191 = CARTESIAN_POINT('Ctrl Pts',(-20.8916094132905,38.8276341783464,123.686162896882)) ;
#31192 = CARTESIAN_POINT('Ctrl Pts',(-20.5951407373615,38.6476450979836,123.631287770219)) ;
#31193 = CARTESIAN_POINT('Ctrl Pts',(-20.8226867659829,38.8374756878536,123.935453060471)) ;
#31194 = CARTESIAN_POINT('Ctrl Pts',(-20.5400039281525,38.6574866074907,123.830719181644)) ;
#31195 = CARTESIAN_POINT('Ctrl Pts',(-20.711078874135,38.8474366346334,124.172221368131)) ;
#31196 = CARTESIAN_POINT('Ctrl Pts',(-20.4507189196892,38.6674475542705,124.020134084588)) ;
#31197 = CARTESIAN_POINT('Ctrl Pts',(-20.558458951886,38.8574744634334,124.387360046542)) ;
#31198 = CARTESIAN_POINT('Ctrl Pts',(-20.3286238767375,38.6774853830706,124.192245792429)) ;
#31199 = CARTESIAN_POINT('Ctrl Pts',(-20.3741695323438,38.8673487731879,124.570081720976)) ;
#31200 = CARTESIAN_POINT('Ctrl Pts',(-20.1811938154597,38.687359692825,124.338423469398)) ;
#31201 = CARTESIAN_POINT('Ctrl Pts',(-20.1567812055592,38.8774184708611,124.72090620419)) ;
#31202 = CARTESIAN_POINT('Ctrl Pts',(-20.0072836517336,38.6974293904982,124.459084262676)) ;
#31203 = CARTESIAN_POINT('Ctrl Pts',(-19.9221504638818,38.8872519421485,124.82924108008)) ;
#31204 = CARTESIAN_POINT('Ctrl Pts',(-19.8195805334962,38.7072628617856,124.545752917569)) ;
#31205 = CARTESIAN_POINT('Ctrl Pts',(-19.6675077755331,38.8972815886784,124.897233739368)) ;
#31206 = CARTESIAN_POINT('Ctrl Pts',(-19.615866693082,38.7172925083155,124.600148473551)) ;
#31207 = CARTESIAN_POINT('Ctrl Pts',(-19.4047212779265,38.9073161030058,124.919189865937)) ;
#31208 = CARTESIAN_POINT('Ctrl Pts',(-19.4056375333307,38.7273270226429,124.61771467157)) ;
#31209 = CARTESIAN_POINT('Ctrl Pts',(-19.1475370275011,38.9171413884767,124.896304082123)) ;
#31210 = CARTESIAN_POINT('Ctrl Pts',(-19.1998910344568,38.7371523081138,124.599407555355)) ;
#31211 = CARTESIAN_POINT('Ctrl Pts',(-18.8935792031542,38.9271456300252,124.828433457309)) ;
#31212 = CARTESIAN_POINT('Ctrl Pts',(-18.9967244455218,38.7471565496623,124.545112555679)) ;
#31213 = CARTESIAN_POINT('Ctrl Pts',(-18.6557514840931,38.9371282751043,124.717603510386)) ;
#31214 = CARTESIAN_POINT('Ctrl Pts',(-18.8064617880754,38.7571391947414,124.456450040447)) ;
#31215 = CARTESIAN_POINT('Ctrl Pts',(-18.439669749991,38.9471734721958,124.566019704998)) ;
#31216 = CARTESIAN_POINT('Ctrl Pts',(-18.633595466131,38.7671843918329,124.335184114137)) ;
#31217 = CARTESIAN_POINT('Ctrl Pts',(-18.2569780632649,38.9569965879559,124.383630345431)) ;
#31218 = CARTESIAN_POINT('Ctrl Pts',(-18.4874417365958,38.7770075075931,124.189274418743)) ;
#31219 = CARTESIAN_POINT('Ctrl Pts',(-18.1050023548241,38.9670311997562,124.168134092341)) ;
#31220 = CARTESIAN_POINT('Ctrl Pts',(-18.3658597612924,38.7870421193933,124.016878306509)) ;
#31221 = CARTESIAN_POINT('Ctrl Pts',(-17.9935211048472,38.9770562085294,123.929428614842)) ;
#31222 = CARTESIAN_POINT('Ctrl Pts',(-18.2766733718385,38.7970671281665,123.825914551769)) ;
#31223 = CARTESIAN_POINT('Ctrl Pts',(-17.9258146375031,38.9869081333709,123.679534933401)) ;
#31224 = CARTESIAN_POINT('Ctrl Pts',(-18.2225068346885,38.8069190530081,123.62600081153)) ;
#31225 = CARTESIAN_POINT('Ctrl Pts',(-17.9017999976252,38.9968990716936,123.418116000194)) ;
#31226 = CARTESIAN_POINT('Ctrl Pts',(-18.2032934378327,38.8169099913308,123.416865957209)) ;
#31227 = CARTESIAN_POINT('Ctrl Pts',(-17.9232192572526,39.0068170568401,123.158331775182)) ;
#31228 = CARTESIAN_POINT('Ctrl Pts',(-18.2204270837738,38.8268279764772,123.209038890302)) ;
#31229 = CARTESIAN_POINT('Ctrl Pts',(-17.9900801459671,39.0168451577356,122.903447812489)) ;
#31230 = CARTESIAN_POINT('Ctrl Pts',(-18.2739141162152,38.8368560773727,123.005131251338)) ;
#31231 = CARTESIAN_POINT('Ctrl Pts',(-18.0985256645866,39.0267303986782,122.66738650819)) ;
#31232 = CARTESIAN_POINT('Ctrl Pts',(-18.3606686866534,38.8467413183153,122.816282007666)) ;
#31233 = CARTESIAN_POINT('Ctrl Pts',(-18.2473354546933,39.0367195116448,122.451127866607)) ;
#31234 = CARTESIAN_POINT('Ctrl Pts',(-18.4797149123304,38.8567304312819,122.643274141846)) ;
#31235 = CARTESIAN_POINT('Ctrl Pts',(-18.4328121554963,39.0467615759856,122.263416874408)) ;
#31236 = CARTESIAN_POINT('Ctrl Pts',(-18.628095065177,38.8667724956227,122.49310404951)) ;
#31237 = CARTESIAN_POINT('Ctrl Pts',(-18.6432316642718,39.0565907773901,122.113588566168)) ;
#31238 = CARTESIAN_POINT('Ctrl Pts',(-18.7964289710917,38.8766016970272,122.373240345266)) ;
#31239 = CARTESIAN_POINT('Ctrl Pts',(-18.8804006960058,39.0665976181483,122.000064282247)) ;
#31240 = CARTESIAN_POINT('Ctrl Pts',(-18.986163304992,38.8866085377854,122.282419197407)) ;
#31241 = CARTESIAN_POINT('Ctrl Pts',(-19.1333031196278,39.0765851423402,121.929712194851)) ;
#31242 = CARTESIAN_POINT('Ctrl Pts',(-19.1884846090727,38.8965960619773,122.226135721828)) ;
#31243 = CARTESIAN_POINT('Ctrl Pts',(-19.3956318554856,39.0866147881488,121.90442252384)) ;
#31244 = CARTESIAN_POINT('Ctrl Pts',(-19.3983474399373,38.9066257077859,122.205902107864)) ;
#31245 = CARTESIAN_POINT('Ctrl Pts',(-19.6543650766534,39.0964888188876,121.924438378725)) ;
#31246 = CARTESIAN_POINT('Ctrl Pts',(-19.6053336278132,38.9164997385247,122.221912828069)) ;
#31247 = CARTESIAN_POINT('Ctrl Pts',(-19.9088952559089,39.1064881417517,121.989562946881)) ;
#31248 = CARTESIAN_POINT('Ctrl Pts',(-19.8089581746776,38.9264990613888,122.274010548606)) ;
#31249 = CARTESIAN_POINT('Ctrl Pts',(-20.1463184204116,39.1163989773273,122.096736593804)) ;
#31250 = CARTESIAN_POINT('Ctrl Pts',(-19.9988971842688,38.9364098969644,122.359747484487)) ;
#31251 = CARTESIAN_POINT('Ctrl Pts',(-20.3645137350782,39.1264532253013,122.245659936878)) ;
#31252 = CARTESIAN_POINT('Ctrl Pts',(-20.1734546335938,38.9464641449384,122.47888456104)) ;
#31253 = CARTESIAN_POINT('Ctrl Pts',(-20.5501363523251,39.136311969564,122.426460600573)) ;
#31254 = CARTESIAN_POINT('Ctrl Pts',(-20.3219537705766,38.9563228892011,122.623523276543)) ;
#31255 = CARTESIAN_POINT('Ctrl Pts',(-20.7048400636721,39.146380055637,122.641049209758)) ;
#31256 = CARTESIAN_POINT('Ctrl Pts',(-20.445718474219,38.9663909752741,122.795193064183)) ;
#31257 = CARTESIAN_POINT('Ctrl Pts',(-20.8175117263284,39.1562355388165,122.87427274074)) ;
#31258 = CARTESIAN_POINT('Ctrl Pts',(-20.5358574288074,38.9762464584537,122.981770549878)) ;
#31259 = CARTESIAN_POINT('Ctrl Pts',(-20.889721867706,39.1662303846107,123.126796707764)) ;
#31260 = CARTESIAN_POINT('Ctrl Pts',(-20.5936275684775,38.9862413042478,123.183789061337)) ;
#31261 = CARTESIAN_POINT('Ctrl Pts',(-20.9165245762999,39.1762616802733,123.389047651322)) ;
#31262 = CARTESIAN_POINT('Ctrl Pts',(-20.6150717949923,38.9962725999104,123.393589604221)) ;
#31263 = CARTESIAN_POINT('Ctrl Pts',(-20.8981112102425,39.1861282235631,123.647684462324)) ;
#31264 = CARTESIAN_POINT('Ctrl Pts',(-20.6003432386068,39.0061391432003,123.600498792257)) ;
#31265 = CARTESIAN_POINT('Ctrl Pts',(-20.8347179859735,39.1961156193265,123.902339731277)) ;
#31266 = CARTESIAN_POINT('Ctrl Pts',(-20.5496307722175,39.0161265389636,123.804223432309)) ;
#31267 = CARTESIAN_POINT('Ctrl Pts',(-20.728622932385,39.2060606600565,124.14122345198)) ;
#31268 = CARTESIAN_POINT('Ctrl Pts',(-20.4647567795798,39.0260715796936,123.9953311149)) ;
#31269 = CARTESIAN_POINT('Ctrl Pts',(-20.5811155220166,39.2161051662732,124.360088757602)) ;
#31270 = CARTESIAN_POINT('Ctrl Pts',(-20.3467526264366,39.0361160859103,124.170424573902)) ;
#31271 = CARTESIAN_POINT('Ctrl Pts',(-20.4012820501656,39.2259686724105,124.546795194446)) ;
#31272 = CARTESIAN_POINT('Ctrl Pts',(-20.2028876468785,39.0459795920477,124.319790982306)) ;
#31273 = CARTESIAN_POINT('Ctrl Pts',(-20.1893406639608,39.2359615332466,124.701780528445)) ;
#31274 = CARTESIAN_POINT('Ctrl Pts',(-20.033335900681,39.0559724528837,124.443780983451)) ;
#31275 = CARTESIAN_POINT('Ctrl Pts',(-19.9552664329016,39.2458877269655,124.816982053056)) ;
#31276 = CARTESIAN_POINT('Ctrl Pts',(-19.8460776484438,39.0658986466027,124.535944103352)) ;
#31277 = CARTESIAN_POINT('Ctrl Pts',(-19.7024842949339,39.2559066529981,124.890499840195)) ;
#31278 = CARTESIAN_POINT('Ctrl Pts',(-19.643852594965,39.0759175726352,124.594760445571)) ;
#31279 = CARTESIAN_POINT('Ctrl Pts',(-19.4434484431289,39.2658216523657,124.918965884066)) ;
#31280 = CARTESIAN_POINT('Ctrl Pts',(-19.4366243284276,39.0858325720028,124.61753546939)) ;
#31281 = CARTESIAN_POINT('Ctrl Pts',(-19.1798154010535,39.275876423923,124.901733325748)) ;
#31282 = CARTESIAN_POINT('Ctrl Pts',(-19.2257177564351,39.0958873435601,124.603751640336)) ;
#31283 = CARTESIAN_POINT('Ctrl Pts',(-18.9280744033614,39.2857353862206,124.840355827184)) ;
#31284 = CARTESIAN_POINT('Ctrl Pts',(-19.0243246392442,39.1057463058577,124.55465185544)) ;
#31285 = CARTESIAN_POINT('Ctrl Pts',(-18.6874294683808,39.2957296300584,124.735252472311)) ;
#31286 = CARTESIAN_POINT('Ctrl Pts',(-18.8318078469648,39.1157405496955,124.470571256637)) ;
#31287 = CARTESIAN_POINT('Ctrl Pts',(-18.4700628513266,39.3056548594826,124.591021419432)) ;
#31288 = CARTESIAN_POINT('Ctrl Pts',(-18.6579133993353,39.1256657791198,124.355188343277)) ;
#31289 = CARTESIAN_POINT('Ctrl Pts',(-18.2791321697973,39.3156828233741,124.409439034504)) ;
#31290 = CARTESIAN_POINT('Ctrl Pts',(-18.5051673400138,39.1356937430112,124.209924100878)) ;
#31291 = CARTESIAN_POINT('Ctrl Pts',(-18.1245827427517,39.3255690830045,124.200558385393)) ;
#31292 = CARTESIAN_POINT('Ctrl Pts',(-18.381526045183,39.1455800026416,124.042820995344)) ;
#31293 = CARTESIAN_POINT('Ctrl Pts',(-18.0068578913663,39.3356008460823,123.964729079241)) ;
#31294 = CARTESIAN_POINT('Ctrl Pts',(-18.2873441695228,39.1556117657195,123.854158607123)) ;
#31295 = CARTESIAN_POINT('Ctrl Pts',(-17.9327236697777,39.3454824723765,123.715808953631)) ;
#31296 = CARTESIAN_POINT('Ctrl Pts',(-18.2280346488682,39.1654933920136,123.65502319765)) ;
#31297 = CARTESIAN_POINT('Ctrl Pts',(-17.9023337792867,39.3555442418626,123.453187507275)) ;
#31298 = CARTESIAN_POINT('Ctrl Pts',(-18.2037205033373,39.1755551614998,123.444926368231)) ;
#31299 = CARTESIAN_POINT('Ctrl Pts',(-17.9176154685571,39.3654021093581,123.194552719115)) ;
#31300 = CARTESIAN_POINT('Ctrl Pts',(-18.2159436064791,39.1854130289952,123.238018412343)) ;
#31301 = CARTESIAN_POINT('Ctrl Pts',(-17.9778056084377,39.3753937344755,122.939007178567)) ;
#31302 = CARTESIAN_POINT('Ctrl Pts',(-18.2640935243759,39.1954046541126,123.033581500678)) ;
#31303 = CARTESIAN_POINT('Ctrl Pts',(-18.0809465923163,39.3853305335837,122.699093789421)) ;
#31304 = CARTESIAN_POINT('Ctrl Pts',(-18.3466042525769,39.2053414532208,122.841649902938)) ;
#31305 = CARTESIAN_POINT('Ctrl Pts',(-18.2246316582653,39.3953213631411,122.479348914402)) ;
#31306 = CARTESIAN_POINT('Ctrl Pts',(-18.4615504185501,39.2153322827782,122.66585281308)) ;
#31307 = CARTESIAN_POINT('Ctrl Pts',(-18.4050975254076,39.4053445988542,122.287476075996)) ;
#31308 = CARTESIAN_POINT('Ctrl Pts',(-18.6059214265816,39.2253555184914,122.512353066652)) ;
#31309 = CARTESIAN_POINT('Ctrl Pts',(-18.6133254066964,39.4152409468834,122.131679228761)) ;
#31310 = CARTESIAN_POINT('Ctrl Pts',(-18.7725024389883,39.2352518665205,122.387713758651)) ;
#31311 = CARTESIAN_POINT('Ctrl Pts',(-18.8473919143103,39.4252305093859,122.012791074316)) ;
#31312 = CARTESIAN_POINT('Ctrl Pts',(-18.9597546642961,39.245241429023,122.292601282324)) ;
#31313 = CARTESIAN_POINT('Ctrl Pts',(-19.0999512728563,39.4352708170704,121.936479082214)) ;
#31314 = CARTESIAN_POINT('Ctrl Pts',(-19.1618012471887,39.2552817367076,122.231549573829)) ;
#31315 = CARTESIAN_POINT('Ctrl Pts',(-19.3567329848095,39.4451131204176,121.905300141157)) ;
#31316 = CARTESIAN_POINT('Ctrl Pts',(-19.3672271092616,39.2651240400548,122.206604238954)) ;
#31317 = CARTESIAN_POINT('Ctrl Pts',(-19.6197445019835,39.4551368286967,121.919081532484)) ;
#31318 = CARTESIAN_POINT('Ctrl Pts',(-19.5776343212279,39.2751477483338,122.217627049978)) ;
#31319 = CARTESIAN_POINT('Ctrl Pts',(-19.9583923044283,39.4683590061644,121.997113385212)) ;
#31320 = CARTESIAN_POINT('Ctrl Pts',(-19.8485635151233,39.2883699258015,122.280050331721)) ;
#31321 = CARTESIAN_POINT('Ctrl Pts',(-20.2706261181306,39.4816515912237,122.162206025503)) ;
#31322 = CARTESIAN_POINT('Ctrl Pts',(-20.0983757918957,39.3016625108608,122.412145538287)) ;
#31323 = CARTESIAN_POINT('Ctrl Pts',(-20.5265366200315,39.4949364471453,122.399782063078)) ;
#31324 = CARTESIAN_POINT('Ctrl Pts',(-20.3030677424335,39.3149473667824,122.602175696939)) ;
#31325 = CARTESIAN_POINT('Ctrl Pts',(-20.6848475062148,39.5049086743181,122.608570519109)) ;
#31326 = CARTESIAN_POINT('Ctrl Pts',(-20.4297258566199,39.3249195939552,122.769211054602)) ;
#31327 = CARTESIAN_POINT('Ctrl Pts',(-20.8041722375231,39.5148172907571,122.840044926829)) ;
#31328 = CARTESIAN_POINT('Ctrl Pts',(-20.5251856336139,39.3348282103942,122.954388023249)) ;
#31329 = CARTESIAN_POINT('Ctrl Pts',(-20.8825021974907,39.5248704961408,123.09232602936)) ;
#31330 = CARTESIAN_POINT('Ctrl Pts',(-20.5878516382789,39.3448814157779,123.156213664846)) ;
#31331 = CARTESIAN_POINT('Ctrl Pts',(-20.9153854640603,39.5347356299011,123.349500706136)) ;
#31332 = CARTESIAN_POINT('Ctrl Pts',(-20.6141617865867,39.3547465495382,123.361949101435)) ;
#31333 = CARTESIAN_POINT('Ctrl Pts',(-20.8994475638338,39.5480746875274,123.699654940672)) ;
#31334 = CARTESIAN_POINT('Ctrl Pts',(-20.6014062025632,39.3680856071645,123.642094456117)) ;
#31335 = CARTESIAN_POINT('Ctrl Pts',(-20.7662626209752,39.5646438748606,124.119481950554)) ;
#31336 = CARTESIAN_POINT('Ctrl Pts',(-20.4948802699597,39.3846547944977,123.977922342078)) ;
#31337 = CARTESIAN_POINT('Ctrl Pts',(-20.4969232972869,39.5812890147116,124.470352991445)) ;
#31338 = CARTESIAN_POINT('Ctrl Pts',(-20.2793689415074,39.4012999343487,124.258669314264)) ;
#31339 = CARTESIAN_POINT('Ctrl Pts',(-20.2201055636797,39.594561317185,124.682635504472)) ;
#31340 = CARTESIAN_POINT('Ctrl Pts',(-20.0579520034563,39.4145722368221,124.428460073727)) ;
#31341 = CARTESIAN_POINT('Ctrl Pts',(-19.9875926506158,39.6045422806326,124.803956293346)) ;
#31342 = CARTESIAN_POINT('Ctrl Pts',(-19.8719346104858,39.4245532002698,124.525525821103)) ;
#31343 = CARTESIAN_POINT('Ctrl Pts',(-19.7385233068285,39.6144841127019,124.882919421765)) ;
#31344 = CARTESIAN_POINT('Ctrl Pts',(-19.6726839339702,39.4344950323391,124.588696443466)) ;
#31345 = CARTESIAN_POINT('Ctrl Pts',(-19.3916274184842,39.6278036819174,124.929289096296)) ;
#31346 = CARTESIAN_POINT('Ctrl Pts',(-19.3951539287029,39.4478146015545,124.625793702536)) ;
#31347 = CARTESIAN_POINT('Ctrl Pts',(-18.9557155359981,39.6443338368501,124.873608604834)) ;
#31348 = CARTESIAN_POINT('Ctrl Pts',(-19.0464382212822,39.4643447564872,124.581253473117)) ;
#31349 = CARTESIAN_POINT('Ctrl Pts',(-18.4827841914937,39.6643555623422,124.629948165702)) ;
#31350 = CARTESIAN_POINT('Ctrl Pts',(-18.6680869357579,39.4843664819793,124.386327764593)) ;
#31351 = CARTESIAN_POINT('Ctrl Pts',(-18.1247857375982,39.684166958949,124.243642886315)) ;
#31352 = CARTESIAN_POINT('Ctrl Pts',(-18.3816862675463,39.5041778785861,124.077284936914)) ;
#31353 = CARTESIAN_POINT('Ctrl Pts',(-17.9175888921553,39.7041522076579,123.754678947954)) ;
#31354 = CARTESIAN_POINT('Ctrl Pts',(-18.2159257535573,39.524163127295,123.686114759911)) ;
#31355 = CARTESIAN_POINT('Ctrl Pts',(-17.8901646194333,39.7240462702938,123.226554358752)) ;
#31356 = CARTESIAN_POINT('Ctrl Pts',(-18.1939835441653,39.5440571899309,123.263614485181)) ;
#31357 = CARTESIAN_POINT('Ctrl Pts',(-18.0441177194512,39.7439779494674,122.719677099901)) ;
#31358 = CARTESIAN_POINT('Ctrl Pts',(-18.3171437873971,39.5639888691045,122.858111428602)) ;
#31359 = CARTESIAN_POINT('Ctrl Pts',(-18.3626008286604,39.7639420039394,122.295272619757)) ;
#31360 = CARTESIAN_POINT('Ctrl Pts',(-18.5719284738746,39.5839529235765,122.518586147516)) ;
#31361 = CARTESIAN_POINT('Ctrl Pts',(-18.8047431638309,39.7838229057023,122.005888410444)) ;
#31362 = CARTESIAN_POINT('Ctrl Pts',(-18.9256420531025,39.6038338253394,122.287076349787)) ;
#31363 = CARTESIAN_POINT('Ctrl Pts',(-19.3204270314315,39.8037615673107,121.883932996576)) ;
#31364 = CARTESIAN_POINT('Ctrl Pts',(-19.3381893000524,39.6237724869478,122.189510074961)) ;
#31365 = CARTESIAN_POINT('Ctrl Pts',(-19.8456885699466,39.823658092566,121.945064977875)) ;
#31366 = CARTESIAN_POINT('Ctrl Pts',(-19.7583997745947,39.6436690122031,122.238414117191)) ;
#31367 = CARTESIAN_POINT('Ctrl Pts',(-20.3189371293568,39.8435531310203,122.180988955681)) ;
#31368 = CARTESIAN_POINT('Ctrl Pts',(-20.1370001890922,39.6635640506575,122.427152812222)) ;
#31369 = CARTESIAN_POINT('Ctrl Pts',(-20.684435302286,39.8635169543264,122.565581974928)) ;
#31370 = CARTESIAN_POINT('Ctrl Pts',(-20.4293997300506,39.6835278739635,122.734826840731)) ;
#31371 = CARTESIAN_POINT('Ctrl Pts',(-20.8961892011034,39.8833910784555,123.049543285432)) ;
#31372 = CARTESIAN_POINT('Ctrl Pts',(-20.5988040313383,39.7034019980926,123.121997016737)) ;
#31373 = CARTESIAN_POINT('Ctrl Pts',(-20.9307446999035,39.9033661541827,123.579345858903)) ;
#31374 = CARTESIAN_POINT('Ctrl Pts',(-20.6264486432097,39.7233770738199,123.54583933781)) ;
#31375 = CARTESIAN_POINT('Ctrl Pts',(-20.7818723368726,39.9233197235393,124.088346140046)) ;
#31376 = CARTESIAN_POINT('Ctrl Pts',(-20.5073509383854,39.7433306431764,123.953040241885)) ;
#31377 = CARTESIAN_POINT('Ctrl Pts',(-20.4708597448831,39.9431576337272,124.514109737929)) ;
#31378 = CARTESIAN_POINT('Ctrl Pts',(-20.2585393443571,39.7631685533643,124.293652633685)) ;
#31379 = CARTESIAN_POINT('Ctrl Pts',(-20.0304987770853,39.9631334622981,124.810695893572)) ;
#31380 = CARTESIAN_POINT('Ctrl Pts',(-19.9062499102217,39.7831443819352,124.53092102101)) ;
#31381 = CARTESIAN_POINT('Ctrl Pts',(-19.5167467254977,39.9830515070084,124.938262136295)) ;
#31382 = CARTESIAN_POINT('Ctrl Pts',(-19.4952471367361,39.8030624266455,124.632973548658)) ;
#31383 = CARTESIAN_POINT('Ctrl Pts',(-18.9912829799873,40.002921752796,124.884310017349)) ;
#31384 = CARTESIAN_POINT('Ctrl Pts',(-19.0748749155325,39.8229326724332,124.589810226705)) ;
#31385 = CARTESIAN_POINT('Ctrl Pts',(-18.512059067701,40.0229707558956,124.651607827821)) ;
#31386 = CARTESIAN_POINT('Ctrl Pts',(-18.691496813196,39.8429816755327,124.403647475634)) ;
#31387 = CARTESIAN_POINT('Ctrl Pts',(-18.1453823899898,40.0427499971364,124.274685535331)) ;
#31388 = CARTESIAN_POINT('Ctrl Pts',(-18.3981551846587,39.8627609167736,124.10210688277)) ;
#31389 = CARTESIAN_POINT('Ctrl Pts',(-17.9259795061986,40.0627800608453,123.789764142162)) ;
#31390 = CARTESIAN_POINT('Ctrl Pts',(-18.2226350126772,39.8827909804824,123.714169148054)) ;
#31391 = CARTESIAN_POINT('Ctrl Pts',(-17.8863640755832,40.0826623457473,123.26273048994)) ;
#31392 = CARTESIAN_POINT('Ctrl Pts',(-18.1909445989057,39.9026732653844,123.292541016045)) ;
#31393 = CARTESIAN_POINT('Ctrl Pts',(-18.0275270007879,40.1025446466403,122.753544083108)) ;
#31394 = CARTESIAN_POINT('Ctrl Pts',(-18.3038777717334,39.9225555662774,122.885191650426)) ;
#31395 = CARTESIAN_POINT('Ctrl Pts',(-18.3357032518353,40.1225277562586,122.320964219485)) ;
#31396 = CARTESIAN_POINT('Ctrl Pts',(-18.5504210502982,39.9425386758957,122.539129268786)) ;
#31397 = CARTESIAN_POINT('Ctrl Pts',(-18.7710249752049,40.1424181516365,122.020953450762)) ;
#31398 = CARTESIAN_POINT('Ctrl Pts',(-18.8986807002394,39.9624290712736,122.299122526392)) ;
#31399 = CARTESIAN_POINT('Ctrl Pts',(-19.2824556627369,40.1623149416708,121.886718883341)) ;
#31400 = CARTESIAN_POINT('Ctrl Pts',(-19.3078267411535,39.9823258613079,122.191737773976)) ;
#31401 = CARTESIAN_POINT('Ctrl Pts',(-19.809682792952,40.1822319956124,121.93454660401)) ;
#31402 = CARTESIAN_POINT('Ctrl Pts',(-19.7296086094093,40.0022429152495,122.230003389753)) ;
#31403 = CARTESIAN_POINT('Ctrl Pts',(-20.290985297749,40.2022355438159,122.160572440253)) ;
#31404 = CARTESIAN_POINT('Ctrl Pts',(-20.1146490294153,40.022246463453,122.410827178833)) ;
#31405 = CARTESIAN_POINT('Ctrl Pts',(-20.6644175476188,40.2221738374685,122.536530476513)) ;
#31406 = CARTESIAN_POINT('Ctrl Pts',(-20.4133927604481,40.0421847571056,122.711596130847)) ;
#31407 = CARTESIAN_POINT('Ctrl Pts',(-20.8870164933769,40.2419953249014,123.014022848812)) ;
#31408 = CARTESIAN_POINT('Ctrl Pts',(-20.591468541711,40.0620062445386,123.093592852938)) ;
#31409 = CARTESIAN_POINT('Ctrl Pts',(-20.9342078753314,40.2619737178923,123.54285440319)) ;
#31410 = CARTESIAN_POINT('Ctrl Pts',(-20.629219041352,40.0819846375294,123.51665686398)) ;
#31411 = CARTESIAN_POINT('Ctrl Pts',(-20.798306014332,40.281872099506,124.054044528013)) ;
#31412 = CARTESIAN_POINT('Ctrl Pts',(-20.5204887803847,40.1018830191431,123.925614389338)) ;
#31413 = CARTESIAN_POINT('Ctrl Pts',(-20.5470819880528,40.2984550302359,124.416062159147)) ;
#31414 = CARTESIAN_POINT('Ctrl Pts',(-20.319521718774,40.118465949873,124.215207873857)) ;
#31415 = CARTESIAN_POINT('Ctrl Pts',(-20.281028441282,40.3117292658247,124.641768863592)) ;
#31416 = CARTESIAN_POINT('Ctrl Pts',(-20.1066630077281,40.1317401854619,124.39578795603)) ;
#31417 = CARTESIAN_POINT('Ctrl Pts',(-20.0530654837522,40.3217756832809,124.774877815114)) ;
#31418 = CARTESIAN_POINT('Ctrl Pts',(-19.9242972790721,40.1417866029181,124.50226984556)) ;
#31419 = CARTESIAN_POINT('Ctrl Pts',(-19.810464403995,40.3316209085002,124.864833820521)) ;
#31420 = CARTESIAN_POINT('Ctrl Pts',(-19.7302036734289,40.1516318281373,124.574233889448)) ;
#31421 = CARTESIAN_POINT('Ctrl Pts',(-19.4658929191224,40.3449558795396,124.928504806225)) ;
#31422 = CARTESIAN_POINT('Ctrl Pts',(-19.4546005727731,40.1649667991767,124.625166764035)) ;
#31423 = CARTESIAN_POINT('Ctrl Pts',(-19.0264390688312,40.3615387363322,124.893652813554)) ;
#31424 = CARTESIAN_POINT('Ctrl Pts',(-19.1029686872478,40.1815496559694,124.597278988789)) ;
#31425 = CARTESIAN_POINT('Ctrl Pts',(-18.6239205040509,40.3781817386816,124.71045606654)) ;
#31426 = CARTESIAN_POINT('Ctrl Pts',(-18.7810022090588,40.1981926583188,124.450732338554)) ;
#31427 = CARTESIAN_POINT('Ctrl Pts',(-18.3550031410799,40.3914254697133,124.489405088402)) ;
#31428 = CARTESIAN_POINT('Ctrl Pts',(-18.5658419708258,40.2114363893504,124.273876441203)) ;
#31429 = CARTESIAN_POINT('Ctrl Pts',(-18.1831556506858,40.4014798643879,124.288773158582)) ;
#31430 = CARTESIAN_POINT('Ctrl Pts',(-18.4283713813035,40.221490784025,124.113372135424)) ;
#31431 = CARTESIAN_POINT('Ctrl Pts',(-18.0512693189918,40.4113209257765,124.066262657595)) ;
#31432 = CARTESIAN_POINT('Ctrl Pts',(-18.3228626055422,40.2313318454136,123.935361746005)) ;
#31433 = CARTESIAN_POINT('Ctrl Pts',(-17.9577246777451,40.421387150133,123.818872622899)) ;
#31434 = CARTESIAN_POINT('Ctrl Pts',(-18.2480294373586,40.2413980697701,123.737449245068)) ;
#31435 = CARTESIAN_POINT('Ctrl Pts',(-17.9095230457467,40.4312677630526,123.563691114021)) ;
#31436 = CARTESIAN_POINT('Ctrl Pts',(-18.2094701905773,40.2512786826897,123.533303479069)) ;
#31437 = CARTESIAN_POINT('Ctrl Pts',(-17.9058281378729,40.4412610562122,123.30114626875)) ;
#31438 = CARTESIAN_POINT('Ctrl Pts',(-18.2065165443278,40.2612719758493,123.323267634952)) ;
#31439 = CARTESIAN_POINT('Ctrl Pts',(-17.9475138799179,40.4512120644359,123.042941598617)) ;
#31440 = CARTESIAN_POINT('Ctrl Pts',(-18.2398673462306,40.271222984073,123.116704268342)) ;
#31441 = CARTESIAN_POINT('Ctrl Pts',(-18.0344070397604,40.4612605787978,122.793614478542)) ;
#31442 = CARTESIAN_POINT('Ctrl Pts',(-18.3093839709595,40.281271498435,122.917243386907)) ;
#31443 = CARTESIAN_POINT('Ctrl Pts',(-18.1603863836437,40.4711020848605,122.567719550063)) ;
#31444 = CARTESIAN_POINT('Ctrl Pts',(-18.4101694281105,40.2911130044976,122.736528509964)) ;
#31445 = CARTESIAN_POINT('Ctrl Pts',(-18.3255788630243,40.4810877374902,122.36388078949)) ;
#31446 = CARTESIAN_POINT('Ctrl Pts',(-18.5423251289196,40.3010986571273,122.573458977904)) ;
#31447 = CARTESIAN_POINT('Ctrl Pts',(-18.5227257140879,40.4910267463351,122.192496536557)) ;
#31448 = CARTESIAN_POINT('Ctrl Pts',(-18.7000440471516,40.3110376659722,122.436353315188)) ;
#31449 = CARTESIAN_POINT('Ctrl Pts',(-18.7489120153398,40.5010676716281,122.056659651422)) ;
#31450 = CARTESIAN_POINT('Ctrl Pts',(-18.8809942079959,40.3210785912652,122.327685771661)) ;
#31451 = CARTESIAN_POINT('Ctrl Pts',(-18.9915421154482,40.510957993383,121.963416273453)) ;
#31452 = CARTESIAN_POINT('Ctrl Pts',(-19.0750990226228,40.3309689130201,122.253093205079)) ;
#31453 = CARTESIAN_POINT('Ctrl Pts',(-19.249284101431,40.5209539667164,121.912814957505)) ;
#31454 = CARTESIAN_POINT('Ctrl Pts',(-19.2812929812387,40.3409648863536,122.212614377811)) ;
#31455 = CARTESIAN_POINT('Ctrl Pts',(-19.5102329048635,40.5308853662985,121.907746825893)) ;
#31456 = CARTESIAN_POINT('Ctrl Pts',(-19.4900519685887,40.3508962859356,122.208562125718)) ;
#31457 = CARTESIAN_POINT('Ctrl Pts',(-19.7700821945994,40.5408909067755,121.947997275359)) ;
#31458 = CARTESIAN_POINT('Ctrl Pts',(-19.697930995272,40.3609018264127,122.240764692487)) ;
#31459 = CARTESIAN_POINT('Ctrl Pts',(-20.0195011590798,40.5509238907068,122.033437044935)) ;
#31460 = CARTESIAN_POINT('Ctrl Pts',(-19.8974654062638,40.370934810344,122.30911863456)) ;
#31461 = CARTESIAN_POINT('Ctrl Pts',(-20.2464637604241,40.5607795215337,122.158246335581)) ;
#31462 = CARTESIAN_POINT('Ctrl Pts',(-20.0790342417892,40.3807904411708,122.408967940428)) ;
#31463 = CARTESIAN_POINT('Ctrl Pts',(-20.4514141919689,40.5707789237268,122.322629146748)) ;
#31464 = CARTESIAN_POINT('Ctrl Pts',(-20.2429931328991,40.390789843364,122.540475886912)) ;
#31465 = CARTESIAN_POINT('Ctrl Pts',(-20.623177160939,40.5806733930879,122.517901168788)) ;
#31466 = CARTESIAN_POINT('Ctrl Pts',(-20.3804017081287,40.400684312725,122.696694807102)) ;
#31467 = CARTESIAN_POINT('Ctrl Pts',(-20.7606139057598,40.5907365072521,122.743776897285)) ;
#31468 = CARTESIAN_POINT('Ctrl Pts',(-20.4903492208581,40.4107474268893,122.87739656958)) ;
#31469 = CARTESIAN_POINT('Ctrl Pts',(-20.8549063786372,40.6005761529685,122.984593090461)) ;
#31470 = CARTESIAN_POINT('Ctrl Pts',(-20.5657810296931,40.4205870726056,123.070050018048)) ;
#31471 = CARTESIAN_POINT('Ctrl Pts',(-20.9074265587478,40.6106393205242,123.243737629738)) ;
#31472 = CARTESIAN_POINT('Ctrl Pts',(-20.6077950427695,40.4306502401614,123.277366118892)) ;
#31473 = CARTESIAN_POINT('Ctrl Pts',(-20.9138213840196,40.6205335763191,123.50369845043)) ;
#31474 = CARTESIAN_POINT('Ctrl Pts',(-20.6129087015084,40.4405444959563,123.48533456448)) ;
#31475 = CARTESIAN_POINT('Ctrl Pts',(-20.8755072031584,40.6304753547788,123.762100783259)) ;
#31476 = CARTESIAN_POINT('Ctrl Pts',(-20.5822552681282,40.4504862744159,123.692055906574)) ;
#31477 = CARTESIAN_POINT('Ctrl Pts',(-20.7924699762297,40.640478047609,124.011537115954)) ;
#31478 = CARTESIAN_POINT('Ctrl Pts',(-20.5158234865121,40.4604889672461,123.891604236471)) ;
#31479 = CARTESIAN_POINT('Ctrl Pts',(-20.6666615752292,40.6505120695628,124.243257679907)) ;
#31480 = CARTESIAN_POINT('Ctrl Pts',(-20.4151748534295,40.4705229891999,124.076979664182)) ;
#31481 = CARTESIAN_POINT('Ctrl Pts',(-20.5058740591058,40.6603598606518,124.446047890609)) ;
#31482 = CARTESIAN_POINT('Ctrl Pts',(-20.2865434507489,40.480370780289,124.239210154722)) ;
#31483 = CARTESIAN_POINT('Ctrl Pts',(-20.3100969713907,40.6703413852009,124.620584309683)) ;
#31484 = CARTESIAN_POINT('Ctrl Pts',(-20.1299205038193,40.490352304838,124.378837647099)) ;
#31485 = CARTESIAN_POINT('Ctrl Pts',(-20.0876630799493,40.6802906086918,124.75801282759)) ;
#31486 = CARTESIAN_POINT('Ctrl Pts',(-19.9519724829499,40.5003015283289,124.488778579875)) ;
#31487 = CARTESIAN_POINT('Ctrl Pts',(-19.8436735816779,40.6902882649084,124.85551512015)) ;
#31488 = CARTESIAN_POINT('Ctrl Pts',(-19.7567802051122,40.5102991845455,124.566778487717)) ;
#31489 = CARTESIAN_POINT('Ctrl Pts',(-19.5853011891557,40.7003284779634,124.908895920478)) ;
#31490 = CARTESIAN_POINT('Ctrl Pts',(-19.5500818185997,40.5203393976006,124.609481080196)) ;
#31491 = CARTESIAN_POINT('Ctrl Pts',(-19.3271425182227,40.7101565252397,124.917006738006)) ;
#31492 = CARTESIAN_POINT('Ctrl Pts',(-19.3435554357432,40.5301674448768,124.615967681454)) ;
#31493 = CARTESIAN_POINT('Ctrl Pts',(-19.0655819825205,40.7202108722721,124.87973320103)) ;
#31494 = CARTESIAN_POINT('Ctrl Pts',(-19.1343072015728,40.5402217919092,124.58614687555)) ;
#31495 = CARTESIAN_POINT('Ctrl Pts',(-18.8174100404169,40.7301520086006,124.798108890604)) ;
#31496 = CARTESIAN_POINT('Ctrl Pts',(-18.9357705393896,40.5501629282377,124.520845572302)) ;
#31497 = CARTESIAN_POINT('Ctrl Pts',(-18.5876566119404,40.7400562416803,124.675804537039)) ;
#31498 = CARTESIAN_POINT('Ctrl Pts',(-18.7519690826901,40.5600671613174,124.423000582265)) ;
#31499 = CARTESIAN_POINT('Ctrl Pts',(-18.3798041844874,40.7501029385239,124.513046489696)) ;
#31500 = CARTESIAN_POINT('Ctrl Pts',(-18.5856882820567,40.5701138581611,124.292792552084)) ;
#31501 = CARTESIAN_POINT('Ctrl Pts',(-18.2058043531865,40.7599984898042,124.319735002295)) ;
#31502 = CARTESIAN_POINT('Ctrl Pts',(-18.4464901583571,40.5800094094413,124.138142422738)) ;
#31503 = CARTESIAN_POINT('Ctrl Pts',(-18.0657367626924,40.7700605676437,124.095504335531)) ;
#31504 = CARTESIAN_POINT('Ctrl Pts',(-18.3344376418936,40.5900714872808,123.958756744868)) ;
#31505 = CARTESIAN_POINT('Ctrl Pts',(-17.9687267603788,40.7799032767398,123.855697491767)) ;
#31506 = CARTESIAN_POINT('Ctrl Pts',(-18.2568316638286,40.5999141963769,123.766911199684)) ;
#31507 = CARTESIAN_POINT('Ctrl Pts',(-17.9134237543617,40.7898940089782,123.599076400319)) ;
#31508 = CARTESIAN_POINT('Ctrl Pts',(-18.2125910590899,40.6099049286153,123.561614081908)) ;
#31509 = CARTESIAN_POINT('Ctrl Pts',(-17.9036209757213,40.799822034207,123.33834843595)) ;
#31510 = CARTESIAN_POINT('Ctrl Pts',(-18.2047506639829,40.6198329538441,123.353032033196)) ;
#31511 = CARTESIAN_POINT('Ctrl Pts',(-17.9390103972283,40.8098101808575,123.07826099235)) ;
#31512 = CARTESIAN_POINT('Ctrl Pts',(-18.2330639096619,40.6298211004947,123.144962455833)) ;
#31513 = CARTESIAN_POINT('Ctrl Pts',(-18.0197805146774,40.8198451986975,122.827221506658)) ;
#31514 = CARTESIAN_POINT('Ctrl Pts',(-18.2976817439703,40.6398561183346,122.944131364963)) ;
#31515 = CARTESIAN_POINT('Ctrl Pts',(-18.1405769536225,40.8297099958027,122.597859805826)) ;
#31516 = CARTESIAN_POINT('Ctrl Pts',(-18.394320133305,40.6497209154398,122.76064343955)) ;
#31517 = CARTESIAN_POINT('Ctrl Pts',(-18.3003100262152,40.8396707281588,122.390481778754)) ;
#31518 = CARTESIAN_POINT('Ctrl Pts',(-18.5221077146717,40.6596816477959,122.594742235113)) ;
#31519 = CARTESIAN_POINT('Ctrl Pts',(-18.4953203364736,40.8497041905558,122.213037685501)) ;
#31520 = CARTESIAN_POINT('Ctrl Pts',(-18.6781171657498,40.6697151101929,122.452788175949)) ;
#31521 = CARTESIAN_POINT('Ctrl Pts',(-18.7146955767961,40.8595897247672,122.073836456238)) ;
#31522 = CARTESIAN_POINT('Ctrl Pts',(-18.8536176951084,40.6796006444043,122.341428911214)) ;
#31523 = CARTESIAN_POINT('Ctrl Pts',(-18.9592101605245,40.8696545654472,121.973078301155)) ;
#31524 = CARTESIAN_POINT('Ctrl Pts',(-19.0492301753213,40.6896654850843,122.260823821511)) ;
#31525 = CARTESIAN_POINT('Ctrl Pts',(-19.2119712899475,40.8795026971761,121.917403865115)) ;
#31526 = CARTESIAN_POINT('Ctrl Pts',(-19.2514386073647,40.6995136168132,122.216286026283)) ;
#31527 = CARTESIAN_POINT('Ctrl Pts',(-19.4752106016322,40.8895301941662,121.905583046178)) ;
#31528 = CARTESIAN_POINT('Ctrl Pts',(-19.4620301548535,40.7095411138033,122.206830852572)) ;
#31529 = CARTESIAN_POINT('Ctrl Pts',(-19.7364587404572,40.8995586462113,121.940346685251)) ;
#31530 = CARTESIAN_POINT('Ctrl Pts',(-19.6710285077072,40.7195695658484,122.234643374607)) ;
#31531 = CARTESIAN_POINT('Ctrl Pts',(-19.9832352577145,40.9094039127754,122.018011497405)) ;
#31532 = CARTESIAN_POINT('Ctrl Pts',(-19.8684484097077,40.7294148324125,122.296776407657)) ;
#31533 = CARTESIAN_POINT('Ctrl Pts',(-20.2165109099258,40.9193945857163,122.138492853158)) ;
#31534 = CARTESIAN_POINT('Ctrl Pts',(-20.0550681579274,40.7394055053534,122.393162648683)) ;
#31535 = CARTESIAN_POINT('Ctrl Pts',(-20.4259458604295,40.9294324678048,122.29886132802)) ;
#31536 = CARTESIAN_POINT('Ctrl Pts',(-20.2226152908657,40.7494433874419,122.521458685121)) ;
#31537 = CARTESIAN_POINT('Ctrl Pts',(-20.6012563123727,40.9392768382444,122.489117146691)) ;
#31538 = CARTESIAN_POINT('Ctrl Pts',(-20.3628619804321,40.7592877578816,122.67366360375)) ;
#31539 = CARTESIAN_POINT('Ctrl Pts',(-20.7432721400069,40.9492616656398,122.709711313099)) ;
#31540 = CARTESIAN_POINT('Ctrl Pts',(-20.4764734396498,40.7692725852769,122.850139473825)) ;
#31541 = CARTESIAN_POINT('Ctrl Pts',(-20.844502824681,40.9592011110451,122.950536538216)) ;
#31542 = CARTESIAN_POINT('Ctrl Pts',(-20.5574566433733,40.7792120306822,123.042799745308)) ;
#31543 = CARTESIAN_POINT('Ctrl Pts',(-20.9028785373405,40.969241115331,123.20781127082)) ;
#31544 = CARTESIAN_POINT('Ctrl Pts',(-20.6041559783071,40.7892520349681,123.24861993569)) ;
#31545 = CARTESIAN_POINT('Ctrl Pts',(-20.9156810985871,40.9791282245166,123.46734861019)) ;
#31546 = CARTESIAN_POINT('Ctrl Pts',(-20.6143967389084,40.7991391441538,123.456249117252)) ;
#31547 = CARTESIAN_POINT('Ctrl Pts',(-20.8831859202662,40.9891282844191,123.728082234662)) ;
#31548 = CARTESIAN_POINT('Ctrl Pts',(-20.5883994360712,40.8091392040562,123.664835757104)) ;
#31549 = CARTESIAN_POINT('Ctrl Pts',(-20.8067389220528,40.9990457003338,123.977282854265)) ;
#31550 = CARTESIAN_POINT('Ctrl Pts',(-20.5272409208135,40.8190566199709,123.864195371173)) ;
#31551 = CARTESIAN_POINT('Ctrl Pts',(-20.6866067690655,41.0090925150746,124.212346711425)) ;
#31552 = CARTESIAN_POINT('Ctrl Pts',(-20.4311340955001,40.8291034347117,124.052246084703)) ;
#31553 = CARTESIAN_POINT('Ctrl Pts',(-20.5303634279957,41.0189679922713,124.419613620439)) ;
#31554 = CARTESIAN_POINT('Ctrl Pts',(-20.3061390542249,40.8389789119084,124.218058285258)) ;
#31555 = CARTESIAN_POINT('Ctrl Pts',(-20.3371972791705,41.0290240879925,124.599886515678)) ;
#31556 = CARTESIAN_POINT('Ctrl Pts',(-20.1516052586008,40.8490350076296,124.362275967077)) ;
#31557 = CARTESIAN_POINT('Ctrl Pts',(-20.1192272911797,41.0389172500076,124.741681401867)) ;
#31558 = CARTESIAN_POINT('Ctrl Pts',(-19.9772293226388,40.8589281696447,124.475710604766)) ;
#31559 = CARTESIAN_POINT('Ctrl Pts',(-19.8759671921668,41.0489794860302,124.845254462117)) ;
#31560 = CARTESIAN_POINT('Ctrl Pts',(-19.7826206014674,40.8689904056673,124.558568216301)) ;
#31561 = CARTESIAN_POINT('Ctrl Pts',(-19.6239559484601,41.0588239516591,124.903758180381)) ;
#31562 = CARTESIAN_POINT('Ctrl Pts',(-19.5810124074109,40.8788348712962,124.605369962764)) ;
#31563 = CARTESIAN_POINT('Ctrl Pts',(-19.3626471098562,41.0687840443633,124.918720690763)) ;
#31564 = CARTESIAN_POINT('Ctrl Pts',(-19.3719656563023,40.8887949640004,124.61733915855)) ;
#31565 = CARTESIAN_POINT('Ctrl Pts',(-19.1007386053563,41.0788223333443,124.887329010187)) ;
#31566 = CARTESIAN_POINT('Ctrl Pts',(-19.16243883266,40.8988332529814,124.592224889164)) ;
#31567 = CARTESIAN_POINT('Ctrl Pts',(-18.8522137572535,41.0886956564505,124.812656518733)) ;
#31568 = CARTESIAN_POINT('Ctrl Pts',(-18.9636200453775,40.9087065760876,124.532486393259)) ;
#31569 = CARTESIAN_POINT('Ctrl Pts',(-18.6158596069558,41.0987688405356,124.693571352366)) ;
#31570 = CARTESIAN_POINT('Ctrl Pts',(-18.7745367877756,40.9187797601727,124.437217376295)) ;
#31571 = CARTESIAN_POINT('Ctrl Pts',(-18.4088042083935,41.1085893528235,124.539431437794)) ;
#31572 = CARTESIAN_POINT('Ctrl Pts',(-18.6088939047249,40.9286002724607,124.313905598339)) ;
#31573 = CARTESIAN_POINT('Ctrl Pts',(-18.2269108302998,41.1186673489393,124.347022071441)) ;
#31574 = CARTESIAN_POINT('Ctrl Pts',(-18.4633794360143,40.9386782685765,124.159977371275)) ;
#31575 = CARTESIAN_POINT('Ctrl Pts',(-18.0843084263497,41.1285214239226,124.130796993338)) ;
#31576 = CARTESIAN_POINT('Ctrl Pts',(-18.349298634213,40.9485323435597,123.986997811558)) ;
#31577 = CARTESIAN_POINT('Ctrl Pts',(-17.9790049811939,41.1385853055063,123.888252695276)) ;
#31578 = CARTESIAN_POINT('Ctrl Pts',(-18.2650563069979,40.9585962251434,123.792961884212)) ;
#31579 = CARTESIAN_POINT('Ctrl Pts',(-17.9185435301409,41.14846873148,123.63561553845)) ;
#31580 = CARTESIAN_POINT('Ctrl Pts',(-18.2166879295781,40.9684796511172,123.590852855347)) ;
#31581 = CARTESIAN_POINT('Ctrl Pts',(-17.9022681371798,41.1584693354011,123.37336067713)) ;
#31582 = CARTESIAN_POINT('Ctrl Pts',(-18.2036681214858,40.9784802550382,123.381049048255)) ;
#31583 = CARTESIAN_POINT('Ctrl Pts',(-17.931383888056,41.168389119739,123.114261971927)) ;
#31584 = CARTESIAN_POINT('Ctrl Pts',(-18.2269611056014,40.9884000393761,123.17377075239)) ;
#31585 = CARTESIAN_POINT('Ctrl Pts',(-18.0060263785442,41.1784364700958,122.861044240447)) ;
#31586 = CARTESIAN_POINT('Ctrl Pts',(-18.2866756080612,40.998447389733,122.971196520026)) ;
#31587 = CARTESIAN_POINT('Ctrl Pts',(-18.1212813811983,41.1883138123301,122.62841137183)) ;
#31588 = CARTESIAN_POINT('Ctrl Pts',(-18.3788795564563,41.0083247319672,122.785091229606)) ;
#31589 = CARTESIAN_POINT('Ctrl Pts',(-18.2781294851284,41.1983836934047,122.415344458296)) ;
#31590 = CARTESIAN_POINT('Ctrl Pts',(-18.504358563971,41.0183946130419,122.614637662932)) ;
#31591 = CARTESIAN_POINT('Ctrl Pts',(-18.4649093676713,41.2082133986064,122.236837854703)) ;
#31592 = CARTESIAN_POINT('Ctrl Pts',(-18.6537818070225,41.0282243182436,122.471833474203)) ;
#31593 = CARTESIAN_POINT('Ctrl Pts',(-18.684754038693,41.2182800597728,122.089775689271)) ;
#31594 = CARTESIAN_POINT('Ctrl Pts',(-18.829657944727,41.03829097941,122.354183767872)) ;
#31595 = CARTESIAN_POINT('Ctrl Pts',(-18.922687539533,41.2281702816401,121.985108837478)) ;
#31596 = CARTESIAN_POINT('Ctrl Pts',(-19.0200040932344,41.0481812012773,122.270450887395)) ;
#31597 = CARTESIAN_POINT('Ctrl Pts',(-19.1775992382533,41.2381624577503,121.922160157756)) ;
#31598 = CARTESIAN_POINT('Ctrl Pts',(-19.223933319871,41.0581733773874,122.22009212209)) ;
#31599 = CARTESIAN_POINT('Ctrl Pts',(-19.4388247420797,41.2481252878629,121.904728591906)) ;
#31600 = CARTESIAN_POINT('Ctrl Pts',(-19.4329133725897,41.0681362075001,122.206147099364)) ;
#31601 = CARTESIAN_POINT('Ctrl Pts',(-19.6976771545585,41.2580295002633,121.932097935364)) ;
#31602 = CARTESIAN_POINT('Ctrl Pts',(-19.6399945510564,41.0780404199004,122.228042530922)) ;
#31603 = CARTESIAN_POINT('Ctrl Pts',(-19.9516776747255,41.2680902143511,122.005343143406)) ;
#31604 = CARTESIAN_POINT('Ctrl Pts',(-19.8431952134582,41.0881011339882,122.286638869231)) ;
#31605 = CARTESIAN_POINT('Ctrl Pts',(-20.1841049252899,41.2779297173339,122.118737500505)) ;
#31606 = CARTESIAN_POINT('Ctrl Pts',(-20.0291359487438,41.097940636971,122.377353840953)) ;
#31607 = CARTESIAN_POINT('Ctrl Pts',(-20.3982213435744,41.2879958559003,122.273999666852)) ;
#31608 = CARTESIAN_POINT('Ctrl Pts',(-20.2004293795964,41.1080067755374,122.501563713022)) ;
#31609 = CARTESIAN_POINT('Ctrl Pts',(-20.5787589735412,41.2978783703863,122.460739928102)) ;
#31610 = CARTESIAN_POINT('Ctrl Pts',(-20.3448588816564,41.1178892900235,122.650955244937)) ;
#31611 = CARTESIAN_POINT('Ctrl Pts',(-20.7261276816334,41.3078706697419,122.678026456324)) ;
#31612 = CARTESIAN_POINT('Ctrl Pts',(-20.4627538900193,41.127881589379,122.82478422743)) ;
#31613 = CARTESIAN_POINT('Ctrl Pts',(-20.8332007283246,41.3178237366953,122.916705335846)) ;
#31614 = CARTESIAN_POINT('Ctrl Pts',(-20.5484123254759,41.1378346563324,123.01572688204)) ;
#31615 = CARTESIAN_POINT('Ctrl Pts',(-20.8976084793145,41.3278584449005,123.172399737523)) ;
#31616 = CARTESIAN_POINT('Ctrl Pts',(-20.5999387072137,41.1478693645376,123.220282482398)) ;
#31617 = CARTESIAN_POINT('Ctrl Pts',(-20.9165553817096,41.3377466658047,123.431576287923)) ;
#31618 = CARTESIAN_POINT('Ctrl Pts',(-20.6150963672015,41.1577575854418,123.427622853528)) ;
#31619 = CARTESIAN_POINT('Ctrl Pts',(-20.8903621464779,41.3477410888351,123.692895458737)) ;
#31620 = CARTESIAN_POINT('Ctrl Pts',(-20.5941421044658,41.1677520084722,123.636678055488)) ;
#31621 = CARTESIAN_POINT('Ctrl Pts',(-20.8194388311831,41.3576864282813,123.944442205965)) ;
#31622 = CARTESIAN_POINT('Ctrl Pts',(-20.5374038559839,41.1776973479184,123.837915073439)) ;
#31623 = CARTESIAN_POINT('Ctrl Pts',(-20.7063724848582,41.3676337728926,124.180145089931)) ;
#31624 = CARTESIAN_POINT('Ctrl Pts',(-20.446951356585,41.1876446925297,124.026477147799)) ;
#31625 = CARTESIAN_POINT('Ctrl Pts',(-20.5523289698857,41.3776816683036,124.394591659)) ;
#31626 = CARTESIAN_POINT('Ctrl Pts',(-20.3237167077923,41.1976925879407,124.198034766973)) ;
#31627 = CARTESIAN_POINT('Ctrl Pts',(-20.3673015896202,41.387529313783,124.575522794134)) ;
#31628 = CARTESIAN_POINT('Ctrl Pts',(-20.1756958838239,41.2075402334201,124.342779178533)) ;
#31629 = CARTESIAN_POINT('Ctrl Pts',(-20.1516704586702,41.397491027697,124.723938642442)) ;
#31630 = CARTESIAN_POINT('Ctrl Pts',(-20.0031916223503,41.2175019473341,124.461512149995)) ;
#31631 = CARTESIAN_POINT('Ctrl Pts',(-19.911780850099,41.4075196519879,124.833098044345)) ;
#31632 = CARTESIAN_POINT('Ctrl Pts',(-19.8112800810594,41.227530571625,124.548840178017)) ;
#31633 = CARTESIAN_POINT('Ctrl Pts',(-19.6596394073023,41.4174300126446,124.898243770015)) ;
#31634 = CARTESIAN_POINT('Ctrl Pts',(-19.6095677408918,41.2374409322817,124.600957108251)) ;
#31635 = CARTESIAN_POINT('Ctrl Pts',(-19.3994113076568,41.4273647112179,124.91935848404)) ;
#31636 = CARTESIAN_POINT('Ctrl Pts',(-19.4013858458597,41.247375630855,124.617849546606)) ;
#31637 = CARTESIAN_POINT('Ctrl Pts',(-19.1367143515178,41.4374065360721,124.894447395017)) ;
#31638 = CARTESIAN_POINT('Ctrl Pts',(-19.1912280682996,41.2574174557092,124.597921306122)) ;
#31639 = CARTESIAN_POINT('Ctrl Pts',(-18.8862194476765,41.4472911098165,124.825610729058)) ;
#31640 = CARTESIAN_POINT('Ctrl Pts',(-18.9908327711166,41.2673020294536,124.542852873517)) ;
#31641 = CARTESIAN_POINT('Ctrl Pts',(-18.6486170762246,41.4572929591797,124.713315149718)) ;
#31642 = CARTESIAN_POINT('Ctrl Pts',(-18.8007506471708,41.2773038788168,124.45301716696)) ;
#31643 = CARTESIAN_POINT('Ctrl Pts',(-18.4357242323319,41.4672122607537,124.562839022651)) ;
#31644 = CARTESIAN_POINT('Ctrl Pts',(-18.6304363934291,41.2872231803909,124.332637291821)) ;
#31645 = CARTESIAN_POINT('Ctrl Pts',(-18.2499195837942,41.477256369099,124.375398346987)) ;
#31646 = CARTESIAN_POINT('Ctrl Pts',(-18.4817919703577,41.2972672887361,124.182685211504)) ;
#31647 = CARTESIAN_POINT('Ctrl Pts',(-18.1017911287502,41.4871407925413,124.162007655832)) ;
#31648 = CARTESIAN_POINT('Ctrl Pts',(-18.3632889812558,41.3071517121784,124.011973815533)) ;
#31649 = CARTESIAN_POINT('Ctrl Pts',(-17.9909819762134,41.4971571544507,123.923238127084)) ;
#31650 = CARTESIAN_POINT('Ctrl Pts',(-18.27464077142,41.3171680740879,123.820958606205)) ;
#31651 = CARTESIAN_POINT('Ctrl Pts',(-17.9238542028585,41.5071938099561,123.66818572458)) ;
#31652 = CARTESIAN_POINT('Ctrl Pts',(-18.2209377383296,41.3272047295932,123.616916796119)) ;
#31653 = CARTESIAN_POINT('Ctrl Pts',(-17.9017753134138,41.5170239401454,123.410773438911)) ;
#31654 = CARTESIAN_POINT('Ctrl Pts',(-18.2032737428897,41.3370348597826,123.410988188349)) ;
#31655 = CARTESIAN_POINT('Ctrl Pts',(-17.9252038428856,41.5270999932353,123.147075094843)) ;
#31656 = CARTESIAN_POINT('Ctrl Pts',(-18.2220155951886,41.3471109128724,123.2000290831)) ;
#31657 = CARTESIAN_POINT('Ctrl Pts',(-17.9924242809587,41.5369522224211,122.896990000681)) ;
#31658 = CARTESIAN_POINT('Ctrl Pts',(-18.2757906890744,41.3569631420582,122.999961690913)) ;
#31659 = CARTESIAN_POINT('Ctrl Pts',(-18.1042623444851,41.5470254302204,122.657109249406)) ;
#31660 = CARTESIAN_POINT('Ctrl Pts',(-18.3652602896576,41.3670363498575,122.808056339764)) ;
#31661 = CARTESIAN_POINT('Ctrl Pts',(-18.2526543868681,41.5568669415718,122.445270485562)) ;
#31662 = CARTESIAN_POINT('Ctrl Pts',(-18.4839724495599,41.3768778612089,122.638585568541)) ;
#31663 = CARTESIAN_POINT('Ctrl Pts',(-18.4370777102109,41.5668278796093,122.259519138152)) ;
#31664 = CARTESIAN_POINT('Ctrl Pts',(-18.6315099644499,41.3868387992465,122.489983811783)) ;
#31665 = CARTESIAN_POINT('Ctrl Pts',(-18.6529080737898,41.5768657415343,122.107878162832)) ;
#31666 = CARTESIAN_POINT('Ctrl Pts',(-18.804173668292,41.3968766611714,122.368670011063)) ;
#31667 = CARTESIAN_POINT('Ctrl Pts',(-18.8877262423687,41.5867399275314,121.997383365689)) ;
#31668 = CARTESIAN_POINT('Ctrl Pts',(-18.9920269264179,41.4067508471685,122.280273361693)) ;
#31669 = CARTESIAN_POINT('Ctrl Pts',(-19.1430711045837,41.5968100871093,121.928030886543)) ;
#31670 = CARTESIAN_POINT('Ctrl Pts',(-19.1963027525332,41.4168210067464,122.22479007538)) ;
#31671 = CARTESIAN_POINT('Ctrl Pts',(-19.4003882644743,41.6066418345351,121.904466477439)) ;
#31672 = CARTESIAN_POINT('Ctrl Pts',(-19.4021553376179,41.4266527541722,122.205937341054)) ;
#31673 = CARTESIAN_POINT('Ctrl Pts',(-19.6632563157754,41.6166779146064,121.925697979521)) ;
#31674 = CARTESIAN_POINT('Ctrl Pts',(-19.6124499841248,41.4366888342435,122.222921102434)) ;
#31675 = CARTESIAN_POINT('Ctrl Pts',(-19.9178188413347,41.6266949614589,121.992773118902)) ;
#31676 = CARTESIAN_POINT('Ctrl Pts',(-19.8161003293912,41.446705881096,122.276579942071)) ;
#31677 = CARTESIAN_POINT('Ctrl Pts',(-20.1538480381938,41.6365772196255,122.10109797781)) ;
#31678 = CARTESIAN_POINT('Ctrl Pts',(-20.0049236160898,41.4565881392626,122.363238243392)) ;
#31679 = CARTESIAN_POINT('Ctrl Pts',(-20.3699075386073,41.6465649024218,122.250068895617)) ;
#31680 = CARTESIAN_POINT('Ctrl Pts',(-20.1777719215884,41.466575822059,122.482413671685)) ;
#31681 = CARTESIAN_POINT('Ctrl Pts',(-20.556247785553,41.6565115591386,122.433432011487)) ;
#31682 = CARTESIAN_POINT('Ctrl Pts',(-20.3268449195173,41.4765224787757,122.629102830338)) ;
#31683 = CARTESIAN_POINT('Ctrl Pts',(-20.7093408277522,41.6665686172188,122.648828544842)) ;
#31684 = CARTESIAN_POINT('Ctrl Pts',(-20.4493206451329,41.4865795368559,122.801419352681)) ;
#31685 = CARTESIAN_POINT('Ctrl Pts',(-20.8203574276063,41.6763867967682,122.881750559428)) ;
#31686 = CARTESIAN_POINT('Ctrl Pts',(-20.5381348730655,41.4963977164053,122.987755393131)) ;
#31687 = CARTESIAN_POINT('Ctrl Pts',(-20.8914554133569,41.6864227312072,123.135713115928)) ;
#31688 = CARTESIAN_POINT('Ctrl Pts',(-20.5950148896598,41.5064336508443,123.190925073507)) ;
#31689 = CARTESIAN_POINT('Ctrl Pts',(-20.9165972820437,41.6964473856362,123.397957733958)) ;
#31690 = CARTESIAN_POINT('Ctrl Pts',(-20.6151299031663,41.5164583052733,123.400720641268)) ;
#31691 = CARTESIAN_POINT('Ctrl Pts',(-20.8967522553727,41.7062994052157,123.656101312759)) ;
#31692 = CARTESIAN_POINT('Ctrl Pts',(-20.5992555699789,41.5263103248528,123.607234825418)) ;
#31693 = CARTESIAN_POINT('Ctrl Pts',(-20.8318758704315,41.7162903189306,123.910477841226)) ;
#31694 = CARTESIAN_POINT('Ctrl Pts',(-20.5473561475517,41.5363012385678,123.810736336764)) ;
#31695 = CARTESIAN_POINT('Ctrl Pts',(-20.7247343585358,41.7262083077702,124.148106422392)) ;
#31696 = CARTESIAN_POINT('Ctrl Pts',(-20.4616447029852,41.5462192274073,124.000839496386)) ;
#31697 = CARTESIAN_POINT('Ctrl Pts',(-20.5764123274112,41.736236418501,124.365906529172)) ;
#31698 = CARTESIAN_POINT('Ctrl Pts',(-20.3429885028579,41.5562473381381,124.175080585433)) ;
#31699 = CARTESIAN_POINT('Ctrl Pts',(-20.395206571467,41.7461216164094,124.552049981452)) ;
#31700 = CARTESIAN_POINT('Ctrl Pts',(-20.1980255691353,41.5661325360465,124.323996153329)) ;
#31701 = CARTESIAN_POINT('Ctrl Pts',(-20.1825881915492,41.7561108916774,124.706022484706)) ;
#31702 = CARTESIAN_POINT('Ctrl Pts',(-20.0279320600952,41.5761218113145,124.447175591284)) ;
#31703 = CARTESIAN_POINT('Ctrl Pts',(-19.944994054816,41.7661523498469,124.820818389465)) ;
#31704 = CARTESIAN_POINT('Ctrl Pts',(-19.837857454139,41.586163269484,124.539013942928)) ;
#31705 = CARTESIAN_POINT('Ctrl Pts',(-19.6965012965203,41.7759838136352,124.891575936423)) ;
#31706 = CARTESIAN_POINT('Ctrl Pts',(-19.6390644965111,41.5959947332723,124.595621546985)) ;
#31707 = CARTESIAN_POINT('Ctrl Pts',(-19.4350641759092,41.7859887459391,124.919157369809)) ;
#31708 = CARTESIAN_POINT('Ctrl Pts',(-19.4299150640357,41.6059996655762,124.61768861319)) ;
#31709 = CARTESIAN_POINT('Ctrl Pts',(-19.1732294916453,41.7959751098338,124.900811143185)) ;
#31710 = CARTESIAN_POINT('Ctrl Pts',(-19.2204473105258,41.615986029471,124.603013545684)) ;
#31711 = CARTESIAN_POINT('Ctrl Pts',(-18.9175714408772,41.8060047387197,124.836821562451)) ;
#31712 = CARTESIAN_POINT('Ctrl Pts',(-19.0159203902611,41.6260156583568,124.551823702806)) ;
#31713 = CARTESIAN_POINT('Ctrl Pts',(-18.6804315219461,41.8158799608281,124.731353527358)) ;
#31714 = CARTESIAN_POINT('Ctrl Pts',(-18.8262081643028,41.6358908804652,124.467451255553)) ;
#31715 = CARTESIAN_POINT('Ctrl Pts',(-18.4623421036418,41.8258811732252,124.584757637499)) ;
#31716 = CARTESIAN_POINT('Ctrl Pts',(-18.6517356019732,41.6458920928623,124.350176231393)) ;
#31717 = CARTESIAN_POINT('Ctrl Pts',(-18.2745387790295,41.8357897524607,124.404326737909)) ;
#31718 = CARTESIAN_POINT('Ctrl Pts',(-18.5014918287593,41.6558006720979,124.205833218676)) ;
#31719 = CARTESIAN_POINT('Ctrl Pts',(-18.1187665880947,41.8458446050167,124.190948411598)) ;
#31720 = CARTESIAN_POINT('Ctrl Pts',(-18.3768724125768,41.6658555246539,124.035131662587)) ;
#31721 = CARTESIAN_POINT('Ctrl Pts',(-18.0043751834666,41.8557031872915,123.958446111396)) ;
#31722 = CARTESIAN_POINT('Ctrl Pts',(-18.2853576981926,41.6757141069286,123.849131183936)) ;
#31723 = CARTESIAN_POINT('Ctrl Pts',(-17.93042449407,41.8657713167342,123.70445148532)) ;
#31724 = CARTESIAN_POINT('Ctrl Pts',(-18.2261951440607,41.6857822363713,123.645935938738)) ;
#31725 = CARTESIAN_POINT('Ctrl Pts',(-17.9023200741687,41.8756267884233,123.446967189866)) ;
#31726 = CARTESIAN_POINT('Ctrl Pts',(-18.2037096291495,41.6956377080604,123.439949220456)) ;
#31727 = CARTESIAN_POINT('Ctrl Pts',(-17.9188032302922,41.8856216368096,123.184839420313)) ;
#31728 = CARTESIAN_POINT('Ctrl Pts',(-18.2168940227441,41.7056325564467,123.23024695042)) ;
#31729 = CARTESIAN_POINT('Ctrl Pts',(-17.9813304619599,41.895652933594,122.928744998837)) ;
#31730 = CARTESIAN_POINT('Ctrl Pts',(-18.2669137962854,41.7156638532311,123.025370923546)) ;
#31731 = CARTESIAN_POINT('Ctrl Pts',(-18.0852555186611,41.9055194698041,122.691192079478)) ;
#31732 = CARTESIAN_POINT('Ctrl Pts',(-18.3500517412046,41.7255303894412,122.835328118647)) ;
#31733 = CARTESIAN_POINT('Ctrl Pts',(-18.2302333322929,41.9155068927649,122.472444933182)) ;
#31734 = CARTESIAN_POINT('Ctrl Pts',(-18.4660321429773,41.7355178124021,122.66032929391)) ;
#31735 = CARTESIAN_POINT('Ctrl Pts',(-18.4101690101242,41.9254518317847,122.282861709824)) ;
#31736 = CARTESIAN_POINT('Ctrl Pts',(-18.6099789904463,41.7454627514218,122.508661363733)) ;
#31737 = CARTESIAN_POINT('Ctrl Pts',(-18.6224325374237,41.9354967176447,122.125972345834)) ;
#31738 = CARTESIAN_POINT('Ctrl Pts',(-18.7797885429512,41.7555076372818,122.38314813357)) ;
#31739 = CARTESIAN_POINT('Ctrl Pts',(-18.8545248231622,41.9453652527309,122.010250360349)) ;
#31740 = CARTESIAN_POINT('Ctrl Pts',(-18.9654611095548,41.7653761723681,122.290568757108)) ;
#31741 = CARTESIAN_POINT('Ctrl Pts',(-19.1054113849967,41.9553311207376,121.935164518734)) ;
#31742 = CARTESIAN_POINT('Ctrl Pts',(-19.1661696157605,41.7753420403747,122.230497995113)) ;
#31743 = CARTESIAN_POINT('Ctrl Pts',(-19.3670697024523,41.9653537681901,121.904899528248)) ;
#31744 = CARTESIAN_POINT('Ctrl Pts',(-19.3754959860251,41.7853646878272,122.206283828786)) ;
#31745 = CARTESIAN_POINT('Ctrl Pts',(-19.6273839317657,41.9752774071977,121.920298317369)) ;
#31746 = CARTESIAN_POINT('Ctrl Pts',(-19.583747310097,41.7952883268348,122.218600653541)) ;
#31747 = CARTESIAN_POINT('Ctrl Pts',(-19.8817304496807,41.9852201322034,121.980174899417)) ;
#31748 = CARTESIAN_POINT('Ctrl Pts',(-19.7872249056599,41.8052310518406,122.266499716191)) ;
#31749 = CARTESIAN_POINT('Ctrl Pts',(-20.1241484576752,41.9952657382553,122.084651122132)) ;
#31750 = CARTESIAN_POINT('Ctrl Pts',(-19.9811601739826,41.8152766578924,122.350078652144)) ;
#31751 = CARTESIAN_POINT('Ctrl Pts',(-20.3408862916986,42.0051271607764,122.22675611249)) ;
#31752 = CARTESIAN_POINT('Ctrl Pts',(-20.1545514860313,41.8251380804135,122.463760663456)) ;
#31753 = CARTESIAN_POINT('Ctrl Pts',(-20.5324507967766,42.0151207292256,122.406346888385)) ;
#31754 = CARTESIAN_POINT('Ctrl Pts',(-20.3078045818973,41.8351316488627,122.607431606924)) ;
#31755 = CARTESIAN_POINT('Ctrl Pts',(-20.6890036597013,42.0250461999809,122.615019061482)) ;
#31756 = CARTESIAN_POINT('Ctrl Pts',(-20.4330486091548,41.845057119618,122.774367895725)) ;
#31757 = CARTESIAN_POINT('Ctrl Pts',(-20.808139363818,42.0350738739368,122.850031069966)) ;
#31758 = CARTESIAN_POINT('Ctrl Pts',(-20.528359143158,41.8550847935739,122.962376508046)) ;
#31759 = CARTESIAN_POINT('Ctrl Pts',(-20.8838479741626,42.0449610519785,123.098617303755)) ;
#31760 = CARTESIAN_POINT('Ctrl Pts',(-20.5889282071218,41.8649719716156,123.161244495286)) ;
#31761 = CARTESIAN_POINT('Ctrl Pts',(-20.9158670631571,42.0549894313466,123.360164459768)) ;
#31762 = CARTESIAN_POINT('Ctrl Pts',(-20.6145455234739,41.8750003509838,123.370482841574)) ;
#31763 = CARTESIAN_POINT('Ctrl Pts',(-20.9023097751863,42.0648836740681,123.619854631483)) ;
#31764 = CARTESIAN_POINT('Ctrl Pts',(-20.6037026459315,41.8848945937052,123.578231501373)) ;
#31765 = CARTESIAN_POINT('Ctrl Pts',(-20.8237470249053,42.078236590719,123.961816174747)) ;
#31766 = CARTESIAN_POINT('Ctrl Pts',(-20.540851905552,41.8982475103561,123.851818955548)) ;
#31767 = CARTESIAN_POINT('Ctrl Pts',(-20.6595997814835,42.0914391084657,124.272009590654)) ;
#31768 = CARTESIAN_POINT('Ctrl Pts',(-20.4095171791971,41.9114500281029,124.099990022592)) ;
#31769 = CARTESIAN_POINT('Ctrl Pts',(-20.4209837962718,42.1047950137467,124.529355053645)) ;
#31770 = CARTESIAN_POINT('Ctrl Pts',(-20.2186534466242,41.9248059333838,124.305833005313)) ;
#31771 = CARTESIAN_POINT('Ctrl Pts',(-20.2138409514704,42.1146916623845,124.686668820964)) ;
#31772 = CARTESIAN_POINT('Ctrl Pts',(-20.0529350989336,41.9347025820217,124.431692934571)) ;
#31773 = CARTESIAN_POINT('Ctrl Pts',(-19.9790784982733,42.124739800437,124.807498749042)) ;
#31774 = CARTESIAN_POINT('Ctrl Pts',(-19.8651277057987,41.9447507200741,124.528356915192)) ;
#31775 = CARTESIAN_POINT('Ctrl Pts',(-19.7308134332186,42.1346307606148,124.884508092935)) ;
#31776 = CARTESIAN_POINT('Ctrl Pts',(-19.6665158148451,41.9546416802519,124.589967046328)) ;
#31777 = CARTESIAN_POINT('Ctrl Pts',(-19.4703782998092,42.1446235964915,124.918232356421)) ;
#31778 = CARTESIAN_POINT('Ctrl Pts',(-19.4581682824578,41.9646345161287,124.616948547809)) ;
#31779 = CARTESIAN_POINT('Ctrl Pts',(-19.2068788945409,42.1546626914931,124.905562765929)) ;
#31780 = CARTESIAN_POINT('Ctrl Pts',(-19.2473681313206,41.9746736111302,124.606814984764)) ;
#31781 = CARTESIAN_POINT('Ctrl Pts',(-18.9545800921988,42.1645000473443,124.849083179674)) ;
#31782 = CARTESIAN_POINT('Ctrl Pts',(-19.0455306742898,41.9845109669814,124.56163402756)) ;
#31783 = CARTESIAN_POINT('Ctrl Pts',(-18.629663451881,42.177892995275,124.713940021359)) ;
#31784 = CARTESIAN_POINT('Ctrl Pts',(-18.7855850543186,41.9979039149121,124.453519158685)) ;
#31785 = CARTESIAN_POINT('Ctrl Pts',(-18.3520925365356,42.1910596717019,124.500678451702)) ;
#31786 = CARTESIAN_POINT('Ctrl Pts',(-18.5635083043611,42.0110705913391,124.282885722299)) ;
#31787 = CARTESIAN_POINT('Ctrl Pts',(-18.1378563760038,42.2044444531087,124.221781306289)) ;
#31788 = CARTESIAN_POINT('Ctrl Pts',(-18.3921499280378,42.0244553727458,124.059804293663)) ;
#31789 = CARTESIAN_POINT('Ctrl Pts',(-18.0179616237773,42.2143062357526,123.991978653527)) ;
#31790 = CARTESIAN_POINT('Ctrl Pts',(-18.2962255485433,42.0343171553897,123.875955881791)) ;
#31791 = CARTESIAN_POINT('Ctrl Pts',(-17.9383202716689,42.2243053837056,123.741625973935)) ;
#31792 = CARTESIAN_POINT('Ctrl Pts',(-18.2325120682241,42.0443163033428,123.675676550641)) ;
#31793 = CARTESIAN_POINT('Ctrl Pts',(-17.9034419632737,42.2342081763227,123.483683307464)) ;
#31794 = CARTESIAN_POINT('Ctrl Pts',(-18.2046075051605,42.0542190959598,123.469320792753)) ;
#31795 = CARTESIAN_POINT('Ctrl Pts',(-17.9141036164672,42.2442577562136,123.21987047093)) ;
#31796 = CARTESIAN_POINT('Ctrl Pts',(-18.2131325074826,42.0642686758508,123.258274986974)) ;
#31797 = CARTESIAN_POINT('Ctrl Pts',(-17.9873542558445,42.2574448300231,122.881031053165)) ;
#31798 = CARTESIAN_POINT('Ctrl Pts',(-18.2717422460334,42.0774557496602,122.987181397706)) ;
#31799 = CARTESIAN_POINT('Ctrl Pts',(-18.1910268972478,42.2741976199943,122.48527825742)) ;
#31800 = CARTESIAN_POINT('Ctrl Pts',(-18.4346521928802,42.0942085396314,122.670610268033)) ;
#31801 = CARTESIAN_POINT('Ctrl Pts',(-18.5127023287359,42.290686272089,122.187393477367)) ;
#31802 = CARTESIAN_POINT('Ctrl Pts',(-18.6920409981402,42.1106971917261,122.432258549758)) ;
#31803 = CARTESIAN_POINT('Ctrl Pts',(-18.8227825349679,42.3040430982724,122.023091316242)) ;
#31804 = CARTESIAN_POINT('Ctrl Pts',(-18.9400618893494,42.1240540179095,122.300845856215)) ;
#31805 = CARTESIAN_POINT('Ctrl Pts',(-19.0702507619016,42.3139394831503,121.942948929694)) ;
#31806 = CARTESIAN_POINT('Ctrl Pts',(-19.1380453748036,42.1339504027875,122.236723914257)) ;
#31807 = CARTESIAN_POINT('Ctrl Pts',(-19.3305991665012,42.3239459976708,121.906474651851)) ;
#31808 = CARTESIAN_POINT('Ctrl Pts',(-19.3463190360728,42.1439569173079,122.2075435789)) ;
#31809 = CARTESIAN_POINT('Ctrl Pts',(-19.6771578660426,42.3371361211872,121.917859655171)) ;
#31810 = CARTESIAN_POINT('Ctrl Pts',(-19.623580039702,42.1571470408243,122.216652401464)) ;
#31811 = CARTESIAN_POINT('Ctrl Pts',(-20.1032957575407,42.3539026823368,122.047670197675)) ;
#31812 = CARTESIAN_POINT('Ctrl Pts',(-19.9644762057803,42.1739136019739,122.320493865006)) ;
#31813 = CARTESIAN_POINT('Ctrl Pts',(-20.5238873611168,42.3736871710448,122.363526341007)) ;
#31814 = CARTESIAN_POINT('Ctrl Pts',(-20.3009572541404,42.1936980906819,122.573177890101)) ;
#31815 = CARTESIAN_POINT('Ctrl Pts',(-20.8150059840566,42.3936326186413,122.806396279347)) ;
#31816 = CARTESIAN_POINT('Ctrl Pts',(-20.5338537200683,42.2136435382784,122.927472140951)) ;
#31817 = CARTESIAN_POINT('Ctrl Pts',(-20.9368565339894,42.4135442807972,123.32140844695)) ;
#31818 = CARTESIAN_POINT('Ctrl Pts',(-20.6313376522247,42.2335552004343,123.33948182386)) ;
#31819 = CARTESIAN_POINT('Ctrl Pts',(-20.8768601174002,42.4334364728161,123.846776921239)) ;
#31820 = CARTESIAN_POINT('Ctrl Pts',(-20.583342978862,42.2534473924532,123.759777675271)) ;
#31821 = CARTESIAN_POINT('Ctrl Pts',(-20.6387749464663,42.4534776033707,124.323184054214)) ;
#31822 = CARTESIAN_POINT('Ctrl Pts',(-20.3928775130821,42.2734885230078,124.140904294275)) ;
#31823 = CARTESIAN_POINT('Ctrl Pts',(-20.2567515623942,42.4732959379863,124.686015098705)) ;
#31824 = CARTESIAN_POINT('Ctrl Pts',(-20.087259484934,42.2933068576234,124.431172000379)) ;
#31825 = CARTESIAN_POINT('Ctrl Pts',(-19.7707111217134,42.4932685032059,124.899002007876)) ;
#31826 = CARTESIAN_POINT('Ctrl Pts',(-19.6984277079127,42.313279422843,124.601563631414)) ;
#31827 = CARTESIAN_POINT('Ctrl Pts',(-19.2430064355605,42.5131577193775,124.933361056965)) ;
#31828 = CARTESIAN_POINT('Ctrl Pts',(-19.2762631018856,42.3331686390146,124.629052843148)) ;
#31829 = CARTESIAN_POINT('Ctrl Pts',(-18.7322443545962,42.5331812937002,124.784326245752)) ;
#31830 = CARTESIAN_POINT('Ctrl Pts',(-18.8676531273989,42.3531922133373,124.509826918718)) ;
#31831 = CARTESIAN_POINT('Ctrl Pts',(-18.3074466869106,42.5529784567885,124.473672881631)) ;
#31832 = CARTESIAN_POINT('Ctrl Pts',(-18.5278123342791,42.3729893764256,124.261304267751)) ;
#31833 = CARTESIAN_POINT('Ctrl Pts',(-18.0107152101051,42.5729439506122,124.03387590139)) ;
#31834 = CARTESIAN_POINT('Ctrl Pts',(-18.2904261458476,42.3929548702494,123.909466818997)) ;
#31835 = CARTESIAN_POINT('Ctrl Pts',(-17.8825244705871,42.5928976583536,123.51911914368)) ;
#31836 = CARTESIAN_POINT('Ctrl Pts',(-18.1878724815504,42.4129085779908,123.497661231514)) ;
#31837 = CARTESIAN_POINT('Ctrl Pts',(-17.9375074674537,42.6128050350802,122.992998485349)) ;
#31838 = CARTESIAN_POINT('Ctrl Pts',(-18.2318581752466,42.4328159547174,123.076763483073)) ;
#31839 = CARTESIAN_POINT('Ctrl Pts',(-18.1669062692067,42.6326572466288,122.517738273591)) ;
#31840 = CARTESIAN_POINT('Ctrl Pts',(-18.4153780968803,42.4526681662659,122.696553635092)) ;
#31841 = CARTESIAN_POINT('Ctrl Pts',(-18.5491943143349,42.6527296335745,122.145651577482)) ;
#31842 = CARTESIAN_POINT('Ctrl Pts',(-18.721207849793,42.4727405532116,122.398884952664)) ;
#31843 = CARTESIAN_POINT('Ctrl Pts',(-19.0301333322148,42.6725675032148,121.929544757103)) ;
#31844 = CARTESIAN_POINT('Ctrl Pts',(-19.1059609684924,42.4925784228519,122.225998529547)) ;
#31845 = CARTESIAN_POINT('Ctrl Pts',(-19.5561067931665,42.6924181577679,121.88822002276)) ;
#31846 = CARTESIAN_POINT('Ctrl Pts',(-19.5267415619836,42.5124290774051,122.19293977911)) ;
#31847 = CARTESIAN_POINT('Ctrl Pts',(-20.0695211678143,42.7124700921084,122.031029897398)) ;
#31848 = CARTESIAN_POINT('Ctrl Pts',(-19.9374722246251,42.5324810117455,122.307188485913)) ;
#31849 = CARTESIAN_POINT('Ctrl Pts',(-20.4987389792293,42.7323032796744,122.33724488066)) ;
#31850 = CARTESIAN_POINT('Ctrl Pts',(-20.2808472827428,42.5523141993116,122.552162457419)) ;
#31851 = CARTESIAN_POINT('Ctrl Pts',(-20.7998323714999,42.7522324919051,122.772792578482)) ;
#31852 = CARTESIAN_POINT('Ctrl Pts',(-20.5217209763658,42.5722434115422,122.900602245168)) ;
#31853 = CARTESIAN_POINT('Ctrl Pts',(-20.9346324231233,42.7721174571195,123.284031475315)) ;
#31854 = CARTESIAN_POINT('Ctrl Pts',(-20.6295592175581,42.5921283767566,123.309594871732)) ;
#31855 = CARTESIAN_POINT('Ctrl Pts',(-20.8856369561692,42.7921911982641,123.815196128951)) ;
#31856 = CARTESIAN_POINT('Ctrl Pts',(-20.5903609317186,42.6122021179012,123.734525730611)) ;
#31857 = CARTESIAN_POINT('Ctrl Pts',(-20.6614795251124,42.8119843800445,124.291210805294)) ;
#31858 = CARTESIAN_POINT('Ctrl Pts',(-20.4110322484531,42.6319952996816,124.115338243655)) ;
#31859 = CARTESIAN_POINT('Ctrl Pts',(-20.2863715695943,42.8319470880472,124.666388958395)) ;
#31860 = CARTESIAN_POINT('Ctrl Pts',(-20.1109437039454,42.6519580076843,124.415478939255)) ;
#31861 = CARTESIAN_POINT('Ctrl Pts',(-19.8046741907438,42.8519300397896,124.890126754003)) ;
#31862 = CARTESIAN_POINT('Ctrl Pts',(-19.7255846106919,42.6719409594268,124.594466924686)) ;
#31863 = CARTESIAN_POINT('Ctrl Pts',(-19.2801592562473,42.8717406595618,124.936699673532)) ;
#31864 = CARTESIAN_POINT('Ctrl Pts',(-19.3059710215937,42.6917515791989,124.631722408354)) ;
#31865 = CARTESIAN_POINT('Ctrl Pts',(-18.7667862152892,42.8917243755947,124.800954951219)) ;
#31866 = CARTESIAN_POINT('Ctrl Pts',(-18.8952733417193,42.7117352952318,124.523123451149)) ;
#31867 = CARTESIAN_POINT('Ctrl Pts',(-18.3326279856665,42.911605839492,124.499507379797)) ;
#31868 = CARTESIAN_POINT('Ctrl Pts',(-18.5479481189047,42.7316167591292,124.281962249473)) ;
#31869 = CARTESIAN_POINT('Ctrl Pts',(-18.0260984755986,42.9315611693364,124.066807185146)) ;
#31870 = CARTESIAN_POINT('Ctrl Pts',(-18.3027271574083,42.7515720889735,123.935799951114)) ;
#31871 = CARTESIAN_POINT('Ctrl Pts',(-17.8857662260403,42.9514366301419,123.557444062347)) ;
#31872 = CARTESIAN_POINT('Ctrl Pts',(-18.1904651245614,42.771447549779,123.528307551792)) ;
#31873 = CARTESIAN_POINT('Ctrl Pts',(-17.9275815086194,42.9714209501934,123.027999899649)) ;
#31874 = CARTESIAN_POINT('Ctrl Pts',(-18.2239197641623,42.7914318698305,123.104753757388)) ;
#31875 = CARTESIAN_POINT('Ctrl Pts',(-18.1472767537667,42.991348982983,122.545930346273)) ;
#31876 = CARTESIAN_POINT('Ctrl Pts',(-18.3996848299053,42.8113599026202,122.719094732473)) ;
#31877 = CARTESIAN_POINT('Ctrl Pts',(-18.4563016259536,43.0079577449228,122.230836526374)) ;
#31878 = CARTESIAN_POINT('Ctrl Pts',(-18.6468908763838,42.82796866456,122.467036542162)) ;
#31879 = CARTESIAN_POINT('Ctrl Pts',(-18.7544287787532,43.0211453836129,122.054087877132)) ;
#31880 = CARTESIAN_POINT('Ctrl Pts',(-18.8854094489693,42.84115630325,122.325626725663)) ;
#31881 = CARTESIAN_POINT('Ctrl Pts',(-18.9997521034799,43.031131817973,121.960916807132)) ;
#31882 = CARTESIAN_POINT('Ctrl Pts',(-19.0816631635093,42.8511427376102,122.251094035391)) ;
#31883 = CARTESIAN_POINT('Ctrl Pts',(-19.2581944108813,43.0411411919324,121.911902702877)) ;
#31884 = CARTESIAN_POINT('Ctrl Pts',(-19.2884287994832,42.8611521115695,122.211885725831)) ;
#31885 = CARTESIAN_POINT('Ctrl Pts',(-19.6074202778413,43.0544312254977,121.907165841963)) ;
#31886 = CARTESIAN_POINT('Ctrl Pts',(-19.5677560175321,42.8744421451348,122.208091120847)) ;
#31887 = CARTESIAN_POINT('Ctrl Pts',(-20.0350687767284,43.0710252131601,122.015093622791)) ;
#31888 = CARTESIAN_POINT('Ctrl Pts',(-19.9099409302065,42.8910361327973,122.294450399826)) ;
#31889 = CARTESIAN_POINT('Ctrl Pts',(-20.4010277793674,43.0876574684357,122.26302842487)) ;
#31890 = CARTESIAN_POINT('Ctrl Pts',(-20.2026637544341,42.9076683880728,122.492780756029)) ;
#31891 = CARTESIAN_POINT('Ctrl Pts',(-20.6289019817072,43.1008998521035,122.526052209373)) ;
#31892 = CARTESIAN_POINT('Ctrl Pts',(-20.3849854274242,42.9209107717406,122.70321807601)) ;
#31893 = CARTESIAN_POINT('Ctrl Pts',(-20.7634137015571,43.1108140603309,122.749188831555)) ;
#31894 = CARTESIAN_POINT('Ctrl Pts',(-20.49258810908,42.9308249799681,122.881725181544)) ;
#31895 = CARTESIAN_POINT('Ctrl Pts',(-20.8581936477321,43.1208706996026,122.995865179697)) ;
#31896 = CARTESIAN_POINT('Ctrl Pts',(-20.5684111153363,42.9408816192397,123.079068425544)) ;
#31897 = CARTESIAN_POINT('Ctrl Pts',(-20.9079570487934,43.1307165060227,123.249794573028)) ;
#31898 = CARTESIAN_POINT('Ctrl Pts',(-20.6082199684139,42.9507274256599,123.282209957339)) ;
#31899 = CARTESIAN_POINT('Ctrl Pts',(-20.9134264774939,43.1407615056559,123.513697714177)) ;
#31900 = CARTESIAN_POINT('Ctrl Pts',(-20.6125910612325,42.960772425293,123.493341293603)) ;
#31901 = CARTESIAN_POINT('Ctrl Pts',(-20.8594473356749,43.1540425280286,123.858497845333)) ;
#31902 = CARTESIAN_POINT('Ctrl Pts',(-20.569416250521,42.9740534476658,123.769136972112)) ;
#31903 = CARTESIAN_POINT('Ctrl Pts',(-20.718508196259,43.1672399745533,124.17971260659)) ;
#31904 = CARTESIAN_POINT('Ctrl Pts',(-20.4566616453272,42.9872508941904,124.026134275498)) ;
#31905 = CARTESIAN_POINT('Ctrl Pts',(-20.4978485962577,43.1806542723603,124.454637161235)) ;
#31906 = CARTESIAN_POINT('Ctrl Pts',(-20.2801208442663,43.0006651919974,124.246084216616)) ;
#31907 = CARTESIAN_POINT('Ctrl Pts',(-20.3035425807458,43.190493337763,124.625241624044)) ;
#31908 = CARTESIAN_POINT('Ctrl Pts',(-20.124676701218,43.0105042574002,124.382563655871)) ;
#31909 = CARTESIAN_POINT('Ctrl Pts',(-20.0797235876443,43.2004765440407,124.762051652017)) ;
#31910 = CARTESIAN_POINT('Ctrl Pts',(-19.9456197990869,43.0204874636778,124.492010372349)) ;
#31911 = CARTESIAN_POINT('Ctrl Pts',(-19.8362597616934,43.2104277789535,124.8575472145)) ;
#31912 = CARTESIAN_POINT('Ctrl Pts',(-19.7508481203091,43.0304386985906,124.568404524437)) ;
#31913 = CARTESIAN_POINT('Ctrl Pts',(-19.5786965198764,43.2204287786551,124.909888505183)) ;
#31914 = CARTESIAN_POINT('Ctrl Pts',(-19.544797096,43.0404396982923,124.610275379233)) ;
#31915 = CARTESIAN_POINT('Ctrl Pts',(-19.3151648430061,43.2304601244425,124.916319914135)) ;
#31916 = CARTESIAN_POINT('Ctrl Pts',(-19.3339717561267,43.0504710440796,124.615418233467)) ;
#31917 = CARTESIAN_POINT('Ctrl Pts',(-19.0590709276985,43.2403138891475,124.877945266862)) ;
#31918 = CARTESIAN_POINT('Ctrl Pts',(-19.1290970496758,43.0603248087846,124.584716300181)) ;
#31919 = CARTESIAN_POINT('Ctrl Pts',(-18.8104522663154,43.2502845428158,124.79531472401)) ;
#31920 = CARTESIAN_POINT('Ctrl Pts',(-18.9302029191281,43.0702954624529,124.518609759504)) ;
#31921 = CARTESIAN_POINT('Ctrl Pts',(-18.5792880259183,43.260281786473,124.670397983482)) ;
#31922 = CARTESIAN_POINT('Ctrl Pts',(-18.7452726496911,43.0802927061101,124.418674422827)) ;
#31923 = CARTESIAN_POINT('Ctrl Pts',(-18.3728375783555,43.2703152424172,124.506422572522)) ;
#31924 = CARTESIAN_POINT('Ctrl Pts',(-18.5801137193159,43.0903261620543,124.287492345244)) ;
#31925 = CARTESIAN_POINT('Ctrl Pts',(-18.2007504134058,43.2801707467176,124.31283503278)) ;
#31926 = CARTESIAN_POINT('Ctrl Pts',(-18.4424457883443,43.1001816663547,124.132620965001)) ;
#31927 = CARTESIAN_POINT('Ctrl Pts',(-18.0626456729148,43.2901701830037,124.089333194053)) ;
#31928 = CARTESIAN_POINT('Ctrl Pts',(-18.3319639343597,43.1101811026408,123.953818381161)) ;
#31929 = CARTESIAN_POINT('Ctrl Pts',(-17.9661552350075,43.3000646425196,123.847830753989)) ;
#31930 = CARTESIAN_POINT('Ctrl Pts',(-18.2547737161696,43.1200755621567,123.760615804186)) ;
#31931 = CARTESIAN_POINT('Ctrl Pts',(-17.9122545173091,43.3101277619712,123.588980661551)) ;
#31932 = CARTESIAN_POINT('Ctrl Pts',(-18.2116553113845,43.1301386816084,123.55353524895)) ;
#31933 = CARTESIAN_POINT('Ctrl Pts',(-17.9040100749574,43.3199673963832,123.330493713353)) ;
#31934 = CARTESIAN_POINT('Ctrl Pts',(-18.2050619671359,43.1399783160204,123.346745951152)) ;
#31935 = CARTESIAN_POINT('Ctrl Pts',(-17.9412644855324,43.330030603869,123.068717754911)) ;
#31936 = CARTESIAN_POINT('Ctrl Pts',(-18.2348676608804,43.1500415235061,123.137325455349)) ;
#31937 = CARTESIAN_POINT('Ctrl Pts',(-18.0222521551209,43.3399247112482,122.821614169064)) ;
#31938 = CARTESIAN_POINT('Ctrl Pts',(-18.2996598001454,43.1599356308853,122.939643522461)) ;
#31939 = CARTESIAN_POINT('Ctrl Pts',(-18.1448649357578,43.3498670434406,122.590937416187)) ;
#31940 = CARTESIAN_POINT('Ctrl Pts',(-18.3977518184139,43.1698779630777,122.755103312914)) ;
#31941 = CARTESIAN_POINT('Ctrl Pts',(-18.3065565946206,43.3598676697556,122.383706851709)) ;
#31942 = CARTESIAN_POINT('Ctrl Pts',(-18.5271067799686,43.1798785893927,122.589320225833)) ;
#31943 = CARTESIAN_POINT('Ctrl Pts',(-18.5028573530525,43.3699094040375,122.207385535582)) ;
#31944 = CARTESIAN_POINT('Ctrl Pts',(-18.6841488602168,43.1899203236746,122.448264772866)) ;
#31945 = CARTESIAN_POINT('Ctrl Pts',(-18.7217003533941,43.3797348299866,122.070323331608)) ;
#31946 = CARTESIAN_POINT('Ctrl Pts',(-18.8592239561885,43.1997457496237,122.338617074552)) ;
#31947 = CARTESIAN_POINT('Ctrl Pts',(-18.9664691272905,43.3897916565143,121.970708884775)) ;
#31948 = CARTESIAN_POINT('Ctrl Pts',(-19.0550398228914,43.2098025761514,122.258927422049)) ;
#31949 = CARTESIAN_POINT('Ctrl Pts',(-19.2216018609428,43.3997190896358,121.916174470016)) ;
#31950 = CARTESIAN_POINT('Ctrl Pts',(-19.2591461961739,43.219730009273,122.215302017841)) ;
#31951 = CARTESIAN_POINT('Ctrl Pts',(-19.4828888562582,43.4096690820421,121.905998966867)) ;
#31952 = CARTESIAN_POINT('Ctrl Pts',(-19.4681756430009,43.2296800016792,122.207163663939)) ;
#31953 = CARTESIAN_POINT('Ctrl Pts',(-19.7446216548047,43.4197242831161,121.942178613796)) ;
#31954 = CARTESIAN_POINT('Ctrl Pts',(-19.6775616803327,43.2397352027532,122.236109468103)) ;
#31955 = CARTESIAN_POINT('Ctrl Pts',(-19.9904509322207,43.4295465571684,122.02094445218)) ;
#31956 = CARTESIAN_POINT('Ctrl Pts',(-19.8742238828704,43.2495574768055,122.299123887706)) ;
#31957 = CARTESIAN_POINT('Ctrl Pts',(-20.2244870380784,43.4396024511276,122.143621831466)) ;
#31958 = CARTESIAN_POINT('Ctrl Pts',(-20.0614519256092,43.2596133707647,122.397267588395)) ;
#31959 = CARTESIAN_POINT('Ctrl Pts',(-20.4310096168158,43.4495431729727,122.303608199071)) ;
#31960 = CARTESIAN_POINT('Ctrl Pts',(-20.2266685268885,43.2695540926099,122.525258131967)) ;
#31961 = CARTESIAN_POINT('Ctrl Pts',(-20.6065731184016,43.4594475170593,122.495763120482)) ;
#31962 = CARTESIAN_POINT('Ctrl Pts',(-20.3671176119606,43.2794584366965,122.678983058845)) ;
#31963 = CARTESIAN_POINT('Ctrl Pts',(-20.7479541652507,43.4694941843588,122.718707024721)) ;
#31964 = CARTESIAN_POINT('Ctrl Pts',(-20.4802208409037,43.2895051039959,122.857339300646)) ;
#31965 = CARTESIAN_POINT('Ctrl Pts',(-20.8472092355886,43.4793897428087,122.95911028977)) ;
#31966 = CARTESIAN_POINT('Ctrl Pts',(-20.5596229418343,43.2994006624459,123.049662215042)) ;
#31967 = CARTESIAN_POINT('Ctrl Pts',(-20.904139618028,43.4894518215134,123.217291078424)) ;
#31968 = CARTESIAN_POINT('Ctrl Pts',(-20.6051653985535,43.3094627411505,123.256207403565)) ;
#31969 = CARTESIAN_POINT('Ctrl Pts',(-20.9152824166523,43.4992945199792,123.475736104278)) ;
#31970 = CARTESIAN_POINT('Ctrl Pts',(-20.6140777067984,43.3193054396163,123.462962813021)) ;
#31971 = CARTESIAN_POINT('Ctrl Pts',(-20.8814961280243,43.5092852938737,123.736067222342)) ;
#31972 = CARTESIAN_POINT('Ctrl Pts',(-20.5870468982505,43.3292962135108,123.671227335157)) ;
#31973 = CARTESIAN_POINT('Ctrl Pts',(-20.8034587033046,43.5192131631086,123.985028739388)) ;
#31974 = CARTESIAN_POINT('Ctrl Pts',(-20.5246153423973,43.3392240827457,123.870395633847)) ;
#31975 = CARTESIAN_POINT('Ctrl Pts',(-20.6830540646815,43.5292018920784,124.218293703487)) ;
#31976 = CARTESIAN_POINT('Ctrl Pts',(-20.4282901545074,43.3492128117156,124.057006673629)) ;
#31977 = CARTESIAN_POINT('Ctrl Pts',(-20.5227971110946,43.5392412940622,124.427851205494)) ;
#31978 = CARTESIAN_POINT('Ctrl Pts',(-20.3000830928166,43.3592522136993,124.224651637506)) ;
#31979 = CARTESIAN_POINT('Ctrl Pts',(-20.3327674227349,43.549081461799,124.603250592089)) ;
#31980 = CARTESIAN_POINT('Ctrl Pts',(-20.1480587518174,43.3690923814361,124.36496932946)) ;
#31981 = CARTESIAN_POINT('Ctrl Pts',(-20.1108004287422,43.5591296721735,124.746255706704)) ;
#31982 = CARTESIAN_POINT('Ctrl Pts',(-19.9704841479097,43.3791405918106,124.479372086508)) ;
#31983 = CARTESIAN_POINT('Ctrl Pts',(-19.8696476488821,43.5690768424612,124.84714360705)) ;
#31984 = CARTESIAN_POINT('Ctrl Pts',(-19.7775615548716,43.3890877620984,124.560080670385)) ;
#31985 = CARTESIAN_POINT('Ctrl Pts',(-19.6157403076391,43.5789876907163,124.905179129313)) ;
#31986 = CARTESIAN_POINT('Ctrl Pts',(-19.5744358437637,43.3989986103534,124.606507405916)) ;
#31987 = CARTESIAN_POINT('Ctrl Pts',(-19.3518069355752,43.5890440183941,124.91818859538)) ;
#31988 = CARTESIAN_POINT('Ctrl Pts',(-19.3632888855343,43.4090549380312,124.616913341816)) ;
#31989 = CARTESIAN_POINT('Ctrl Pts',(-19.0949363387433,43.5988944311626,124.886068138014)) ;
#31990 = CARTESIAN_POINT('Ctrl Pts',(-19.1577934324893,43.4189053507997,124.591215484819)) ;
#31991 = CARTESIAN_POINT('Ctrl Pts',(-18.8429401699179,43.6089213169963,124.809086046414)) ;
#31992 = CARTESIAN_POINT('Ctrl Pts',(-18.9561969026727,43.4289322366334,124.529628381766)) ;
#31993 = CARTESIAN_POINT('Ctrl Pts',(-18.608395133658,43.6189499326271,124.688881455388)) ;
#31994 = CARTESIAN_POINT('Ctrl Pts',(-18.7685615614303,43.4389608522643,124.433463244299)) ;
#31995 = CARTESIAN_POINT('Ctrl Pts',(-18.4018522456686,43.6287951560046,124.53309241998)) ;
#31996 = CARTESIAN_POINT('Ctrl Pts',(-18.6033288833992,43.4488060756417,124.308831339944)) ;
#31997 = CARTESIAN_POINT('Ctrl Pts',(-18.2223621198309,43.6387858381062,124.34147662207)) ;
#31998 = CARTESIAN_POINT('Ctrl Pts',(-18.4597378987131,43.4587967577433,124.15553787085)) ;
#31999 = CARTESIAN_POINT('Ctrl Pts',(-18.0786893213183,43.6488237267386,124.120254417819)) ;
#32000 = CARTESIAN_POINT('Ctrl Pts',(-18.344800860244,43.4688346463758,123.97855920037)) ;
#32001 = CARTESIAN_POINT('Ctrl Pts',(-17.977176387725,43.6586680618418,123.882292776737)) ;
#32002 = CARTESIAN_POINT('Ctrl Pts',(-18.2635921771929,43.4786789814789,123.788190198657)) ;
#32003 = CARTESIAN_POINT('Ctrl Pts',(-17.917193628408,43.6686530240393,123.626883148383)) ;
#32004 = CARTESIAN_POINT('Ctrl Pts',(-18.2156072828888,43.4886639436764,123.583862392775)) ;
#32005 = CARTESIAN_POINT('Ctrl Pts',(-17.9024116244684,43.6785919655727,123.366078461576)) ;
#32006 = CARTESIAN_POINT('Ctrl Pts',(-18.2037829771252,43.4986028852098,123.375219006614)) ;
#32007 = CARTESIAN_POINT('Ctrl Pts',(-17.9335320666697,43.6886338505441,123.104055220491)) ;
#32008 = CARTESIAN_POINT('Ctrl Pts',(-18.2286806289882,43.5086447701812,123.165600448032)) ;
#32009 = CARTESIAN_POINT('Ctrl Pts',(-18.008352723709,43.6985203984524,122.855226846736)) ;
#32010 = CARTESIAN_POINT('Ctrl Pts',(-18.2885381427592,43.5185313180895,122.966538824401)) ;
#32011 = CARTESIAN_POINT('Ctrl Pts',(-18.1261385188554,43.7085143239524,122.620528575572)) ;
#32012 = CARTESIAN_POINT('Ctrl Pts',(-18.3827677656657,43.5285252435895,122.778780862316)) ;
#32013 = CARTESIAN_POINT('Ctrl Pts',(-18.2819245676956,43.7184504150789,122.410933846051)) ;
#32014 = CARTESIAN_POINT('Ctrl Pts',(-18.5073972462572,43.538461334716,122.61110613432)) ;
#32015 = CARTESIAN_POINT('Ctrl Pts',(-18.4734970875813,43.7284796840588,122.229979319978)) ;
#32016 = CARTESIAN_POINT('Ctrl Pts',(-18.6606561040544,43.5484906036959,122.466343315554)) ;
#32017 = CARTESIAN_POINT('Ctrl Pts',(-18.6902358432055,43.7383620666181,122.086843147979)) ;
#32018 = CARTESIAN_POINT('Ctrl Pts',(-18.8340470312142,43.5583729862552,122.351835729643)) ;
#32019 = CARTESIAN_POINT('Ctrl Pts',(-18.9325293093004,43.748414583706,121.981687073779)) ;
#32020 = CARTESIAN_POINT('Ctrl Pts',(-19.0278824125168,43.5684255033431,122.267711767066)) ;
#32021 = CARTESIAN_POINT('Ctrl Pts',(-19.1854080916355,43.7583087045299,121.921017634688)) ;
#32022 = CARTESIAN_POINT('Ctrl Pts',(-19.2301849629632,43.578319624167,122.219177394001)) ;
#32023 = CARTESIAN_POINT('Ctrl Pts',(-19.4492993318414,43.7683706839503,121.904850471576)) ;
#32024 = CARTESIAN_POINT('Ctrl Pts',(-19.4412982796223,43.5883816035874,122.2062446672)) ;
#32025 = CARTESIAN_POINT('Ctrl Pts',(-19.7063573702631,43.7782152171792,121.934076663056)) ;
#32026 = CARTESIAN_POINT('Ctrl Pts',(-19.6469435446541,43.5982261368164,122.22962650948)) ;
#32027 = CARTESIAN_POINT('Ctrl Pts',(-19.9576002327423,43.7881752960855,122.007446102476)) ;
#32028 = CARTESIAN_POINT('Ctrl Pts',(-19.8479372613017,43.6081862157226,122.288322719679)) ;
#32029 = CARTESIAN_POINT('Ctrl Pts',(-20.1938925036668,43.7982135726581,122.124695495129)) ;
#32030 = CARTESIAN_POINT('Ctrl Pts',(-20.0369707873508,43.6182244922952,122.382123111982)) ;
#32031 = CARTESIAN_POINT('Ctrl Pts',(-20.403085266942,43.8080869591959,122.278251260109)) ;
#32032 = CARTESIAN_POINT('Ctrl Pts',(-20.2043238013652,43.6280978788331,122.504967832787)) ;
#32033 = CARTESIAN_POINT('Ctrl Pts',(-20.5859442921562,43.818159901963,122.469575837394)) ;
#32034 = CARTESIAN_POINT('Ctrl Pts',(-20.3506106669078,43.6381708216001,122.65802830527)) ;
#32035 = CARTESIAN_POINT('Ctrl Pts',(-20.7294563688574,43.8279813160913,122.684155238316)) ;
#32036 = CARTESIAN_POINT('Ctrl Pts',(-20.4654190257997,43.6479922357285,122.829691205274)) ;
#32037 = CARTESIAN_POINT('Ctrl Pts',(-20.8364643232835,43.8380559461636,122.926263897482)) ;
#32038 = CARTESIAN_POINT('Ctrl Pts',(-20.5510249269012,43.6580668658008,123.023378728422)) ;
#32039 = CARTESIAN_POINT('Ctrl Pts',(-20.8984148212984,43.8479225834805,123.178073112069)) ;
#32040 = CARTESIAN_POINT('Ctrl Pts',(-20.6005844237704,43.6679335031176,123.224825316576)) ;
#32041 = CARTESIAN_POINT('Ctrl Pts',(-20.9166483132866,43.8579461288523,123.440837266538)) ;
#32042 = CARTESIAN_POINT('Ctrl Pts',(-20.6151706983292,43.6779570484894,123.435036712492)) ;
#32043 = CARTESIAN_POINT('Ctrl Pts',(-20.8883395523817,43.8679718803695,123.702794177763)) ;
#32044 = CARTESIAN_POINT('Ctrl Pts',(-20.5925230028488,43.6879828000066,123.644602236926)) ;
#32045 = CARTESIAN_POINT('Ctrl Pts',(-20.8166599479504,43.8778254673789,123.951603594725)) ;
#32046 = CARTESIAN_POINT('Ctrl Pts',(-20.5351790633335,43.697836387016,123.843648589782)) ;
#32047 = CARTESIAN_POINT('Ctrl Pts',(-20.702060923653,43.8878024276068,124.187422142841)) ;
#32048 = CARTESIAN_POINT('Ctrl Pts',(-20.4434995981191,43.7078133472439,124.032303014082)) ;
#32049 = CARTESIAN_POINT('Ctrl Pts',(-20.5472263847729,43.8978235706353,124.400424003541)) ;
#32050 = CARTESIAN_POINT('Ctrl Pts',(-20.3196315437923,43.7178344902724,124.202704210316)) ;
#32051 = CARTESIAN_POINT('Ctrl Pts',(-20.3607073265626,43.9077061766552,124.581187205771)) ;
#32052 = CARTESIAN_POINT('Ctrl Pts',(-20.1704166645511,43.7277170962923,124.34731388807)) ;
#32053 = CARTESIAN_POINT('Ctrl Pts',(-20.141598516524,43.9177746472879,124.729426223139)) ;
#32054 = CARTESIAN_POINT('Ctrl Pts',(-19.9951291156329,43.737785566925,124.465904948293)) ;
#32055 = CARTESIAN_POINT('Ctrl Pts',(-19.9058383854937,43.9276047304716,124.835123522503)) ;
#32056 = CARTESIAN_POINT('Ctrl Pts',(-19.8065220003896,43.7476156501087,124.550461981873)) ;
#32057 = CARTESIAN_POINT('Ctrl Pts',(-19.6494502413749,43.937671290152,124.900110672069)) ;
#32058 = CARTESIAN_POINT('Ctrl Pts',(-19.6014111164167,43.7576822097891,124.602451541965)) ;
#32059 = CARTESIAN_POINT('Ctrl Pts',(-19.3902067493444,43.9475615399812,124.919096378298)) ;
#32060 = CARTESIAN_POINT('Ctrl Pts',(-19.3940171383949,43.7675724596183,124.617639759188)) ;
#32061 = CARTESIAN_POINT('Ctrl Pts',(-19.1289291993489,43.95755370573,124.893086593962)) ;
#32062 = CARTESIAN_POINT('Ctrl Pts',(-19.1849952828708,43.7775646253671,124.59683180778)) ;
#32063 = CARTESIAN_POINT('Ctrl Pts',(-18.8769378575391,43.9675165493261,124.822071866951)) ;
#32064 = CARTESIAN_POINT('Ctrl Pts',(-18.9834026165215,43.7875274689632,124.54001992677)) ;
#32065 = CARTESIAN_POINT('Ctrl Pts',(-18.6421796236828,43.9774207181539,124.709636238937)) ;
#32066 = CARTESIAN_POINT('Ctrl Pts',(-18.7955967231379,43.797431637791,124.450071716623)) ;
#32067 = CARTESIAN_POINT('Ctrl Pts',(-18.4273472596352,43.9874815930482,124.555590382771)) ;
#32068 = CARTESIAN_POINT('Ctrl Pts',(-18.6237306573745,43.8074925126853,124.32683478731)) ;
#32069 = CARTESIAN_POINT('Ctrl Pts',(-18.2462912417937,43.9973204963776,124.370950929424)) ;
#32070 = CARTESIAN_POINT('Ctrl Pts',(-18.4788866747654,43.8173314160147,124.179124065439)) ;
#32071 = CARTESIAN_POINT('Ctrl Pts',(-18.096473040413,44.0073888727515,124.152920066805)) ;
#32072 = CARTESIAN_POINT('Ctrl Pts',(-18.3590318811178,43.8273997923886,124.004699145389)) ;
#32073 = CARTESIAN_POINT('Ctrl Pts',(-17.9888795242822,44.0172694893841,123.916566377132)) ;
#32074 = CARTESIAN_POINT('Ctrl Pts',(-18.2729574087279,43.8372804090212,123.815617033052)) ;
#32075 = CARTESIAN_POINT('Ctrl Pts',(-17.9227396809683,44.0272606496131,123.662515814642)) ;
#32076 = CARTESIAN_POINT('Ctrl Pts',(-18.2200454142358,43.8472715692502,123.612376795175)) ;
#32077 = CARTESIAN_POINT('Ctrl Pts',(-17.9017478866056,44.0372137230452,123.40176367561)) ;
#32078 = CARTESIAN_POINT('Ctrl Pts',(-18.2032518302433,43.8572246426823,123.403775507638)) ;
#32079 = CARTESIAN_POINT('Ctrl Pts',(-17.9266347799871,44.0472495586578,123.139231148737)) ;
#32080 = CARTESIAN_POINT('Ctrl Pts',(-18.2231612008556,43.867260478295,123.193749351306)) ;
#32081 = CARTESIAN_POINT('Ctrl Pts',(-17.9955495886584,44.057139685388,122.888614558069)) ;
#32082 = CARTESIAN_POINT('Ctrl Pts',(-18.2782926266805,43.8771506050251,122.993256851643)) ;
#32083 = CARTESIAN_POINT('Ctrl Pts',(-18.1076878440328,44.0671318671573,122.651194666647)) ;
#32084 = CARTESIAN_POINT('Ctrl Pts',(-18.3680028793089,43.8871427867944,122.803320956342)) ;
#32085 = CARTESIAN_POINT('Ctrl Pts',(-18.2587247866769,44.0770778071318,122.437883820146)) ;
#32086 = CARTESIAN_POINT('Ctrl Pts',(-18.4888319257956,43.8970887267689,122.632672501952)) ;
#32087 = CARTESIAN_POINT('Ctrl Pts',(-18.4441648499972,44.0870249908912,122.253628827194)) ;
#32088 = CARTESIAN_POINT('Ctrl Pts',(-18.6371833541905,43.9070359105284,122.485268533601)) ;
#32089 = CARTESIAN_POINT('Ctrl Pts',(-18.6611045195494,44.0970729291816,122.103115117568)) ;
#32090 = CARTESIAN_POINT('Ctrl Pts',(-18.8107350578741,43.9170838488187,122.364857168353)) ;
#32091 = CARTESIAN_POINT('Ctrl Pts',(-18.8960216519544,44.1069205639951,121.9945561486)) ;
#32092 = CARTESIAN_POINT('Ctrl Pts',(-18.9986675796601,43.9269314836323,122.278010099489)) ;
#32093 = CARTESIAN_POINT('Ctrl Pts',(-19.1488932353645,44.1168822776931,121.926880369107)) ;
#32094 = CARTESIAN_POINT('Ctrl Pts',(-19.200964338225,43.9368931973302,122.223868984643)) ;
#32095 = CARTESIAN_POINT('Ctrl Pts',(-19.4114837782062,44.1269109135143,121.904316948058)) ;
#32096 = CARTESIAN_POINT('Ctrl Pts',(-19.4110368048726,43.9469218331514,122.205817721799)) ;
#32097 = CARTESIAN_POINT('Ctrl Pts',(-19.6708855677709,44.136821228266,121.927328148373)) ;
#32098 = CARTESIAN_POINT('Ctrl Pts',(-19.6185575864657,43.9568321479032,122.224226080018)) ;
#32099 = CARTESIAN_POINT('Ctrl Pts',(-19.923172854028,44.1467560989287,121.994541369525)) ;
#32100 = CARTESIAN_POINT('Ctrl Pts',(-19.8203870878445,43.9667670185658,122.277995832626)) ;
#32101 = CARTESIAN_POINT('Ctrl Pts',(-20.1623656622643,44.1567972813305,122.105936279633)) ;
#32102 = CARTESIAN_POINT('Ctrl Pts',(-20.011741745876,43.9768082009676,122.367111237361)) ;
#32103 = CARTESIAN_POINT('Ctrl Pts',(-20.3754115587803,44.1666842527952,122.254696080828)) ;
#32104 = CARTESIAN_POINT('Ctrl Pts',(-20.1821781748641,43.9866951724323,122.486118021261)) ;
#32105 = CARTESIAN_POINT('Ctrl Pts',(-20.5616797006254,44.1766836850578,122.439998156239)) ;
#32106 = CARTESIAN_POINT('Ctrl Pts',(-20.3311931547893,43.9966946046949,122.634359041277)) ;
#32107 = CARTESIAN_POINT('Ctrl Pts',(-20.7119248209942,44.1866037503144,122.653074790023)) ;
#32108 = CARTESIAN_POINT('Ctrl Pts',(-20.4513895765128,44.0066146699516,122.804819385592)) ;
#32109 = CARTESIAN_POINT('Ctrl Pts',(-20.8242248480084,44.1966406028986,122.89171516179)) ;
#32110 = CARTESIAN_POINT('Ctrl Pts',(-20.5412304078257,44.0166515225357,122.995731440884)) ;
#32111 = CARTESIAN_POINT('Ctrl Pts',(-20.8925256088344,44.2065532622386,123.143101297578)) ;
#32112 = CARTESIAN_POINT('Ctrl Pts',(-20.5958716458054,44.0265641818757,123.19683949956)) ;
#32113 = CARTESIAN_POINT('Ctrl Pts',(-20.9168966357386,44.2165444741535,123.404542148438)) ;
#32114 = CARTESIAN_POINT('Ctrl Pts',(-20.6153694127085,44.0365553937906,123.405991922717)) ;
#32115 = CARTESIAN_POINT('Ctrl Pts',(-20.8948063197256,44.2265861155566,123.667478543077)) ;
#32116 = CARTESIAN_POINT('Ctrl Pts',(-20.597697972569,44.0465970351937,123.616341249776)) ;
#32117 = CARTESIAN_POINT('Ctrl Pts',(-20.8294398407361,44.2364149097636,123.917397995982)) ;
#32118 = CARTESIAN_POINT('Ctrl Pts',(-20.5454060288172,44.0564258294008,123.816275945776)) ;
#32119 = CARTESIAN_POINT('Ctrl Pts',(-20.7190966284838,44.2464913208849,124.158051348321)) ;
#32120 = CARTESIAN_POINT('Ctrl Pts',(-20.45713223089,44.066502240522,124.008799361129)) ;
#32121 = CARTESIAN_POINT('Ctrl Pts',(-20.5720419186679,44.2563434539274,124.371206621261)) ;
#32122 = CARTESIAN_POINT('Ctrl Pts',(-20.3394898756421,44.0763543735645,124.179323355511)) ;
#32123 = CARTESIAN_POINT('Ctrl Pts',(-20.3863598082827,44.2664166882687,124.559814357932)) ;
#32124 = CARTESIAN_POINT('Ctrl Pts',(-20.1909447374728,44.0864276079058,124.330210536534)) ;
#32125 = CARTESIAN_POINT('Ctrl Pts',(-20.1756188492781,44.2762581895953,124.709761183194)) ;
#32126 = CARTESIAN_POINT('Ctrl Pts',(-20.0223534395185,44.0962691092324,124.450168264063)) ;
#32127 = CARTESIAN_POINT('Ctrl Pts',(-19.9396571120249,44.2862191411901,124.823064731638)) ;
#32128 = CARTESIAN_POINT('Ctrl Pts',(-19.833584900295,44.1062300608272,124.540812125368)) ;
#32129 = CARTESIAN_POINT('Ctrl Pts',(-19.6855192485354,44.2962569589108,124.893713217866)) ;
#32130 = CARTESIAN_POINT('Ctrl Pts',(-19.630274821082,44.1162678785479,124.597332072431)) ;
#32131 = CARTESIAN_POINT('Ctrl Pts',(-19.4272568805915,44.3061313081678,124.919231077549)) ;
#32132 = CARTESIAN_POINT('Ctrl Pts',(-19.4236658581151,44.1261422278049,124.617747552398)) ;
#32133 = CARTESIAN_POINT('Ctrl Pts',(-19.1634421663118,44.31620085891,124.899117334135)) ;
#32134 = CARTESIAN_POINT('Ctrl Pts',(-19.2126137105638,44.1362117785471,124.601657806731)) ;
#32135 = CARTESIAN_POINT('Ctrl Pts',(-18.9130262792897,44.3260348784186,124.835165719918)) ;
#32136 = CARTESIAN_POINT('Ctrl Pts',(-19.0122816736547,44.1460457980557,124.55049803559)) ;
#32137 = CARTESIAN_POINT('Ctrl Pts',(-18.6724761256092,44.3360690329981,124.727189304434)) ;
#32138 = CARTESIAN_POINT('Ctrl Pts',(-18.8198408751358,44.1560799526353,124.464118191425)) ;
#32139 = CARTESIAN_POINT('Ctrl Pts',(-18.4550666358706,44.3460849588206,124.578799029693)) ;
#32140 = CARTESIAN_POINT('Ctrl Pts',(-18.6459125515534,44.1660958784577,124.345407061156)) ;
#32141 = CARTESIAN_POINT('Ctrl Pts',(-18.2689206934433,44.3559672140149,124.397708730824)) ;
#32142 = CARTESIAN_POINT('Ctrl Pts',(-18.4969953334488,44.175978133652,124.200536340073)) ;
#32143 = CARTESIAN_POINT('Ctrl Pts',(-18.1151639542311,44.3659560205258,124.184994122571)) ;
#32144 = CARTESIAN_POINT('Ctrl Pts',(-18.3739888404937,44.1859669401629,124.030365648299)) ;
#32145 = CARTESIAN_POINT('Ctrl Pts',(-18.0009287364672,44.3759045877885,123.949788452977)) ;
#32146 = CARTESIAN_POINT('Ctrl Pts',(-18.2825994652639,44.1959155074256,123.842202101952)) ;
#32147 = CARTESIAN_POINT('Ctrl Pts',(-17.9287930124207,44.3859593930905,123.695625807384)) ;
#32148 = CARTESIAN_POINT('Ctrl Pts',(-18.2248894332105,44.2059703127276,123.638872216548)) ;
#32149 = CARTESIAN_POINT('Ctrl Pts',(-17.9021400804517,44.3957781763541,123.438965134921)) ;
#32150 = CARTESIAN_POINT('Ctrl Pts',(-18.2035656682634,44.2157890959912,123.433544841874)) ;
#32151 = CARTESIAN_POINT('Ctrl Pts',(-17.9201546965115,44.4058139487147,123.175857889878)) ;
#32152 = CARTESIAN_POINT('Ctrl Pts',(-18.2179757049312,44.2258248683518,123.223058844661)) ;
#32153 = CARTESIAN_POINT('Ctrl Pts',(-17.9842443392215,44.4158386477433,122.920324456169)) ;
#32154 = CARTESIAN_POINT('Ctrl Pts',(-18.2692459457446,44.2358495673804,123.018631708746)) ;
#32155 = CARTESIAN_POINT('Ctrl Pts',(-18.0893534627256,44.4256906510024,122.683715321304)) ;
#32156 = CARTESIAN_POINT('Ctrl Pts',(-18.3533314265156,44.2457015706395,122.8293444755)) ;
#32157 = CARTESIAN_POINT('Ctrl Pts',(-18.2356357013134,44.4356815853996,122.46572907487)) ;
#32158 = CARTESIAN_POINT('Ctrl Pts',(-18.4703557257671,44.2556925050367,122.654954642238)) ;
#32159 = CARTESIAN_POINT('Ctrl Pts',(-18.41613673709,44.4455995078307,122.277671975149)) ;
#32160 = CARTESIAN_POINT('Ctrl Pts',(-18.6147549895924,44.2656104274678,122.504508093951)) ;
#32161 = CARTESIAN_POINT('Ctrl Pts',(-18.6288136047377,44.455627863513,122.122084840499)) ;
#32162 = CARTESIAN_POINT('Ctrl Pts',(-18.7848954782,44.2756387831502,122.380036963716)) ;
#32163 = CARTESIAN_POINT('Ctrl Pts',(-18.8618504936233,44.4655121480236,122.007331995514)) ;
#32164 = CARTESIAN_POINT('Ctrl Pts',(-18.9713236802826,44.2855230676607,122.288233368328)) ;
#32165 = CARTESIAN_POINT('Ctrl Pts',(-19.1138322342733,44.4755048319315,121.933421901147)) ;
#32166 = CARTESIAN_POINT('Ctrl Pts',(-19.1729084429983,44.2955157515686,122.229103542104)) ;
#32167 = CARTESIAN_POINT('Ctrl Pts',(-19.3758137501504,44.4855335689392,121.904740742867)) ;
#32168 = CARTESIAN_POINT('Ctrl Pts',(-19.3824934791347,44.3055444885763,122.206156839405)) ;
#32169 = CARTESIAN_POINT('Ctrl Pts',(-19.6350667634332,44.4954189655681,121.921395206069)) ;
#32170 = CARTESIAN_POINT('Ctrl Pts',(-19.5898954555801,44.3154298852052,122.219478539478)) ;
#32171 = CARTESIAN_POINT('Ctrl Pts',(-19.8901602887943,44.505406850982,121.983076127047)) ;
#32172 = CARTESIAN_POINT('Ctrl Pts',(-19.7939705951904,44.3254177706191,122.268821404401)) ;
#32173 = CARTESIAN_POINT('Ctrl Pts',(-20.1298803582596,44.5153575536426,122.087637628189)) ;
#32174 = CARTESIAN_POINT('Ctrl Pts',(-19.9857471730679,44.3353684732797,122.35246874884)) ;
#32175 = CARTESIAN_POINT('Ctrl Pts',(-20.3496330623717,44.52539787174,122.233619868658)) ;
#32176 = CARTESIAN_POINT('Ctrl Pts',(-20.1615504313535,44.3454087913771,122.469252999656)) ;
#32177 = CARTESIAN_POINT('Ctrl Pts',(-20.5377640234238,44.5352724370732,122.412390214829)) ;
#32178 = CARTESIAN_POINT('Ctrl Pts',(-20.3120561285973,44.3552833567104,122.612267503124)) ;
#32179 = CARTESIAN_POINT('Ctrl Pts',(-20.6941762400211,44.5452720971343,122.62349750357)) ;
#32180 = CARTESIAN_POINT('Ctrl Pts',(-20.4371874373751,44.3652830167714,122.781152089198)) ;
#32181 = CARTESIAN_POINT('Ctrl Pts',(-20.8107568463258,44.555181092302,122.856392682696)) ;
#32182 = CARTESIAN_POINT('Ctrl Pts',(-20.5304535425006,44.3751920119392,122.967466996356)) ;
#32183 = CARTESIAN_POINT('Ctrl Pts',(-20.8861166779856,44.5652358334653,123.109601455861)) ;
#32184 = CARTESIAN_POINT('Ctrl Pts',(-20.5907433453259,44.3852467531024,123.170033530578)) ;
#32185 = CARTESIAN_POINT('Ctrl Pts',(-20.9160838152059,44.5750944453791,123.36698258296)) ;
#32186 = CARTESIAN_POINT('Ctrl Pts',(-20.6147190097219,44.3951053650162,123.375937681712)) ;
#32187 = CARTESIAN_POINT('Ctrl Pts',(-20.9007482951995,44.5851625676584,123.631078613714)) ;
#32188 = CARTESIAN_POINT('Ctrl Pts',(-20.6024526333435,44.4051734872955,123.587214747284)) ;
#32189 = CARTESIAN_POINT('Ctrl Pts',(-20.8410433869187,44.5950180383616,123.883116987979)) ;
#32190 = CARTESIAN_POINT('Ctrl Pts',(-20.5546908119095,44.4150289579987,123.788845432467)) ;
#32191 = CARTESIAN_POINT('Ctrl Pts',(-20.737768269546,44.605012897855,124.124606144448)) ;
#32192 = CARTESIAN_POINT('Ctrl Pts',(-20.4720727081621,44.4250238174921,123.982037522316)) ;
#32193 = CARTESIAN_POINT('Ctrl Pts',(-20.5931261612872,44.6150441511969,124.344997164701)) ;
#32194 = CARTESIAN_POINT('Ctrl Pts',(-20.3563607533755,44.435055070834,124.158351473366)) ;
#32195 = CARTESIAN_POINT('Ctrl Pts',(-20.4156755541826,44.62491085007,124.534060702266)) ;
#32196 = CARTESIAN_POINT('Ctrl Pts',(-20.2144020898501,44.4449217697071,124.309603448869)) ;
#32197 = CARTESIAN_POINT('Ctrl Pts',(-20.2058546846897,44.6348976658212,124.691655677439)) ;
#32198 = CARTESIAN_POINT('Ctrl Pts',(-20.0465467658949,44.4549085854583,124.435681091647)) ;
#32199 = CARTESIAN_POINT('Ctrl Pts',(-19.9727822075021,44.6448448710167,124.810089850081)) ;
#32200 = CARTESIAN_POINT('Ctrl Pts',(-19.8600899289393,44.4648557906538,124.530430271056)) ;
#32201 = CARTESIAN_POINT('Ctrl Pts',(-19.7202958616412,44.6548878591429,124.886862052342)) ;
#32202 = CARTESIAN_POINT('Ctrl Pts',(-19.6581014661053,44.4748987787801,124.591850096019)) ;
#32203 = CARTESIAN_POINT('Ctrl Pts',(-19.4628869098935,44.6647552137644,124.91822843966)) ;
#32204 = CARTESIAN_POINT('Ctrl Pts',(-19.4521748954927,44.4847661334015,124.616945312954)) ;
#32205 = CARTESIAN_POINT('Ctrl Pts',(-19.201339436511,44.6747211070625,124.904992081208)) ;
#32206 = CARTESIAN_POINT('Ctrl Pts',(-19.242936917876,44.4947320266996,124.606358443205)) ;
#32207 = CARTESIAN_POINT('Ctrl Pts',(-18.9446146117008,44.6847448844386,124.845931776589)) ;
#32208 = CARTESIAN_POINT('Ctrl Pts',(-19.0375565977731,44.5047558040757,124.559112343262)) ;
#32209 = CARTESIAN_POINT('Ctrl Pts',(-18.7044247703961,44.6946704323703,124.744265398415)) ;
#32210 = CARTESIAN_POINT('Ctrl Pts',(-18.8454040419128,44.5146813520074,124.477781340274)) ;
#32211 = CARTESIAN_POINT('Ctrl Pts',(-18.4848477732278,44.7046109087913,124.602728279973)) ;
#32212 = CARTESIAN_POINT('Ctrl Pts',(-18.6697413477393,44.5246218284284,124.364553593259)) ;
#32213 = CARTESIAN_POINT('Ctrl Pts',(-18.2913709521149,44.7146571184542,124.423127645142)) ;
#32214 = CARTESIAN_POINT('Ctrl Pts',(-18.5149583948213,44.5346680380913,124.220874721725)) ;
#32215 = CARTESIAN_POINT('Ctrl Pts',(-18.1347068986328,44.724518375116,124.216672914137)) ;
#32216 = CARTESIAN_POINT('Ctrl Pts',(-18.3896255050784,44.5445292947531,124.055712452699)) ;
#32217 = CARTESIAN_POINT('Ctrl Pts',(-18.0143070451238,44.7345120033913,123.983318570089)) ;
#32218 = CARTESIAN_POINT('Ctrl Pts',(-18.2933036525415,44.5545229230284,123.869030062897)) ;
#32219 = CARTESIAN_POINT('Ctrl Pts',(-17.936633762989,44.7444374007015,123.734282199344)) ;
#32220 = CARTESIAN_POINT('Ctrl Pts',(-18.2311629143838,44.5644483203386,123.669801734943)) ;
#32221 = CARTESIAN_POINT('Ctrl Pts',(-17.9030399617659,44.7544653086117,123.472943722699)) ;
#32222 = CARTESIAN_POINT('Ctrl Pts',(-18.2042856479589,44.5744762282489,123.46073129079)) ;
#32223 = CARTESIAN_POINT('Ctrl Pts',(-17.9148956263581,44.7643516242809,123.213374011942)) ;
#32224 = CARTESIAN_POINT('Ctrl Pts',(-18.2137679274287,44.584362543918,123.253075513145)) ;
#32225 = CARTESIAN_POINT('Ctrl Pts',(-17.9723197114155,44.7743832191847,122.95612772885)) ;
#32226 = CARTESIAN_POINT('Ctrl Pts',(-18.2597049813133,44.5943941388218,123.047278048275)) ;
#32227 = CARTESIAN_POINT('Ctrl Pts',(-18.0718425713874,44.7842654621364,122.716214046185)) ;
#32228 = CARTESIAN_POINT('Ctrl Pts',(-18.3393211701474,44.6042763817735,122.855346286345)) ;
#32229 = CARTESIAN_POINT('Ctrl Pts',(-18.2138824565932,44.7943249331663,122.493298818431)) ;
#32230 = CARTESIAN_POINT('Ctrl Pts',(-18.452951139445,44.6143358528034,122.677012948951)) ;
#32231 = CARTESIAN_POINT('Ctrl Pts',(-18.3890982744024,44.8041913778294,122.302163339125)) ;
#32232 = CARTESIAN_POINT('Ctrl Pts',(-18.5931221262605,44.6242022974665,122.524103052415)) ;
#32233 = CARTESIAN_POINT('Ctrl Pts',(-18.5963979569655,44.8141575022781,122.142117824611)) ;
#32234 = CARTESIAN_POINT('Ctrl Pts',(-18.7589604790486,44.6341684219152,122.396064874445)) ;
#32235 = CARTESIAN_POINT('Ctrl Pts',(-18.8300300927451,44.8241877456692,122.020087986119)) ;
#32236 = CARTESIAN_POINT('Ctrl Pts',(-18.9458651244295,44.6441986653064,122.298439056251)) ;
#32237 = CARTESIAN_POINT('Ctrl Pts',(-19.0777784031114,44.8340807806223,121.941205272921)) ;
#32238 = CARTESIAN_POINT('Ctrl Pts',(-19.1440629425059,44.6540917002594,122.235330716498)) ;
#32239 = CARTESIAN_POINT('Ctrl Pts',(-19.3395157430304,44.8441316948591,121.905920090679)) ;
#32240 = CARTESIAN_POINT('Ctrl Pts',(-19.3534531408236,44.6641426144963,122.207100459181)) ;
#32241 = CARTESIAN_POINT('Ctrl Pts',(-19.5992088007417,44.8540215210837,121.916417743617)) ;
#32242 = CARTESIAN_POINT('Ctrl Pts',(-19.561205041554,44.6740324407208,122.215496012711)) ;
#32243 = CARTESIAN_POINT('Ctrl Pts',(-19.9417558495349,44.8673563361306,121.990481112151)) ;
#32244 = CARTESIAN_POINT('Ctrl Pts',(-19.8352567550235,44.6873672557678,122.274745507017)) ;
#32245 = CARTESIAN_POINT('Ctrl Pts',(-20.2554040575952,44.8806334273021,122.152088557895)) ;
#32246 = CARTESIAN_POINT('Ctrl Pts',(-20.0861971038527,44.7006443469392,122.404050615546)) ;
#32247 = CARTESIAN_POINT('Ctrl Pts',(-20.5136611155883,44.8938817159004,122.385626670228)) ;
#32248 = CARTESIAN_POINT('Ctrl Pts',(-20.2927670421858,44.7138926355375,122.590851388565)) ;
#32249 = CARTESIAN_POINT('Ctrl Pts',(-20.6757307463464,44.9039365573945,122.59426491759)) ;
#32250 = CARTESIAN_POINT('Ctrl Pts',(-20.4224319383683,44.7239474770316,122.757766151545)) ;
#32251 = CARTESIAN_POINT('Ctrl Pts',(-20.7967932245961,44.913767546702,122.822543238522)) ;
#32252 = CARTESIAN_POINT('Ctrl Pts',(-20.5192820748052,44.7337784663392,122.940386237297)) ;
#32253 = CARTESIAN_POINT('Ctrl Pts',(-20.8785256178797,44.9238441110252,123.074368365477)) ;
#32254 = CARTESIAN_POINT('Ctrl Pts',(-20.5846700573935,44.7438550306624,123.141847246608)) ;
#32255 = CARTESIAN_POINT('Ctrl Pts',(-20.9144646604309,44.9336934361592,123.330718388823)) ;
#32256 = CARTESIAN_POINT('Ctrl Pts',(-20.6134249986564,44.7537043557963,123.346922032747)) ;
#32257 = CARTESIAN_POINT('Ctrl Pts',(-20.9029627808752,44.9470414357965,123.681317025944)) ;
#32258 = CARTESIAN_POINT('Ctrl Pts',(-20.60421795921,44.7670523554336,123.627426785072)) ;
#32259 = CARTESIAN_POINT('Ctrl Pts',(-20.7745082951822,44.963626195333,124.10295325502)) ;
#32260 = CARTESIAN_POINT('Ctrl Pts',(-20.5014772079403,44.7836371149701,123.964697051323)) ;
#32261 = CARTESIAN_POINT('Ctrl Pts',(-20.5110259009966,44.9801947466811,124.455768261803)) ;
#32262 = CARTESIAN_POINT('Ctrl Pts',(-20.2906509869384,44.8002056663183,124.247002496847)) ;
#32263 = CARTESIAN_POINT('Ctrl Pts',(-20.2351348038895,44.9935545715001,124.672943272086)) ;
#32264 = CARTESIAN_POINT('Ctrl Pts',(-20.0699761236227,44.8135654911373,124.420705379304)) ;
#32265 = CARTESIAN_POINT('Ctrl Pts',(-20.0058393288218,45.0034599803308,124.796167835363)) ;
#32266 = CARTESIAN_POINT('Ctrl Pts',(-19.8865323249825,44.8234708999679,124.519294746871)) ;
#32267 = CARTESIAN_POINT('Ctrl Pts',(-19.757418400852,45.0134200069148,124.878510971796)) ;
#32268 = CARTESIAN_POINT('Ctrl Pts',(-19.6878011258136,44.833430926552,124.585169321105)) ;
#32269 = CARTESIAN_POINT('Ctrl Pts',(-19.4127381950797,45.0266775911001,124.929494089017)) ;
#32270 = CARTESIAN_POINT('Ctrl Pts',(-19.4120406279165,44.8466885107373,124.62595768779)) ;
#32271 = CARTESIAN_POINT('Ctrl Pts',(-18.9730728854828,45.0433288025948,124.878933487773)) ;
#32272 = CARTESIAN_POINT('Ctrl Pts',(-19.0603260702002,44.8633397222319,124.585513496632)) ;
#32273 = CARTESIAN_POINT('Ctrl Pts',(-18.4995381186548,45.0632470167051,124.642306903848)) ;
#32274 = CARTESIAN_POINT('Ctrl Pts',(-18.6814904260909,44.8832579363422,124.396215029442)) ;
#32275 = CARTESIAN_POINT('Ctrl Pts',(-18.1350210819867,45.0831247799259,124.259778759138)) ;
#32276 = CARTESIAN_POINT('Ctrl Pts',(-18.3898754178223,44.9031356995631,124.090194473814)) ;
#32277 = CARTESIAN_POINT('Ctrl Pts',(-17.9219902774577,45.1031374477131,123.772503946077)) ;
#32278 = CARTESIAN_POINT('Ctrl Pts',(-18.219447255777,44.9231483673502,123.700376068826)) ;
#32279 = CARTESIAN_POINT('Ctrl Pts',(-17.8878614143457,45.1229499703797,123.246927329174)) ;
#32280 = CARTESIAN_POINT('Ctrl Pts',(-18.1921410117766,44.9429608900168,123.279913768998)) ;
#32281 = CARTESIAN_POINT('Ctrl Pts',(-18.0355408684965,45.1429332703796,122.736855760796)) ;
#32282 = CARTESIAN_POINT('Ctrl Pts',(-18.3102818169754,44.9629441900167,122.8718555916)) ;
#32283 = CARTESIAN_POINT('Ctrl Pts',(-18.3474404946756,45.1628275474809,122.309788228837)) ;
#32284 = CARTESIAN_POINT('Ctrl Pts',(-18.5597996758674,44.982838467118,122.530199273158)) ;
#32285 = CARTESIAN_POINT('Ctrl Pts',(-18.786662149823,45.1827603092387,122.0135853007)) ;
#32286 = CARTESIAN_POINT('Ctrl Pts',(-18.9111760676998,45.0027712288758,122.293234567284)) ;
#32287 = CARTESIAN_POINT('Ctrl Pts',(-19.3015601046736,45.2027263150034,121.885187082688)) ;
#32288 = CARTESIAN_POINT('Ctrl Pts',(-19.3230941010408,45.0227372346405,122.190513534484)) ;
#32289 = CARTESIAN_POINT('Ctrl Pts',(-19.8271247057948,45.2226048471683,121.939586650986)) ;
#32290 = CARTESIAN_POINT('Ctrl Pts',(-19.7435470906285,45.0426157668054,122.234031125667)) ;
#32291 = CARTESIAN_POINT('Ctrl Pts',(-20.3041812489775,45.2425445138286,122.170281678288)) ;
#32292 = CARTESIAN_POINT('Ctrl Pts',(-20.125193674908,45.0625554334657,122.418585724291)) ;
#32293 = CARTESIAN_POINT('Ctrl Pts',(-20.673234757221,45.262439388474,122.549040856896)) ;
#32294 = CARTESIAN_POINT('Ctrl Pts',(-20.4204384003569,45.0824503081111,122.721592696201)) ;
#32295 = CARTESIAN_POINT('Ctrl Pts',(-20.8914226002841,45.2823465277673,123.03092366853)) ;
#32296 = CARTESIAN_POINT('Ctrl Pts',(-20.5949902713448,45.1023574474044,123.107099401626)) ;
#32297 = CARTESIAN_POINT('Ctrl Pts',(-20.933006994823,45.3022570758458,123.558648564266)) ;
#32298 = CARTESIAN_POINT('Ctrl Pts',(-20.6282585345272,45.1222679954829,123.529280226432)) ;
#32299 = CARTESIAN_POINT('Ctrl Pts',(-20.7897928711044,45.322325661203,124.072332126759)) ;
#32300 = CARTESIAN_POINT('Ctrl Pts',(-20.513688465567,45.1423365808401,123.940226547894)) ;
#32301 = CARTESIAN_POINT('Ctrl Pts',(-20.4845776581537,45.3421074585177,124.500648372566)) ;
#32302 = CARTESIAN_POINT('Ctrl Pts',(-20.269515271003,45.1621183781549,124.282882031287)) ;
#32303 = CARTESIAN_POINT('Ctrl Pts',(-20.0473359397164,45.3621150054623,124.802932073758)) ;
#32304 = CARTESIAN_POINT('Ctrl Pts',(-19.9197218860292,45.1821259250994,124.524709061024)) ;
#32305 = CARTESIAN_POINT('Ctrl Pts',(-19.5376317009415,45.3819367437651,124.936721152217)) ;
#32306 = CARTESIAN_POINT('Ctrl Pts',(-19.5119562871531,45.2019476634022,124.631740691942)) ;
#32307 = CARTESIAN_POINT('Ctrl Pts',(-19.0088087615849,45.4019167636693,124.889143040385)) ;
#32308 = CARTESIAN_POINT('Ctrl Pts',(-19.0888977818351,45.2219276833064,124.593677332525)) ;
#32309 = CARTESIAN_POINT('Ctrl Pts',(-18.5296775435496,45.4218342149315,124.664000015216)) ;
#32310 = CARTESIAN_POINT('Ctrl Pts',(-18.7055922193586,45.2418451345686,124.413561830565)) ;
#32311 = CARTESIAN_POINT('Ctrl Pts',(-18.1560490205525,45.4417091361042,124.2905332235)) ;
#32312 = CARTESIAN_POINT('Ctrl Pts',(-18.4066894730446,45.2617200557413,124.114786420847)) ;
#32313 = CARTESIAN_POINT('Ctrl Pts',(-17.9309504550834,45.461733504655,123.80830220994)) ;
#32314 = CARTESIAN_POINT('Ctrl Pts',(-18.2266120673935,45.2817444242922,123.729001254374)) ;
#32315 = CARTESIAN_POINT('Ctrl Pts',(-17.8844372685422,45.4816001890285,123.282245957211)) ;
#32316 = CARTESIAN_POINT('Ctrl Pts',(-18.1894029640175,45.3016111086656,123.308154786778)) ;
#32317 = CARTESIAN_POINT('Ctrl Pts',(-18.0199005695342,45.5015440108747,122.769835234287)) ;
#32318 = CARTESIAN_POINT('Ctrl Pts',(-18.2977757249971,45.3215549305118,122.898226217715)) ;
#32319 = CARTESIAN_POINT('Ctrl Pts',(-18.3217175474885,45.5214513801262,122.335254029468)) ;
#32320 = CARTESIAN_POINT('Ctrl Pts',(-18.5392315505227,45.3414622997634,122.550561763219)) ;
#32321 = CARTESIAN_POINT('Ctrl Pts',(-18.7524316861596,45.5413260778729,122.029454998175)) ;
#32322 = CARTESIAN_POINT('Ctrl Pts',(-18.8838052127124,45.3613369975101,122.305924073514)) ;
#32323 = CARTESIAN_POINT('Ctrl Pts',(-19.2643939100382,45.5613080203947,121.888099189238)) ;
#32324 = CARTESIAN_POINT('Ctrl Pts',(-19.2933758171969,45.3813189400318,122.192842065019)) ;
#32325 = CARTESIAN_POINT('Ctrl Pts',(-19.7916381676523,45.5812106873055,121.930204794695)) ;
#32326 = CARTESIAN_POINT('Ctrl Pts',(-19.7151717616758,45.4012216069426,122.226529377587)) ;
#32327 = CARTESIAN_POINT('Ctrl Pts',(-20.2724895989063,45.6010660448442,122.147814462636)) ;
#32328 = CARTESIAN_POINT('Ctrl Pts',(-20.0998523930469,45.4210769644813,122.400620504394)) ;
#32329 = CARTESIAN_POINT('Ctrl Pts',(-20.6536580199716,45.6211300835602,122.520640262332)) ;
#32330 = CARTESIAN_POINT('Ctrl Pts',(-20.4047844905581,45.4411410031973,122.698883170157)) ;
#32331 = CARTESIAN_POINT('Ctrl Pts',(-20.8822424651067,45.6409852632853,122.996499598304)) ;
#32332 = CARTESIAN_POINT('Ctrl Pts',(-20.5876495721056,45.4609961829224,123.07957274604)) ;
#32333 = CARTESIAN_POINT('Ctrl Pts',(-20.9354305273725,45.6609653679497,123.524661889087)) ;
#32334 = CARTESIAN_POINT('Ctrl Pts',(-20.6301960379111,45.4809762875868,123.502103333297)) ;
#32335 = CARTESIAN_POINT('Ctrl Pts',(-20.8068347567717,45.6807744731195,124.035365380666)) ;
#32336 = CARTESIAN_POINT('Ctrl Pts',(-20.5273174457036,45.5007853927566,123.910665095287)) ;
#32337 = CARTESIAN_POINT('Ctrl Pts',(-20.5095739145416,45.7007670934602,124.475605981024)) ;
#32338 = CARTESIAN_POINT('Ctrl Pts',(-20.2894986134957,45.5207780130973,124.262859246648)) ;
#32339 = CARTESIAN_POINT('Ctrl Pts',(-20.1539637829234,45.7173065759643,124.734247767366)) ;
#32340 = CARTESIAN_POINT('Ctrl Pts',(-20.005029677627,45.5373174956014,124.469758245705)) ;
#32341 = CARTESIAN_POINT('Ctrl Pts',(-19.826276696828,45.7306708940285,124.860455779892)) ;
#32342 = CARTESIAN_POINT('Ctrl Pts',(-19.7428532302614,45.5506818136656,124.570733098296)) ;
#32343 = CARTESIAN_POINT('Ctrl Pts',(-19.4853999049105,45.74388849653,124.927543476285)) ;
#32344 = CARTESIAN_POINT('Ctrl Pts',(-19.4702042800056,45.5638994161671,124.624395485871)) ;
#32345 = CARTESIAN_POINT('Ctrl Pts',(-19.0437646821752,45.7605460908078,124.897999792884)) ;
#32346 = CARTESIAN_POINT('Ctrl Pts',(-19.1168393059101,45.5805570104449,124.60076273691)) ;
#32347 = CARTESIAN_POINT('Ctrl Pts',(-18.5604443553513,45.7804117928495,124.685196121248)) ;
#32348 = CARTESIAN_POINT('Ctrl Pts',(-18.7301974465919,45.6004227124867,124.430507595726)) ;
#32349 = CARTESIAN_POINT('Ctrl Pts',(-18.240630590451,45.7970415195396,124.380241225691)) ;
#32350 = CARTESIAN_POINT('Ctrl Pts',(-18.4743626408579,45.6170524391767,124.186562638723)) ;
#32351 = CARTESIAN_POINT('Ctrl Pts',(-18.0589348454478,45.8103306346774,124.081934291346)) ;
#32352 = CARTESIAN_POINT('Ctrl Pts',(-18.3289929495072,45.6303415543145,123.947896101221)) ;
#32353 = CARTESIAN_POINT('Ctrl Pts',(-17.9633418369383,45.8202949816545,123.838171148512)) ;
#32354 = CARTESIAN_POINT('Ctrl Pts',(-18.2525232679131,45.6403059012916,123.752891352259)) ;
#32355 = CARTESIAN_POINT('Ctrl Pts',(-17.9115389081574,45.830223349656,123.582470100099)) ;
#32356 = CARTESIAN_POINT('Ctrl Pts',(-18.2110838276306,45.6502342692931,123.548318177483)) ;
#32357 = CARTESIAN_POINT('Ctrl Pts',(-17.9020047414413,45.8435067827447,123.233481404821)) ;
#32358 = CARTESIAN_POINT('Ctrl Pts',(-18.2034517092472,45.6635177023819,123.269181304791)) ;
#32359 = CARTESIAN_POINT('Ctrl Pts',(-18.0050894429486,45.8601588604851,122.80309786385)) ;
#32360 = CARTESIAN_POINT('Ctrl Pts',(-18.2859374204291,45.6801697801222,122.924806771228)) ;
#32361 = CARTESIAN_POINT('Ctrl Pts',(-18.2472042450846,45.8767102297859,122.435821289861)) ;
#32362 = CARTESIAN_POINT('Ctrl Pts',(-18.4796083339964,45.696721149423,122.631034810004)) ;
#32363 = CARTESIAN_POINT('Ctrl Pts',(-18.5078328375495,45.8899976579349,122.203411111269)) ;
#32364 = CARTESIAN_POINT('Ctrl Pts',(-18.6881326846269,45.710008577572,122.445080306261)) ;
#32365 = CARTESIAN_POINT('Ctrl Pts',(-18.7324749007102,45.900042197635,122.064839904029)) ;
#32366 = CARTESIAN_POINT('Ctrl Pts',(-18.8678435288482,45.7200531172721,122.334231042964)) ;
#32367 = CARTESIAN_POINT('Ctrl Pts',(-18.9727512214166,45.9098850394588,121.969029204104)) ;
#32368 = CARTESIAN_POINT('Ctrl Pts',(-19.0600665012445,45.7298959590959,122.257583020281)) ;
#32369 = CARTESIAN_POINT('Ctrl Pts',(-19.2294892302823,45.9198693237057,121.91505230479)) ;
#32370 = CARTESIAN_POINT('Ctrl Pts',(-19.2654570275077,45.7398802433429,122.214404142504)) ;
#32371 = CARTESIAN_POINT('Ctrl Pts',(-19.4908293876516,45.9298189691049,121.906556619496)) ;
#32372 = CARTESIAN_POINT('Ctrl Pts',(-19.4745292486748,45.749829888742,122.207609741249)) ;
#32373 = CARTESIAN_POINT('Ctrl Pts',(-19.7510268140243,45.9398187307933,121.943434488528)) ;
#32374 = CARTESIAN_POINT('Ctrl Pts',(-19.6826867913636,45.7598296504304,122.23711429284)) ;
#32375 = CARTESIAN_POINT('Ctrl Pts',(-20.0015055166855,45.9498500767522,122.02559641534)) ;
#32376 = CARTESIAN_POINT('Ctrl Pts',(-19.8830690113146,45.7698609963893,122.302845959369)) ;
#32377 = CARTESIAN_POINT('Ctrl Pts',(-20.230012990869,45.9597050312293,122.147483174595)) ;
#32378 = CARTESIAN_POINT('Ctrl Pts',(-20.0658738423898,45.7797159508665,122.400357316511)) ;
#32379 = CARTESIAN_POINT('Ctrl Pts',(-20.4366698390954,45.9696775692299,122.308599139529)) ;
#32380 = CARTESIAN_POINT('Ctrl Pts',(-20.2311978645646,45.789688488867,122.529251805209)) ;
#32381 = CARTESIAN_POINT('Ctrl Pts',(-20.6126387229705,45.9796725629648,122.503651259972)) ;
#32382 = CARTESIAN_POINT('Ctrl Pts',(-20.3719712626983,45.7996834826019,122.685294957718)) ;
#32383 = CARTESIAN_POINT('Ctrl Pts',(-20.7523044634586,45.9897066217589,122.727282847818)) ;
#32384 = CARTESIAN_POINT('Ctrl Pts',(-20.4837019244027,45.809717541396,122.86420139806)) ;
#32385 = CARTESIAN_POINT('Ctrl Pts',(-20.8496612407523,45.9995619645819,122.967303410869)) ;
#32386 = CARTESIAN_POINT('Ctrl Pts',(-20.5615851977692,45.819572884219,123.056218516308)) ;
#32387 = CARTESIAN_POINT('Ctrl Pts',(-20.9049869101856,46.0095614439275,123.224140951696)) ;
#32388 = CARTESIAN_POINT('Ctrl Pts',(-20.6058435342198,45.8295723635646,123.261688948786)) ;
#32389 = CARTESIAN_POINT('Ctrl Pts',(-20.9150723248034,46.0194558926828,123.484010185289)) ;
#32390 = CARTESIAN_POINT('Ctrl Pts',(-20.6139096475916,45.8394668123199,123.469584210841)) ;
#32391 = CARTESIAN_POINT('Ctrl Pts',(-20.8792184641045,46.0295190121173,123.745970407933)) ;
#32392 = CARTESIAN_POINT('Ctrl Pts',(-20.5852243537012,45.8495299317544,123.67915211632)) ;
#32393 = CARTESIAN_POINT('Ctrl Pts',(-20.8004631964166,46.0393586573585,123.992305910844)) ;
#32394 = CARTESIAN_POINT('Ctrl Pts',(-20.5222181446683,45.8593695769957,123.876219533294)) ;
#32395 = CARTESIAN_POINT('Ctrl Pts',(-20.6777341782391,46.0494218215446,124.226510235197)) ;
#32396 = CARTESIAN_POINT('Ctrl Pts',(-20.4240329804487,45.8694327411817,124.063582012675)) ;
#32397 = CARTESIAN_POINT('Ctrl Pts',(-20.5187010120317,46.0593160912934,124.432251752361)) ;
#32398 = CARTESIAN_POINT('Ctrl Pts',(-20.2968048726953,45.8793270109305,124.228173673899)) ;
#32399 = CARTESIAN_POINT('Ctrl Pts',(-20.3259612493778,46.0692578173072,124.608573010416)) ;
#32400 = CARTESIAN_POINT('Ctrl Pts',(-20.1426117715884,45.8892687369444,124.369228956089)) ;
#32401 = CARTESIAN_POINT('Ctrl Pts',(-20.1041752620859,46.0792607059666,124.749748717296)) ;
#32402 = CARTESIAN_POINT('Ctrl Pts',(-19.965181898146,45.8992716256037,124.48216768824)) ;
#32403 = CARTESIAN_POINT('Ctrl Pts',(-19.8602243413917,46.0893005547606,124.850170623594)) ;
#32404 = CARTESIAN_POINT('Ctrl Pts',(-19.770020308728,45.9093114743977,124.562503212813)) ;
#32405 = CARTESIAN_POINT('Ctrl Pts',(-19.6081586045614,46.0991247702215,124.906078173757)) ;
#32406 = CARTESIAN_POINT('Ctrl Pts',(-19.5683677549541,45.9191356898586,124.607227074532)) ;
#32407 = CARTESIAN_POINT('Ctrl Pts',(-19.3441646598656,46.109181613715,124.918003343611)) ;
#32408 = CARTESIAN_POINT('Ctrl Pts',(-19.3571724382085,45.9291925333521,124.616765131644)) ;
#32409 = CARTESIAN_POINT('Ctrl Pts',(-19.0854647176779,46.119110223111,124.883999596897)) ;
#32410 = CARTESIAN_POINT('Ctrl Pts',(-19.150213020904,45.9391211427481,124.589560066791)) ;
#32411 = CARTESIAN_POINT('Ctrl Pts',(-18.8357963857665,46.1290621071489,124.806111234111)) ;
#32412 = CARTESIAN_POINT('Ctrl Pts',(-18.9504791821078,45.949073026786,124.527247495769)) ;
#32413 = CARTESIAN_POINT('Ctrl Pts',(-18.6013290923237,46.1391150599565,124.684426223968)) ;
#32414 = CARTESIAN_POINT('Ctrl Pts',(-18.7629062354974,45.9591259795936,124.429897589284)) ;
#32415 = CARTESIAN_POINT('Ctrl Pts',(-18.3960311454174,46.1489379364227,124.527912441961)) ;
#32416 = CARTESIAN_POINT('Ctrl Pts',(-18.5986696124886,45.9689488560598,124.304685323724)) ;
#32417 = CARTESIAN_POINT('Ctrl Pts',(-18.2165638688177,46.1589936689928,124.333973843009)) ;
#32418 = CARTESIAN_POINT('Ctrl Pts',(-18.455097186173,45.9790045886299,124.149533032839)) ;
#32419 = CARTESIAN_POINT('Ctrl Pts',(-18.0755063145666,46.1689344339805,124.114086515428)) ;
#32420 = CARTESIAN_POINT('Ctrl Pts',(-18.3422530053555,45.9889453536176,123.973622294175)) ;
#32421 = CARTESIAN_POINT('Ctrl Pts',(-17.9743911402895,46.1788387668861,123.874249737998)) ;
#32422 = CARTESIAN_POINT('Ctrl Pts',(-18.2613628144267,45.9988496865232,123.781752514046)) ;
#32423 = CARTESIAN_POINT('Ctrl Pts',(-17.9157922099519,46.1888854357668,123.616841983496)) ;
#32424 = CARTESIAN_POINT('Ctrl Pts',(-18.2144855602764,46.0088963554039,123.575825794976)) ;
#32425 = CARTESIAN_POINT('Ctrl Pts',(-17.9027335515217,46.1987809990726,123.357082770937)) ;
#32426 = CARTESIAN_POINT('Ctrl Pts',(-18.2040405772589,46.0187919187097,123.368018794538)) ;
#32427 = CARTESIAN_POINT('Ctrl Pts',(-17.9355083348723,46.2088430567729,123.094739738878)) ;
#32428 = CARTESIAN_POINT('Ctrl Pts',(-18.2302623332334,46.02885397641,123.158144462417)) ;
#32429 = CARTESIAN_POINT('Ctrl Pts',(-18.0115191596736,46.2186858344004,122.847471415839)) ;
#32430 = CARTESIAN_POINT('Ctrl Pts',(-18.2910726074192,46.0386967540375,122.960331026345)) ;
#32431 = CARTESIAN_POINT('Ctrl Pts',(-18.1304936326855,46.2286763126523,122.613475678947)) ;
#32432 = CARTESIAN_POINT('Ctrl Pts',(-18.3862537375702,46.0486872322894,122.773135382181)) ;
#32433 = CARTESIAN_POINT('Ctrl Pts',(-18.2873793152529,46.2386052852958,122.404966075839)) ;
#32434 = CARTESIAN_POINT('Ctrl Pts',(-18.5117634954812,46.0586162049329,122.60632910476)) ;
#32435 = CARTESIAN_POINT('Ctrl Pts',(-18.4789900283898,46.2485964221754,122.225460708948)) ;
#32436 = CARTESIAN_POINT('Ctrl Pts',(-18.6650531643566,46.0686073418125,122.462726177038)) ;
#32437 = CARTESIAN_POINT('Ctrl Pts',(-18.6997158872876,46.2586185396643,122.081771774985)) ;
#32438 = CARTESIAN_POINT('Ctrl Pts',(-18.8416348469598,46.0786294593014,122.347776532043)) ;
#32439 = CARTESIAN_POINT('Ctrl Pts',(-18.9390004515799,46.2685190500665,121.97961691748)) ;
#32440 = CARTESIAN_POINT('Ctrl Pts',(-19.0330627062083,46.0885299697036,122.266054470778)) ;
#32441 = CARTESIAN_POINT('Ctrl Pts',(-19.1945546489749,46.2785080428126,121.919635191703)) ;
#32442 = CARTESIAN_POINT('Ctrl Pts',(-19.2375063079573,46.0985189624497,122.218070771051)) ;
#32443 = CARTESIAN_POINT('Ctrl Pts',(-19.4560195398829,46.2884732868632,121.905154403475)) ;
#32444 = CARTESIAN_POINT('Ctrl Pts',(-19.4466780569291,46.1084842065003,122.206487877725)) ;
#32445 = CARTESIAN_POINT('Ctrl Pts',(-19.7145391120576,46.2983775513764,121.93549611882)) ;
#32446 = CARTESIAN_POINT('Ctrl Pts',(-19.653492980395,46.1183884710135,122.230762786779)) ;
#32447 = CARTESIAN_POINT('Ctrl Pts',(-19.9676465193919,46.3084356430746,122.011573715253)) ;
#32448 = CARTESIAN_POINT('Ctrl Pts',(-19.8559786088564,46.1284465627118,122.291626492136)) ;
#32449 = CARTESIAN_POINT('Ctrl Pts',(-20.1989353902242,46.318285583503,122.127826794879)) ;
#32450 = CARTESIAN_POINT('Ctrl Pts',(-20.0410082397393,46.1382965031402,122.384630018431)) ;
#32451 = CARTESIAN_POINT('Ctrl Pts',(-20.4106296400589,46.3283125946766,122.284718430549)) ;
#32452 = CARTESIAN_POINT('Ctrl Pts',(-20.2103627795123,46.1483235143137,122.510144538498)) ;
#32453 = CARTESIAN_POINT('Ctrl Pts',(-20.5914073282754,46.3383411812886,122.476498822217)) ;
#32454 = CARTESIAN_POINT('Ctrl Pts',(-20.3549837916193,46.1583521009257,122.663570001819)) ;
#32455 = CARTESIAN_POINT('Ctrl Pts',(-20.7338884447941,46.3481863954013,122.692436981991)) ;
#32456 = CARTESIAN_POINT('Ctrl Pts',(-20.4689669204349,46.1681973150384,122.836320620193)) ;
#32457 = CARTESIAN_POINT('Ctrl Pts',(-20.838883297733,46.3581771435809,122.933081577216)) ;
#32458 = CARTESIAN_POINT('Ctrl Pts',(-20.5529614728706,46.178188063218,123.028836705902)) ;
#32459 = CARTESIAN_POINT('Ctrl Pts',(-20.9002222159883,46.3682147771664,123.1896289369)) ;
#32460 = CARTESIAN_POINT('Ctrl Pts',(-20.6020311735636,46.1882256968035,123.234075045714)) ;
#32461 = CARTESIAN_POINT('Ctrl Pts',(-20.9162101455242,46.3780600663792,123.447862222641)) ;
#32462 = CARTESIAN_POINT('Ctrl Pts',(-20.614820050469,46.1980709860163,123.440660827507)) ;
#32463 = CARTESIAN_POINT('Ctrl Pts',(-20.8872976540046,46.3880414671851,123.708544539136)) ;
#32464 = CARTESIAN_POINT('Ctrl Pts',(-20.5916887966278,46.2080523868222,123.649206325939)) ;
#32465 = CARTESIAN_POINT('Ctrl Pts',(-20.8137082785738,46.397993700175,123.959520057968)) ;
#32466 = CARTESIAN_POINT('Ctrl Pts',(-20.5328161531047,46.2180046198121,123.849986010889)) ;
#32467 = CARTESIAN_POINT('Ctrl Pts',(-20.6974169783614,46.4079925116317,124.195165716517)) ;
#32468 = CARTESIAN_POINT('Ctrl Pts',(-20.4397820581274,46.2280034312688,124.038501896986)) ;
#32469 = CARTESIAN_POINT('Ctrl Pts',(-20.5409623495954,46.4180316155623,124.407564420263)) ;
#32470 = CARTESIAN_POINT('Ctrl Pts',(-20.3146171987756,46.2380425351995,124.208420165923)) ;
#32471 = CARTESIAN_POINT('Ctrl Pts',(-20.3544390959673,46.4278565579816,124.586111387913)) ;
#32472 = CARTESIAN_POINT('Ctrl Pts',(-20.1653985485672,46.2478674776188,124.351256099726)) ;
#32473 = CARTESIAN_POINT('Ctrl Pts',(-20.134995919871,46.4379112454576,124.733256870576)) ;
#32474 = CARTESIAN_POINT('Ctrl Pts',(-19.9898432095306,46.2579221650947,124.468971664984)) ;
#32475 = CARTESIAN_POINT('Ctrl Pts',(-19.8958234362632,46.4478540478144,124.838477290274)) ;
#32476 = CARTESIAN_POINT('Ctrl Pts',(-19.7985051353793,46.2678649674515,124.553146698639)) ;
#32477 = CARTESIAN_POINT('Ctrl Pts',(-19.6432030628621,46.4577578437542,124.901101950844)) ;
#32478 = CARTESIAN_POINT('Ctrl Pts',(-19.5964092448346,46.2777687633913,124.603245250316)) ;
#32479 = CARTESIAN_POINT('Ctrl Pts',(-19.3798141419767,46.4678046231292,124.919009575157)) ;
#32480 = CARTESIAN_POINT('Ctrl Pts',(-19.3856978663707,46.2878155427663,124.61757028202)) ;
#32481 = CARTESIAN_POINT('Ctrl Pts',(-19.1211811679258,46.4777002814238,124.891553789188)) ;
#32482 = CARTESIAN_POINT('Ctrl Pts',(-19.1787923210989,46.2977112010609,124.595604707242)) ;
#32483 = CARTESIAN_POINT('Ctrl Pts',(-18.8671103311317,46.4877618486744,124.818449852984)) ;
#32484 = CARTESIAN_POINT('Ctrl Pts',(-18.9755356841084,46.3077727683115,124.537120502504)) ;
#32485 = CARTESIAN_POINT('Ctrl Pts',(-18.6346615958398,46.4976064931117,124.704865605345)) ;
#32486 = CARTESIAN_POINT('Ctrl Pts',(-18.7895780913401,46.3176174127489,124.446252657151)) ;
#32487 = CARTESIAN_POINT('Ctrl Pts',(-18.4224718070244,46.5075665393544,124.551629282646)) ;
#32488 = CARTESIAN_POINT('Ctrl Pts',(-18.6198270211866,46.3275774589915,124.32366317014)) ;
#32489 = CARTESIAN_POINT('Ctrl Pts',(-18.2390573894743,46.5176048353728,124.362048863107)) ;
#32490 = CARTESIAN_POINT('Ctrl Pts',(-18.4730960549805,46.3376157550099,124.171998104319)) ;
#32491 = CARTESIAN_POINT('Ctrl Pts',(-18.0933321835797,46.5274781767911,124.147328823137)) ;
#32492 = CARTESIAN_POINT('Ctrl Pts',(-18.3565170542774,46.3474890964282,124.00022237033)) ;
#32493 = CARTESIAN_POINT('Ctrl Pts',(-17.9850644966569,46.5375512805904,123.905828159884)) ;
#32494 = CARTESIAN_POINT('Ctrl Pts',(-18.2699035102688,46.3575622002275,123.80702119456)) ;
#32495 = CARTESIAN_POINT('Ctrl Pts',(-17.9216561766812,46.5473720957093,123.655604769692)) ;
#32496 = CARTESIAN_POINT('Ctrl Pts',(-18.219177873809,46.3673830153464,123.606843503252)) ;
#32497 = CARTESIAN_POINT('Ctrl Pts',(-17.9018683250634,46.5574489607873,123.391584873684)) ;
#32498 = CARTESIAN_POINT('Ctrl Pts',(-18.2033482278461,46.3774598804244,123.395627180007)) ;
#32499 = CARTESIAN_POINT('Ctrl Pts',(-17.9277757499098,46.5673137004426,123.133615388447)) ;
#32500 = CARTESIAN_POINT('Ctrl Pts',(-18.2240747548872,46.3873246200797,123.189252631798)) ;
#32501 = CARTESIAN_POINT('Ctrl Pts',(-17.9985297244048,46.5773361036839,122.879929630516)) ;
#32502 = CARTESIAN_POINT('Ctrl Pts',(-18.2806784477161,46.397347023321,122.98630413088)) ;
#32503 = CARTESIAN_POINT('Ctrl Pts',(-18.1129004945136,46.5873618279724,122.642565399525)) ;
#32504 = CARTESIAN_POINT('Ctrl Pts',(-18.3721757093272,46.4073727476095,122.796412980426)) ;
#32505 = CARTESIAN_POINT('Ctrl Pts',(-18.2637366876288,46.5972166109937,122.432070963929)) ;
#32506 = CARTESIAN_POINT('Ctrl Pts',(-18.4928445100312,46.4172275306308,122.628018630033)) ;
#32507 = CARTESIAN_POINT('Ctrl Pts',(-18.4506972916997,46.607195454717,122.248181197861)) ;
#32508 = CARTESIAN_POINT('Ctrl Pts',(-18.6424130861803,46.4272063743541,122.48090728997)) ;
#32509 = CARTESIAN_POINT('Ctrl Pts',(-18.6678559884878,46.6172143469536,122.099336220667)) ;
#32510 = CARTESIAN_POINT('Ctrl Pts',(-18.8161403445689,46.4372252665907,122.361831725201)) ;
#32511 = CARTESIAN_POINT('Ctrl Pts',(-18.9041339832422,46.6270975559946,121.991423381431)) ;
#32512 = CARTESIAN_POINT('Ctrl Pts',(-19.0051620983221,46.4471084756317,122.275502163927)) ;
#32513 = CARTESIAN_POINT('Ctrl Pts',(-19.1602204279234,46.6371658653348,121.925081449906)) ;
#32514 = CARTESIAN_POINT('Ctrl Pts',(-19.2100316746212,46.4571767849719,122.222428931168)) ;
#32515 = CARTESIAN_POINT('Ctrl Pts',(-19.4177614318243,46.6469959906675,121.904397063364)) ;
#32516 = CARTESIAN_POINT('Ctrl Pts',(-19.4160632754822,46.4670069103046,122.205881850108)) ;
#32517 = CARTESIAN_POINT('Ctrl Pts',(-19.6811124793488,46.6570625430445,121.928980404509)) ;
#32518 = CARTESIAN_POINT('Ctrl Pts',(-19.6267444075026,46.4770734626816,122.22554879681)) ;
#32519 = CARTESIAN_POINT('Ctrl Pts',(-19.93175625164,46.6669527799382,121.997866497326)) ;
#32520 = CARTESIAN_POINT('Ctrl Pts',(-19.8272585403738,46.4869636995753,122.280657725669)) ;
#32521 = CARTESIAN_POINT('Ctrl Pts',(-20.1692553844016,46.6769450047322,122.109835361796)) ;
#32522 = CARTESIAN_POINT('Ctrl Pts',(-20.0172576312731,46.4969559243693,122.370232872609)) ;
#32523 = CARTESIAN_POINT('Ctrl Pts',(-20.3829389131417,46.6869076250832,122.261097188161)) ;
#32524 = CARTESIAN_POINT('Ctrl Pts',(-20.1882040373504,46.5069185447203,122.491242289893)) ;
#32525 = CARTESIAN_POINT('Ctrl Pts',(-20.5665204839457,46.6968126278463,122.445649602459)) ;
#32526 = CARTESIAN_POINT('Ctrl Pts',(-20.3350687382439,46.5168235474834,122.638883718221)) ;
#32527 = CARTESIAN_POINT('Ctrl Pts',(-20.7173901651887,46.7068703902444,122.662639131591)) ;
#32528 = CARTESIAN_POINT('Ctrl Pts',(-20.4557645655042,46.5268813098816,122.812475613443)) ;
#32529 = CARTESIAN_POINT('Ctrl Pts',(-20.8262181894773,46.7167209096232,122.89753556539)) ;
#32530 = CARTESIAN_POINT('Ctrl Pts',(-20.5428264841465,46.5367318292604,123.000391752439)) ;
#32531 = CARTESIAN_POINT('Ctrl Pts',(-20.8943773618054,46.7267524866214,123.15217347503)) ;
#32532 = CARTESIAN_POINT('Ctrl Pts',(-20.5973539588229,46.5467634062585,123.204102140928)) ;
#32533 = CARTESIAN_POINT('Ctrl Pts',(-20.9167369790523,46.7367622217263,123.414295804395)) ;
#32534 = CARTESIAN_POINT('Ctrl Pts',(-20.6152416326084,46.5567731413635,123.413799972381)) ;
#32535 = CARTESIAN_POINT('Ctrl Pts',(-20.8937123153054,46.7466717983526,123.673666920638)) ;
#32536 = CARTESIAN_POINT('Ctrl Pts',(-20.596822009193,46.5666827179897,123.621296152954)) ;
#32537 = CARTESIAN_POINT('Ctrl Pts',(-20.8265171674148,46.7565991842093,123.925758286608)) ;
#32538 = CARTESIAN_POINT('Ctrl Pts',(-20.5430662495124,46.5766101038464,123.822968723922)) ;
#32539 = CARTESIAN_POINT('Ctrl Pts',(-20.7150850922258,46.7666441186995,124.165042883978)) ;
#32540 = CARTESIAN_POINT('Ctrl Pts',(-20.4539206594605,46.5866550383367,124.014396623228)) ;
#32541 = CARTESIAN_POINT('Ctrl Pts',(-20.566303423748,46.7765300508875,124.378031588581)) ;
#32542 = CARTESIAN_POINT('Ctrl Pts',(-20.3348959856929,46.5965409705246,124.184786987194)) ;
#32543 = CARTESIAN_POINT('Ctrl Pts',(-20.3811494336437,46.7865233568405,124.56424680321)) ;
#32544 = CARTESIAN_POINT('Ctrl Pts',(-20.1867731294926,46.6065342764777,124.333759263123)) ;
#32545 = CARTESIAN_POINT('Ctrl Pts',(-20.167426750717,46.7964689946224,124.714688252167)) ;
#32546 = CARTESIAN_POINT('Ctrl Pts',(-20.0157955364757,46.6164799142595,124.454112381368)) ;
#32547 = CARTESIAN_POINT('Ctrl Pts',(-19.9310071201226,46.8064162629683,124.826243396208)) ;
#32548 = CARTESIAN_POINT('Ctrl Pts',(-19.8266604269535,46.6264271826054,124.543356680596)) ;
#32549 = CARTESIAN_POINT('Ctrl Pts',(-19.6762006528589,46.8164641651054,124.895457669008)) ;
#32550 = CARTESIAN_POINT('Ctrl Pts',(-19.6228151502625,46.6364750847425,124.598728484168)) ;
#32551 = CARTESIAN_POINT('Ctrl Pts',(-19.4184961828357,46.8263118599456,124.91911890289)) ;
#32552 = CARTESIAN_POINT('Ctrl Pts',(-19.4166527254704,46.6463227795827,124.617657767164)) ;
#32553 = CARTESIAN_POINT('Ctrl Pts',(-19.1575612607115,46.83627336969,124.898251094209)) ;
#32554 = CARTESIAN_POINT('Ctrl Pts',(-19.2079051028574,46.6562842893271,124.600964154411)) ;
#32555 = CARTESIAN_POINT('Ctrl Pts',(-18.902556312997,46.8463027612989,124.831598304346)) ;
#32556 = CARTESIAN_POINT('Ctrl Pts',(-19.0039009355955,46.666313680936,124.54764240293)) ;
#32557 = CARTESIAN_POINT('Ctrl Pts',(-18.6658571373904,46.8562102568536,124.723148671996)) ;
#32558 = CARTESIAN_POINT('Ctrl Pts',(-18.8145420155273,46.6762211764908,124.460883498429)) ;
#32559 = CARTESIAN_POINT('Ctrl Pts',(-18.4504873824993,46.8661556485166,124.575124657286)) ;
#32560 = CARTESIAN_POINT('Ctrl Pts',(-18.6422462094197,46.6861665681538,124.342465111585)) ;
#32561 = CARTESIAN_POINT('Ctrl Pts',(-18.262882041295,46.876157566114,124.390984128)) ;
#32562 = CARTESIAN_POINT('Ctrl Pts',(-18.4921615041804,46.6961684857511,124.195153273134)) ;
#32563 = CARTESIAN_POINT('Ctrl Pts',(-18.1099479381027,46.8861976336662,124.176016249327)) ;
#32564 = CARTESIAN_POINT('Ctrl Pts',(-18.3698136515618,46.7062085533033,124.023179206255)) ;
#32565 = CARTESIAN_POINT('Ctrl Pts',(-17.998547175216,46.896021945106,123.943090129844)) ;
#32566 = CARTESIAN_POINT('Ctrl Pts',(-18.280692897445,46.7160328647431,123.836839731432)) ;
#32567 = CARTESIAN_POINT('Ctrl Pts',(-17.9273097685191,46.9060781862621,123.688632681324)) ;
#32568 = CARTESIAN_POINT('Ctrl Pts',(-18.2237021026595,46.7260891058992,123.633273756565)) ;
#32569 = CARTESIAN_POINT('Ctrl Pts',(-17.9019600484687,46.9160091079977,123.4288626675)) ;
#32570 = CARTESIAN_POINT('Ctrl Pts',(-18.2034216287563,46.7360200276349,123.425458357104)) ;
#32571 = CARTESIAN_POINT('Ctrl Pts',(-17.9215882488076,46.925952344074,123.168336310537)) ;
#32572 = CARTESIAN_POINT('Ctrl Pts',(-18.2191232721713,46.7459632637111,123.217037686628)) ;
#32573 = CARTESIAN_POINT('Ctrl Pts',(-17.9861745623724,46.9359336280864,122.914073624315)) ;
#32574 = CARTESIAN_POINT('Ctrl Pts',(-18.2707913566683,46.7559445477236,123.01362751071)) ;
#32575 = CARTESIAN_POINT('Ctrl Pts',(-18.0949933336756,46.9459779297121,122.673631325158)) ;
#32576 = CARTESIAN_POINT('Ctrl Pts',(-18.3578456757999,46.7659888493492,122.821273187654)) ;
#32577 = CARTESIAN_POINT('Ctrl Pts',(-18.2402478329783,46.9558060109315,122.460027367171)) ;
#32578 = CARTESIAN_POINT('Ctrl Pts',(-18.474047818082,46.7758169305687,122.650390426094)) ;
#32579 = CARTESIAN_POINT('Ctrl Pts',(-18.4247793331419,46.9658826137807,122.270186990604)) ;
#32580 = CARTESIAN_POINT('Ctrl Pts',(-18.6216725361831,46.7858935334178,122.498517174402)) ;
#32581 = CARTESIAN_POINT('Ctrl Pts',(-18.6347009617729,46.9757346928992,122.118553078034)) ;
#32582 = CARTESIAN_POINT('Ctrl Pts',(-18.789608433041,46.7957456125364,122.377209782781)) ;
#32583 = CARTESIAN_POINT('Ctrl Pts',(-18.8728048873028,46.9858079512082,122.002979006205)) ;
#32584 = CARTESIAN_POINT('Ctrl Pts',(-18.9800913870549,46.8058188708453,122.28474940667)) ;
#32585 = CARTESIAN_POINT('Ctrl Pts',(-19.1215801045156,46.9956494105884,121.93222329205)) ;
#32586 = CARTESIAN_POINT('Ctrl Pts',(-19.1791102655951,46.8156603302256,122.228144091495)) ;
#32587 = CARTESIAN_POINT('Ctrl Pts',(-19.381859343394,47.0056105060008,121.904442012515)) ;
#32588 = CARTESIAN_POINT('Ctrl Pts',(-19.3873331982892,46.8256214256379,122.205917820199)) ;
#32589 = CARTESIAN_POINT('Ctrl Pts',(-19.6449738782894,47.0156477903975,121.922928491226)) ;
#32590 = CARTESIAN_POINT('Ctrl Pts',(-19.5978250114014,46.8356587100347,122.220705838776)) ;
#32591 = CARTESIAN_POINT('Ctrl Pts',(-19.8969217299239,47.0255241291328,121.985363214302)) ;
#32592 = CARTESIAN_POINT('Ctrl Pts',(-19.7993828256105,46.8455350487699,122.270652190592)) ;
#32593 = CARTESIAN_POINT('Ctrl Pts',(-20.1386279884017,47.0355862552861,122.092504779786)) ;
#32594 = CARTESIAN_POINT('Ctrl Pts',(-19.9927485620531,46.8555971749232,122.356364359904)) ;
#32595 = CARTESIAN_POINT('Ctrl Pts',(-20.3539188130597,47.0454544292626,122.237128270037)) ;
#32596 = CARTESIAN_POINT('Ctrl Pts',(-20.1649812567676,46.8654653488997,122.472061612692)) ;
#32597 = CARTESIAN_POINT('Ctrl Pts',(-20.5437493740665,47.0554599777664,122.419010050859)) ;
#32598 = CARTESIAN_POINT('Ctrl Pts',(-20.3168466298338,46.8754708974035,122.617565974457)) ;
#32599 = CARTESIAN_POINT('Ctrl Pts',(-20.6987362985448,47.065442609662,122.630724270001)) ;
#32600 = CARTESIAN_POINT('Ctrl Pts',(-20.440837183443,46.8854535292991,122.786936385641)) ;
#32601 = CARTESIAN_POINT('Ctrl Pts',(-20.8150425909332,47.0754865520838,122.867637130232)) ;
#32602 = CARTESIAN_POINT('Ctrl Pts',(-20.5338834673555,46.8954974717209,122.976466203145)) ;
#32603 = CARTESIAN_POINT('Ctrl Pts',(-20.8872078791894,47.0853147001109,123.115624213289)) ;
#32604 = CARTESIAN_POINT('Ctrl Pts',(-20.5916167561873,46.9053256197481,123.174854489363)) ;
#32605 = CARTESIAN_POINT('Ctrl Pts',(-20.9165166534759,47.0953045674853,123.37650718992)) ;
#32606 = CARTESIAN_POINT('Ctrl Pts',(-20.6150653220902,46.9153154871225,123.383560557976)) ;
#32607 = CARTESIAN_POINT('Ctrl Pts',(-20.8993091493922,47.1053483064408,123.639884268201)) ;
#32608 = CARTESIAN_POINT('Ctrl Pts',(-20.6013007427833,46.925359226078,123.594262430873)) ;
#32609 = CARTESIAN_POINT('Ctrl Pts',(-20.8385403650369,47.1151700549788,123.890732974447)) ;
#32610 = CARTESIAN_POINT('Ctrl Pts',(-20.5526874481851,46.9351809746159,123.794940790409)) ;
#32611 = CARTESIAN_POINT('Ctrl Pts',(-20.7334869965978,47.1252050325885,124.132613019297)) ;
#32612 = CARTESIAN_POINT('Ctrl Pts',(-20.4686462451259,46.9452159522256,123.988445566052)) ;
#32613 = CARTESIAN_POINT('Ctrl Pts',(-20.5875612969449,47.1352299453462,124.351957946675)) ;
#32614 = CARTESIAN_POINT('Ctrl Pts',(-20.3519069440029,46.9552408649833,124.163922368766)) ;
#32615 = CARTESIAN_POINT('Ctrl Pts',(-20.4093144805832,47.14508188844,124.539733165987)) ;
#32616 = CARTESIAN_POINT('Ctrl Pts',(-20.209311228941,46.9650928080772,124.314143082127)) ;
#32617 = CARTESIAN_POINT('Ctrl Pts',(-20.1985036701278,47.1550728497691,124.69617951058)) ;
#32618 = CARTESIAN_POINT('Ctrl Pts',(-20.0406637063053,46.9750837694063,124.439301445059)) ;
#32619 = CARTESIAN_POINT('Ctrl Pts',(-19.9654674976531,47.1649907246376,124.812968953075)) ;
#32620 = CARTESIAN_POINT('Ctrl Pts',(-19.8542359521288,46.9850016442747,124.532734341221)) ;
#32621 = CARTESIAN_POINT('Ctrl Pts',(-19.71297510293,47.1750192436388,124.88839013585)) ;
#32622 = CARTESIAN_POINT('Ctrl Pts',(-19.652242507693,46.9950301632759,124.593072964507)) ;
#32623 = CARTESIAN_POINT('Ctrl Pts',(-19.4549854354218,47.1849029224366,124.918522015687)) ;
#32624 = CARTESIAN_POINT('Ctrl Pts',(-19.4458515655707,47.0049138420738,124.617180149726)) ;
#32625 = CARTESIAN_POINT('Ctrl Pts',(-19.1927415406444,47.1948978658764,124.903808702217)) ;
#32626 = CARTESIAN_POINT('Ctrl Pts',(-19.2360564571309,47.0149087855135,124.605411359916)) ;
#32627 = CARTESIAN_POINT('Ctrl Pts',(-18.9363215273581,47.2049247196988,124.843152452533)) ;
#32628 = CARTESIAN_POINT('Ctrl Pts',(-19.0309200183396,47.0249356393359,124.55688809248)) ;
#32629 = CARTESIAN_POINT('Ctrl Pts',(-18.6976217950589,47.2148088840377,124.740702605869)) ;
#32630 = CARTESIAN_POINT('Ctrl Pts',(-18.8399600159307,47.0348198036749,124.47493012311)) ;
#32631 = CARTESIAN_POINT('Ctrl Pts',(-18.4778918251213,47.2247969820801,124.597178175501)) ;
#32632 = CARTESIAN_POINT('Ctrl Pts',(-18.6641751118157,47.0448079017172,124.360112235116)) ;
#32633 = CARTESIAN_POINT('Ctrl Pts',(-18.2869868870465,47.2347480885372,124.418412493407)) ;
#32634 = CARTESIAN_POINT('Ctrl Pts',(-18.511450049831,47.0547590081743,124.2171012666)) ;
#32635 = CARTESIAN_POINT('Ctrl Pts',(-18.1286864683151,47.2447931397053,124.207190353518)) ;
#32636 = CARTESIAN_POINT('Ctrl Pts',(-18.3848081587268,47.0648040593424,124.048124631986)) ;
#32637 = CARTESIAN_POINT('Ctrl Pts',(-18.0115053675036,47.2546549000636,123.976037450219)) ;
#32638 = CARTESIAN_POINT('Ctrl Pts',(-18.2910618397786,47.0746658197007,123.863203703224)) ;
#32639 = CARTESIAN_POINT('Ctrl Pts',(-17.9346962187188,47.264617716894,123.725744078448)) ;
#32640 = CARTESIAN_POINT('Ctrl Pts',(-18.2296126464617,47.0846286365312,123.662969789116)) ;
#32641 = CARTESIAN_POINT('Ctrl Pts',(-17.9027315659369,47.2746523981748,123.463999492697)) ;
#32642 = CARTESIAN_POINT('Ctrl Pts',(-18.2040389739103,47.0946633178119,123.453574331988)) ;
#32643 = CARTESIAN_POINT('Ctrl Pts',(-17.9160504867167,47.2845374279556,123.204536864795)) ;
#32644 = CARTESIAN_POINT('Ctrl Pts',(-18.214692073012,47.1045483475927,123.246004576489)) ;
#32645 = CARTESIAN_POINT('Ctrl Pts',(-17.9753215326006,47.2946030213536,122.946793722897)) ;
#32646 = CARTESIAN_POINT('Ctrl Pts',(-18.2621069751575,47.1146139409907,123.039809496486)) ;
#32647 = CARTESIAN_POINT('Ctrl Pts',(-18.0759175402315,47.3044421897151,122.708557598471)) ;
#32648 = CARTESIAN_POINT('Ctrl Pts',(-18.3425816822834,47.1244531093522,122.84922032325)) ;
#32649 = CARTESIAN_POINT('Ctrl Pts',(-18.2191949884316,47.3145047874566,122.486339905974)) ;
#32650 = CARTESIAN_POINT('Ctrl Pts',(-18.4572019469866,47.1345157070937,122.671444952012)) ;
#32651 = CARTESIAN_POINT('Ctrl Pts',(-18.396159615514,47.3244017998635,122.295722821703)) ;
#32652 = CARTESIAN_POINT('Ctrl Pts',(-18.5987718917569,47.1444127195006,122.518950162102)) ;
#32653 = CARTESIAN_POINT('Ctrl Pts',(-18.6037098264549,47.3343331216891,122.137504758704)) ;
#32654 = CARTESIAN_POINT('Ctrl Pts',(-18.7648105710639,47.1543440413262,122.392374154288)) ;
#32655 = CARTESIAN_POINT('Ctrl Pts',(-18.8382907890392,47.3443748844436,122.016648795488)) ;
#32656 = CARTESIAN_POINT('Ctrl Pts',(-18.9524743954627,47.1643858040807,122.295687495838)) ;
#32657 = CARTESIAN_POINT('Ctrl Pts',(-19.0864023365642,47.3542630833343,121.939374027969)) ;
#32658 = CARTESIAN_POINT('Ctrl Pts',(-19.1509626756622,47.1742740029714,122.233865749171)) ;
#32659 = CARTESIAN_POINT('Ctrl Pts',(-19.3468297085847,47.3642570219342,121.905591956175)) ;
#32660 = CARTESIAN_POINT('Ctrl Pts',(-19.3593042135663,47.1842679415713,122.206837953697)) ;
#32661 = CARTESIAN_POINT('Ctrl Pts',(-19.6078094898697,47.374197842971,121.917497147633)) ;
#32662 = CARTESIAN_POINT('Ctrl Pts',(-19.568087947677,47.1942087626082,122.216359938901)) ;
#32663 = CARTESIAN_POINT('Ctrl Pts',(-19.8632760200849,47.3841572252593,121.974310927408)) ;
#32664 = CARTESIAN_POINT('Ctrl Pts',(-19.772461509312,47.2041681448964,122.261808795976)) ;
#32665 = CARTESIAN_POINT('Ctrl Pts',(-20.1060266518377,47.3941549849116,122.074874782439)) ;
#32666 = CARTESIAN_POINT('Ctrl Pts',(-19.966662791665,47.2141659045487,122.342257824521)) ;
#32667 = CARTESIAN_POINT('Ctrl Pts',(-20.3282563986287,47.4041911211139,122.216891398893)) ;
#32668 = CARTESIAN_POINT('Ctrl Pts',(-20.1444477453573,47.224202040751,122.455869277174)) ;
#32669 = CARTESIAN_POINT('Ctrl Pts',(-20.5190751999569,47.4140419186048,122.391820347718)) ;
#32670 = CARTESIAN_POINT('Ctrl Pts',(-20.2971040399441,47.2340528382419,122.595810607946)) ;
#32671 = CARTESIAN_POINT('Ctrl Pts',(-20.6789956607079,47.4240027836811,122.599038839022)) ;
#32672 = CARTESIAN_POINT('Ctrl Pts',(-20.4250421187195,47.2440137033182,122.76158395382)) ;
#32673 = CARTESIAN_POINT('Ctrl Pts',(-20.8010651623618,47.4340316513115,122.832629226849)) ;
#32674 = CARTESIAN_POINT('Ctrl Pts',(-20.5226996700031,47.2540425709486,122.948455205887)) ;
#32675 = CARTESIAN_POINT('Ctrl Pts',(-20.8798481803655,47.4439418874479,123.080846336945)) ;
#32676 = CARTESIAN_POINT('Ctrl Pts',(-20.5857281550626,47.263952807085,123.147028060503)) ;
#32677 = CARTESIAN_POINT('Ctrl Pts',(-20.9151022554273,47.4538768407624,123.339542816455)) ;
#32678 = CARTESIAN_POINT('Ctrl Pts',(-20.6139336294218,47.2738877603996,123.353984836361)) ;
#32679 = CARTESIAN_POINT('Ctrl Pts',(-20.9045535939109,47.463917771172,123.603190649991)) ;
#32680 = CARTESIAN_POINT('Ctrl Pts',(-20.605496940888,47.2839286908091,123.564903155438)) ;
#32681 = CARTESIAN_POINT('Ctrl Pts',(-20.849402115707,47.4738056679536,123.857124325427)) ;
#32682 = CARTESIAN_POINT('Ctrl Pts',(-20.5613779800688,47.2938165875907,123.768050447587)) ;
#32683 = CARTESIAN_POINT('Ctrl Pts',(-20.750444918412,47.4837951196123,124.1002641636)) ;
#32684 = CARTESIAN_POINT('Ctrl Pts',(-20.4822143310711,47.3038060392494,123.962563117497)) ;
#32685 = CARTESIAN_POINT('Ctrl Pts',(-20.6110220669267,47.4937542099777,124.321740017003)) ;
#32686 = CARTESIAN_POINT('Ctrl Pts',(-20.3706779971095,47.3137651296148,124.13974493574)) ;
#32687 = CARTESIAN_POINT('Ctrl Pts',(-20.4368281965108,47.503651522284,124.514904688104)) ;
#32688 = CARTESIAN_POINT('Ctrl Pts',(-20.2313246021344,47.3236624419211,124.294278151825)) ;
#32689 = CARTESIAN_POINT('Ctrl Pts',(-20.2283967744204,47.5137079481842,124.677338457595)) ;
#32690 = CARTESIAN_POINT('Ctrl Pts',(-20.064580902708,47.3337188678213,124.424226901582)) ;
#32691 = CARTESIAN_POINT('Ctrl Pts',(-19.9992773799533,47.523577950774,124.798958001509)) ;
#32692 = CARTESIAN_POINT('Ctrl Pts',(-19.8812864635495,47.3435888704111,124.521524526354)) ;
#32693 = CARTESIAN_POINT('Ctrl Pts',(-19.7493845402161,47.5335818839512,124.880515352736)) ;
#32694 = CARTESIAN_POINT('Ctrl Pts',(-19.6813728797849,47.3535928035883,124.586772510695)) ;
#32695 = CARTESIAN_POINT('Ctrl Pts',(-19.4894723640348,47.5435691444151,124.917254732859)) ;
#32696 = CARTESIAN_POINT('Ctrl Pts',(-19.4734436940258,47.3635800640522,124.616166289918)) ;
#32697 = CARTESIAN_POINT('Ctrl Pts',(-19.2261503135035,47.5535961960008,124.908119289949)) ;
#32698 = CARTESIAN_POINT('Ctrl Pts',(-19.2627853251842,47.3736071156379,124.608859963816)) ;
#32699 = CARTESIAN_POINT('Ctrl Pts',(-18.9718149570964,47.5634872858269,124.854385043497)) ;
#32700 = CARTESIAN_POINT('Ctrl Pts',(-19.0593192486441,47.383498205464,124.565875589659)) ;
#32701 = CARTESIAN_POINT('Ctrl Pts',(-18.6475331408761,47.576785040608,124.724300286802)) ;
#32702 = CARTESIAN_POINT('Ctrl Pts',(-18.7998792298712,47.3967959602451,124.461806395647)) ;
#32703 = CARTESIAN_POINT('Ctrl Pts',(-18.3663382799237,47.5899831002161,124.51451143139)) ;
#32704 = CARTESIAN_POINT('Ctrl Pts',(-18.5749054443382,47.4099940198532,124.29395298759)) ;
#32705 = CARTESIAN_POINT('Ctrl Pts',(-18.1483991888473,47.6033798407853,124.238054641967)) ;
#32706 = CARTESIAN_POINT('Ctrl Pts',(-18.4005844644017,47.4233907604224,124.072822927662)) ;
#32707 = CARTESIAN_POINT('Ctrl Pts',(-18.025347143704,47.6132507528587,124.009644853001)) ;
#32708 = CARTESIAN_POINT('Ctrl Pts',(-18.3021342785884,47.4332616724959,123.890089214301)) ;
#32709 = CARTESIAN_POINT('Ctrl Pts',(-17.9421929511721,47.6233243146269,123.758382877817)) ;
#32710 = CARTESIAN_POINT('Ctrl Pts',(-18.2356106624253,47.443335234264,123.689082422527)) ;
#32711 = CARTESIAN_POINT('Ctrl Pts',(-17.9045616883877,47.6331457272152,123.502983370987)) ;
#32712 = CARTESIAN_POINT('Ctrl Pts',(-18.2055029686415,47.4531566468523,123.484761871704)) ;
#32713 = CARTESIAN_POINT('Ctrl Pts',(-17.911781843042,47.6432197444462,123.238412336144)) ;
#32714 = CARTESIAN_POINT('Ctrl Pts',(-18.2112771669349,47.4632306640834,123.273106890456)) ;
#32715 = CARTESIAN_POINT('Ctrl Pts',(-17.9808569614933,47.6563785314108,122.899509564629)) ;
#32716 = CARTESIAN_POINT('Ctrl Pts',(-18.2665340443339,47.4763894510479,123.001975913631)) ;
#32717 = CARTESIAN_POINT('Ctrl Pts',(-18.1386436633673,47.669744634505,122.581350825213)) ;
#32718 = CARTESIAN_POINT('Ctrl Pts',(-18.3927847615618,47.4897555541421,122.74742093734)) ;
#32719 = CARTESIAN_POINT('Ctrl Pts',(-18.370652315842,47.683058569394,122.319320691079)) ;
#32720 = CARTESIAN_POINT('Ctrl Pts',(-18.5783616726508,47.5030694890312,122.537834646464)) ;
#32721 = CARTESIAN_POINT('Ctrl Pts',(-18.5739282398627,47.6929586088415,122.157012936139)) ;
#32722 = CARTESIAN_POINT('Ctrl Pts',(-18.7409870352096,47.5129695284786,122.407978673393)) ;
#32723 = CARTESIAN_POINT('Ctrl Pts',(-18.8036181717246,47.702923011976,122.031241515346)) ;
#32724 = CARTESIAN_POINT('Ctrl Pts',(-18.9247363827808,47.5229339316132,122.307361838149)) ;
#32725 = CARTESIAN_POINT('Ctrl Pts',(-19.0533535758895,47.7129529790972,121.946938831321)) ;
#32726 = CARTESIAN_POINT('Ctrl Pts',(-19.1245251698578,47.5329638987343,122.239917409977)) ;
#32727 = CARTESIAN_POINT('Ctrl Pts',(-19.3105838879911,47.7228552557062,121.907675661922)) ;
#32728 = CARTESIAN_POINT('Ctrl Pts',(-19.3303061564412,47.5428661753434,122.208504383687)) ;
#32729 = CARTESIAN_POINT('Ctrl Pts',(-19.6591650885652,47.7361211848754,121.914819682812)) ;
#32730 = CARTESIAN_POINT('Ctrl Pts',(-19.609187461542,47.5561321045125,122.214219997551)) ;
#32731 = CARTESIAN_POINT('Ctrl Pts',(-20.0833550247634,47.7527427159818,122.037930509702)) ;
#32732 = CARTESIAN_POINT('Ctrl Pts',(-19.9485240134624,47.5727536356189,122.312705495618)) ;
#32733 = CARTESIAN_POINT('Ctrl Pts',(-20.510453729545,47.7726175446265,122.348898697034)) ;
#32734 = CARTESIAN_POINT('Ctrl Pts',(-20.2902038142842,47.5926284642636,122.561462978366)) ;
#32735 = CARTESIAN_POINT('Ctrl Pts',(-20.7582479358267,47.7892907527283,122.71623189636)) ;
#32736 = CARTESIAN_POINT('Ctrl Pts',(-20.4884640703777,47.6093016723655,122.855376229388)) ;
#32737 = CARTESIAN_POINT('Ctrl Pts',(-20.8714295868913,47.8025418777096,123.04557591284)) ;
#32738 = CARTESIAN_POINT('Ctrl Pts',(-20.5789911114765,47.6225527973467,123.118807090608)) ;
#32739 = CARTESIAN_POINT('Ctrl Pts',(-20.9269298434521,47.8157841965304,123.389178316211)) ;
#32740 = CARTESIAN_POINT('Ctrl Pts',(-20.6233964746189,47.6357951161676,123.393706836067)) ;
#32741 = CARTESIAN_POINT('Ctrl Pts',(-20.881145520325,47.8325174368699,123.831476120658)) ;
#32742 = CARTESIAN_POINT('Ctrl Pts',(-20.5867718080052,47.652528356507,123.747531615695)) ;
#32743 = CARTESIAN_POINT('Ctrl Pts',(-20.6511822086368,47.8523465850579,124.305796219641)) ;
#32744 = CARTESIAN_POINT('Ctrl Pts',(-20.4028036328943,47.672357504695,124.126994379831)) ;
#32745 = CARTESIAN_POINT('Ctrl Pts',(-20.2723934902227,47.8722712801585,124.675711001554)) ;
#32746 = CARTESIAN_POINT('Ctrl Pts',(-20.0997742015209,47.6922821997956,124.422927479501)) ;
#32747 = CARTESIAN_POINT('Ctrl Pts',(-19.7899432576281,47.8921945087419,124.89417687357)) ;
#32748 = CARTESIAN_POINT('Ctrl Pts',(-19.7138146109579,47.7122054283791,124.597703165401)) ;
#32749 = CARTESIAN_POINT('Ctrl Pts',(-19.2619554888101,47.912121647868,124.935052545408)) ;
#32750 = CARTESIAN_POINT('Ctrl Pts',(-19.2914239665457,47.7321325675052,124.630406187641)) ;
#32751 = CARTESIAN_POINT('Ctrl Pts',(-18.7527354696576,47.9319981104837,124.794293876189)) ;
#32752 = CARTESIAN_POINT('Ctrl Pts',(-18.8840463051201,47.7520090301208,124.51780103702)) ;
#32753 = CARTESIAN_POINT('Ctrl Pts',(-18.3198015893089,47.951975339089,124.486914551041)) ;
#32754 = CARTESIAN_POINT('Ctrl Pts',(-18.5376979391742,47.7719862587261,124.271898997653)) ;
#32755 = CARTESIAN_POINT('Ctrl Pts',(-18.0187050938315,47.9719101970627,124.050892286809)) ;
#32756 = CARTESIAN_POINT('Ctrl Pts',(-18.2968188352507,47.7919211166998,123.923081749406)) ;
#32757 = CARTESIAN_POINT('Ctrl Pts',(-17.8842318765923,47.9918066459935,123.539502996666)) ;
#32758 = CARTESIAN_POINT('Ctrl Pts',(-18.1892385060343,47.8118175656306,123.51396964369)) ;
#32759 = CARTESIAN_POINT('Ctrl Pts',(-17.9318165298211,48.0117279300601,123.012148120241)) ;
#32760 = CARTESIAN_POINT('Ctrl Pts',(-18.227305199235,47.8317388496972,123.092084787911)) ;
#32761 = CARTESIAN_POINT('Ctrl Pts',(-18.1570558911766,48.0316845797311,122.53190203543)) ;
#32762 = CARTESIAN_POINT('Ctrl Pts',(-18.4074959798686,47.8516954993682,122.7078870895)) ;
#32763 = CARTESIAN_POINT('Ctrl Pts',(-18.5309774065162,48.0515618728427,122.158784664484)) ;
#32764 = CARTESIAN_POINT('Ctrl Pts',(-18.7066337296029,47.8715727924798,122.409391583344)) ;
#32765 = CARTESIAN_POINT('Ctrl Pts',(-19.0095199143223,48.0714483450711,121.934235959805)) ;
#32766 = CARTESIAN_POINT('Ctrl Pts',(-19.0894691453368,47.8914592647082,122.229752104761)) ;
#32767 = CARTESIAN_POINT('Ctrl Pts',(-19.540633493891,48.0915099109951,121.886851609452)) ;
#32768 = CARTESIAN_POINT('Ctrl Pts',(-19.5143591422602,47.9115208306322,122.191844655207)) ;
#32769 = CARTESIAN_POINT('Ctrl Pts',(-20.0501821768271,48.1113503185359,122.022521216227)) ;
#32770 = CARTESIAN_POINT('Ctrl Pts',(-19.9220001526352,47.931361238173,122.300380806211)) ;
#32771 = CARTESIAN_POINT('Ctrl Pts',(-20.4843799802069,48.1312016425088,122.322303458234)) ;
#32772 = CARTESIAN_POINT('Ctrl Pts',(-20.2693591621974,47.9512125621459,122.540208559723)) ;
#32773 = CARTESIAN_POINT('Ctrl Pts',(-20.7926161664346,48.1512549124602,122.757030819445)) ;
#32774 = CARTESIAN_POINT('Ctrl Pts',(-20.5159469547042,47.9712658320974,122.887990515959)) ;
#32775 = CARTESIAN_POINT('Ctrl Pts',(-20.93252583496,48.1710755698436,123.265061844735)) ;
#32776 = CARTESIAN_POINT('Ctrl Pts',(-20.627874051427,47.9910864894807,123.294417505765)) ;
#32777 = CARTESIAN_POINT('Ctrl Pts',(-20.8912365983079,48.1910469911741,123.794086280571)) ;
#32778 = CARTESIAN_POINT('Ctrl Pts',(-20.5948408958009,48.0110579108112,123.717637230084)) ;
#32779 = CARTESIAN_POINT('Ctrl Pts',(-20.6727225902505,48.2109404835378,124.275764014104)) ;
#32780 = CARTESIAN_POINT('Ctrl Pts',(-20.4200275548019,48.0309514031749,124.102979505904)) ;
#32781 = CARTESIAN_POINT('Ctrl Pts',(-20.3004819424767,48.2309645697788,124.655976968053)) ;
#32782 = CARTESIAN_POINT('Ctrl Pts',(-20.1222337727236,48.050975489416,124.407148369197)) ;
#32783 = CARTESIAN_POINT('Ctrl Pts',(-19.8260643109497,48.2507694488917,124.884148701362)) ;
#32784 = CARTESIAN_POINT('Ctrl Pts',(-19.7426971430051,48.0707803685288,124.589684526452)) ;
#32785 = CARTESIAN_POINT('Ctrl Pts',(-19.298401689414,48.2707284645896,124.938563164576)) ;
#32786 = CARTESIAN_POINT('Ctrl Pts',(-19.3205664831375,48.0907393842267,124.633213331361)) ;
#32787 = CARTESIAN_POINT('Ctrl Pts',(-18.7834401752579,48.2907144882186,124.808270536172)) ;
#32788 = CARTESIAN_POINT('Ctrl Pts',(-18.9085977754014,48.1107254078558,124.528976723537)) ;
#32789 = CARTESIAN_POINT('Ctrl Pts',(-18.3471324483424,48.3105229839791,124.513544556307)) ;
#32790 = CARTESIAN_POINT('Ctrl Pts',(-18.5595521151312,48.1305339036163,124.29319269375)) ;
#32791 = CARTESIAN_POINT('Ctrl Pts',(-18.0344280932835,48.3305056230847,124.084394876722)) ;
#32792 = CARTESIAN_POINT('Ctrl Pts',(-18.3093912303342,48.1505165427219,123.949870956698)) ;
#32793 = CARTESIAN_POINT('Ctrl Pts',(-17.8877491679608,48.3503870708787,123.576606049549)) ;
#32794 = CARTESIAN_POINT('Ctrl Pts',(-18.1920510956395,48.1703979905159,123.543638317555)) ;
#32795 = CARTESIAN_POINT('Ctrl Pts',(-17.9228534217252,48.3703435376163,123.047472668677)) ;
#32796 = CARTESIAN_POINT('Ctrl Pts',(-18.2201380308155,48.1903544572534,123.120331605847)) ;
#32797 = CARTESIAN_POINT('Ctrl Pts',(-18.1353200268485,48.3902209345718,122.563676201082)) ;
#32798 = CARTESIAN_POINT('Ctrl Pts',(-18.3901149639764,48.210231854209,122.733295384716)) ;
#32799 = CARTESIAN_POINT('Ctrl Pts',(-18.5017348375152,48.4102028807471,122.179310317759)) ;
#32800 = CARTESIAN_POINT('Ctrl Pts',(-18.6832494823206,48.2302138003843,122.425805199473)) ;
#32801 = CARTESIAN_POINT('Ctrl Pts',(-18.9763255338847,48.4301319797839,121.943845821942)) ;
#32802 = CARTESIAN_POINT('Ctrl Pts',(-19.0629244628759,48.250142899421,122.237437292873)) ;
#32803 = CARTESIAN_POINT('Ctrl Pts',(-19.5025485758174,48.4500606029965,121.8844085627)) ;
#32804 = CARTESIAN_POINT('Ctrl Pts',(-19.4839018350502,48.2700715226336,122.189890020095)) ;
#32805 = CARTESIAN_POINT('Ctrl Pts',(-20.0154041734413,48.4698949271029,122.006602474331)) ;
#32806 = CARTESIAN_POINT('Ctrl Pts',(-19.8941925598735,48.28990584674,122.287654399379)) ;
#32807 = CARTESIAN_POINT('Ctrl Pts',(-20.3852740340378,48.4865472144863,122.249514009236)) ;
#32808 = CARTESIAN_POINT('Ctrl Pts',(-20.1900656488884,48.3065581341234,122.481970779686)) ;
#32809 = CARTESIAN_POINT('Ctrl Pts',(-20.6170557319961,48.4998077155085,122.509808729621)) ;
#32810 = CARTESIAN_POINT('Ctrl Pts',(-20.3755074720273,48.3198186351457,122.690222602484)) ;
#32811 = CARTESIAN_POINT('Ctrl Pts',(-20.7555225669231,48.5098091927098,122.73319887295)) ;
#32812 = CARTESIAN_POINT('Ctrl Pts',(-20.4862754159992,48.3298201123469,122.868932815288)) ;
#32813 = CARTESIAN_POINT('Ctrl Pts',(-20.8529891978789,48.5198412135693,122.978158629166)) ;
#32814 = CARTESIAN_POINT('Ctrl Pts',(-20.5642475521182,48.3398521332064,123.064902698722)) ;
#32815 = CARTESIAN_POINT('Ctrl Pts',(-20.9058519382839,48.5297047572949,123.231906669117)) ;
#32816 = CARTESIAN_POINT('Ctrl Pts',(-20.6065360580068,48.349715676932,123.267899228391)) ;
#32817 = CARTESIAN_POINT('Ctrl Pts',(-20.9146324101858,48.539673470965,123.493731289981)) ;
#32818 = CARTESIAN_POINT('Ctrl Pts',(-20.613556026208,48.3596843906021,123.477368180223)) ;
#32819 = CARTESIAN_POINT('Ctrl Pts',(-20.8648547231583,48.5530192183687,123.840870176946)) ;
#32820 = CARTESIAN_POINT('Ctrl Pts',(-20.5737423451447,48.3730301380058,123.755033409764)) ;
#32821 = CARTESIAN_POINT('Ctrl Pts',(-20.7281894338226,48.5661697734414,124.16259745941)) ;
#32822 = CARTESIAN_POINT('Ctrl Pts',(-20.4644056241511,48.3861806930785,124.012444016206)) ;
#32823 = CARTESIAN_POINT('Ctrl Pts',(-20.5118249048892,48.5795551539912,124.439903596676)) ;
#32824 = CARTESIAN_POINT('Ctrl Pts',(-20.2913023607941,48.3995660736284,124.234297052958)) ;
#32825 = CARTESIAN_POINT('Ctrl Pts',(-20.3188115906214,48.5894430899841,124.613917552832)) ;
#32826 = CARTESIAN_POINT('Ctrl Pts',(-20.1368920377986,48.4094540096212,124.373504600187)) ;
#32827 = CARTESIAN_POINT('Ctrl Pts',(-20.0965059871697,48.5994342797967,124.753554193822)) ;
#32828 = CARTESIAN_POINT('Ctrl Pts',(-19.9590458940921,48.4194451994339,124.485212524752)) ;
#32829 = CARTESIAN_POINT('Ctrl Pts',(-19.8542566549361,48.609386378335,124.852215716831)) ;
#32830 = CARTESIAN_POINT('Ctrl Pts',(-19.7652457303651,48.4293972979721,124.5641395104)) ;
#32831 = CARTESIAN_POINT('Ctrl Pts',(-19.5961577410576,48.6194326347855,124.907656726796)) ;
#32832 = CARTESIAN_POINT('Ctrl Pts',(-19.5587661686804,48.4394435544226,124.608490145194)) ;
#32833 = CARTESIAN_POINT('Ctrl Pts',(-19.337504837007,48.6292820821796,124.917439257159)) ;
#32834 = CARTESIAN_POINT('Ctrl Pts',(-19.3518437348216,48.4492930018168,124.616313910644)) ;
#32835 = CARTESIAN_POINT('Ctrl Pts',(-19.078037022272,48.6392447346748,124.882575057759)) ;
#32836 = CARTESIAN_POINT('Ctrl Pts',(-19.1442698490704,48.4592556543119,124.588420320008)) ;
#32837 = CARTESIAN_POINT('Ctrl Pts',(-18.8271502999389,48.6492678203169,124.802367820736)) ;
#32838 = CARTESIAN_POINT('Ctrl Pts',(-18.9435612086211,48.469278739954,124.524252395797)) ;
#32839 = CARTESIAN_POINT('Ctrl Pts',(-18.5961153422512,48.6591929360738,124.681264951306)) ;
#32840 = CARTESIAN_POINT('Ctrl Pts',(-18.7587343441336,48.479203855711,124.427368128863)) ;
#32841 = CARTESIAN_POINT('Ctrl Pts',(-18.3870750955819,48.6692454144736,124.519790373217)) ;
#32842 = CARTESIAN_POINT('Ctrl Pts',(-18.5915035653785,48.4892563341108,124.298186706336)) ;
#32843 = CARTESIAN_POINT('Ctrl Pts',(-18.2126444694148,48.6790969131764,124.328462267053)) ;
#32844 = CARTESIAN_POINT('Ctrl Pts',(-18.4519607973613,48.4991078328135,124.14512276976)) ;
#32845 = CARTESIAN_POINT('Ctrl Pts',(-18.0718445075732,48.6890686523789,124.107495060904)) ;
#32846 = CARTESIAN_POINT('Ctrl Pts',(-18.339322775097,48.509079572016,123.968347874547)) ;
#32847 = CARTESIAN_POINT('Ctrl Pts',(-17.9713155069276,48.6990638601446,123.86478462589)) ;
#32848 = CARTESIAN_POINT('Ctrl Pts',(-18.2589016723393,48.5190747797817,123.774178726449)) ;
#32849 = CARTESIAN_POINT('Ctrl Pts',(-17.9145635742469,48.7090978616136,123.607305099869)) ;
#32850 = CARTESIAN_POINT('Ctrl Pts',(-18.213502337176,48.5291087812508,123.568194649321)) ;
#32851 = CARTESIAN_POINT('Ctrl Pts',(-17.9031654069168,48.718953219706,123.348541528174)) ;
#32852 = CARTESIAN_POINT('Ctrl Pts',(-18.2043860513762,48.5389641393431,123.361183881843)) ;
#32853 = CARTESIAN_POINT('Ctrl Pts',(-17.937003026666,48.7289526952993,123.088000944887)) ;
#32854 = CARTESIAN_POINT('Ctrl Pts',(-18.231458353244,48.5489636149364,123.152751774568)) ;
#32855 = CARTESIAN_POINT('Ctrl Pts',(-18.0144858731634,48.7388471437944,122.839746756377)) ;
#32856 = CARTESIAN_POINT('Ctrl Pts',(-18.29344667902,48.5588580634315,122.954149283923)) ;
#32857 = CARTESIAN_POINT('Ctrl Pts',(-18.1359580112243,48.7489102680221,122.604899456879)) ;
#32858 = CARTESIAN_POINT('Ctrl Pts',(-18.3906263763058,48.5689211876593,122.766272439426)) ;
#32859 = CARTESIAN_POINT('Ctrl Pts',(-18.2926260056632,48.7587498943507,122.399136493447)) ;
#32860 = CARTESIAN_POINT('Ctrl Pts',(-18.5159623218924,48.5787608139879,122.601663664949)) ;
#32861 = CARTESIAN_POINT('Ctrl Pts',(-18.4866726839865,48.7688131293937,122.219522458127)) ;
#32862 = CARTESIAN_POINT('Ctrl Pts',(-18.6712011734618,48.5888240490308,122.457974012859)) ;
#32863 = CARTESIAN_POINT('Ctrl Pts',(-18.7053931823134,48.7787071346277,122.078888414331)) ;
#32864 = CARTESIAN_POINT('Ctrl Pts',(-18.8461785372344,48.5987180542649,122.345468767959)) ;
#32865 = CARTESIAN_POINT('Ctrl Pts',(-18.9460602718396,48.7886498478435,121.977234200229)) ;
#32866 = CARTESIAN_POINT('Ctrl Pts',(-19.038712845065,48.6086607674806,122.264147453385)) ;
#32867 = CARTESIAN_POINT('Ctrl Pts',(-19.2023805082056,48.7986555876417,121.918479266341)) ;
#32868 = CARTESIAN_POINT('Ctrl Pts',(-19.2437694535632,48.6186665072788,122.217145598752)) ;
#32869 = CARTESIAN_POINT('Ctrl Pts',(-19.4653884139487,48.8086764897881,121.905400360003)) ;
#32870 = CARTESIAN_POINT('Ctrl Pts',(-19.4541758671944,48.6286874094252,122.206684634383)) ;
#32871 = CARTESIAN_POINT('Ctrl Pts',(-19.7233301714243,48.818567259837,121.937466358609)) ;
#32872 = CARTESIAN_POINT('Ctrl Pts',(-19.660528678975,48.6385781794741,122.232339509988)) ;
#32873 = CARTESIAN_POINT('Ctrl Pts',(-19.9744129235702,48.8285586706167,122.014229612701)) ;
#32874 = CARTESIAN_POINT('Ctrl Pts',(-19.8613941678022,48.6485695902538,122.29375209031)) ;
#32875 = CARTESIAN_POINT('Ctrl Pts',(-20.2073088426993,48.8385070162812,122.13298779378)) ;
#32876 = CARTESIAN_POINT('Ctrl Pts',(-20.0477097505346,48.6585179359183,122.388760413796)) ;
#32877 = CARTESIAN_POINT('Ctrl Pts',(-20.4163278633967,48.8484518743424,122.289901832939)) ;
#32878 = CARTESIAN_POINT('Ctrl Pts',(-20.2149235466463,48.6684627939795,122.514293137704)) ;
#32879 = CARTESIAN_POINT('Ctrl Pts',(-20.5965846062851,48.8585067097353,122.483065165235)) ;
#32880 = CARTESIAN_POINT('Ctrl Pts',(-20.3591274717753,48.6785176293724,122.66882529591)) ;
#32881 = CARTESIAN_POINT('Ctrl Pts',(-20.7376368968491,48.8683290818368,122.699266149593)) ;
#32882 = CARTESIAN_POINT('Ctrl Pts',(-20.4719672538664,48.6883400014739,122.841786671009)) ;
#32883 = CARTESIAN_POINT('Ctrl Pts',(-20.8418372689003,48.8783849492805,122.942091527948)) ;
#32884 = CARTESIAN_POINT('Ctrl Pts',(-20.555325764693,48.6983958689176,123.036047837099)) ;
#32885 = CARTESIAN_POINT('Ctrl Pts',(-20.9011534756052,48.8883256791384,123.196510502706)) ;
#32886 = CARTESIAN_POINT('Ctrl Pts',(-20.6027766814318,48.7083365987755,123.239583219455)) ;
#32887 = CARTESIAN_POINT('Ctrl Pts',(-20.9161549876618,48.8982300176895,123.456358415646)) ;
#32888 = CARTESIAN_POINT('Ctrl Pts',(-20.6147759351108,48.7182409373267,123.447461235112)) ;
#32889 = CARTESIAN_POINT('Ctrl Pts',(-20.8852105592629,48.908276699118,123.718532273713)) ;
#32890 = CARTESIAN_POINT('Ctrl Pts',(-20.5900184387417,48.7282876187551,123.657200174612)) ;
#32891 = CARTESIAN_POINT('Ctrl Pts',(-20.810567540589,48.9181722065873,123.967677397249)) ;
#32892 = CARTESIAN_POINT('Ctrl Pts',(-20.530302315986,48.7381831262244,123.856515274534)) ;
#32893 = CARTESIAN_POINT('Ctrl Pts',(-20.6918640066937,48.9282344750859,124.203918318717)) ;
#32894 = CARTESIAN_POINT('Ctrl Pts',(-20.4353377019454,48.748245394723,124.045507277748)) ;
#32895 = CARTESIAN_POINT('Ctrl Pts',(-20.5374874732684,48.9380764653565,124.4114706526)) ;
#32896 = CARTESIAN_POINT('Ctrl Pts',(-20.3118353640093,48.7580873849936,124.211547452761)) ;
#32897 = CARTESIAN_POINT('Ctrl Pts',(-20.346982966348,48.9480698822375,124.59217583248)) ;
#32898 = CARTESIAN_POINT('Ctrl Pts',(-20.1594306094742,48.7680808018746,124.356110185967)) ;
#32899 = CARTESIAN_POINT('Ctrl Pts',(-20.1294622771985,48.9579943700896,124.736115686117)) ;
#32900 = CARTESIAN_POINT('Ctrl Pts',(-19.9854133980772,48.7780052897268,124.471260339818)) ;
#32901 = CARTESIAN_POINT('Ctrl Pts',(-19.8885974147487,48.9679940039981,124.841121711921)) ;
#32902 = CARTESIAN_POINT('Ctrl Pts',(-19.7927208876813,48.7880049236352,124.555263504968)) ;
#32903 = CARTESIAN_POINT('Ctrl Pts',(-19.6334469697658,48.9779801142549,124.9026502756)) ;
#32904 = CARTESIAN_POINT('Ctrl Pts',(-19.5886002554755,48.797991033892,124.604484611095)) ;
#32905 = CARTESIAN_POINT('Ctrl Pts',(-19.3702291570135,48.988016065442,124.918743054803)) ;
#32906 = CARTESIAN_POINT('Ctrl Pts',(-19.3780258273931,48.8080269850791,124.617357030523)) ;
#32907 = CARTESIAN_POINT('Ctrl Pts',(-19.1128025382839,48.9978727037768,124.889803469788)) ;
#32908 = CARTESIAN_POINT('Ctrl Pts',(-19.1720854580198,48.8178836234139,124.594203711341)) ;
#32909 = CARTESIAN_POINT('Ctrl Pts',(-18.8606911455665,49.0078716638548,124.815911669425)) ;
#32910 = CARTESIAN_POINT('Ctrl Pts',(-18.9703969207896,48.8278825834919,124.535088685264)) ;
#32911 = CARTESIAN_POINT('Ctrl Pts',(-18.6274774420179,49.0177668941686,124.700789980476)) ;
#32912 = CARTESIAN_POINT('Ctrl Pts',(-18.7838272068471,48.8377778138057,124.442990132716)) ;
#32913 = CARTESIAN_POINT('Ctrl Pts',(-18.4143731818113,49.0278274066372,124.544376734575)) ;
#32914 = CARTESIAN_POINT('Ctrl Pts',(-18.6133446125383,48.8478383262744,124.317858101007)) ;
#32915 = CARTESIAN_POINT('Ctrl Pts',(-18.2353571530203,49.0376766981834,124.357410469631)) ;
#32916 = CARTESIAN_POINT('Ctrl Pts',(-18.4701335294732,48.8576876178205,124.168284578467)) ;
#32917 = CARTESIAN_POINT('Ctrl Pts',(-18.0883869155088,49.0477038841156,124.13870846236)) ;
#32918 = CARTESIAN_POINT('Ctrl Pts',(-18.3525585546623,48.8677148037527,123.993322118891)) ;
#32919 = CARTESIAN_POINT('Ctrl Pts',(-17.9822338382996,49.0577324205749,123.89747926818)) ;
#32920 = CARTESIAN_POINT('Ctrl Pts',(-18.2676375508408,48.8777433402121,123.800338060987)) ;
#32921 = CARTESIAN_POINT('Ctrl Pts',(-17.9202532459207,49.0675776605399,123.646304603655)) ;
#32922 = CARTESIAN_POINT('Ctrl Pts',(-18.2180547698184,48.887588580177,123.599398834632)) ;
#32923 = CARTESIAN_POINT('Ctrl Pts',(-17.9018658552473,49.0775683554631,123.384397836007)) ;
#32924 = CARTESIAN_POINT('Ctrl Pts',(-18.2033462475352,48.8975792751002,123.389873479783)) ;
#32925 = CARTESIAN_POINT('Ctrl Pts',(-17.9299430170255,49.0876061762217,123.122114050778)) ;
#32926 = CARTESIAN_POINT('Ctrl Pts',(-18.2258094796159,48.9076170958588,123.180046505559)) ;
#32927 = CARTESIAN_POINT('Ctrl Pts',(-18.0013047262961,49.0974507699987,122.873439403411)) ;
#32928 = CARTESIAN_POINT('Ctrl Pts',(-18.2828999451431,48.9174616896358,122.981108076686)) ;
#32929 = CARTESIAN_POINT('Ctrl Pts',(-18.1158511804771,49.1074347653747,122.637421711162)) ;
#32930 = CARTESIAN_POINT('Ctrl Pts',(-18.3745381797035,48.9274456850118,122.792294678741)) ;
#32931 = CARTESIAN_POINT('Ctrl Pts',(-18.2691440175312,49.1173838139361,122.425609469171)) ;
#32932 = CARTESIAN_POINT('Ctrl Pts',(-18.4971732750292,48.9373947335732,122.622845958059)) ;
#32933 = CARTESIAN_POINT('Ctrl Pts',(-18.4576938725769,49.1273862529106,122.242453382412)) ;
#32934 = CARTESIAN_POINT('Ctrl Pts',(-18.6480139645982,48.9473971725478,122.476322036241)) ;
#32935 = CARTESIAN_POINT('Ctrl Pts',(-18.6757844901155,49.137407494207,122.094840814009)) ;
#32936 = CARTESIAN_POINT('Ctrl Pts',(-18.8224872183678,48.9574184138441,122.358233056651)) ;
#32937 = CARTESIAN_POINT('Ctrl Pts',(-18.912980073684,49.1473001726465,121.988431832938)) ;
#32938 = CARTESIAN_POINT('Ctrl Pts',(-19.0122435443815,48.9673110922836,122.273107306657)) ;
#32939 = CARTESIAN_POINT('Ctrl Pts',(-19.1674232251513,49.1572902265941,121.923790931797)) ;
#32940 = CARTESIAN_POINT('Ctrl Pts',(-19.2157981795932,48.9773011462313,122.221395753359)) ;
#32941 = CARTESIAN_POINT('Ctrl Pts',(-19.4284019621495,49.1672485877426,121.904559887262)) ;
#32942 = CARTESIAN_POINT('Ctrl Pts',(-19.4245809128314,48.9872595073797,122.206012139739)) ;
#32943 = CARTESIAN_POINT('Ctrl Pts',(-19.6873094646854,49.1771482146274,121.930145178779)) ;
#32944 = CARTESIAN_POINT('Ctrl Pts',(-19.6317061102632,48.9971591342646,122.226481354379)) ;
#32945 = CARTESIAN_POINT('Ctrl Pts',(-19.941526102593,49.1871961114308,122.001425268329)) ;
#32946 = CARTESIAN_POINT('Ctrl Pts',(-19.8350792979722,49.0072070310679,122.283506510641)) ;
#32947 = CARTESIAN_POINT('Ctrl Pts',(-20.1760417540059,49.1970914690668,122.113872563223)) ;
#32948 = CARTESIAN_POINT('Ctrl Pts',(-20.022690714718,49.0171023887039,122.373464959482)) ;
#32949 = CARTESIAN_POINT('Ctrl Pts',(-20.3909878097268,49.2071531215235,122.267804384145)) ;
#32950 = CARTESIAN_POINT('Ctrl Pts',(-20.1946471758079,49.0271640411606,122.496611400077)) ;
#32951 = CARTESIAN_POINT('Ctrl Pts',(-20.5720068053571,49.2169977257954,122.452644101985)) ;
#32952 = CARTESIAN_POINT('Ctrl Pts',(-20.3394609075565,49.0370086454325,122.644483128646)) ;
#32953 = CARTESIAN_POINT('Ctrl Pts',(-20.7206623097227,49.2269578474934,122.668068984939)) ;
#32954 = CARTESIAN_POINT('Ctrl Pts',(-20.4583844503407,49.0469687671305,122.816823184735)) ;
#32955 = CARTESIAN_POINT('Ctrl Pts',(-20.8300406886576,49.2369958818559,122.90810181371)) ;
#32956 = CARTESIAN_POINT('Ctrl Pts',(-20.5458863746886,49.0570068014931,123.008849944546)) ;
#32957 = CARTESIAN_POINT('Ctrl Pts',(-20.895474107219,49.2468701944424,123.15923667191)) ;
#32958 = CARTESIAN_POINT('Ctrl Pts',(-20.5982321097899,49.0668811140795,123.209757165169)) ;
#32959 = CARTESIAN_POINT('Ctrl Pts',(-20.9167021696326,49.2569396752251,123.422962968094)) ;
#32960 = CARTESIAN_POINT('Ctrl Pts',(-20.6152137829838,49.0769505948622,123.420738590608)) ;
#32961 = CARTESIAN_POINT('Ctrl Pts',(-20.8925309748415,49.2667740112422,123.680288852952)) ;
#32962 = CARTESIAN_POINT('Ctrl Pts',(-20.5958761715019,49.0867849308793,123.626598057855)) ;
#32963 = CARTESIAN_POINT('Ctrl Pts',(-20.8233682239885,49.2768069689704,123.934702843844)) ;
#32964 = CARTESIAN_POINT('Ctrl Pts',(-20.5405453724813,49.0968178886076,123.830129187291)) ;
#32965 = CARTESIAN_POINT('Ctrl Pts',(-20.7105597644519,49.2868273675456,124.172644633411)) ;
#32966 = CARTESIAN_POINT('Ctrl Pts',(-20.4502978908563,49.1068382871827,124.020482314942)) ;
#32967 = CARTESIAN_POINT('Ctrl Pts',(-20.5610300420917,49.2966929413168,124.38445939655)) ;
#32968 = CARTESIAN_POINT('Ctrl Pts',(-20.3306741735145,49.116703860954,124.189932981708)) ;
#32969 = CARTESIAN_POINT('Ctrl Pts',(-20.3732384290242,49.3067618159729,124.570826297004)) ;
#32970 = CARTESIAN_POINT('Ctrl Pts',(-20.1804402169388,49.12677273561,124.33902629884)) ;
#32971 = CARTESIAN_POINT('Ctrl Pts',(-20.1607506292362,49.3166072468784,124.718462326025)) ;
#32972 = CARTESIAN_POINT('Ctrl Pts',(-20.0104505595802,49.1366181665155,124.457133981811)) ;
#32973 = CARTESIAN_POINT('Ctrl Pts',(-19.9230300882037,49.3265868717491,124.829197136237)) ;
#32974 = CARTESIAN_POINT('Ctrl Pts',(-19.820274187598,49.1465977913862,124.545721370372)) ;
#32975 = CARTESIAN_POINT('Ctrl Pts',(-19.6685730451368,49.3366055546632,124.896756529863)) ;
#32976 = CARTESIAN_POINT('Ctrl Pts',(-19.6167084117739,49.1566164743003,124.599768387045)) ;
#32977 = CARTESIAN_POINT('Ctrl Pts',(-19.4098038796016,49.346488819847,124.919356964503)) ;
#32978 = CARTESIAN_POINT('Ctrl Pts',(-19.4096939213468,49.1664997394842,124.617848281741)) ;
#32979 = CARTESIAN_POINT('Ctrl Pts',(-19.1462832607712,49.3565571139384,124.89615090551)) ;
#32980 = CARTESIAN_POINT('Ctrl Pts',(-19.1988771347697,49.1765680335755,124.599282999011)) ;
#32981 = CARTESIAN_POINT('Ctrl Pts',(-18.8966752356581,49.3663872441237,124.829435060277)) ;
#32982 = CARTESIAN_POINT('Ctrl Pts',(-18.999191990857,49.1863981637609,124.545910321874)) ;
#32983 = CARTESIAN_POINT('Ctrl Pts',(-18.656744831752,49.3764537923389,124.718117896912)) ;
#32984 = CARTESIAN_POINT('Ctrl Pts',(-18.8072474823496,49.196464711976,124.456856234754)) ;
#32985 = CARTESIAN_POINT('Ctrl Pts',(-18.4436181844938,49.3863440410275,124.569306863408)) ;
#32986 = CARTESIAN_POINT('Ctrl Pts',(-18.6367470167291,49.2063549606646,124.337807652728)) ;
#32987 = CARTESIAN_POINT('Ctrl Pts',(-18.2572992166369,49.3963362228035,124.384299698902)) ;
#32988 = CARTESIAN_POINT('Ctrl Pts',(-18.4876920638657,49.2163471424406,124.189801941018)) ;
#32989 = CARTESIAN_POINT('Ctrl Pts',(-18.1065741069592,49.4062990034313,124.170232758712)) ;
#32990 = CARTESIAN_POINT('Ctrl Pts',(-18.3671123543255,49.2263099230684,124.018548569717)) ;
#32991 = CARTESIAN_POINT('Ctrl Pts',(-17.9953598077173,49.4162034081051,123.934891647468)) ;
#32992 = CARTESIAN_POINT('Ctrl Pts',(-18.2781412702089,49.2362143277422,123.830276340777)) ;
#32993 = CARTESIAN_POINT('Ctrl Pts',(-17.9258209627765,49.4262634025841,123.679859999836)) ;
#32994 = CARTESIAN_POINT('Ctrl Pts',(-18.2225102077793,49.2462743222212,123.626250739129)) ;
#32995 = CARTESIAN_POINT('Ctrl Pts',(-17.9019035489539,49.4361120245539,123.422136143483)) ;
#32996 = CARTESIAN_POINT('Ctrl Pts',(-18.2033764111946,49.256122944191,123.42007277146)) ;
#32997 = CARTESIAN_POINT('Ctrl Pts',(-17.9228967151139,49.4461424639657,123.159399391363)) ;
#32998 = CARTESIAN_POINT('Ctrl Pts',(-18.2201708355214,49.2661533836029,123.209883266575)) ;
#32999 = CARTESIAN_POINT('Ctrl Pts',(-17.9895783325629,49.4561521796005,122.90491683128)) ;
#33000 = CARTESIAN_POINT('Ctrl Pts',(-18.2735161375883,49.2761630992376,123.006297255522)) ;
#33001 = CARTESIAN_POINT('Ctrl Pts',(-18.0980952655541,49.4660629322931,122.668183285469)) ;
#33002 = CARTESIAN_POINT('Ctrl Pts',(-18.3603293441848,49.2860738519302,122.816911054056)) ;
#33003 = CARTESIAN_POINT('Ctrl Pts',(-18.245826326081,49.4759922052395,122.453085432562)) ;
#33004 = CARTESIAN_POINT('Ctrl Pts',(-18.4785136798849,49.2960031248766,122.644833143533)) ;
#33005 = CARTESIAN_POINT('Ctrl Pts',(-18.4308927790873,49.4860348966322,122.264952869192)) ;
#33006 = CARTESIAN_POINT('Ctrl Pts',(-18.6265668504671,49.3060458162693,122.494326860631)) ;
#33007 = CARTESIAN_POINT('Ctrl Pts',(-18.6423948660931,49.4959214298497,122.114039679069)) ;
#33008 = CARTESIAN_POINT('Ctrl Pts',(-18.7957676964125,49.3159323494868,122.373596652419)) ;
#33009 = CARTESIAN_POINT('Ctrl Pts',(-18.8791977037883,49.5059145747817,122.000547015104)) ;
#33010 = CARTESIAN_POINT('Ctrl Pts',(-18.9852096849577,49.3259254944189,122.282802310595)) ;
#33011 = CARTESIAN_POINT('Ctrl Pts',(-19.1309496466814,49.5158602556182,121.930322869947)) ;
#33012 = CARTESIAN_POINT('Ctrl Pts',(-19.1866107041673,49.3358711752553,122.226622847818)) ;
#33013 = CARTESIAN_POINT('Ctrl Pts',(-19.3910719340289,49.5258075127667,121.904340399635)) ;
#33014 = CARTESIAN_POINT('Ctrl Pts',(-19.3947080350026,49.3458184324039,122.205836499033)) ;
#33015 = CARTESIAN_POINT('Ctrl Pts',(-19.6543477211243,49.5358554166387,121.924410607122)) ;
#33016 = CARTESIAN_POINT('Ctrl Pts',(-19.605328890607,49.3558663362759,122.221892336368)) ;
#33017 = CARTESIAN_POINT('Ctrl Pts',(-19.9051063909627,49.5457031157367,121.988376325681)) ;
#33018 = CARTESIAN_POINT('Ctrl Pts',(-19.8059348407056,49.3657140353738,122.273064246999)) ;
#33019 = CARTESIAN_POINT('Ctrl Pts',(-20.1440032593785,49.5556646067154,122.095383178499)) ;
#33020 = CARTESIAN_POINT('Ctrl Pts',(-19.9970522508123,49.3756755263525,122.358669026334)) ;
#33021 = CARTESIAN_POINT('Ctrl Pts',(-20.3619888762732,49.5656940691293,122.243550726972)) ;
#33022 = CARTESIAN_POINT('Ctrl Pts',(-20.1714411021644,49.3857049887665,122.47720268182)) ;
#33023 = CARTESIAN_POINT('Ctrl Pts',(-20.5487252565727,49.5756013002292,122.424969613015)) ;
#33024 = CARTESIAN_POINT('Ctrl Pts',(-20.3208300784889,49.3956122198664,122.622336896963)) ;
#33025 = CARTESIAN_POINT('Ctrl Pts',(-20.7021484057419,49.5855476789066,122.636565942067)) ;
#33026 = CARTESIAN_POINT('Ctrl Pts',(-20.4435688760117,49.4055585985438,122.791613175442)) ;
#33027 = CARTESIAN_POINT('Ctrl Pts',(-20.817273052069,49.5955524477155,122.872960551607)) ;
#33028 = CARTESIAN_POINT('Ctrl Pts',(-20.5356691966512,49.4155633673526,122.980728486746)) ;
#33029 = CARTESIAN_POINT('Ctrl Pts',(-20.8894241945035,49.6055735687357,123.126222955828)) ;
#33030 = CARTESIAN_POINT('Ctrl Pts',(-20.5933907246933,49.4255844883728,123.183338265928)) ;
#33031 = CARTESIAN_POINT('Ctrl Pts',(-20.9164510303163,49.6154644345883,123.384745011977)) ;
#33032 = CARTESIAN_POINT('Ctrl Pts',(-20.6150128120107,49.4354753542255,123.390155041313)) ;
#33033 = CARTESIAN_POINT('Ctrl Pts',(-20.8983831554368,49.6254552433476,123.64665553533)) ;
#33034 = CARTESIAN_POINT('Ctrl Pts',(-20.6005593184925,49.4454661629847,123.599683344797)) ;
#33035 = CARTESIAN_POINT('Ctrl Pts',(-20.8353127628865,49.6354059015279,123.900441641724)) ;
#33036 = CARTESIAN_POINT('Ctrl Pts',(-20.550103868979,49.4554168211651,123.802711999998)) ;
#33037 = CARTESIAN_POINT('Ctrl Pts',(-20.7296226128942,49.64534211117,124.139186358957)) ;
#33038 = CARTESIAN_POINT('Ctrl Pts',(-20.4655527511557,49.4653530308072,123.993707659371)) ;
#33039 = CARTESIAN_POINT('Ctrl Pts',(-20.5836489640743,49.6553252778949,124.357211327668)) ;
#33040 = CARTESIAN_POINT('Ctrl Pts',(-20.3487747338897,49.475336197532,124.168127991278)) ;
#33041 = CARTESIAN_POINT('Ctrl Pts',(-20.4006247563479,49.6653690751052,124.547345114736)) ;
#33042 = CARTESIAN_POINT('Ctrl Pts',(-20.2023558633861,49.4853799947423,124.320235708206)) ;
#33043 = CARTESIAN_POINT('Ctrl Pts',(-20.1922492122206,49.6751972912734,124.70000920038)) ;
#33044 = CARTESIAN_POINT('Ctrl Pts',(-20.0356569367093,49.4952082109106,124.442367083583)) ;
#33045 = CARTESIAN_POINT('Ctrl Pts',(-19.9548171286621,49.6852738587427,124.817128808093)) ;
#33046 = CARTESIAN_POINT('Ctrl Pts',(-19.84571140594,49.5052847783798,124.536063826559)) ;
#33047 = CARTESIAN_POINT('Ctrl Pts',(-19.706248503042,49.6951259444321,124.889748332412)) ;
#33048 = CARTESIAN_POINT('Ctrl Pts',(-19.646857742828,49.5151368640692,124.594160163181)) ;
#33049 = CARTESIAN_POINT('Ctrl Pts',(-19.4431934347657,49.7051992118375,124.918954084388)) ;
#33050 = CARTESIAN_POINT('Ctrl Pts',(-19.436413489415,49.5252101314746,124.617525881266)) ;
#33051 = CARTESIAN_POINT('Ctrl Pts',(-19.1850858539182,49.7150406282611,124.902355961624)) ;
#33052 = CARTESIAN_POINT('Ctrl Pts',(-19.2299283962633,49.5350515478982,124.604248517549)) ;
#33053 = CARTESIAN_POINT('Ctrl Pts',(-18.93051882681,49.7250018864038,124.841407931651)) ;
#33054 = CARTESIAN_POINT('Ctrl Pts',(-19.0262747888918,49.545012806041,124.555491422723)) ;
#33055 = CARTESIAN_POINT('Ctrl Pts',(-18.6887821551517,49.7350385628358,124.735926054212)) ;
#33056 = CARTESIAN_POINT('Ctrl Pts',(-18.8328848873509,49.5550494824729,124.471106955947)) ;
#33057 = CARTESIAN_POINT('Ctrl Pts',(-18.472223638631,49.7449171706996,124.592716974689)) ;
#33058 = CARTESIAN_POINT('Ctrl Pts',(-18.6596380365307,49.5649280903367,124.356541193233)) ;
#33059 = CARTESIAN_POINT('Ctrl Pts',(-18.2803615486336,49.7549773993384,124.410883615209)) ;
#33060 = CARTESIAN_POINT('Ctrl Pts',(-18.5061473145343,49.5749883189755,124.211075281749)) ;
#33061 = CARTESIAN_POINT('Ctrl Pts',(-18.1259078276829,49.7648443834992,124.2025693445)) ;
#33062 = CARTESIAN_POINT('Ctrl Pts',(-18.3825837898089,49.5848553031363,124.044425304176)) ;
#33063 = CARTESIAN_POINT('Ctrl Pts',(-18.007919160607,49.7748499497519,123.967632043592)) ;
#33064 = CARTESIAN_POINT('Ctrl Pts',(-18.2881916293145,49.594860869389,123.856476155528)) ;
#33065 = CARTESIAN_POINT('Ctrl Pts',(-17.9327202356782,49.7848337381665,123.716228002346)) ;
#33066 = CARTESIAN_POINT('Ctrl Pts',(-18.2280312110072,49.6048446578036,123.655353491718)) ;
#33067 = CARTESIAN_POINT('Ctrl Pts',(-17.9024202751919,49.7948795949691,123.453999545748)) ;
#33068 = CARTESIAN_POINT('Ctrl Pts',(-18.2037899069106,49.6148905146063,123.445570751579)) ;
#33069 = CARTESIAN_POINT('Ctrl Pts',(-17.9174338428605,49.8047054721851,123.196221483282)) ;
#33070 = CARTESIAN_POINT('Ctrl Pts',(-18.2157993021619,49.6247163918222,123.23934924798)) ;
#33071 = CARTESIAN_POINT('Ctrl Pts',(-17.9771398351836,49.8146959480264,122.940561425494)) ;
#33072 = CARTESIAN_POINT('Ctrl Pts',(-18.2635625340082,49.6347068676635,123.034820978752)) ;
#33073 = CARTESIAN_POINT('Ctrl Pts',(-18.0815158765867,49.8247395239252,122.698141841169)) ;
#33074 = CARTESIAN_POINT('Ctrl Pts',(-18.3470620957204,49.6447504435623,122.840884636504)) ;
#33075 = CARTESIAN_POINT('Ctrl Pts',(-18.2227460406671,49.8345613162232,122.482103844544)) ;
#33076 = CARTESIAN_POINT('Ctrl Pts',(-18.4600443913908,49.6545722358604,122.668054229687)) ;
#33077 = CARTESIAN_POINT('Ctrl Pts',(-18.4027042307795,49.8445962818491,122.289342033901)) ;
#33078 = CARTESIAN_POINT('Ctrl Pts',(-18.6040097854602,49.6646072014862,122.513843584762)) ;
#33079 = CARTESIAN_POINT('Ctrl Pts',(-18.6136336981396,49.8546211987822,122.131496311253)) ;
#33080 = CARTESIAN_POINT('Ctrl Pts',(-18.772752461505,49.6746321184193,122.38756577421)) ;
#33081 = CARTESIAN_POINT('Ctrl Pts',(-18.844452425863,49.8644731371583,122.014217927815)) ;
#33082 = CARTESIAN_POINT('Ctrl Pts',(-18.9574059859319,49.6844840567954,122.293741978756)) ;
#33083 = CARTESIAN_POINT('Ctrl Pts',(-19.0954698169911,49.8744641131831,121.937362207403)) ;
#33084 = CARTESIAN_POINT('Ctrl Pts',(-19.1582192690863,49.6944750328202,122.232255812791)) ;
#33085 = CARTESIAN_POINT('Ctrl Pts',(-19.3541562238253,49.8843819339867,121.905312031361)) ;
#33086 = CARTESIAN_POINT('Ctrl Pts',(-19.3651677277275,49.7043928536238,122.206614010283)) ;
#33087 = CARTESIAN_POINT('Ctrl Pts',(-19.6173285205986,49.8944106545513,121.918768394832)) ;
#33088 = CARTESIAN_POINT('Ctrl Pts',(-19.5757056845183,49.7144215741884,122.217377365489)) ;
#33089 = CARTESIAN_POINT('Ctrl Pts',(-19.8705237928236,49.9042935811605,121.976696588945)) ;
#33090 = CARTESIAN_POINT('Ctrl Pts',(-19.7782617108459,49.7243045007976,122.263718061929)) ;
#33091 = CARTESIAN_POINT('Ctrl Pts',(-20.1128653758692,49.91429786628,122.078541501099)) ;
#33092 = CARTESIAN_POINT('Ctrl Pts',(-19.9721356237173,49.7343087859171,122.345192269613)) ;
#33093 = CARTESIAN_POINT('Ctrl Pts',(-20.3334334359267,49.9242815474878,122.22068996082)) ;
#33094 = CARTESIAN_POINT('Ctrl Pts',(-20.1485909406997,49.7442924671249,122.458909422584)) ;
#33095 = CARTESIAN_POINT('Ctrl Pts',(-20.5268216963565,49.9343225462177,122.400179102875)) ;
#33096 = CARTESIAN_POINT('Ctrl Pts',(-20.3033028181441,49.7543334658549,122.602499480691)) ;
#33097 = CARTESIAN_POINT('Ctrl Pts',(-20.683102613612,49.9441549910849,122.605949735523)) ;
#33098 = CARTESIAN_POINT('Ctrl Pts',(-20.4283285548429,49.764165910722,122.767114266815)) ;
#33099 = CARTESIAN_POINT('Ctrl Pts',(-20.8039177883312,49.9541499895152,122.839164524174)) ;
#33100 = CARTESIAN_POINT('Ctrl Pts',(-20.5249823843959,49.7741609091523,122.953685109195)) ;
#33101 = CARTESIAN_POINT('Ctrl Pts',(-20.8821585762413,49.9641815382648,123.090919199762)) ;
#33102 = CARTESIAN_POINT('Ctrl Pts',(-20.5875768107398,49.7841924579019,123.155088321944)) ;
#33103 = CARTESIAN_POINT('Ctrl Pts',(-20.9152659613685,49.9740469165703,123.348034537658)) ;
#33104 = CARTESIAN_POINT('Ctrl Pts',(-20.6140645490356,49.7940578362074,123.3607797692)) ;
#33105 = CARTESIAN_POINT('Ctrl Pts',(-20.9038469302478,49.9840087640306,123.609580354995)) ;
#33106 = CARTESIAN_POINT('Ctrl Pts',(-20.6049313502839,49.8040196836677,123.57001630993)) ;
#33107 = CARTESIAN_POINT('Ctrl Pts',(-20.8463577366402,49.9940437048448,123.8669305923)) ;
#33108 = CARTESIAN_POINT('Ctrl Pts',(-20.5589419045982,49.814054624482,123.77589695398)) ;
#33109 = CARTESIAN_POINT('Ctrl Pts',(-20.7469555508652,50.003928665862,124.106966043971)) ;
#33110 = CARTESIAN_POINT('Ctrl Pts',(-20.4794221918956,49.8239395854991,123.967925670353)) ;
#33111 = CARTESIAN_POINT('Ctrl Pts',(-20.6048292012254,50.0139942747808,124.330001338928)) ;
#33112 = CARTESIAN_POINT('Ctrl Pts',(-20.3657227455692,49.8340051944179,124.146355087729)) ;
#33113 = CARTESIAN_POINT('Ctrl Pts',(-20.4302906277304,50.0238334498225,124.520821628096)) ;
#33114 = CARTESIAN_POINT('Ctrl Pts',(-20.2260937730439,49.8438443694597,124.299012279554)) ;
#33115 = CARTESIAN_POINT('Ctrl Pts',(-20.2208961768224,50.0338960053224,124.682260919657)) ;
#33116 = CARTESIAN_POINT('Ctrl Pts',(-20.0585794010133,49.8539069249596,124.42816542681)) ;
#33117 = CARTESIAN_POINT('Ctrl Pts',(-19.990330202873,50.0437931800154,124.802645968509)) ;
#33118 = CARTESIAN_POINT('Ctrl Pts',(-19.8741279016726,49.8638040996525,124.524475111746)) ;
#33119 = CARTESIAN_POINT('Ctrl Pts',(-19.7418079589796,50.0537238949387,124.882264366511)) ;
#33120 = CARTESIAN_POINT('Ctrl Pts',(-19.6753109887391,49.8737348145758,124.588171796186)) ;
#33121 = CARTESIAN_POINT('Ctrl Pts',(-19.4802461248259,50.0637679230163,124.91762289268)) ;
#33122 = CARTESIAN_POINT('Ctrl Pts',(-19.4660617807019,49.8837788426534,124.616460713011)) ;
#33123 = CARTESIAN_POINT('Ctrl Pts',(-19.2206304688887,50.0736541248696,124.907397165842)) ;
#33124 = CARTESIAN_POINT('Ctrl Pts',(-19.2583695113846,49.8936650445067,124.608282273323)) ;
#33125 = CARTESIAN_POINT('Ctrl Pts',(-18.9639476699514,50.0836472913365,124.852050273482)) ;
#33126 = CARTESIAN_POINT('Ctrl Pts',(-19.0530228963227,49.9036582109736,124.564006892753)) ;
#33127 = CARTESIAN_POINT('Ctrl Pts',(-18.7219951492464,50.0935867623236,124.753556604735)) ;
#33128 = CARTESIAN_POINT('Ctrl Pts',(-18.8594602370748,49.9135976819608,124.485214036914)) ;
#33129 = CARTESIAN_POINT('Ctrl Pts',(-18.4991286839628,50.1036032766778,124.613546547454)) ;
#33130 = CARTESIAN_POINT('Ctrl Pts',(-18.6811659438584,49.9236141963149,124.37320785353)) ;
#33131 = CARTESIAN_POINT('Ctrl Pts',(-18.305447857855,50.1135333031546,124.438612238836)) ;
#33132 = CARTESIAN_POINT('Ctrl Pts',(-18.5262199636435,49.9335442227918,124.233262162402)) ;
#33133 = CARTESIAN_POINT('Ctrl Pts',(-18.1432330982203,50.1235858386641,124.23014085339)) ;
#33134 = CARTESIAN_POINT('Ctrl Pts',(-18.396446423529,49.9435967583012,124.066486379902)) ;
#33135 = CARTESIAN_POINT('Ctrl Pts',(-18.0220679537995,50.1334322418838,124.001499451881)) ;
#33136 = CARTESIAN_POINT('Ctrl Pts',(-18.2995125219658,49.9534431615209,123.883574567668)) ;
#33137 = CARTESIAN_POINT('Ctrl Pts',(-17.9407108291128,50.1433942847378,123.752685556883)) ;
#33138 = CARTESIAN_POINT('Ctrl Pts',(-18.2344247243619,49.963405204375,123.684524241367)) ;
#33139 = CARTESIAN_POINT('Ctrl Pts',(-17.903879790198,50.1534228355285,123.491714650898)) ;
#33140 = CARTESIAN_POINT('Ctrl Pts',(-18.2049577020538,49.9734337551656,123.475747861428)) ;
#33141 = CARTESIAN_POINT('Ctrl Pts',(-17.9127260347505,50.1633331612461,123.23144379837)) ;
#33142 = CARTESIAN_POINT('Ctrl Pts',(-18.212032467387,49.9833440808833,123.267531271564)) ;
#33143 = CARTESIAN_POINT('Ctrl Pts',(-17.9660995838745,50.1732680730757,122.975870378448)) ;
#33144 = CARTESIAN_POINT('Ctrl Pts',(-18.2547290835788,49.9932789927128,123.063072178671)) ;
#33145 = CARTESIAN_POINT('Ctrl Pts',(-18.0642927488552,50.1833090798438,122.730962183356)) ;
#33146 = CARTESIAN_POINT('Ctrl Pts',(-18.3332815219319,50.0033199994809,122.867144823383)) ;
#33147 = CARTESIAN_POINT('Ctrl Pts',(-18.201255664043,50.193196712676,122.510138724716)) ;
#33148 = CARTESIAN_POINT('Ctrl Pts',(-18.4428498771025,50.0132076323131,122.690484981077)) ;
#33149 = CARTESIAN_POINT('Ctrl Pts',(-18.3759163267486,50.203187143774,122.314146410369)) ;
#33150 = CARTESIAN_POINT('Ctrl Pts',(-18.5825766919906,50.0231980634112,122.533689671197)) ;
#33151 = CARTESIAN_POINT('Ctrl Pts',(-18.5813368510253,50.2131425803313,122.152125343484)) ;
#33152 = CARTESIAN_POINT('Ctrl Pts',(-18.7469116404268,50.0331534999684,122.404071093068)) ;
#33153 = CARTESIAN_POINT('Ctrl Pts',(-18.8104932141694,50.2230535284306,122.028377092564)) ;
#33154 = CARTESIAN_POINT('Ctrl Pts',(-18.9302356832612,50.0430644480677,122.305070539431)) ;
#33155 = CARTESIAN_POINT('Ctrl Pts',(-19.0601191774314,50.2330656045283,121.945157820195)) ;
#33156 = CARTESIAN_POINT('Ctrl Pts',(-19.1299354530242,50.0530765241654,122.238492965492)) ;
#33157 = CARTESIAN_POINT('Ctrl Pts',(-19.3208286510922,50.2430929266033,121.907019503274)) ;
#33158 = CARTESIAN_POINT('Ctrl Pts',(-19.3385035281413,50.0631038462404,122.207980229758)) ;
#33159 = CARTESIAN_POINT('Ctrl Pts',(-19.5798646279409,50.2529517015574,121.913948569486)) ;
#33160 = CARTESIAN_POINT('Ctrl Pts',(-19.5457290400626,50.0729626211945,122.213520711451)) ;
#33161 = CARTESIAN_POINT('Ctrl Pts',(-19.9254133373517,50.2663778943698,121.984759551957)) ;
#33162 = CARTESIAN_POINT('Ctrl Pts',(-19.8221850711281,50.086388814007,122.270169142813)) ;
#33163 = CARTESIAN_POINT('Ctrl Pts',(-20.2369013110527,50.2794619101513,122.13968280904)) ;
#33164 = CARTESIAN_POINT('Ctrl Pts',(-20.0713939474092,50.0994728297884,122.394125151919)) ;
#33165 = CARTESIAN_POINT('Ctrl Pts',(-20.5024950621529,50.2929353589065,122.373723117195)) ;
#33166 = CARTESIAN_POINT('Ctrl Pts',(-20.2838339357162,50.1129462785436,122.581328603426)) ;
#33167 = CARTESIAN_POINT('Ctrl Pts',(-20.6634968410946,50.3027683167123,122.575877232274)) ;
#33168 = CARTESIAN_POINT('Ctrl Pts',(-20.4126446009124,50.1227792363495,122.743055923512)) ;
#33169 = CARTESIAN_POINT('Ctrl Pts',(-20.7895391335986,50.312731590163,122.805346777483)) ;
#33170 = CARTESIAN_POINT('Ctrl Pts',(-20.5134783878091,50.1327425098001,122.926629108663)) ;
#33171 = CARTESIAN_POINT('Ctrl Pts',(-20.8739118055342,50.322768663981,123.05524832364)) ;
#33172 = CARTESIAN_POINT('Ctrl Pts',(-20.5809791128739,50.1427795836181,123.126549935224)) ;
#33173 = CARTESIAN_POINT('Ctrl Pts',(-20.9134611751376,50.3326436669926,123.311752830501)) ;
#33174 = CARTESIAN_POINT('Ctrl Pts',(-20.6126206731099,50.1526545866297,123.331753172435)) ;
#33175 = CARTESIAN_POINT('Ctrl Pts',(-20.9077542261225,50.3427113466188,123.576222416539)) ;
#33176 = CARTESIAN_POINT('Ctrl Pts',(-20.6080572696327,50.1627222662559,123.543329200487)) ;
#33177 = CARTESIAN_POINT('Ctrl Pts',(-20.857508009601,50.3525521968365,123.829932935511)) ;
#33178 = CARTESIAN_POINT('Ctrl Pts',(-20.5678626302659,50.1725631164736,123.746296581769)) ;
#33179 = CARTESIAN_POINT('Ctrl Pts',(-20.7314548291478,50.3658883953125,124.156910684336)) ;
#33180 = CARTESIAN_POINT('Ctrl Pts',(-20.4670213805127,50.1858993149496,124.00788851066)) ;
#33181 = CARTESIAN_POINT('Ctrl Pts',(-20.524653068368,50.3791059191269,124.440925618285)) ;
#33182 = CARTESIAN_POINT('Ctrl Pts',(-20.3015547453208,50.199116838764,124.235123745287)) ;
#33183 = CARTESIAN_POINT('Ctrl Pts',(-20.252395006723,50.3924408456182,124.66151880778)) ;
#33184 = CARTESIAN_POINT('Ctrl Pts',(-20.0837839668042,50.2124517652553,124.411566257854)) ;
#33185 = CARTESIAN_POINT('Ctrl Pts',(-20.0229851842833,50.4024239462128,124.788869046757)) ;
#33186 = CARTESIAN_POINT('Ctrl Pts',(-19.9002502106648,50.2224348658499,124.513455083149)) ;
#33187 = CARTESIAN_POINT('Ctrl Pts',(-19.7733522297728,50.4124687221124,124.874590001612)) ;
#33188 = CARTESIAN_POINT('Ctrl Pts',(-19.7005468471622,50.2324796417495,124.582032094973)) ;
#33189 = CARTESIAN_POINT('Ctrl Pts',(-19.5185568926512,50.4222866452983,124.915250650633)) ;
#33190 = CARTESIAN_POINT('Ctrl Pts',(-19.4967086995116,50.2422975649354,124.614562632195)) ;
#33191 = CARTESIAN_POINT('Ctrl Pts',(-19.2545052235582,50.4323359592536,124.911493375565)) ;
#33192 = CARTESIAN_POINT('Ctrl Pts',(-19.2854717860523,50.2523468788908,124.611560855551)) ;
#33193 = CARTESIAN_POINT('Ctrl Pts',(-18.9112636456039,50.4456396998762,124.845209773811)) ;
#33194 = CARTESIAN_POINT('Ctrl Pts',(-19.0108574254215,50.2656506195133,124.558525723013)) ;
#33195 = CARTESIAN_POINT('Ctrl Pts',(-18.5163636183236,50.4621298953529,124.654888417403)) ;
#33196 = CARTESIAN_POINT('Ctrl Pts',(-18.6949672451094,50.28214081499,124.406294866323)) ;
#33197 = CARTESIAN_POINT('Ctrl Pts',(-18.2061311342259,50.4788490602775,124.336917792434)) ;
#33198 = CARTESIAN_POINT('Ctrl Pts',(-18.4467378517919,50.2988599799146,124.151872297986)) ;
#33199 = CARTESIAN_POINT('Ctrl Pts',(-18.0368827272804,50.4920100539476,124.035219084609)) ;
#33200 = CARTESIAN_POINT('Ctrl Pts',(-18.311368220634,50.3120209735847,123.910554390484)) ;
#33201 = CARTESIAN_POINT('Ctrl Pts',(-17.9492027072533,50.5020062760529,123.787616040863)) ;
#33202 = CARTESIAN_POINT('Ctrl Pts',(-18.2412163833771,50.32201719569,123.712463854449)) ;
#33203 = CARTESIAN_POINT('Ctrl Pts',(-17.9063100733637,50.5120301155866,123.527712476807)) ;
#33204 = CARTESIAN_POINT('Ctrl Pts',(-18.2069016114084,50.3320410352238,123.504545668271)) ;
#33205 = CARTESIAN_POINT('Ctrl Pts',(-17.9093431973629,50.5252234375799,123.180991999699)) ;
#33206 = CARTESIAN_POINT('Ctrl Pts',(-18.2093282776367,50.345234357217,123.227157652856)) ;
#33207 = CARTESIAN_POINT('Ctrl Pts',(-18.027118283777,50.5418826093572,122.754212984447)) ;
#33208 = CARTESIAN_POINT('Ctrl Pts',(-18.3035426189576,50.3618935289943,122.885745424795)) ;
#33209 = CARTESIAN_POINT('Ctrl Pts',(-18.333937561739,50.5617927848429,122.323039035125)) ;
#33210 = CARTESIAN_POINT('Ctrl Pts',(-18.5489966706976,50.38180370448,122.540800132755)) ;
#33211 = CARTESIAN_POINT('Ctrl Pts',(-18.7684393921744,50.5816827726873,122.021820822919)) ;
#33212 = CARTESIAN_POINT('Ctrl Pts',(-18.8965968570353,50.4016936923244,122.299823770032)) ;
#33213 = CARTESIAN_POINT('Ctrl Pts',(-19.2825937715403,50.6016882207021,121.886677539595)) ;
#33214 = CARTESIAN_POINT('Ctrl Pts',(-19.307919625913,50.4216991403392,122.191706067227)) ;
#33215 = CARTESIAN_POINT('Ctrl Pts',(-19.8078113963263,50.6215246147294,121.934169205366)) ;
#33216 = CARTESIAN_POINT('Ctrl Pts',(-19.7280952319297,50.4415355343665,122.229696987763)) ;
#33217 = CARTESIAN_POINT('Ctrl Pts',(-20.2892513212485,50.6415324086261,122.159662815759)) ;
#33218 = CARTESIAN_POINT('Ctrl Pts',(-20.1132481557937,50.4615433282632,122.410089630547)) ;
#33219 = CARTESIAN_POINT('Ctrl Pts',(-20.6617398847741,50.66135904492,122.532541564671)) ;
#33220 = CARTESIAN_POINT('Ctrl Pts',(-20.4112416638867,50.4813699645572,122.708392168977)) ;
#33221 = CARTESIAN_POINT('Ctrl Pts',(-20.8871620269531,50.6813379878739,123.013304098428)) ;
#33222 = CARTESIAN_POINT('Ctrl Pts',(-20.5915810553221,50.501348907511,123.093001677507)) ;
#33223 = CARTESIAN_POINT('Ctrl Pts',(-20.9339369378857,50.701269789743,123.540918150504)) ;
#33224 = CARTESIAN_POINT('Ctrl Pts',(-20.6290028531258,50.5212807093801,123.515093416669)) ;
#33225 = CARTESIAN_POINT('Ctrl Pts',(-20.8002489892957,50.7210940902405,124.050742162796)) ;
#33226 = CARTESIAN_POINT('Ctrl Pts',(-20.5220534268662,50.5411050098776,123.922954725086)) ;
#33227 = CARTESIAN_POINT('Ctrl Pts',(-20.4959470937685,50.7411900915803,124.489434446394)) ;
#33228 = CARTESIAN_POINT('Ctrl Pts',(-20.2786119963971,50.5612010112175,124.273908331322)) ;
#33229 = CARTESIAN_POINT('Ctrl Pts',(-20.0674250455001,50.7609485076843,124.793529199864)) ;
#33230 = CARTESIAN_POINT('Ctrl Pts',(-19.9357982255067,50.5809594273214,124.517186790158)) ;
#33231 = CARTESIAN_POINT('Ctrl Pts',(-19.5529196248031,50.7810422005684,124.935512899744)) ;
#33232 = CARTESIAN_POINT('Ctrl Pts',(-19.524171586782,50.6010531202055,124.630773511285)) ;
#33233 = CARTESIAN_POINT('Ctrl Pts',(-19.2053312341041,50.7941531664751,124.907880339345)) ;
#33234 = CARTESIAN_POINT('Ctrl Pts',(-19.2461441930599,50.6141640861122,124.608669210494)) ;
#33235 = CARTESIAN_POINT('Ctrl Pts',(-19.035117438896,50.8008665412629,124.864312062334)) ;
#33236 = CARTESIAN_POINT('Ctrl Pts',(-19.1099467513572,50.6208774609001,124.573813086965)) ;
#33237 = CARTESIAN_POINT('',(-20.7227191491167,12.1498929727495,122.68753928809)) ;
#33238 = CARTESIAN_POINT('',(-20.4664913274138,12.,122.732834476394)) ;
#33239 = CARTESIAN_POINT('Ctrl Pts',(-20.7227191491167,12.1498929727495,122.68753928809)) ;
#33240 = CARTESIAN_POINT('Ctrl Pts',(-20.7010586156241,12.1380608205066,122.687740528906)) ;
#33241 = CARTESIAN_POINT('Ctrl Pts',(-20.6788750303579,12.1257316308462,122.688962697014)) ;
#33242 = CARTESIAN_POINT('Ctrl Pts',(-20.6565183911447,12.1130842758946,122.691175310439)) ;
#33243 = CARTESIAN_POINT('Ctrl Pts',(-20.6339362615787,12.1003093589914,122.693410240411)) ;
#33244 = CARTESIAN_POINT('Ctrl Pts',(-20.6111778962031,12.0872098262344,122.696655512741)) ;
#33245 = CARTESIAN_POINT('Ctrl Pts',(-20.5885827815958,12.0739700078726,122.700830016118)) ;
#33246 = CARTESIAN_POINT('Ctrl Pts',(-20.5650612529886,12.0601873485781,122.705175676775)) ;
#33247 = CARTESIAN_POINT('Ctrl Pts',(-20.541716986944,12.046252664071,122.710528106775)) ;
#33248 = CARTESIAN_POINT('Ctrl Pts',(-20.5189045693268,12.0323738925062,122.716744901924)) ;
#33249 = CARTESIAN_POINT('Ctrl Pts',(-20.5010561838023,12.021515172065,122.721608908816)) ;
#33250 = CARTESIAN_POINT('Ctrl Pts',(-20.4835327586187,12.0106906783193,122.72700084837)) ;
#33251 = CARTESIAN_POINT('Ctrl Pts',(-20.4664913276595,11.9999999999988,122.732834476261)) ;
#33252 = CARTESIAN_POINT('',(-17.9096492507572,12.,123.379771111334)) ;
#33253 = CARTESIAN_POINT('Ctrl Pts',(-20.4664913276595,11.9999999999988,122.732834476261)) ;
#33254 = CARTESIAN_POINT('Ctrl Pts',(-20.4509543572035,11.9999999999989,122.704060366312)) ;
#33255 = CARTESIAN_POINT('Ctrl Pts',(-20.4342538607019,12.,122.675825907815)) ;
#33256 = CARTESIAN_POINT('Ctrl Pts',(-20.4164330413058,12.,122.648224859268)) ;
#33257 = CARTESIAN_POINT('Ctrl Pts',(-20.3766729892274,12.,122.586644125901)) ;
#33258 = CARTESIAN_POINT('Ctrl Pts',(-20.3313233976647,12.,122.528197448024)) ;
#33259 = CARTESIAN_POINT('Ctrl Pts',(-20.2807728582503,12.,122.473687896805)) ;
#33260 = CARTESIAN_POINT('Ctrl Pts',(-20.2341054743954,12.,122.423365621712)) ;
#33261 = CARTESIAN_POINT('Ctrl Pts',(-20.1829884635469,11.9999999994,122.376380466302)) ;
#33262 = CARTESIAN_POINT('Ctrl Pts',(-20.1278748005212,11.9999999999304,122.333498241347)) ;
#33263 = CARTESIAN_POINT('Ctrl Pts',(-20.1234434404153,11.9999999999731,122.330050338042)) ;
#33264 = CARTESIAN_POINT('Ctrl Pts',(-20.1189862610655,12.,122.32662898048)) ;
#33265 = CARTESIAN_POINT('Ctrl Pts',(-20.1145035075594,12.,122.323234577862)) ;
#33266 = CARTESIAN_POINT('Ctrl Pts',(-20.0669031140567,12.,122.287190905126)) ;
#33267 = CARTESIAN_POINT('Ctrl Pts',(-20.0164366742931,12.0000000052168,122.254200732626)) ;
#33268 = CARTESIAN_POINT('Ctrl Pts',(-19.9637911702411,12.0000000018168,122.224745622377)) ;
#33269 = CARTESIAN_POINT('Ctrl Pts',(-19.9499756315567,12.0000000009246,122.217015841413)) ;
#33270 = CARTESIAN_POINT('Ctrl Pts',(-19.9360102767224,12.,122.209529633199)) ;
#33271 = CARTESIAN_POINT('Ctrl Pts',(-19.9219080603125,12.,122.202295954535)) ;
#33272 = CARTESIAN_POINT('Ctrl Pts',(-19.8542244544787,12.,122.167577904465)) ;
#33273 = CARTESIAN_POINT('Ctrl Pts',(-19.7833590089754,12.,122.138660939201)) ;
#33274 = CARTESIAN_POINT('Ctrl Pts',(-19.7093663209473,12.,122.115884324254)) ;
#33275 = CARTESIAN_POINT('Ctrl Pts',(-19.6563392668767,12.,122.099561403375)) ;
#33276 = CARTESIAN_POINT('Ctrl Pts',(-19.6017001635138,12.0000000149114,122.086390904151)) ;
#33277 = CARTESIAN_POINT('Ctrl Pts',(-19.546212003709,12.0000000073334,122.076657410532)) ;
#33278 = CARTESIAN_POINT('Ctrl Pts',(-19.5244859763294,12.0000000043663,122.072846324535)) ;
#33279 = CARTESIAN_POINT('Ctrl Pts',(-19.5026303315761,12.,122.069562280034)) ;
#33280 = CARTESIAN_POINT('Ctrl Pts',(-19.4806930068947,12.,122.066822797438)) ;
#33281 = CARTESIAN_POINT('Ctrl Pts',(-19.402879099977,12.,122.057105575911)) ;
#33282 = CARTESIAN_POINT('Ctrl Pts',(-19.3241008842937,12.,122.054249810868)) ;
#33283 = CARTESIAN_POINT('Ctrl Pts',(-19.2452460130912,12.,122.058247839665)) ;
#33284 = CARTESIAN_POINT('Ctrl Pts',(-19.1665569481981,12.,122.062237461899)) ;
#33285 = CARTESIAN_POINT('Ctrl Pts',(-19.0877130844164,12.,122.073053895301)) ;
#33286 = CARTESIAN_POINT('Ctrl Pts',(-19.0093824990468,12.,122.090995385507)) ;
#33287 = CARTESIAN_POINT('Ctrl Pts',(-18.9507187051536,12.,122.104432229858)) ;
#33288 = CARTESIAN_POINT('Ctrl Pts',(-18.8923478250649,12.0000000102563,122.121865317184)) ;
#33289 = CARTESIAN_POINT('Ctrl Pts',(-18.8351097436429,12.0000000043775,122.143167364287)) ;
#33290 = CARTESIAN_POINT('Ctrl Pts',(-18.8161414792467,12.0000000024293,122.150226700512)) ;
#33291 = CARTESIAN_POINT('Ctrl Pts',(-18.7972980263926,12.,122.157710808519)) ;
#33292 = CARTESIAN_POINT('Ctrl Pts',(-18.7786111581444,12.,122.165614672269)) ;
#33293 = CARTESIAN_POINT('Ctrl Pts',(-18.7118018157948,12.,122.193872587514)) ;
#33294 = CARTESIAN_POINT('Ctrl Pts',(-18.6470553315846,12.0000000003845,122.227471732854)) ;
#33295 = CARTESIAN_POINT('Ctrl Pts',(-18.5852217646428,12.0000000000663,122.265859882284)) ;
#33296 = CARTESIAN_POINT('Ctrl Pts',(-18.5776852993161,12.0000000000275,122.270538748011)) ;
#33297 = CARTESIAN_POINT('Ctrl Pts',(-18.5701921517252,12.,122.275288711735)) ;
#33298 = CARTESIAN_POINT('Ctrl Pts',(-18.5627438981913,12.,122.280108735924)) ;
#33299 = CARTESIAN_POINT('Ctrl Pts',(-18.4980309831752,12.,122.32198671635)) ;
#33300 = CARTESIAN_POINT('Ctrl Pts',(-18.4366368756665,11.9999999928402,122.369197267935)) ;
#33301 = CARTESIAN_POINT('Ctrl Pts',(-18.3787222199717,11.9999999993994,122.422020424971)) ;
#33302 = CARTESIAN_POINT('Ctrl Pts',(-18.3753891921239,11.9999999997769,122.425060433606)) ;
#33303 = CARTESIAN_POINT('Ctrl Pts',(-18.3720676802587,12.,122.428119043496)) ;
#33304 = CARTESIAN_POINT('Ctrl Pts',(-18.3687577121273,12.,122.431196312548)) ;
#33305 = CARTESIAN_POINT('Ctrl Pts',(-18.3264247986708,12.,122.470553115778)) ;
#33306 = CARTESIAN_POINT('Ctrl Pts',(-18.2859739515088,12.0000000189751,122.512967788025)) ;
#33307 = CARTESIAN_POINT('Ctrl Pts',(-18.2480707810569,12.0000000101354,122.557909386313)) ;
#33308 = CARTESIAN_POINT('Ctrl Pts',(-18.2316777870941,12.0000000063122,122.577346476684)) ;
#33309 = CARTESIAN_POINT('Ctrl Pts',(-18.2157618098082,12.,122.59725577119)) ;
#33310 = CARTESIAN_POINT('Ctrl Pts',(-18.2003787759881,12.,122.617592113997)) ;
#33311 = CARTESIAN_POINT('Ctrl Pts',(-18.1495353272504,12.,122.684807061005)) ;
#33312 = CARTESIAN_POINT('Ctrl Pts',(-18.1045662126026,12.,122.756621216588)) ;
#33313 = CARTESIAN_POINT('Ctrl Pts',(-18.0659377442576,12.,122.832173109989)) ;
#33314 = CARTESIAN_POINT('Ctrl Pts',(-18.027387955545,12.,122.907571117009)) ;
#33315 = CARTESIAN_POINT('Ctrl Pts',(-17.995114699564,12.,122.986761016303)) ;
#33316 = CARTESIAN_POINT('Ctrl Pts',(-17.9698216577103,12.,123.069272641495)) ;
#33317 = CARTESIAN_POINT('Ctrl Pts',(-17.9521228336151,12.,123.127010210132)) ;
#33318 = CARTESIAN_POINT('Ctrl Pts',(-17.9378542916193,12.0000000080963,123.186339136655)) ;
#33319 = CARTESIAN_POINT('Ctrl Pts',(-17.9272125111136,12.0000000042853,123.246300595191)) ;
#33320 = CARTESIAN_POINT('Ctrl Pts',(-17.9226767295839,12.0000000026609,123.271857603811)) ;
#33321 = CARTESIAN_POINT('Ctrl Pts',(-17.9187998924811,12.,123.297528881935)) ;
#33322 = CARTESIAN_POINT('Ctrl Pts',(-17.915597481249,12.,123.323237316211)) ;
#33323 = CARTESIAN_POINT('Ctrl Pts',(-17.9132521442838,12.,123.342065298271)) ;
#33324 = CARTESIAN_POINT('Ctrl Pts',(-17.9112692183144,12.,123.360907769294)) ;
#33325 = CARTESIAN_POINT('Ctrl Pts',(-17.9096492507572,12.,123.379771111334)) ;
#33326 = CARTESIAN_POINT('Ctrl Pts',(-17.9096492507572,12.,123.379771111334)) ;
#33327 = CARTESIAN_POINT('Ctrl Pts',(-17.9100667346536,12.0007217907825,123.36087892436)) ;
#33328 = CARTESIAN_POINT('Ctrl Pts',(-17.9144060035305,12.0047464667125,123.255581124476)) ;
#33329 = CARTESIAN_POINT('Ctrl Pts',(-17.9427499485555,12.0121810504321,123.062292370625)) ;
#33330 = CARTESIAN_POINT('Ctrl Pts',(-18.0251977237691,12.0221110972068,122.814691316201)) ;
#33331 = CARTESIAN_POINT('Ctrl Pts',(-18.1490393731302,12.0320625395439,122.584356522223)) ;
#33332 = CARTESIAN_POINT('Ctrl Pts',(-18.3128249788135,12.0421093367232,122.377284739554)) ;
#33333 = CARTESIAN_POINT('Ctrl Pts',(-18.5060148098008,12.0519572774033,122.205087588693)) ;
#33334 = CARTESIAN_POINT('Ctrl Pts',(-18.7282729224672,12.0619189087459,122.066794754727)) ;
#33335 = CARTESIAN_POINT('Ctrl Pts',(-18.9729503385559,12.0719475681218,121.968835081685)) ;
#33336 = CARTESIAN_POINT('Ctrl Pts',(-19.227831787757,12.08185787101,121.915407496624)) ;
#33337 = CARTESIAN_POINT('Ctrl Pts',(-19.4887612039821,12.0917927655722,121.906342273827)) ;
#33338 = CARTESIAN_POINT('Ctrl Pts',(-19.7500144690061,12.1018338642391,121.943349818059)) ;
#33339 = CARTESIAN_POINT('Ctrl Pts',(-19.9971083719985,12.1117211467435,122.023739879768)) ;
#33340 = CARTESIAN_POINT('Ctrl Pts',(-20.2290950029525,12.121712887254,122.146694306298)) ;
#33341 = CARTESIAN_POINT('Ctrl Pts',(-20.4353231818005,12.1316634364894,122.307485013012)) ;
#33342 = CARTESIAN_POINT('Ctrl Pts',(-20.6005848561123,12.1410363173938,122.490103477729)) ;
#33343 = CARTESIAN_POINT('Ctrl Pts',(-20.6877151581443,12.1471236046148,122.624050429204)) ;
#33344 = CARTESIAN_POINT('Ctrl Pts',(-20.7227191491167,12.1498929727495,122.68753928809)) ;
#33345 = CARTESIAN_POINT('Origin',(-20.3808735729049,12.,126.250122109236)) ;
#33346 = CARTESIAN_POINT('',(-20.4601832664426,12.,122.734993854115)) ;
#33347 = CARTESIAN_POINT('',(-20.4664913274138,12.,122.732834476394)) ;
#33348 = CARTESIAN_POINT('',(-18.1640505668151,12.,123.521006833268)) ;
#33349 = CARTESIAN_POINT('Origin',(-19.4092722359532,12.,123.411814366564)) ;
#33350 = CARTESIAN_POINT('',(-17.9353686287936,11.9999999997025,123.599289317459)) ;
#33351 = CARTESIAN_POINT('',(-18.1640505668151,12.,123.521006833268)) ;
#33352 = CARTESIAN_POINT('Ctrl Pts',(-17.9096492507572,12.,123.379771111334)) ;
#33353 = CARTESIAN_POINT('Ctrl Pts',(-17.9111794973639,12.,123.416636495257)) ;
#33354 = CARTESIAN_POINT('Ctrl Pts',(-17.9140858729415,12.0000000000049,123.453367630287)) ;
#33355 = CARTESIAN_POINT('Ctrl Pts',(-17.9226794425075,12.0000000000049,123.526662996257)) ;
#33356 = CARTESIAN_POINT('Ctrl Pts',(-17.9283556505042,12.,123.563110613297)) ;
#33357 = CARTESIAN_POINT('Ctrl Pts',(-17.9353686298462,12.,123.599289317255)) ;
#33358 = CARTESIAN_POINT('Origin',(-19.4092722359532,16.5113612779716,123.411814366564)) ;
#33359 = CARTESIAN_POINT('Ctrl Pts',(-20.5919043739536,12.7298332115048,123.006991903941)) ;
#33360 = CARTESIAN_POINT('Ctrl Pts',(-20.5874582960172,12.7292023169138,122.994003648584)) ;
#33361 = CARTESIAN_POINT('Ctrl Pts',(-20.5827987528111,12.7285719416166,122.981089421798)) ;
#33362 = CARTESIAN_POINT('Ctrl Pts',(-20.574287862775,12.7274715784339,122.958665623562)) ;
#33363 = CARTESIAN_POINT('Ctrl Pts',(-20.5705305117346,12.7270013881013,122.94912179947)) ;
#33364 = CARTESIAN_POINT('Ctrl Pts',(-20.5626714838065,12.7260484071683,122.929858515579)) ;
#33365 = CARTESIAN_POINT('Ctrl Pts',(-20.5585633641852,12.7255656767293,122.920142554556)) ;
#33366 = CARTESIAN_POINT('Ctrl Pts',(-20.5487412627525,12.7244460890821,122.897708635331)) ;
#33367 = CARTESIAN_POINT('Ctrl Pts',(-20.5429364852264,12.7238096798513,122.885031927171)) ;
#33368 = CARTESIAN_POINT('Ctrl Pts',(-20.5226828266888,12.7216707323095,122.842687232925)) ;
#33369 = CARTESIAN_POINT('Ctrl Pts',(-20.5072714673937,12.7201741098457,122.813494564159)) ;
#33370 = CARTESIAN_POINT('Ctrl Pts',(-20.4765507937487,12.7174143135874,122.760496400936)) ;
#33371 = CARTESIAN_POINT('Ctrl Pts',(-20.4615536051481,12.716148146437,122.736534761797)) ;
#33372 = CARTESIAN_POINT('Ctrl Pts',(-20.4278471509029,12.7134373221124,122.686533887782)) ;
#33373 = CARTESIAN_POINT('Ctrl Pts',(-20.4089225377984,12.7119923140302,122.660664676273)) ;
#33374 = CARTESIAN_POINT('Ctrl Pts',(-20.3859313068839,12.7103070073287,122.631646513355)) ;
#33375 = CARTESIAN_POINT('Ctrl Pts',(-20.382814149153,12.7100799261839,122.627760182863)) ;
#33376 = CARTESIAN_POINT('Ctrl Pts',(-20.3774854041029,12.7096940665411,122.621197319607)) ;
#33377 = CARTESIAN_POINT('Ctrl Pts',(-20.3752857428806,12.7095354497977,122.618511172157)) ;
#33378 = CARTESIAN_POINT('Ctrl Pts',(-20.3711723084536,12.709240043704,122.613530471045)) ;
#33379 = CARTESIAN_POINT('Ctrl Pts',(-20.3692614428512,12.7091032950564,122.611233546223)) ;
#33380 = CARTESIAN_POINT('Ctrl Pts',(-20.3653693291752,12.708825721361,122.606589066027)) ;
#33381 = CARTESIAN_POINT('Ctrl Pts',(-20.3633876261552,12.7086848907517,122.604241918789)) ;
#33382 = CARTESIAN_POINT('Ctrl Pts',(-20.3587473404578,12.708356274068,122.598786843592)) ;
#33383 = CARTESIAN_POINT('Ctrl Pts',(-20.3560821193224,12.7081683963687,122.595684614761)) ;
#33384 = CARTESIAN_POINT('Ctrl Pts',(-20.3478130767288,12.7075881318747,122.586154747251)) ;
#33385 = CARTESIAN_POINT('Ctrl Pts',(-20.3421586935067,12.7071950422528,122.579771355263)) ;
#33386 = CARTESIAN_POINT('Ctrl Pts',(-20.3088992949423,12.7049038791851,122.542989150078)) ;
#33387 = CARTESIAN_POINT('Ctrl Pts',(-20.2798755959217,12.7029855180402,122.51390804049)) ;
#33388 = CARTESIAN_POINT('Ctrl Pts',(-20.2184469078676,12.6990993462048,122.458141237711)) ;
#33389 = CARTESIAN_POINT('Ctrl Pts',(-20.1860224438698,12.6971407738768,122.431551495952)) ;
#33390 = CARTESIAN_POINT('Ctrl Pts',(-20.1369800085691,12.6943095255758,122.395298026217)) ;
#33391 = CARTESIAN_POINT('Ctrl Pts',(-20.1213787048448,12.6934261763327,122.384308426099)) ;
#33392 = CARTESIAN_POINT('Ctrl Pts',(-20.0965715902114,12.6920468103064,122.367670698848)) ;
#33393 = CARTESIAN_POINT('Ctrl Pts',(-20.0875338440553,12.6915493493308,122.361777417857)) ;
#33394 = CARTESIAN_POINT('Ctrl Pts',(-20.0722271807047,12.6907149958544,122.352076421277)) ;
#33395 = CARTESIAN_POINT('Ctrl Pts',(-20.0659990140571,12.6903777307108,122.348205551803)) ;
#33396 = CARTESIAN_POINT('Ctrl Pts',(-20.0545623835731,12.6897623694749,122.341236323024)) ;
#33397 = CARTESIAN_POINT('Ctrl Pts',(-20.0493647604295,12.6894841745259,122.338120610274)) ;
#33398 = CARTESIAN_POINT('Ctrl Pts',(-20.0391592041141,12.688940740664,122.332103339086)) ;
#33399 = CARTESIAN_POINT('Ctrl Pts',(-20.0341533674478,12.6886754879462,122.32919852184)) ;
#33400 = CARTESIAN_POINT('Ctrl Pts',(-20.0226611470541,12.6880694385187,122.322636009766)) ;
#33401 = CARTESIAN_POINT('Ctrl Pts',(-20.0161618837293,12.687728792848,122.319001296964)) ;
#33402 = CARTESIAN_POINT('Ctrl Pts',(-19.9984421190923,12.6868055644523,122.309298351561)) ;
#33403 = CARTESIAN_POINT('Ctrl Pts',(-19.9871605541439,12.6862237144543,122.303343433842)) ;
#33404 = CARTESIAN_POINT('Ctrl Pts',(-19.9339037825458,12.6835033315254,122.276266173459)) ;
#33405 = CARTESIAN_POINT('Ctrl Pts',(-19.8908496740945,12.681379834111,122.257348579191)) ;
#33406 = CARTESIAN_POINT('Ctrl Pts',(-19.8128001830863,12.6776381537056,122.228182191831)) ;
#33407 = CARTESIAN_POINT('Ctrl Pts',(-19.7782297944157,12.6760162922282,122.216954437728)) ;
#33408 = CARTESIAN_POINT('Ctrl Pts',(-19.7189160196954,12.6732469844032,122.20051061311)) ;
#33409 = CARTESIAN_POINT('Ctrl Pts',(-19.6944145696779,12.6721070555401,122.194510018847)) ;
#33410 = CARTESIAN_POINT('Ctrl Pts',(-19.6641240256707,12.6706964537624,122.188056368476)) ;
#33411 = CARTESIAN_POINT('Ctrl Pts',(-19.6584912153566,12.6704340966092,122.18689682956)) ;
#33412 = CARTESIAN_POINT('Ctrl Pts',(-19.6499400281158,12.6700356924186,122.185197955526)) ;
#33413 = CARTESIAN_POINT('Ctrl Pts',(-19.6470273887578,12.669899970342,122.184630071821)) ;
#33414 = CARTESIAN_POINT('Ctrl Pts',(-19.6411154293813,12.6696244369637,122.183499241513)) ;
#33415 = CARTESIAN_POINT('Ctrl Pts',(-19.6381160149756,12.6694846198386,122.182936896065)) ;
#33416 = CARTESIAN_POINT('Ctrl Pts',(-19.6316505764505,12.6691831706065,122.181749214646)) ;
#33417 = CARTESIAN_POINT('Ctrl Pts',(-19.6281839097497,12.6690214986468,122.181127532615)) ;
#33418 = CARTESIAN_POINT('Ctrl Pts',(-19.6188584768404,12.6685864781895,122.179495839296)) ;
#33419 = CARTESIAN_POINT('Ctrl Pts',(-19.6129950704492,12.6683128313736,122.178512963329)) ;
#33420 = CARTESIAN_POINT('Ctrl Pts',(-19.5821839874874,12.6668741420245,122.173573856816)) ;
#33421 = CARTESIAN_POINT('Ctrl Pts',(-19.5571279908566,12.6657014134404,122.170332720993)) ;
#33422 = CARTESIAN_POINT('Ctrl Pts',(-19.4910593494478,12.6626047780172,122.163814926806)) ;
#33423 = CARTESIAN_POINT('Ctrl Pts',(-19.4499531256098,12.6606726915156,122.16179964462)) ;
#33424 = CARTESIAN_POINT('Ctrl Pts',(-19.3810909584357,12.6574663634508,122.161824427958)) ;
#33425 = CARTESIAN_POINT('Ctrl Pts',(-19.3533672570836,12.6561833626144,122.162757243192)) ;
#33426 = CARTESIAN_POINT('Ctrl Pts',(-19.3131826908954,12.6543268053868,122.165450006401)) ;
#33427 = CARTESIAN_POINT('Ctrl Pts',(-19.3006813626391,12.6537496800746,122.166476925026)) ;
#33428 = CARTESIAN_POINT('Ctrl Pts',(-19.2782653869539,12.6527147674379,122.168658387553)) ;
#33429 = CARTESIAN_POINT('Ctrl Pts',(-19.268345111649,12.6522567364059,122.169743865703)) ;
#33430 = CARTESIAN_POINT('Ctrl Pts',(-19.2470262054446,12.6512718612793,122.172335282709)) ;
#33431 = CARTESIAN_POINT('Ctrl Pts',(-19.2356331903504,12.6507451913567,122.173879935112)) ;
#33432 = CARTESIAN_POINT('Ctrl Pts',(-19.2018478313302,12.6491813744363,122.178936102775)) ;
#33433 = CARTESIAN_POINT('Ctrl Pts',(-19.1795278985088,12.6481455987097,122.1828997066)) ;
#33434 = CARTESIAN_POINT('Ctrl Pts',(-19.0840932163382,12.6436958619431,122.202538113423)) ;
#33435 = CARTESIAN_POINT('Ctrl Pts',(-19.0123577181082,12.6402984837699,122.224148841466)) ;
#33436 = CARTESIAN_POINT('Ctrl Pts',(-18.925032714619,12.6360191620718,122.25925787892)) ;
#33437 = CARTESIAN_POINT('Ctrl Pts',(-18.9072506943902,12.6351389733826,122.266891338895)) ;
#33438 = CARTESIAN_POINT('Ctrl Pts',(-18.8801150158276,12.6337789901851,122.279293896089)) ;
#33439 = CARTESIAN_POINT('Ctrl Pts',(-18.8706322051877,12.6333005085761,122.283773190043)) ;
#33440 = CARTESIAN_POINT('Ctrl Pts',(-18.8610038414272,12.632811123212,122.28847033258)) ;
#33441 = CARTESIAN_POINT('Ctrl Pts',(-18.860800803836,12.6328008017,122.288569451474)) ;
#33442 = CARTESIAN_POINT('Ctrl Pts',(-18.8604029314302,12.6327805724786,122.288763818432)) ;
#33443 = CARTESIAN_POINT('Ctrl Pts',(-18.860208094397,12.6327706647844,122.288859062215)) ;
#33444 = CARTESIAN_POINT('Ctrl Pts',(-18.8598261936814,12.6327512417364,122.289045873025)) ;
#33445 = CARTESIAN_POINT('Ctrl Pts',(-18.85963912813,12.6327417264042,122.289137436082)) ;
#33446 = CARTESIAN_POINT('Ctrl Pts',(-18.8592723663165,12.6327230678687,122.289317068785)) ;
#33447 = CARTESIAN_POINT('Ctrl Pts',(-18.8590926683012,12.6327139246828,122.289405134839)) ;
#33448 = CARTESIAN_POINT('Ctrl Pts',(-18.8587402609276,12.6326959913847,122.289577946927)) ;
#33449 = CARTESIAN_POINT('Ctrl Pts',(-18.8585675499598,12.6326872012879,122.28966268969)) ;
#33450 = CARTESIAN_POINT('Ctrl Pts',(-18.8582287580403,12.6326699562002,122.289829019171)) ;
#33451 = CARTESIAN_POINT('Ctrl Pts',(-18.8580626756292,12.6326615012237,122.289910602901)) ;
#33452 = CARTESIAN_POINT('Ctrl Pts',(-18.8577368028425,12.632644909431,122.290070769387)) ;
#33453 = CARTESIAN_POINT('Ctrl Pts',(-18.8575770111154,12.6326367726271,122.290149349424)) ;
#33454 = CARTESIAN_POINT('Ctrl Pts',(-18.8572634013213,12.6326208012057,122.290303655087)) ;
#33455 = CARTESIAN_POINT('Ctrl Pts',(-18.8571095819159,12.6326129665944,122.290379378276)) ;
#33456 = CARTESIAN_POINT('Ctrl Pts',(-18.8568076159666,12.6325975844553,122.290528109172)) ;
#33457 = CARTESIAN_POINT('Ctrl Pts',(-18.8566594684449,12.6325900369459,122.290601114529)) ;
#33458 = CARTESIAN_POINT('Ctrl Pts',(-18.8563685630119,12.63257521478,122.290744540968)) ;
#33459 = CARTESIAN_POINT('Ctrl Pts',(-18.8562258041211,12.6325679401361,122.29081495994)) ;
#33460 = CARTESIAN_POINT('Ctrl Pts',(-18.8559454087077,12.6325536502667,122.290953337762)) ;
#33461 = CARTESIAN_POINT('Ctrl Pts',(-18.8558077712247,12.6325466350494,122.291021294708)) ;
#33462 = CARTESIAN_POINT('Ctrl Pts',(-18.8555373663725,12.6325328513444,122.291154865994)) ;
#33463 = CARTESIAN_POINT('Ctrl Pts',(-18.8554045981134,12.6325260828639,122.291220478591)) ;
#33464 = CARTESIAN_POINT('Ctrl Pts',(-18.8551436933356,12.6325127806346,122.291349472528)) ;
#33465 = CARTESIAN_POINT('Ctrl Pts',(-18.8550155560846,12.6325062468968,122.291412852225)) ;
#33466 = CARTESIAN_POINT('Ctrl Pts',(-18.8547636888582,12.6324934028497,122.29153748546)) ;
#33467 = CARTESIAN_POINT('Ctrl Pts',(-18.8546399580043,12.63248709254,122.291598737592)) ;
#33468 = CARTESIAN_POINT('Ctrl Pts',(-18.8543966903674,12.6324746846061,122.291719215792)) ;
#33469 = CARTESIAN_POINT('Ctrl Pts',(-18.854277153185,12.6324685870025,122.291778440366)) ;
#33470 = CARTESIAN_POINT('Ctrl Pts',(-18.8540420728504,12.6324565943971,122.291894957549)) ;
#33471 = CARTESIAN_POINT('Ctrl Pts',(-18.8539265288778,12.6324506993911,122.291952249006)) ;
#33472 = CARTESIAN_POINT('Ctrl Pts',(-18.8536992450398,12.6324391024022,122.292064989514)) ;
#33473 = CARTESIAN_POINT('Ctrl Pts',(-18.8535875045862,12.6324334004239,122.29212043742)) ;
#33474 = CARTESIAN_POINT('Ctrl Pts',(-18.8533676479513,12.6324221804159,122.292229575811)) ;
#33475 = CARTESIAN_POINT('Ctrl Pts',(-18.8532595314138,12.6324166624,122.292283265148)) ;
#33476 = CARTESIAN_POINT('Ctrl Pts',(-18.8530467536773,12.6324058017891,122.292388966369)) ;
#33477 = CARTESIAN_POINT('Ctrl Pts',(-18.852942091726,12.6324004591854,122.292440977404)) ;
#33478 = CARTESIAN_POINT('Ctrl Pts',(-18.8527360618065,12.6323899412494,122.292543398586)) ;
#33479 = CARTESIAN_POINT('Ctrl Pts',(-18.8526346936263,12.6323847659338,122.292593807709)) ;
#33480 = CARTESIAN_POINT('Ctrl Pts',(-18.8524350996326,12.6323745749139,122.292693097118)) ;
#33481 = CARTESIAN_POINT('Ctrl Pts',(-18.8523368733561,12.6323695592114,122.29274197659)) ;
#33482 = CARTESIAN_POINT('Ctrl Pts',(-18.8521434194413,12.6323596801533,122.292838275129)) ;
#33483 = CARTESIAN_POINT('Ctrl Pts',(-18.8520481912971,12.6323548167953,122.29288569348)) ;
#33484 = CARTESIAN_POINT('Ctrl Pts',(-18.8518605969686,12.6323452355151,122.292979134973)) ;
#33485 = CARTESIAN_POINT('Ctrl Pts',(-18.8517682305587,12.6323405176031,122.293025157332)) ;
#33486 = CARTESIAN_POINT('Ctrl Pts',(-18.851586230627,12.6323312206861,122.2931158685)) ;
#33487 = CARTESIAN_POINT('Ctrl Pts',(-18.8514965968201,12.6323266416867,122.293160556623)) ;
#33488 = CARTESIAN_POINT('Ctrl Pts',(-18.8513199396624,12.6323176163998,122.293248657901)) ;
#33489 = CARTESIAN_POINT('Ctrl Pts',(-18.851232915995,12.6323131701149,122.293292070446)) ;
#33490 = CARTESIAN_POINT('Ctrl Pts',(-18.8510613633768,12.6323044043985,122.293377676028)) ;
#33491 = CARTESIAN_POINT('Ctrl Pts',(-18.850976833945,12.63230008496,122.293419868591)) ;
#33492 = CARTESIAN_POINT('Ctrl Pts',(-18.8508101590981,12.6322915673309,122.293503087348)) ;
#33493 = CARTESIAN_POINT('Ctrl Pts',(-18.850728013559,12.6322873691502,122.293544112942)) ;
#33494 = CARTESIAN_POINT('Ctrl Pts',(-18.8505660023795,12.6322790887634,122.293625047793)) ;
#33495 = CARTESIAN_POINT('Ctrl Pts',(-18.8504861363609,12.632275006553,122.293664956624)) ;
#33496 = CARTESIAN_POINT('Ctrl Pts',(-18.8503285846757,12.6322669530628,122.293743705865)) ;
#33497 = CARTESIAN_POINT('Ctrl Pts',(-18.8502508988245,12.6322629817876,122.293782545794)) ;
#33498 = CARTESIAN_POINT('Ctrl Pts',(-18.8500976136337,12.6322551454121,122.293859202448)) ;
#33499 = CARTESIAN_POINT('Ctrl Pts',(-18.8500220139255,12.6322512803059,122.293897018822)) ;
#33500 = CARTESIAN_POINT('Ctrl Pts',(-18.8498728106033,12.6322436516842,122.29397167201)) ;
#33501 = CARTESIAN_POINT('Ctrl Pts',(-18.8497992071395,12.6322398881885,122.294008508251)) ;
#33502 = CARTESIAN_POINT('Ctrl Pts',(-18.8496539118487,12.6322324585051,122.294081241963)) ;
#33503 = CARTESIAN_POINT('Ctrl Pts',(-18.8495822197,12.6322287923122,122.294117139132)) ;
#33504 = CARTESIAN_POINT('Ctrl Pts',(-18.8494406658337,12.6322215531152,122.294188033983)) ;
#33505 = CARTESIAN_POINT('Ctrl Pts',(-18.849370803934,12.6322179801123,122.294223031324)) ;
#33506 = CARTESIAN_POINT('Ctrl Pts',(-18.8492328337509,12.6322109233979,122.294292163715)) ;
#33507 = CARTESIAN_POINT('Ctrl Pts',(-18.8491647251495,12.6322074396799,122.29432629852)) ;
#33508 = CARTESIAN_POINT('Ctrl Pts',(-18.8490301882414,12.6322005578142,122.294393741386)) ;
#33509 = CARTESIAN_POINT('Ctrl Pts',(-18.8489637597144,12.6321971596645,122.294427049179)) ;
#33510 = CARTESIAN_POINT('Ctrl Pts',(-18.8488325124516,12.6321904453557,122.29449287225)) ;
#33511 = CARTESIAN_POINT('Ctrl Pts',(-18.8487676938904,12.6321871292143,122.294525387087)) ;
#33512 = CARTESIAN_POINT('Ctrl Pts',(-18.8486396006622,12.6321805755767,122.294589656251)) ;
#33513 = CARTESIAN_POINT('Ctrl Pts',(-18.8485763257236,12.6321773380746,122.294621410384)) ;
#33514 = CARTESIAN_POINT('Ctrl Pts',(-18.8484512563821,12.6321709384976,122.294684188953)) ;
#33515 = CARTESIAN_POINT('Ctrl Pts',(-18.8483894617543,12.6321677764187,122.294715213192)) ;
#33516 = CARTESIAN_POINT('Ctrl Pts',(-18.8482672920752,12.6321615245914,122.29477656166)) ;
#33517 = CARTESIAN_POINT('Ctrl Pts',(-18.8482069170872,12.6321584348532,122.294806885566)) ;
#33518 = CARTESIAN_POINT('Ctrl Pts',(-18.8480875295977,12.6321523248064,122.294866861177)) ;
#33519 = CARTESIAN_POINT('Ctrl Pts',(-18.8480285167885,12.6321493044888,122.294896512765)) ;
#33520 = CARTESIAN_POINT('Ctrl Pts',(-18.8479117983704,12.6321433304733,122.29495517071)) ;
#33521 = CARTESIAN_POINT('Ctrl Pts',(-18.8478540926495,12.632140376776,122.294984176868)) ;
#33522 = CARTESIAN_POINT('Ctrl Pts',(-18.8477399358622,12.6321345333301,122.295041569607)) ;
#33523 = CARTESIAN_POINT('Ctrl Pts',(-18.8476834847199,12.6321316435834,122.295069955986)) ;
#33524 = CARTESIAN_POINT('Ctrl Pts',(-18.8475717866948,12.6321259254765,122.295126133796)) ;
#33525 = CARTESIAN_POINT('Ctrl Pts',(-18.847516539838,12.6321230971231,122.295153924987)) ;
#33526 = CARTESIAN_POINT('Ctrl Pts',(-18.8474072027659,12.6321174993812,122.295208935705)) ;
#33527 = CARTESIAN_POINT('Ctrl Pts',(-18.8473531123719,12.6321147299887,122.295236155109)) ;
#33528 = CARTESIAN_POINT('Ctrl Pts',(-18.847246042138,12.6321092478244,122.295290044814)) ;
#33529 = CARTESIAN_POINT('Ctrl Pts',(-18.8471930623221,12.6321065350586,122.295316714903)) ;
#33530 = CARTESIAN_POINT('Ctrl Pts',(-18.847088169118,12.6321011639028,122.2953695276)) ;
#33531 = CARTESIAN_POINT('Ctrl Pts',(-18.847036255879,12.6320985055249,122.295395669944)) ;
#33532 = CARTESIAN_POINT('Ctrl Pts',(-18.8469334541267,12.632093241023,122.295447447592)) ;
#33533 = CARTESIAN_POINT('Ctrl Pts',(-18.8468825654951,12.6320906348972,122.295473082778)) ;
#33534 = CARTESIAN_POINT('Ctrl Pts',(-18.8467817731904,12.6320854728756,122.295523865619)) ;
#33535 = CARTESIAN_POINT('Ctrl Pts',(-18.846731869175,12.6320829169663,122.29554901328)) ;
#33536 = CARTESIAN_POINT('Ctrl Pts',(-18.8466330070026,12.6320778533874,122.295598840276)) ;
#33537 = CARTESIAN_POINT('Ctrl Pts',(-18.8465840488835,12.6320753457235,122.295623519436)) ;
#33538 = CARTESIAN_POINT('Ctrl Pts',(-18.846487042062,12.6320703767801,122.295672427334)) ;
#33539 = CARTESIAN_POINT('Ctrl Pts',(-18.8464389931377,12.6320679154928,122.295696656037)) ;
#33540 = CARTESIAN_POINT('Ctrl Pts',(-18.8463437686625,12.6320630374672,122.295744680755)) ;
#33541 = CARTESIAN_POINT('Ctrl Pts',(-18.8462965932748,12.6320606207405,122.29576847655)) ;
#33542 = CARTESIAN_POINT('Ctrl Pts',(-18.8462030825305,12.6320558301382,122.295815651855)) ;
#33543 = CARTESIAN_POINT('Ctrl Pts',(-18.8461567469141,12.6320534562524,122.295839031365)) ;
#33544 = CARTESIAN_POINT('Ctrl Pts',(-18.8460648831526,12.6320487496731,122.295885390138)) ;
#33545 = CARTESIAN_POINT('Ctrl Pts',(-18.8460193549114,12.6320464169778,122.295908369325)) ;
#33546 = CARTESIAN_POINT('Ctrl Pts',(-18.8459290731657,12.6320417911115,122.295953943604)) ;
#33547 = CARTESIAN_POINT('Ctrl Pts',(-18.8458843203151,12.6320394979768,122.295976538248)) ;
#33548 = CARTESIAN_POINT('Ctrl Pts',(-18.8457955610847,12.6320349497919,122.296021357362)) ;
#33549 = CARTESIAN_POINT('Ctrl Pts',(-18.8457515541166,12.6320326947142,122.296043582017)) ;
#33550 = CARTESIAN_POINT('Ctrl Pts',(-18.8456642572285,12.6320282211438,122.296087675683)) ;
#33551 = CARTESIAN_POINT('Ctrl Pts',(-18.8456209671826,12.6320260026471,122.296109544651)) ;
#33552 = CARTESIAN_POINT('Ctrl Pts',(-18.8455350756518,12.6320216007862,122.296152941019)) ;
#33553 = CARTESIAN_POINT('Ctrl Pts',(-18.8454924744056,12.6320194174368,122.296174468199)) ;
#33554 = CARTESIAN_POINT('Ctrl Pts',(-18.8454079345044,12.6320150845467,122.29621719382)) ;
#33555 = CARTESIAN_POINT('Ctrl Pts',(-18.8453659955881,12.632012934995,122.296238392297)) ;
#33556 = CARTESIAN_POINT('Ctrl Pts',(-18.8452827539264,12.6320086683532,122.296280473587)) ;
#33557 = CARTESIAN_POINT('Ctrl Pts',(-18.8452414513663,12.6320065512747,122.296301356216)) ;
#33558 = CARTESIAN_POINT('Ctrl Pts',(-18.8451112824266,12.6319998788775,122.296367178882)) ;
#33559 = CARTESIAN_POINT('Ctrl Pts',(-18.8450224204141,12.6319953235254,122.296412127165)) ;
#33560 = CARTESIAN_POINT('Ctrl Pts',(-18.8448453327161,12.6319862447871,122.296501728442)) ;
#33561 = CARTESIAN_POINT('Ctrl Pts',(-18.8447571069507,12.6319817214013,122.296546381289)) ;
#33562 = CARTESIAN_POINT('Ctrl Pts',(-18.8445812650707,12.6319727052414,122.296635404637)) ;
#33563 = CARTESIAN_POINT('Ctrl Pts',(-18.8444936487542,12.6319682124613,122.296679775063)) ;
#33564 = CARTESIAN_POINT('Ctrl Pts',(-18.8443189985797,12.6319592561309,122.296768246811)) ;
#33565 = CARTESIAN_POINT('Ctrl Pts',(-18.8442319648159,12.6319547925897,122.296812347916)) ;
#33566 = CARTESIAN_POINT('Ctrl Pts',(-18.8440584536272,12.6319458934097,122.296900293756)) ;
#33567 = CARTESIAN_POINT('Ctrl Pts',(-18.8439719760347,12.6319414577663,122.296944138415)) ;
#33568 = CARTESIAN_POINT('Ctrl Pts',(-18.8437995508156,12.6319326130407,122.297031584258)) ;
#33569 = CARTESIAN_POINT('Ctrl Pts',(-18.8437136030792,12.6319282039566,122.297075185345)) ;
#33570 = CARTESIAN_POINT('Ctrl Pts',(-18.8435422113537,12.6319194110155,122.297162156893)) ;
#33571 = CARTESIAN_POINT('Ctrl Pts',(-18.8434567672829,12.6319150271577,122.297205527253)) ;
#33572 = CARTESIAN_POINT('Ctrl Pts',(-18.8432863571278,12.6319062833578,122.297292049997)) ;
#33573 = CARTESIAN_POINT('Ctrl Pts',(-18.8432013908638,12.6319019234098,122.297335202337)) ;
#33574 = CARTESIAN_POINT('Ctrl Pts',(-18.8430319099121,12.6318932260836,122.297421302054)) ;
#33575 = CARTESIAN_POINT('Ctrl Pts',(-18.8429473953669,12.631888888716,122.297464249232)) ;
#33576 = CARTESIAN_POINT('Ctrl Pts',(-18.8427787924205,12.6318802352545,122.297549951172)) ;
#33577 = CARTESIAN_POINT('Ctrl Pts',(-18.8426947039215,12.6318759191586,122.297592705865)) ;
#33578 = CARTESIAN_POINT('Ctrl Pts',(-18.8425269269947,12.6318673069107,122.297678035739)) ;
#33579 = CARTESIAN_POINT('Ctrl Pts',(-18.8424432386552,12.631863010766,122.297720610763)) ;
#33580 = CARTESIAN_POINT('Ctrl Pts',(-18.8422762364909,12.6318544371166,122.297805593973)) ;
#33581 = CARTESIAN_POINT('Ctrl Pts',(-18.8421929225562,12.6318501596088,122.297848002111)) ;
#33582 = CARTESIAN_POINT('Ctrl Pts',(-18.8359759930584,12.6315309480047,122.301013397779)) ;
#33583 = CARTESIAN_POINT('Ctrl Pts',(-18.8298682818942,12.6312157651259,122.304186977921)) ;
#33584 = CARTESIAN_POINT('Ctrl Pts',(-18.8172837982111,12.6305629803702,122.310858477853)) ;
#33585 = CARTESIAN_POINT('Ctrl Pts',(-18.8108110832586,12.6302253536001,122.31436348947)) ;
#33586 = CARTESIAN_POINT('Ctrl Pts',(-18.7931089059569,12.6292966963258,122.32415250149)) ;
#33587 = CARTESIAN_POINT('Ctrl Pts',(-18.7819449551622,12.6287051223298,122.33055303697)) ;
#33588 = CARTESIAN_POINT('Ctrl Pts',(-18.739331492069,12.6264236172791,122.355866416145)) ;
#33589 = CARTESIAN_POINT('Ctrl Pts',(-18.7086218185486,12.6247289117547,122.375988294816)) ;
#33590 = CARTESIAN_POINT('Ctrl Pts',(-18.6666112199279,12.6223413244011,122.406239020898)) ;
#33591 = CARTESIAN_POINT('Ctrl Pts',(-18.6545405745837,12.6216468710371,122.415266684362)) ;
#33592 = CARTESIAN_POINT('Ctrl Pts',(-18.6391345846768,12.6207502099447,122.427229351818)) ;
#33593 = CARTESIAN_POINT('Ctrl Pts',(-18.6356475495466,12.6205465592115,122.429966874391)) ;
#33594 = CARTESIAN_POINT('Ctrl Pts',(-18.6299302728566,12.6202115335793,122.434504631282)) ;
#33595 = CARTESIAN_POINT('Ctrl Pts',(-18.6276915315442,12.6200800595681,122.436294086583)) ;
#33596 = CARTESIAN_POINT('Ctrl Pts',(-18.6245114773303,12.6198929037464,122.438853919667)) ;
#33597 = CARTESIAN_POINT('Ctrl Pts',(-18.6235651061448,12.6198371560234,122.439617994593)) ;
#33598 = CARTESIAN_POINT('Ctrl Pts',(-18.6212908234769,12.6197030636183,122.441459679734)) ;
#33599 = CARTESIAN_POINT('Ctrl Pts',(-18.6199640046755,12.6196247339192,122.442538636595)) ;
#33600 = CARTESIAN_POINT('Ctrl Pts',(-18.6148764975289,12.6193240089442,122.446693124195)) ;
#33601 = CARTESIAN_POINT('Ctrl Pts',(-18.6111315416416,12.6191018553758,122.449787841994)) ;
#33602 = CARTESIAN_POINT('Ctrl Pts',(-18.5953781676455,12.6181638902404,122.462961256232)) ;
#33603 = CARTESIAN_POINT('Ctrl Pts',(-18.583541828003,12.6174504462069,122.473243603067)) ;
#33604 = CARTESIAN_POINT('Ctrl Pts',(-18.5483328833257,12.6152953134125,122.505011650978)) ;
#33605 = CARTESIAN_POINT('Ctrl Pts',(-18.5255824463411,12.6138570837495,122.527167492912)) ;
#33606 = CARTESIAN_POINT('Ctrl Pts',(-18.4953990243446,12.611865868209,122.558889531879)) ;
#33607 = CARTESIAN_POINT('Ctrl Pts',(-18.4872244686767,12.6113176320481,122.567733248597)) ;
#33608 = CARTESIAN_POINT('Ctrl Pts',(-18.4733022493931,12.6103673277936,122.583238746288)) ;
#33609 = CARTESIAN_POINT('Ctrl Pts',(-18.4674947653121,12.6099657237916,122.589845651081)) ;
#33610 = CARTESIAN_POINT('Ctrl Pts',(-18.461737832456,12.6095621867674,122.596536159339)) ;
#33611 = CARTESIAN_POINT('Ctrl Pts',(-18.4617181500391,12.6095608070475,122.596559035239)) ;
#33612 = CARTESIAN_POINT('Ctrl Pts',(-18.461678929959,12.6095580576264,122.596604622137)) ;
#33613 = CARTESIAN_POINT('Ctrl Pts',(-18.4616593920997,12.6095566879124,122.59662733334)) ;
#33614 = CARTESIAN_POINT('Ctrl Pts',(-18.4616204591511,12.6095539583668,122.596672593077)) ;
#33615 = CARTESIAN_POINT('Ctrl Pts',(-18.4616010640651,12.6095525985364,122.596695141584)) ;
#33616 = CARTESIAN_POINT('Ctrl Pts',(-18.4615624145393,12.6095498886117,122.596740078328)) ;
#33617 = CARTESIAN_POINT('Ctrl Pts',(-18.4615431602748,12.6095485385307,122.596762466339)) ;
#33618 = CARTESIAN_POINT('Ctrl Pts',(-18.461504791375,12.6095458480362,122.596807083202)) ;
#33619 = CARTESIAN_POINT('Ctrl Pts',(-18.4614856764583,12.609544507604,122.59682931236)) ;
#33620 = CARTESIAN_POINT('Ctrl Pts',(-18.4614475841884,12.6095418362648,122.596873613853)) ;
#33621 = CARTESIAN_POINT('Ctrl Pts',(-18.4614286068381,12.6095405053589,122.596895686162)) ;
#33622 = CARTESIAN_POINT('Ctrl Pts',(-18.4613907879158,12.6095378529499,122.596939675966)) ;
#33623 = CARTESIAN_POINT('Ctrl Pts',(-18.4613719464074,12.6095365314521,122.596961593365)) ;
#33624 = CARTESIAN_POINT('Ctrl Pts',(-18.4613343977169,12.6095338977599,122.597005274973)) ;
#33625 = CARTESIAN_POINT('Ctrl Pts',(-18.46131569052,12.6095325855653,122.597027039178)) ;
#33626 = CARTESIAN_POINT('Ctrl Pts',(-18.461278408422,12.6095299703395,122.597070416694)) ;
#33627 = CARTESIAN_POINT('Ctrl Pts',(-18.4612598338192,12.6095286673301,122.597092029637)) ;
#33628 = CARTESIAN_POINT('Ctrl Pts',(-18.461222814797,12.609526070329,122.597135107026)) ;
#33629 = CARTESIAN_POINT('Ctrl Pts',(-18.4612043707521,12.6095247763644,122.597156571015)) ;
#33630 = CARTESIAN_POINT('Ctrl Pts',(-18.4611676131826,12.6095221974788,122.59719935004)) ;
#33631 = CARTESIAN_POINT('Ctrl Pts',(-18.4611492988601,12.6095209125027,122.597220665985)) ;
#33632 = CARTESIAN_POINT('Ctrl Pts',(-18.4611127976523,12.6095183513802,122.59726315245)) ;
#33633 = CARTESIAN_POINT('Ctrl Pts',(-18.4610946110612,12.6095170752553,122.597284322607)) ;
#33634 = CARTESIAN_POINT('Ctrl Pts',(-18.4610583638588,12.6095145317351,122.597326519134)) ;
#33635 = CARTESIAN_POINT('Ctrl Pts',(-18.4610403033948,12.609513264351,122.597347545312)) ;
#33636 = CARTESIAN_POINT('Ctrl Pts',(-18.4610043072333,12.6095107382297,122.597389455234)) ;
#33637 = CARTESIAN_POINT('Ctrl Pts',(-18.4609863714188,12.609509479485,122.597410339095)) ;
#33638 = CARTESIAN_POINT('Ctrl Pts',(-18.4609506232812,12.6095069705552,122.59745196581)) ;
#33639 = CARTESIAN_POINT('Ctrl Pts',(-18.4609328107254,12.6095057203545,122.597472708916)) ;
#33640 = CARTESIAN_POINT('Ctrl Pts',(-18.4608973071031,12.6095032283744,122.597514056395)) ;
#33641 = CARTESIAN_POINT('Ctrl Pts',(-18.4608796160897,12.6095019865993,122.597534660688)) ;
#33642 = CARTESIAN_POINT('Ctrl Pts',(-18.4608443546439,12.6094995114089,122.597575731545)) ;
#33643 = CARTESIAN_POINT('Ctrl Pts',(-18.460826783901,12.6094982779724,122.597596198451)) ;
#33644 = CARTESIAN_POINT('Ctrl Pts',(-18.4607917613206,12.6094958193435,122.597636996433)) ;
#33645 = CARTESIAN_POINT('Ctrl Pts',(-18.4607743094319,12.6094945941482,122.597657327549)) ;
#33646 = CARTESIAN_POINT('Ctrl Pts',(-18.4607395224066,12.6094921518525,122.597697856404)) ;
#33647 = CARTESIAN_POINT('Ctrl Pts',(-18.460722187613,12.6094909347769,122.597718053725)) ;
#33648 = CARTESIAN_POINT('Ctrl Pts',(-18.4606876341617,12.6094885086794,122.597758315657)) ;
#33649 = CARTESIAN_POINT('Ctrl Pts',(-18.4606704153043,12.6094872996442,122.597778380482)) ;
#33650 = CARTESIAN_POINT('Ctrl Pts',(-18.4606360920355,12.6094848895107,122.597818379339)) ;
#33651 = CARTESIAN_POINT('Ctrl Pts',(-18.4606189876851,12.6094836884174,122.597838313282)) ;
#33652 = CARTESIAN_POINT('Ctrl Pts',(-18.4605848914725,12.6094812940323,122.597878052607)) ;
#33653 = CARTESIAN_POINT('Ctrl Pts',(-18.4605678998635,12.6094801007589,122.597897857676)) ;
#33654 = CARTESIAN_POINT('Ctrl Pts',(-18.4605340293663,12.6094777220318,122.59793733893)) ;
#33655 = CARTESIAN_POINT('Ctrl Pts',(-18.4605171498181,12.6094765365324,122.597957015869)) ;
#33656 = CARTESIAN_POINT('Ctrl Pts',(-18.4604835004398,12.6094741731442,122.597996244315)) ;
#33657 = CARTESIAN_POINT('Ctrl Pts',(-18.4604667310949,12.6094729952902,122.59801579524)) ;
#33658 = CARTESIAN_POINT('Ctrl Pts',(-18.4604333012486,12.6094706471332,122.59805477263)) ;
#33659 = CARTESIAN_POINT('Ctrl Pts',(-18.4604166409078,12.6094694768422,122.598074198893)) ;
#33660 = CARTESIAN_POINT('Ctrl Pts',(-18.4603834273502,12.6094671436922,122.598112928916)) ;
#33661 = CARTESIAN_POINT('Ctrl Pts',(-18.4603668743855,12.6094659808515,122.598132232368)) ;
#33662 = CARTESIAN_POINT('Ctrl Pts',(-18.4603338755982,12.6094636626054,122.598170716702)) ;
#33663 = CARTESIAN_POINT('Ctrl Pts',(-18.4603174292141,12.609462507161,122.598189898225)) ;
#33664 = CARTESIAN_POINT('Ctrl Pts',(-18.460284641383,12.6094602035543,122.598228141227)) ;
#33665 = CARTESIAN_POINT('Ctrl Pts',(-18.4602683000927,12.6094590554035,122.59824720251)) ;
#33666 = CARTESIAN_POINT('Ctrl Pts',(-18.460235720693,12.6094567662621,122.598285207037)) ;
#33667 = CARTESIAN_POINT('Ctrl Pts',(-18.4602194828837,12.6094556252932,122.598304149917)) ;
#33668 = CARTESIAN_POINT('Ctrl Pts',(-18.4601871105868,12.6094533505273,122.598341917431)) ;
#33669 = CARTESIAN_POINT('Ctrl Pts',(-18.4601709755477,12.609452216692,122.598360742694)) ;
#33670 = CARTESIAN_POINT('Ctrl Pts',(-18.4601388064741,12.6094499560322,122.598398277636)) ;
#33671 = CARTESIAN_POINT('Ctrl Pts',(-18.4601227726865,12.6094488292255,122.598416987011)) ;
#33672 = CARTESIAN_POINT('Ctrl Pts',(-18.4600908048319,12.6094465825341,122.598454291634)) ;
#33673 = CARTESIAN_POINT('Ctrl Pts',(-18.4600748709927,12.609445462666,122.598472886602)) ;
#33674 = CARTESIAN_POINT('Ctrl Pts',(-18.4600431020616,12.6094432297849,122.598509963503)) ;
#33675 = CARTESIAN_POINT('Ctrl Pts',(-18.4600272669724,12.6094421167727,122.598528445419)) ;
#33676 = CARTESIAN_POINT('Ctrl Pts',(-18.4599956945988,12.6094398975388,122.598565297278)) ;
#33677 = CARTESIAN_POINT('Ctrl Pts',(-18.4599799571594,12.6094387913067,122.598583667388)) ;
#33678 = CARTESIAN_POINT('Ctrl Pts',(-18.459948578622,12.6094365855317,122.598620297301)) ;
#33679 = CARTESIAN_POINT('Ctrl Pts',(-18.4599329375119,12.6094354859884,122.598638557106)) ;
#33680 = CARTESIAN_POINT('Ctrl Pts',(-18.4599017508851,12.60943329354,122.598674967243)) ;
#33681 = CARTESIAN_POINT('Ctrl Pts',(-18.4598862051093,12.6094322006171,122.598693117866)) ;
#33682 = CARTESIAN_POINT('Ctrl Pts',(-18.4598552076536,12.6094300213056,122.598729311349)) ;
#33683 = CARTESIAN_POINT('Ctrl Pts',(-18.4598397560122,12.6094289349202,122.598747354152)) ;
#33684 = CARTESIAN_POINT('Ctrl Pts',(-18.4598089454057,12.6094267685853,122.598783333616)) ;
#33685 = CARTESIAN_POINT('Ctrl Pts',(-18.4597935866557,12.6094256886514,122.598801270014)) ;
#33686 = CARTESIAN_POINT('Ctrl Pts',(-18.4597629607741,12.6094235351465,122.598837037867)) ;
#33687 = CARTESIAN_POINT('Ctrl Pts',(-18.4597476937627,12.6094224615845,122.598854869169)) ;
#33688 = CARTESIAN_POINT('Ctrl Pts',(-18.459717250441,12.6094203207602,122.598890427866)) ;
#33689 = CARTESIAN_POINT('Ctrl Pts',(-18.4597020740995,12.6094192534963,122.598908155284)) ;
#33690 = CARTESIAN_POINT('Ctrl Pts',(-18.4596718109145,12.609417125185,122.598943507583)) ;
#33691 = CARTESIAN_POINT('Ctrl Pts',(-18.4596567240353,12.6094160641356,122.598961132494)) ;
#33692 = CARTESIAN_POINT('Ctrl Pts',(-18.4596266391364,12.6094139482099,122.598996280487)) ;
#33693 = CARTESIAN_POINT('Ctrl Pts',(-18.4596116408026,12.6094128933119,122.599013803925)) ;
#33694 = CARTESIAN_POINT('Ctrl Pts',(-18.4595817314313,12.6094107895803,122.599048750767)) ;
#33695 = CARTESIAN_POINT('Ctrl Pts',(-18.4595668203246,12.6094097407422,122.599066174239)) ;
#33696 = CARTESIAN_POINT('Ctrl Pts',(-18.4595370854242,12.6094076491331,122.599100921096)) ;
#33697 = CARTESIAN_POINT('Ctrl Pts',(-18.4595222611085,12.6094066063256,122.599118245078)) ;
#33698 = CARTESIAN_POINT('Ctrl Pts',(-18.4594926963092,12.6094045265341,122.59915279699)) ;
#33699 = CARTESIAN_POINT('Ctrl Pts',(-18.4594779567372,12.6094034896145,122.599170023842)) ;
#33700 = CARTESIAN_POINT('Ctrl Pts',(-18.4594485627125,12.6094014216904,122.599204379956)) ;
#33701 = CARTESIAN_POINT('Ctrl Pts',(-18.4594339076772,12.6094003906454,122.599221509888)) ;
#33702 = CARTESIAN_POINT('Ctrl Pts',(-18.4594046802912,12.6093983343003,122.599255674974)) ;
#33703 = CARTESIAN_POINT('Ctrl Pts',(-18.4593901083494,12.6093973090295,122.59927270964)) ;
#33704 = CARTESIAN_POINT('Ctrl Pts',(-18.4593610461059,12.6093952641605,122.599306685385)) ;
#33705 = CARTESIAN_POINT('Ctrl Pts',(-18.4593465560063,12.6093942445771,122.599323626217)) ;
#33706 = CARTESIAN_POINT('Ctrl Pts',(-18.4593176579707,12.6093922111209,122.599357413651)) ;
#33707 = CARTESIAN_POINT('Ctrl Pts',(-18.4593032493365,12.6093911971995,122.599374261059)) ;
#33708 = CARTESIAN_POINT('Ctrl Pts',(-18.4592745117047,12.6093891748908,122.599407864569)) ;
#33709 = CARTESIAN_POINT('Ctrl Pts',(-18.4592601830087,12.609388166525,122.599424620308)) ;
#33710 = CARTESIAN_POINT('Ctrl Pts',(-18.4592316052021,12.6093861553253,122.599458040511)) ;
#33711 = CARTESIAN_POINT('Ctrl Pts',(-18.4592173558299,12.6093851524732,122.599474705271)) ;
#33712 = CARTESIAN_POINT('Ctrl Pts',(-18.4591889348375,12.6093831521728,122.599507945629)) ;
#33713 = CARTESIAN_POINT('Ctrl Pts',(-18.459174763505,12.6093821547452,122.599524520882)) ;
#33714 = CARTESIAN_POINT('Ctrl Pts',(-18.4591464981643,12.6093801652645,122.599557582698)) ;
#33715 = CARTESIAN_POINT('Ctrl Pts',(-18.4591324040815,12.6093791732067,122.599574069339)) ;
#33716 = CARTESIAN_POINT('Ctrl Pts',(-18.4591042920639,12.6093771943841,122.599606955279)) ;
#33717 = CARTESIAN_POINT('Ctrl Pts',(-18.4590902742304,12.6093762076268,122.599623354451)) ;
#33718 = CARTESIAN_POINT('Ctrl Pts',(-18.4590623136088,12.6093742393287,122.599656066715)) ;
#33719 = CARTESIAN_POINT('Ctrl Pts',(-18.459048370972,12.6093732577989,122.599672379621)) ;
#33720 = CARTESIAN_POINT('Ctrl Pts',(-18.4590205603283,12.6093712999276,122.599704919812)) ;
#33721 = CARTESIAN_POINT('Ctrl Pts',(-18.4590066922013,12.609370323578,122.59972114723)) ;
#33722 = CARTESIAN_POINT('Ctrl Pts',(-18.4589790287884,12.6093683759421,122.59975351851)) ;
#33723 = CARTESIAN_POINT('Ctrl Pts',(-18.458965233855,12.6093674046811,122.599769661951)) ;
#33724 = CARTESIAN_POINT('Ctrl Pts',(-18.458937717021,12.6093654672368,122.59980186503)) ;
#33725 = CARTESIAN_POINT('Ctrl Pts',(-18.4589239947938,12.609364501031,122.59981792504)) ;
#33726 = CARTESIAN_POINT('Ctrl Pts',(-18.4588966214556,12.6093625735632,122.599849963474)) ;
#33727 = CARTESIAN_POINT('Ctrl Pts',(-18.4588829706057,12.60936161232,122.599865941583)) ;
#33728 = CARTESIAN_POINT('Ctrl Pts',(-18.4588557401595,12.6093596947882,122.599897816027)) ;
#33729 = CARTESIAN_POINT('Ctrl Pts',(-18.4588421601709,12.6093587384723,122.599913712813)) ;
#33730 = CARTESIAN_POINT('Ctrl Pts',(-18.4588150699696,12.6093568306919,122.599945426317)) ;
#33731 = CARTESIAN_POINT('Ctrl Pts',(-18.4588015598415,12.6093558792338,122.599961242927)) ;
#33732 = CARTESIAN_POINT('Ctrl Pts',(-18.4587746080911,12.6093539810804,122.59999279754)) ;
#33733 = CARTESIAN_POINT('Ctrl Pts',(-18.4587611666923,12.6093530344013,122.600008535274)) ;
#33734 = CARTESIAN_POINT('Ctrl Pts',(-18.4587343524859,12.609351145813,122.600039932012)) ;
#33735 = CARTESIAN_POINT('Ctrl Pts',(-18.4587209792818,12.6093502038762,122.600055591471)) ;
#33736 = CARTESIAN_POINT('Ctrl Pts',(-18.4586943003721,12.6093483246964,122.600086832916)) ;
#33737 = CARTESIAN_POINT('Ctrl Pts',(-18.4586809946577,12.6093473874531,122.600102414904)) ;
#33738 = CARTESIAN_POINT('Ctrl Pts',(-18.4586544482189,12.6093455174846,122.600133504319)) ;
#33739 = CARTESIAN_POINT('Ctrl Pts',(-18.4586412083282,12.6093445848184,122.600149010763)) ;
#33740 = CARTESIAN_POINT('Ctrl Pts',(-18.4586147950053,12.6093427241084,122.600179947347)) ;
#33741 = CARTESIAN_POINT('Ctrl Pts',(-18.4586016208327,12.6093417960127,122.600195378348)) ;
#33742 = CARTESIAN_POINT('Ctrl Pts',(-18.4585753373632,12.6093399443331,122.600226165877)) ;
#33743 = CARTESIAN_POINT('Ctrl Pts',(-18.4585622279331,12.6093390207401,122.600241522555)) ;
#33744 = CARTESIAN_POINT('Ctrl Pts',(-18.4585360728926,12.6093371779922,122.600272162653)) ;
#33745 = CARTESIAN_POINT('Ctrl Pts',(-18.4585230273456,12.6093362588421,122.600287445993)) ;
#33746 = CARTESIAN_POINT('Ctrl Pts',(-18.4584969991102,12.6093344249132,122.60031794052)) ;
#33747 = CARTESIAN_POINT('Ctrl Pts',(-18.4584840165725,12.6093335101454,122.600333151524)) ;
#33748 = CARTESIAN_POINT('Ctrl Pts',(-18.4584581136756,12.6093316849338,122.600363502156)) ;
#33749 = CARTESIAN_POINT('Ctrl Pts',(-18.4584451933963,12.609330774496,122.600378641682)) ;
#33750 = CARTESIAN_POINT('Ctrl Pts',(-18.4584194137448,12.6093289578559,122.600408850828)) ;
#33751 = CARTESIAN_POINT('Ctrl Pts',(-18.4584065545495,12.6093280516663,122.600423920233)) ;
#33752 = CARTESIAN_POINT('Ctrl Pts',(-18.4583808983417,12.6093262436131,122.60045398762)) ;
#33753 = CARTESIAN_POINT('Ctrl Pts',(-18.4583681004896,12.6093253416907,122.600468986579)) ;
#33754 = CARTESIAN_POINT('Ctrl Pts',(-18.4583425626679,12.6093235418697,122.600498918094)) ;
#33755 = CARTESIAN_POINT('Ctrl Pts',(-18.4583298239715,12.6093226440611,122.600513849151)) ;
#33756 = CARTESIAN_POINT('Ctrl Pts',(-18.458304406629,12.6093208526213,122.6005436423)) ;
#33757 = CARTESIAN_POINT('Ctrl Pts',(-18.4582917272025,12.6093199589353,122.600558505301)) ;
#33758 = CARTESIAN_POINT('Ctrl Pts',(-18.458266426828,12.6093181756307,122.600588164162)) ;
#33759 = CARTESIAN_POINT('Ctrl Pts',(-18.4582538056884,12.6093172859988,122.60060296024)) ;
#33760 = CARTESIAN_POINT('Ctrl Pts',(-18.4582286214437,12.6093155107718,122.600632485756)) ;
#33761 = CARTESIAN_POINT('Ctrl Pts',(-18.458216058113,12.6093146251611,122.600647215453)) ;
#33762 = CARTESIAN_POINT('Ctrl Pts',(-18.458190987638,12.6093128578468,122.600676610354)) ;
#33763 = CARTESIAN_POINT('Ctrl Pts',(-18.4581784810713,12.6093119761842,122.600691274875)) ;
#33764 = CARTESIAN_POINT('Ctrl Pts',(-18.4581535230788,12.6093102166932,122.600720540633)) ;
#33765 = CARTESIAN_POINT('Ctrl Pts',(-18.4581410721763,12.609309338902,122.60073514125)) ;
#33766 = CARTESIAN_POINT('Ctrl Pts',(-18.4581162264057,12.6093075872175,122.600764278134)) ;
#33767 = CARTESIAN_POINT('Ctrl Pts',(-18.4581038309577,12.6093067132835,122.600778815075)) ;
#33768 = CARTESIAN_POINT('Ctrl Pts',(-18.4580790947115,12.6093049692166,122.600807826213)) ;
#33769 = CARTESIAN_POINT('Ctrl Pts',(-18.4580667538103,12.6093040990766,122.600822300525)) ;
#33770 = CARTESIAN_POINT('Ctrl Pts',(-18.4580421260732,12.6093023625571,122.600851187072)) ;
#33771 = CARTESIAN_POINT('Ctrl Pts',(-18.4580298390942,12.6093014961677,122.600865599469)) ;
#33772 = CARTESIAN_POINT('Ctrl Pts',(-18.4580053181317,12.6092997670746,122.600894363426)) ;
#33773 = CARTESIAN_POINT('Ctrl Pts',(-18.4579930842709,12.6092989043797,122.600908714835)) ;
#33774 = CARTESIAN_POINT('Ctrl Pts',(-18.4579686688931,12.6092971826304,122.600937357563)) ;
#33775 = CARTESIAN_POINT('Ctrl Pts',(-18.4579564875071,12.6092963235854,122.600951648722)) ;
#33776 = CARTESIAN_POINT('Ctrl Pts',(-18.4579321755381,12.6092946090277,122.60098017274)) ;
#33777 = CARTESIAN_POINT('Ctrl Pts',(-18.4579200453207,12.609293753541,122.600994405165)) ;
#33778 = CARTESIAN_POINT('Ctrl Pts',(-18.4578958375331,12.6092920462307,122.601022809534)) ;
#33779 = CARTESIAN_POINT('Ctrl Pts',(-18.4578837587607,12.6092911943226,122.601036982884)) ;
#33780 = CARTESIAN_POINT('Ctrl Pts',(-18.4578596512629,12.6092894939864,122.601065272138)) ;
#33781 = CARTESIAN_POINT('Ctrl Pts',(-18.4578476226887,12.6092886455694,122.60107938786)) ;
#33782 = CARTESIAN_POINT('Ctrl Pts',(-18.4578236156322,12.6092869522193,122.601107561791)) ;
#33783 = CARTESIAN_POINT('Ctrl Pts',(-18.4578116370117,12.6092861072768,122.601121620156)) ;
#33784 = CARTESIAN_POINT('Ctrl Pts',(-18.457787727346,12.6092844206989,122.601149682311)) ;
#33785 = CARTESIAN_POINT('Ctrl Pts',(-18.4577757971843,12.609283579126,122.601163685059)) ;
#33786 = CARTESIAN_POINT('Ctrl Pts',(-18.4577519858381,12.6092818993868,122.601191634319)) ;
#33787 = CARTESIAN_POINT('Ctrl Pts',(-18.4577401041467,12.6092810611849,122.601205581421)) ;
#33788 = CARTESIAN_POINT('Ctrl Pts',(-18.4577163882053,12.6092793880801,122.601233421177)) ;
#33789 = CARTESIAN_POINT('Ctrl Pts',(-18.4577045541045,12.6092785531878,122.60124731365)) ;
#33790 = CARTESIAN_POINT('Ctrl Pts',(-18.4576809326251,12.6092768866519,122.601275044979)) ;
#33791 = CARTESIAN_POINT('Ctrl Pts',(-18.4576691454202,12.6092760550207,122.601288883625)) ;
#33792 = CARTESIAN_POINT('Ctrl Pts',(-18.457645616997,12.6092743949557,122.601316508148)) ;
#33793 = CARTESIAN_POINT('Ctrl Pts',(-18.4576338759057,12.609273566531,122.601330293871)) ;
#33794 = CARTESIAN_POINT('Ctrl Pts',(-18.4576104398768,12.6092719128912,122.601357812337)) ;
#33795 = CARTESIAN_POINT('Ctrl Pts',(-18.4575987446434,12.6092710876554,122.601371545423)) ;
#33796 = CARTESIAN_POINT('Ctrl Pts',(-18.4575753983673,12.6092694402556,122.601398960906)) ;
#33797 = CARTESIAN_POINT('Ctrl Pts',(-18.4575637477879,12.6092686181244,122.601412642755)) ;
#33798 = CARTESIAN_POINT('Ctrl Pts',(-18.4575404915852,12.6092669769882,122.601439954852)) ;
#33799 = CARTESIAN_POINT('Ctrl Pts',(-18.4575288855393,12.6092661579536,122.601453585591)) ;
#33800 = CARTESIAN_POINT('Ctrl Pts',(-18.4575057165708,12.6092645228817,122.601480797608)) ;
#33801 = CARTESIAN_POINT('Ctrl Pts',(-18.4574941538756,12.6092637068607,122.601494378615)) ;
#33802 = CARTESIAN_POINT('Ctrl Pts',(-18.4574710725384,12.6092620778821,122.60152149006)) ;
#33803 = CARTESIAN_POINT('Ctrl Pts',(-18.4574595531777,12.6092612648741,122.601535021339)) ;
#33804 = CARTESIAN_POINT('Ctrl Pts',(-18.4574365566691,12.6092596417921,122.601562035478)) ;
#33805 = CARTESIAN_POINT('Ctrl Pts',(-18.4574250796714,12.6092588317289,122.601575518157)) ;
#33806 = CARTESIAN_POINT('Ctrl Pts',(-18.4574021675679,12.6092572145145,122.601602435463)) ;
#33807 = CARTESIAN_POINT('Ctrl Pts',(-18.457390732468,12.6092564073639,122.601615870077)) ;
#33808 = CARTESIAN_POINT('Ctrl Pts',(-18.4573679031169,12.6092547959015,122.601642692465)) ;
#33809 = CARTESIAN_POINT('Ctrl Pts',(-18.4573565091921,12.6092539916129,122.601656079851)) ;
#33810 = CARTESIAN_POINT('Ctrl Pts',(-18.457333761452,12.6092523858228,122.601682808639)) ;
#33811 = CARTESIAN_POINT('Ctrl Pts',(-18.4573224079669,12.6092515843448,122.601696149648)) ;
#33812 = CARTESIAN_POINT('Ctrl Pts',(-18.4572997407641,12.6092499841521,122.601722786072)) ;
#33813 = CARTESIAN_POINT('Ctrl Pts',(-18.4572884270274,12.6092491854363,122.601736081506)) ;
#33814 = CARTESIAN_POINT('Ctrl Pts',(-18.4572658399085,12.60924759081,122.601762626076)) ;
#33815 = CARTESIAN_POINT('Ctrl Pts',(-18.4572545659102,12.6092467948561,122.601775875933)) ;
#33816 = CARTESIAN_POINT('Ctrl Pts',(-18.4572320558713,12.609245205585,122.601802332156)) ;
#33817 = CARTESIAN_POINT('Ctrl Pts',(-18.4572208203674,12.6092444123058,122.601815537888)) ;
#33818 = CARTESIAN_POINT('Ctrl Pts',(-18.4571983879089,12.609242828426,122.601841905153)) ;
#33819 = CARTESIAN_POINT('Ctrl Pts',(-18.4571871907465,12.609242037811,122.601855066927)) ;
#33820 = CARTESIAN_POINT('Ctrl Pts',(-18.4571648332459,12.6092404591383,122.601881348295)) ;
#33821 = CARTESIAN_POINT('Ctrl Pts',(-18.4571536732682,12.6092396711063,122.601894467461)) ;
#33822 = CARTESIAN_POINT('Ctrl Pts',(-18.4571313915593,12.6092380977004,122.601920661929)) ;
#33823 = CARTESIAN_POINT('Ctrl Pts',(-18.4571202690711,12.6092373122732,122.601933738118)) ;
#33824 = CARTESIAN_POINT('Ctrl Pts',(-18.4570980593876,12.609235743869,122.601959850092)) ;
#33825 = CARTESIAN_POINT('Ctrl Pts',(-18.4570869729658,12.6092349609467,122.601972884965)) ;
#33826 = CARTESIAN_POINT('Ctrl Pts',(-18.4570648359499,12.6092333975903,122.60199891367)) ;
#33827 = CARTESIAN_POINT('Ctrl Pts',(-18.4570537851656,12.6092326171429,122.602011907722)) ;
#33828 = CARTESIAN_POINT('Ctrl Pts',(-18.4570317199976,12.6092310587773,122.602037854101)) ;
#33829 = CARTESIAN_POINT('Ctrl Pts',(-18.4570207049007,12.6092302808088,122.602050807262)) ;
#33830 = CARTESIAN_POINT('Ctrl Pts',(-18.4569987083611,12.6092287272073,122.60207667508)) ;
#33831 = CARTESIAN_POINT('Ctrl Pts',(-18.4569877275509,12.6092279516191,122.602089588988)) ;
#33832 = CARTESIAN_POINT('Ctrl Pts',(-18.4569658004547,12.60922640284,122.602115377267)) ;
#33833 = CARTESIAN_POINT('Ctrl Pts',(-18.4569548536685,12.6092256296139,122.602128252221)) ;
#33834 = CARTESIAN_POINT('Ctrl Pts',(-18.4569329949719,12.6092240855844,122.602153962168)) ;
#33835 = CARTESIAN_POINT('Ctrl Pts',(-18.4569220823415,12.6092233147302,122.602166798004)) ;
#33836 = CARTESIAN_POINT('Ctrl Pts',(-18.4569002884575,12.6092217751975,122.60219243382)) ;
#33837 = CARTESIAN_POINT('Ctrl Pts',(-18.4568894083333,12.6092210065989,122.602205232468)) ;
#33838 = CARTESIAN_POINT('Ctrl Pts',(-18.4568676808509,12.609219471676,122.602230792264)) ;
#33839 = CARTESIAN_POINT('Ctrl Pts',(-18.4568568332239,12.6092187053329,122.602243553726)) ;
#33840 = CARTESIAN_POINT('Ctrl Pts',(-18.4568351700342,12.6092171748715,122.602269039965)) ;
#33841 = CARTESIAN_POINT('Ctrl Pts',(-18.4568243544449,12.6092164107516,122.602281764772)) ;
#33842 = CARTESIAN_POINT('Ctrl Pts',(-18.4568027537335,12.6092148846244,122.602307179571)) ;
#33843 = CARTESIAN_POINT('Ctrl Pts',(-18.4567919690989,12.6092141226515,122.602319868988)) ;
#33844 = CARTESIAN_POINT('Ctrl Pts',(-18.4567704313574,12.6092126008937,122.602345211751)) ;
#33845 = CARTESIAN_POINT('Ctrl Pts',(-18.4567596776703,12.6092118410679,122.602357865778)) ;
#33846 = CARTESIAN_POINT('Ctrl Pts',(-18.4567382008342,12.6092103235344,122.602383138917)) ;
#33847 = CARTESIAN_POINT('Ctrl Pts',(-18.4567274776408,12.6092095658237,122.602395758079)) ;
#33848 = CARTESIAN_POINT('Ctrl Pts',(-18.4567060599776,12.6092080523927,122.602420963616)) ;
#33849 = CARTESIAN_POINT('Ctrl Pts',(-18.4566953662781,12.6092072967269,122.602433549082)) ;
#33850 = CARTESIAN_POINT('Ctrl Pts',(-18.4566740075616,12.609205787383,122.602458687266)) ;
#33851 = CARTESIAN_POINT('Ctrl Pts',(-18.4566633427467,12.6092050337193,122.602471239744)) ;
#33852 = CARTESIAN_POINT('Ctrl Pts',(-18.4566420426704,12.6092035284416,122.60249631092)) ;
#33853 = CARTESIAN_POINT('Ctrl Pts',(-18.4566314068469,12.6092027767879,122.602508830277)) ;
#33854 = CARTESIAN_POINT('Ctrl Pts',(-18.4566101622527,12.6092012753537,122.602533838146)) ;
#33855 = CARTESIAN_POINT('Ctrl Pts',(-18.4565995540587,12.609200525614,122.602546325977)) ;
#33856 = CARTESIAN_POINT('Ctrl Pts',(-18.45657836624,12.6091990281154,122.602571269001)) ;
#33857 = CARTESIAN_POINT('Ctrl Pts',(-18.4565677858606,12.6091982803032,122.60258372508)) ;
#33858 = CARTESIAN_POINT('Ctrl Pts',(-18.456546652051,12.6091967865452,122.602608606501)) ;
#33859 = CARTESIAN_POINT('Ctrl Pts',(-18.4565360986608,12.6091960406023,122.602621031793)) ;
#33860 = CARTESIAN_POINT('Ctrl Pts',(-18.4565150183354,12.6091945505484,122.602645852213)) ;
#33861 = CARTESIAN_POINT('Ctrl Pts',(-18.4565044913614,12.6091938064347,122.602658247385)) ;
#33862 = CARTESIAN_POINT('Ctrl Pts',(-18.4564834638496,12.6091923200381,122.60268300758)) ;
#33863 = CARTESIAN_POINT('Ctrl Pts',(-18.4564729630377,12.6091915777359,122.602695372923)) ;
#33864 = CARTESIAN_POINT('Ctrl Pts',(-18.4564519865588,12.6091900948712,122.602720074975)) ;
#33865 = CARTESIAN_POINT('Ctrl Pts',(-18.4564415111882,12.6091893543297,122.602732411333)) ;
#33866 = CARTESIAN_POINT('Ctrl Pts',(-18.4564205848243,12.6091878749326,122.602757056309)) ;
#33867 = CARTESIAN_POINT('Ctrl Pts',(-18.456410134092,12.6091871360954,122.602769364619)) ;
#33868 = CARTESIAN_POINT('Ctrl Pts',(-18.4563892581176,12.6091856601858,122.602793952182)) ;
#33869 = CARTESIAN_POINT('Ctrl Pts',(-18.4563788322551,12.6091849230696,122.602806232165)) ;
#33870 = CARTESIAN_POINT('Ctrl Pts',(-18.4563580034952,12.6091834504235,122.602830766042)) ;
#33871 = CARTESIAN_POINT('Ctrl Pts',(-18.456347601324,12.6091827149451,122.60284301908)) ;
#33872 = CARTESIAN_POINT('Ctrl Pts',(-18.4563268202517,12.6091812455965,122.602867498701)) ;
#33873 = CARTESIAN_POINT('Ctrl Pts',(-18.4563164414381,12.6091805117326,122.602879725179)) ;
#33874 = CARTESIAN_POINT('Ctrl Pts',(-18.4562957065655,12.6091790455768,122.602904152283)) ;
#33875 = CARTESIAN_POINT('Ctrl Pts',(-18.4562853504939,12.6091783132841,122.602916352922)) ;
#33876 = CARTESIAN_POINT('Ctrl Pts',(-18.456264661426,12.6091768502936,122.602940727963)) ;
#33877 = CARTESIAN_POINT('Ctrl Pts',(-18.4562543279906,12.6091761195649,122.60295290288)) ;
#33878 = CARTESIAN_POINT('Ctrl Pts',(-18.4562336824289,12.6091746595776,122.602977228553)) ;
#33879 = CARTESIAN_POINT('Ctrl Pts',(-18.456223370633,12.6091739303426,122.602989378918)) ;
#33880 = CARTESIAN_POINT('Ctrl Pts',(-18.4562027687069,12.6091724733682,122.603013655059)) ;
#33881 = CARTESIAN_POINT('Ctrl Pts',(-18.4561924782268,12.6091717456042,122.603025781246)) ;
#33882 = CARTESIAN_POINT('Ctrl Pts',(-18.4561719189495,12.6091702915734,122.603050009007)) ;
#33883 = CARTESIAN_POINT('Ctrl Pts',(-18.4561616496515,12.6091695652712,122.603062111169)) ;
#33884 = CARTESIAN_POINT('Ctrl Pts',(-18.4561411309177,12.6091681140354,122.603086293019)) ;
#33885 = CARTESIAN_POINT('Ctrl Pts',(-18.4561308819322,12.6091673891337,122.603098372174)) ;
#33886 = CARTESIAN_POINT('Ctrl Pts',(-18.4561104034437,12.6091659406723,122.603122508455)) ;
#33887 = CARTESIAN_POINT('Ctrl Pts',(-18.4561001742442,12.6091652171341,122.603134565219)) ;
#33888 = CARTESIAN_POINT('Ctrl Pts',(-18.4560797352498,12.6091637713943,122.603158656804)) ;
#33889 = CARTESIAN_POINT('Ctrl Pts',(-18.4560695255338,12.6091630491984,122.603170691529)) ;
#33890 = CARTESIAN_POINT('Ctrl Pts',(-18.4560491242262,12.6091616060528,122.603194740539)) ;
#33891 = CARTESIAN_POINT('Ctrl Pts',(-18.4560389330718,12.6091608851341,122.603206754306)) ;
#33892 = CARTESIAN_POINT('Ctrl Pts',(-18.4560185697823,12.6091594446066,122.60323076034)) ;
#33893 = CARTESIAN_POINT('Ctrl Pts',(-18.4560083971751,12.6091587249643,122.603242753161)) ;
#33894 = CARTESIAN_POINT('Ctrl Pts',(-18.4559880696742,12.6091572868975,122.603266718838)) ;
#33895 = CARTESIAN_POINT('Ctrl Pts',(-18.4559779148352,12.6091565684767,122.603278691627)) ;
#33896 = CARTESIAN_POINT('Ctrl Pts',(-18.4559576228706,12.609155132853,122.603302617234)) ;
#33897 = CARTESIAN_POINT('Ctrl Pts',(-18.4559474854854,12.6091544156318,122.603314570357)) ;
#33898 = CARTESIAN_POINT('Ctrl Pts',(-18.4559272279107,12.6091529823705,122.603338457238)) ;
#33899 = CARTESIAN_POINT('Ctrl Pts',(-18.4559171076743,12.6091522663273,122.60335039105)) ;
#33900 = CARTESIAN_POINT('Ctrl Pts',(-18.4558968825211,12.6091508352896,122.603374241516)) ;
#33901 = CARTESIAN_POINT('Ctrl Pts',(-18.4558867783399,12.6091501203472,122.603386157302)) ;
#33902 = CARTESIAN_POINT('Ctrl Pts',(-18.4525865532531,12.6089166003089,122.60727823614)) ;
#33903 = CARTESIAN_POINT('Ctrl Pts',(-18.4493201556422,12.6086836122397,122.611178441831)) ;
#33904 = CARTESIAN_POINT('Ctrl Pts',(-18.4427860608728,12.6082137208018,122.61907787582)) ;
#33905 = CARTESIAN_POINT('Ctrl Pts',(-18.4395191565058,12.6079768161092,122.623077632859)) ;
#33906 = CARTESIAN_POINT('Ctrl Pts',(-18.4310030379767,12.607353995484,122.633637035963)) ;
#33907 = CARTESIAN_POINT('Ctrl Pts',(-18.4257950153832,12.6069677676902,122.640229544653)) ;
#33908 = CARTESIAN_POINT('Ctrl Pts',(-18.4046821908045,12.6053795869096,122.667516021047)) ;
#33909 = CARTESIAN_POINT('Ctrl Pts',(-18.3893610527256,12.6041734218622,122.688653011638)) ;
#33910 = CARTESIAN_POINT('Ctrl Pts',(-18.3529129052066,12.6011651823234,122.742401438485)) ;
#33911 = CARTESIAN_POINT('Ctrl Pts',(-18.3326229997539,12.5993626216852,122.775547790086)) ;
#33912 = CARTESIAN_POINT('Ctrl Pts',(-18.3013519866437,12.5963632708674,122.832424970965)) ;
#33913 = CARTESIAN_POINT('Ctrl Pts',(-18.2895120049532,12.5951615783711,122.855652172758)) ;
#33914 = CARTESIAN_POINT('Ctrl Pts',(-18.2703914513972,12.593095089258,122.89625208293)) ;
#33915 = CARTESIAN_POINT('Ctrl Pts',(-18.2627613193706,12.5922298594008,122.913450412196)) ;
#33916 = CARTESIAN_POINT('Ctrl Pts',(-18.2499877366282,12.5907044710171,122.944089752005)) ;
#33917 = CARTESIAN_POINT('Ctrl Pts',(-18.2446827567534,12.5900441144143,122.957459646358)) ;
#33918 = CARTESIAN_POINT('Ctrl Pts',(-18.2353291203443,12.5888274830707,122.982274097568)) ;
#33919 = CARTESIAN_POINT('Ctrl Pts',(-18.2312141630492,12.5882711300283,122.99369182571)) ;
#33920 = CARTESIAN_POINT('Ctrl Pts',(-18.2229299205174,12.5871046002402,123.017771759504)) ;
#33921 = CARTESIAN_POINT('Ctrl Pts',(-18.2187955958389,12.5864945832314,123.030444419716)) ;
#33922 = CARTESIAN_POINT('Ctrl Pts',(-18.2098459446753,12.5851071080092,123.059442132694)) ;
#33923 = CARTESIAN_POINT('Ctrl Pts',(-18.2051597522571,12.584330175324,123.075804322379)) ;
#33924 = CARTESIAN_POINT('Ctrl Pts',(-18.1854365614143,12.5808139437484,123.150391114535)) ;
#33925 = CARTESIAN_POINT('Ctrl Pts',(-18.1742789802543,12.5781077443402,123.209558201588)) ;
#33926 = CARTESIAN_POINT('Ctrl Pts',(-18.165247831701,12.5745318941421,123.288253428153)) ;
#33927 = CARTESIAN_POINT('Ctrl Pts',(-18.16350681498,12.5736690269321,123.307255619287)) ;
#33928 = CARTESIAN_POINT('Ctrl Pts',(-18.1615964095027,12.5724013181765,123.335112169401)) ;
#33929 = CARTESIAN_POINT('Ctrl Pts',(-18.1610850246052,12.5719991670501,123.343940371386)) ;
#33930 = CARTESIAN_POINT('Ctrl Pts',(-18.1603375499634,12.5712780638727,123.359748000308)) ;
#33931 = CARTESIAN_POINT('Ctrl Pts',(-18.1600661919462,12.5709594194692,123.366725395004)) ;
#33932 = CARTESIAN_POINT('Ctrl Pts',(-18.1597337725983,12.5704610579918,123.377623699465)) ;
#33933 = CARTESIAN_POINT('Ctrl Pts',(-18.1596326747349,12.5702816908487,123.381543257494)) ;
#33934 = CARTESIAN_POINT('Ctrl Pts',(-18.1594749622181,12.5699391371406,123.389022887593)) ;
#33935 = CARTESIAN_POINT('Ctrl Pts',(-18.1594151137971,12.5697759802535,123.392582854411)) ;
#33936 = CARTESIAN_POINT('Ctrl Pts',(-18.1593127468001,12.5694015118614,123.400747354398)) ;
#33937 = CARTESIAN_POINT('Ctrl Pts',(-18.1592804598205,12.5691901144887,123.405351959994)) ;
#33938 = CARTESIAN_POINT('Ctrl Pts',(-18.1592615668958,12.5686058998872,123.418064265863)) ;
#33939 = CARTESIAN_POINT('Ctrl Pts',(-18.1593283983234,12.56823263766,123.426171796609)) ;
#33940 = CARTESIAN_POINT('Ctrl Pts',(-18.1603410424638,12.5656339807923,123.482511597288)) ;
#33941 = CARTESIAN_POINT('Ctrl Pts',(-18.163999479661,12.5633855848756,123.530653991032)) ;
#33942 = CARTESIAN_POINT('Ctrl Pts',(-18.1725008576885,12.5604202766196,123.593851863788)) ;
#33943 = CARTESIAN_POINT('Ctrl Pts',(-18.1748574905667,12.5596994256428,123.609200632076)) ;
#33944 = CARTESIAN_POINT('Ctrl Pts',(-18.1785726741852,12.5586895171967,123.630717019025)) ;
#33945 = CARTESIAN_POINT('Ctrl Pts',(-18.179692897117,12.5583981840394,123.636924189808)) ;
#33946 = CARTESIAN_POINT('Ctrl Pts',(-18.1829555265562,12.5575847272444,123.654251083616)) ;
#33947 = CARTESIAN_POINT('Ctrl Pts',(-18.1852021322485,12.5570633752392,123.665350590171)) ;
#33948 = CARTESIAN_POINT('Ctrl Pts',(-18.1894573506843,12.5561392430665,123.684996896142)) ;
#33949 = CARTESIAN_POINT('Ctrl Pts',(-18.1914057643807,12.5557361882895,123.693555926983)) ;
#33950 = CARTESIAN_POINT('Ctrl Pts',(-18.1949804564033,12.5550299474947,123.708528437142)) ;
#33951 = CARTESIAN_POINT('Ctrl Pts',(-18.1965678028148,12.5547266290454,123.714950843448)) ;
#33952 = CARTESIAN_POINT('Ctrl Pts',(-18.2064236114327,12.5529027183308,123.753510660049)) ;
#33953 = CARTESIAN_POINT('Ctrl Pts',(-18.2159181742257,12.5513860474914,123.785321078119)) ;
#33954 = CARTESIAN_POINT('Ctrl Pts',(-18.2403913060296,12.5479301803482,123.856800295266)) ;
#33955 = CARTESIAN_POINT('Ctrl Pts',(-18.256144517483,12.5459920929378,123.896160895776)) ;
#33956 = CARTESIAN_POINT('Ctrl Pts',(-18.2864139935278,12.5426776230831,123.961895636907)) ;
#33957 = CARTESIAN_POINT('Ctrl Pts',(-18.2999391767815,12.5413037041773,123.988685414957)) ;
#33958 = CARTESIAN_POINT('Ctrl Pts',(-18.320906782015,12.5393171539216,124.026746593144)) ;
#33959 = CARTESIAN_POINT('Ctrl Pts',(-18.3275883115474,12.5387028867431,124.038425005822)) ;
#33960 = CARTESIAN_POINT('Ctrl Pts',(-18.3556361347127,12.536195800442,124.085662894323)) ;
#33961 = CARTESIAN_POINT('Ctrl Pts',(-18.3785776511792,12.5343059321058,124.120255989233)) ;
#33962 = CARTESIAN_POINT('Ctrl Pts',(-18.4101818565052,12.5318698935927,124.163117873568)) ;
#33963 = CARTESIAN_POINT('Ctrl Pts',(-18.4173007033859,12.5313310269654,124.172492369061)) ;
#33964 = CARTESIAN_POINT('Ctrl Pts',(-18.4313730475718,12.5302840802971,124.19049006801)) ;
#33965 = CARTESIAN_POINT('Ctrl Pts',(-18.4383108759122,12.5297761075774,124.199124157621)) ;
#33966 = CARTESIAN_POINT('Ctrl Pts',(-18.4533915502747,12.5286888169279,124.217389407441)) ;
#33967 = CARTESIAN_POINT('Ctrl Pts',(-18.4615672703638,12.5281094294142,124.226991849584)) ;
#33968 = CARTESIAN_POINT('Ctrl Pts',(-18.4845192563594,12.5265097938742,124.253137051531)) ;
#33969 = CARTESIAN_POINT('Ctrl Pts',(-18.4995926633929,12.5254888445002,124.269412760923)) ;
#33970 = CARTESIAN_POINT('Ctrl Pts',(-18.5195792903258,12.5241721058226,124.289873429297)) ;
#33971 = CARTESIAN_POINT('Ctrl Pts',(-18.5241028558643,12.5238764342211,124.294433437138)) ;
#33972 = CARTESIAN_POINT('Ctrl Pts',(-18.5405636894689,12.5228089620947,124.310773049197)) ;
#33973 = CARTESIAN_POINT('Ctrl Pts',(-18.5527026030115,12.5220375731304,124.322347023014)) ;
#33974 = CARTESIAN_POINT('Ctrl Pts',(-18.5700761768795,12.5209559049256,124.338257046934)) ;
#33975 = CARTESIAN_POINT('Ctrl Pts',(-18.5751188771855,12.5206445121482,124.342799994797)) ;
#33976 = CARTESIAN_POINT('Ctrl Pts',(-18.5843306904589,12.5200803581075,124.35096394748)) ;
#33977 = CARTESIAN_POINT('Ctrl Pts',(-18.5884872763372,12.5198274973713,124.354598827182)) ;
#33978 = CARTESIAN_POINT('Ctrl Pts',(-18.592727570617,12.5195712806371,124.358257611463)) ;
#33979 = CARTESIAN_POINT('Ctrl Pts',(-18.5927873260139,12.5195676703064,124.358309162189)) ;
#33980 = CARTESIAN_POINT('Ctrl Pts',(-18.592910094574,12.5195602535262,124.358415053825)) ;
#33981 = CARTESIAN_POINT('Ctrl Pts',(-18.5929731084797,12.5195564470705,124.358469394273)) ;
#33982 = CARTESIAN_POINT('Ctrl Pts',(-18.5931026313235,12.5195486238256,124.358581066583)) ;
#33983 = CARTESIAN_POINT('Ctrl Pts',(-18.5931691408466,12.5195446070449,124.358638397704)) ;
#33984 = CARTESIAN_POINT('Ctrl Pts',(-18.5974290272613,12.5192873625404,124.362309631823)) ;
#33985 = CARTESIAN_POINT('Ctrl Pts',(-18.6016463663815,12.5190343856636,124.365895652304)) ;
#33986 = CARTESIAN_POINT('Ctrl Pts',(-18.6135298933015,12.5183260590913,124.375865007776)) ;
#33987 = CARTESIAN_POINT('Ctrl Pts',(-18.6212488855807,12.5178711532404,124.382184767406)) ;
#33988 = CARTESIAN_POINT('Ctrl Pts',(-18.6555580665324,12.515869903977,124.409595289082)) ;
#33989 = CARTESIAN_POINT('Ctrl Pts',(-18.6829251267248,12.5143270073461,124.429690436628)) ;
#33990 = CARTESIAN_POINT('Ctrl Pts',(-18.7226073663886,12.5121443943146,124.456412198331)) ;
#33991 = CARTESIAN_POINT('Ctrl Pts',(-18.7342675376822,12.5115094511746,124.463984470882)) ;
#33992 = CARTESIAN_POINT('Ctrl Pts',(-18.7525659017382,12.5105219566522,124.475438291917)) ;
#33993 = CARTESIAN_POINT('Ctrl Pts',(-18.7591177055339,12.510170121583,124.479455762419)) ;
#33994 = CARTESIAN_POINT('Ctrl Pts',(-18.7723131984089,12.5094648408645,124.487380535072)) ;
#33995 = CARTESIAN_POINT('Ctrl Pts',(-18.7789568118582,12.5091114085974,124.491287323184)) ;
#33996 = CARTESIAN_POINT('Ctrl Pts',(-18.7928288430077,12.5083767482813,124.499273066317)) ;
#33997 = CARTESIAN_POINT('Ctrl Pts',(-18.8000626144571,12.5079954898734,124.503341973614)) ;
#33998 = CARTESIAN_POINT('Ctrl Pts',(-18.8178914408251,12.5070601940569,124.513138024327)) ;
#33999 = CARTESIAN_POINT('Ctrl Pts',(-18.8285297648535,12.5065058464089,124.51878465749)) ;
#34000 = CARTESIAN_POINT('Ctrl Pts',(-18.8636555260427,12.504687503885,124.536783051956)) ;
#34001 = CARTESIAN_POINT('Ctrl Pts',(-18.8884680125031,12.5034217123461,124.548482785353)) ;
#34002 = CARTESIAN_POINT('Ctrl Pts',(-18.9170795524814,12.5019848010171,124.560840196506)) ;
#34003 = CARTESIAN_POINT('Ctrl Pts',(-18.9205206079246,12.5018123569094,124.562308104777)) ;
#34004 = CARTESIAN_POINT('Ctrl Pts',(-18.9349243828199,12.5010921092351,124.568376278954)) ;
#34005 = CARTESIAN_POINT('Ctrl Pts',(-18.9459458895193,12.5005447913997,124.572835486676)) ;
#34006 = CARTESIAN_POINT('Ctrl Pts',(-18.9618279327031,12.4997619912918,124.578999051979)) ;
#34007 = CARTESIAN_POINT('Ctrl Pts',(-18.9666379635638,12.4995256926901,124.580831644217)) ;
#34008 = CARTESIAN_POINT('Ctrl Pts',(-18.9765575075591,12.4990399327147,124.584540929438)) ;
#34009 = CARTESIAN_POINT('Ctrl Pts',(-18.9816682291636,12.4987904909948,124.586414060509)) ;
#34010 = CARTESIAN_POINT('Ctrl Pts',(-18.9930455574497,12.4982368851615,124.590499870135)) ;
#34011 = CARTESIAN_POINT('Ctrl Pts',(-18.9993179073584,12.4979328146393,124.592696076545)) ;
#34012 = CARTESIAN_POINT('Ctrl Pts',(-19.0162415559115,12.4971151278367,124.598470649607)) ;
#34013 = CARTESIAN_POINT('Ctrl Pts',(-19.0269240884848,12.496601884366,124.601955595345)) ;
#34014 = CARTESIAN_POINT('Ctrl Pts',(-19.0749501033363,12.494305123,124.616909684163)) ;
#34015 = CARTESIAN_POINT('Ctrl Pts',(-19.1127718729647,12.4925242973508,124.626768496694)) ;
#34016 = CARTESIAN_POINT('Ctrl Pts',(-19.1589462935164,12.490364924625,124.63651963671)) ;
#34017 = CARTESIAN_POINT('Ctrl Pts',(-19.1669157852112,12.4899927817394,124.638121598312)) ;
#34018 = CARTESIAN_POINT('Ctrl Pts',(-19.1862628250434,12.4890904852428,124.641814615874)) ;
#34019 = CARTESIAN_POINT('Ctrl Pts',(-19.1976548641831,12.4885601304442,124.643825688614)) ;
#34020 = CARTESIAN_POINT('Ctrl Pts',(-19.2212395008405,12.487463705819,124.647652384872)) ;
#34021 = CARTESIAN_POINT('Ctrl Pts',(-19.2334343613903,12.4868976313976,124.649446362685)) ;
#34022 = CARTESIAN_POINT('Ctrl Pts',(-19.2663850521429,12.4853700324784,124.653796867446)) ;
#34023 = CARTESIAN_POINT('Ctrl Pts',(-19.2871817664673,12.4844079186929,124.65601338391)) ;
#34024 = CARTESIAN_POINT('Ctrl Pts',(-19.328721165881,12.4824902465458,124.6593891006)) ;
#34025 = CARTESIAN_POINT('Ctrl Pts',(-19.3494568386484,12.4815349858296,124.660555057773)) ;
#34026 = CARTESIAN_POINT('Ctrl Pts',(-19.3773598515602,12.4802533046945,124.661427403579)) ;
#34027 = CARTESIAN_POINT('Ctrl Pts',(-19.3845095588496,12.4799252384598,124.661589527502)) ;
#34028 = CARTESIAN_POINT('Ctrl Pts',(-19.3978908438063,12.4793119461118,124.661778082675)) ;
#34029 = CARTESIAN_POINT('Ctrl Pts',(-19.4041219845727,12.4790266301873,124.661819287687)) ;
#34030 = CARTESIAN_POINT('Ctrl Pts',(-19.4111976064019,12.4787028504042,124.661813168995)) ;
#34031 = CARTESIAN_POINT('Ctrl Pts',(-19.4120420302898,12.4786642129511,124.661811583109)) ;
#34032 = CARTESIAN_POINT('Ctrl Pts',(-19.413700226622,12.4785883465893,124.661806788625)) ;
#34033 = CARTESIAN_POINT('Ctrl Pts',(-19.4145139988482,12.4785511174707,124.661803641011)) ;
#34034 = CARTESIAN_POINT('Ctrl Pts',(-19.4167657493379,12.4784481099324,124.661792732446)) ;
#34035 = CARTESIAN_POINT('Ctrl Pts',(-19.4182037184386,12.4783823375982,124.661783284793)) ;
#34036 = CARTESIAN_POINT('Ctrl Pts',(-19.4312954648374,12.4777835907201,124.661674677872)) ;
#34037 = CARTESIAN_POINT('Ctrl Pts',(-19.4429473575433,12.4772511677643,124.661415025728)) ;
#34038 = CARTESIAN_POINT('Ctrl Pts',(-19.4947838962647,12.4748822775592,124.659534333487)) ;
#34039 = CARTESIAN_POINT('Ctrl Pts',(-19.5348799973414,12.4730484851251,124.656137491742)) ;
#34040 = CARTESIAN_POINT('Ctrl Pts',(-19.5855071166865,12.470710967934,124.649376168536)) ;
#34041 = CARTESIAN_POINT('Ctrl Pts',(-19.5962526625424,12.4702136104057,124.647798292927)) ;
#34042 = CARTESIAN_POINT('Ctrl Pts',(-19.6189267086288,12.4691611438915,124.644166377784)) ;
#34043 = CARTESIAN_POINT('Ctrl Pts',(-19.6308487028074,12.4686059918,124.64207870637)) ;
#34044 = CARTESIAN_POINT('Ctrl Pts',(-19.6570835676851,12.4673800285823,124.637090973545)) ;
#34045 = CARTESIAN_POINT('Ctrl Pts',(-19.6713797464438,12.466709097,124.634112559026)) ;
#34046 = CARTESIAN_POINT('Ctrl Pts',(-19.7036828148005,12.4651861610484,124.626789850256)) ;
#34047 = CARTESIAN_POINT('Ctrl Pts',(-19.7216519587391,12.464334056648,124.62229440476)) ;
#34048 = CARTESIAN_POINT('Ctrl Pts',(-19.75770732225,12.4626143365884,124.612417882623)) ;
#34049 = CARTESIAN_POINT('Ctrl Pts',(-19.775784999438,12.461746942986,124.607023222533)) ;
#34050 = CARTESIAN_POINT('Ctrl Pts',(-19.8008073059715,12.4605398074368,124.598935065143)) ;
#34051 = CARTESIAN_POINT('Ctrl Pts',(-19.8078604000528,12.4601988218568,124.596585542749)) ;
#34052 = CARTESIAN_POINT('Ctrl Pts',(-19.8205519891478,12.4595840127048,124.592231567729)) ;
#34053 = CARTESIAN_POINT('Ctrl Pts',(-19.826197844593,12.45931007174,124.590249278334)) ;
#34054 = CARTESIAN_POINT('Ctrl Pts',(-19.8329781494603,12.4589804475995,124.587813851763)) ;
#34055 = CARTESIAN_POINT('Ctrl Pts',(-19.8341264369782,12.4589246015404,124.587399496702)) ;
#34056 = CARTESIAN_POINT('Ctrl Pts',(-19.8360700331839,12.4588300375781,124.586694937977)) ;
#34057 = CARTESIAN_POINT('Ctrl Pts',(-19.8368656571794,12.4587913161993,124.586405607349)) ;
#34058 = CARTESIAN_POINT('Ctrl Pts',(-19.8476490265035,12.4582663595678,124.582471800163)) ;
#34059 = CARTESIAN_POINT('Ctrl Pts',(-19.8575901888211,12.4577806270418,124.578700843971)) ;
#34060 = CARTESIAN_POINT('Ctrl Pts',(-19.8996954286532,12.4557138785777,124.562111666141)) ;
#34061 = CARTESIAN_POINT('Ctrl Pts',(-19.9313675343519,12.454135113902,124.54808690434)) ;
#34062 = CARTESIAN_POINT('Ctrl Pts',(-19.9742945888471,12.4519458704999,124.526904132726)) ;
#34063 = CARTESIAN_POINT('Ctrl Pts',(-19.9860787812128,12.451339609491,124.520854336017)) ;
#34064 = CARTESIAN_POINT('Ctrl Pts',(-20.0079194981663,12.4502052961452,124.50919941458)) ;
#34065 = CARTESIAN_POINT('Ctrl Pts',(-20.0179990712181,12.4496774589668,124.5036404183)) ;
#34066 = CARTESIAN_POINT('Ctrl Pts',(-20.0392382977169,12.4485555501177,124.491541199843)) ;
#34067 = CARTESIAN_POINT('Ctrl Pts',(-20.050376132214,12.4479614234722,124.484965365511)) ;
#34068 = CARTESIAN_POINT('Ctrl Pts',(-20.0819285385337,12.4462612055226,124.465670125176)) ;
#34069 = CARTESIAN_POINT('Ctrl Pts',(-20.1020807471657,12.4451543168983,124.452532784703)) ;
#34070 = CARTESIAN_POINT('Ctrl Pts',(-20.1354694140684,12.4432847135922,124.429366719317)) ;
#34071 = CARTESIAN_POINT('Ctrl Pts',(-20.1489079573111,12.4425220069596,124.419640807127)) ;
#34072 = CARTESIAN_POINT('Ctrl Pts',(-20.1674306744609,12.4414569082213,124.40566524036)) ;
#34073 = CARTESIAN_POINT('Ctrl Pts',(-20.1726806502959,12.4411534284501,124.401638275377)) ;
#34074 = CARTESIAN_POINT('Ctrl Pts',(-20.1821686190583,12.440602129374,124.394240191788)) ;
#34075 = CARTESIAN_POINT('Ctrl Pts',(-20.1864171508693,12.4403542164487,124.390882853714)) ;
#34076 = CARTESIAN_POINT('Ctrl Pts',(-20.1947162523244,12.4398679201218,124.384236558636)) ;
#34077 = CARTESIAN_POINT('Ctrl Pts',(-20.1987682996674,12.4396295378058,124.380949645044)) ;
#34078 = CARTESIAN_POINT('Ctrl Pts',(-20.2095128408346,12.4389947417754,124.372121850109)) ;
#34079 = CARTESIAN_POINT('Ctrl Pts',(-20.216168347234,12.4385986993679,124.36653639678)) ;
#34080 = CARTESIAN_POINT('Ctrl Pts',(-20.2413279731527,12.4370894775508,124.344970835657)) ;
#34081 = CARTESIAN_POINT('Ctrl Pts',(-20.2594200714513,12.4359787896424,124.328518466747)) ;
#34082 = CARTESIAN_POINT('Ctrl Pts',(-20.2943475365323,12.4337713443,124.294832691494)) ;
#34083 = CARTESIAN_POINT('Ctrl Pts',(-20.3111904638408,12.432675097936,124.277622169044)) ;
#34084 = CARTESIAN_POINT('Ctrl Pts',(-20.333631552458,12.4311643786801,124.253325409506)) ;
#34085 = CARTESIAN_POINT('Ctrl Pts',(-20.3396657453099,12.4307529240648,124.2466490199)) ;
#34086 = CARTESIAN_POINT('Ctrl Pts',(-20.3500692061044,12.4300340589982,124.234885455946)) ;
#34087 = CARTESIAN_POINT('Ctrl Pts',(-20.3544706145966,12.4297268749925,124.229827191592)) ;
#34088 = CARTESIAN_POINT('Ctrl Pts',(-20.363098406707,12.4291185414802,124.219749198019)) ;
#34089 = CARTESIAN_POINT('Ctrl Pts',(-20.3673263863814,12.4288174128017,124.214731112212)) ;
#34090 = CARTESIAN_POINT('Ctrl Pts',(-20.3765593598748,12.4281530286161,124.203595955381)) ;
#34091 = CARTESIAN_POINT('Ctrl Pts',(-20.3815462429687,12.4277896750253,124.197464237233)) ;
#34092 = CARTESIAN_POINT('Ctrl Pts',(-20.3941793850878,12.4268574237199,124.18162640335)) ;
#34093 = CARTESIAN_POINT('Ctrl Pts',(-20.4017404800292,12.4262880910952,124.171853475638)) ;
#34094 = CARTESIAN_POINT('Ctrl Pts',(-20.4274939936011,12.4243085935446,124.137526595876)) ;
#34095 = CARTESIAN_POINT('Ctrl Pts',(-20.4449300513644,12.4228956682421,124.112418870795)) ;
#34096 = CARTESIAN_POINT('Ctrl Pts',(-20.469207392235,12.4208201469499,124.074570018575)) ;
#34097 = CARTESIAN_POINT('Ctrl Pts',(-20.4767761285141,12.4201559539261,124.06230881979)) ;
#34098 = CARTESIAN_POINT('Ctrl Pts',(-20.4887980366023,12.4190728407009,124.042058462036)) ;
#34099 = CARTESIAN_POINT('Ctrl Pts',(-20.4933784570965,12.4186529411241,124.03414649349)) ;
#34100 = CARTESIAN_POINT('Ctrl Pts',(-20.502492205297,12.4178020039793,124.017997899938)) ;
#34101 = CARTESIAN_POINT('Ctrl Pts',(-20.5070202293992,12.4173710150697,124.009758946748)) ;
#34102 = CARTESIAN_POINT('Ctrl Pts',(-20.5177380695046,12.4163299815716,123.989725179554)) ;
#34103 = CARTESIAN_POINT('Ctrl Pts',(-20.5238331377591,12.4157202482998,123.97788097832)) ;
#34104 = CARTESIAN_POINT('Ctrl Pts',(-20.549562384813,12.4130639262777,123.925855502576)) ;
#34105 = CARTESIAN_POINT('Ctrl Pts',(-20.5672215044172,12.4110196529471,123.884734438593)) ;
#34106 = CARTESIAN_POINT('Ctrl Pts',(-20.5912787219728,12.4078209736192,123.819231482994)) ;
#34107 = CARTESIAN_POINT('Ctrl Pts',(-20.5992090760481,12.4066713963321,123.795452677033)) ;
#34108 = CARTESIAN_POINT('Ctrl Pts',(-20.6134828954529,12.4043947279938,123.747938523882)) ;
#34109 = CARTESIAN_POINT('Ctrl Pts',(-20.6198522642245,12.4032681519348,123.724222369372)) ;
#34110 = CARTESIAN_POINT('Ctrl Pts',(-20.6278648432713,12.4016775444763,123.690445560328)) ;
#34111 = CARTESIAN_POINT('Ctrl Pts',(-20.630089924705,12.4012122315028,123.680528817956)) ;
#34112 = CARTESIAN_POINT('Ctrl Pts',(-20.6345985502187,12.4002161936719,123.659221633624)) ;
#34113 = CARTESIAN_POINT('Ctrl Pts',(-20.6368447426512,12.3996857949994,123.647824269576)) ;
#34114 = CARTESIAN_POINT('Ctrl Pts',(-20.6422802606537,12.398306040833,123.618063151031)) ;
#34115 = CARTESIAN_POINT('Ctrl Pts',(-20.6452183096808,12.3974576105,123.599656468766)) ;
#34116 = CARTESIAN_POINT('Ctrl Pts',(-20.6519275933222,12.3952029601296,123.550598591595)) ;
#34117 = CARTESIAN_POINT('Ctrl Pts',(-20.6549765077723,12.3937969104405,123.51986182271)) ;
#34118 = CARTESIAN_POINT('Ctrl Pts',(-20.6575153890148,12.3919190119312,123.478847204014)) ;
#34119 = CARTESIAN_POINT('Ctrl Pts',(-20.6580215512615,12.3914517052291,123.468643206792)) ;
#34120 = CARTESIAN_POINT('Ctrl Pts',(-20.6586924466314,12.3906279597365,123.450667248269)) ;
#34121 = CARTESIAN_POINT('Ctrl Pts',(-20.6589098750464,12.3902717591962,123.442897799713)) ;
#34122 = CARTESIAN_POINT('Ctrl Pts',(-20.659207098202,12.389540769035,123.426963657059)) ;
#34123 = CARTESIAN_POINT('Ctrl Pts',(-20.6592793849912,12.3891659660142,123.418799189831)) ;
#34124 = CARTESIAN_POINT('Ctrl Pts',(-20.6592617171154,12.3883059014497,123.400079272028)) ;
#34125 = CARTESIAN_POINT('Ctrl Pts',(-20.6591180570055,12.3878204651731,123.38952449959)) ;
#34126 = CARTESIAN_POINT('Ctrl Pts',(-20.6583399274576,12.3864571946517,123.359917895475)) ;
#34127 = CARTESIAN_POINT('Ctrl Pts',(-20.6574033270884,12.3855785366258,123.340876944267)) ;
#34128 = CARTESIAN_POINT('Ctrl Pts',(-20.6539585003184,12.3833707138074,123.293129342754)) ;
#34129 = CARTESIAN_POINT('Ctrl Pts',(-20.6508924846443,12.382041487259,123.264473947319)) ;
#34130 = CARTESIAN_POINT('Ctrl Pts',(-20.6459225966224,12.3804176361351,123.229500566442)) ;
#34131 = CARTESIAN_POINT('Ctrl Pts',(-20.6449556855264,12.3801184788421,123.223058309291)) ;
#34132 = CARTESIAN_POINT('Ctrl Pts',(-20.6430293169588,12.379552562887,123.210873175451)) ;
#34133 = CARTESIAN_POINT('Ctrl Pts',(-20.642080010145,12.3792857265701,123.205128882462)) ;
#34134 = CARTESIAN_POINT('Ctrl Pts',(-20.6398694252935,12.378689954479,123.192309932808)) ;
#34135 = CARTESIAN_POINT('Ctrl Pts',(-20.6385872017436,12.3783611252823,123.185239094201)) ;
#34136 = CARTESIAN_POINT('Ctrl Pts',(-20.6322424548513,12.3768086416373,123.151891430073)) ;
#34137 = CARTESIAN_POINT('Ctrl Pts',(-20.6263979526738,12.3755875762307,123.125770518323)) ;
#34138 = CARTESIAN_POINT('Ctrl Pts',(-20.6148857093288,12.3734802186777,123.081101018021)) ;
#34139 = CARTESIAN_POINT('Ctrl Pts',(-20.6096165317935,12.372594938087,123.062459626244)) ;
#34140 = CARTESIAN_POINT('Ctrl Pts',(-20.6001020320911,12.3711151039714,123.031561316766)) ;
#34141 = CARTESIAN_POINT('Ctrl Pts',(-20.5960984489603,12.3705218271716,123.019243959999)) ;
#34142 = CARTESIAN_POINT('Ctrl Pts',(-20.5919008645526,12.3699275081133,123.006981651862)) ;
#34143 = CARTESIAN_POINT('Ctrl Pts',(-20.5919008187226,12.3097986802463,123.006981518046)) ;
#34144 = CARTESIAN_POINT('Ctrl Pts',(-20.5959679259066,12.3103772675894,123.018862784893)) ;
#34145 = CARTESIAN_POINT('Ctrl Pts',(-20.5998545754055,12.3109562954671,123.030800851875)) ;
#34146 = CARTESIAN_POINT('Ctrl Pts',(-20.6035607346876,12.31153530454,123.042795421432)) ;
#34147 = CARTESIAN_POINT('Ctrl Pts',(-20.6248655183692,12.3148637267982,123.111745968429)) ;
#34148 = CARTESIAN_POINT('Ctrl Pts',(-20.640159292875,12.3181590011121,123.182412191089)) ;
#34149 = CARTESIAN_POINT('Ctrl Pts',(-20.649270492558,12.3214523073791,123.254003328633)) ;
#34150 = CARTESIAN_POINT('Ctrl Pts',(-20.6584395622931,12.3247665311775,123.326049179388)) ;
#34151 = CARTESIAN_POINT('Ctrl Pts',(-20.6613122235796,12.3281113715718,123.398756812874)) ;
#34152 = CARTESIAN_POINT('Ctrl Pts',(-20.6578559614911,12.331432491669,123.471301175167)) ;
#34153 = CARTESIAN_POINT('Ctrl Pts',(-20.6543934482099,12.3347596185333,123.543976745329)) ;
#34154 = CARTESIAN_POINT('Ctrl Pts',(-20.6445924883426,12.3380646087419,123.616209428573)) ;
#34155 = CARTESIAN_POINT('Ctrl Pts',(-20.6285649359542,12.3414306615,123.687178328985)) ;
#34156 = CARTESIAN_POINT('Ctrl Pts',(-20.6126520997966,12.3447726219402,123.757639273811)) ;
#34157 = CARTESIAN_POINT('Ctrl Pts',(-20.590661759836,12.3480897793102,123.826588099236)) ;
#34158 = CARTESIAN_POINT('Ctrl Pts',(-20.5628388308981,12.351357610961,123.893253990093)) ;
#34159 = CARTESIAN_POINT('Ctrl Pts',(-20.5531745685128,12.3524926885286,123.916410310652)) ;
#34160 = CARTESIAN_POINT('Ctrl Pts',(-20.5428153628591,12.3536262784784,123.939270123424)) ;
#34161 = CARTESIAN_POINT('Ctrl Pts',(-20.5317752294988,12.3547689257512,123.961802575126)) ;
#34162 = CARTESIAN_POINT('Ctrl Pts',(-20.5108163442102,12.3569381579818,124.0045787858)) ;
#34163 = CARTESIAN_POINT('Ctrl Pts',(-20.4874304463061,12.3591457818808,124.0461201067)) ;
#34164 = CARTESIAN_POINT('Ctrl Pts',(-20.4617310904093,12.3613560336666,124.086225487286)) ;
#34165 = CARTESIAN_POINT('Ctrl Pts',(-20.4228614531263,12.364698984578,124.146883878986)) ;
#34166 = CARTESIAN_POINT('Ctrl Pts',(-20.3788207145505,12.3679748327242,124.204068391805)) ;
#34167 = CARTESIAN_POINT('Ctrl Pts',(-20.330098410005,12.3712568822117,124.257142206669)) ;
#34168 = CARTESIAN_POINT('Ctrl Pts',(-20.2811120419599,12.37455671964,124.310503669202)) ;
#34169 = CARTESIAN_POINT('Ctrl Pts',(-20.227580251143,12.3779005627734,124.359505786526)) ;
#34170 = CARTESIAN_POINT('Ctrl Pts',(-20.1701073888366,12.3812115960284,124.403595527009)) ;
#34171 = CARTESIAN_POINT('Ctrl Pts',(-20.1123795154289,12.3845373205691,124.447880896747)) ;
#34172 = CARTESIAN_POINT('Ctrl Pts',(-20.0508971122197,12.3878420276153,124.487040359335)) ;
#34173 = CARTESIAN_POINT('Ctrl Pts',(-19.9863588595697,12.3912102426386,124.520629512979)) ;
#34174 = CARTESIAN_POINT('Ctrl Pts',(-19.9308684806042,12.3941062542349,124.549509669914)) ;
#34175 = CARTESIAN_POINT('Ctrl Pts',(-19.8732884005457,12.3969908898565,124.574183755512)) ;
#34176 = CARTESIAN_POINT('Ctrl Pts',(-19.814101322745,12.3998259425229,124.594444237049)) ;
#34177 = CARTESIAN_POINT('Ctrl Pts',(-19.8049052026207,12.4002664353779,124.597592184691)) ;
#34178 = CARTESIAN_POINT('Ctrl Pts',(-19.7956726543642,12.4007060969951,124.600632769874)) ;
#34179 = CARTESIAN_POINT('Ctrl Pts',(-19.786405553344,12.4011453145424,124.603565372853)) ;
#34180 = CARTESIAN_POINT('Ctrl Pts',(-19.7170359751187,12.4044331103635,124.625517591919)) ;
#34181 = CARTESIAN_POINT('Ctrl Pts',(-19.645888839699,12.4077540678437,124.641369545238)) ;
#34182 = CARTESIAN_POINT('Ctrl Pts',(-19.5737661106502,12.4111439811015,124.650943805026)) ;
#34183 = CARTESIAN_POINT('Ctrl Pts',(-19.50230985836,12.4145025686118,124.660429590325)) ;
#34184 = CARTESIAN_POINT('Ctrl Pts',(-19.430168452585,12.4177998987068,124.663716935233)) ;
#34185 = CARTESIAN_POINT('Ctrl Pts',(-19.3581406945466,12.4210504446412,124.66076815496)) ;
#34186 = CARTESIAN_POINT('Ctrl Pts',(-19.2854416744532,12.4243312840098,124.657791893556)) ;
#34187 = CARTESIAN_POINT('Ctrl Pts',(-19.2131478831709,12.4276641706043,124.648474605693)) ;
#34188 = CARTESIAN_POINT('Ctrl Pts',(-19.1420743743969,12.4310490229632,124.632922593895)) ;
#34189 = CARTESIAN_POINT('Ctrl Pts',(-19.071424242274,12.4344137121492,124.617463223629)) ;
#34190 = CARTESIAN_POINT('Ctrl Pts',(-19.0022480648928,12.4377416309172,124.595901484794)) ;
#34191 = CARTESIAN_POINT('Ctrl Pts',(-18.9353230016292,12.4410246690359,124.568478588955)) ;
#34192 = CARTESIAN_POINT('Ctrl Pts',(-18.9096039882164,12.4422863264374,124.557940088258)) ;
#34193 = CARTESIAN_POINT('Ctrl Pts',(-18.8842435556656,12.4435427967642,124.546546678268)) ;
#34194 = CARTESIAN_POINT('Ctrl Pts',(-18.8592840273916,12.4448018250339,124.53431736011)) ;
#34195 = CARTESIAN_POINT('Ctrl Pts',(-18.75389161528,12.4501181124575,124.482678670265)) ;
#34196 = CARTESIAN_POINT('Ctrl Pts',(-18.6563002355626,12.4555339951191,124.416456661723)) ;
#34197 = CARTESIAN_POINT('Ctrl Pts',(-18.5693811238693,12.4609547040084,124.33760209597)) ;
#34198 = CARTESIAN_POINT('Ctrl Pts',(-18.5155204329295,12.4643137250622,124.288738718141)) ;
#34199 = CARTESIAN_POINT('Ctrl Pts',(-18.4660255868903,12.4676210838886,124.235267338101)) ;
#34200 = CARTESIAN_POINT('Ctrl Pts',(-18.421460314933,12.4709151894271,124.177795834203)) ;
#34201 = CARTESIAN_POINT('Ctrl Pts',(-18.3769039711297,12.4742086350285,124.120335844079)) ;
#34202 = CARTESIAN_POINT('Ctrl Pts',(-18.3374488791071,12.477526026371,124.059101803663)) ;
#34203 = CARTESIAN_POINT('Ctrl Pts',(-18.3035398956969,12.480906710666,123.994786056946)) ;
#34204 = CARTESIAN_POINT('Ctrl Pts',(-18.273330930655,12.4839185076417,123.937488198125)) ;
#34205 = CARTESIAN_POINT('Ctrl Pts',(-18.2476214510531,12.486897790467,123.877929793882)) ;
#34206 = CARTESIAN_POINT('Ctrl Pts',(-18.2266423654683,12.4898239518789,123.816643453356)) ;
#34207 = CARTESIAN_POINT('Ctrl Pts',(-18.2243056994885,12.4901498698888,123.80981733568)) ;
#34208 = CARTESIAN_POINT('Ctrl Pts',(-18.2220278588499,12.4904755343012,123.802970140349)) ;
#34209 = CARTESIAN_POINT('Ctrl Pts',(-18.2198098607987,12.4908011212469,123.796104957352)) ;
#34210 = CARTESIAN_POINT('Ctrl Pts',(-18.1974413096866,12.4940846715785,123.72686946064)) ;
#34211 = CARTESIAN_POINT('Ctrl Pts',(-18.1811618838124,12.4974253874866,123.655819011934)) ;
#34212 = CARTESIAN_POINT('Ctrl Pts',(-18.1711542091949,12.5007987881958,123.58375549571)) ;
#34213 = CARTESIAN_POINT('Ctrl Pts',(-18.1612141385254,12.5041494008733,123.512178783703)) ;
#34214 = CARTESIAN_POINT('Ctrl Pts',(-18.1574994841532,12.5074328201644,123.439874501978)) ;
#34215 = CARTESIAN_POINT('Ctrl Pts',(-18.1600525528208,12.5107289079967,123.367653486248)) ;
#34216 = CARTESIAN_POINT('Ctrl Pts',(-18.1626092701643,12.5140297063784,123.295329257047)) ;
#34217 = CARTESIAN_POINT('Ctrl Pts',(-18.171441973291,12.5173692988662,123.223364167744)) ;
#34218 = CARTESIAN_POINT('Ctrl Pts',(-18.1864509887407,12.5206842314647,123.152568927952)) ;
#34219 = CARTESIAN_POINT('Ctrl Pts',(-18.2077946755634,12.5253982570752,123.051894008153)) ;
#34220 = CARTESIAN_POINT('Ctrl Pts',(-18.2414891520986,12.5300422781028,122.954240933681)) ;
#34221 = CARTESIAN_POINT('Ctrl Pts',(-18.2867692424076,12.5347791480646,122.861826158003)) ;
#34222 = CARTESIAN_POINT('Ctrl Pts',(-18.3053018325031,12.5367178913122,122.824001914616)) ;
#34223 = CARTESIAN_POINT('Ctrl Pts',(-18.3257344508473,12.538661680911,122.787138435358)) ;
#34224 = CARTESIAN_POINT('Ctrl Pts',(-18.347988906045,12.5405951669528,122.751376864801)) ;
#34225 = CARTESIAN_POINT('Ctrl Pts',(-18.4246887379185,12.5472589137405,122.62812484965)) ;
#34226 = CARTESIAN_POINT('Ctrl Pts',(-18.5222717230523,12.5538432931049,122.519175649303)) ;
#34227 = CARTESIAN_POINT('Ctrl Pts',(-18.6363622964908,12.5605176564878,122.429414129616)) ;
#34228 = CARTESIAN_POINT('Ctrl Pts',(-18.6934296541356,12.5638561293409,122.384516005324)) ;
#34229 = CARTESIAN_POINT('Ctrl Pts',(-18.7543012385188,12.5671710938438,122.34467533864)) ;
#34230 = CARTESIAN_POINT('Ctrl Pts',(-18.8182864537173,12.5704815138147,122.310344527998)) ;
#34231 = CARTESIAN_POINT('Ctrl Pts',(-18.878035625681,12.5735727724985,122.278286536127)) ;
#34232 = CARTESIAN_POINT('Ctrl Pts',(-18.9402928786006,12.5766714230685,122.251143940954)) ;
#34233 = CARTESIAN_POINT('Ctrl Pts',(-19.0044431491614,12.5797954008838,122.229184496079)) ;
#34234 = CARTESIAN_POINT('Ctrl Pts',(-19.0091190551512,12.5800231072746,122.227583874618)) ;
#34235 = CARTESIAN_POINT('Ctrl Pts',(-19.0138047230683,12.580250794863,122.226010895838)) ;
#34236 = CARTESIAN_POINT('Ctrl Pts',(-19.0184991675638,12.5804783681921,122.22446588819)) ;
#34237 = CARTESIAN_POINT('Ctrl Pts',(-19.087094062903,12.5838036537943,122.201890344265)) ;
#34238 = CARTESIAN_POINT('Ctrl Pts',(-19.157516417056,12.5870877342977,122.185301422084)) ;
#34239 = CARTESIAN_POINT('Ctrl Pts',(-19.228976203807,12.590400895558,122.174885370676)) ;
#34240 = CARTESIAN_POINT('Ctrl Pts',(-19.3005480738815,12.593719253449,122.164452981889)) ;
#34241 = CARTESIAN_POINT('Ctrl Pts',(-19.3728909905207,12.5970766281283,122.160252175256)) ;
#34242 = CARTESIAN_POINT('Ctrl Pts',(-19.4451903276682,12.6003730862129,122.162330516823)) ;
#34243 = CARTESIAN_POINT('Ctrl Pts',(-19.5909202431352,12.6070175808509,122.166519719005)) ;
#34244 = CARTESIAN_POINT('Ctrl Pts',(-19.7347890275704,12.6135840949886,122.196169604076)) ;
#34245 = CARTESIAN_POINT('Ctrl Pts',(-19.8702966648422,12.6203324938027,122.249938092582)) ;
#34246 = CARTESIAN_POINT('Ctrl Pts',(-19.90045071297,12.6218341917639,122.261903009267)) ;
#34247 = CARTESIAN_POINT('Ctrl Pts',(-19.9301277965717,12.6233279003994,122.275037368455)) ;
#34248 = CARTESIAN_POINT('Ctrl Pts',(-19.9592604445148,12.6248187332792,122.289311373019)) ;
#34249 = CARTESIAN_POINT('Ctrl Pts',(-20.0602104252377,12.629984743275,122.338773422894)) ;
#34250 = CARTESIAN_POINT('Ctrl Pts',(-20.1540280917424,12.6351103129767,122.401627929583)) ;
#34251 = CARTESIAN_POINT('Ctrl Pts',(-20.2381746311039,12.6402255782778,122.476175109484)) ;
#34252 = CARTESIAN_POINT('Ctrl Pts',(-20.3467958775309,12.6468286601993,122.572404944483)) ;
#34253 = CARTESIAN_POINT('Ctrl Pts',(-20.4378292876924,12.6534583240344,122.686812124415)) ;
#34254 = CARTESIAN_POINT('Ctrl Pts',(-20.5071984569157,12.6601281682878,122.814271051483)) ;
#34255 = CARTESIAN_POINT('Ctrl Pts',(-20.5408008134123,12.6633590342025,122.876012028835)) ;
#34256 = CARTESIAN_POINT('Ctrl Pts',(-20.5691355300788,12.6665486843384,122.940477674066)) ;
#34257 = CARTESIAN_POINT('Ctrl Pts',(-20.5919010929731,12.6697683433189,123.006982319198)) ;
#34258 = CARTESIAN_POINT('Ctrl Pts',(-20.5445170967909,10.1799890803629,123.023196933748)) ;
#34259 = CARTESIAN_POINT('Ctrl Pts',(-20.8283303707622,9.99999999995305,122.926041870788)) ;
#34260 = CARTESIAN_POINT('Ctrl Pts',(-20.5894888412031,10.186615931181,123.154521494311)) ;
#34261 = CARTESIAN_POINT('Ctrl Pts',(-20.8845408160738,10.0066268507712,123.090165629839)) ;
#34262 = CARTESIAN_POINT('Ctrl Pts',(-20.6334208464893,10.199846557662,123.432353270138)) ;
#34263 = CARTESIAN_POINT('Ctrl Pts',(-20.9394617691535,10.0198574772522,123.437507823533)) ;
#34264 = CARTESIAN_POINT('Ctrl Pts',(-20.5528814488852,10.2198221789206,123.849407494597)) ;
#34265 = CARTESIAN_POINT('Ctrl Pts',(-20.8387858493865,10.0398330985108,123.958797508314)) ;
#34266 = CARTESIAN_POINT('Ctrl Pts',(-20.3351890798294,10.2397395138226,124.21264452173)) ;
#34267 = CARTESIAN_POINT('Ctrl Pts',(-20.5666727976471,10.0597504334128,124.41284983941)) ;
#34268 = CARTESIAN_POINT('Ctrl Pts',(-20.0078940908122,10.2596127905386,124.479989674566)) ;
#34269 = CARTESIAN_POINT('Ctrl Pts',(-20.157556275823,10.0796237101287,124.747029739255)) ;
#34270 = CARTESIAN_POINT('Ctrl Pts',(-19.6059540280892,10.2796372807025,124.620350189469)) ;
#34271 = CARTESIAN_POINT('Ctrl Pts',(-19.6551315118272,10.0996482002927,124.922482691242)) ;
#34272 = CARTESIAN_POINT('Ctrl Pts',(-19.1834791470516,10.2995051218533,124.615075219233)) ;
#34273 = CARTESIAN_POINT('Ctrl Pts',(-19.1270395365889,10.1195160414434,124.915890798242)) ;
#34274 = CARTESIAN_POINT('Ctrl Pts',(-18.7864839057826,10.3194507727328,124.466021113069)) ;
#34275 = CARTESIAN_POINT('Ctrl Pts',(-18.6307952227997,10.139461692323,124.729575809499)) ;
#34276 = CARTESIAN_POINT('Ctrl Pts',(-18.4649063701951,10.3393561733498,124.190844404071)) ;
#34277 = CARTESIAN_POINT('Ctrl Pts',(-18.228822407821,10.15936709294,124.385607616928)) ;
#34278 = CARTESIAN_POINT('Ctrl Pts',(-18.2561330011468,10.3592304011661,123.82343533093)) ;
#34279 = CARTESIAN_POINT('Ctrl Pts',(-17.9678535156375,10.1792413207563,123.926349000821)) ;
#34280 = CARTESIAN_POINT('Ctrl Pts',(-18.1848402354332,10.3792161920437,123.40449567957)) ;
#34281 = CARTESIAN_POINT('Ctrl Pts',(-17.8787342095081,10.1992271116339,123.402675114316)) ;
#34282 = CARTESIAN_POINT('Ctrl Pts',(-18.2606699010585,10.3991104347035,122.98837126667)) ;
#34283 = CARTESIAN_POINT('Ctrl Pts',(-17.9735177003611,10.2191213542937,122.882519964991)) ;
#34284 = CARTESIAN_POINT('Ctrl Pts',(-18.4728612596363,10.4189891507756,122.622758653604)) ;
#34285 = CARTESIAN_POINT('Ctrl Pts',(-18.2387528910192,10.2390000703658,122.425502981396)) ;
#34286 = CARTESIAN_POINT('Ctrl Pts',(-18.7999520439114,10.4390286006202,122.349765919269)) ;
#34287 = CARTESIAN_POINT('Ctrl Pts',(-18.6476140899653,10.2590395202104,122.084258749039)) ;
#34288 = CARTESIAN_POINT('Ctrl Pts',(-19.1972003355021,10.458891762158,122.205978453982)) ;
#34289 = CARTESIAN_POINT('Ctrl Pts',(-19.1441721120908,10.2789026817482,121.904520881741)) ;
#34290 = CARTESIAN_POINT('Ctrl Pts',(-19.6218813508038,10.4788711301723,122.206142579944)) ;
#34291 = CARTESIAN_POINT('Ctrl Pts',(-19.675023206704,10.2988820497624,121.904721686649)) ;
#34292 = CARTESIAN_POINT('Ctrl Pts',(-20.0180063674985,10.4986817106951,122.349636080019)) ;
#34293 = CARTESIAN_POINT('Ctrl Pts',(-20.1701799765576,10.3186926302853,122.084083785717)) ;
#34294 = CARTESIAN_POINT('Ctrl Pts',(-20.3444408594761,10.5186626389807,122.621421727286)) ;
#34295 = CARTESIAN_POINT('Ctrl Pts',(-20.578226084232,10.3386735585708,122.423812224516)) ;
#34296 = CARTESIAN_POINT('Ctrl Pts',(-20.5574140360782,10.5385553108501,122.986919561501)) ;
#34297 = CARTESIAN_POINT('Ctrl Pts',(-20.8444469589225,10.3585662304403,122.880680954071)) ;
#34298 = CARTESIAN_POINT('Ctrl Pts',(-20.6337210602673,10.5584816411372,123.403677138751)) ;
#34299 = CARTESIAN_POINT('Ctrl Pts',(-20.9398341758615,10.3784925607274,123.40162915944)) ;
#34300 = CARTESIAN_POINT('Ctrl Pts',(-20.5626906544988,10.5784521952295,123.822322212015)) ;
#34301 = CARTESIAN_POINT('Ctrl Pts',(-20.8510572231467,10.3984631148197,123.924927290917)) ;
#34302 = CARTESIAN_POINT('Ctrl Pts',(-20.3894921739839,10.5949840343171,124.128174611121)) ;
#34303 = CARTESIAN_POINT('Ctrl Pts',(-20.6345446352502,10.4149949539073,124.307272603932)) ;
#34304 = CARTESIAN_POINT('Ctrl Pts',(-20.1931290904253,10.6083237731447,124.328455789616)) ;
#34305 = CARTESIAN_POINT('Ctrl Pts',(-20.3891097553324,10.4283346927348,124.557601822234)) ;
#34306 = CARTESIAN_POINT('Ctrl Pts',(-20.0213870270135,10.6183560153633,124.45086066554)) ;
#34307 = CARTESIAN_POINT('Ctrl Pts',(-20.1744300570666,10.4383669349535,124.710615084661)) ;
#34308 = CARTESIAN_POINT('Ctrl Pts',(-19.8344327780229,10.6282137160067,124.54030505442)) ;
#34309 = CARTESIAN_POINT('Ctrl Pts',(-19.9407404802696,10.4482246355969,124.822421617956)) ;
#34310 = CARTESIAN_POINT('Ctrl Pts',(-19.6321963819504,10.638205580646,124.597047913329)) ;
#34311 = CARTESIAN_POINT('Ctrl Pts',(-19.6879423525452,10.4582165002362,124.893352629504)) ;
#34312 = CARTESIAN_POINT('Ctrl Pts',(-19.424609722569,10.6481281304061,124.617626313307)) ;
#34313 = CARTESIAN_POINT('Ctrl Pts',(-19.4284710425149,10.4681390499963,124.9190803154)) ;
#34314 = CARTESIAN_POINT('Ctrl Pts',(-19.1462074516632,10.6614059038996,124.597234583046)) ;
#34315 = CARTESIAN_POINT('Ctrl Pts',(-19.0804105140679,10.4814168234897,124.893583985702)) ;
#34316 = CARTESIAN_POINT('Ctrl Pts',(-18.8783190629616,10.6747532428402,124.503658368855)) ;
#34317 = CARTESIAN_POINT('Ctrl Pts',(-18.7455859092542,10.4947641624304,124.776616835827)) ;
#34318 = CARTESIAN_POINT('Ctrl Pts',(-18.6486031256444,10.6879604746334,124.347593152274)) ;
#34319 = CARTESIAN_POINT('Ctrl Pts',(-18.4584522381977,10.5079713942236,124.581549246975)) ;
#34320 = CARTESIAN_POINT('Ctrl Pts',(-18.4978121198163,10.6979475907231,124.201545393376)) ;
#34321 = CARTESIAN_POINT('Ctrl Pts',(-18.2699588379995,10.5179585103133,124.398989341585)) ;
#34322 = CARTESIAN_POINT('Ctrl Pts',(-18.3749610360081,10.7078984963028,124.032167626381)) ;
#34323 = CARTESIAN_POINT('Ctrl Pts',(-18.1163933969042,10.527909415893,124.187269395878)) ;
#34324 = CARTESIAN_POINT('Ctrl Pts',(-18.2826761324805,10.7179535983103,123.842018510299)) ;
#34325 = CARTESIAN_POINT('Ctrl Pts',(-18.0010345813188,10.5379645179005,123.949583784576)) ;
#34326 = CARTESIAN_POINT('Ctrl Pts',(-18.2257894495901,10.7277752716314,123.643501818388)) ;
#34327 = CARTESIAN_POINT('Ctrl Pts',(-17.9299233420751,10.5477861912216,123.701439503976)) ;
#34328 = CARTESIAN_POINT('Ctrl Pts',(-18.2033755349775,10.7378337427063,123.433255143292)) ;
#34329 = CARTESIAN_POINT('Ctrl Pts',(-17.901904058555,10.5578446622965,123.438628667081)) ;
#34330 = CARTESIAN_POINT('Ctrl Pts',(-18.2179011335089,10.7477583538828,123.225094347349)) ;
#34331 = CARTESIAN_POINT('Ctrl Pts',(-17.9200547530426,10.567769273473,123.1784374172)) ;
#34332 = CARTESIAN_POINT('Ctrl Pts',(-18.2846726130989,10.7610356927832,122.954084571752)) ;
#34333 = CARTESIAN_POINT('Ctrl Pts',(-18.0035329036583,10.5810466123734,122.839624585017)) ;
#34334 = CARTESIAN_POINT('Ctrl Pts',(-18.4211117191118,10.7743345720208,122.706442666777)) ;
#34335 = CARTESIAN_POINT('Ctrl Pts',(-18.1740788904205,10.5943454916109,122.530096455794)) ;
#34336 = CARTESIAN_POINT('Ctrl Pts',(-18.6137282560997,10.7875734441915,122.505480302123)) ;
#34337 = CARTESIAN_POINT('Ctrl Pts',(-18.414829088899,10.6075843637816,122.278909287776)) ;
#34338 = CARTESIAN_POINT('Ctrl Pts',(-18.7832424185157,10.7975800623281,122.380894161506)) ;
#34339 = CARTESIAN_POINT('Ctrl Pts',(-18.6267237903737,10.6175909819183,122.123170592557)) ;
#34340 = CARTESIAN_POINT('Ctrl Pts',(-18.9724474720446,10.8076110073896,122.287775791708)) ;
#34341 = CARTESIAN_POINT('Ctrl Pts',(-18.8632279358149,10.6276219269797,122.006771081539)) ;
#34342 = CARTESIAN_POINT('Ctrl Pts',(-19.1713300500782,10.8174671807414,122.229578165669)) ;
#34343 = CARTESIAN_POINT('Ctrl Pts',(-19.1118308518097,10.6374781003316,121.934021032192)) ;
#34344 = CARTESIAN_POINT('Ctrl Pts',(-19.3802073449411,10.8274664517043,122.206207727251)) ;
#34345 = CARTESIAN_POINT('Ctrl Pts',(-19.3729271808597,10.6474773712945,121.904805274405)) ;
#34346 = CARTESIAN_POINT('Ctrl Pts',(-19.5878599933699,10.8373609034616,122.219083370884)) ;
#34347 = CARTESIAN_POINT('Ctrl Pts',(-19.6324934400016,10.6573718230518,121.920897070104)) ;
#34348 = CARTESIAN_POINT('Ctrl Pts',(-19.7934840277289,10.847424219271,122.268698552168)) ;
#34349 = CARTESIAN_POINT('Ctrl Pts',(-19.8895240952947,10.6674351388611,121.982913347052)) ;
#34350 = CARTESIAN_POINT('Ctrl Pts',(-19.9832086160557,10.8572630760106,122.351185619817)) ;
#34351 = CARTESIAN_POINT('Ctrl Pts',(-20.1266813029748,10.6772739956008,122.086019825829)) ;
#34352 = CARTESIAN_POINT('Ctrl Pts',(-20.1597838606521,10.8673291978282,122.467764324916)) ;
#34353 = CARTESIAN_POINT('Ctrl Pts',(-20.3474018173166,10.6873401174184,122.23174090198)) ;
#34354 = CARTESIAN_POINT('Ctrl Pts',(-20.3106209535211,10.8772124255524,122.610700532014)) ;
#34355 = CARTESIAN_POINT('Ctrl Pts',(-20.5359503275938,10.6972233451426,122.410409425855)) ;
#34356 = CARTESIAN_POINT('Ctrl Pts',(-20.4360184408181,10.8872018868312,122.779136894016)) ;
#34357 = CARTESIAN_POINT('Ctrl Pts',(-20.6926994160956,10.7072128064214,122.620953380514)) ;
#34358 = CARTESIAN_POINT('Ctrl Pts',(-20.5299682723289,10.8971655972577,122.966365986146)) ;
#34359 = CARTESIAN_POINT('Ctrl Pts',(-20.8101391926436,10.7171765168479,122.85498870408)) ;
#34360 = CARTESIAN_POINT('Ctrl Pts',(-20.5903840833054,10.9071605999886,123.167636072351)) ;
#34361 = CARTESIAN_POINT('Ctrl Pts',(-20.8856615342813,10.7271715195788,123.106575647553)) ;
#34362 = CARTESIAN_POINT('Ctrl Pts',(-20.6147046372521,10.9171969309989,123.377214474421)) ;
#34363 = CARTESIAN_POINT('Ctrl Pts',(-20.9160649147942,10.737207850589,123.36854831693)) ;
#34364 = CARTESIAN_POINT('Ctrl Pts',(-20.602840741777,10.9270431603412,123.583885830223)) ;
#34365 = CARTESIAN_POINT('Ctrl Pts',(-20.9012376686418,10.7470540799313,123.626888226554)) ;
#34366 = CARTESIAN_POINT('Ctrl Pts',(-20.5549910593693,10.9370286586164,123.788252345139)) ;
#34367 = CARTESIAN_POINT('Ctrl Pts',(-20.8414280632278,10.7570395782066,123.882347119875)) ;
#34368 = CARTESIAN_POINT('Ctrl Pts',(-20.4729131510359,10.9469635615994,123.98035400042)) ;
#34369 = CARTESIAN_POINT('Ctrl Pts',(-20.7388329137616,10.7669744811896,124.122475498286)) ;
#34370 = CARTESIAN_POINT('Ctrl Pts',(-20.3571965408839,10.9570210646946,124.157283328264)) ;
#34371 = CARTESIAN_POINT('Ctrl Pts',(-20.5941893978565,10.7770319842848,124.343638489548)) ;
#34372 = CARTESIAN_POINT('Ctrl Pts',(-20.2161055904513,10.9668427210651,124.308072643193)) ;
#34373 = CARTESIAN_POINT('Ctrl Pts',(-20.4178270375078,10.7868536406553,124.532127444564)) ;
#34374 = CARTESIAN_POINT('Ctrl Pts',(-20.0473038580147,10.9768987837303,124.435324360385)) ;
#34375 = CARTESIAN_POINT('Ctrl Pts',(-20.2068264506129,10.7969097033205,124.691194003482)) ;
#34376 = CARTESIAN_POINT('Ctrl Pts',(-19.8609387437001,10.9868394484335,124.529907956578)) ;
#34377 = CARTESIAN_POINT('Ctrl Pts',(-19.9738709151532,10.8068503680237,124.809425923897)) ;
#34378 = CARTESIAN_POINT('Ctrl Pts',(-19.6619073820417,10.996743852382,124.591096321842)) ;
#34379 = CARTESIAN_POINT('Ctrl Pts',(-19.7250819168236,10.8167547719722,124.885913848149)) ;
#34380 = CARTESIAN_POINT('Ctrl Pts',(-19.4523135812511,11.0067903373756,124.6170333815)) ;
#34381 = CARTESIAN_POINT('Ctrl Pts',(-19.4630900672469,10.8268012569657,124.91833758783)) ;
#34382 = CARTESIAN_POINT('Ctrl Pts',(-19.2444994497963,11.0166865651873,124.606521749711)) ;
#34383 = CARTESIAN_POINT('Ctrl Pts',(-19.2033217041948,10.8366974847775,124.905200421556)) ;
#34384 = CARTESIAN_POINT('Ctrl Pts',(-19.038362504801,11.0267461487508,124.559366648931)) ;
#34385 = CARTESIAN_POINT('Ctrl Pts',(-18.9456501548506,10.8467570683409,124.84625892515)) ;
#34386 = CARTESIAN_POINT('Ctrl Pts',(-18.8475263552642,11.0365981584196,124.478841690953)) ;
#34387 = CARTESIAN_POINT('Ctrl Pts',(-18.7071032762533,10.8566090780098,124.745604613622)) ;
#34388 = CARTESIAN_POINT('Ctrl Pts',(-18.6712543899711,11.0465606898592,124.365745599051)) ;
#34389 = CARTESIAN_POINT('Ctrl Pts',(-18.486761846583,10.8665716094494,124.604236201888)) ;
#34390 = CARTESIAN_POINT('Ctrl Pts',(-18.5164393691186,11.0565922380985,124.222526123336)) ;
#34391 = CARTESIAN_POINT('Ctrl Pts',(-18.2932415519354,10.8766031576887,124.425213596777)) ;
#34392 = CARTESIAN_POINT('Ctrl Pts',(-18.3904718457185,11.0664836493116,124.057073079274)) ;
#34393 = CARTESIAN_POINT('Ctrl Pts',(-18.1357799385702,10.8864945689018,124.218398117889)) ;
#34394 = CARTESIAN_POINT('Ctrl Pts',(-18.2936007393847,11.0764999030196,123.870096289376)) ;
#34395 = CARTESIAN_POINT('Ctrl Pts',(-18.0146891208495,10.8965108226097,123.984678099448)) ;
#34396 = CARTESIAN_POINT('Ctrl Pts',(-18.2310191009212,11.0865300058643,123.668736110514)) ;
#34397 = CARTESIAN_POINT('Ctrl Pts',(-17.9364599064169,10.9065409254544,123.732978598367)) ;
#34398 = CARTESIAN_POINT('Ctrl Pts',(-18.2044167485645,11.096386454818,123.463224365483)) ;
#34399 = CARTESIAN_POINT('Ctrl Pts',(-17.9032046925238,10.9163973744082,123.476088297532)) ;
#34400 = CARTESIAN_POINT('Ctrl Pts',(-18.2137726552221,11.1063854655903,123.253255515666)) ;
#34401 = CARTESIAN_POINT('Ctrl Pts',(-17.9148974746838,10.9263963851804,123.213627004968)) ;
#34402 = CARTESIAN_POINT('Ctrl Pts',(-18.2587594656026,11.1162806825083,123.050114933331)) ;
#34403 = CARTESIAN_POINT('Ctrl Pts',(-17.9711291548573,10.9362916020984,122.959700121577)) ;
#34404 = CARTESIAN_POINT('Ctrl Pts',(-18.3396629587075,11.1263411978656,122.85472528768)) ;
#34405 = CARTESIAN_POINT('Ctrl Pts',(-18.0722565350831,10.9463521174558,122.715462501304)) ;
#34406 = CARTESIAN_POINT('Ctrl Pts',(-18.4508021074728,11.1361904912527,122.67999776762)) ;
#34407 = CARTESIAN_POINT('Ctrl Pts',(-18.2111793287359,10.9562014108428,122.497051143114)) ;
#34408 = CARTESIAN_POINT('Ctrl Pts',(-18.5927075074045,11.1462176669327,122.524117766382)) ;
#34409 = CARTESIAN_POINT('Ctrl Pts',(-18.3885596784698,10.9662285865229,122.302199917905)) ;
#34410 = CARTESIAN_POINT('Ctrl Pts',(-18.7598974171996,11.1562462425598,122.39565716601)) ;
#34411 = CARTESIAN_POINT('Ctrl Pts',(-18.5975457775066,10.97625716215,122.141622604238)) ;
#34412 = CARTESIAN_POINT('Ctrl Pts',(-18.9432305176374,11.1660913361057,122.299619707887)) ;
#34413 = CARTESIAN_POINT('Ctrl Pts',(-18.8267122579824,10.9861022556959,122.021573575525)) ;
#34414 = CARTESIAN_POINT('Ctrl Pts',(-19.1432259259205,11.1760825775375,122.235411488495)) ;
#34415 = CARTESIAN_POINT('Ctrl Pts',(-19.076706172588,10.9960934971277,121.941311591206)) ;
#34416 = CARTESIAN_POINT('Ctrl Pts',(-19.3523221570473,11.1861183586808,122.207211675339)) ;
#34417 = CARTESIAN_POINT('Ctrl Pts',(-19.33807608883,11.0061292782709,121.90605998594)) ;
#34418 = CARTESIAN_POINT('Ctrl Pts',(-19.5592805247249,11.1959705644105,122.215313540189)) ;
#34419 = CARTESIAN_POINT('Ctrl Pts',(-19.5967752495453,11.0159814840007,121.916185579001)) ;
#34420 = CARTESIAN_POINT('Ctrl Pts',(-19.7640786083089,11.2059326585275,122.259120874168)) ;
#34421 = CARTESIAN_POINT('Ctrl Pts',(-19.8527735772525,11.0259435781177,121.970943280824)) ;
#34422 = CARTESIAN_POINT('Ctrl Pts',(-19.9592440107104,11.2159552193546,122.338540115345)) ;
#34423 = CARTESIAN_POINT('Ctrl Pts',(-20.0967309230037,11.0359661389448,122.070215768885)) ;
#34424 = CARTESIAN_POINT('Ctrl Pts',(-20.1360936806095,11.2258829910061,122.449415578369)) ;
#34425 = CARTESIAN_POINT('Ctrl Pts',(-20.3177943873976,11.0458939105963,122.208809071597)) ;
#34426 = CARTESIAN_POINT('Ctrl Pts',(-20.2927527732055,11.235925375131,122.59092205436)) ;
#34427 = CARTESIAN_POINT('Ctrl Pts',(-20.5136192108406,11.0559362947211,122.385690857769)) ;
#34428 = CARTESIAN_POINT('Ctrl Pts',(-20.4205680894076,11.2458145992016,122.754908938647)) ;
#34429 = CARTESIAN_POINT('Ctrl Pts',(-20.6733901754155,11.0658255187918,122.590674219362)) ;
#34430 = CARTESIAN_POINT('Ctrl Pts',(-20.5192928454941,11.2558038473689,122.940253974445)) ;
#34431 = CARTESIAN_POINT('Ctrl Pts',(-20.7967974985827,11.0758147669591,122.82235502115)) ;
#34432 = CARTESIAN_POINT('Ctrl Pts',(-20.5839847168731,11.2657624244109,123.139363117153)) ;
#34433 = CARTESIAN_POINT('Ctrl Pts',(-20.877663904031,11.0857733440011,123.071241395872)) ;
#34434 = CARTESIAN_POINT('Ctrl Pts',(-20.6134608095792,11.2756619935022,123.345397790749)) ;
#34435 = CARTESIAN_POINT('Ctrl Pts',(-20.9145104547974,11.0956729130923,123.328785419535)) ;
#34436 = CARTESIAN_POINT('Ctrl Pts',(-20.6065401284065,11.2857099055862,123.556501597487)) ;
#34437 = CARTESIAN_POINT('Ctrl Pts',(-20.9058609614837,11.1057208251763,123.592665004886)) ;
#34438 = CARTESIAN_POINT('Ctrl Pts',(-20.5638788823548,11.2956052598934,123.760144762529)) ;
#34439 = CARTESIAN_POINT('Ctrl Pts',(-20.8525354819889,11.1156161794835,123.84722011856)) ;
#34440 = CARTESIAN_POINT('Ctrl Pts',(-20.4852553344784,11.3056669103846,123.956492429052)) ;
#34441 = CARTESIAN_POINT('Ctrl Pts',(-20.7542573599522,11.1256778299747,124.092654877051)) ;
#34442 = CARTESIAN_POINT('Ctrl Pts',(-20.3761505871013,11.315511525847,124.132371029593)) ;
#34443 = CARTESIAN_POINT('Ctrl Pts',(-20.6178768119948,11.1355224454372,124.312504919937)) ;
#34444 = CARTESIAN_POINT('Ctrl Pts',(-20.237114111558,11.3254716047484,124.288935623539)) ;
#34445 = CARTESIAN_POINT('Ctrl Pts',(-20.4440816601254,11.1454825243386,124.508211665925)) ;
#34446 = CARTESIAN_POINT('Ctrl Pts',(-20.0714663398208,11.3355097991068,124.419675506507)) ;
#34447 = CARTESIAN_POINT('Ctrl Pts',(-20.237022783302,11.155520718697,124.671637321571)) ;
#34448 = CARTESIAN_POINT('Ctrl Pts',(-19.8888323535182,11.3453835145064,124.518385640457)) ;
#34449 = CARTESIAN_POINT('Ctrl Pts',(-20.0087297938928,11.1653944340966,124.79502640491)) ;
#34450 = CARTESIAN_POINT('Ctrl Pts',(-19.6879284940433,11.3554552240407,124.585159910392)) ;
#34451 = CARTESIAN_POINT('Ctrl Pts',(-19.7576006731065,11.1754661436308,124.878495075327)) ;
#34452 = CARTESIAN_POINT('Ctrl Pts',(-19.4834310386215,11.3652876644932,124.615427060217)) ;
#34453 = CARTESIAN_POINT('Ctrl Pts',(-19.5019775459642,11.1852985840833,124.916330182975)) ;
#34454 = CARTESIAN_POINT('Ctrl Pts',(-19.2726002542326,11.3753194854186,124.610200309681)) ;
#34455 = CARTESIAN_POINT('Ctrl Pts',(-19.23843916646,11.1953304050088,124.909797495745)) ;
#34456 = CARTESIAN_POINT('Ctrl Pts',(-19.0662276962164,11.3853398553042,124.567903119432)) ;
#34457 = CARTESIAN_POINT('Ctrl Pts',(-18.9804733109485,11.2053507748943,124.856926970569)) ;
#34458 = CARTESIAN_POINT('Ctrl Pts',(-18.8731273416045,11.3952066264379,124.492104200881)) ;
#34459 = CARTESIAN_POINT('Ctrl Pts',(-18.7390964606754,11.2152175460281,124.762178595667)) ;
#34460 = CARTESIAN_POINT('Ctrl Pts',(-18.6924952829997,11.4052773976273,124.381703676241)) ;
#34461 = CARTESIAN_POINT('Ctrl Pts',(-18.5133063352231,11.2252883172175,124.624178813751)) ;
#34462 = CARTESIAN_POINT('Ctrl Pts',(-18.5373237843845,11.4151205581489,124.244779697978)) ;
#34463 = CARTESIAN_POINT('Ctrl Pts',(-18.319340401592,11.2351314777391,124.453023478545)) ;
#34464 = CARTESIAN_POINT('Ctrl Pts',(-18.4059602071296,11.4251007913353,124.081184277243)) ;
#34465 = CARTESIAN_POINT('Ctrl Pts',(-18.1551353492068,11.2451117109255,124.248529269584)) ;
#34466 = CARTESIAN_POINT('Ctrl Pts',(-18.3049653385912,11.4351193113705,123.896363057127)) ;
#34467 = CARTESIAN_POINT('Ctrl Pts',(-18.028891195505,11.2551302309607,124.017503067195)) ;
#34468 = CARTESIAN_POINT('Ctrl Pts',(-18.2380760069019,11.4450026197542,123.69961958379)) ;
#34469 = CARTESIAN_POINT('Ctrl Pts',(-17.9452787246737,11.2650135393444,123.771572840956)) ;
#34470 = CARTESIAN_POINT('Ctrl Pts',(-18.2058712454328,11.455070903925,123.490451765677)) ;
#34471 = CARTESIAN_POINT('Ctrl Pts',(-17.9050223247957,11.2750818235151,123.51011355244)) ;
#34472 = CARTESIAN_POINT('Ctrl Pts',(-18.2101233464429,11.4649010305926,123.283800583045)) ;
#34473 = CARTESIAN_POINT('Ctrl Pts',(-17.9103370637522,11.2849119501828,123.251798025959)) ;
#34474 = CARTESIAN_POINT('Ctrl Pts',(-18.250874219467,11.4749676027992,123.076164349147)) ;
#34475 = CARTESIAN_POINT('Ctrl Pts',(-17.9612752713621,11.2949785223893,122.992253063274)) ;
#34476 = CARTESIAN_POINT('Ctrl Pts',(-18.3258631651741,11.4848577590399,122.882207935105)) ;
#34477 = CARTESIAN_POINT('Ctrl Pts',(-18.0550114913503,11.30486867863,122.749806436383)) ;
#34478 = CARTESIAN_POINT('Ctrl Pts',(-18.4340938733603,11.4948502866163,122.702175775169)) ;
#34479 = CARTESIAN_POINT('Ctrl Pts',(-18.1902998279347,11.3148612062065,122.524765958855)) ;
#34480 = CARTESIAN_POINT('Ctrl Pts',(-18.5716561470465,11.5048117764906,122.544271291541)) ;
#34481 = CARTESIAN_POINT('Ctrl Pts',(-18.3622527777214,11.3248226960808,122.327384835922)) ;
#34482 = CARTESIAN_POINT('Ctrl Pts',(-18.733397668661,11.5147209983778,122.412963329841)) ;
#34483 = CARTESIAN_POINT('Ctrl Pts',(-18.5644303505111,11.334731917968,122.163249256317)) ;
#34484 = CARTESIAN_POINT('Ctrl Pts',(-18.9180612846803,11.5247695781881,122.310386430444)) ;
#34485 = CARTESIAN_POINT('Ctrl Pts',(-18.7952595963168,11.3447804977783,122.03502817518)) ;
#34486 = CARTESIAN_POINT('Ctrl Pts',(-19.1144372305553,11.5346525526582,122.242490101265)) ;
#34487 = CARTESIAN_POINT('Ctrl Pts',(-19.0407305551372,11.3546634722484,121.95015733424)) ;
#34488 = CARTESIAN_POINT('Ctrl Pts',(-19.3218535876862,11.5446474638009,122.208905343626)) ;
#34489 = CARTESIAN_POINT('Ctrl Pts',(-19.3000011957466,11.364658383391,121.908176470979)) ;
#34490 = CARTESIAN_POINT('Ctrl Pts',(-19.5325030834212,11.5546678503745,122.212142964224)) ;
#34491 = CARTESIAN_POINT('Ctrl Pts',(-19.5633130308723,11.3746787699646,121.912223489053)) ;
#34492 = CARTESIAN_POINT('Ctrl Pts',(-19.7371085501306,11.5645779542315,122.251347857035)) ;
#34493 = CARTESIAN_POINT('Ctrl Pts',(-19.8190707586294,11.3845888738217,121.961229817073)) ;
#34494 = CARTESIAN_POINT('Ctrl Pts',(-19.9323591296137,11.5745056664414,122.325110819767)) ;
#34495 = CARTESIAN_POINT('Ctrl Pts',(-20.0631345837559,11.3945165860316,122.053434027818)) ;
#34496 = CARTESIAN_POINT('Ctrl Pts',(-20.1138182396832,11.5845487762087,122.433038429192)) ;
#34497 = CARTESIAN_POINT('Ctrl Pts',(-20.2899581916419,11.4045596957989,122.188343592996)) ;
#34498 = CARTESIAN_POINT('Ctrl Pts',(-20.2713872169236,11.5944351966642,122.568595596171)) ;
#34499 = CARTESIAN_POINT('Ctrl Pts',(-20.4869200799301,11.4144461162544,122.357790944898)) ;
#34500 = CARTESIAN_POINT('Ctrl Pts',(-20.4047088338096,11.6044283742699,122.730945445389)) ;
#34501 = CARTESIAN_POINT('Ctrl Pts',(-20.6535719341279,11.42443929386,122.560728657127)) ;
#34502 = CARTESIAN_POINT('Ctrl Pts',(-20.5072617933259,11.6143740371738,122.913157719128)) ;
#34503 = CARTESIAN_POINT('Ctrl Pts',(-20.7817631202892,11.434384956764,122.788494689885)) ;
#34504 = CARTESIAN_POINT('Ctrl Pts',(-20.5770363442089,11.624321333379,123.110307996559)) ;
#34505 = CARTESIAN_POINT('Ctrl Pts',(-20.8689810113342,11.4443322529691,123.034933251559)) ;
#34506 = CARTESIAN_POINT('Ctrl Pts',(-20.6116338746559,11.6343690989569,123.318685651132)) ;
#34507 = CARTESIAN_POINT('Ctrl Pts',(-20.9122274632923,11.454380018547,123.295405142893)) ;
#34508 = CARTESIAN_POINT('Ctrl Pts',(-20.6097306714455,11.6442173121745,123.525714223304)) ;
#34509 = CARTESIAN_POINT('Ctrl Pts',(-20.9098479557393,11.4642282317647,123.55419225068)) ;
#34510 = CARTESIAN_POINT('Ctrl Pts',(-20.5721619278645,11.6541768849686,123.731697031123)) ;
#34511 = CARTESIAN_POINT('Ctrl Pts',(-20.8628861918604,11.4741878045588,123.811671085789)) ;
#34512 = CARTESIAN_POINT('Ctrl Pts',(-20.4984904473743,11.6642135060011,123.92941246265)) ;
#34513 = CARTESIAN_POINT('Ctrl Pts',(-20.7707963195394,11.4842244255913,124.05881501279)) ;
#34514 = CARTESIAN_POINT('Ctrl Pts',(-20.3935356094815,11.6740940208114,124.108691624986)) ;
#34515 = CARTESIAN_POINT('Ctrl Pts',(-20.6396015638699,11.4941049404016,124.282914554995)) ;
#34516 = CARTESIAN_POINT('Ctrl Pts',(-20.2567978653035,11.6841466721185,124.269794367337)) ;
#34517 = CARTESIAN_POINT('Ctrl Pts',(-20.468678971524,11.5041575917087,124.484292270333)) ;
#34518 = CARTESIAN_POINT('Ctrl Pts',(-20.0967123068534,11.6940420703985,124.40270437159)) ;
#34519 = CARTESIAN_POINT('Ctrl Pts',(-20.268570770948,11.5140529899886,124.650429772434)) ;
#34520 = CARTESIAN_POINT('Ctrl Pts',(-19.9132571297185,11.7040921921046,124.507462775467)) ;
#34521 = CARTESIAN_POINT('Ctrl Pts',(-20.0392516107157,11.5241031116947,124.781376915265)) ;
#34522 = CARTESIAN_POINT('Ctrl Pts',(-19.7176472157066,11.7139764716465,124.577647205215)) ;
#34523 = CARTESIAN_POINT('Ctrl Pts',(-19.7947379346561,11.5339873912366,124.869107009974)) ;
#34524 = CARTESIAN_POINT('Ctrl Pts',(-19.5106395256385,11.7239712529384,124.613575520575)) ;
#34525 = CARTESIAN_POINT('Ctrl Pts',(-19.535977954542,11.5439821725286,124.914016453037)) ;
#34526 = CARTESIAN_POINT('Ctrl Pts',(-19.3014914963835,11.7339190981252,124.612936959039)) ;
#34527 = CARTESIAN_POINT('Ctrl Pts',(-19.2745423775974,11.5539300177154,124.913217278896)) ;
#34528 = CARTESIAN_POINT('Ctrl Pts',(-19.0958351736706,11.7438560615126,124.576338079464)) ;
#34529 = CARTESIAN_POINT('Ctrl Pts',(-19.0174715357775,11.5638669811028,124.867467501011)) ;
#34530 = CARTESIAN_POINT('Ctrl Pts',(-18.8986161272856,11.7538390262498,124.504485391709)) ;
#34531 = CARTESIAN_POINT('Ctrl Pts',(-18.7709478903142,11.57384994584,124.777650445181)) ;
#34532 = CARTESIAN_POINT('Ctrl Pts',(-18.7159988224537,11.7638828776654,124.398530286436)) ;
#34533 = CARTESIAN_POINT('Ctrl Pts',(-18.5426769439272,11.5838937972556,124.645205762121)) ;
#34534 = CARTESIAN_POINT('Ctrl Pts',(-18.5576631664198,11.7737110790002,124.265735860728)) ;
#34535 = CARTESIAN_POINT('Ctrl Pts',(-18.3447570489577,11.5937219985904,124.479210868713)) ;
#34536 = CARTESIAN_POINT('Ctrl Pts',(-18.4214033173466,11.7837876515982,124.103588886124)) ;
#34537 = CARTESIAN_POINT('Ctrl Pts',(-18.1744334770161,11.6037985711884,124.276526674695)) ;
#34538 = CARTESIAN_POINT('Ctrl Pts',(-18.3175955543511,11.7936397316058,123.92430715972)) ;
#34539 = CARTESIAN_POINT('Ctrl Pts',(-18.0446742699967,11.613650651196,124.052422800999)) ;
#34540 = CARTESIAN_POINT('Ctrl Pts',(-18.2447567569921,11.8037130166099,123.725492716322)) ;
#34541 = CARTESIAN_POINT('Ctrl Pts',(-17.9536271836293,11.6237239362001,123.80390465871)) ;
#34542 = CARTESIAN_POINT('Ctrl Pts',(-18.2084461708989,11.8135543683204,123.521791919159)) ;
#34543 = CARTESIAN_POINT('Ctrl Pts',(-17.9082400348832,11.6335652879105,123.549277141693)) ;
#34544 = CARTESIAN_POINT('Ctrl Pts',(-18.2072783331998,11.8235158677169,123.312385813251)) ;
#34545 = CARTESIAN_POINT('Ctrl Pts',(-17.9067818388404,11.6435267873071,123.287519099371)) ;
#34546 = CARTESIAN_POINT('Ctrl Pts',(-18.2431187666664,11.8335516438469,123.104460989179)) ;
#34547 = CARTESIAN_POINT('Ctrl Pts',(-17.951583816613,11.653562563437,123.027613430396)) ;
#34548 = CARTESIAN_POINT('Ctrl Pts',(-18.313260700151,11.8434400704844,122.908768536338)) ;
#34549 = CARTESIAN_POINT('Ctrl Pts',(-18.039263006394,11.6634509900746,122.782997516974)) ;
#34550 = CARTESIAN_POINT('Ctrl Pts',(-18.4172968730816,11.8534553925594,122.725703223709)) ;
#34551 = CARTESIAN_POINT('Ctrl Pts',(-18.1693096864973,11.6734663121495,122.554166702765)) ;
#34552 = CARTESIAN_POINT('Ctrl Pts',(-18.5521138610027,11.8634857414596,122.563558399555)) ;
#34553 = CARTESIAN_POINT('Ctrl Pts',(-18.3378320340471,11.6834966610498,122.351486710927)) ;
#34554 = CARTESIAN_POINT('Ctrl Pts',(-18.7097629865951,11.8733291170662,122.429511598476)) ;
#34555 = CARTESIAN_POINT('Ctrl Pts',(-18.5348954405883,11.6933400366564,122.183928683916)) ;
#34556 = CARTESIAN_POINT('Ctrl Pts',(-18.8914357075047,11.8833585539634,122.322486366911)) ;
#34557 = CARTESIAN_POINT('Ctrl Pts',(-18.7619871989478,11.7033694735536,122.050148739799)) ;
#34558 = CARTESIAN_POINT('Ctrl Pts',(-19.0891853403317,11.8933904318963,122.249153011441)) ;
#34559 = CARTESIAN_POINT('Ctrl Pts',(-19.0091747228791,11.7134013514865,121.958483598084)) ;
#34560 = CARTESIAN_POINT('Ctrl Pts',(-19.2923854095674,11.9032200550018,122.211622723258)) ;
#34561 = CARTESIAN_POINT('Ctrl Pts',(-19.2631763810866,11.723230974592,121.911572238441)) ;
#34562 = CARTESIAN_POINT('Ctrl Pts',(-19.5023882087078,11.9132095261549,122.209287327401)) ;
#34563 = CARTESIAN_POINT('Ctrl Pts',(-19.5256800788835,11.733220445745,121.908654949402)) ;
#34564 = CARTESIAN_POINT('Ctrl Pts',(-19.7106392401679,11.9232533749173,122.244164803758)) ;
#34565 = CARTESIAN_POINT('Ctrl Pts',(-19.7859934260146,11.7432642945074,121.952253536854)) ;
#34566 = CARTESIAN_POINT('Ctrl Pts',(-19.9054125620073,11.933075080449,122.312709524051)) ;
#34567 = CARTESIAN_POINT('Ctrl Pts',(-20.0294606191332,11.7530860000391,122.037936667124)) ;
#34568 = CARTESIAN_POINT('Ctrl Pts',(-20.0894867289459,11.9431101202768,122.415781902165)) ;
#34569 = CARTESIAN_POINT('Ctrl Pts',(-20.2595522205111,11.763121039867,122.166778899323)) ;
#34570 = CARTESIAN_POINT('Ctrl Pts',(-20.2523369083129,11.9531348271682,122.54956886486)) ;
#34571 = CARTESIAN_POINT('Ctrl Pts',(-20.4631137172292,11.7731457467584,122.334014058128)) ;
#34572 = CARTESIAN_POINT('Ctrl Pts',(-20.3874578810136,11.962987531509,122.706561960871)) ;
#34573 = CARTESIAN_POINT('Ctrl Pts',(-20.6320140503792,11.7829984510992,122.53025751933)) ;
#34574 = CARTESIAN_POINT('Ctrl Pts',(-20.4950292100305,11.9729756537167,122.88687951836)) ;
#34575 = CARTESIAN_POINT('Ctrl Pts',(-20.7664764700505,11.7929865733069,122.755655719677)) ;
#34576 = CARTESIAN_POINT('Ctrl Pts',(-20.5692290588118,11.982904123824,123.081978843733)) ;
#34577 = CARTESIAN_POINT('Ctrl Pts',(-20.8592244693061,11.8029150434141,122.999531121784)) ;
#34578 = CARTESIAN_POINT('Ctrl Pts',(-20.6090083992339,11.9928931009912,123.28818688241)) ;
#34579 = CARTESIAN_POINT('Ctrl Pts',(-20.908946487162,11.8129040205813,123.257291767324)) ;
#34580 = CARTESIAN_POINT('Ctrl Pts',(-20.6120343021104,12.0029309082709,123.499185950342)) ;
#34581 = CARTESIAN_POINT('Ctrl Pts',(-20.9127267285164,11.822941827861,123.521040547075)) ;
#34582 = CARTESIAN_POINT('Ctrl Pts',(-20.5793530027892,12.0127772091342,123.703591668076)) ;
#34583 = CARTESIAN_POINT('Ctrl Pts',(-20.8718727621147,11.8327881287243,123.776548267518)) ;
#34584 = CARTESIAN_POINT('Ctrl Pts',(-20.5108877173329,12.0228029525135,123.902937612404)) ;
#34585 = CARTESIAN_POINT('Ctrl Pts',(-20.7862889532544,11.8428138721037,124.025729898037)) ;
#34586 = CARTESIAN_POINT('Ctrl Pts',(-20.4083149981522,12.0328338189525,124.087198060114)) ;
#34587 = CARTESIAN_POINT('Ctrl Pts',(-20.6580711492703,11.8528447385427,124.256054351239)) ;
#34588 = CARTESIAN_POINT('Ctrl Pts',(-20.278204027201,12.0426711777513,124.247942559337)) ;
#34589 = CARTESIAN_POINT('Ctrl Pts',(-20.4954300470344,11.8626820973415,124.456984258303)) ;
#34590 = CARTESIAN_POINT('Ctrl Pts',(-20.1200700787013,12.052663138685,124.386216766339)) ;
#34591 = CARTESIAN_POINT('Ctrl Pts',(-20.2977609080955,11.8726740582752,124.629825264853)) ;
#34592 = CARTESIAN_POINT('Ctrl Pts',(-19.9393758024445,12.0626955012416,124.495014747097)) ;
#34593 = CARTESIAN_POINT('Ctrl Pts',(-20.0718918884513,11.8827064208318,124.765820716472)) ;
#34594 = CARTESIAN_POINT('Ctrl Pts',(-19.7459234684514,12.072560661816,124.569749829319)) ;
#34595 = CARTESIAN_POINT('Ctrl Pts',(-19.8300749226539,11.8925715814062,124.8592375948)) ;
#34596 = CARTESIAN_POINT('Ctrl Pts',(-19.5405372405183,12.0825225663937,124.610739722099)) ;
#34597 = CARTESIAN_POINT('Ctrl Pts',(-19.5733413955224,11.9025334859838,124.91047253432)) ;
#34598 = CARTESIAN_POINT('Ctrl Pts',(-19.3296285023073,12.0925574964694,124.615133939641)) ;
#34599 = CARTESIAN_POINT('Ctrl Pts',(-19.3097054567176,11.9125684160596,124.915962853165)) ;
#34600 = CARTESIAN_POINT('Ctrl Pts',(-19.12418262518,12.102442443323,124.58366381539)) ;
#34601 = CARTESIAN_POINT('Ctrl Pts',(-19.052897931185,11.9224533629132,124.876622619273)) ;
#34602 = CARTESIAN_POINT('Ctrl Pts',(-18.9237994034088,12.1125081196345,124.515756077525)) ;
#34603 = CARTESIAN_POINT('Ctrl Pts',(-18.8024198540118,11.9325190392247,124.791735612514)) ;
#34604 = CARTESIAN_POINT('Ctrl Pts',(-18.7422682640068,12.1223470392694,124.416531181598)) ;
#34605 = CARTESIAN_POINT('Ctrl Pts',(-18.5755065294537,11.9423579588596,124.66770191258)) ;
#34606 = CARTESIAN_POINT('Ctrl Pts',(-18.5769155643104,12.1324105490038,124.284598448374)) ;
#34607 = CARTESIAN_POINT('Ctrl Pts',(-18.36881738441,11.952421468594,124.502784045041)) ;
#34608 = CARTESIAN_POINT('Ctrl Pts',(-18.4394382528722,12.1423041621656,124.128483209612)) ;
#34609 = CARTESIAN_POINT('Ctrl Pts',(-18.196972359284,11.9623150817557,124.307637940831)) ;
#34610 = CARTESIAN_POINT('Ctrl Pts',(-18.330159277488,12.152248168979,123.950297968068)) ;
#34611 = CARTESIAN_POINT('Ctrl Pts',(-18.0603757684666,11.9722590885692,124.084904760915)) ;
#34612 = CARTESIAN_POINT('Ctrl Pts',(-18.2529261348415,12.1622491233333,123.754711085262)) ;
#34613 = CARTESIAN_POINT('Ctrl Pts',(-17.9638367966722,11.9822600429234,123.84042009983)) ;
#34614 = CARTESIAN_POINT('Ctrl Pts',(-18.2110463667562,12.1722878810256,123.547880865785)) ;
#34615 = CARTESIAN_POINT('Ctrl Pts',(-17.9114896577593,11.9922988006158,123.581881819459)) ;
#34616 = CARTESIAN_POINT('Ctrl Pts',(-18.2053758043967,12.1821120651956,123.341406321408)) ;
#34617 = CARTESIAN_POINT('Ctrl Pts',(-17.9044041218427,12.0021229847857,123.323787975378)) ;
#34618 = CARTESIAN_POINT('Ctrl Pts',(-18.2360503167514,12.192170130795,123.132209463155)) ;
#34619 = CARTESIAN_POINT('Ctrl Pts',(-17.942749948479,12.0121810503852,123.062292370607)) ;
#34620 = CARTESIAN_POINT('Ctrl Pts',(-18.302006424845,12.2021001775697,122.934128152636)) ;
#34621 = CARTESIAN_POINT('Ctrl Pts',(-18.0251977236969,12.0221110971599,122.81469131617)) ;
#34622 = CARTESIAN_POINT('Ctrl Pts',(-18.4010777311963,12.2120516199068,122.749859407281)) ;
#34623 = CARTESIAN_POINT('Ctrl Pts',(-18.1490393730645,12.032062539497,122.58435652218)) ;
#34624 = CARTESIAN_POINT('Ctrl Pts',(-18.5321045118858,12.2220984170861,122.584200624693)) ;
#34625 = CARTESIAN_POINT('Ctrl Pts',(-18.3128249787563,12.0421093366763,122.3772847395)) ;
#34626 = CARTESIAN_POINT('Ctrl Pts',(-18.6866546754837,12.2319463577662,122.446441479111)) ;
#34627 = CARTESIAN_POINT('Ctrl Pts',(-18.5060148097537,12.0519572773564,122.20508758863)) ;
#34628 = CARTESIAN_POINT('Ctrl Pts',(-18.8644598958187,12.2419079891088,122.335805361285)) ;
#34629 = CARTESIAN_POINT('Ctrl Pts',(-18.7282729224317,12.061918908699,122.066794754657)) ;
#34630 = CARTESIAN_POINT('Ctrl Pts',(-19.0602009714326,12.2519366484847,122.257435573529)) ;
#34631 = CARTESIAN_POINT('Ctrl Pts',(-18.9729503385331,12.0719475680749,121.96883508161)) ;
#34632 = CARTESIAN_POINT('Ctrl Pts',(-19.2641055065429,12.2618469513729,122.214691358915)) ;
#34633 = CARTESIAN_POINT('Ctrl Pts',(-19.2278317877476,12.081857870963,121.915407496546)) ;
#34634 = CARTESIAN_POINT('Ctrl Pts',(-19.472848854405,12.2717818459351,122.20743693277)) ;
#34635 = CARTESIAN_POINT('Ctrl Pts',(-19.4887612039863,12.0917927655252,121.906342273748)) ;
#34636 = CARTESIAN_POINT('Ctrl Pts',(-19.6818517454895,12.281822944602,122.237040740592)) ;
#34637 = CARTESIAN_POINT('Ctrl Pts',(-19.7500144690239,12.1018338641922,121.943349817982)) ;
#34638 = CARTESIAN_POINT('Ctrl Pts',(-19.8795274393584,12.2917102271064,122.301350610276)) ;
#34639 = CARTESIAN_POINT('Ctrl Pts',(-19.9971083720291,12.1117211466965,122.023739879695)) ;
#34640 = CARTESIAN_POINT('Ctrl Pts',(-20.0651177529335,12.3017019676169,122.399712129327)) ;
#34641 = CARTESIAN_POINT('Ctrl Pts',(-20.2290950029952,12.121712887207,122.146694306232)) ;
#34642 = CARTESIAN_POINT('Ctrl Pts',(-20.2301016245503,12.3116525168523,122.52834286884)) ;
#34643 = CARTESIAN_POINT('Ctrl Pts',(-20.4353231818541,12.1316634364425,122.307485012955)) ;
#34644 = CARTESIAN_POINT('Ctrl Pts',(-20.3702511436106,12.3215881944871,122.68320837822)) ;
#34645 = CARTESIAN_POINT('Ctrl Pts',(-20.6105080303752,12.1415991140773,122.501068844244)) ;
#34646 = CARTESIAN_POINT('Ctrl Pts',(-20.4821440049613,12.3315736122799,122.86084640938)) ;
#34647 = CARTESIAN_POINT('Ctrl Pts',(-20.750371753323,12.15158453187,122.723117938281)) ;
#34648 = CARTESIAN_POINT('Ctrl Pts',(-20.561588894867,12.3416024051504,123.056141240279)) ;
#34649 = CARTESIAN_POINT('Ctrl Pts',(-20.8496752814838,12.1616133247405,122.967237619822)) ;
#34650 = CARTESIAN_POINT('Ctrl Pts',(-20.605473389762,12.3514819163783,123.25914772635)) ;
#34651 = CARTESIAN_POINT('Ctrl Pts',(-20.9045281451374,12.1714928359685,123.220996340635)) ;
#34652 = CARTESIAN_POINT('Ctrl Pts',(-20.6140174461044,12.3614754530513,123.469077690765)) ;
#34653 = CARTESIAN_POINT('Ctrl Pts',(-20.9152054114084,12.1814863726414,123.483408955601)) ;
#34654 = CARTESIAN_POINT('Ctrl Pts',(-20.5854395929456,12.3715077213151,123.67803354945)) ;
#34655 = CARTESIAN_POINT('Ctrl Pts',(-20.8794802828438,12.1915186409053,123.744603500806)) ;
#34656 = CARTESIAN_POINT('Ctrl Pts',(-20.5225086633852,12.381371683321,123.875648773567)) ;
#34657 = CARTESIAN_POINT('Ctrl Pts',(-20.8008139738613,12.2013826029112,123.991621606328)) ;
#34658 = CARTESIAN_POINT('Ctrl Pts',(-20.4242612791623,12.3914417446659,124.063150375643)) ;
#34659 = CARTESIAN_POINT('Ctrl Pts',(-20.6780021897342,12.2114526642561,124.225997440443)) ;
#34660 = CARTESIAN_POINT('Ctrl Pts',(-20.2978479151584,12.4012841090146,124.22697472228)) ;
#34661 = CARTESIAN_POINT('Ctrl Pts',(-20.5199833627417,12.2212950286048,124.430776031816)) ;
#34662 = CARTESIAN_POINT('Ctrl Pts',(-20.1436024751154,12.4112447815171,124.368597953825)) ;
#34663 = CARTESIAN_POINT('Ctrl Pts',(-20.3271747466949,12.2312557011072,124.607803018329)) ;
#34664 = CARTESIAN_POINT('Ctrl Pts',(-19.9655160234336,12.4212828525849,124.481805478694)) ;
#34665 = CARTESIAN_POINT('Ctrl Pts',(-20.1045650508994,12.2412937721751,124.749310160121)) ;
#34666 = CARTESIAN_POINT('Ctrl Pts',(-19.7737887271615,12.4311564675453,124.561434581507)) ;
#34667 = CARTESIAN_POINT('Ctrl Pts',(-19.8649051460095,12.2511673871355,124.848843922395)) ;
#34668 = CARTESIAN_POINT('Ctrl Pts',(-19.5671291833791,12.4412287021266,124.607402354197)) ;
#34669 = CARTESIAN_POINT('Ctrl Pts',(-19.6065797304147,12.2612396217167,124.906300997573)) ;
#34670 = CARTESIAN_POINT('Ctrl Pts',(-19.3607684693909,12.4510527205754,124.616796315158)) ;
#34671 = CARTESIAN_POINT('Ctrl Pts',(-19.3486297183274,12.2710636401655,124.918040759742)) ;
#34672 = CARTESIAN_POINT('Ctrl Pts',(-19.1509428265166,12.4611176415514,124.589849021404)) ;
#34673 = CARTESIAN_POINT('Ctrl Pts',(-19.0863456687307,12.2811285611415,124.884353810288)) ;
#34674 = CARTESIAN_POINT('Ctrl Pts',(-18.8857365452566,12.4743279398461,124.507174456424)) ;
#34675 = CARTESIAN_POINT('Ctrl Pts',(-18.7548496615418,12.2943388594363,124.781008020419)) ;
#34676 = CARTESIAN_POINT('Ctrl Pts',(-18.6462382926402,12.4876433865781,124.356312359537)) ;
#34677 = CARTESIAN_POINT('Ctrl Pts',(-18.4555083324541,12.3076543061683,124.592460114514)) ;
#34678 = CARTESIAN_POINT('Ctrl Pts',(-18.4564387488717,12.5009336318454,124.15121232202)) ;
#34679 = CARTESIAN_POINT('Ctrl Pts',(-18.218215898367,12.3209445514355,124.336043204895)) ;
#34680 = CARTESIAN_POINT('Ctrl Pts',(-18.3421528810108,12.5109843814525,123.973529884011)) ;
#34681 = CARTESIAN_POINT('Ctrl Pts',(-18.0753697674162,12.3309953010427,124.113946532607)) ;
#34682 = CARTESIAN_POINT('Ctrl Pts',(-18.261991671417,12.5207969884347,123.783417454446)) ;
#34683 = CARTESIAN_POINT('Ctrl Pts',(-17.9751686261835,12.3408079080249,123.87630326557)) ;
#34684 = CARTESIAN_POINT('Ctrl Pts',(-18.2145854633708,12.530868086429,123.5770937702)) ;
#34685 = CARTESIAN_POINT('Ctrl Pts',(-17.9159132712724,12.3508790060192,123.618399594221)) ;
#34686 = CARTESIAN_POINT('Ctrl Pts',(-18.2041287449214,12.5407576592038,123.369434972959)) ;
#34687 = CARTESIAN_POINT('Ctrl Pts',(-17.9028470179378,12.360768578794,123.35882151871)) ;
#34688 = CARTESIAN_POINT('Ctrl Pts',(-18.2378495819674,12.5540277660071,123.092473664091)) ;
#34689 = CARTESIAN_POINT('Ctrl Pts',(-17.944990032383,12.3740386855973,123.012644489427)) ;
#34690 = CARTESIAN_POINT('Ctrl Pts',(-18.3698646515677,12.5706444529296,122.764802678493)) ;
#34691 = CARTESIAN_POINT('Ctrl Pts',(-18.1100382420037,12.3906553725198,122.60301895944)) ;
#34692 = CARTESIAN_POINT('Ctrl Pts',(-18.6050396672439,12.5872184962459,122.502279793378)) ;
#34693 = CARTESIAN_POINT('Ctrl Pts',(-18.4039538091135,12.407229415836,122.274921978535)) ;
#34694 = CARTESIAN_POINT('Ctrl Pts',(-18.8388843969827,12.6005150636777,122.349174786392)) ;
#34695 = CARTESIAN_POINT('Ctrl Pts',(-18.6963080999189,12.4205259832679,122.083501484913)) ;
#34696 = CARTESIAN_POINT('Ctrl Pts',(-19.032708382408,12.6105451272551,122.266104245232)) ;
#34697 = CARTESIAN_POINT('Ctrl Pts',(-18.9385791928831,12.4305560468453,121.979673523447)) ;
#34698 = CARTESIAN_POINT('Ctrl Pts',(-19.2351868358827,12.6204390191043,122.218590201878)) ;
#34699 = CARTESIAN_POINT('Ctrl Pts',(-19.1916818709367,12.4404499386945,121.92028162813)) ;
#34700 = CARTESIAN_POINT('Ctrl Pts',(-19.5133724231769,12.6336917748899,122.2020040059)) ;
#34701 = CARTESIAN_POINT('Ctrl Pts',(-19.5394009792706,12.45370269448,121.899549493542)) ;
#34702 = CARTESIAN_POINT('Ctrl Pts',(-19.8616244702295,12.6504198798823,122.274010765671)) ;
#34703 = CARTESIAN_POINT('Ctrl Pts',(-19.9747293753449,12.4704307994725,121.989564308793)) ;
#34704 = CARTESIAN_POINT('Ctrl Pts',(-20.2206924205023,12.6702507163608,122.495213042442)) ;
#34705 = CARTESIAN_POINT('Ctrl Pts',(-20.4235566592419,12.490261635951,122.266069036596)) ;
#34706 = CARTESIAN_POINT('Ctrl Pts',(-20.4846749217705,12.690176108251,122.826464817505)) ;
#34707 = CARTESIAN_POINT('Ctrl Pts',(-20.753532722758,12.5101870278411,122.680135635445)) ;
#34708 = CARTESIAN_POINT('Ctrl Pts',(-20.6197750422256,12.710101321603,123.228081726851)) ;
#34709 = CARTESIAN_POINT('Ctrl Pts',(-20.9224041261866,12.5301122411931,123.182157120568)) ;
#34710 = CARTESIAN_POINT('Ctrl Pts',(-20.6098235900098,12.7300263350881,123.651575664266)) ;
#34711 = CARTESIAN_POINT('Ctrl Pts',(-20.9099617273898,12.5500372546782,123.711523704273)) ;
#34712 = CARTESIAN_POINT('Ctrl Pts',(-20.4568446708067,12.7499028067881,124.045572962216)) ;
#34713 = CARTESIAN_POINT('Ctrl Pts',(-20.7187360423288,12.5699137263783,124.204018044757)) ;
#34714 = CARTESIAN_POINT('Ctrl Pts',(-20.1773211945259,12.7698821246969,124.36546202135)) ;
#34715 = CARTESIAN_POINT('Ctrl Pts',(-20.369330064379,12.5898930442871,124.603877601749)) ;
#34716 = CARTESIAN_POINT('Ctrl Pts',(-19.8060899945786,12.7898151282729,124.57002813045)) ;
#34717 = CARTESIAN_POINT('Ctrl Pts',(-19.9052905888401,12.6098260478631,124.859582769338)) ;
#34718 = CARTESIAN_POINT('Ctrl Pts',(-19.3882558614324,12.8097103983006,124.635945221289)) ;
#34719 = CARTESIAN_POINT('Ctrl Pts',(-19.3829989743663,12.6297213178908,124.941977004647)) ;
#34720 = CARTESIAN_POINT('Ctrl Pts',(-18.9723404365734,12.8296317362065,124.55563458962)) ;
#34721 = CARTESIAN_POINT('Ctrl Pts',(-18.863106015617,12.6496426557967,124.841587523939)) ;
#34722 = CARTESIAN_POINT('Ctrl Pts',(-18.6081781423476,12.8495893594727,124.337737107174)) ;
#34723 = CARTESIAN_POINT('Ctrl Pts',(-18.4079042834639,12.6696002790628,124.569214869041)) ;
#34724 = CARTESIAN_POINT('Ctrl Pts',(-18.3412557610278,12.8694691914299,124.010060659351)) ;
#34725 = CARTESIAN_POINT('Ctrl Pts',(-18.0742532723479,12.68948011102,124.159620153189)) ;
#34726 = CARTESIAN_POINT('Ctrl Pts',(-18.2010112247405,12.8893510427268,123.611173077498)) ;
#34727 = CARTESIAN_POINT('Ctrl Pts',(-17.8989480656809,12.7093619623169,123.661012507465)) ;
#34728 = CARTESIAN_POINT('Ctrl Pts',(-18.2061520734863,12.9094220598306,123.184494838161)) ;
#34729 = CARTESIAN_POINT('Ctrl Pts',(-17.9053743363055,12.7294329794208,123.127663535491)) ;
#34730 = CARTESIAN_POINT('Ctrl Pts',(-18.3545914950356,12.9292292835837,122.790282514626)) ;
#34731 = CARTESIAN_POINT('Ctrl Pts',(-18.0909224032178,12.7492402031738,122.634900991588)) ;
#34732 = CARTESIAN_POINT('Ctrl Pts',(-18.6302173582225,12.9492104191524,122.467021464749)) ;
#34733 = CARTESIAN_POINT('Ctrl Pts',(-18.4354537166866,12.7692213387426,122.230824135061)) ;
#34734 = CARTESIAN_POINT('Ctrl Pts',(-18.9990267978771,12.9691379124917,122.258503177642)) ;
#34735 = CARTESIAN_POINT('Ctrl Pts',(-18.8964641845817,12.7891488320818,121.970176160886)) ;
#34736 = CARTESIAN_POINT('Ctrl Pts',(-19.414525111865,12.9889585738495,122.187284802443)) ;
#34737 = CARTESIAN_POINT('Ctrl Pts',(-19.4158344326454,12.8089694934396,121.881151656018)) ;
#34738 = CARTESIAN_POINT('Ctrl Pts',(-19.8347816721657,13.0090557630713,122.26378936849)) ;
#34739 = CARTESIAN_POINT('Ctrl Pts',(-19.941156659121,12.8290666826614,121.976780869957)) ;
#34740 = CARTESIAN_POINT('Ctrl Pts',(-20.1980367737812,13.0288194420796,122.475474924502)) ;
#34741 = CARTESIAN_POINT('Ctrl Pts',(-20.3952240685032,12.8488303616698,122.241384544903)) ;
#34742 = CARTESIAN_POINT('Ctrl Pts',(-20.47137453339,13.0488767207527,122.802591270838)) ;
#34743 = CARTESIAN_POINT('Ctrl Pts',(-20.7368987004734,12.8688876403428,122.650278782987)) ;
#34744 = CARTESIAN_POINT('Ctrl Pts',(-20.6146542104524,13.0686721445001,123.198479778478)) ;
#34745 = CARTESIAN_POINT('Ctrl Pts',(-20.9159999986636,12.8886830640902,123.145136393703)) ;
#34746 = CARTESIAN_POINT('Ctrl Pts',(-20.6155493708649,13.0886357892277,123.622911309277)) ;
#34747 = CARTESIAN_POINT('Ctrl Pts',(-20.9171224626867,12.9086467088179,123.675675466357)) ;
#34748 = CARTESIAN_POINT('Ctrl Pts',(-20.4704208826885,13.1086192805018,124.022266658295)) ;
#34749 = CARTESIAN_POINT('Ctrl Pts',(-20.7357148690054,12.9286302000919,124.174870580525)) ;
#34750 = CARTESIAN_POINT('Ctrl Pts',(-20.2007675400314,13.1284267756511,124.345835412524)) ;
#34751 = CARTESIAN_POINT('Ctrl Pts',(-20.3986521463661,12.9484376952412,124.579332558928)) ;
#34752 = CARTESIAN_POINT('Ctrl Pts',(-19.834022972994,13.1484093663712,124.560193591737)) ;
#34753 = CARTESIAN_POINT('Ctrl Pts',(-19.9402235763346,12.9684202859613,124.847283742943)) ;
#34754 = CARTESIAN_POINT('Ctrl Pts',(-19.4180361300331,13.1682920203624,124.636116448361)) ;
#34755 = CARTESIAN_POINT('Ctrl Pts',(-19.420241605384,12.9883029399526,124.942191223887)) ;
#34756 = CARTESIAN_POINT('Ctrl Pts',(-18.9996554886756,13.1882502652255,124.565604893307)) ;
#34757 = CARTESIAN_POINT('Ctrl Pts',(-18.897265373855,13.0082611848157,124.854056149891)) ;
#34758 = CARTESIAN_POINT('Ctrl Pts',(-18.6317218676168,13.2081258522671,124.357573974673)) ;
#34759 = CARTESIAN_POINT('Ctrl Pts',(-18.4373467192626,13.0281367718572,124.594021898984)) ;
#34760 = CARTESIAN_POINT('Ctrl Pts',(-18.3552399068354,13.2281067404023,124.035038294504)) ;
#34761 = CARTESIAN_POINT('Ctrl Pts',(-18.0917408139602,13.0481176599925,124.1908552924)) ;
#34762 = CARTESIAN_POINT('Ctrl Pts',(-18.206044297576,13.2480418815133,123.638227388492)) ;
#34763 = CARTESIAN_POINT('Ctrl Pts',(-17.9052414354233,13.0680528011035,123.694844185539)) ;
#34764 = CARTESIAN_POINT('Ctrl Pts',(-18.2009152531286,13.2679538995244,123.214915566106)) ;
#34765 = CARTESIAN_POINT('Ctrl Pts',(-17.8988271166159,13.0879648191146,123.165702838914)) ;
#34766 = CARTESIAN_POINT('Ctrl Pts',(-18.3399734278226,13.287842117768,122.815536644445)) ;
#34767 = CARTESIAN_POINT('Ctrl Pts',(-18.0726376302732,13.1078530373582,122.666485551937)) ;
#34768 = CARTESIAN_POINT('Ctrl Pts',(-18.5625167302271,13.3044404216149,122.541702141202)) ;
#34769 = CARTESIAN_POINT('Ctrl Pts',(-18.350835637743,13.1244513412051,122.324166060029)) ;
#34770 = CARTESIAN_POINT('Ctrl Pts',(-18.7884633242958,13.3177130115177,122.377888779236)) ;
#34771 = CARTESIAN_POINT('Ctrl Pts',(-18.6332461345366,13.1377239311079,122.119417599734)) ;
#34772 = CARTESIAN_POINT('Ctrl Pts',(-18.9775497688346,13.3277204264686,122.285661961006)) ;
#34773 = CARTESIAN_POINT('Ctrl Pts',(-18.8696106143379,13.1477313460587,122.004127651188)) ;
#34774 = CARTESIAN_POINT('Ctrl Pts',(-19.1798541137618,13.3377277732012,122.227841226343)) ;
#34775 = CARTESIAN_POINT('Ctrl Pts',(-19.1224757065686,13.1577386927914,121.9318494161)) ;
#34776 = CARTESIAN_POINT('Ctrl Pts',(-19.4571882805755,13.3509941330028,122.198742528533)) ;
#34777 = CARTESIAN_POINT('Ctrl Pts',(-19.4692111889478,13.171005052593,121.89547658206)) ;
#34778 = CARTESIAN_POINT('Ctrl Pts',(-19.8041191619441,13.3675087906257,122.253086418136)) ;
#34779 = CARTESIAN_POINT('Ctrl Pts',(-19.9027886653429,13.1875197102159,121.96339145382)) ;
#34780 = CARTESIAN_POINT('Ctrl Pts',(-20.1135332813589,13.3841062238684,122.422657976203)) ;
#34781 = CARTESIAN_POINT('Ctrl Pts',(-20.2896179417095,13.2041171434586,122.175375538801)) ;
#34782 = CARTESIAN_POINT('Ctrl Pts',(-20.3161488488574,13.3974542210134,122.616898131359)) ;
#34783 = CARTESIAN_POINT('Ctrl Pts',(-20.5428541366847,13.2174651406036,122.418153018411)) ;
#34784 = CARTESIAN_POINT('Ctrl Pts',(-20.4392682471211,13.407349975365,122.78458790923)) ;
#34785 = CARTESIAN_POINT('Ctrl Pts',(-20.6967627805078,13.2273608949552,122.627767557119)) ;
#34786 = CARTESIAN_POINT('Ctrl Pts',(-20.5324892710804,13.4173379292963,122.972722988984)) ;
#34787 = CARTESIAN_POINT('Ctrl Pts',(-20.8132896637827,13.2373488488865,122.862934128943)) ;
#34788 = CARTESIAN_POINT('Ctrl Pts',(-20.5915443850433,13.4272951530011,123.173577963998)) ;
#34789 = CARTESIAN_POINT('Ctrl Pts',(-20.8871117691411,13.2473060725913,123.114002366609)) ;
#34790 = CARTESIAN_POINT('Ctrl Pts',(-20.6149084211195,13.4373306995577,123.383244466026)) ;
#34791 = CARTESIAN_POINT('Ctrl Pts',(-20.9163194698178,13.2573416191479,123.376085199786)) ;
#34792 = CARTESIAN_POINT('Ctrl Pts',(-20.6018663431854,13.4472178108339,123.590706984687)) ;
#34793 = CARTESIAN_POINT('Ctrl Pts',(-20.9000197112505,13.267228730424,123.63541352092)) ;
#34794 = CARTESIAN_POINT('Ctrl Pts',(-20.5528158490788,13.4572092159347,123.794940084393)) ;
#34795 = CARTESIAN_POINT('Ctrl Pts',(-20.8387093067792,13.2772201355249,123.890705618854)) ;
#34796 = CARTESIAN_POINT('Ctrl Pts',(-20.4693700177335,13.4671548371495,123.986654821614)) ;
#34797 = CARTESIAN_POINT('Ctrl Pts',(-20.7344045825384,13.2871657567396,124.130350209197)) ;
#34798 = CARTESIAN_POINT('Ctrl Pts',(-20.3542090233936,13.4771040854178,124.161276470942)) ;
#34799 = CARTESIAN_POINT('Ctrl Pts',(-20.5904556481203,13.297115005008,124.34862888779)) ;
#34800 = CARTESIAN_POINT('Ctrl Pts',(-20.2089077397589,13.4871505805864,124.314549867347)) ;
#34801 = CARTESIAN_POINT('Ctrl Pts',(-20.40883104897,13.3071615001766,124.540222615125)) ;
#34802 = CARTESIAN_POINT('Ctrl Pts',(-20.0426037732206,13.4970019233779,124.438001198331)) ;
#34803 = CARTESIAN_POINT('Ctrl Pts',(-20.2009526791305,13.3170128429681,124.694539108577)) ;
#34804 = CARTESIAN_POINT('Ctrl Pts',(-19.8553954660048,13.5069737035053,124.532292944024)) ;
#34805 = CARTESIAN_POINT('Ctrl Pts',(-19.9669434550626,13.3269846230954,124.812406349875)) ;
#34806 = CARTESIAN_POINT('Ctrl Pts',(-19.6541253092378,13.516968903483,124.592783946963)) ;
#34807 = CARTESIAN_POINT('Ctrl Pts',(-19.7153564891538,13.3369798230732,124.888022808534)) ;
#34808 = CARTESIAN_POINT('Ctrl Pts',(-19.444620176713,13.527002895179,124.617242515377)) ;
#34809 = CARTESIAN_POINT('Ctrl Pts',(-19.4534753611661,13.3470138147692,124.91859882113)) ;
#34810 = CARTESIAN_POINT('Ctrl Pts',(-19.2377415370854,13.5368583001515,124.605497638602)) ;
#34811 = CARTESIAN_POINT('Ctrl Pts',(-19.1948766730109,13.3568692197417,124.903920505653)) ;
#34812 = CARTESIAN_POINT('Ctrl Pts',(-19.0330890851524,13.5468575979973,124.557608984223)) ;
#34813 = CARTESIAN_POINT('Ctrl Pts',(-18.9390603846548,13.3668685175874,124.844062381802)) ;
#34814 = CARTESIAN_POINT('Ctrl Pts',(-18.8417203854023,13.5567527106025,124.475953276878)) ;
#34815 = CARTESIAN_POINT('Ctrl Pts',(-18.6998481883224,13.3767636301927,124.741995186998)) ;
#34816 = CARTESIAN_POINT('Ctrl Pts',(-18.6645864621206,13.5668133561375,124.360423798942)) ;
#34817 = CARTESIAN_POINT('Ctrl Pts',(-18.4784292945403,13.3868242757276,124.597585675385)) ;
#34818 = CARTESIAN_POINT('Ctrl Pts',(-18.5133398637062,13.5766622331267,124.218993175225)) ;
#34819 = CARTESIAN_POINT('Ctrl Pts',(-18.2893688820631,13.3966731527169,124.420799145547)) ;
#34820 = CARTESIAN_POINT('Ctrl Pts',(-18.3862631485546,13.5866909442203,124.050762009217)) ;
#34821 = CARTESIAN_POINT('Ctrl Pts',(-18.1305208052828,13.4067018638104,124.210511784237)) ;
#34822 = CARTESIAN_POINT('Ctrl Pts',(-18.2908283109245,13.5967203454764,123.862742118593)) ;
#34823 = CARTESIAN_POINT('Ctrl Pts',(-18.0112247909558,13.4167312650665,123.975488167426)) ;
#34824 = CARTESIAN_POINT('Ctrl Pts',(-18.2302062670491,13.6065605372724,123.664948493123)) ;
#34825 = CARTESIAN_POINT('Ctrl Pts',(-17.9354445008445,13.4265714568625,123.728246471196)) ;
#34826 = CARTESIAN_POINT('Ctrl Pts',(-18.2040444170886,13.6165639664654,123.456299673931)) ;
#34827 = CARTESIAN_POINT('Ctrl Pts',(-17.9027395318293,13.4365748860555,123.467435684468)) ;
#34828 = CARTESIAN_POINT('Ctrl Pts',(-18.2145600866286,13.6265494789316,123.246600447077)) ;
#34829 = CARTESIAN_POINT('Ctrl Pts',(-17.9158814572938,13.4465603985218,123.205311390365)) ;
#34830 = CARTESIAN_POINT('Ctrl Pts',(-18.2617823017495,13.6365905753156,123.040875922897)) ;
#34831 = CARTESIAN_POINT('Ctrl Pts',(-17.9749065837084,13.4566014949057,122.948155155558)) ;
#34832 = CARTESIAN_POINT('Ctrl Pts',(-18.3421364497269,13.6464337712666,122.850159429394)) ;
#34833 = CARTESIAN_POINT('Ctrl Pts',(-18.075347036012,13.4664446908567,122.709757985418)) ;
#34834 = CARTESIAN_POINT('Ctrl Pts',(-18.4556351281271,13.656420082321,122.67358245955)) ;
#34835 = CARTESIAN_POINT('Ctrl Pts',(-18.2172182814588,13.4764310019111,122.489035231078)) ;
#34836 = CARTESIAN_POINT('Ctrl Pts',(-18.5972804388859,13.6663547675787,122.520040996224)) ;
#34837 = CARTESIAN_POINT('Ctrl Pts',(-18.3942732512021,13.4863656871689,122.297106419583)) ;
#34838 = CARTESIAN_POINT('Ctrl Pts',(-18.7655457253041,13.6764123287957,122.392050964971)) ;
#34839 = CARTESIAN_POINT('Ctrl Pts',(-18.6046031877323,13.4964232483859,122.137116873828)) ;
#34840 = CARTESIAN_POINT('Ctrl Pts',(-18.948971596639,13.6862339704043,122.297188134367)) ;
#34841 = CARTESIAN_POINT('Ctrl Pts',(-18.8338850494827,13.5062448899945,122.018535713122)) ;
#34842 = CARTESIAN_POINT('Ctrl Pts',(-19.150630895694,13.6962900339953,122.233780317479)) ;
#34843 = CARTESIAN_POINT('Ctrl Pts',(-19.0859583258677,13.5163009535855,121.939273611485)) ;
#34844 = CARTESIAN_POINT('Ctrl Pts',(-19.3579055678042,13.7062307097571,122.207035465086)) ;
#34845 = CARTESIAN_POINT('Ctrl Pts',(-19.3450516698188,13.5262416293473,121.905839973704)) ;
#34846 = CARTESIAN_POINT('Ctrl Pts',(-19.5659365047634,13.7161350685454,122.215998316577)) ;
#34847 = CARTESIAN_POINT('Ctrl Pts',(-19.6050909750298,13.5361459881356,121.917041144566)) ;
#34848 = CARTESIAN_POINT('Ctrl Pts',(-19.7721240618805,13.7261817231212,122.26171766678)) ;
#34849 = CARTESIAN_POINT('Ctrl Pts',(-19.8628258516087,13.5461926427114,121.974187922095)) ;
#34850 = CARTESIAN_POINT('Ctrl Pts',(-19.9644220298839,13.7360773177641,122.341175721282)) ;
#34851 = CARTESIAN_POINT('Ctrl Pts',(-20.1031997644219,13.5560882373542,122.073508487828)) ;
#34852 = CARTESIAN_POINT('Ctrl Pts',(-20.1429187786372,13.7461392644209,122.454645564807)) ;
#34853 = CARTESIAN_POINT('Ctrl Pts',(-20.3263218440841,13.5661501840111,122.215343672174)) ;
#34854 = CARTESIAN_POINT('Ctrl Pts',(-20.2957594945872,13.7559888883531,122.594367289572)) ;
#34855 = CARTESIAN_POINT('Ctrl Pts',(-20.517374964591,13.5759998079433,122.389994620087)) ;
#34856 = CARTESIAN_POINT('Ctrl Pts',(-20.4240087228008,13.7659521273829,122.75995684231)) ;
#34857 = CARTESIAN_POINT('Ctrl Pts',(-20.67768845555,13.5859630469731,122.596980439525)) ;
#34858 = CARTESIAN_POINT('Ctrl Pts',(-20.5219126757159,13.7759767021588,122.946597688754)) ;
#34859 = CARTESIAN_POINT('Ctrl Pts',(-20.8000704182634,13.5959876217489,122.830280403279)) ;
#34860 = CARTESIAN_POINT('Ctrl Pts',(-20.5853680857787,13.7858952648465,123.145221491814)) ;
#34861 = CARTESIAN_POINT('Ctrl Pts',(-20.8793920084504,13.6059061844367,123.078559981852)) ;
#34862 = CARTESIAN_POINT('Ctrl Pts',(-20.6139486861192,13.7958874515705,123.353347867714)) ;
#34863 = CARTESIAN_POINT('Ctrl Pts',(-20.9151199376275,13.6158983711606,123.338717822212)) ;
#34864 = CARTESIAN_POINT('Ctrl Pts',(-20.6055443985715,13.8059222501547,123.564135174219)) ;
#34865 = CARTESIAN_POINT('Ctrl Pts',(-20.9046168526757,13.6259331697448,123.60220196331)) ;
#34866 = CARTESIAN_POINT('Ctrl Pts',(-20.5618138969041,13.8157774408283,123.766670893346)) ;
#34867 = CARTESIAN_POINT('Ctrl Pts',(-20.849955662852,13.6357883604185,123.855372966765)) ;
#34868 = CARTESIAN_POINT('Ctrl Pts',(-20.4827162908005,13.8257767889813,123.961402445332)) ;
#34869 = CARTESIAN_POINT('Ctrl Pts',(-20.7510855574627,13.6457877085715,124.098788324471)) ;
#34870 = CARTESIAN_POINT('Ctrl Pts',(-20.3723265103831,13.8356719146565,124.137764210175)) ;
#34871 = CARTESIAN_POINT('Ctrl Pts',(-20.6130996724061,13.6556828342466,124.319242233536)) ;
#34872 = CARTESIAN_POINT('Ctrl Pts',(-20.2306869988819,13.8457324576046,124.294801970209)) ;
#34873 = CARTESIAN_POINT('Ctrl Pts',(-20.4360519660552,13.6657433771948,124.515540628951)) ;
#34874 = CARTESIAN_POINT('Ctrl Pts',(-20.0674724058813,13.8555817318715,124.422248257044)) ;
#34875 = CARTESIAN_POINT('Ctrl Pts',(-20.232034145729,13.6755926514616,124.674850715028)) ;
#34876 = CARTESIAN_POINT('Ctrl Pts',(-19.8815742262112,13.8656089564414,124.521635316517)) ;
#34877 = CARTESIAN_POINT('Ctrl Pts',(-19.9996623311439,13.6856198760316,124.799086161261)) ;
#34878 = CARTESIAN_POINT('Ctrl Pts',(-19.6810321497663,13.8756373556292,124.586723666077)) ;
#34879 = CARTESIAN_POINT('Ctrl Pts',(-19.7489854255022,13.6956482752193,124.880448501891)) ;
#34880 = CARTESIAN_POINT('Ctrl Pts',(-19.4761166290859,13.8854831060427,124.615846164903)) ;
#34881 = CARTESIAN_POINT('Ctrl Pts',(-19.4928401900541,13.7054940256328,124.916853671166)) ;
#34882 = CARTESIAN_POINT('Ctrl Pts',(-19.2662085926654,13.8954718964434,124.609433443135)) ;
#34883 = CARTESIAN_POINT('Ctrl Pts',(-19.2304548877746,13.7154828160336,124.908839488413)) ;
#34884 = CARTESIAN_POINT('Ctrl Pts',(-19.0595750845739,13.9055168248431,124.565911416118)) ;
#34885 = CARTESIAN_POINT('Ctrl Pts',(-18.9721627761569,13.7255277444333,124.85443884089)) ;
#34886 = CARTESIAN_POINT('Ctrl Pts',(-18.8677390185657,13.9153413096321,124.489339185228)) ;
#34887 = CARTESIAN_POINT('Ctrl Pts',(-18.7323658376194,13.7353522292223,124.758724681373)) ;
#34888 = CARTESIAN_POINT('Ctrl Pts',(-18.6878125716597,13.9253987071733,124.378319657156)) ;
#34889 = CARTESIAN_POINT('Ctrl Pts',(-18.507457139935,13.7454096267634,124.6199518073)) ;
#34890 = CARTESIAN_POINT('Ctrl Pts',(-18.5321161135312,13.9353247987595,124.239354765055)) ;
#34891 = CARTESIAN_POINT('Ctrl Pts',(-18.3128349524242,13.7553357183497,124.446246569744)) ;
#34892 = CARTESIAN_POINT('Ctrl Pts',(-18.4021255349772,13.945279583904,124.075342585797)) ;
#34893 = CARTESIAN_POINT('Ctrl Pts',(-18.1503452309058,13.7652905034942,124.241231958288)) ;
#34894 = CARTESIAN_POINT('Ctrl Pts',(-18.3019676622171,13.9553169535617,123.889610890228)) ;
#34895 = CARTESIAN_POINT('Ctrl Pts',(-18.0251465108619,13.7753278731519,124.009068223175)) ;
#34896 = CARTESIAN_POINT('Ctrl Pts',(-18.2364086645203,13.9652057636833,123.692318961985)) ;
#34897 = CARTESIAN_POINT('Ctrl Pts',(-17.9431959783341,13.7852166832734,123.762452941038)) ;
#34898 = CARTESIAN_POINT('Ctrl Pts',(-18.2054221774035,13.9751951227343,123.484614442852)) ;
#34899 = CARTESIAN_POINT('Ctrl Pts',(-17.9044614030354,13.7952060423245,123.502822293368)) ;
#34900 = CARTESIAN_POINT('Ctrl Pts',(-18.2111097202979,13.9851536701904,123.275338157667)) ;
#34901 = CARTESIAN_POINT('Ctrl Pts',(-17.911569338574,13.8051645897806,123.241226463724)) ;
#34902 = CARTESIAN_POINT('Ctrl Pts',(-18.2523005245241,13.9950532467415,123.071321965387)) ;
#34903 = CARTESIAN_POINT('Ctrl Pts',(-17.9630567197214,13.8150641663317,122.986205100585)) ;
#34904 = CARTESIAN_POINT('Ctrl Pts',(-18.3294851382835,14.0051011585722,122.874712691268)) ;
#34905 = CARTESIAN_POINT('Ctrl Pts',(-18.0595361492294,13.8251120781624,122.740443216443)) ;
#34906 = CARTESIAN_POINT('Ctrl Pts',(-18.4378511245041,14.0149965064327,122.697097031468)) ;
#34907 = CARTESIAN_POINT('Ctrl Pts',(-18.1949930035499,13.8350074260229,122.518422190222)) ;
#34908 = CARTESIAN_POINT('Ctrl Pts',(-18.5776635026499,14.0250581829639,122.538393890947)) ;
#34909 = CARTESIAN_POINT('Ctrl Pts',(-18.3697572977385,13.8450691025541,122.320042659878)) ;
#34910 = CARTESIAN_POINT('Ctrl Pts',(-18.7393445312316,14.0349027007131,122.409181627727)) ;
#34911 = CARTESIAN_POINT('Ctrl Pts',(-18.5718588198082,13.8549136203033,122.158525512857)) ;
#34912 = CARTESIAN_POINT('Ctrl Pts',(-18.9227751263348,14.0448631444279,122.308189876658)) ;
#34913 = CARTESIAN_POINT('Ctrl Pts',(-18.8011469810285,13.864874064018,122.032284729757)) ;
#34914 = CARTESIAN_POINT('Ctrl Pts',(-19.1226020522299,14.0548999772461,122.240434925921)) ;
#34915 = CARTESIAN_POINT('Ctrl Pts',(-19.0509301231039,13.8749108968362,121.947590006931)) ;
#34916 = CARTESIAN_POINT('Ctrl Pts',(-19.3278464181783,14.0647787739929,122.208569582796)) ;
#34917 = CARTESIAN_POINT('Ctrl Pts',(-19.3074865101941,13.884789693583,121.907757156914)) ;
#34918 = CARTESIAN_POINT('Ctrl Pts',(-19.5392604494556,14.0748380901212,122.212835075085)) ;
#34919 = CARTESIAN_POINT('Ctrl Pts',(-19.5717537455762,13.8948490097114,121.913088025212)) ;
#34920 = CARTESIAN_POINT('Ctrl Pts',(-19.7428603551298,14.0847085368744,122.252978784912)) ;
#34921 = CARTESIAN_POINT('Ctrl Pts',(-19.826254951217,13.9047194564646,121.963266910839)) ;
#34922 = CARTESIAN_POINT('Ctrl Pts',(-19.9389874347738,14.0947011751325,122.328256871601)) ;
#34923 = CARTESIAN_POINT('Ctrl Pts',(-20.0714142577625,13.9147120947226,122.057363864447)) ;
#34924 = CARTESIAN_POINT('Ctrl Pts',(-20.1195329190691,14.1047331906804,122.437257388524)) ;
#34925 = CARTESIAN_POINT('Ctrl Pts',(-20.2970965036966,13.9247441102706,122.193613633155)) ;
#34926 = CARTESIAN_POINT('Ctrl Pts',(-20.2760952863307,14.114599046987,122.573331296322)) ;
#34927 = CARTESIAN_POINT('Ctrl Pts',(-20.4928009018914,13.9346099665771,122.363706237524)) ;
#34928 = CARTESIAN_POINT('Ctrl Pts',(-20.4093323895338,14.1246683364561,122.737799807902)) ;
#34929 = CARTESIAN_POINT('Ctrl Pts',(-20.6593476165087,13.9446792560463,122.569291069307)) ;
#34930 = CARTESIAN_POINT('Ctrl Pts',(-20.5097252080318,14.1345118940074,122.918773104725)) ;
#34931 = CARTESIAN_POINT('Ctrl Pts',(-20.7848399903139,13.9545228135976,122.795508554564)) ;
#34932 = CARTESIAN_POINT('Ctrl Pts',(-20.5787488120301,14.1444920207952,123.116900923629)) ;
#34933 = CARTESIAN_POINT('Ctrl Pts',(-20.8711200645983,13.9645029403854,123.043168459395)) ;
#34934 = CARTESIAN_POINT('Ctrl Pts',(-20.6120524726319,14.1545105693952,123.324867150909)) ;
#34935 = CARTESIAN_POINT('Ctrl Pts',(-20.9127502837677,13.9745214889854,123.303126129529)) ;
#34936 = CARTESIAN_POINT('Ctrl Pts',(-20.6092267809851,14.1643938699184,123.532651027033)) ;
#34937 = CARTESIAN_POINT('Ctrl Pts',(-20.9092186327876,13.9844047895085,123.562857078082)) ;
#34938 = CARTESIAN_POINT('Ctrl Pts',(-20.5695586363973,14.1744621569665,123.740532636129)) ;
#34939 = CARTESIAN_POINT('Ctrl Pts',(-20.8596340363421,13.9944730765567,123.822708783232)) ;
#34940 = CARTESIAN_POINT('Ctrl Pts',(-20.4963791598284,14.1842922799851,123.933839607261)) ;
#34941 = CARTESIAN_POINT('Ctrl Pts',(-20.7681595372406,14.0043031995753,124.064344085661)) ;
#34942 = CARTESIAN_POINT('Ctrl Pts',(-20.3884763220446,14.1943588639105,124.115856989045)) ;
#34943 = CARTESIAN_POINT('Ctrl Pts',(-20.6332814623645,14.0143697835007,124.291865630692)) ;
#34944 = CARTESIAN_POINT('Ctrl Pts',(-20.2528909010088,14.2042489769249,124.273525084078)) ;
#34945 = CARTESIAN_POINT('Ctrl Pts',(-20.4637992773558,14.0242598965151,124.488951781999)) ;
#34946 = CARTESIAN_POINT('Ctrl Pts',(-20.0906371997248,14.2142416656876,124.406937747112)) ;
#34947 = CARTESIAN_POINT('Ctrl Pts',(-20.2609821100597,14.0342525852777,124.655717889256)) ;
#34948 = CARTESIAN_POINT('Ctrl Pts',(-19.9081695184652,14.2242025540433,124.509708404688)) ;
#34949 = CARTESIAN_POINT('Ctrl Pts',(-20.0328972096413,14.0442134736335,124.784181661486)) ;
#34950 = CARTESIAN_POINT('Ctrl Pts',(-19.7116219047513,14.2341204989233,124.579266374256)) ;
#34951 = CARTESIAN_POINT('Ctrl Pts',(-19.7872119389101,14.0541314185135,124.871129498616)) ;
#34952 = CARTESIAN_POINT('Ctrl Pts',(-19.5041267455453,14.2441282520195,124.61419846985)) ;
#34953 = CARTESIAN_POINT('Ctrl Pts',(-19.5278429325292,14.0641391716097,124.914794637659)) ;
#34954 = CARTESIAN_POINT('Ctrl Pts',(-19.2932629141695,14.2541593459786,124.612140808349)) ;
#34955 = CARTESIAN_POINT('Ctrl Pts',(-19.2642632651781,14.0741702655688,124.912222739692)) ;
#34956 = CARTESIAN_POINT('Ctrl Pts',(-19.0896342106667,14.2640073140066,124.57465995118)) ;
#34957 = CARTESIAN_POINT('Ctrl Pts',(-19.0097259981317,14.0840182335967,124.865371406534)) ;
#34958 = CARTESIAN_POINT('Ctrl Pts',(-18.8913548972053,14.2740692701324,124.501004306892)) ;
#34959 = CARTESIAN_POINT('Ctrl Pts',(-18.7618772163678,14.0940801897226,124.773301901486)) ;
#34960 = CARTESIAN_POINT('Ctrl Pts',(-18.7119419266118,14.2839664817336,124.395611023166)) ;
#34961 = CARTESIAN_POINT('Ctrl Pts',(-18.5376101428636,14.1039774013237,124.64155978923)) ;
#34962 = CARTESIAN_POINT('Ctrl Pts',(-18.5525741212308,14.2938976483982,124.260736428545)) ;
#34963 = CARTESIAN_POINT('Ctrl Pts',(-18.3384000135409,14.1139085679884,124.472965869056)) ;
#34964 = CARTESIAN_POINT('Ctrl Pts',(-18.4177287010278,14.3039398326024,124.098297375406)) ;
#34965 = CARTESIAN_POINT('Ctrl Pts',(-18.1698435133763,14.1239507521926,124.269917095333)) ;
#34966 = CARTESIAN_POINT('Ctrl Pts',(-18.3146195122506,14.3138265008555,123.917815954086)) ;
#34967 = CARTESIAN_POINT('Ctrl Pts',(-18.0409566998059,14.1338374204457,124.044314254014)) ;
#34968 = CARTESIAN_POINT('Ctrl Pts',(-18.2433338154398,14.3238196128338,123.720204704618)) ;
#34969 = CARTESIAN_POINT('Ctrl Pts',(-17.9518498697471,14.143830532424,123.797299870413)) ;
#34970 = CARTESIAN_POINT('Ctrl Pts',(-18.2076886193533,14.3337652904496,123.514175880864)) ;
#34971 = CARTESIAN_POINT('Ctrl Pts',(-17.9072936183919,14.1537762100398,123.539763194416)) ;
#34972 = CARTESIAN_POINT('Ctrl Pts',(-18.2079318857893,14.3437125934346,123.305042620039)) ;
#34973 = CARTESIAN_POINT('Ctrl Pts',(-17.9075982210939,14.1637235130248,123.278346044338)) ;
#34974 = CARTESIAN_POINT('Ctrl Pts',(-18.2450800860336,14.3537603171813,123.09710524755)) ;
#34975 = CARTESIAN_POINT('Ctrl Pts',(-17.9540338466966,14.1737712367715,123.018424649751)) ;
#34976 = CARTESIAN_POINT('Ctrl Pts',(-18.3161751561514,14.3636086909439,122.902654315691)) ;
#34977 = CARTESIAN_POINT('Ctrl Pts',(-18.0429036249904,14.183619610534,122.775359841239)) ;
#34978 = CARTESIAN_POINT('Ctrl Pts',(-18.420516020689,14.3735676633896,122.72113759086)) ;
#34979 = CARTESIAN_POINT('Ctrl Pts',(-18.1733306007622,14.1935785829798,122.548463907935)) ;
#34980 = CARTESIAN_POINT('Ctrl Pts',(-18.5561553946168,14.3836065252707,122.559457330409)) ;
#34981 = CARTESIAN_POINT('Ctrl Pts',(-18.3428801887361,14.2036174448609,122.346364098496)) ;
#34982 = CARTESIAN_POINT('Ctrl Pts',(-18.7150352575607,14.3934851294425,122.425678518084)) ;
#34983 = CARTESIAN_POINT('Ctrl Pts',(-18.5414813531674,14.2134960490327,122.179140432191)) ;
#34984 = CARTESIAN_POINT('Ctrl Pts',(-18.8977873014348,14.4035366706458,122.319642116266)) ;
#34985 = CARTESIAN_POINT('Ctrl Pts',(-18.7699215574905,14.223547590236,122.046595739421)) ;
#34986 = CARTESIAN_POINT('Ctrl Pts',(-19.0931303673642,14.4134320686262,122.247993391467)) ;
#34987 = CARTESIAN_POINT('Ctrl Pts',(-19.0141015690506,14.2334429882164,121.957035255703)) ;
#34988 = CARTESIAN_POINT('Ctrl Pts',(-19.3010884804579,14.4234833011715,122.21067275502)) ;
#34989 = CARTESIAN_POINT('Ctrl Pts',(-19.274049100191,14.2434942207616,121.910385335616)) ;
#34990 = CARTESIAN_POINT('Ctrl Pts',(-19.5089481133767,14.4333694917958,122.210014197756)) ;
#34991 = CARTESIAN_POINT('Ctrl Pts',(-19.5338747027571,14.253380411386,121.909562985826)) ;
#34992 = CARTESIAN_POINT('Ctrl Pts',(-19.7159932801428,14.4433620311115,122.245450565557)) ;
#34993 = CARTESIAN_POINT('Ctrl Pts',(-19.7926811889732,14.2633729507017,121.95385946467)) ;
#34994 = CARTESIAN_POINT('Ctrl Pts',(-19.9128752055225,14.4533104770063,122.316060788436)) ;
#34995 = CARTESIAN_POINT('Ctrl Pts',(-20.0387837795195,14.2733213965964,122.042123340341)) ;
#34996 = CARTESIAN_POINT('Ctrl Pts',(-20.0944137100652,14.4632472795382,122.419388130175)) ;
#34997 = CARTESIAN_POINT('Ctrl Pts',(-20.2657069288682,14.2832581991283,122.171283774694)) ;
#34998 = CARTESIAN_POINT('Ctrl Pts',(-20.2562053966534,14.4732302869895,122.553111371439)) ;
#34999 = CARTESIAN_POINT('Ctrl Pts',(-20.4679459835785,14.2932412065796,122.338438899013)) ;
#35000 = CARTESIAN_POINT('Ctrl Pts',(-20.3928213225405,14.4832741284043,122.714082144546)) ;
#35001 = CARTESIAN_POINT('Ctrl Pts',(-20.6387149775049,14.3032850479944,122.539652891453)) ;
#35002 = CARTESIAN_POINT('Ctrl Pts',(-20.4975727490238,14.4931023270282,122.892216003962)) ;
#35003 = CARTESIAN_POINT('Ctrl Pts',(-20.7696539437526,14.3131132466183,122.762322078402)) ;
#35004 = CARTESIAN_POINT('Ctrl Pts',(-20.5716961928806,14.5031789204704,123.09062015157)) ;
#35005 = CARTESIAN_POINT('Ctrl Pts',(-20.8623069214646,14.3231898400606,123.010327296313)) ;
#35006 = CARTESIAN_POINT('Ctrl Pts',(-20.6095053348988,14.513030919812,123.29430613063)) ;
#35007 = CARTESIAN_POINT('Ctrl Pts',(-20.9095673064433,14.3330418394022,123.264936220777)) ;
#35008 = CARTESIAN_POINT('Ctrl Pts',(-20.6115890759441,14.5231045066358,123.506038201766)) ;
#35009 = CARTESIAN_POINT('Ctrl Pts',(-20.9121706249676,14.343115426226,123.529600919864)) ;
#35010 = CARTESIAN_POINT('Ctrl Pts',(-20.5776337189286,14.5329447317333,123.710123522401)) ;
#35011 = CARTESIAN_POINT('Ctrl Pts',(-20.8697248958997,14.3529556513235,123.784708643361)) ;
#35012 = CARTESIAN_POINT('Ctrl Pts',(-20.5085876603415,14.542910435762,123.907911470471)) ;
#35013 = CARTESIAN_POINT('Ctrl Pts',(-20.7834156859523,14.3629213553522,124.031943418865)) ;
#35014 = CARTESIAN_POINT('Ctrl Pts',(-20.4053409396209,14.5529370690686,124.091700513601)) ;
#35015 = CARTESIAN_POINT('Ctrl Pts',(-20.6543560175657,14.3729479886588,124.261678938425)) ;
#35016 = CARTESIAN_POINT('Ctrl Pts',(-20.2733679541214,14.5628513647804,124.253019570529)) ;
#35017 = CARTESIAN_POINT('Ctrl Pts',(-20.489388131609,14.3828622843705,124.463327357363)) ;
#35018 = CARTESIAN_POINT('Ctrl Pts',(-20.1144447570708,14.5728396534728,124.390287718717)) ;
#35019 = CARTESIAN_POINT('Ctrl Pts',(-20.290732899766,14.392850573063,124.63491140998)) ;
#35020 = CARTESIAN_POINT('Ctrl Pts',(-19.93300982332,14.5828783866312,124.498080446046)) ;
#35021 = CARTESIAN_POINT('Ctrl Pts',(-20.0639385669917,14.4028893062214,124.769650931618)) ;
#35022 = CARTESIAN_POINT('Ctrl Pts',(-19.739575472665,14.5927217184587,124.571609128069)) ;
#35023 = CARTESIAN_POINT('Ctrl Pts',(-19.8221438934976,14.4127326380489,124.8615606774)) ;
#35024 = CARTESIAN_POINT('Ctrl Pts',(-19.5325945345893,14.6027494443383,124.611640004367)) ;
#35025 = CARTESIAN_POINT('Ctrl Pts',(-19.5634174500555,14.4227603639285,124.911597480162)) ;
#35026 = CARTESIAN_POINT('Ctrl Pts',(-19.3216956220107,14.6127817807269,124.614552263941)) ;
#35027 = CARTESIAN_POINT('Ctrl Pts',(-19.2997938732226,14.4327927003171,124.915236180564)) ;
#35028 = CARTESIAN_POINT('Ctrl Pts',(-19.1176575039999,14.6226112810275,124.581899390616)) ;
#35029 = CARTESIAN_POINT('Ctrl Pts',(-19.0447452472137,14.4426222006177,124.874418148629)) ;
#35030 = CARTESIAN_POINT('Ctrl Pts',(-18.9189866148987,14.6326007849443,124.513805611947)) ;
#35031 = CARTESIAN_POINT('Ctrl Pts',(-18.796407103044,14.4526117045345,124.789299015811)) ;
#35032 = CARTESIAN_POINT('Ctrl Pts',(-18.7344236623876,14.6426446254567,124.411231786097)) ;
#35033 = CARTESIAN_POINT('Ctrl Pts',(-18.5657044122113,14.4626555450469,124.661080239987)) ;
#35034 = CARTESIAN_POINT('Ctrl Pts',(-18.5738301995033,14.6524663312247,124.281444401144)) ;
#35035 = CARTESIAN_POINT('Ctrl Pts',(-18.3649628203968,14.4724772508149,124.498843726506)) ;
#35036 = CARTESIAN_POINT('Ctrl Pts',(-18.4348762560386,14.6625013783571,124.122702247143)) ;
#35037 = CARTESIAN_POINT('Ctrl Pts',(-18.1912720234791,14.4825122979473,124.30041474658)) ;
#35038 = CARTESIAN_POINT('Ctrl Pts',(-18.3262031256769,14.672526055794,123.942122520734)) ;
#35039 = CARTESIAN_POINT('Ctrl Pts',(-18.0554322543384,14.4925369753842,124.074689128033)) ;
#35040 = CARTESIAN_POINT('Ctrl Pts',(-18.2514273159942,14.6823788706484,123.748954040769)) ;
#35041 = CARTESIAN_POINT('Ctrl Pts',(-17.9619640242134,14.5023897902386,123.833226852774)) ;
#35042 = CARTESIAN_POINT('Ctrl Pts',(-18.2104197904952,14.692366580256,123.543040108188)) ;
#35043 = CARTESIAN_POINT('Ctrl Pts',(-17.9107066773587,14.5123774998462,123.575833839673)) ;
#35044 = CARTESIAN_POINT('Ctrl Pts',(-18.2058049225117,14.7022965902501,123.334323737137)) ;
#35045 = CARTESIAN_POINT('Ctrl Pts',(-17.9049402190557,14.5223075098402,123.314937805643)) ;
#35046 = CARTESIAN_POINT('Ctrl Pts',(-18.2373702335,14.7122863454692,123.126689249675)) ;
#35047 = CARTESIAN_POINT('Ctrl Pts',(-17.9443990826617,14.5322972650594,123.055394867525)) ;
#35048 = CARTESIAN_POINT('Ctrl Pts',(-18.3050137193924,14.7223129541521,122.927042802694)) ;
#35049 = CARTESIAN_POINT('Ctrl Pts',(-18.0289554644761,14.5423238737423,122.805837532128)) ;
#35050 = CARTESIAN_POINT('Ctrl Pts',(-18.4046749189677,14.732196894174,122.744715504703)) ;
#35051 = CARTESIAN_POINT('Ctrl Pts',(-18.1535342536619,14.5522078137641,122.577928818051)) ;
#35052 = CARTESIAN_POINT('Ctrl Pts',(-18.5354880156566,14.7421861217125,122.580419937995)) ;
#35053 = CARTESIAN_POINT('Ctrl Pts',(-18.3170525413856,14.5621970413027,122.3725606859)) ;
#35054 = CARTESIAN_POINT('Ctrl Pts',(-18.6939694465223,14.7522289922362,122.44092045882)) ;
#35055 = CARTESIAN_POINT('Ctrl Pts',(-18.5151557257253,14.5722399118263,122.198188061641)) ;
#35056 = CARTESIAN_POINT('Ctrl Pts',(-18.8703137137284,14.7620613789916,122.333079749863)) ;
#35057 = CARTESIAN_POINT('Ctrl Pts',(-18.7355880780225,14.5820722985817,122.063388638373)) ;
#35058 = CARTESIAN_POINT('Ctrl Pts',(-19.0656282841589,14.7720546721632,122.255693489157)) ;
#35059 = CARTESIAN_POINT('Ctrl Pts',(-18.9797323075833,14.5920655917533,121.966658037037)) ;
#35060 = CARTESIAN_POINT('Ctrl Pts',(-19.2723122403626,14.7820866778116,122.213661473494)) ;
#35061 = CARTESIAN_POINT('Ctrl Pts',(-19.2380876823512,14.6020975974018,121.914120317217)) ;
#35062 = CARTESIAN_POINT('Ctrl Pts',(-19.4796224788741,14.7919519337806,122.207990741201)) ;
#35063 = CARTESIAN_POINT('Ctrl Pts',(-19.4972262784245,14.6119628533708,121.907034280903)) ;
#35064 = CARTESIAN_POINT('Ctrl Pts',(-19.686880956539,14.8019138136881,122.238115152982)) ;
#35065 = CARTESIAN_POINT('Ctrl Pts',(-19.7562992627318,14.6219247332783,121.94469233049)) ;
#35066 = CARTESIAN_POINT('Ctrl Pts',(-19.8870940592205,14.81194874705,122.304572113576)) ;
#35067 = CARTESIAN_POINT('Ctrl Pts',(-20.0065648350641,14.6319596666402,122.027765848193)) ;
#35068 = CARTESIAN_POINT('Ctrl Pts',(-20.0701544259768,14.8218337054293,122.402996415654)) ;
#35069 = CARTESIAN_POINT('Ctrl Pts',(-20.2353895991696,14.6418446250194,122.15079871557)) ;
#35070 = CARTESIAN_POINT('Ctrl Pts',(-20.2362472111695,14.8318993323519,122.534060407699)) ;
#35071 = CARTESIAN_POINT('Ctrl Pts',(-20.4430039040202,14.6519102519421,122.314630587394)) ;
#35072 = CARTESIAN_POINT('Ctrl Pts',(-20.3740932209751,14.8417384380163,122.688329422969)) ;
#35073 = CARTESIAN_POINT('Ctrl Pts',(-20.6153099875451,14.6617493576065,122.507469086889)) ;
#35074 = CARTESIAN_POINT('Ctrl Pts',(-20.4857432775784,14.8518012530216,122.867986014556)) ;
#35075 = CARTESIAN_POINT('Ctrl Pts',(-20.754870275489,14.6718121726118,122.73204108607)) ;
#35076 = CARTESIAN_POINT('Ctrl Pts',(-20.5630404308717,14.8616974590703,123.061166562861)) ;
#35077 = CARTESIAN_POINT('Ctrl Pts',(-20.8514895077048,14.6817083786605,122.973518167633)) ;
#35078 = CARTESIAN_POINT('Ctrl Pts',(-20.6063727048954,14.8716382820956,123.265587679795)) ;
#35079 = CARTESIAN_POINT('Ctrl Pts',(-20.9056522988101,14.6916492016857,123.229045388468)) ;
#35080 = CARTESIAN_POINT('Ctrl Pts',(-20.6136516344617,14.8816428650742,123.47581329813)) ;
#35081 = CARTESIAN_POINT('Ctrl Pts',(-20.9147482972965,14.7016537846644,123.491827573855)) ;
#35082 = CARTESIAN_POINT('Ctrl Pts',(-20.5840199308421,14.891663759519,123.684384900853)) ;
#35083 = CARTESIAN_POINT('Ctrl Pts',(-20.8777060566585,14.7116746791091,123.752541737889)) ;
#35084 = CARTESIAN_POINT('Ctrl Pts',(-20.5197082244626,14.9015556801084,123.882155751433)) ;
#35085 = CARTESIAN_POINT('Ctrl Pts',(-20.7973137584208,14.7215665996986,123.999754867633)) ;
#35086 = CARTESIAN_POINT('Ctrl Pts',(-20.4213024996246,14.9115491124538,124.067769431274)) ;
#35087 = CARTESIAN_POINT('Ctrl Pts',(-20.6743041570178,14.731560032044,124.231770793008)) ;
#35088 = CARTESIAN_POINT('Ctrl Pts',(-20.2927239230316,14.9214947173536,124.232648085746)) ;
#35089 = CARTESIAN_POINT('Ctrl Pts',(-20.5135786632447,14.7415056369438,124.437867633148)) ;
#35090 = CARTESIAN_POINT('Ctrl Pts',(-20.1377200748608,14.9314419908352,124.373043867283)) ;
#35091 = CARTESIAN_POINT('Ctrl Pts',(-20.3198218573986,14.7514529104254,124.613360457507)) ;
#35092 = CARTESIAN_POINT('Ctrl Pts',(-19.9587916673367,14.9414899053115,124.485309172283)) ;
#35093 = CARTESIAN_POINT('Ctrl Pts',(-20.0961599099741,14.7615008249017,124.753689774918)) ;
#35094 = CARTESIAN_POINT('Ctrl Pts',(-19.7670469759163,14.9513375456589,124.563382819774)) ;
#35095 = CARTESIAN_POINT('Ctrl Pts',(-19.8564776376896,14.7713484652491,124.851279444963)) ;
#35096 = CARTESIAN_POINT('Ctrl Pts',(-19.5624646344758,14.9612992610355,124.608121127697)) ;
#35097 = CARTESIAN_POINT('Ctrl Pts',(-19.6007489896313,14.7813101806256,124.907199618472)) ;
#35098 = CARTESIAN_POINT('Ctrl Pts',(-19.3517826029045,14.9713278846083,124.61644912002)) ;
#35099 = CARTESIAN_POINT('Ctrl Pts',(-19.337396297839,14.7913388041985,124.917606836361)) ;
#35100 = CARTESIAN_POINT('Ctrl Pts',(-19.145332332827,14.9812382466747,124.588473295284)) ;
#35101 = CARTESIAN_POINT('Ctrl Pts',(-19.0793336230859,14.8012491662649,124.882634265832)) ;
#35102 = CARTESIAN_POINT('Ctrl Pts',(-18.9462038692032,14.9911729403271,124.525440044832)) ;
#35103 = CARTESIAN_POINT('Ctrl Pts',(-18.8304237660686,14.8111838599173,124.803839977421)) ;
#35104 = CARTESIAN_POINT('Ctrl Pts',(-18.7591614865791,15.001214783455,124.427569567412)) ;
#35105 = CARTESIAN_POINT('Ctrl Pts',(-18.5966220484601,14.8212257030451,124.681499373947)) ;
#35106 = CARTESIAN_POINT('Ctrl Pts',(-18.5944360678556,15.0110992890254,124.300855256588)) ;
#35107 = CARTESIAN_POINT('Ctrl Pts',(-18.3907168604578,14.8311102086156,124.5231041557)) ;
#35108 = CARTESIAN_POINT('Ctrl Pts',(-18.4524001316479,15.0211013928106,124.145842998901)) ;
#35109 = CARTESIAN_POINT('Ctrl Pts',(-18.2131739735761,14.8411123124008,124.329336878976)) ;
#35110 = CARTESIAN_POINT('Ctrl Pts',(-18.3402023620306,15.0310197442256,123.970045804479)) ;
#35111 = CARTESIAN_POINT('Ctrl Pts',(-18.0729290956119,14.8510306638158,124.109588770711)) ;
#35112 = CARTESIAN_POINT('Ctrl Pts',(-18.2592672869496,15.0410674002465,123.774968507367)) ;
#35113 = CARTESIAN_POINT('Ctrl Pts',(-17.9717628131797,14.8610783198367,123.865741080734)) ;
#35114 = CARTESIAN_POINT('Ctrl Pts',(-18.2139943917343,15.0509385932747,123.572398931231)) ;
#35115 = CARTESIAN_POINT('Ctrl Pts',(-17.91517451057,14.8709495128648,123.612528140346)) ;
#35116 = CARTESIAN_POINT('Ctrl Pts',(-18.2043671465967,15.0610043064182,123.361053655738)) ;
#35117 = CARTESIAN_POINT('Ctrl Pts',(-17.9031429830698,14.8810152260084,123.348347430976)) ;
#35118 = CARTESIAN_POINT('Ctrl Pts',(-18.2307795956915,15.0708567669908,123.155558216153)) ;
#35119 = CARTESIAN_POINT('Ctrl Pts',(-17.9361624248919,14.890867686581,123.091474379818)) ;
#35120 = CARTESIAN_POINT('Ctrl Pts',(-18.314927021648,15.0842852297134,122.886155404172)) ;
#35121 = CARTESIAN_POINT('Ctrl Pts',(-18.0413449334992,14.9042961493036,122.754742299767)) ;
#35122 = CARTESIAN_POINT('Ctrl Pts',(-18.4633001207492,15.0973661772305,122.650732206668)) ;
#35123 = CARTESIAN_POINT('Ctrl Pts',(-18.2267874469452,14.9173770968207,122.460483907538)) ;
#35124 = CARTESIAN_POINT('Ctrl Pts',(-18.6709215131284,15.110840675465,122.458175069999)) ;
#35125 = CARTESIAN_POINT('Ctrl Pts',(-18.4863543902457,14.9308515950552,122.219747666795)) ;
#35126 = CARTESIAN_POINT('Ctrl Pts',(-18.8447665738617,15.1206727790745,122.346277793249)) ;
#35127 = CARTESIAN_POINT('Ctrl Pts',(-18.703654434162,14.9406836986647,122.079886991897)) ;
#35128 = CARTESIAN_POINT('Ctrl Pts',(-19.0375991766532,15.1306386822012,122.264426190155)) ;
#35129 = CARTESIAN_POINT('Ctrl Pts',(-18.9446987350961,14.9506496017914,121.977572950956)) ;
#35130 = CARTESIAN_POINT('Ctrl Pts',(-19.2431027809361,15.1406660915114,122.217314375215)) ;
#35131 = CARTESIAN_POINT('Ctrl Pts',(-19.201576591091,14.9606770111016,121.918685704646)) ;
#35132 = CARTESIAN_POINT('Ctrl Pts',(-19.4511603917055,15.150577122878,122.206669239406)) ;
#35133 = CARTESIAN_POINT('Ctrl Pts',(-19.4616556588076,14.9705880424682,121.905384721544)) ;
#35134 = CARTESIAN_POINT('Ctrl Pts',(-19.7276733496542,15.163821430499,122.240072867962)) ;
#35135 = CARTESIAN_POINT('Ctrl Pts',(-19.8072618039582,14.9838323500892,121.947128778278)) ;
#35136 = CARTESIAN_POINT('Ctrl Pts',(-20.0569080569754,15.1805219131702,122.372778838028)) ;
#35137 = CARTESIAN_POINT('Ctrl Pts',(-20.2188550942101,15.0005328327604,122.11304531212)) ;
#35138 = CARTESIAN_POINT('Ctrl Pts',(-20.3183298277955,15.197028742326,122.607156814012)) ;
#35139 = CARTESIAN_POINT('Ctrl Pts',(-20.5455679442295,15.0170396619161,122.405960959444)) ;
#35140 = CARTESIAN_POINT('Ctrl Pts',(-20.4717021929632,15.2103393705636,122.841112767138)) ;
#35141 = CARTESIAN_POINT('Ctrl Pts',(-20.737326239263,15.0303502901537,122.698457845472)) ;
#35142 = CARTESIAN_POINT('Ctrl Pts',(-20.5546889086436,15.2203319341037,123.034149268203)) ;
#35143 = CARTESIAN_POINT('Ctrl Pts',(-20.8410482038523,15.0403428536938,122.939743261864)) ;
#35144 = CARTESIAN_POINT('Ctrl Pts',(-20.6028117634593,15.2303620171052,123.239415681091)) ;
#35145 = CARTESIAN_POINT('Ctrl Pts',(-20.9012011781756,15.0503729366954,123.196334518987)) ;
#35146 = CARTESIAN_POINT('Ctrl Pts',(-20.6188231290724,15.243535621103,123.51597584994)) ;
#35147 = CARTESIAN_POINT('Ctrl Pts',(-20.9212136814525,15.0635465406931,123.542009444159)) ;
#35148 = CARTESIAN_POINT('Ctrl Pts',(-20.5476924046879,15.2601733263344,123.862358698214)) ;
#35149 = CARTESIAN_POINT('Ctrl Pts',(-20.8322977308668,15.0801842459246,123.975012112059)) ;
#35150 = CARTESIAN_POINT('Ctrl Pts',(-20.3266298052787,15.2800550889018,124.222868771879)) ;
#35151 = CARTESIAN_POINT('Ctrl Pts',(-20.5559470864742,15.100066008492,124.425649304141)) ;
#35152 = CARTESIAN_POINT('Ctrl Pts',(-20.0488038588937,15.2967514411183,124.443780899376)) ;
#35153 = CARTESIAN_POINT('Ctrl Pts',(-20.2087222530753,15.1167623607085,124.701752625818)) ;
#35154 = CARTESIAN_POINT('Ctrl Pts',(-19.7952370287234,15.3099084689074,124.554316113986)) ;
#35155 = CARTESIAN_POINT('Ctrl Pts',(-19.8917080630765,15.1299193884976,124.839949683747)) ;
#35156 = CARTESIAN_POINT('Ctrl Pts',(-19.5219729563658,15.3232858235509,124.620769738121)) ;
#35157 = CARTESIAN_POINT('Ctrl Pts',(-19.5501536847706,15.1432967431411,124.923007742519)) ;
#35158 = CARTESIAN_POINT('Ctrl Pts',(-19.1705511769297,15.3398166578097,124.612563673835)) ;
#35159 = CARTESIAN_POINT('Ctrl Pts',(-19.1108554066157,15.1598275773999,124.912748434197)) ;
#35160 = CARTESIAN_POINT('Ctrl Pts',(-18.7747945960682,15.3597813475528,124.459104510139)) ;
#35161 = CARTESIAN_POINT('Ctrl Pts',(-18.6161685027827,15.179792267143,124.720920100974)) ;
#35162 = CARTESIAN_POINT('Ctrl Pts',(-18.4561643055464,15.3796978409765,124.180149863833)) ;
#35163 = CARTESIAN_POINT('Ctrl Pts',(-18.2178819294633,15.1997087605666,124.372224270665)) ;
#35164 = CARTESIAN_POINT('Ctrl Pts',(-18.2513709239315,15.399587560326,123.810085056575)) ;
#35165 = CARTESIAN_POINT('Ctrl Pts',(-17.9618943673674,15.2195984799162,123.909642300163)) ;
#35166 = CARTESIAN_POINT('Ctrl Pts',(-18.185122044345,15.4195942899739,123.38994096914)) ;
#35167 = CARTESIAN_POINT('Ctrl Pts',(-17.8790867339496,15.2396052095641,123.384461553135)) ;
#35168 = CARTESIAN_POINT('Ctrl Pts',(-18.2652543652805,15.4394323436208,122.975722101847)) ;
#35169 = CARTESIAN_POINT('Ctrl Pts',(-17.9792551414106,15.259443263211,122.866690154542)) ;
#35170 = CARTESIAN_POINT('Ctrl Pts',(-18.4831677244092,15.4594256818344,122.610800320768)) ;
#35171 = CARTESIAN_POINT('Ctrl Pts',(-18.2516493429581,15.2794366014246,122.410539526365)) ;
#35172 = CARTESIAN_POINT('Ctrl Pts',(-18.8109961180814,15.479308481241,122.343735818946)) ;
#35173 = CARTESIAN_POINT('Ctrl Pts',(-18.661435692943,15.2993194008312,122.076711965895)) ;
#35174 = CARTESIAN_POINT('Ctrl Pts',(-19.2100433870964,15.4992006621597,122.203893854528)) ;
#35175 = CARTESIAN_POINT('Ctrl Pts',(-19.1602442446261,15.3192115817499,121.901912195457)) ;
#35176 = CARTESIAN_POINT('Ctrl Pts',(-19.6333249972784,15.5191028406548,122.207913004512)) ;
#35177 = CARTESIAN_POINT('Ctrl Pts',(-19.6893450348299,15.3391137602449,121.906937811133)) ;
#35178 = CARTESIAN_POINT('Ctrl Pts',(-20.0320344555378,15.5391401518585,122.357748545318)) ;
#35179 = CARTESIAN_POINT('Ctrl Pts',(-20.1877316481342,15.3591510714487,122.094234259149)) ;
#35180 = CARTESIAN_POINT('Ctrl Pts',(-20.3526586672201,15.5589525933994,122.631285692703)) ;
#35181 = CARTESIAN_POINT('Ctrl Pts',(-20.5885091138789,15.3789635129896,122.43615506045)) ;
#35182 = CARTESIAN_POINT('Ctrl Pts',(-20.5630361294496,15.5790178341343,123.002216406184)) ;
#35183 = CARTESIAN_POINT('Ctrl Pts',(-20.851480272865,15.3990287537244,122.89981981938)) ;
#35184 = CARTESIAN_POINT('Ctrl Pts',(-20.633508538707,15.5987750389901,123.416561760013)) ;
#35185 = CARTESIAN_POINT('Ctrl Pts',(-20.9395694670028,15.4187859585803,123.417748054594)) ;
#35186 = CARTESIAN_POINT('Ctrl Pts',(-20.5580007528934,15.6188083116358,123.835558911533)) ;
#35187 = CARTESIAN_POINT('Ctrl Pts',(-20.8451846343238,15.438819231226,123.941494843155)) ;
#35188 = CARTESIAN_POINT('Ctrl Pts',(-20.3461462838386,15.6386212200896,124.199911351364)) ;
#35189 = CARTESIAN_POINT('Ctrl Pts',(-20.5803681949972,15.4586321396798,124.39693299142)) ;
#35190 = CARTESIAN_POINT('Ctrl Pts',(-20.0203388845668,15.6586173662171,124.472784286855)) ;
#35191 = CARTESIAN_POINT('Ctrl Pts',(-20.1731096406132,15.4786282858072,124.738024765077)) ;
#35192 = CARTESIAN_POINT('Ctrl Pts',(-19.6233743789427,15.6784791194396,124.617449122825)) ;
#35193 = CARTESIAN_POINT('Ctrl Pts',(-19.6769061894304,15.4984900390297,124.91885633034)) ;
#35194 = CARTESIAN_POINT('Ctrl Pts',(-19.1967590474696,15.6985476365677,124.617705022532)) ;
#35195 = CARTESIAN_POINT('Ctrl Pts',(-19.1436360481896,15.5185585561579,124.919177517844)) ;
#35196 = CARTESIAN_POINT('Ctrl Pts',(-18.8003320264179,15.7183785095645,124.473760456347)) ;
#35197 = CARTESIAN_POINT('Ctrl Pts',(-18.6481039856048,15.5383894291547,124.73924884154)) ;
#35198 = CARTESIAN_POINT('Ctrl Pts',(-18.4747503929125,15.7383004203812,124.20293742243)) ;
#35199 = CARTESIAN_POINT('Ctrl Pts',(-18.2411262733989,15.5583113399714,124.400722475614)) ;
#35200 = CARTESIAN_POINT('Ctrl Pts',(-18.2610720953533,15.7582298638165,123.836921398904)) ;
#35201 = CARTESIAN_POINT('Ctrl Pts',(-17.9740267389869,15.5782407834067,123.943204335261)) ;
#35202 = CARTESIAN_POINT('Ctrl Pts',(-18.185068198707,15.7781395339329,123.420531358687)) ;
#35203 = CARTESIAN_POINT('Ctrl Pts',(-17.8790194222821,15.5981504535231,123.422718308583)) ;
#35204 = CARTESIAN_POINT('Ctrl Pts',(-18.2548638512684,15.7980128911957,123.003722761479)) ;
#35205 = CARTESIAN_POINT('Ctrl Pts',(-17.9662605747909,15.6180238107859,122.901708304032)) ;
#35206 = CARTESIAN_POINT('Ctrl Pts',(-18.4639568410273,15.8180044258137,122.633696412297)) ;
#35207 = CARTESIAN_POINT('Ctrl Pts',(-18.2276238438955,15.6380153454039,122.439173769106)) ;
#35208 = CARTESIAN_POINT('Ctrl Pts',(-18.7847146040937,15.8378700432244,122.358763046612)) ;
#35209 = CARTESIAN_POINT('Ctrl Pts',(-18.6285678008825,15.6578809628146,122.095505124919)) ;
#35210 = CARTESIAN_POINT('Ctrl Pts',(-19.182109206407,15.8578509730526,122.208558793697)) ;
#35211 = CARTESIAN_POINT('Ctrl Pts',(-19.1253095706603,15.6778618926428,121.907746173934)) ;
#35212 = CARTESIAN_POINT('Ctrl Pts',(-19.606033490729,15.8777894351358,122.203463863361)) ;
#35213 = CARTESIAN_POINT('Ctrl Pts',(-19.6552143908166,15.6978003547259,121.90137366034)) ;
#35214 = CARTESIAN_POINT('Ctrl Pts',(-20.0055761170638,15.8976816283575,122.342403399768)) ;
#35215 = CARTESIAN_POINT('Ctrl Pts',(-20.1546433032403,15.7176925479477,122.075043824331)) ;
#35216 = CARTESIAN_POINT('Ctrl Pts',(-20.3347791009066,15.9176523433929,122.61046686242)) ;
#35217 = CARTESIAN_POINT('Ctrl Pts',(-20.5661496332586,15.737663262983,122.410119645755)) ;
#35218 = CARTESIAN_POINT('Ctrl Pts',(-20.551706715397,15.937462015059,122.971635608473)) ;
#35219 = CARTESIAN_POINT('Ctrl Pts',(-20.83731237547,15.7574729346492,122.861577302678)) ;
#35220 = CARTESIAN_POINT('Ctrl Pts',(-20.6333723481961,15.9574552317502,123.388667733852)) ;
#35221 = CARTESIAN_POINT('Ctrl Pts',(-20.9393997365277,15.7774661513403,123.38286609659)) ;
#35222 = CARTESIAN_POINT('Ctrl Pts',(-20.5685874573327,15.9773061439465,123.805925874308)) ;
#35223 = CARTESIAN_POINT('Ctrl Pts',(-20.858421608188,15.7973170635367,123.904440437754)) ;
#35224 = CARTESIAN_POINT('Ctrl Pts',(-20.3629339575336,15.9973807502655,124.179831486359)) ;
#35225 = CARTESIAN_POINT('Ctrl Pts',(-20.6013666269511,15.8173916698557,124.371819409612)) ;
#35226 = CARTESIAN_POINT('Ctrl Pts',(-20.0986057487275,16.0138973821489,124.411216269807)) ;
#35227 = CARTESIAN_POINT('Ctrl Pts',(-20.2709357009448,15.833908301739,124.661071335377)) ;
#35228 = CARTESIAN_POINT('Ctrl Pts',(-19.8472305510429,16.027236089843,124.535405517903)) ;
#35229 = CARTESIAN_POINT('Ctrl Pts',(-19.9567400193942,15.8472470094331,124.816295037055)) ;
#35230 = CARTESIAN_POINT('Ctrl Pts',(-19.648689899929,16.0370784641513,124.593781061793)) ;
#35231 = CARTESIAN_POINT('Ctrl Pts',(-19.7085577801925,15.8570893837414,124.889269258824)) ;
#35232 = CARTESIAN_POINT('Ctrl Pts',(-19.4386553018546,16.047133484134,124.61748484339)) ;
#35233 = CARTESIAN_POINT('Ctrl Pts',(-19.4460289923746,15.8671444037242,124.918903925126)) ;
#35234 = CARTESIAN_POINT('Ctrl Pts',(-19.1610280376061,16.0603656407916,124.600218445625)) ;
#35235 = CARTESIAN_POINT('Ctrl Pts',(-19.0989283678052,15.8803765603817,124.897309206235)) ;
#35236 = CARTESIAN_POINT('Ctrl Pts',(-18.825889100884,16.0769806081367,124.488333617129)) ;
#35237 = CARTESIAN_POINT('Ctrl Pts',(-18.680086550185,15.8969915277269,124.757481852965)) ;
#35238 = CARTESIAN_POINT('Ctrl Pts',(-18.5495711916303,16.0935751951479,124.269005818189)) ;
#35239 = CARTESIAN_POINT('Ctrl Pts',(-18.3346327391999,15.9135861147381,124.483293406466)) ;
#35240 = CARTESIAN_POINT('Ctrl Pts',(-18.383354158807,16.1068087635033,124.045842736508)) ;
#35241 = CARTESIAN_POINT('Ctrl Pts',(-18.1268897361385,15.9268196830935,124.204366870093)) ;
#35242 = CARTESIAN_POINT('Ctrl Pts',(-18.2885245171761,16.1168523813119,123.857213437139)) ;
#35243 = CARTESIAN_POINT('Ctrl Pts',(-18.0083439444266,15.9368633009021,123.968576154178)) ;
#35244 = CARTESIAN_POINT('Ctrl Pts',(-18.2287506235429,16.1267393055468,123.658118953478)) ;
#35245 = CARTESIAN_POINT('Ctrl Pts',(-17.9336253681046,15.946750225137,123.719711066809)) ;
#35246 = CARTESIAN_POINT('Ctrl Pts',(-18.2038316638123,16.1367299599936,123.449583936804)) ;
#35247 = CARTESIAN_POINT('Ctrl Pts',(-17.9024744065146,15.9567408795837,123.459039355826)) ;
#35248 = CARTESIAN_POINT('Ctrl Pts',(-18.2155127325471,16.1466917184475,123.240472594879)) ;
#35249 = CARTESIAN_POINT('Ctrl Pts',(-17.9170694040816,15.9667026380377,123.197660756738)) ;
#35250 = CARTESIAN_POINT('Ctrl Pts',(-18.2792368886857,16.1600315835148,122.967353209043)) ;
#35251 = CARTESIAN_POINT('Ctrl Pts',(-17.9967391762759,15.9800425031049,122.856207482252)) ;
#35252 = CARTESIAN_POINT('Ctrl Pts',(-18.41302923077,16.1733403664281,122.718017566954)) ;
#35253 = CARTESIAN_POINT('Ctrl Pts',(-18.1639736695268,15.9933512860182,122.544568270946)) ;
#35254 = CARTESIAN_POINT('Ctrl Pts',(-18.6026009651151,16.1865361238721,122.515452306746)) ;
#35255 = CARTESIAN_POINT('Ctrl Pts',(-18.4009205226465,16.0065470434623,122.291373957954)) ;
#35256 = CARTESIAN_POINT('Ctrl Pts',(-18.7697316480871,16.1964980075486,122.389244608376)) ;
#35257 = CARTESIAN_POINT('Ctrl Pts',(-18.6098352781677,16.0165089271388,122.133609050734)) ;
#35258 = CARTESIAN_POINT('Ctrl Pts',(-18.9579132109796,16.2065411170633,122.293505577334)) ;
#35259 = CARTESIAN_POINT('Ctrl Pts',(-18.8450601919875,16.0265520366534,122.013933523756)) ;
#35260 = CARTESIAN_POINT('Ctrl Pts',(-19.1559583596013,16.2163933670625,122.232828073835)) ;
#35261 = CARTESIAN_POINT('Ctrl Pts',(-19.092616128857,16.0364042866527,121.938083702869)) ;
#35262 = CARTESIAN_POINT('Ctrl Pts',(-19.3639266023041,16.226364904013,122.20664426832)) ;
#35263 = CARTESIAN_POINT('Ctrl Pts',(-19.3525761374323,16.0463758236031,121.905351203631)) ;
#35264 = CARTESIAN_POINT('Ctrl Pts',(-19.5738352772956,16.2363601694905,122.217013254614)) ;
#35265 = CARTESIAN_POINT('Ctrl Pts',(-19.6149622143299,16.0563710890807,121.918309627784)) ;
#35266 = CARTESIAN_POINT('Ctrl Pts',(-19.7794415898056,16.2463941423641,122.264093918599)) ;
#35267 = CARTESIAN_POINT('Ctrl Pts',(-19.8719707676454,16.0664050619543,121.977157725159)) ;
#35268 = CARTESIAN_POINT('Ctrl Pts',(-19.9704548769762,16.2562495571265,122.344410165683)) ;
#35269 = CARTESIAN_POINT('Ctrl Pts',(-20.1107386746549,16.0762604767166,122.077550542913)) ;
#35270 = CARTESIAN_POINT('Ctrl Pts',(-20.1472714092236,16.2662488346353,122.458039635008)) ;
#35271 = CARTESIAN_POINT('Ctrl Pts',(-20.3317609231756,16.0862597542255,122.219585083256)) ;
#35272 = CARTESIAN_POINT('Ctrl Pts',(-20.3002692337498,16.2761440187983,122.599043469478)) ;
#35273 = CARTESIAN_POINT('Ctrl Pts',(-20.5230102658659,16.0961549383885,122.395838020229)) ;
#35274 = CARTESIAN_POINT('Ctrl Pts',(-20.4285086882037,16.2862043984391,122.767195696691)) ;
#35275 = CARTESIAN_POINT('Ctrl Pts',(-20.6833117694854,16.1062153180293,122.606026601001)) ;
#35276 = CARTESIAN_POINT('Ctrl Pts',(-20.5237070485476,16.2960542674472,122.951113827602)) ;
#35277 = CARTESIAN_POINT('Ctrl Pts',(-20.8023123453879,16.1160651870374,122.835923343439)) ;
#35278 = CARTESIAN_POINT('Ctrl Pts',(-20.5871150710927,16.3060858286551,123.152237015231)) ;
#35279 = CARTESIAN_POINT('Ctrl Pts',(-20.8815749659165,16.1260967482452,123.087326542216)) ;
#35280 = CARTESIAN_POINT('Ctrl Pts',(-20.6141638262457,16.3160962775374,123.360962196681)) ;
#35281 = CARTESIAN_POINT('Ctrl Pts',(-20.9153886456371,16.1361071971276,123.348232716797)) ;
#35282 = CARTESIAN_POINT('Ctrl Pts',(-20.6048907446535,16.3260030169544,123.569019571295)) ;
#35283 = CARTESIAN_POINT('Ctrl Pts',(-20.9038000062821,16.1460139365446,123.608304860469)) ;
#35284 = CARTESIAN_POINT('Ctrl Pts',(-20.5598881669259,16.3359410330228,123.773031366739)) ;
#35285 = CARTESIAN_POINT('Ctrl Pts',(-20.8475493443514,16.155951952613,123.863320444471)) ;
#35286 = CARTESIAN_POINT('Ctrl Pts',(-20.4797215293116,16.3459462794739,123.967521538131)) ;
#35287 = CARTESIAN_POINT('Ctrl Pts',(-20.7473434746321,16.1659571990641,124.106434248702)) ;
#35288 = CARTESIAN_POINT('Ctrl Pts',(-20.3663921716625,16.3559803405302,124.145428527425)) ;
#35289 = CARTESIAN_POINT('Ctrl Pts',(-20.6056840714309,16.1759912601204,124.328819428223)) ;
#35290 = CARTESIAN_POINT('Ctrl Pts',(-20.2268261020098,16.3658254215884,124.29828451982)) ;
#35291 = CARTESIAN_POINT('Ctrl Pts',(-20.4312280688976,16.1858363411786,124.519891626443)) ;
#35292 = CARTESIAN_POINT('Ctrl Pts',(-20.0607710857715,16.3758112275419,124.42667346357)) ;
#35293 = CARTESIAN_POINT('Ctrl Pts',(-20.2236607635386,16.1958221471321,124.680379963882)) ;
#35294 = CARTESIAN_POINT('Ctrl Pts',(-19.8759009892187,16.3857460480961,124.523947203319)) ;
#35295 = CARTESIAN_POINT('Ctrl Pts',(-19.992574051782,16.2057569676862,124.801974564884)) ;
#35296 = CARTESIAN_POINT('Ctrl Pts',(-19.6745001645774,16.3958035732283,124.588229437951)) ;
#35297 = CARTESIAN_POINT('Ctrl Pts',(-19.740823924335,16.2158144928185,124.882329808667)) ;
#35298 = CARTESIAN_POINT('Ctrl Pts',(-19.4699018787836,16.4056252238796,124.616221674398)) ;
#35299 = CARTESIAN_POINT('Ctrl Pts',(-19.4850756391592,16.2256361434698,124.917322735198)) ;
#35300 = CARTESIAN_POINT('Ctrl Pts',(-19.2586509012011,16.4156812873844,124.608469860798)) ;
#35301 = CARTESIAN_POINT('Ctrl Pts',(-19.221011935614,16.2356922069746,124.907635447908)) ;
#35302 = CARTESIAN_POINT('Ctrl Pts',(-19.0543812444969,16.4256219544483,124.56429049855)) ;
#35303 = CARTESIAN_POINT('Ctrl Pts',(-18.9656740001609,16.2456328740385,124.852413667888)) ;
#35304 = CARTESIAN_POINT('Ctrl Pts',(-18.861349537296,16.4355263481143,124.486210004502)) ;
#35305 = CARTESIAN_POINT('Ctrl Pts',(-18.7243829673622,16.2555372677045,124.754815092922)) ;
#35306 = CARTESIAN_POINT('Ctrl Pts',(-18.6823656137702,16.4455728718773,124.374110855955)) ;
#35307 = CARTESIAN_POINT('Ctrl Pts',(-18.5006518514753,16.2655837914675,124.614693286705)) ;
#35308 = CARTESIAN_POINT('Ctrl Pts',(-18.5277366886048,16.4554689548937,124.234866899934)) ;
#35309 = CARTESIAN_POINT('Ctrl Pts',(-18.3073636532671,16.2754798744839,124.44063973377)) ;
#35310 = CARTESIAN_POINT('Ctrl Pts',(-18.397512504775,16.4655356541237,124.068090149014)) ;
#35311 = CARTESIAN_POINT('Ctrl Pts',(-18.1445816441947,16.2855465737139,124.232170442809)) ;
#35312 = CARTESIAN_POINT('Ctrl Pts',(-18.3003784994557,16.4753592645248,123.885799724295)) ;
#35313 = CARTESIAN_POINT('Ctrl Pts',(-18.0231616074264,16.2953701841149,124.004307682012)) ;
#35314 = CARTESIAN_POINT('Ctrl Pts',(-18.2345231615704,16.4854151247023,123.684941160413)) ;
#35315 = CARTESIAN_POINT('Ctrl Pts',(-17.9408403239872,16.3054260442924,123.753235338672)) ;
#35316 = CARTESIAN_POINT('Ctrl Pts',(-18.2051689662618,16.4953482710072,123.478162940321)) ;
#35317 = CARTESIAN_POINT('Ctrl Pts',(-17.9041452012384,16.3153591905974,123.494762458896)) ;
#35318 = CARTESIAN_POINT('Ctrl Pts',(-18.2117436428783,16.5052935267778,123.269210161589)) ;
#35319 = CARTESIAN_POINT('Ctrl Pts',(-17.9123613232578,16.325304446368,123.233570994395)) ;
#35320 = CARTESIAN_POINT('Ctrl Pts',(-18.2545082390918,16.5152768252163,123.063705916951)) ;
#35321 = CARTESIAN_POINT('Ctrl Pts',(-17.9658149649303,16.3352877448065,122.976690048521)) ;
#35322 = CARTESIAN_POINT('Ctrl Pts',(-18.3329769113409,16.5253140053629,122.867842390834)) ;
#35323 = CARTESIAN_POINT('Ctrl Pts',(-18.0638986665553,16.3453249249531,122.731859880821)) ;
#35324 = CARTESIAN_POINT('Ctrl Pts',(-18.4419820599427,16.5351685580724,122.691641388023)) ;
#35325 = CARTESIAN_POINT('Ctrl Pts',(-18.2001537296948,16.3551794776626,122.511606700081)) ;
#35326 = CARTESIAN_POINT('Ctrl Pts',(-18.581699061968,16.5451680765197,122.534616193338)) ;
#35327 = CARTESIAN_POINT('Ctrl Pts',(-18.3747984970513,16.3651789961099,122.315323705835)) ;
#35328 = CARTESIAN_POINT('Ctrl Pts',(-18.7447549291817,16.5550631589818,122.405380089369)) ;
#35329 = CARTESIAN_POINT('Ctrl Pts',(-18.578617637937,16.3750740785719,122.153776522229)) ;
#35330 = CARTESIAN_POINT('Ctrl Pts',(-18.9307890892371,16.5651237044879,122.304812169695)) ;
#35331 = CARTESIAN_POINT('Ctrl Pts',(-18.8111591522384,16.3851346240781,122.028064932937)) ;
#35332 = CARTESIAN_POINT('Ctrl Pts',(-19.1272493004739,16.5749730117359,122.239351514005)) ;
#35333 = CARTESIAN_POINT('Ctrl Pts',(-19.0567347651513,16.3949839313261,121.946236873257)) ;
#35334 = CARTESIAN_POINT('Ctrl Pts',(-19.3356895472675,16.5850001018232,122.207921910754)) ;
#35335 = CARTESIAN_POINT('Ctrl Pts',(-19.317284759462,16.4050110214134,121.906948036718)) ;
#35336 = CARTESIAN_POINT('Ctrl Pts',(-19.5464580747962,16.5950290059602,122.213723078869)) ;
#35337 = CARTESIAN_POINT('Ctrl Pts',(-19.5807454043867,16.4150399255504,121.914197470352)) ;
#35338 = CARTESIAN_POINT('Ctrl Pts',(-19.7492714933066,16.6048728710595,122.254846303391)) ;
#35339 = CARTESIAN_POINT('Ctrl Pts',(-19.8342636546969,16.4248837906497,121.965599859019)) ;
#35340 = CARTESIAN_POINT('Ctrl Pts',(-19.9450340387056,16.6148686977679,122.331249053741)) ;
#35341 = CARTESIAN_POINT('Ctrl Pts',(-20.0789676317577,16.4348796173581,122.06110173883)) ;
#35342 = CARTESIAN_POINT('Ctrl Pts',(-20.1248865780728,16.6248939144169,122.441136839792)) ;
#35343 = CARTESIAN_POINT('Ctrl Pts',(-20.3037842342036,16.4449048340071,122.198459857555)) ;
#35344 = CARTESIAN_POINT('Ctrl Pts',(-20.28097718897,16.6347837465745,122.57849001676)) ;
#35345 = CARTESIAN_POINT('Ctrl Pts',(-20.4988993121672,16.4547946661646,122.370150559319)) ;
#35346 = CARTESIAN_POINT('Ctrl Pts',(-20.4123923595961,16.6447746026592,122.742330187419)) ;
#35347 = CARTESIAN_POINT('Ctrl Pts',(-20.663169704395,16.4647855222494,122.574949866222)) ;
#35348 = CARTESIAN_POINT('Ctrl Pts',(-20.5128694027826,16.6547196972521,122.925680754585)) ;
#35349 = CARTESIAN_POINT('Ctrl Pts',(-20.7887677401165,16.4747306168422,122.804137700904)) ;
#35350 = CARTESIAN_POINT('Ctrl Pts',(-20.5804045472884,16.6646716010202,123.12370981409)) ;
#35351 = CARTESIAN_POINT('Ctrl Pts',(-20.8731883104947,16.4846825206104,123.05167397304)) ;
#35352 = CARTESIAN_POINT('Ctrl Pts',(-20.6126176827345,16.6747080004896,123.332227708226)) ;
#35353 = CARTESIAN_POINT('Ctrl Pts',(-20.9134563189701,16.4947189200798,123.312320962723)) ;
#35354 = CARTESIAN_POINT('Ctrl Pts',(-20.6083540179915,16.6845970705783,123.540090086078)) ;
#35355 = CARTESIAN_POINT('Ctrl Pts',(-20.9081282977021,16.5046079901685,123.572149884736)) ;
#35356 = CARTESIAN_POINT('Ctrl Pts',(-20.5680279223368,16.6945863599492,123.746183169029)) ;
#35357 = CARTESIAN_POINT('Ctrl Pts',(-20.8577220599026,16.5145972795394,123.829766727651)) ;
#35358 = CARTESIAN_POINT('Ctrl Pts',(-20.4926169706463,16.7045449261589,123.941483709514)) ;
#35359 = CARTESIAN_POINT('Ctrl Pts',(-20.7634596189807,16.5245558457491,124.073893349029)) ;
#35360 = CARTESIAN_POINT('Ctrl Pts',(-20.3855116246943,16.7144444973757,124.119942910735)) ;
#35361 = CARTESIAN_POINT('Ctrl Pts',(-20.6295786199548,16.5344554169658,124.29696878482)) ;
#35362 = CARTESIAN_POINT('Ctrl Pts',(-20.2469681262543,16.7244924117899,124.279374314369)) ;
#35363 = CARTESIAN_POINT('Ctrl Pts',(-20.4564004098942,16.5445033313801,124.496258761837)) ;
#35364 = CARTESIAN_POINT('Ctrl Pts',(-20.0853998211911,16.7343877546505,124.410470530884)) ;
#35365 = CARTESIAN_POINT('Ctrl Pts',(-20.2544401348051,16.5543986742407,124.660130610511)) ;
#35366 = CARTESIAN_POINT('Ctrl Pts',(-19.9005296097113,16.7444494485979,124.513218405503)) ;
#35367 = CARTESIAN_POINT('Ctrl Pts',(-20.0233532789504,16.5644603681881,124.78856641835)) ;
#35368 = CARTESIAN_POINT('Ctrl Pts',(-19.7049244472247,16.7542939016821,124.580859195891)) ;
#35369 = CARTESIAN_POINT('Ctrl Pts',(-19.7788459931225,16.5743048212723,124.873119039316)) ;
#35370 = CARTESIAN_POINT('Ctrl Pts',(-19.4982683090675,16.7642545866405,124.614617061562)) ;
#35371 = CARTESIAN_POINT('Ctrl Pts',(-19.520525537516,16.5842655062307,124.915317434052)) ;
#35372 = CARTESIAN_POINT('Ctrl Pts',(-19.2872959543148,16.7742905191491,124.611604709264)) ;
#35373 = CARTESIAN_POINT('Ctrl Pts',(-19.256810212926,16.5943014387393,124.911553126571)) ;
#35374 = CARTESIAN_POINT('Ctrl Pts',(-19.083065641411,16.7841791348371,124.572793885594)) ;
#35375 = CARTESIAN_POINT('Ctrl Pts',(-19.0015211293755,16.6041900544273,124.863040443371)) ;
#35376 = CARTESIAN_POINT('Ctrl Pts',(-18.8860375470221,16.7941935439796,124.498559615146)) ;
#35377 = CARTESIAN_POINT('Ctrl Pts',(-18.755235682163,16.6142044635698,124.770248444089)) ;
#35378 = CARTESIAN_POINT('Ctrl Pts',(-18.7048442029777,16.8042273529374,124.390576815252)) ;
#35379 = CARTESIAN_POINT('Ctrl Pts',(-18.5287435554277,16.6242382725276,124.635270964775)) ;
#35380 = CARTESIAN_POINT('Ctrl Pts',(-18.5479851568458,16.8140578071936,124.255979370359)) ;
#35381 = CARTESIAN_POINT('Ctrl Pts',(-18.3326680458869,16.6340687267837,124.467023867627)) ;
#35382 = CARTESIAN_POINT('Ctrl Pts',(-18.4135706987232,16.8241354747718,124.092266151809)) ;
#35383 = CARTESIAN_POINT('Ctrl Pts',(-18.1646495930641,16.644146394362,124.262383242849)) ;
#35384 = CARTESIAN_POINT('Ctrl Pts',(-18.3118178527469,16.833987342894,123.911815748702)) ;
#35385 = CARTESIAN_POINT('Ctrl Pts',(-18.0374571776765,16.6539982624842,124.036819495962)) ;
#35386 = CARTESIAN_POINT('Ctrl Pts',(-18.2412580423385,16.8440603804594,123.712187854895)) ;
#35387 = CARTESIAN_POINT('Ctrl Pts',(-17.9492568482379,16.6640713000495,123.787285292021)) ;
#35388 = CARTESIAN_POINT('Ctrl Pts',(-18.2072505630093,16.8539029338102,123.508062557237)) ;
#35389 = CARTESIAN_POINT('Ctrl Pts',(-17.9067465101857,16.6739138534004,123.532127399556)) ;
#35390 = CARTESIAN_POINT('Ctrl Pts',(-18.2085239591176,16.8638833293037,123.298256187537)) ;
#35391 = CARTESIAN_POINT('Ctrl Pts',(-17.9083377642427,16.6838942488938,123.269869124287)) ;
#35392 = CARTESIAN_POINT('Ctrl Pts',(-18.2467556082462,16.8739018072815,123.091139951509)) ;
#35393 = CARTESIAN_POINT('Ctrl Pts',(-17.9561266808108,16.6939127268717,123.01097372099)) ;
#35394 = CARTESIAN_POINT('Ctrl Pts',(-18.3189697446899,16.8837851215876,122.896288022926)) ;
#35395 = CARTESIAN_POINT('Ctrl Pts',(-18.0463942839959,16.7037960411777,122.767407615418)) ;
#35396 = CARTESIAN_POINT('Ctrl Pts',(-18.425934681268,16.8938534241263,122.713676624745)) ;
#35397 = CARTESIAN_POINT('Ctrl Pts',(-18.180099801531,16.7138643437165,122.539143460638)) ;
#35398 = CARTESIAN_POINT('Ctrl Pts',(-18.5595970562926,16.9036834713997,122.556016451482)) ;
#35399 = CARTESIAN_POINT('Ctrl Pts',(-18.3471784468663,16.7236943909899,122.342066798558)) ;
#35400 = CARTESIAN_POINT('Ctrl Pts',(-18.722208363347,16.9137503428152,122.42061719112)) ;
#35401 = CARTESIAN_POINT('Ctrl Pts',(-18.5504420735464,16.7337612624054,122.172817736583)) ;
#35402 = CARTESIAN_POINT('Ctrl Pts',(-18.9027264908965,16.9236393816143,122.317430530049)) ;
#35403 = CARTESIAN_POINT('Ctrl Pts',(-18.7760904676287,16.7436503012044,122.043833574467)) ;
#35404 = CARTESIAN_POINT('Ctrl Pts',(-19.1003612730022,16.9336360797484,122.246020456028)) ;
#35405 = CARTESIAN_POINT('Ctrl Pts',(-19.0231340622893,16.7536469993385,121.954570731794)) ;
#35406 = CARTESIAN_POINT('Ctrl Pts',(-19.3065267658046,16.9435885054603,122.210251377386)) ;
#35407 = CARTESIAN_POINT('Ctrl Pts',(-19.280841415143,16.7635994250505,121.909859064131)) ;
#35408 = CARTESIAN_POINT('Ctrl Pts',(-19.5155081682475,16.9535298076933,122.210531944557)) ;
#35409 = CARTESIAN_POINT('Ctrl Pts',(-19.5420687998033,16.7735407272835,121.910209653744)) ;
#35410 = CARTESIAN_POINT('Ctrl Pts',(-19.7222133629213,16.9635130467772,122.24703377313)) ;
#35411 = CARTESIAN_POINT('Ctrl Pts',(-19.8004505578653,16.7835239663674,121.955836958288)) ;
#35412 = CARTESIAN_POINT('Ctrl Pts',(-19.9203861587656,16.9735518483458,122.319565863544)) ;
#35413 = CARTESIAN_POINT('Ctrl Pts',(-20.0481664431419,16.793562767936,122.046501857169)) ;
#35414 = CARTESIAN_POINT('Ctrl Pts',(-20.0997203161893,16.9833999544674,122.423063092642)) ;
#35415 = CARTESIAN_POINT('Ctrl Pts',(-20.272335374715,16.8034108740576,122.175874105988)) ;
#35416 = CARTESIAN_POINT('Ctrl Pts',(-20.2618757976447,16.9934601500428,122.558817396899)) ;
#35417 = CARTESIAN_POINT('Ctrl Pts',(-20.4750293999112,16.813471069633,122.34556681789)) ;
#35418 = CARTESIAN_POINT('Ctrl Pts',(-20.3956688355369,17.0033578333542,122.718192247894)) ;
#35419 = CARTESIAN_POINT('Ctrl Pts',(-20.6422713391214,16.8233687529444,122.544786148039)) ;
#35420 = CARTESIAN_POINT('Ctrl Pts',(-20.5006942150535,17.0132888737282,122.898630233536)) ;
#35421 = CARTESIAN_POINT('Ctrl Pts',(-20.7735531877414,16.8332997933184,122.770334392625)) ;
#35422 = CARTESIAN_POINT('Ctrl Pts',(-20.5733879414346,17.0233310913848,123.096836226167)) ;
#35423 = CARTESIAN_POINT('Ctrl Pts',(-20.8644201008699,16.843342010975,123.018091751104)) ;
#35424 = CARTESIAN_POINT('Ctrl Pts',(-20.61013604455,17.0332177521188,123.301420117355)) ;
#35425 = CARTESIAN_POINT('Ctrl Pts',(-20.9103551820702,16.853228671709,123.273822727996)) ;
#35426 = CARTESIAN_POINT('Ctrl Pts',(-20.6111628873651,17.0432108607212,123.511493426387)) ;
#35427 = CARTESIAN_POINT('Ctrl Pts',(-20.9116383536985,16.8632217803114,123.536414570105)) ;
#35428 = CARTESIAN_POINT('Ctrl Pts',(-20.5757869989794,17.0531565593595,123.717568908306)) ;
#35429 = CARTESIAN_POINT('Ctrl Pts',(-20.8674180472619,16.8731674789497,123.794009449911)) ;
#35430 = CARTESIAN_POINT('Ctrl Pts',(-20.5055557491606,17.0631037816305,123.91455588214)) ;
#35431 = CARTESIAN_POINT('Ctrl Pts',(-20.7796283028681,16.8831147012207,124.040243534273)) ;
#35432 = CARTESIAN_POINT('Ctrl Pts',(-20.400941475518,17.0731518072107,124.098065903988)) ;
#35433 = CARTESIAN_POINT('Ctrl Pts',(-20.6488602157031,16.8931627268008,124.269630633143)) ;
#35434 = CARTESIAN_POINT('Ctrl Pts',(-20.2688802244909,17.0829990543536,124.257492396339)) ;
#35435 = CARTESIAN_POINT('Ctrl Pts',(-20.4837823786793,16.9030099739437,124.46891451259)) ;
#35436 = CARTESIAN_POINT('Ctrl Pts',(-20.1097187274717,17.0929622314443,124.39364708618)) ;
#35437 = CARTESIAN_POINT('Ctrl Pts',(-20.2848296698449,16.9129731510345,124.639107596635)) ;
#35438 = CARTESIAN_POINT('Ctrl Pts',(-19.9279652479733,17.1029919524777,124.500535991782)) ;
#35439 = CARTESIAN_POINT('Ctrl Pts',(-20.0576375878004,16.9230028720679,124.772718134016)) ;
#35440 = CARTESIAN_POINT('Ctrl Pts',(-19.7329501884367,17.1128964200106,124.573568512816)) ;
#35441 = CARTESIAN_POINT('Ctrl Pts',(-19.8138676647044,16.9329073396008,124.864008421911)) ;
#35442 = CARTESIAN_POINT('Ctrl Pts',(-19.5257911753333,17.1229209058404,124.612154491612)) ;
#35443 = CARTESIAN_POINT('Ctrl Pts',(-19.5549188176483,16.9429318254305,124.912240141171)) ;
#35444 = CARTESIAN_POINT('Ctrl Pts',(-19.31756391383,17.1328247409643,124.61433347866)) ;
#35445 = CARTESIAN_POINT('Ctrl Pts',(-19.2946338276939,16.9528356605544,124.914963066567)) ;
#35446 = CARTESIAN_POINT('Ctrl Pts',(-19.1091090081414,17.1428759316743,124.579872920246)) ;
#35447 = CARTESIAN_POINT('Ctrl Pts',(-19.0340655772847,16.9628868512645,124.871886584531)) ;
#35448 = CARTESIAN_POINT('Ctrl Pts',(-18.9130563367156,17.1527603743326,124.510927123554)) ;
#35449 = CARTESIAN_POINT('Ctrl Pts',(-18.7889990252693,16.9727712939228,124.785703184487)) ;
#35450 = CARTESIAN_POINT('Ctrl Pts',(-18.7298067492815,17.1627533821844,124.408227429551)) ;
#35451 = CARTESIAN_POINT('Ctrl Pts',(-18.5599373548678,16.9827643017746,124.657327597642)) ;
#35452 = CARTESIAN_POINT('Ctrl Pts',(-18.5679203831117,17.1727017019007,124.275788607794)) ;
#35453 = CARTESIAN_POINT('Ctrl Pts',(-18.3575795914543,16.9927126214909,124.491777975057)) ;
#35454 = CARTESIAN_POINT('Ctrl Pts',(-18.4314404984795,17.1826385406102,124.117654900574)) ;
#35455 = CARTESIAN_POINT('Ctrl Pts',(-18.1869801387972,17.0026494602004,124.294109650158)) ;
#35456 = CARTESIAN_POINT('Ctrl Pts',(-18.3237434951537,17.1926215295298,123.937489058372)) ;
#35457 = CARTESIAN_POINT('Ctrl Pts',(-18.0523597653878,17.0126324491199,124.068901521774)) ;
#35458 = CARTESIAN_POINT('Ctrl Pts',(-18.2488910018654,17.2026654088939,123.740073906393)) ;
#35459 = CARTESIAN_POINT('Ctrl Pts',(-17.9587951854012,17.022676328484,123.822132392041)) ;
#35460 = CARTESIAN_POINT('Ctrl Pts',(-18.2098074279025,17.2124934742523,123.537154265796)) ;
#35461 = CARTESIAN_POINT('Ctrl Pts',(-17.909941640764,17.0325043938425,123.568481191402)) ;
#35462 = CARTESIAN_POINT('Ctrl Pts',(-18.2063795196312,17.2225705628072,123.325376725486)) ;
#35463 = CARTESIAN_POINT('Ctrl Pts',(-17.9056580144005,17.0425814823974,123.303759681479)) ;
#35464 = CARTESIAN_POINT('Ctrl Pts',(-18.2389039387934,17.2324207149635,123.120811528731)) ;
#35465 = CARTESIAN_POINT('Ctrl Pts',(-17.94631501662,17.0524316345537,123.048052157432)) ;
#35466 = CARTESIAN_POINT('Ctrl Pts',(-18.3079172661289,17.2425011954158,122.920496194751)) ;
#35467 = CARTESIAN_POINT('Ctrl Pts',(-18.0325827863602,17.062512115006,122.797658849557)) ;
#35468 = CARTESIAN_POINT('Ctrl Pts',(-18.4078418322244,17.2523156931847,122.739922505072)) ;
#35469 = CARTESIAN_POINT('Ctrl Pts',(-18.1574904407199,17.0723266127749,122.571941098785)) ;
#35470 = CARTESIAN_POINT('Ctrl Pts',(-18.5406376489348,17.2623839892048,122.575157598147)) ;
#35471 = CARTESIAN_POINT('Ctrl Pts',(-18.3234861663254,17.082394908795,122.365986190106)) ;
#35472 = CARTESIAN_POINT('Ctrl Pts',(-18.6974563857139,17.2722828216876,122.43827365892)) ;
#35473 = CARTESIAN_POINT('Ctrl Pts',(-18.5195111942605,17.0922937412777,122.194881832849)) ;
#35474 = CARTESIAN_POINT('Ctrl Pts',(-18.878314400253,17.2823357017021,122.329011502217)) ;
#35475 = CARTESIAN_POINT('Ctrl Pts',(-18.7455842875556,17.1023466212923,122.058305557844)) ;
#35476 = CARTESIAN_POINT('Ctrl Pts',(-19.0718160918219,17.2922055171983,122.253987097039)) ;
#35477 = CARTESIAN_POINT('Ctrl Pts',(-18.9874629412771,17.1122164367885,121.964526142738)) ;
#35478 = CARTESIAN_POINT('Ctrl Pts',(-19.2795008716947,17.3022781982811,122.212830255507)) ;
#35479 = CARTESIAN_POINT('Ctrl Pts',(-19.2470688770151,17.1222891178713,121.913081725727)) ;
#35480 = CARTESIAN_POINT('Ctrl Pts',(-19.4861827851385,17.312110676852,122.208383210554)) ;
#35481 = CARTESIAN_POINT('Ctrl Pts',(-19.505422587491,17.1321215964422,121.907524514954)) ;
#35482 = CARTESIAN_POINT('Ctrl Pts',(-19.6946785789896,17.3221413108381,122.23992020577)) ;
#35483 = CARTESIAN_POINT('Ctrl Pts',(-19.7660419705,17.1421522304283,121.94694754642)) ;
#35484 = CARTESIAN_POINT('Ctrl Pts',(-19.8943714717527,17.3321728680573,122.307777090262)) ;
#35485 = CARTESIAN_POINT('Ctrl Pts',(-20.0156574865041,17.1521837876475,122.031770158995)) ;
#35486 = CARTESIAN_POINT('Ctrl Pts',(-20.0757133418564,17.342002576929,122.406842625941)) ;
#35487 = CARTESIAN_POINT('Ctrl Pts',(-20.24233509567,17.1620134965191,122.155604235023)) ;
#35488 = CARTESIAN_POINT('Ctrl Pts',(-20.2401293619726,17.3519920257311,122.53751027012)) ;
#35489 = CARTESIAN_POINT('Ctrl Pts',(-20.447854041674,17.1720029453212,122.318940433041)) ;
#35490 = CARTESIAN_POINT('Ctrl Pts',(-20.3797110879383,17.3620358781311,122.695945873639)) ;
#35491 = CARTESIAN_POINT('Ctrl Pts',(-20.6223297570002,17.1820467977213,122.51698601017)) ;
#35492 = CARTESIAN_POINT('Ctrl Pts',(-20.4875963394876,17.3718575914632,122.872002282074)) ;
#35493 = CARTESIAN_POINT('Ctrl Pts',(-20.7571853343679,17.1918685110533,122.737058592074)) ;
#35494 = CARTESIAN_POINT('Ctrl Pts',(-20.565398754166,17.3818925964519,123.068098579527)) ;
#35495 = CARTESIAN_POINT('Ctrl Pts',(-20.8544363835335,17.2019035160421,122.982179630629)) ;
#35496 = CARTESIAN_POINT('Ctrl Pts',(-20.6073560537494,17.3919174348995,123.274640875661)) ;
#35497 = CARTESIAN_POINT('Ctrl Pts',(-20.9068811374708,17.2119283544897,123.240357855684)) ;
#35498 = CARTESIAN_POINT('Ctrl Pts',(-20.6131626095599,17.4017696478547,123.481683897343)) ;
#35499 = CARTESIAN_POINT('Ctrl Pts',(-20.9141373279867,17.2217805674449,123.499162698655)) ;
#35500 = CARTESIAN_POINT('Ctrl Pts',(-20.5828638631299,17.4117596040485,123.689490947812)) ;
#35501 = CARTESIAN_POINT('Ctrl Pts',(-20.8762617533052,17.2317705236386,123.758921385057)) ;
#35502 = CARTESIAN_POINT('Ctrl Pts',(-20.5173607069601,17.4216877143317,123.887673199299)) ;
#35503 = CARTESIAN_POINT('Ctrl Pts',(-20.7943806136614,17.2416986339219,124.006649024924)) ;
#35504 = CARTESIAN_POINT('Ctrl Pts',(-20.4181341555085,17.4316763144113,124.072748693797)) ;
#35505 = CARTESIAN_POINT('Ctrl Pts',(-20.6703453852788,17.2516872340014,124.237992487167)) ;
#35506 = CARTESIAN_POINT('Ctrl Pts',(-20.2875580116088,17.4417029063388,124.238230031649)) ;
#35507 = CARTESIAN_POINT('Ctrl Pts',(-20.5071235398505,17.2617138259289,124.44484280022)) ;
#35508 = CARTESIAN_POINT('Ctrl Pts',(-20.1326042864627,17.451588034403,124.376702910318)) ;
#35509 = CARTESIAN_POINT('Ctrl Pts',(-20.3134293623921,17.2715989539931,124.617932747041)) ;
#35510 = CARTESIAN_POINT('Ctrl Pts',(-19.9543077801982,17.4615791518765,124.487754355148)) ;
#35511 = CARTESIAN_POINT('Ctrl Pts',(-20.090557366876,17.2815900714667,124.756745161421)) ;
#35512 = CARTESIAN_POINT('Ctrl Pts',(-19.7583141539382,17.4716197677283,124.566132788164)) ;
#35513 = CARTESIAN_POINT('Ctrl Pts',(-19.8455645964528,17.2916306873184,124.854716110679)) ;
#35514 = CARTESIAN_POINT('Ctrl Pts',(-19.5560340189507,17.481452758582,124.608731196182)) ;
#35515 = CARTESIAN_POINT('Ctrl Pts',(-19.5927130154579,17.3014636781722,124.90796206647)) ;
#35516 = CARTESIAN_POINT('Ctrl Pts',(-19.3460857373288,17.4914458900323,124.61627350105)) ;
#35517 = CARTESIAN_POINT('Ctrl Pts',(-19.3302774501978,17.3114568096224,124.917387511102)) ;
#35518 = CARTESIAN_POINT('Ctrl Pts',(-19.1372544365684,17.5014779384677,124.586697623401)) ;
#35519 = CARTESIAN_POINT('Ctrl Pts',(-19.0692386893075,17.3214888580579,124.880415353166)) ;
#35520 = CARTESIAN_POINT('Ctrl Pts',(-18.9400052555549,17.5113431850101,124.522647715946)) ;
#35521 = CARTESIAN_POINT('Ctrl Pts',(-18.8226772574824,17.3313541046003,124.800350459947)) ;
#35522 = CARTESIAN_POINT('Ctrl Pts',(-18.7547863337693,17.5213050598369,124.424885268183)) ;
#35523 = CARTESIAN_POINT('Ctrl Pts',(-18.5911545600196,17.3413159794271,124.678145049342)) ;
#35524 = CARTESIAN_POINT('Ctrl Pts',(-18.5883681930039,17.5313400229482,124.295243637519)) ;
#35525 = CARTESIAN_POINT('Ctrl Pts',(-18.3831334191365,17.3513509425383,124.516091097568)) ;
#35526 = CARTESIAN_POINT('Ctrl Pts',(-18.4488134106994,17.5412248674106,124.141223324118)) ;
#35527 = CARTESIAN_POINT('Ctrl Pts',(-18.2086914289876,17.3612357870008,124.323563591866)) ;
#35528 = CARTESIAN_POINT('Ctrl Pts',(-18.3361743130609,17.5512909202513,123.962114608032)) ;
#35529 = CARTESIAN_POINT('Ctrl Pts',(-18.0678947666069,17.3713018398415,124.099676485574)) ;
#35530 = CARTESIAN_POINT('Ctrl Pts',(-18.2579149300862,17.5611284361603,123.770636276305)) ;
#35531 = CARTESIAN_POINT('Ctrl Pts',(-17.9700726313158,17.3811393557505,123.860326944407)) ;
#35532 = CARTESIAN_POINT('Ctrl Pts',(-18.2128572603931,17.5711971842692,123.563847910291)) ;
#35533 = CARTESIAN_POINT('Ctrl Pts',(-17.9137531150226,17.3912081038593,123.601841075216)) ;
#35534 = CARTESIAN_POINT('Ctrl Pts',(-18.2046218359309,17.5810777013002,123.356259866829)) ;
#35535 = CARTESIAN_POINT('Ctrl Pts',(-17.9034613927267,17.4010886208904,123.342355402498)) ;
#35536 = CARTESIAN_POINT('Ctrl Pts',(-18.2324382002903,17.5910688882346,123.148094680984)) ;
#35537 = CARTESIAN_POINT('Ctrl Pts',(-17.938234492748,17.4110798078248,123.082149155365)) ;
#35538 = CARTESIAN_POINT('Ctrl Pts',(-18.2957212303086,17.6010219545096,122.948615518676)) ;
#35539 = CARTESIAN_POINT('Ctrl Pts',(-18.0173408798839,17.4210328740997,122.832800782662)) ;
#35540 = CARTESIAN_POINT('Ctrl Pts',(-18.3935237813903,17.6110577920422,122.761687553403)) ;
#35541 = CARTESIAN_POINT('Ctrl Pts',(-18.139596406472,17.4310687116323,122.599142062299)) ;
#35542 = CARTESIAN_POINT('Ctrl Pts',(-18.5203340583895,17.6209479182536,122.596896263532)) ;
#35543 = CARTESIAN_POINT('Ctrl Pts',(-18.2981116221093,17.4409588378438,122.393154239506)) ;
#35544 = CARTESIAN_POINT('Ctrl Pts',(-18.6751694912199,17.6309401001616,122.454946682161)) ;
#35545 = CARTESIAN_POINT('Ctrl Pts',(-18.4916578231094,17.4509510197518,122.21571919075)) ;
#35546 = CARTESIAN_POINT('Ctrl Pts',(-18.8515274887847,17.6408860401002,122.342614062486)) ;
#35547 = CARTESIAN_POINT('Ctrl Pts',(-18.7121069675816,17.4608969596903,122.07530556897)) ;
#35548 = CARTESIAN_POINT('Ctrl Pts',(-19.0445828832562,17.6508332238642,122.262203190812)) ;
#35549 = CARTESIAN_POINT('Ctrl Pts',(-18.953427454247,17.4708441434544,121.974794440386)) ;
#35550 = CARTESIAN_POINT('Ctrl Pts',(-19.2507687647506,17.6608811621717,122.21630679009)) ;
#35551 = CARTESIAN_POINT('Ctrl Pts',(-19.2111603866877,17.4808920817619,121.917426601143)) ;
#35552 = CARTESIAN_POINT('Ctrl Pts',(-19.4575859789318,17.670728796912,122.206920104581)) ;
#35553 = CARTESIAN_POINT('Ctrl Pts',(-19.4696824314126,17.4907397165021,121.905695967062)) ;
#35554 = CARTESIAN_POINT('Ctrl Pts',(-19.6653420100825,17.6806905108858,122.233242738369)) ;
#35555 = CARTESIAN_POINT('Ctrl Pts',(-19.7293772424128,17.500701430476,121.938602055707)) ;
#35556 = CARTESIAN_POINT('Ctrl Pts',(-19.8666582474384,17.6907191456766,122.295917378937)) ;
#35557 = CARTESIAN_POINT('Ctrl Pts',(-19.9810217546006,17.5107300652668,122.01694801998)) ;
#35558 = CARTESIAN_POINT('Ctrl Pts',(-20.0518343532791,17.7006294642738,122.391384008924)) ;
#35559 = CARTESIAN_POINT('Ctrl Pts',(-20.2124907996751,17.5206403838639,122.13628388166)) ;
#35560 = CARTESIAN_POINT('Ctrl Pts',(-20.2183778744694,17.7105643205853,122.517438880118)) ;
#35561 = CARTESIAN_POINT('Ctrl Pts',(-20.4206686080911,17.5305752401755,122.293854796861)) ;
#35562 = CARTESIAN_POINT('Ctrl Pts',(-20.3618650760254,17.720605556546,122.672260820024)) ;
#35563 = CARTESIAN_POINT('Ctrl Pts',(-20.6000255829358,17.5406164761362,122.487384162128)) ;
#35564 = CARTESIAN_POINT('Ctrl Pts',(-20.4746913192289,17.730492328126,122.846848178747)) ;
#35565 = CARTESIAN_POINT('Ctrl Pts',(-20.7410561134647,17.5505032477161,122.705620024143)) ;
#35566 = CARTESIAN_POINT('Ctrl Pts',(-20.5566303036143,17.7404925068322,123.040424795211)) ;
#35567 = CARTESIAN_POINT('Ctrl Pts',(-20.8434772707926,17.5605034264223,122.947591960543)) ;
#35568 = CARTESIAN_POINT('Ctrl Pts',(-20.6035135712802,17.7504097850418,123.243613328282)) ;
#35569 = CARTESIAN_POINT('Ctrl Pts',(-20.90207862794,17.5704207046319,123.20157834967)) ;
#35570 = CARTESIAN_POINT('Ctrl Pts',(-20.6144792344301,17.7604570314554,123.454524019583)) ;
#35571 = CARTESIAN_POINT('Ctrl Pts',(-20.9157828895286,17.5804679510456,123.465216930617)) ;
#35572 = CARTESIAN_POINT('Ctrl Pts',(-20.5893156501157,17.7703309204367,123.660606188454)) ;
#35573 = CARTESIAN_POINT('Ctrl Pts',(-20.8843256016214,17.5903418400269,123.722819362007)) ;
#35574 = CARTESIAN_POINT('Ctrl Pts',(-20.5277259008089,17.7803929380173,123.862949653921)) ;
#35575 = CARTESIAN_POINT('Ctrl Pts',(-20.8073356879099,17.6004038576075,123.975747950664)) ;
#35576 = CARTESIAN_POINT('Ctrl Pts',(-20.4337117630159,17.7902639997516,124.047969554099)) ;
#35577 = CARTESIAN_POINT('Ctrl Pts',(-20.6898154916365,17.6102749193418,124.207021563606)) ;
#35578 = CARTESIAN_POINT('Ctrl Pts',(-20.3079243206762,17.8002580631119,124.216261726582)) ;
#35579 = CARTESIAN_POINT('Ctrl Pts',(-20.5325789116927,17.620268982702,124.417385134035)) ;
#35580 = CARTESIAN_POINT('Ctrl Pts',(-20.1539268427788,17.8102902211453,124.360359874933)) ;
#35581 = CARTESIAN_POINT('Ctrl Pts',(-20.3400800617219,17.6303011407355,124.597505830215)) ;
#35582 = CARTESIAN_POINT('Ctrl Pts',(-19.9804372227752,17.8201540973854,124.473993821074)) ;
#35583 = CARTESIAN_POINT('Ctrl Pts',(-20.1232165513051,17.6401650169756,124.739545873225)) ;
#35584 = CARTESIAN_POINT('Ctrl Pts',(-19.7859124945591,17.8302246120237,124.557495151561)) ;
#35585 = CARTESIAN_POINT('Ctrl Pts',(-19.8800594521313,17.6502355316139,124.843920027553)) ;
#35586 = CARTESIAN_POINT('Ctrl Pts',(-19.5845131324371,17.8400652489647,124.604874841152)) ;
#35587 = CARTESIAN_POINT('Ctrl Pts',(-19.6283095577408,17.6600761685548,124.903141838368)) ;
#35588 = CARTESIAN_POINT('Ctrl Pts',(-19.3753651784529,17.8500323778049,124.617404469325)) ;
#35589 = CARTESIAN_POINT('Ctrl Pts',(-19.3668752747088,17.670043297395,124.918801259621)) ;
#35590 = CARTESIAN_POINT('Ctrl Pts',(-19.1662372548247,17.8600463509294,124.593093186389)) ;
#35591 = CARTESIAN_POINT('Ctrl Pts',(-19.1054626464857,17.6800572705196,124.888408905299)) ;
#35592 = CARTESIAN_POINT('Ctrl Pts',(-18.8985829814894,17.8733310847927,124.513236748648)) ;
#35593 = CARTESIAN_POINT('Ctrl Pts',(-18.7709105569149,17.6933420043829,124.788587304153)) ;
#35594 = CARTESIAN_POINT('Ctrl Pts',(-18.6588816082281,17.8865563495074,124.366233166193)) ;
#35595 = CARTESIAN_POINT('Ctrl Pts',(-18.471311575917,17.7065672690976,124.604860086417)) ;
#35596 = CARTESIAN_POINT('Ctrl Pts',(-18.4660643936239,17.8998668720623,124.16345986531)) ;
#35597 = CARTESIAN_POINT('Ctrl Pts',(-18.2302475347785,17.7198777916525,124.351352544066)) ;
#35598 = CARTESIAN_POINT('Ctrl Pts',(-18.3496539207817,17.9098955169645,123.987675168725)) ;
#35599 = CARTESIAN_POINT('Ctrl Pts',(-18.0847456432416,17.7299064365547,124.131627885485)) ;
#35600 = CARTESIAN_POINT('Ctrl Pts',(-18.2666046768902,17.9197765493184,123.797265561307)) ;
#35601 = CARTESIAN_POINT('Ctrl Pts',(-17.9809344251841,17.7397874689086,123.893612632068)) ;
#35602 = CARTESIAN_POINT('Ctrl Pts',(-18.2169614950972,17.9297575219985,123.593391497918)) ;
#35603 = CARTESIAN_POINT('Ctrl Pts',(-17.918882981317,17.7497684415886,123.638771587208)) ;
#35604 = CARTESIAN_POINT('Ctrl Pts',(-18.203650414156,17.9397386495845,123.383995886292)) ;
#35605 = CARTESIAN_POINT('Ctrl Pts',(-17.9022490540059,17.7597495691746,123.3770209592)) ;
#35606 = CARTESIAN_POINT('Ctrl Pts',(-18.2339270986067,17.9529818398459,123.107154473442)) ;
#35607 = CARTESIAN_POINT('Ctrl Pts',(-17.9400860620383,17.7729927594361,123.030998917168)) ;
#35608 = CARTESIAN_POINT('Ctrl Pts',(-18.3623848961341,17.9696498352067,122.77698011445)) ;
#35609 = CARTESIAN_POINT('Ctrl Pts',(-18.1006895819579,17.7896607547969,122.618237447399)) ;
#35610 = CARTESIAN_POINT('Ctrl Pts',(-18.5937018814127,17.9861703352187,122.512467682985)) ;
#35611 = CARTESIAN_POINT('Ctrl Pts',(-18.38978122094,17.8061812548089,122.287658244962)) ;
#35612 = CARTESIAN_POINT('Ctrl Pts',(-18.8258934089198,17.9994833515347,122.356347563406)) ;
#35613 = CARTESIAN_POINT('Ctrl Pts',(-18.6800705189778,17.8194942711249,122.09246633177)) ;
#35614 = CARTESIAN_POINT('Ctrl Pts',(-19.0164028181987,18.0093999097677,122.271568361071)) ;
#35615 = CARTESIAN_POINT('Ctrl Pts',(-18.9181973224311,17.8294108293579,121.986503440677)) ;
#35616 = CARTESIAN_POINT('Ctrl Pts',(-19.2209294726659,18.0194275780706,122.220690420935)) ;
#35617 = CARTESIAN_POINT('Ctrl Pts',(-19.1738622433812,17.8394384976607,121.922906470972)) ;
#35618 = CARTESIAN_POINT('Ctrl Pts',(-19.4974318665862,18.0326081678152,122.200829010894)) ;
#35619 = CARTESIAN_POINT('Ctrl Pts',(-19.5194723945111,17.8526190874054,121.898080551873)) ;
#35620 = CARTESIAN_POINT('Ctrl Pts',(-19.8468976293333,18.0493563069346,122.268323420744)) ;
#35621 = CARTESIAN_POINT('Ctrl Pts',(-19.9563231936463,17.8693672265248,121.98245538237)) ;
#35622 = CARTESIAN_POINT('Ctrl Pts',(-20.208402785875,18.0691510494452,122.484267090907)) ;
#35623 = CARTESIAN_POINT('Ctrl Pts',(-20.4081951552993,17.8891619690354,122.252387033686)) ;
#35624 = CARTESIAN_POINT('Ctrl Pts',(-20.4779851808533,18.089195442254,122.814181391248)) ;
#35625 = CARTESIAN_POINT('Ctrl Pts',(-20.7451718133563,17.9092063618442,122.664783040621)) ;
#35626 = CARTESIAN_POINT('Ctrl Pts',(-20.6171002054309,18.1090346245527,123.212537767396)) ;
#35627 = CARTESIAN_POINT('Ctrl Pts',(-20.9190608631241,17.9290455441429,123.162728597943)) ;
#35628 = CARTESIAN_POINT('Ctrl Pts',(-20.6129501344917,18.1289599482456,123.636081201346)) ;
#35629 = CARTESIAN_POINT('Ctrl Pts',(-20.9138698456781,17.9489708678357,123.692157121914)) ;
#35630 = CARTESIAN_POINT('Ctrl Pts',(-20.4644170209885,18.1488835862971,124.032892736758)) ;
#35631 = CARTESIAN_POINT('Ctrl Pts',(-20.7282004988174,17.9688945058873,124.188169695687)) ;
#35632 = CARTESIAN_POINT('Ctrl Pts',(-20.1895488356295,18.1688084597626,124.355214759084)) ;
#35633 = CARTESIAN_POINT('Ctrl Pts',(-20.3846133571134,17.9888193793528,124.591069561722)) ;
#35634 = CARTESIAN_POINT('Ctrl Pts',(-19.8222522044971,18.1886870668415,124.564420794737)) ;
#35635 = CARTESIAN_POINT('Ctrl Pts',(-19.9254924403146,18.0086979864317,124.852574068787)) ;
#35636 = CARTESIAN_POINT('Ctrl Pts',(-19.4036094051165,18.2086645096735,124.636282835696)) ;
#35637 = CARTESIAN_POINT('Ctrl Pts',(-19.4021887856864,18.0286754292637,124.9423992146)) ;
#35638 = CARTESIAN_POINT('Ctrl Pts',(-18.9865333106449,18.2285963577582,124.560840820189)) ;
#35639 = CARTESIAN_POINT('Ctrl Pts',(-18.8808448567096,18.0486072773484,124.848094480844)) ;
#35640 = CARTESIAN_POINT('Ctrl Pts',(-18.6207574150074,18.2484916261008,124.348382771225)) ;
#35641 = CARTESIAN_POINT('Ctrl Pts',(-18.423627145768,18.0685025456909,124.582520931737)) ;
#35642 = CARTESIAN_POINT('Ctrl Pts',(-18.3486814493143,18.2684141245129,124.02368906418)) ;
#35643 = CARTESIAN_POINT('Ctrl Pts',(-18.0835339662769,18.0884250441031,124.176653707857)) ;
#35644 = CARTESIAN_POINT('Ctrl Pts',(-18.2035687666535,18.2883736063889,123.62485045441)) ;
#35645 = CARTESIAN_POINT('Ctrl Pts',(-17.9021445000079,18.1083845259791,123.678105539873)) ;
#35646 = CARTESIAN_POINT('Ctrl Pts',(-18.203194006856,18.3082513588482,123.202260983975)) ;
#35647 = CARTESIAN_POINT('Ctrl Pts',(-17.9016770429554,18.1282622784384,123.149870596729)) ;
#35648 = CARTESIAN_POINT('Ctrl Pts',(-18.3459964134725,18.3281331495828,122.804281369069)) ;
#35649 = CARTESIAN_POINT('Ctrl Pts',(-18.0801792550094,18.148144069173,122.65239779118)) ;
#35650 = CARTESIAN_POINT('Ctrl Pts',(-18.6191997385848,18.3482064884338,122.476442912359)) ;
#35651 = CARTESIAN_POINT('Ctrl Pts',(-18.4216843161546,18.1682174080239,122.242598944776)) ;
#35652 = CARTESIAN_POINT('Ctrl Pts',(-18.9830102331295,18.3680109556696,122.264221298364)) ;
#35653 = CARTESIAN_POINT('Ctrl Pts',(-18.8764446817884,18.1880218752597,121.977323375749)) ;
#35654 = CARTESIAN_POINT('Ctrl Pts',(-19.4008308381281,18.3879942960774,122.187305861743)) ;
#35655 = CARTESIAN_POINT('Ctrl Pts',(-19.398720028265,18.2080052156676,121.881178045639)) ;
#35656 = CARTESIAN_POINT('Ctrl Pts',(-19.8183304642668,18.4079092606754,122.258027106077)) ;
#35657 = CARTESIAN_POINT('Ctrl Pts',(-19.9205934708434,18.2279201802656,121.969578564998)) ;
#35658 = CARTESIAN_POINT('Ctrl Pts',(-20.1864288478707,18.4277777953917,122.465496330421)) ;
#35659 = CARTESIAN_POINT('Ctrl Pts',(-20.380715850587,18.2477887149819,122.228912632694)) ;
#35660 = CARTESIAN_POINT('Ctrl Pts',(-20.4635196115804,18.4478301796035,122.789385037709)) ;
#35661 = CARTESIAN_POINT('Ctrl Pts',(-20.727080948349,18.2678410991936,122.633772923459)) ;
#35662 = CARTESIAN_POINT('Ctrl Pts',(-20.6120028434724,18.4676041433927,123.182923094544)) ;
#35663 = CARTESIAN_POINT('Ctrl Pts',(-20.9126860426802,18.2876150629828,123.125692137809)) ;
#35664 = CARTESIAN_POINT('Ctrl Pts',(-20.6176815723447,18.487658522414,123.609124769732)) ;
#35665 = CARTESIAN_POINT('Ctrl Pts',(-20.9197870561748,18.3076694420042,123.658444810711)) ;
#35666 = CARTESIAN_POINT('Ctrl Pts',(-20.4791262983683,18.5074552599873,124.006731982983)) ;
#35667 = CARTESIAN_POINT('Ctrl Pts',(-20.7465962163271,18.3274661795774,124.155452562242)) ;
#35668 = CARTESIAN_POINT('Ctrl Pts',(-20.2119627746794,18.5274230723387,124.33658343425)) ;
#35669 = CARTESIAN_POINT('Ctrl Pts',(-20.4126446943069,18.3474339919289,124.567768827169)) ;
#35670 = CARTESIAN_POINT('Ctrl Pts',(-19.8479424439338,18.5473820484038,124.554891666292)) ;
#35671 = CARTESIAN_POINT('Ctrl Pts',(-19.9576212451573,18.367392967994,124.840656736509)) ;
#35672 = CARTESIAN_POINT('Ctrl Pts',(-19.4327602934189,18.5672769666812,124.635860460392)) ;
#35673 = CARTESIAN_POINT('Ctrl Pts',(-19.4386451944318,18.3872878862713,124.941871042753)) ;
#35674 = CARTESIAN_POINT('Ctrl Pts',(-19.0147820526511,18.5871732791315,124.570804620221)) ;
#35675 = CARTESIAN_POINT('Ctrl Pts',(-18.9161726452975,18.4071841987217,124.860555263163)) ;
#35676 = CARTESIAN_POINT('Ctrl Pts',(-18.6435903312615,18.6070812125056,124.367280330836)) ;
#35677 = CARTESIAN_POINT('Ctrl Pts',(-18.4521815633457,18.4270921320958,124.606153931654)) ;
#35678 = CARTESIAN_POINT('Ctrl Pts',(-18.3636220458617,18.6270311027941,124.048654042255)) ;
#35679 = CARTESIAN_POINT('Ctrl Pts',(-18.1022181076318,18.4470420223842,124.207874213634)) ;
#35680 = CARTESIAN_POINT('Ctrl Pts',(-18.2093224184274,18.6469083332954,123.655139111936)) ;
#35681 = CARTESIAN_POINT('Ctrl Pts',(-17.9093397629679,18.4669192528855,123.71598284327)) ;
#35682 = CARTESIAN_POINT('Ctrl Pts',(-18.1982991555925,18.6668910021664,123.230417623875)) ;
#35683 = CARTESIAN_POINT('Ctrl Pts',(-17.8955552161012,18.4869019217566,123.185081472564)) ;
#35684 = CARTESIAN_POINT('Ctrl Pts',(-18.3328317480087,18.6868238887468,122.828454448446)) ;
#35685 = CARTESIAN_POINT('Ctrl Pts',(-18.0637189575334,18.5068348083369,122.682625101203)) ;
#35686 = CARTESIAN_POINT('Ctrl Pts',(-18.5959241687473,18.7067366347647,122.496751886595)) ;
#35687 = CARTESIAN_POINT('Ctrl Pts',(-18.3925705509658,18.5267475543548,122.267998602656)) ;
#35688 = CARTESIAN_POINT('Ctrl Pts',(-18.8956709172905,18.7233063561065,122.311665038351)) ;
#35689 = CARTESIAN_POINT('Ctrl Pts',(-18.7672818816645,18.5433172756967,122.036622749407)) ;
#35690 = CARTESIAN_POINT('Ctrl Pts',(-19.1634796639719,18.7366063674115,122.231169175464)) ;
#35691 = CARTESIAN_POINT('Ctrl Pts',(-19.1020056145129,18.5566172870017,121.936011376236)) ;
#35692 = CARTESIAN_POINT('Ctrl Pts',(-19.44044901437,18.7498765551614,122.198083479457)) ;
#35693 = CARTESIAN_POINT('Ctrl Pts',(-19.4482877506097,18.5698874747515,121.894651385031)) ;
#35694 = CARTESIAN_POINT('Ctrl Pts',(-19.7904919604174,18.7665039375268,122.248222801517)) ;
#35695 = CARTESIAN_POINT('Ctrl Pts',(-19.8857560482336,18.586514857117,121.957313792309)) ;
#35696 = CARTESIAN_POINT('Ctrl Pts',(-20.1021440207609,18.783126227272,122.414835522395)) ;
#35697 = CARTESIAN_POINT('Ctrl Pts',(-20.2753787251755,18.6031371468622,122.165595250292)) ;
#35698 = CARTESIAN_POINT('Ctrl Pts',(-20.3055329334675,18.7963714416665,122.605057021473)) ;
#35699 = CARTESIAN_POINT('Ctrl Pts',(-20.5295847929719,18.6163823612567,122.403352527165)) ;
#35700 = CARTESIAN_POINT('Ctrl Pts',(-20.4311881436849,18.8062834066272,122.771300615763)) ;
#35701 = CARTESIAN_POINT('Ctrl Pts',(-20.6866624263793,18.6262943262174,122.611158628131)) ;
#35702 = CARTESIAN_POINT('Ctrl Pts',(-20.5272430540412,18.8163420297916,122.959664946299)) ;
#35703 = CARTESIAN_POINT('Ctrl Pts',(-20.8067318368844,18.6363529493818,122.846612050216)) ;
#35704 = CARTESIAN_POINT('Ctrl Pts',(-20.5880949584386,18.8261821439075,123.157414828597)) ;
#35705 = CARTESIAN_POINT('Ctrl Pts',(-20.8827997470549,18.6461930634976,123.093798587246)) ;
#35706 = CARTESIAN_POINT('Ctrl Pts',(-20.6144765414881,18.8362479288651,123.367346989237)) ;
#35707 = CARTESIAN_POINT('Ctrl Pts',(-20.9157793857665,18.6562588484553,123.356213554675)) ;
#35708 = CARTESIAN_POINT('Ctrl Pts',(-20.6041033810044,18.846131246653,123.574893561351)) ;
#35709 = CARTESIAN_POINT('Ctrl Pts',(-20.9028157444031,18.6661421662431,123.61564679858)) ;
#35710 = CARTESIAN_POINT('Ctrl Pts',(-20.557811278042,18.8561206845115,123.779716355101)) ;
#35711 = CARTESIAN_POINT('Ctrl Pts',(-20.8449533316888,18.6761316041017,123.871675964838)) ;
#35712 = CARTESIAN_POINT('Ctrl Pts',(-20.4767860972541,18.8660843985643,123.972890703501)) ;
#35713 = CARTESIAN_POINT('Ctrl Pts',(-20.7436744284791,18.6860953181544,124.113145006434)) ;
#35714 = CARTESIAN_POINT('Ctrl Pts',(-20.3632771377155,18.8760794102235,124.149739579038)) ;
#35715 = CARTESIAN_POINT('Ctrl Pts',(-20.601790555913,18.6960903298137,124.334207674829)) ;
#35716 = CARTESIAN_POINT('Ctrl Pts',(-20.2199721057436,18.8861157019177,124.304588195844)) ;
#35717 = CARTESIAN_POINT('Ctrl Pts',(-20.4226612590581,18.7061266215079,124.527770408806)) ;
#35718 = CARTESIAN_POINT('Ctrl Pts',(-20.0553231898177,18.8959620796112,124.430069749636)) ;
#35719 = CARTESIAN_POINT('Ctrl Pts',(-20.2168518530314,18.7159729992014,124.684624557597)) ;
#35720 = CARTESIAN_POINT('Ctrl Pts',(-19.8690215673185,18.9059470237619,124.526730415756)) ;
#35721 = CARTESIAN_POINT('Ctrl Pts',(-19.9839760536342,18.7259579433521,124.805452933114)) ;
#35722 = CARTESIAN_POINT('Ctrl Pts',(-19.6697047219603,18.9158839948918,124.589408387716)) ;
#35723 = CARTESIAN_POINT('Ctrl Pts',(-19.7348307743304,18.735894914482,124.88380310373)) ;
#35724 = CARTESIAN_POINT('Ctrl Pts',(-19.4602197023148,18.9259337795236,124.616715999974)) ;
#35725 = CARTESIAN_POINT('Ctrl Pts',(-19.4729748038797,18.7459446991137,124.917940423266)) ;
#35726 = CARTESIAN_POINT('Ctrl Pts',(-19.2533184450846,18.9357842416011,124.607579273782)) ;
#35727 = CARTESIAN_POINT('Ctrl Pts',(-19.2143479954999,18.7557951611912,124.906522324795)) ;
#35728 = CARTESIAN_POINT('Ctrl Pts',(-19.0485745773188,18.9457562551215,124.562644959168)) ;
#35729 = CARTESIAN_POINT('Ctrl Pts',(-18.9584174462434,18.7657671747116,124.850357149064)) ;
#35730 = CARTESIAN_POINT('Ctrl Pts',(-18.8542477972193,18.9557514022409,124.482609220366)) ;
#35731 = CARTESIAN_POINT('Ctrl Pts',(-18.715507831181,18.7757623218311,124.750315034933)) ;
#35732 = CARTESIAN_POINT('Ctrl Pts',(-18.6762610468344,18.965785371977,124.369422704143)) ;
#35733 = CARTESIAN_POINT('Ctrl Pts',(-18.4930228487092,18.7857962915672,124.608834245191)) ;
#35734 = CARTESIAN_POINT('Ctrl Pts',(-18.5231511574649,18.9756409176476,124.229798349696)) ;
#35735 = CARTESIAN_POINT('Ctrl Pts',(-18.3016334314437,18.7956518372378,124.434305714766)) ;
#35736 = CARTESIAN_POINT('Ctrl Pts',(-18.3945701733205,18.9856396746608,124.063548623651)) ;
#35737 = CARTESIAN_POINT('Ctrl Pts',(-18.1409049402288,18.805650594251,124.226495189786)) ;
#35738 = CARTESIAN_POINT('Ctrl Pts',(-18.2975958365009,18.995536809898,123.879424723443)) ;
#35739 = CARTESIAN_POINT('Ctrl Pts',(-18.0196844553745,18.8155477294882,123.99634137888)) ;
#35740 = CARTESIAN_POINT('Ctrl Pts',(-18.2330434105871,19.0055899057376,123.678199215092)) ;
#35741 = CARTESIAN_POINT('Ctrl Pts',(-17.9389912916734,18.8256008253278,123.744810346015)) ;
#35742 = CARTESIAN_POINT('Ctrl Pts',(-18.2048687725473,19.0154734144682,123.472321453931)) ;
#35743 = CARTESIAN_POINT('Ctrl Pts',(-17.9037702161994,18.8354843340584,123.487463211665)) ;
#35744 = CARTESIAN_POINT('Ctrl Pts',(-18.2124671547143,19.0254682871143,123.262341510424)) ;
#35745 = CARTESIAN_POINT('Ctrl Pts',(-17.9132654844711,18.8454792067045,123.224988077214)) ;
#35746 = CARTESIAN_POINT('Ctrl Pts',(-18.2568443718026,19.03548824875,123.056405743036)) ;
#35747 = CARTESIAN_POINT('Ctrl Pts',(-17.9687343277872,18.8554991683402,122.967567757769)) ;
#35748 = CARTESIAN_POINT('Ctrl Pts',(-18.3352281082984,19.0453936125498,122.863482475236)) ;
#35749 = CARTESIAN_POINT('Ctrl Pts',(-18.0667115840273,18.86540453214,122.726412358602)) ;
#35750 = CARTESIAN_POINT('Ctrl Pts',(-18.4459450487129,19.0553342001574,122.686255011705)) ;
#35751 = CARTESIAN_POINT('Ctrl Pts',(-18.2051056277496,18.8753451197476,122.50487638209)) ;
#35752 = CARTESIAN_POINT('Ctrl Pts',(-18.5865641592456,19.065337018258,122.529862565855)) ;
#35753 = CARTESIAN_POINT('Ctrl Pts',(-18.3808775939559,18.8853479378482,122.30938398515)) ;
#35754 = CARTESIAN_POINT('Ctrl Pts',(-18.7529137805727,19.0753717299822,122.400141597635)) ;
#35755 = CARTESIAN_POINT('Ctrl Pts',(-18.5888129419414,18.8953826495723,122.147230647386)) ;
#35756 = CARTESIAN_POINT('Ctrl Pts',(-18.9355927334257,19.0852166367195,122.302823707512)) ;
#35757 = CARTESIAN_POINT('Ctrl Pts',(-18.8171608789113,18.9052275563097,122.025580673966)) ;
#35758 = CARTESIAN_POINT('Ctrl Pts',(-19.135044952863,19.0952024892885,122.237424139112)) ;
#35759 = CARTESIAN_POINT('Ctrl Pts',(-19.0664754950351,18.9152134088786,121.943828689827)) ;
#35760 = CARTESIAN_POINT('Ctrl Pts',(-19.3418110241518,19.1051372977015,122.207643930743)) ;
#35761 = CARTESIAN_POINT('Ctrl Pts',(-19.324933039813,18.9251482172917,121.906600838768)) ;
#35762 = CARTESIAN_POINT('Ctrl Pts',(-19.5531110415552,19.1151948247826,122.214485106709)) ;
#35763 = CARTESIAN_POINT('Ctrl Pts',(-19.5890580305802,18.9352057443728,121.915149697204)) ;
#35764 = CARTESIAN_POINT('Ctrl Pts',(-19.7552767450465,19.1250164797797,122.256593308277)) ;
#35765 = CARTESIAN_POINT('Ctrl Pts',(-19.8417664438669,18.9450273993699,121.967782613236)) ;
#35766 = CARTESIAN_POINT('Ctrl Pts',(-19.9517461949997,19.1350725239527,122.334610066435)) ;
#35767 = CARTESIAN_POINT('Ctrl Pts',(-20.0873540689594,18.9550834435429,122.065301217986)) ;
#35768 = CARTESIAN_POINT('Ctrl Pts',(-20.1294455067056,19.1450132639979,122.44461757867)) ;
#35769 = CARTESIAN_POINT('Ctrl Pts',(-20.3094798343404,18.965024183588,122.202808615077)) ;
#35770 = CARTESIAN_POINT('Ctrl Pts',(-20.2852002013898,19.1549173850707,122.582803466189)) ;
#35771 = CARTESIAN_POINT('Ctrl Pts',(-20.5041752042794,18.9749283046609,122.37553951635)) ;
#35772 = CARTESIAN_POINT('Ctrl Pts',(-20.4163570695297,19.164964926225,122.748363557703)) ;
#35773 = CARTESIAN_POINT('Ctrl Pts',(-20.6681231447569,18.9849758458152,122.582488035547)) ;
#35774 = CARTESIAN_POINT('Ctrl Pts',(-20.5154426781397,19.1748636778254,122.931394298921)) ;
#35775 = CARTESIAN_POINT('Ctrl Pts',(-20.7919825436342,18.9948745974155,122.811275811251)) ;
#35776 = CARTESIAN_POINT('Ctrl Pts',(-20.5823095621663,19.1849121567912,123.13175874193)) ;
#35777 = CARTESIAN_POINT('Ctrl Pts',(-20.8755683817589,19.0049230763813,123.061730492488)) ;
#35778 = CARTESIAN_POINT('Ctrl Pts',(-20.6128955919429,19.1947996538749,123.337384367782)) ;
#35779 = CARTESIAN_POINT('Ctrl Pts',(-20.9138033740023,19.0148105734651,123.318762800782)) ;
#35780 = CARTESIAN_POINT('Ctrl Pts',(-20.6076449007628,19.204792744173,123.547386563793)) ;
#35781 = CARTESIAN_POINT('Ctrl Pts',(-20.9072423075694,19.0248036637631,123.581265757215)) ;
#35782 = CARTESIAN_POINT('Ctrl Pts',(-20.5661040890578,19.2147449142333,123.752459949604)) ;
#35783 = CARTESIAN_POINT('Ctrl Pts',(-20.8553184944802,19.0347558338234,123.837608299637)) ;
#35784 = CARTESIAN_POINT('Ctrl Pts',(-20.4899691627066,19.2246833341478,123.947015816567)) ;
#35785 = CARTESIAN_POINT('Ctrl Pts',(-20.7601517685362,19.044694253738,124.080804362986)) ;
#35786 = CARTESIAN_POINT('Ctrl Pts',(-20.3808817205689,19.2346684642334,124.126388705012)) ;
#35787 = CARTESIAN_POINT('Ctrl Pts',(-20.6237942336124,19.0546793838236,124.305021774799)) ;
#35788 = CARTESIAN_POINT('Ctrl Pts',(-20.241378136144,19.2447051536475,124.284677346866)) ;
#35789 = CARTESIAN_POINT('Ctrl Pts',(-20.4494165140451,19.0647160732376,124.502884010829)) ;
#35790 = CARTESIAN_POINT('Ctrl Pts',(-20.0796809670724,19.25455983764,124.414229163885)) ;
#35791 = CARTESIAN_POINT('Ctrl Pts',(-20.2472957010154,19.0745707572301,124.664826057178)) ;
#35792 = CARTESIAN_POINT('Ctrl Pts',(-19.8954624316429,19.2645593216878,124.515427636075)) ;
#35793 = CARTESIAN_POINT('Ctrl Pts',(-20.0170234288381,19.084570241278,124.791326058975)) ;
#35794 = CARTESIAN_POINT('Ctrl Pts',(-19.6985533037412,19.2744544104647,124.582628798739)) ;
#35795 = CARTESIAN_POINT('Ctrl Pts',(-19.7708869846868,19.0944653300549,124.875329679464)) ;
#35796 = CARTESIAN_POINT('Ctrl Pts',(-19.4895873463579,19.2845149651109,124.615123526839)) ;
#35797 = CARTESIAN_POINT('Ctrl Pts',(-19.5096800897253,19.1045258847011,124.915950078739)) ;
#35798 = CARTESIAN_POINT('Ctrl Pts',(-19.2825491814808,19.2943642294838,124.611047104812)) ;
#35799 = CARTESIAN_POINT('Ctrl Pts',(-19.2508813050705,19.1143751490739,124.910856545267)) ;
#35800 = CARTESIAN_POINT('Ctrl Pts',(-19.0756100518396,19.3043914819316,124.570889809376)) ;
#35801 = CARTESIAN_POINT('Ctrl Pts',(-18.9922070756682,19.1244024015218,124.860661757926)) ;
#35802 = CARTESIAN_POINT('Ctrl Pts',(-18.8789515708921,19.3144197795018,124.494880706852)) ;
#35803 = CARTESIAN_POINT('Ctrl Pts',(-18.7463833098718,19.1344306990919,124.765652294149)) ;
#35804 = CARTESIAN_POINT('Ctrl Pts',(-18.701566831824,19.3242659085078,124.388210448307)) ;
#35805 = CARTESIAN_POINT('Ctrl Pts',(-18.5246504441737,19.1442768280979,124.63231552407)) ;
#35806 = CARTESIAN_POINT('Ctrl Pts',(-18.5427028733491,19.3342598138698,124.250713710067)) ;
#35807 = CARTESIAN_POINT('Ctrl Pts',(-18.3260692253039,19.15427073346,124.460445802983)) ;
#35808 = CARTESIAN_POINT('Ctrl Pts',(-18.4100146534908,19.3442839115529,124.086985981103)) ;
#35809 = CARTESIAN_POINT('Ctrl Pts',(-18.1602075358963,19.1642948311431,124.255787351985)) ;
#35810 = CARTESIAN_POINT('Ctrl Pts',(-18.3089126305251,19.3541737394069,123.90530352091)) ;
#35811 = CARTESIAN_POINT('Ctrl Pts',(-18.0338280399236,19.1741846589971,124.02868439438)) ;
#35812 = CARTESIAN_POINT('Ctrl Pts',(-18.2399042502461,19.3641657208373,123.706908085251)) ;
#35813 = CARTESIAN_POINT('Ctrl Pts',(-17.9475659143818,19.1841766404275,123.780690475597)) ;
#35814 = CARTESIAN_POINT('Ctrl Pts',(-18.2065905895425,19.3741127256032,123.50046117222)) ;
#35815 = CARTESIAN_POINT('Ctrl Pts',(-17.9059220810719,19.1941236451933,123.522631607334)) ;
#35816 = CARTESIAN_POINT('Ctrl Pts',(-18.2092454060776,19.384062376993,123.291296502426)) ;
#35817 = CARTESIAN_POINT('Ctrl Pts',(-17.9092390394881,19.2040732965831,123.261175270485)) ;
#35818 = CARTESIAN_POINT('Ctrl Pts',(-18.2486861191594,19.3940993799704,123.084011953046)) ;
#35819 = CARTESIAN_POINT('Ctrl Pts',(-17.9585383067173,19.2141102995605,123.002069407988)) ;
#35820 = CARTESIAN_POINT('Ctrl Pts',(-18.3222825230277,19.4039882884054,122.889570998935)) ;
#35821 = CARTESIAN_POINT('Ctrl Pts',(-18.0505326597858,19.2239992079956,122.75901679837)) ;
#35822 = CARTESIAN_POINT('Ctrl Pts',(-18.4292681158825,19.4139776208829,122.708864244681)) ;
#35823 = CARTESIAN_POINT('Ctrl Pts',(-18.1842635125467,19.233988540473,122.533132432026)) ;
#35824 = CARTESIAN_POINT('Ctrl Pts',(-18.5657022346844,19.42393617632,122.550072619534)) ;
#35825 = CARTESIAN_POINT('Ctrl Pts',(-18.3548053009727,19.2439470959102,122.334641591402)) ;
#35826 = CARTESIAN_POINT('Ctrl Pts',(-18.7263649466662,19.4338357475205,122.417759602104)) ;
#35827 = CARTESIAN_POINT('Ctrl Pts',(-18.5556335270532,19.2538466671106,122.169248739328)) ;
#35828 = CARTESIAN_POINT('Ctrl Pts',(-18.9102833479291,19.4438836727725,122.313900274746)) ;
#35829 = CARTESIAN_POINT('Ctrl Pts',(-18.7855306745669,19.2638945923626,122.039423510043)) ;
#35830 = CARTESIAN_POINT('Ctrl Pts',(-19.1064125465237,19.4537789722985,122.244448286497)) ;
#35831 = CARTESIAN_POINT('Ctrl Pts',(-19.0306926009138,19.2737898918887,121.952607002174)) ;
#35832 = CARTESIAN_POINT('Ctrl Pts',(-19.3150144344435,19.4638408287464,122.209510718595)) ;
#35833 = CARTESIAN_POINT('Ctrl Pts',(-19.2914444276043,19.2838517483366,121.908933829256)) ;
#35834 = CARTESIAN_POINT('Ctrl Pts',(-19.521965316198,19.4736846751631,122.211242753843)) ;
#35835 = CARTESIAN_POINT('Ctrl Pts',(-19.5501343610647,19.2936955947532,121.911097613334)) ;
#35836 = CARTESIAN_POINT('Ctrl Pts',(-19.7280448443102,19.4836476242911,122.248623144845)) ;
#35837 = CARTESIAN_POINT('Ctrl Pts',(-19.8077343935963,19.3036585438813,121.95782219521)) ;
#35838 = CARTESIAN_POINT('Ctrl Pts',(-19.9258004100159,19.4936816607191,122.322067326375)) ;
#35839 = CARTESIAN_POINT('Ctrl Pts',(-20.0549291177515,19.3136925803093,122.049626314935)) ;
#35840 = CARTESIAN_POINT('Ctrl Pts',(-20.1052428274456,19.5035690876772,122.426981156448)) ;
#35841 = CARTESIAN_POINT('Ctrl Pts',(-20.279233546627,19.3235800072674,122.180768204286)) ;
#35842 = CARTESIAN_POINT('Ctrl Pts',(-20.2660510972554,19.5135835220135,122.562891810069)) ;
#35843 = CARTESIAN_POINT('Ctrl Pts',(-20.4802444747732,19.3335944416037,122.350655841033)) ;
#35844 = CARTESIAN_POINT('Ctrl Pts',(-20.4006689400157,19.5236184666485,122.725307394749)) ;
#35845 = CARTESIAN_POINT('Ctrl Pts',(-20.64851754086,19.3436293862386,122.55367450977)) ;
#35846 = CARTESIAN_POINT('Ctrl Pts',(-20.5034449260328,19.5334508166795,122.90468153521)) ;
#35847 = CARTESIAN_POINT('Ctrl Pts',(-20.7769890299039,19.3534617362697,122.777893029289)) ;
#35848 = CARTESIAN_POINT('Ctrl Pts',(-20.5752821949681,19.5435262557967,123.10390261523)) ;
#35849 = CARTESIAN_POINT('Ctrl Pts',(-20.8667862747104,19.3635371753869,123.026918659829)) ;
#35850 = CARTESIAN_POINT('Ctrl Pts',(-20.6107689996992,19.5533787210313,123.308014325579)) ;
#35851 = CARTESIAN_POINT('Ctrl Pts',(-20.9111458115888,19.3733896406215,123.282059452488)) ;
#35852 = CARTESIAN_POINT('Ctrl Pts',(-20.6104349718264,19.5634515986082,123.519742050673)) ;
#35853 = CARTESIAN_POINT('Ctrl Pts',(-20.9107290325101,19.3834625181983,123.546718673393)) ;
#35854 = CARTESIAN_POINT('Ctrl Pts',(-20.5741538852815,19.5732941948007,123.723476229926)) ;
#35855 = CARTESIAN_POINT('Ctrl Pts',(-20.8653781809411,19.3933051143909,123.801387925584)) ;
#35856 = CARTESIAN_POINT('Ctrl Pts',(-20.5027249485285,19.583274578916,123.920753137784)) ;
#35857 = CARTESIAN_POINT('Ctrl Pts',(-20.7760923679228,19.4032854985061,124.047984519864)) ;
#35858 = CARTESIAN_POINT('Ctrl Pts',(-20.3973703972249,19.5932930595648,124.10312422854)) ;
#35859 = CARTESIAN_POINT('Ctrl Pts',(-20.64439975022,19.4133039791549,124.275948701182)) ;
#35860 = CARTESIAN_POINT('Ctrl Pts',(-20.2640988385909,19.6031763745651,124.262563519958)) ;
#35861 = CARTESIAN_POINT('Ctrl Pts',(-20.477809965381,19.4231872941553,124.475248963888)) ;
#35862 = CARTESIAN_POINT('Ctrl Pts',(-20.1021786910339,19.6132446716556,124.398835786557)) ;
#35863 = CARTESIAN_POINT('Ctrl Pts',(-20.2754104278424,19.4332555912458,124.645589428326)) ;
#35864 = CARTESIAN_POINT('Ctrl Pts',(-19.923452222074,19.6230747400279,124.502661288851)) ;
#35865 = CARTESIAN_POINT('Ctrl Pts',(-20.0520012191857,19.443085659618,124.775372441356)) ;
#35866 = CARTESIAN_POINT('Ctrl Pts',(-19.7249017076277,19.6331415324963,124.575813941918)) ;
#35867 = CARTESIAN_POINT('Ctrl Pts',(-19.8038135625344,19.4531524520865,124.866813416566)) ;
#35868 = CARTESIAN_POINT('Ctrl Pts',(-19.5202469349877,19.6430308659848,124.612640504371)) ;
#35869 = CARTESIAN_POINT('Ctrl Pts',(-19.5479941097324,19.463041785575,124.912847154489)) ;
#35870 = CARTESIAN_POINT('Ctrl Pts',(-19.3100107554735,19.6530329974009,124.613711705916)) ;
#35871 = CARTESIAN_POINT('Ctrl Pts',(-19.2851987471254,19.473043916991,124.91418637848)) ;
#35872 = CARTESIAN_POINT('Ctrl Pts',(-19.1043078669417,19.6629568670219,124.578660210897)) ;
#35873 = CARTESIAN_POINT('Ctrl Pts',(-19.0280693627493,19.4829677866121,124.87037205227)) ;
#35874 = CARTESIAN_POINT('Ctrl Pts',(-18.9055323179189,19.6730003825391,124.507541988361)) ;
#35875 = CARTESIAN_POINT('Ctrl Pts',(-18.7796000674566,19.4930113021293,124.781474531123)) ;
#35876 = CARTESIAN_POINT('Ctrl Pts',(-18.7248906132605,19.6828825954274,124.404844874836)) ;
#35877 = CARTESIAN_POINT('Ctrl Pts',(-18.5537969175997,19.5028935150175,124.653102677006)) ;
#35878 = CARTESIAN_POINT('Ctrl Pts',(-18.5618762979718,19.6929506726468,124.269896713313)) ;
#35879 = CARTESIAN_POINT('Ctrl Pts',(-18.3500292627666,19.512961592237,124.484417808862)) ;
#35880 = CARTESIAN_POINT('Ctrl Pts',(-18.42770753592,19.702789177381,124.112435729889)) ;
#35881 = CARTESIAN_POINT('Ctrl Pts',(-18.1823173294474,19.5228000969712,124.287590469328)) ;
#35882 = CARTESIAN_POINT('Ctrl Pts',(-18.3203002755283,19.7128519458104,123.930208646522)) ;
#35883 = CARTESIAN_POINT('Ctrl Pts',(-18.048058520279,19.5328628654006,124.059806890009)) ;
#35884 = CARTESIAN_POINT('Ctrl Pts',(-18.2475857905658,19.7227489390931,123.735249596216)) ;
#35885 = CARTESIAN_POINT('Ctrl Pts',(-17.9571650618056,19.5427598586833,123.81610713825)) ;
#35886 = CARTESIAN_POINT('Ctrl Pts',(-18.2090139650098,19.7326801667279,123.530063285988)) ;
#35887 = CARTESIAN_POINT('Ctrl Pts',(-17.9089504190964,19.552691086318,123.559623490834)) ;
#35888 = CARTESIAN_POINT('Ctrl Pts',(-18.206860266534,19.74272232537,123.318958748455)) ;
#35889 = CARTESIAN_POINT('Ctrl Pts',(-17.9062584822313,19.5627332449602,123.295743025401)) ;
#35890 = CARTESIAN_POINT('Ctrl Pts',(-18.2407132566598,19.7526090349011,123.113875533513)) ;
#35891 = CARTESIAN_POINT('Ctrl Pts',(-17.948575137129,19.5726199544913,123.039387974095)) ;
#35892 = CARTESIAN_POINT('Ctrl Pts',(-18.3100612563688,19.7626020073297,122.915577612345)) ;
#35893 = CARTESIAN_POINT('Ctrl Pts',(-18.0352605666354,19.5826129269199,122.791515506219)) ;
#35894 = CARTESIAN_POINT('Ctrl Pts',(-18.4123864646547,19.7725482018663,122.733228885072)) ;
#35895 = CARTESIAN_POINT('Ctrl Pts',(-18.1631676695272,19.5925591214565,122.563579250509)) ;
#35896 = CARTESIAN_POINT('Ctrl Pts',(-18.544466725532,19.7824935767178,122.571123242096)) ;
#35897 = CARTESIAN_POINT('Ctrl Pts',(-18.3282687770874,19.602504496308,122.360947075169)) ;
#35898 = CARTESIAN_POINT('Ctrl Pts',(-18.7046124165122,19.7925484960777,122.433182725376)) ;
#35899 = CARTESIAN_POINT('Ctrl Pts',(-18.5284509193159,19.6125594156678,122.188521930162)) ;
#35900 = CARTESIAN_POINT('Ctrl Pts',(-18.8818996060472,19.8023700155212,122.327286077013)) ;
#35901 = CARTESIAN_POINT('Ctrl Pts',(-18.7500615821666,19.6223809351113,122.056150769532)) ;
#35902 = CARTESIAN_POINT('Ctrl Pts',(-19.0795285112847,19.8124357842881,122.251735177665)) ;
#35903 = CARTESIAN_POINT('Ctrl Pts',(-18.9970975871785,19.6324467038783,121.961712899022)) ;
#35904 = CARTESIAN_POINT('Ctrl Pts',(-19.2839777888797,19.8223377059431,122.212355081407)) ;
#35905 = CARTESIAN_POINT('Ctrl Pts',(-19.2526602062973,19.6423486255333,121.912488218157)) ;
#35906 = CARTESIAN_POINT('Ctrl Pts',(-19.4950664842811,19.8323807647642,122.208839746125)) ;
#35907 = CARTESIAN_POINT('Ctrl Pts',(-19.5165208729991,19.6523916843543,121.908094752739)) ;
#35908 = CARTESIAN_POINT('Ctrl Pts',(-19.7007200879061,19.8422867588069,122.241689755879)) ;
#35909 = CARTESIAN_POINT('Ctrl Pts',(-19.7735886685329,19.662297678397,121.949158051642)) ;
#35910 = CARTESIAN_POINT('Ctrl Pts',(-19.8983711923909,19.8522245318887,122.309384254829)) ;
#35911 = CARTESIAN_POINT('Ctrl Pts',(-20.020652879947,19.6722354514788,122.033777229836)) ;
#35912 = CARTESIAN_POINT('Ctrl Pts',(-20.0830422576944,19.862264895621,122.41160883403)) ;
#35913 = CARTESIAN_POINT('Ctrl Pts',(-20.2514911587516,19.6822758152111,122.161558568132)) ;
#35914 = CARTESIAN_POINT('Ctrl Pts',(-20.2447669194783,19.8721522393445,122.542209039445)) ;
#35915 = CARTESIAN_POINT('Ctrl Pts',(-20.4536472526917,19.6921631589346,122.324810150198)) ;
#35916 = CARTESIAN_POINT('Ctrl Pts',(-20.383052541564,19.8821444699132,122.700322050731)) ;
#35917 = CARTESIAN_POINT('Ctrl Pts',(-20.6265036650204,19.7021553895033,122.522452222895)) ;
#35918 = CARTESIAN_POINT('Ctrl Pts',(-20.4912730530166,19.8920929976968,122.879309922931)) ;
#35919 = CARTESIAN_POINT('Ctrl Pts',(-20.7617787532514,19.712103917287,122.746188030243)) ;
#35920 = CARTESIAN_POINT('Ctrl Pts',(-20.5669463250774,19.9020297814201,123.074005487427)) ;
#35921 = CARTESIAN_POINT('Ctrl Pts',(-20.8563695651835,19.7220407010102,122.989558473114)) ;
#35922 = CARTESIAN_POINT('Ctrl Pts',(-20.6081237683006,19.912012782217,123.279827787106)) ;
#35923 = CARTESIAN_POINT('Ctrl Pts',(-20.9078402628114,19.7320237018072,123.246836830898)) ;
#35924 = CARTESIAN_POINT('Ctrl Pts',(-20.6125768739177,19.9220566690578,123.490910400367)) ;
#35925 = CARTESIAN_POINT('Ctrl Pts',(-20.9134056045136,19.7420675886479,123.510689929297)) ;
#35926 = CARTESIAN_POINT('Ctrl Pts',(-20.5814828811847,19.9318846926323,123.695206220071)) ;
#35927 = CARTESIAN_POINT('Ctrl Pts',(-20.8745366917446,19.7518956122225,123.766060949748)) ;
#35928 = CARTESIAN_POINT('Ctrl Pts',(-20.5138218279158,19.941961940846,123.895916711096)) ;
#35929 = CARTESIAN_POINT('Ctrl Pts',(-20.7899593278494,19.7619728604362,124.01694825061)) ;
#35930 = CARTESIAN_POINT('Ctrl Pts',(-20.4147085608249,19.9518114961513,124.077785912975)) ;
#35931 = CARTESIAN_POINT('Ctrl Pts',(-20.6660660069684,19.7718224157414,124.244285226942)) ;
#35932 = CARTESIAN_POINT('Ctrl Pts',(-20.2825893140887,19.961894204349,124.243476019033)) ;
#35933 = CARTESIAN_POINT('Ctrl Pts',(-20.5009161893585,19.7819051239392,124.451396677713)) ;
#35934 = CARTESIAN_POINT('Ctrl Pts',(-20.1280154651316,19.9717067972754,124.38015779365)) ;
#35935 = CARTESIAN_POINT('Ctrl Pts',(-20.3076968301649,19.7917177168656,124.622248846317)) ;
#35936 = CARTESIAN_POINT('Ctrl Pts',(-19.9477519695599,19.9817739895334,124.49096411443)) ;
#35937 = CARTESIAN_POINT('Ctrl Pts',(-20.0823669714387,19.8017849091236,124.760755273393)) ;
#35938 = CARTESIAN_POINT('Ctrl Pts',(-19.7541568951815,19.991672818996,124.56745105753)) ;
#35939 = CARTESIAN_POINT('Ctrl Pts',(-19.8403718039721,19.8116837385861,124.856362880301)) ;
#35940 = CARTESIAN_POINT('Ctrl Pts',(-19.5471389116745,20.0017268101862,124.609885515152)) ;
#35941 = CARTESIAN_POINT('Ctrl Pts',(-19.581599257852,19.8217377297763,124.909404420848)) ;
#35942 = CARTESIAN_POINT('Ctrl Pts',(-19.3396458322229,20.0115985349694,124.615811551427)) ;
#35943 = CARTESIAN_POINT('Ctrl Pts',(-19.3222318233438,19.8316094545595,124.916810422216)) ;
#35944 = CARTESIAN_POINT('Ctrl Pts',(-19.1302124053593,20.0216689770996,124.585074256382)) ;
#35945 = CARTESIAN_POINT('Ctrl Pts',(-19.0604406240676,19.8416798966898,124.878387276265)) ;
#35946 = CARTESIAN_POINT('Ctrl Pts',(-18.9339520390974,20.0315020555299,124.520082076835)) ;
#35947 = CARTESIAN_POINT('Ctrl Pts',(-18.8151144576221,19.85151297512,124.797145106949)) ;
#35948 = CARTESIAN_POINT('Ctrl Pts',(-18.7480434856124,20.0415325290313,124.420574067109)) ;
#35949 = CARTESIAN_POINT('Ctrl Pts',(-18.5827297026726,19.8615434486214,124.672758530755)) ;
#35950 = CARTESIAN_POINT('Ctrl Pts',(-18.5825831311572,20.0515641283299,124.289788081662)) ;
#35951 = CARTESIAN_POINT('Ctrl Pts',(-18.3759053293707,19.8715750479201,124.509274829731)) ;
#35952 = CARTESIAN_POINT('Ctrl Pts',(-18.4448629357415,20.0613938293681,124.13573633142)) ;
#35953 = CARTESIAN_POINT('Ctrl Pts',(-18.2037555510445,19.8814047489583,124.316708019018)) ;
#35954 = CARTESIAN_POINT('Ctrl Pts',(-18.3336698872255,20.0713832674246,123.957571401983)) ;
#35955 = CARTESIAN_POINT('Ctrl Pts',(-18.0647658072251,19.8913941870148,124.094000670372)) ;
#35956 = CARTESIAN_POINT('Ctrl Pts',(-18.2551742977455,20.0814271706407,123.761552123901)) ;
#35957 = CARTESIAN_POINT('Ctrl Pts',(-17.9666480382396,19.9014380902309,123.848976044815)) ;
#35958 = CARTESIAN_POINT('Ctrl Pts',(-18.2124417079699,20.0912486914542,123.559542282254)) ;
#35959 = CARTESIAN_POINT('Ctrl Pts',(-17.9132339250631,19.9112596110443,123.596462120668)) ;
#35960 = CARTESIAN_POINT('Ctrl Pts',(-18.2047766515983,20.1012844157013,123.348703573776)) ;
#35961 = CARTESIAN_POINT('Ctrl Pts',(-17.9036546812584,19.9212953352915,123.33291376826)) ;
#35962 = CARTESIAN_POINT('Ctrl Pts',(-18.2343404621047,20.1113065696338,123.140074801071)) ;
#35963 = CARTESIAN_POINT('Ctrl Pts',(-17.9406113336805,19.9313174892239,123.072128085438)) ;
#35964 = CARTESIAN_POINT('Ctrl Pts',(-18.2983054280949,20.1211688013911,122.942870332528)) ;
#35965 = CARTESIAN_POINT('Ctrl Pts',(-18.0205697572418,19.9411797209812,122.825622198573)) ;
#35966 = CARTESIAN_POINT('Ctrl Pts',(-18.3959846631864,20.131127871849,122.757674344572)) ;
#35967 = CARTESIAN_POINT('Ctrl Pts',(-18.1426708876465,19.9511387914392,122.59412792976)) ;
#35968 = CARTESIAN_POINT('Ctrl Pts',(-18.525566423674,20.1411630442251,122.591200036149)) ;
#35969 = CARTESIAN_POINT('Ctrl Pts',(-18.30464968217,19.9611739638153,122.386036390994)) ;
#35970 = CARTESIAN_POINT('Ctrl Pts',(-18.6794843882295,20.1510434293834,122.45168426529)) ;
#35971 = CARTESIAN_POINT('Ctrl Pts',(-18.4970491713778,19.9710543489736,122.211642765618)) ;
#35972 = CARTESIAN_POINT('Ctrl Pts',(-18.8583463704345,20.1611001439773,122.33899114382)) ;
#35973 = CARTESIAN_POINT('Ctrl Pts',(-18.7206276526731,19.9811110635675,122.070778322251)) ;
#35974 = CARTESIAN_POINT('Ctrl Pts',(-19.0506399135892,20.1709794125494,122.260478579803)) ;
#35975 = CARTESIAN_POINT('Ctrl Pts',(-18.9609961306176,19.9909903321396,121.972639347057)) ;
#35976 = CARTESIAN_POINT('Ctrl Pts',(-19.2558093771799,20.1809703700351,122.21550063428)) ;
#35977 = CARTESIAN_POINT('Ctrl Pts',(-19.2174586026776,20.0009812896253,121.916419162023)) ;
#35978 = CARTESIAN_POINT('Ctrl Pts',(-19.466736361105,20.1910110286703,122.20725269721)) ;
#35979 = CARTESIAN_POINT('Ctrl Pts',(-19.4811173295956,20.0110219482604,121.906111456717)) ;
#35980 = CARTESIAN_POINT('Ctrl Pts',(-19.6716056707991,20.2008440083783,122.234820237226)) ;
#35981 = CARTESIAN_POINT('Ctrl Pts',(-19.737204609292,20.0208549279685,121.940573290785)) ;
#35982 = CARTESIAN_POINT('Ctrl Pts',(-19.8719676861379,20.210837141628,122.297989647427)) ;
#35983 = CARTESIAN_POINT('Ctrl Pts',(-19.9876565139977,20.0308480612182,122.019537420659)) ;
#35984 = CARTESIAN_POINT('Ctrl Pts',(-20.0588521291231,20.2208691940113,122.395761902795)) ;
#35985 = CARTESIAN_POINT('Ctrl Pts',(-20.2212609501669,20.0408801136015,122.141754795269)) ;
#35986 = CARTESIAN_POINT('Ctrl Pts',(-20.2232832799828,20.2307344229627,122.522142243572)) ;
#35987 = CARTESIAN_POINT('Ctrl Pts',(-20.4267990070475,20.0507453425528,122.299732570572)) ;
#35988 = CARTESIAN_POINT('Ctrl Pts',(-20.3650928807111,20.2406963642059,122.676265084852)) ;
#35989 = CARTESIAN_POINT('Ctrl Pts',(-20.6040593214111,20.060707283796,122.492388017691)) ;
#35990 = CARTESIAN_POINT('Ctrl Pts',(-20.4785174817246,20.2507310792426,122.854128710168)) ;
#35991 = CARTESIAN_POINT('Ctrl Pts',(-20.7458379854083,20.0707419988328,122.714718839224)) ;
#35992 = CARTESIAN_POINT('Ctrl Pts',(-20.5584598459099,20.2606168495867,123.045995752101)) ;
#35993 = CARTESIAN_POINT('Ctrl Pts',(-20.8457638320902,20.0806277691768,122.954554133182)) ;
#35994 = CARTESIAN_POINT('Ctrl Pts',(-20.6046719527906,20.2706794469754,123.252408259714)) ;
#35995 = CARTESIAN_POINT('Ctrl Pts',(-20.9035264744634,20.0906903665656,123.212570178588)) ;
#35996 = CARTESIAN_POINT('Ctrl Pts',(-20.6142327360248,20.2805298588107,123.459290301903)) ;
#35997 = CARTESIAN_POINT('Ctrl Pts',(-20.9154749498567,20.1005407784008,123.471173528854)) ;
#35998 = CARTESIAN_POINT('Ctrl Pts',(-20.5877918422668,20.2905570280966,123.668422397058)) ;
#35999 = CARTESIAN_POINT('Ctrl Pts',(-20.8824212203994,20.1105679476868,123.7325883034)) ;
#36000 = CARTESIAN_POINT('Ctrl Pts',(-20.5249072417576,20.3005845088108,123.869644711752)) ;
#36001 = CARTESIAN_POINT('Ctrl Pts',(-20.803813048132,20.120595428401,123.984115444754)) ;
#36002 = CARTESIAN_POINT('Ctrl Pts',(-20.4301831206918,20.3104275613901,124.053614638865)) ;
#36003 = CARTESIAN_POINT('Ctrl Pts',(-20.6854052877138,20.1304384809802,124.214077225358)) ;
#36004 = CARTESIAN_POINT('Ctrl Pts',(-20.3034580062551,20.3204214648287,124.221197227413)) ;
#36005 = CARTESIAN_POINT('Ctrl Pts',(-20.5269966913831,20.1404323844189,124.423553915881)) ;
#36006 = CARTESIAN_POINT('Ctrl Pts',(-20.1487806009657,20.3304485876051,124.364425720184)) ;
#36007 = CARTESIAN_POINT('Ctrl Pts',(-20.3336481312911,20.1504595071953,124.602587618379)) ;
#36008 = CARTESIAN_POINT('Ctrl Pts',(-19.9741372933805,20.3403392924971,124.477286085174)) ;
#36009 = CARTESIAN_POINT('Ctrl Pts',(-20.1153421999281,20.1603502120873,124.743661057591)) ;
#36010 = CARTESIAN_POINT('Ctrl Pts',(-19.7807153610016,20.3503313193475,124.559212631353)) ;
#36011 = CARTESIAN_POINT('Ctrl Pts',(-19.8735636289023,20.1703422389376,124.846066786596)) ;
#36012 = CARTESIAN_POINT('Ctrl Pts',(-19.5769304517105,20.360277300836,124.606034161387)) ;
#36013 = CARTESIAN_POINT('Ctrl Pts',(-19.618831660726,20.1802882204262,124.904591118411)) ;
#36014 = CARTESIAN_POINT('Ctrl Pts',(-19.3680954416651,20.3702244734579,124.617184177661)) ;
#36015 = CARTESIAN_POINT('Ctrl Pts',(-19.3577875500311,20.1902353930481,124.918525903607)) ;
#36016 = CARTESIAN_POINT('Ctrl Pts',(-19.1584407875054,20.3802724147841,124.591416106205)) ;
#36017 = CARTESIAN_POINT('Ctrl Pts',(-19.095719576205,20.2002833343742,124.886313111821)) ;
#36018 = CARTESIAN_POINT('Ctrl Pts',(-18.9604121411015,20.3901200485918,124.531032969309)) ;
#36019 = CARTESIAN_POINT('Ctrl Pts',(-18.8481841830394,20.210130968182,124.810831448452)) ;
#36020 = CARTESIAN_POINT('Ctrl Pts',(-18.7734517586268,20.4000817632769,124.436686230099)) ;
#36021 = CARTESIAN_POINT('Ctrl Pts',(-18.6144848556616,20.2200926828671,124.692895466092)) ;
#36022 = CARTESIAN_POINT('Ctrl Pts',(-18.604728389867,20.4101103961554,124.310240172556)) ;
#36023 = CARTESIAN_POINT('Ctrl Pts',(-18.4035822759997,20.2301213157456,124.534835645164)) ;
#36024 = CARTESIAN_POINT('Ctrl Pts',(-18.4621885899076,20.4200207216905,124.158296132863)) ;
#36025 = CARTESIAN_POINT('Ctrl Pts',(-18.2254094105171,20.2400316412807,124.344903540078)) ;
#36026 = CARTESIAN_POINT('Ctrl Pts',(-18.3474529168086,20.4299555521623,123.983766306947)) ;
#36027 = CARTESIAN_POINT('Ctrl Pts',(-18.0819921053429,20.2499664717524,124.126739575405)) ;
#36028 = CARTESIAN_POINT('Ctrl Pts',(-18.2640446601778,20.4399968845442,123.789842819283)) ;
#36029 = CARTESIAN_POINT('Ctrl Pts',(-17.9777343204526,20.2600078041344,123.884334153657)) ;
#36030 = CARTESIAN_POINT('Ctrl Pts',(-18.21621844815,20.4498897579831,123.587439108983)) ;
#36031 = CARTESIAN_POINT('Ctrl Pts',(-17.9179543451556,20.2699006775733,123.631328380926)) ;
#36032 = CARTESIAN_POINT('Ctrl Pts',(-18.203638204828,20.459858923801,123.378224162259)) ;
#36033 = CARTESIAN_POINT('Ctrl Pts',(-17.9022315155995,20.2798698433911,123.369810686239)) ;
#36034 = CARTESIAN_POINT('Ctrl Pts',(-18.2280625767773,20.4698876575175,123.168828358653)) ;
#36035 = CARTESIAN_POINT('Ctrl Pts',(-17.9327660606948,20.2898985771077,123.108061591315)) ;
#36036 = CARTESIAN_POINT('Ctrl Pts',(-18.3069889150334,20.4830801762886,122.902870280924)) ;
#36037 = CARTESIAN_POINT('Ctrl Pts',(-18.0314212955399,20.3030910958788,122.775637805925)) ;
#36038 = CARTESIAN_POINT('Ctrl Pts',(-18.4552942626579,20.4964400443313,122.660681326423)) ;
#36039 = CARTESIAN_POINT('Ctrl Pts',(-18.2167817772331,20.3164509639215,122.472918789016)) ;
#36040 = CARTESIAN_POINT('Ctrl Pts',(-18.657015951964,20.5096653814802,122.469309191778)) ;
#36041 = CARTESIAN_POINT('Ctrl Pts',(-18.4689719566791,20.3296763010703,122.233665328746)) ;
#36042 = CARTESIAN_POINT('Ctrl Pts',(-18.8316741273677,20.5196466073208,122.353005072726)) ;
#36043 = CARTESIAN_POINT('Ctrl Pts',(-18.6872891439272,20.339657526911,122.088295732231)) ;
#36044 = CARTESIAN_POINT('Ctrl Pts',(-19.0250769115555,20.5296821743037,122.268720045023)) ;
#36045 = CARTESIAN_POINT('Ctrl Pts',(-18.9290457583326,20.3496930938939,121.982939786395)) ;
#36046 = CARTESIAN_POINT('Ctrl Pts',(-19.2265825671295,20.5395452522658,122.219728041552)) ;
#36047 = CARTESIAN_POINT('Ctrl Pts',(-19.1809279027558,20.3595561718559,121.921703115425)) ;
#36048 = CARTESIAN_POINT('Ctrl Pts',(-19.4378331047405,20.5496155510669,122.206147359895)) ;
#36049 = CARTESIAN_POINT('Ctrl Pts',(-19.4449915418414,20.369626470657,121.90472989406)) ;
#36050 = CARTESIAN_POINT('Ctrl Pts',(-19.6434998813334,20.5594578496347,122.228940856017)) ;
#36051 = CARTESIAN_POINT('Ctrl Pts',(-19.7020745055616,20.3794687692249,121.933224576269)) ;
#36052 = CARTESIAN_POINT('Ctrl Pts',(-19.8446762990893,20.5694185478045,122.287051453372)) ;
#36053 = CARTESIAN_POINT('Ctrl Pts',(-19.9535442297023,20.3894294673946,122.005865433009)) ;
#36054 = CARTESIAN_POINT('Ctrl Pts',(-20.0339789138857,20.579456581984,122.380301038949)) ;
#36055 = CARTESIAN_POINT('Ctrl Pts',(-20.1901714045635,20.3994675015741,122.122429978449)) ;
#36056 = CARTESIAN_POINT('Ctrl Pts',(-20.2016869726508,20.5893303188304,122.50266789996)) ;
#36057 = CARTESIAN_POINT('Ctrl Pts',(-20.3998046709524,20.4093412384206,122.275390622906)) ;
#36058 = CARTESIAN_POINT('Ctrl Pts',(-20.3484287632797,20.5994021027557,122.65527287763)) ;
#36059 = CARTESIAN_POINT('Ctrl Pts',(-20.5832300951719,20.4194130223459,122.466148916906)) ;
#36060 = CARTESIAN_POINT('Ctrl Pts',(-20.4637684790007,20.6092342239569,122.82682741127)) ;
#36061 = CARTESIAN_POINT('Ctrl Pts',(-20.7274022481796,20.429245143547,122.680593266566)) ;
#36062 = CARTESIAN_POINT('Ctrl Pts',(-20.549786388294,20.6192672479823,123.019405571818)) ;
#36063 = CARTESIAN_POINT('Ctrl Pts',(-20.8349222723643,20.4392781675725,122.921317142766)) ;
#36064 = CARTESIAN_POINT('Ctrl Pts',(-20.600454739304,20.629283128179,123.223797814881)) ;
#36065 = CARTESIAN_POINT('Ctrl Pts',(-20.8982551028601,20.4492940477692,123.176808341206)) ;
#36066 = CARTESIAN_POINT('Ctrl Pts',(-20.6150583626326,20.6391666472732,123.431067002261)) ;
#36067 = CARTESIAN_POINT('Ctrl Pts',(-20.9165069215873,20.4591775668633,123.435894221685)) ;
#36068 = CARTESIAN_POINT('Ctrl Pts',(-20.5934884418527,20.6491570596368,123.639971139436)) ;
#36069 = CARTESIAN_POINT('Ctrl Pts',(-20.8895420040993,20.469167979227,123.697025786591)) ;
#36070 = CARTESIAN_POINT('Ctrl Pts',(-20.5172126026985,20.6624202228403,123.908195883155)) ;
#36071 = CARTESIAN_POINT('Ctrl Pts',(-20.7941934592288,20.4824311424304,124.032297262021)) ;
#36072 = CARTESIAN_POINT('Ctrl Pts',(-20.3727499039758,20.6756977930915,124.150760947289)) ;
#36073 = CARTESIAN_POINT('Ctrl Pts',(-20.6136449750528,20.4957087126816,124.335469275546)) ;
#36074 = CARTESIAN_POINT('Ctrl Pts',(-20.1718067412588,20.6890280955981,124.346077378148)) ;
#36075 = CARTESIAN_POINT('Ctrl Pts',(-20.3624251620804,20.5090390151882,124.579659196416)) ;
#36076 = CARTESIAN_POINT('Ctrl Pts',(-19.9998354457734,20.6989267774145,124.463273965374)) ;
#36077 = CARTESIAN_POINT('Ctrl Pts',(-20.1474678125602,20.5189376970046,124.726143222235)) ;
#36078 = CARTESIAN_POINT('Ctrl Pts',(-19.8085029004183,20.708916292462,124.549834225346)) ;
#36079 = CARTESIAN_POINT('Ctrl Pts',(-19.9082988338511,20.5289272120522,124.834343756677)) ;
#36080 = CARTESIAN_POINT('Ctrl Pts',(-19.6058699471084,20.718864344237,124.601638834298)) ;
#36081 = CARTESIAN_POINT('Ctrl Pts',(-19.65500875944,20.5388752638272,124.899096739241)) ;
#36082 = CARTESIAN_POINT('Ctrl Pts',(-19.3975069469639,20.7288057475155,124.617723893743)) ;
#36083 = CARTESIAN_POINT('Ctrl Pts',(-19.3945515389807,20.5488166671057,124.91919968873)) ;
#36084 = CARTESIAN_POINT('Ctrl Pts',(-19.1194310874959,20.7420924122965,124.5908661902)) ;
#36085 = CARTESIAN_POINT('Ctrl Pts',(-19.0469745336925,20.5621033318866,124.885630332434)) ;
#36086 = CARTESIAN_POINT('Ctrl Pts',(-18.7886547609525,20.7587028339513,124.467201444823)) ;
#36087 = CARTESIAN_POINT('Ctrl Pts',(-18.6334863377583,20.5787137535414,124.731039345146)) ;
#36088 = CARTESIAN_POINT('Ctrl Pts',(-18.4662665698674,20.7786140962021,124.192751228819)) ;
#36089 = CARTESIAN_POINT('Ctrl Pts',(-18.2305106418052,20.5986250157922,124.387975748698)) ;
#36090 = CARTESIAN_POINT('Ctrl Pts',(-18.2563995968813,20.7985582253669,123.82423191738)) ;
#36091 = CARTESIAN_POINT('Ctrl Pts',(-17.9681790721331,20.6185691449571,123.927324296511)) ;
#36092 = CARTESIAN_POINT('Ctrl Pts',(-18.1850241779996,20.8184813879721,123.406707624286)) ;
#36093 = CARTESIAN_POINT('Ctrl Pts',(-17.8789643903476,20.6384923075623,123.405418987404)) ;
#36094 = CARTESIAN_POINT('Ctrl Pts',(-18.2596109544151,20.8383715103787,122.990352378829)) ;
#36095 = CARTESIAN_POINT('Ctrl Pts',(-17.9722011637848,20.6583824299688,122.884976490785)) ;
#36096 = CARTESIAN_POINT('Ctrl Pts',(-18.4732404987063,20.8583764639788,122.622607393527)) ;
#36097 = CARTESIAN_POINT('Ctrl Pts',(-18.2392413285388,20.678387383569,122.425297035584)) ;
#36098 = CARTESIAN_POINT('Ctrl Pts',(-18.7967167999957,20.8782147209944,122.351758323974)) ;
#36099 = CARTESIAN_POINT('Ctrl Pts',(-18.643587622069,20.6982256405846,122.086739272728)) ;
#36100 = CARTESIAN_POINT('Ctrl Pts',(-19.1960471170997,20.8982090217809,122.206055805286)) ;
#36101 = CARTESIAN_POINT('Ctrl Pts',(-19.1427514572013,20.7182199413711,121.90461393122)) ;
#36102 = CARTESIAN_POINT('Ctrl Pts',(-19.6188717893715,20.9180942638254,122.205753928318)) ;
#36103 = CARTESIAN_POINT('Ctrl Pts',(-19.6712810445399,20.7381051834155,121.90423957277)) ;
#36104 = CARTESIAN_POINT('Ctrl Pts',(-20.0166066720332,20.9379692103013,122.348559948617)) ;
#36105 = CARTESIAN_POINT('Ctrl Pts',(-20.1684474704946,20.7579801298915,122.082748587441)) ;
#36106 = CARTESIAN_POINT('Ctrl Pts',(-20.3441382460836,20.9580022802424,122.620951616946)) ;
#36107 = CARTESIAN_POINT('Ctrl Pts',(-20.5778609765498,20.7780131998326,122.423240113324)) ;
#36108 = CARTESIAN_POINT('Ctrl Pts',(-20.5570102326951,20.9778907871428,122.986308371611)) ;
#36109 = CARTESIAN_POINT('Ctrl Pts',(-20.8439482663196,20.797901706733,122.879935963117)) ;
#36110 = CARTESIAN_POINT('Ctrl Pts',(-20.6337603887322,20.9977456469241,123.401507209435)) ;
#36111 = CARTESIAN_POINT('Ctrl Pts',(-20.9398845190647,20.8177565665142,123.398932664503)) ;
#36112 = CARTESIAN_POINT('Ctrl Pts',(-20.5628715307167,21.0177964807118,123.821804823539)) ;
#36113 = CARTESIAN_POINT('Ctrl Pts',(-20.851271999308,20.837807400302,123.92430520719)) ;
#36114 = CARTESIAN_POINT('Ctrl Pts',(-20.356096985501,21.037562422601,124.187831810963)) ;
#36115 = CARTESIAN_POINT('Ctrl Pts',(-20.5928049105319,20.8575733421912,124.381835472943)) ;
#36116 = CARTESIAN_POINT('Ctrl Pts',(-20.0335794669859,21.0575751540604,124.465226345288)) ;
#36117 = CARTESIAN_POINT('Ctrl Pts',(-20.1896580437977,20.8775860736505,124.728578782412)) ;
#36118 = CARTESIAN_POINT('Ctrl Pts',(-19.637720643514,21.0774679890039,124.614558860712)) ;
#36119 = CARTESIAN_POINT('Ctrl Pts',(-19.6948360554423,20.8974789085941,124.91524382122)) ;
#36120 = CARTESIAN_POINT('Ctrl Pts',(-19.214589507988,21.0973750123435,124.620545648609)) ;
#36121 = CARTESIAN_POINT('Ctrl Pts',(-19.1659236264402,20.9173859319337,124.922728040003)) ;
#36122 = CARTESIAN_POINT('Ctrl Pts',(-18.8142996405734,21.1172902772442,124.482107958723)) ;
#36123 = CARTESIAN_POINT('Ctrl Pts',(-18.6655619226655,20.9373011968343,124.749682544209)) ;
#36124 = CARTESIAN_POINT('Ctrl Pts',(-18.4838027384896,21.1373219694039,124.213487981599)) ;
#36125 = CARTESIAN_POINT('Ctrl Pts',(-18.252439701957,20.9573328889941,124.413908184247)) ;
#36126 = CARTESIAN_POINT('Ctrl Pts',(-18.2668088815555,21.1571650159769,123.851596586135)) ;
#36127 = CARTESIAN_POINT('Ctrl Pts',(-17.9811972980463,20.9771759355671,123.961546540822)) ;
#36128 = CARTESIAN_POINT('Ctrl Pts',(-18.1851023806558,21.1770815638767,123.436137199122)) ;
#36129 = CARTESIAN_POINT('Ctrl Pts',(-17.8790621516015,20.9970924834669,123.442223784008)) ;
#36130 = CARTESIAN_POINT('Ctrl Pts',(-18.2502145798426,21.197013806868,123.017317548737)) ;
#36131 = CARTESIAN_POINT('Ctrl Pts',(-17.9604499278129,21.0170247264581,122.918699625123)) ;
#36132 = CARTESIAN_POINT('Ctrl Pts',(-18.453820244144,21.2169176416773,122.646330539081)) ;
#36133 = CARTESIAN_POINT('Ctrl Pts',(-18.2149540833388,21.0369285612675,122.454965536669)) ;
#36134 = CARTESIAN_POINT('Ctrl Pts',(-18.771411200767,21.2368180418648,122.366728476114)) ;
#36135 = CARTESIAN_POINT('Ctrl Pts',(-18.6119399165711,21.056828961455,122.105461255076)) ;
#36136 = CARTESIAN_POINT('Ctrl Pts',(-19.1662802143597,21.2567677182441,122.211733257638)) ;
#36137 = CARTESIAN_POINT('Ctrl Pts',(-19.1055245266933,21.0767786378343,121.911714229282)) ;
#36138 = CARTESIAN_POINT('Ctrl Pts',(-19.5899666832492,21.2767002424645,122.200890341999)) ;
#36139 = CARTESIAN_POINT('Ctrl Pts',(-19.6351319246328,21.0967111620546,121.898157077983)) ;
#36140 = CARTESIAN_POINT('Ctrl Pts',(-19.9918071979918,21.2966202514507,122.334860446379)) ;
#36141 = CARTESIAN_POINT('Ctrl Pts',(-20.1374331359612,21.1166311710408,122.065615887808)) ;
#36142 = CARTESIAN_POINT('Ctrl Pts',(-20.3243261883736,21.3165771576268,122.598408286184)) ;
#36143 = CARTESIAN_POINT('Ctrl Pts',(-20.5530840766553,21.136588077217,122.395047352142)) ;
#36144 = CARTESIAN_POINT('Ctrl Pts',(-20.5465500206849,21.3364629971283,122.958223520543)) ;
#36145 = CARTESIAN_POINT('Ctrl Pts',(-20.8308668600017,21.1564739167185,122.844813593055)) ;
#36146 = CARTESIAN_POINT('Ctrl Pts',(-20.6329313729834,21.3564341692642,123.373889795751)) ;
#36147 = CARTESIAN_POINT('Ctrl Pts',(-20.9388483134395,21.1764450888544,123.364394953385)) ;
#36148 = CARTESIAN_POINT('Ctrl Pts',(-20.5733172895036,21.3762483662486,123.791020354018)) ;
#36149 = CARTESIAN_POINT('Ctrl Pts',(-20.8643333248792,21.1962592858388,123.885809151941)) ;
#36150 = CARTESIAN_POINT('Ctrl Pts',(-20.3738339937494,21.3962295522168,124.166047638378)) ;
#36151 = CARTESIAN_POINT('Ctrl Pts',(-20.614991472528,21.216240471807,124.35458992432)) ;
#36152 = CARTESIAN_POINT('Ctrl Pts',(-20.1119197884198,21.4128050576061,124.401919568806)) ;
#36153 = CARTESIAN_POINT('Ctrl Pts',(-20.287577123205,21.2328159771962,124.649450004778)) ;
#36154 = CARTESIAN_POINT('Ctrl Pts',(-19.8627851378671,21.4261145054697,124.529357888635)) ;
#36155 = CARTESIAN_POINT('Ctrl Pts',(-19.9761906951506,21.2461254250599,124.808734121351)) ;
#36156 = CARTESIAN_POINT('Ctrl Pts',(-19.5941578117551,21.4394822032463,124.611771760159)) ;
#36157 = CARTESIAN_POINT('Ctrl Pts',(-19.6403422561872,21.2594931228365,124.911767929995)) ;
#36158 = CARTESIAN_POINT('Ctrl Pts',(-19.2437108626746,21.4559727749122,124.6246956008)) ;
#36159 = CARTESIAN_POINT('Ctrl Pts',(-19.2023540010319,21.2759836945023,124.927912591816)) ;
#36160 = CARTESIAN_POINT('Ctrl Pts',(-18.8402511753296,21.475893047245,124.495996346843)) ;
#36161 = CARTESIAN_POINT('Ctrl Pts',(-18.6980130161418,21.2959039668352,124.767055416111)) ;
#36162 = CARTESIAN_POINT('Ctrl Pts',(-18.5605799960303,21.492510082966,124.28007609183)) ;
#36163 = CARTESIAN_POINT('Ctrl Pts',(-18.3484015779362,21.3125210025561,124.497134075303)) ;
#36164 = CARTESIAN_POINT('Ctrl Pts',(-18.3909714744252,21.5058009332471,124.057970104108)) ;
#36165 = CARTESIAN_POINT('Ctrl Pts',(-18.1364098503335,21.3258118528373,124.219524949663)) ;
#36166 = CARTESIAN_POINT('Ctrl Pts',(-18.2945586514006,21.5157699784016,123.871912739408)) ;
#36167 = CARTESIAN_POINT('Ctrl Pts',(-18.015887138759,21.3357808979917,123.986950081611)) ;
#36168 = CARTESIAN_POINT('Ctrl Pts',(-18.2319181244892,21.5256733690351,123.673331471138)) ;
#36169 = CARTESIAN_POINT('Ctrl Pts',(-17.9375848219048,21.3456842886253,123.738726404517)) ;
#36170 = CARTESIAN_POINT('Ctrl Pts',(-18.2044053248853,21.5357311551478,123.46370878248)) ;
#36171 = CARTESIAN_POINT('Ctrl Pts',(-17.9031917372576,21.355742074738,123.47669498645)) ;
#36172 = CARTESIAN_POINT('Ctrl Pts',(-18.213339943562,21.5455831917976,123.256751493961)) ;
#36173 = CARTESIAN_POINT('Ctrl Pts',(-17.9143537184473,21.3655941113878,123.218009520756)) ;
#36174 = CARTESIAN_POINT('Ctrl Pts',(-18.2735424653214,21.5589483159408,122.982353800711)) ;
#36175 = CARTESIAN_POINT('Ctrl Pts',(-17.9896212280207,21.378959235531,122.874956967983)) ;
#36176 = CARTESIAN_POINT('Ctrl Pts',(-18.4029674767116,21.5721743789038,122.732632420697)) ;
#36177 = CARTESIAN_POINT('Ctrl Pts',(-18.1513956642549,21.392185298494,122.562838107793)) ;
#36178 = CARTESIAN_POINT('Ctrl Pts',(-18.5911529593693,21.5854780271861,122.525730956398)) ;
#36179 = CARTESIAN_POINT('Ctrl Pts',(-18.3866109363126,21.4054889467763,122.304222180904)) ;
#36180 = CARTESIAN_POINT('Ctrl Pts',(-18.7572783870989,21.5954695583491,122.397143887496)) ;
#36181 = CARTESIAN_POINT('Ctrl Pts',(-18.5942688365446,21.4154804779393,122.143483381853)) ;
#36182 = CARTESIAN_POINT('Ctrl Pts',(-18.9441977840221,21.6055090061484,122.299154895599)) ;
#36183 = CARTESIAN_POINT('Ctrl Pts',(-18.8279161165518,21.4255199257386,122.020995347781)) ;
#36184 = CARTESIAN_POINT('Ctrl Pts',(-19.1413056725189,21.6153527816622,122.236053528025)) ;
#36185 = CARTESIAN_POINT('Ctrl Pts',(-19.0743002770626,21.4353637012524,121.942115783789)) ;
#36186 = CARTESIAN_POINT('Ctrl Pts',(-19.3492278326637,21.6253384230499,122.207322375982)) ;
#36187 = CARTESIAN_POINT('Ctrl Pts',(-19.3342026170247,21.4453493426401,121.906199088032)) ;
#36188 = CARTESIAN_POINT('Ctrl Pts',(-19.5580238062598,21.6352752074117,122.21497981521)) ;
#36189 = CARTESIAN_POINT('Ctrl Pts',(-19.5951977714933,21.4552861270019,121.91576806339)) ;
#36190 = CARTESIAN_POINT('Ctrl Pts',(-19.7645659584739,21.645325041879,122.259368244298)) ;
#36191 = CARTESIAN_POINT('Ctrl Pts',(-19.8533761100118,21.4653359614692,121.971250859227)) ;
#36192 = CARTESIAN_POINT('Ctrl Pts',(-19.9564732011589,21.6551754913822,122.337234509043)) ;
#36193 = CARTESIAN_POINT('Ctrl Pts',(-20.0932613279301,21.4751864109724,122.068581121227)) ;
#36194 = CARTESIAN_POINT('Ctrl Pts',(-20.1343652145138,21.6651475053643,122.448110905834)) ;
#36195 = CARTESIAN_POINT('Ctrl Pts',(-20.3156279273217,21.4851584249544,122.207174295896)) ;
#36196 = CARTESIAN_POINT('Ctrl Pts',(-20.2906914128935,21.6751426632114,122.588577277018)) ;
#36197 = CARTESIAN_POINT('Ctrl Pts',(-20.5110376062556,21.4951535828016,122.382755229648)) ;
#36198 = CARTESIAN_POINT('Ctrl Pts',(-20.4205236147211,21.6851765895751,122.754811362263)) ;
#36199 = CARTESIAN_POINT('Ctrl Pts',(-20.6733301023757,21.5051875091653,122.590546133559)) ;
#36200 = CARTESIAN_POINT('Ctrl Pts',(-20.5180643029118,21.6950322980075,122.937635457501)) ;
#36201 = CARTESIAN_POINT('Ctrl Pts',(-20.7952585398595,21.5150432175976,122.819075138362)) ;
#36202 = CARTESIAN_POINT('Ctrl Pts',(-20.5835791686227,21.7050304473461,123.137322140165)) ;
#36203 = CARTESIAN_POINT('Ctrl Pts',(-20.8771547989075,21.5250413669363,123.068682710127)) ;
#36204 = CARTESIAN_POINT('Ctrl Pts',(-20.6133259213828,21.7149298505197,123.343332794389)) ;
#36205 = CARTESIAN_POINT('Ctrl Pts',(-20.9143410126889,21.5349407701099,123.326195883174)) ;
#36206 = CARTESIAN_POINT('Ctrl Pts',(-20.6067986597741,21.7249810474082,123.554517472211)) ;
#36207 = CARTESIAN_POINT('Ctrl Pts',(-20.9061847000465,21.5449919669983,123.590176807793)) ;
#36208 = CARTESIAN_POINT('Ctrl Pts',(-20.5644486467122,21.734863371221,123.757928803125)) ;
#36209 = CARTESIAN_POINT('Ctrl Pts',(-20.8532498235943,21.5548742908112,123.844441837928)) ;
#36210 = CARTESIAN_POINT('Ctrl Pts',(-20.4869932248377,21.7448582668776,123.953249465948)) ;
#36211 = CARTESIAN_POINT('Ctrl Pts',(-20.7564330307127,21.5648691864678,124.088593766692)) ;
#36212 = CARTESIAN_POINT('Ctrl Pts',(-20.376239486151,21.7548793662602,124.132475484503)) ;
#36213 = CARTESIAN_POINT('Ctrl Pts',(-20.6179931769502,21.5748902858503,124.312627761406)) ;
#36214 = CARTESIAN_POINT('Ctrl Pts',(-20.2377724390061,21.7647866341222,124.288062190397)) ;
#36215 = CARTESIAN_POINT('Ctrl Pts',(-20.4449112035146,21.5847975537124,124.507113190918)) ;
#36216 = CARTESIAN_POINT('Ctrl Pts',(-20.0741502835799,21.7747249779475,124.417970243514)) ;
#36217 = CARTESIAN_POINT('Ctrl Pts',(-20.2403849662949,21.5947358975377,124.669500522517)) ;
#36218 = CARTESIAN_POINT('Ctrl Pts',(-19.8892850130631,21.784728397248,124.518280702167)) ;
#36219 = CARTESIAN_POINT('Ctrl Pts',(-20.0093045735682,21.6047393168382,124.794890972802)) ;
#36220 = CARTESIAN_POINT('Ctrl Pts',(-19.6891120590807,21.7947629479551,124.584833460336)) ;
#36221 = CARTESIAN_POINT('Ctrl Pts',(-19.7590892507581,21.6147738675453,124.878084487148)) ;
#36222 = CARTESIAN_POINT('Ctrl Pts',(-19.484395225653,21.8046078975607,124.615389634734)) ;
#36223 = CARTESIAN_POINT('Ctrl Pts',(-19.5031930456701,21.6246188171509,124.916282417734)) ;
#36224 = CARTESIAN_POINT('Ctrl Pts',(-19.2745575619711,21.8145937396736,124.610253310873)) ;
#36225 = CARTESIAN_POINT('Ctrl Pts',(-19.2408957415277,21.6346046592638,124.909864611277)) ;
#36226 = CARTESIAN_POINT('Ctrl Pts',(-19.0697507053397,21.8245285470427,124.569104542372)) ;
#36227 = CARTESIAN_POINT('Ctrl Pts',(-18.9848863453613,21.6445394666328,124.858431106642)) ;
#36228 = CARTESIAN_POINT('Ctrl Pts',(-18.8729297754626,21.834586088756,124.491928841901)) ;
#36229 = CARTESIAN_POINT('Ctrl Pts',(-18.738859338047,21.6545970083461,124.761963952315)) ;
#36230 = CARTESIAN_POINT('Ctrl Pts',(-18.6965214907536,21.8444076862681,124.384579575107)) ;
#36231 = CARTESIAN_POINT('Ctrl Pts',(-18.5183469904229,21.6644186058583,124.62777914016)) ;
#36232 = CARTESIAN_POINT('Ctrl Pts',(-18.5374995717357,21.8544639457486,124.245294446865)) ;
#36233 = CARTESIAN_POINT('Ctrl Pts',(-18.3195680415118,21.6744748653387,124.453674665884)) ;
#36234 = CARTESIAN_POINT('Ctrl Pts',(-18.4068771812102,21.864403882049,124.082167341671)) ;
#36235 = CARTESIAN_POINT('Ctrl Pts',(-18.156287854602,21.6844148016391,124.249767117472)) ;
#36236 = CARTESIAN_POINT('Ctrl Pts',(-18.3063513222259,21.8743110027934,123.899756894152)) ;
#36237 = CARTESIAN_POINT('Ctrl Pts',(-18.0306281551785,21.6943219223836,124.02175476564)) ;
#36238 = CARTESIAN_POINT('Ctrl Pts',(-18.2381764644266,21.8843539087187,123.699938324222)) ;
#36239 = CARTESIAN_POINT('Ctrl Pts',(-17.9454073047727,21.7043648283088,123.771982422698)) ;
#36240 = CARTESIAN_POINT('Ctrl Pts',(-18.2061259507257,21.8942616898179,123.494118034549)) ;
#36241 = CARTESIAN_POINT('Ctrl Pts',(-17.9053416811519,21.714272609408,123.514706921446)) ;
#36242 = CARTESIAN_POINT('Ctrl Pts',(-18.2099726092004,21.9042720588203,123.283696769241)) ;
#36243 = CARTESIAN_POINT('Ctrl Pts',(-17.9101476584396,21.7242829784104,123.251680239074)) ;
#36244 = CARTESIAN_POINT('Ctrl Pts',(-18.250799150117,21.9143028973891,123.076808306462)) ;
#36245 = CARTESIAN_POINT('Ctrl Pts',(-17.9611784249109,21.7343138169792,122.993069232997)) ;
#36246 = CARTESIAN_POINT('Ctrl Pts',(-18.3252324167252,21.9241557370288,122.88350173726)) ;
#36247 = CARTESIAN_POINT('Ctrl Pts',(-18.0542181018734,21.7441666566189,122.751434398964)) ;
#36248 = CARTESIAN_POINT('Ctrl Pts',(-18.4332250657028,21.9341437381937,122.703441071799)) ;
#36249 = CARTESIAN_POINT('Ctrl Pts',(-18.189207059747,21.7541546577839,122.526357242262)) ;
#36250 = CARTESIAN_POINT('Ctrl Pts',(-18.5700375225545,21.9440725571729,122.545786789656)) ;
#36251 = CARTESIAN_POINT('Ctrl Pts',(-18.3602212352636,21.7640834767631,122.329287537154)) ;
#36252 = CARTESIAN_POINT('Ctrl Pts',(-18.732888520769,21.9540602598952,122.413224493809)) ;
#36253 = CARTESIAN_POINT('Ctrl Pts',(-18.5637837492415,21.7740711794854,122.16358286203)) ;
#36254 = CARTESIAN_POINT('Ctrl Pts',(-18.9173249515201,21.9640962596979,122.31077716545)) ;
#36255 = CARTESIAN_POINT('Ctrl Pts',(-18.7943281091717,21.7841071792881,122.035521757749)) ;
#36256 = CARTESIAN_POINT('Ctrl Pts',(-19.1130605451374,21.9739511294993,122.242820238378)) ;
#36257 = CARTESIAN_POINT('Ctrl Pts',(-19.0389977515647,21.7939620490895,121.950573238967)) ;
#36258 = CARTESIAN_POINT('Ctrl Pts',(-19.3205261715052,21.9839505599228,122.209124296924)) ;
#36259 = CARTESIAN_POINT('Ctrl Pts',(-19.298329579095,21.803961479513,121.908451210336)) ;
#36260 = CARTESIAN_POINT('Ctrl Pts',(-19.5285708919945,21.9938456773881,122.211711498228)) ;
#36261 = CARTESIAN_POINT('Ctrl Pts',(-19.5583862374027,21.8138565969783,121.911683181333)) ;
#36262 = CARTESIAN_POINT('Ctrl Pts',(-19.7363587174108,22.0039061709051,122.251037909545)) ;
#36263 = CARTESIAN_POINT('Ctrl Pts',(-19.8181211650705,21.8239170904953,121.960839136464)) ;
#36264 = CARTESIAN_POINT('Ctrl Pts',(-19.9300913010617,22.0137556511063,122.324185172849)) ;
#36265 = CARTESIAN_POINT('Ctrl Pts',(-20.0602885784537,21.8337665706965,122.052271697225)) ;
#36266 = CARTESIAN_POINT('Ctrl Pts',(-20.1116425157324,22.0237821013701,122.431281071649)) ;
#36267 = CARTESIAN_POINT('Ctrl Pts',(-20.2872285090302,21.8437930209603,122.18613995206)) ;
#36268 = CARTESIAN_POINT('Ctrl Pts',(-20.2715450400608,22.0338133918482,122.568785511319)) ;
#36269 = CARTESIAN_POINT('Ctrl Pts',(-20.4871079315914,21.8538243114383,122.358018915005)) ;
#36270 = CARTESIAN_POINT('Ctrl Pts',(-20.4029602797824,22.0436547795,122.728588268752)) ;
#36271 = CARTESIAN_POINT('Ctrl Pts',(-20.65137916474,21.8636656990902,122.557772038518)) ;
#36272 = CARTESIAN_POINT('Ctrl Pts',(-20.5066507219347,22.0536581803912,122.911527607421)) ;
#36273 = CARTESIAN_POINT('Ctrl Pts',(-20.7809938112544,21.8736690999814,122.786445434029)) ;
#36274 = CARTESIAN_POINT('Ctrl Pts',(-20.5768052643418,22.0636425631824,123.109399042822)) ;
#36275 = CARTESIAN_POINT('Ctrl Pts',(-20.8686887483968,21.8836534827725,123.033784325638)) ;
#36276 = CARTESIAN_POINT('Ctrl Pts',(-20.6115199861339,22.0736816531958,123.317556791633)) ;
#36277 = CARTESIAN_POINT('Ctrl Pts',(-20.9120839655967,21.8936925727859,123.293981073997)) ;
#36278 = CARTESIAN_POINT('Ctrl Pts',(-20.6098913500393,22.0835274621049,123.524555130428)) ;
#36279 = CARTESIAN_POINT('Ctrl Pts',(-20.9100499299617,21.9035383816951,123.552730180822)) ;
#36280 = CARTESIAN_POINT('Ctrl Pts',(-20.5722452970051,22.0935118849239,123.731024894997)) ;
#36281 = CARTESIAN_POINT('Ctrl Pts',(-20.8629939223635,21.9135228045141,123.810817924697)) ;
#36282 = CARTESIAN_POINT('Ctrl Pts',(-20.4997117600218,22.1034515101651,123.927025671405)) ;
#36283 = CARTESIAN_POINT('Ctrl Pts',(-20.7723283117608,21.9234624297553,124.055819959663)) ;
#36284 = CARTESIAN_POINT('Ctrl Pts',(-20.3931662714284,22.1134911996838,124.109206689079)) ;
#36285 = CARTESIAN_POINT('Ctrl Pts',(-20.63914792108,21.933502119274,124.283546922081)) ;
#36286 = CARTESIAN_POINT('Ctrl Pts',(-20.2587285375417,22.1233793881024,124.267780927574)) ;
#36287 = CARTESIAN_POINT('Ctrl Pts',(-20.4711013651506,21.9433903076926,124.48176644605)) ;
#36288 = CARTESIAN_POINT('Ctrl Pts',(-20.0974265999504,22.1333689141044,124.402255862019)) ;
#36289 = CARTESIAN_POINT('Ctrl Pts',(-20.269474706559,21.9533798336946,124.649861364024)) ;
#36290 = CARTESIAN_POINT('Ctrl Pts',(-19.9157102403435,22.1433274154596,124.506217438115)) ;
#36291 = CARTESIAN_POINT('Ctrl Pts',(-20.0423296293175,21.9633383350498,124.779814856074)) ;
#36292 = CARTESIAN_POINT('Ctrl Pts',(-19.7200260725257,22.1532270094633,124.577119056446)) ;
#36293 = CARTESIAN_POINT('Ctrl Pts',(-19.7977240449939,21.9732379290534,124.868443422862)) ;
#36294 = CARTESIAN_POINT('Ctrl Pts',(-19.5119529377031,22.1632748975846,124.61342395275)) ;
#36295 = CARTESIAN_POINT('Ctrl Pts',(-19.5376330731209,21.9832858171747,124.913825837569)) ;
#36296 = CARTESIAN_POINT('Ctrl Pts',(-19.3038874510347,22.1731703228301,124.613217769104)) ;
#36297 = CARTESIAN_POINT('Ctrl Pts',(-19.2775503015468,21.9931812424203,124.913569399203)) ;
#36298 = CARTESIAN_POINT('Ctrl Pts',(-19.0956337768571,22.1832317135307,124.576318144067)) ;
#36299 = CARTESIAN_POINT('Ctrl Pts',(-19.0172333059116,22.0032426331209,124.867446190306)) ;
#36300 = CARTESIAN_POINT('Ctrl Pts',(-18.9011658613922,22.1930772972174,124.505398277424)) ;
#36301 = CARTESIAN_POINT('Ctrl Pts',(-18.7741467328154,22.0130882168075,124.778797095508)) ;
#36302 = CARTESIAN_POINT('Ctrl Pts',(-18.7194990589113,22.2030402705266,124.401179624215)) ;
#36303 = CARTESIAN_POINT('Ctrl Pts',(-18.5470623485629,22.0230511901167,124.648524437501)) ;
#36304 = CARTESIAN_POINT('Ctrl Pts',(-18.5578335683124,22.2130659373523,124.265923043721)) ;
#36305 = CARTESIAN_POINT('Ctrl Pts',(-18.3449798305137,22.0330768569425,124.47945461935)) ;
#36306 = CARTESIAN_POINT('Ctrl Pts',(-18.4235409053948,22.2229804152186,124.106527257626)) ;
#36307 = CARTESIAN_POINT('Ctrl Pts',(-18.177112665249,22.0429913348088,124.280209964975)) ;
#36308 = CARTESIAN_POINT('Ctrl Pts',(-18.3178094286118,22.2329689298936,123.925078039381)) ;
#36309 = CARTESIAN_POINT('Ctrl Pts',(-18.0449474119097,22.0529798494838,124.05339871137)) ;
#36310 = CARTESIAN_POINT('Ctrl Pts',(-18.2452217442394,22.2430130408091,123.726808026642)) ;
#36311 = CARTESIAN_POINT('Ctrl Pts',(-17.9542118486561,22.0630239603992,123.805561752145)) ;
#36312 = CARTESIAN_POINT('Ctrl Pts',(-18.2084565806548,22.2528411784036,123.523457249866)) ;
#36313 = CARTESIAN_POINT('Ctrl Pts',(-17.9082542484671,22.0728520979938,123.551371969029)) ;
#36314 = CARTESIAN_POINT('Ctrl Pts',(-18.2074383421507,22.2629177464626,123.311661356134)) ;
#36315 = CARTESIAN_POINT('Ctrl Pts',(-17.9069805911585,22.0829286660527,123.286627562754)) ;
#36316 = CARTESIAN_POINT('Ctrl Pts',(-18.2423241793869,22.2727699083667,123.107451203336)) ;
#36317 = CARTESIAN_POINT('Ctrl Pts',(-17.9505873021255,22.0927808279569,123.031363437646)) ;
#36318 = CARTESIAN_POINT('Ctrl Pts',(-18.3135102543039,22.2828428703236,122.908047647564)) ;
#36319 = CARTESIAN_POINT('Ctrl Pts',(-18.0395690379803,22.1028537899137,122.782109150531)) ;
#36320 = CARTESIAN_POINT('Ctrl Pts',(-18.4158946807527,22.2926854323265,122.728210968454)) ;
#36321 = CARTESIAN_POINT('Ctrl Pts',(-18.1675496052285,22.1126963519166,122.557311692055)) ;
#36322 = CARTESIAN_POINT('Ctrl Pts',(-18.549238880053,22.3026658688203,122.566223969324)) ;
#36323 = CARTESIAN_POINT('Ctrl Pts',(-18.3342296704848,22.1226767884104,122.354827390297)) ;
#36324 = CARTESIAN_POINT('Ctrl Pts',(-18.7095577945463,22.3126841741447,122.429637874185)) ;
#36325 = CARTESIAN_POINT('Ctrl Pts',(-18.5346278830322,22.1326950937348,122.184094280937)) ;
#36326 = CARTESIAN_POINT('Ctrl Pts',(-18.8885239198384,22.3225681380641,122.324009756949)) ;
#36327 = CARTESIAN_POINT('Ctrl Pts',(-18.7583362356208,22.1425790576543,122.052058163441)) ;
#36328 = CARTESIAN_POINT('Ctrl Pts',(-19.0866690738758,22.3326340148027,122.249785568809)) ;
#36329 = CARTESIAN_POINT('Ctrl Pts',(-19.0060171333041,22.1526449343928,121.959277593411)) ;
#36330 = CARTESIAN_POINT('Ctrl Pts',(-19.2900221608687,22.3424731156636,122.211822747741)) ;
#36331 = CARTESIAN_POINT('Ctrl Pts',(-19.2602098520489,22.1624840352537,121.911823353311)) ;
#36332 = CARTESIAN_POINT('Ctrl Pts',(-19.5009224073841,22.3525061985293,122.209172430537)) ;
#36333 = CARTESIAN_POINT('Ctrl Pts',(-19.5238350449233,22.1725171181195,121.908510218205)) ;
#36334 = CARTESIAN_POINT('Ctrl Pts',(-19.7087834710141,22.3625278838048,122.243664453097)) ;
#36335 = CARTESIAN_POINT('Ctrl Pts',(-19.7836614016693,22.1825388033949,121.951624796593)) ;
#36336 = CARTESIAN_POINT('Ctrl Pts',(-19.9045062463924,22.3723945789033,122.312314874088)) ;
#36337 = CARTESIAN_POINT('Ctrl Pts',(-20.0283161574621,22.1924054984934,122.03743793613)) ;
#36338 = CARTESIAN_POINT('Ctrl Pts',(-20.0873367852254,22.3823544686378,122.414394213939)) ;
#36339 = CARTESIAN_POINT('Ctrl Pts',(-20.2568547841088,22.202365388228,122.165037255686)) ;
#36340 = CARTESIAN_POINT('Ctrl Pts',(-20.2506677841391,22.3923894564633,122.547902606798)) ;
#36341 = CARTESIAN_POINT('Ctrl Pts',(-20.4610185639065,22.2124003760535,122.331922477381)) ;
#36342 = CARTESIAN_POINT('Ctrl Pts',(-20.3865916163423,22.4022761605376,122.705186554573)) ;
#36343 = CARTESIAN_POINT('Ctrl Pts',(-20.6309241389178,22.2222870801277,122.528528183471)) ;
#36344 = CARTESIAN_POINT('Ctrl Pts',(-20.4949858769458,22.4123413047705,122.886876646557)) ;
#36345 = CARTESIAN_POINT('Ctrl Pts',(-20.7664168563428,22.2323522243607,122.755640405129)) ;
#36346 = CARTESIAN_POINT('Ctrl Pts',(-20.5687197159867,22.422180595499,123.080175375466)) ;
#36347 = CARTESIAN_POINT('Ctrl Pts',(-20.8585847062321,22.2421915150892,122.99726519042)) ;
#36348 = CARTESIAN_POINT('Ctrl Pts',(-20.6089305970685,22.4322431529375,123.287840199753)) ;
#36349 = CARTESIAN_POINT('Ctrl Pts',(-20.9088481490265,22.2522540725277,123.256845872691)) ;
#36350 = CARTESIAN_POINT('Ctrl Pts',(-20.6121922591228,22.4421402041896,123.495893346216)) ;
#36351 = CARTESIAN_POINT('Ctrl Pts',(-20.9129252441813,22.2621511237797,123.516913308376)) ;
#36352 = CARTESIAN_POINT('Ctrl Pts',(-20.5798565032163,22.4520714109378,123.702154164007)) ;
#36353 = CARTESIAN_POINT('Ctrl Pts',(-20.8725051637959,22.272082330528,123.774739999832)) ;
#36354 = CARTESIAN_POINT('Ctrl Pts',(-20.5112221625243,22.4621135951567,123.901801813168)) ;
#36355 = CARTESIAN_POINT('Ctrl Pts',(-20.7867121317539,22.2821245147468,124.024299304351)) ;
#36356 = CARTESIAN_POINT('Ctrl Pts',(-20.4106758088328,22.4720002232676,124.083722626987)) ;
#36357 = CARTESIAN_POINT('Ctrl Pts',(-20.6610284500668,22.2920111428578,124.251701155103)) ;
#36358 = CARTESIAN_POINT('Ctrl Pts',(-20.278945382695,22.4819934958,124.2473690502)) ;
#36359 = CARTESIAN_POINT('Ctrl Pts',(-20.4963649928886,22.3020044153902,124.456259102505)) ;
#36360 = CARTESIAN_POINT('Ctrl Pts',(-20.1215083587096,22.4919385713414,124.384944915974)) ;
#36361 = CARTESIAN_POINT('Ctrl Pts',(-20.2995680280864,22.3119494909316,124.628229064156)) ;
#36362 = CARTESIAN_POINT('Ctrl Pts',(-19.9426983959548,22.5018881220697,124.493496277981)) ;
#36363 = CARTESIAN_POINT('Ctrl Pts',(-20.0760548365221,22.3218990416599,124.763918115398)) ;
#36364 = CARTESIAN_POINT('Ctrl Pts',(-19.7459427076918,22.5119274569177,124.569841858884)) ;
#36365 = CARTESIAN_POINT('Ctrl Pts',(-19.8301102215501,22.3319383765079,124.859349625997)) ;
#36366 = CARTESIAN_POINT('Ctrl Pts',(-19.5420901927288,22.5218135958616,124.610431047829)) ;
#36367 = CARTESIAN_POINT('Ctrl Pts',(-19.5752934234481,22.3418245154518,124.910085821223)) ;
#36368 = CARTESIAN_POINT('Ctrl Pts',(-19.331980404051,22.5318117088353,124.615326987992)) ;
#36369 = CARTESIAN_POINT('Ctrl Pts',(-19.3126560173054,22.3518226284255,124.916205138693)) ;
#36370 = CARTESIAN_POINT('Ctrl Pts',(-19.1257731714612,22.5417314711877,124.584031987848)) ;
#36371 = CARTESIAN_POINT('Ctrl Pts',(-19.0548963058817,22.3617423907779,124.877085616193)) ;
#36372 = CARTESIAN_POINT('Ctrl Pts',(-18.925760197074,22.5517708668004,124.51667777525)) ;
#36373 = CARTESIAN_POINT('Ctrl Pts',(-18.8048804750503,22.3717817863906,124.792892259327)) ;
#36374 = CARTESIAN_POINT('Ctrl Pts',(-18.7429037014523,22.5616800525887,124.416866967638)) ;
#36375 = CARTESIAN_POINT('Ctrl Pts',(-18.5763093839728,22.3816909721789,124.668127742405)) ;
#36376 = CARTESIAN_POINT('Ctrl Pts',(-18.579362600272,22.5716152367462,124.286939430316)) ;
#36377 = CARTESIAN_POINT('Ctrl Pts',(-18.3718830460243,22.3916261563363,124.50571721687)) ;
#36378 = CARTESIAN_POINT('Ctrl Pts',(-18.4395493540934,22.5816562941321,124.128790649976)) ;
#36379 = CARTESIAN_POINT('Ctrl Pts',(-18.19711721559,22.4016672137223,124.308030847495)) ;
#36380 = CARTESIAN_POINT('Ctrl Pts',(-18.3308735820911,22.5915434521654,123.951591507098)) ;
#36381 = CARTESIAN_POINT('Ctrl Pts',(-18.0612726926849,22.4115543717555,124.086530580813)) ;
#36382 = CARTESIAN_POINT('Ctrl Pts',(-18.253489695394,22.6015357318413,123.756310473585)) ;
#36383 = CARTESIAN_POINT('Ctrl Pts',(-17.964543684815,22.4215466514315,123.84242873292)) ;
#36384 = CARTESIAN_POINT('Ctrl Pts',(-18.2114252982926,22.6114842488863,123.551423040072)) ;
#36385 = CARTESIAN_POINT('Ctrl Pts',(-17.9119640314251,22.4314951684765,123.58631871419)) ;
#36386 = CARTESIAN_POINT('Ctrl Pts',(-18.2052879099196,22.6214210264567,123.342628586766)) ;
#36387 = CARTESIAN_POINT('Ctrl Pts',(-17.9042933597284,22.4414319460469,123.325324977712)) ;
#36388 = CARTESIAN_POINT('Ctrl Pts',(-18.2353818524349,22.6314040626037,123.134895795784)) ;
#36389 = CARTESIAN_POINT('Ctrl Pts',(-17.9419119920146,22.4514149821938,123.065658904075)) ;
#36390 = CARTESIAN_POINT('Ctrl Pts',(-18.3018390798526,22.6414478141974,122.934500268376)) ;
#36391 = CARTESIAN_POINT('Ctrl Pts',(-18.0249844509372,22.4614587337876,122.815165001318)) ;
#36392 = CARTESIAN_POINT('Ctrl Pts',(-18.3995334670519,22.65127634341,122.752393803793)) ;
#36393 = CARTESIAN_POINT('Ctrl Pts',(-18.1471041894018,22.4712872630001,122.587531223325)) ;
#36394 = CARTESIAN_POINT('Ctrl Pts',(-18.5304390769983,22.6613517043187,122.585924560108)) ;
#36395 = CARTESIAN_POINT('Ctrl Pts',(-18.3107369255047,22.4813626239088,122.379445782513)) ;
#36396 = CARTESIAN_POINT('Ctrl Pts',(-18.6848484847896,22.6712083032059,122.447668513297)) ;
#36397 = CARTESIAN_POINT('Ctrl Pts',(-18.5037504475516,22.491219222796,122.206625869237)) ;
#36398 = CARTESIAN_POINT('Ctrl Pts',(-18.8644168488015,22.6812712972238,122.335891874011)) ;
#36399 = CARTESIAN_POINT('Ctrl Pts',(-18.7282113464364,22.5012822168139,122.066906399774)) ;
#36400 = CARTESIAN_POINT('Ctrl Pts',(-19.0571331275604,22.6911492315132,122.25842835509)) ;
#36401 = CARTESIAN_POINT('Ctrl Pts',(-18.9691081441107,22.5111601511034,121.97007787481)) ;
#36402 = CARTESIAN_POINT('Ctrl Pts',(-19.2627566660564,22.7011498790713,122.214769477626)) ;
#36403 = CARTESIAN_POINT('Ctrl Pts',(-19.2261379991783,22.5211607986615,121.915505689018)) ;
#36404 = CARTESIAN_POINT('Ctrl Pts',(-19.4711669419206,22.7110677255094,122.207377365738)) ;
#36405 = CARTESIAN_POINT('Ctrl Pts',(-19.486651608723,22.5310786450995,121.906267040759)) ;
#36406 = CARTESIAN_POINT('Ctrl Pts',(-19.6803914078797,22.721118842515,122.236721719079)) ;
#36407 = CARTESIAN_POINT('Ctrl Pts',(-19.7481817747925,22.5411297621052,121.942948938025)) ;
#36408 = CARTESIAN_POINT('Ctrl Pts',(-19.8778768048327,22.7309895778256,122.300577463833)) ;
#36409 = CARTESIAN_POINT('Ctrl Pts',(-19.9950390178961,22.5510004974158,122.022770439516)) ;
#36410 = CARTESIAN_POINT('Ctrl Pts',(-20.0649458105329,22.7410602850686,122.39964958428)) ;
#36411 = CARTESIAN_POINT('Ctrl Pts',(-20.228874215615,22.5610712046588,122.146611832899)) ;
#36412 = CARTESIAN_POINT('Ctrl Pts',(-20.2281280729297,22.7508932925205,122.526586135203)) ;
#36413 = CARTESIAN_POINT('Ctrl Pts',(-20.4328520597014,22.5709042121106,122.305284591609)) ;
#36414 = CARTESIAN_POINT('Ctrl Pts',(-20.3700041193385,22.7609237848228,122.682583660361)) ;
#36415 = CARTESIAN_POINT('Ctrl Pts',(-20.6101957114901,22.5809347044129,122.500282658212)) ;
#36416 = CARTESIAN_POINT('Ctrl Pts',(-20.4821412733727,22.7709553798962,122.861209839806)) ;
#36417 = CARTESIAN_POINT('Ctrl Pts',(-20.7503657378208,22.5909662994864,122.723566173328)) ;
#36418 = CARTESIAN_POINT('Ctrl Pts',(-20.5603509074772,22.7807850790344,123.052474175343)) ;
#36419 = CARTESIAN_POINT('Ctrl Pts',(-20.8481266307931,22.6007959986246,122.962648437227)) ;
#36420 = CARTESIAN_POINT('Ctrl Pts',(-20.6054919636736,22.790774528916,123.257581426922)) ;
#36421 = CARTESIAN_POINT('Ctrl Pts',(-20.904551077319,22.6107854485062,123.219033095619)) ;
#36422 = CARTESIAN_POINT('Ctrl Pts',(-20.6138461179592,22.8008183867317,123.468567262756)) ;
#36423 = CARTESIAN_POINT('Ctrl Pts',(-20.9149919746833,22.6208293063218,123.482765312891)) ;
#36424 = CARTESIAN_POINT('Ctrl Pts',(-20.5864922399839,22.8106400773219,123.673230555573)) ;
#36425 = CARTESIAN_POINT('Ctrl Pts',(-20.8807975539066,22.6306509969121,123.738595413786)) ;
#36426 = CARTESIAN_POINT('Ctrl Pts',(-20.5231490604348,22.8206751678623,123.874462180045)) ;
#36427 = CARTESIAN_POINT('Ctrl Pts',(-20.80161663366,22.6406860874524,123.990134218066)) ;
#36428 = CARTESIAN_POINT('Ctrl Pts',(-20.4254247657349,22.830699686845,124.061198211658)) ;
#36429 = CARTESIAN_POINT('Ctrl Pts',(-20.6794595799392,22.6507106064352,124.22355335811)) ;
#36430 = CARTESIAN_POINT('Ctrl Pts',(-20.2991731667971,22.8405595322552,124.225579994862)) ;
#36431 = CARTESIAN_POINT('Ctrl Pts',(-20.5216428900064,22.6605704518454,124.429030130097)) ;
#36432 = CARTESIAN_POINT('Ctrl Pts',(-20.1451242577046,22.8505193085708,124.367400091411)) ;
#36433 = CARTESIAN_POINT('Ctrl Pts',(-20.3290800370849,22.670530228161,124.606303874625)) ;
#36434 = CARTESIAN_POINT('Ctrl Pts',(-19.9674278032907,22.8605475058855,124.480844125221)) ;
#36435 = CARTESIAN_POINT('Ctrl Pts',(-20.1069583811312,22.6805584254756,124.748107125951)) ;
#36436 = CARTESIAN_POINT('Ctrl Pts',(-19.7751521418593,22.8704550481758,124.56097363697)) ;
#36437 = CARTESIAN_POINT('Ctrl Pts',(-19.8666123895731,22.690465967766,124.848267265669)) ;
#36438 = CARTESIAN_POINT('Ctrl Pts',(-19.5693646949917,22.8804876987396,124.607138562997)) ;
#36439 = CARTESIAN_POINT('Ctrl Pts',(-19.6093776535682,22.7004986183298,124.905971285035)) ;
#36440 = CARTESIAN_POINT('Ctrl Pts',(-19.3617911177059,22.8903716551663,124.616789062193)) ;
#36441 = CARTESIAN_POINT('Ctrl Pts',(-19.3499098381939,22.7103825747565,124.918032249286)) ;
#36442 = CARTESIAN_POINT('Ctrl Pts',(-19.1534263144048,22.9003613565281,124.590486564837)) ;
#36443 = CARTESIAN_POINT('Ctrl Pts',(-19.0894539707891,22.7203722761183,124.885151798247)) ;
#36444 = CARTESIAN_POINT('Ctrl Pts',(-18.9518995245256,22.9104023518042,124.527657154102)) ;
#36445 = CARTESIAN_POINT('Ctrl Pts',(-18.8375462306779,22.7304132713943,124.806612946829)) ;
#36446 = CARTESIAN_POINT('Ctrl Pts',(-18.768077928406,22.9202352410725,124.433102961583)) ;
#36447 = CARTESIAN_POINT('Ctrl Pts',(-18.6077694356937,22.7402461606627,124.688417721226)) ;
#36448 = CARTESIAN_POINT('Ctrl Pts',(-18.6004184578311,22.93022839944,124.306510185862)) ;
#36449 = CARTESIAN_POINT('Ctrl Pts',(-18.398196469038,22.7502393190301,124.530174726627)) ;
#36450 = CARTESIAN_POINT('Ctrl Pts',(-18.4570423276391,22.9402604417921,124.151821923113)) ;
#36451 = CARTESIAN_POINT('Ctrl Pts',(-18.2189780473495,22.7602713613823,124.336812835457)) ;
#36452 = CARTESIAN_POINT('Ctrl Pts',(-18.3444002375447,22.9501256857505,123.977691444909)) ;
#36453 = CARTESIAN_POINT('Ctrl Pts',(-18.0781770519716,22.7701366053407,124.119147819027)) ;
#36454 = CARTESIAN_POINT('Ctrl Pts',(-18.2623606113742,22.9600875769965,123.78499218241)) ;
#36455 = CARTESIAN_POINT('Ctrl Pts',(-17.9756297430065,22.7800984965867,123.878272519258)) ;
#36456 = CARTESIAN_POINT('Ctrl Pts',(-18.2150170839736,22.970122477015,123.579418516963)) ;
#36457 = CARTESIAN_POINT('Ctrl Pts',(-17.9164527323649,22.7901333966051,123.621304920699)) ;
#36458 = CARTESIAN_POINT('Ctrl Pts',(-18.2039051887294,22.9800075574296,123.371873650446)) ;
#36459 = CARTESIAN_POINT('Ctrl Pts',(-17.9025653495676,22.8000184770197,123.361873137657)) ;
#36460 = CARTESIAN_POINT('Ctrl Pts',(-18.2294709369507,22.9900727295544,123.161850154122)) ;
#36461 = CARTESIAN_POINT('Ctrl Pts',(-17.9345250196127,22.8100836491446,123.099344214686)) ;
#36462 = CARTESIAN_POINT('Ctrl Pts',(-18.2896793781521,22.9999199642779,122.963757686704)) ;
#36463 = CARTESIAN_POINT('Ctrl Pts',(-18.0097882000835,22.8199308838681,122.851728714275)) ;
#36464 = CARTESIAN_POINT('Ctrl Pts',(-18.3846575460078,23.0099507755956,122.775493829682)) ;
#36465 = CARTESIAN_POINT('Ctrl Pts',(-18.1285132436954,22.8299616951858,122.616400101457)) ;
#36466 = CARTESIAN_POINT('Ctrl Pts',(-18.5109834152174,23.0199603915091,122.607165887845)) ;
#36467 = CARTESIAN_POINT('Ctrl Pts',(-18.2864226562606,22.8399713110993,122.405991657267)) ;
#36468 = CARTESIAN_POINT('Ctrl Pts',(-18.6629287718639,23.0298711709128,122.464629523893)) ;
#36469 = CARTESIAN_POINT('Ctrl Pts',(-18.4763564295157,22.849882090503,122.227822802707)) ;
#36470 = CARTESIAN_POINT('Ctrl Pts',(-18.8373784129168,23.0398004367019,122.349974057845)) ;
#36471 = CARTESIAN_POINT('Ctrl Pts',(-18.6944202111385,22.859811356292,122.084505529284)) ;
#36472 = CARTESIAN_POINT('Ctrl Pts',(-19.0313295538799,23.0498431300145,122.266578270263)) ;
#36473 = CARTESIAN_POINT('Ctrl Pts',(-18.9368601501054,22.8698540496047,121.980263237203)) ;
#36474 = CARTESIAN_POINT('Ctrl Pts',(-19.2336083459502,23.0597296627092,122.218742068884)) ;
#36475 = CARTESIAN_POINT('Ctrl Pts',(-19.1897096706309,22.8797405822994,121.920470478076)) ;
#36476 = CARTESIAN_POINT('Ctrl Pts',(-19.4433140464625,23.0697228078125,122.206271347254)) ;
#36477 = CARTESIAN_POINT('Ctrl Pts',(-19.4518420605105,22.8897337274027,121.904884777568)) ;
#36478 = CARTESIAN_POINT('Ctrl Pts',(-19.6510110881743,23.0796684884866,122.230368010918)) ;
#36479 = CARTESIAN_POINT('Ctrl Pts',(-19.7114632832779,22.8996794080768,121.93500831667)) ;
#36480 = CARTESIAN_POINT('Ctrl Pts',(-19.8515326787835,23.0896157461133,122.289763971548)) ;
#36481 = CARTESIAN_POINT('Ctrl Pts',(-19.9621146838214,22.9096266657035,122.009255961529)) ;
#36482 = CARTESIAN_POINT('Ctrl Pts',(-20.0404673828271,23.0996636482348,122.38422357924)) ;
#36483 = CARTESIAN_POINT('Ctrl Pts',(-20.1982818352808,22.919674567825,122.127332902598)) ;
#36484 = CARTESIAN_POINT('Ctrl Pts',(-20.2068601688876,23.1095113538565,122.507411205616)) ;
#36485 = CARTESIAN_POINT('Ctrl Pts',(-20.4062715090899,22.9295222734466,122.281319880636)) ;
#36486 = CARTESIAN_POINT('Ctrl Pts',(-20.3514553093839,23.1194728204906,122.658891921361)) ;
#36487 = CARTESIAN_POINT('Ctrl Pts',(-20.587013493731,22.9394837400808,122.470672801433)) ;
#36488 = CARTESIAN_POINT('Ctrl Pts',(-20.4681173020612,23.1295023737588,122.83453984717)) ;
#36489 = CARTESIAN_POINT('Ctrl Pts',(-20.7328386956585,22.949513293349,122.690234279915)) ;
#36490 = CARTESIAN_POINT('Ctrl Pts',(-20.5515843547797,23.1394092657862,123.025360354087)) ;
#36491 = CARTESIAN_POINT('Ctrl Pts',(-20.837170043744,22.9594201853764,122.928761227123)) ;
#36492 = CARTESIAN_POINT('Ctrl Pts',(-20.6012418234421,23.1493569098992,123.228492863603)) ;
#36493 = CARTESIAN_POINT('Ctrl Pts',(-20.8992391771588,22.9693678294894,123.182677656163)) ;
#36494 = CARTESIAN_POINT('Ctrl Pts',(-20.6150800343719,23.1593569529281,123.438296909276)) ;
#36495 = CARTESIAN_POINT('Ctrl Pts',(-20.9165341377997,22.9793678725182,123.444932969308)) ;
#36496 = CARTESIAN_POINT('Ctrl Pts',(-20.5918224314329,23.1693957189221,123.648041713659)) ;
#36497 = CARTESIAN_POINT('Ctrl Pts',(-20.8874593438765,22.9894066385123,123.707113721917)) ;
#36498 = CARTESIAN_POINT('Ctrl Pts',(-20.5341745069886,23.1792207809443,123.846402561714)) ;
#36499 = CARTESIAN_POINT('Ctrl Pts',(-20.8153966816102,22.9992317005345,123.955064177267)) ;
#36500 = CARTESIAN_POINT('Ctrl Pts',(-20.4411557623912,23.1892753282707,124.036199337756)) ;
#36501 = CARTESIAN_POINT('Ctrl Pts',(-20.6991206974634,23.0092862478609,124.192308936978)) ;
#36502 = CARTESIAN_POINT('Ctrl Pts',(-20.3176702770705,23.1992185717199,124.204874255302)) ;
#36503 = CARTESIAN_POINT('Ctrl Pts',(-20.5447615014033,23.0192294913101,124.403151003518)) ;
#36504 = CARTESIAN_POINT('Ctrl Pts',(-20.1678477489804,23.2091207433278,124.349412148835)) ;
#36505 = CARTESIAN_POINT('Ctrl Pts',(-20.3574813482785,23.029131662918,124.583821375394)) ;
#36506 = CARTESIAN_POINT('Ctrl Pts',(-19.9925143602655,23.219173578938,124.467395725293)) ;
#36507 = CARTESIAN_POINT('Ctrl Pts',(-20.1383129463047,23.0391844985282,124.731298547817)) ;
#36508 = CARTESIAN_POINT('Ctrl Pts',(-19.8028310164097,23.2290466366235,124.551692861004)) ;
#36509 = CARTESIAN_POINT('Ctrl Pts',(-19.9012076725371,23.0490575562137,124.836667408576)) ;
#36510 = CARTESIAN_POINT('Ctrl Pts',(-19.599035620592,23.2390418981492,124.602895730111)) ;
#36511 = CARTESIAN_POINT('Ctrl Pts',(-19.6464624451239,23.0590528177394,124.900668231928)) ;
#36512 = CARTESIAN_POINT('Ctrl Pts',(-19.3887803257811,23.2490672675697,124.617604462307)) ;
#36513 = CARTESIAN_POINT('Ctrl Pts',(-19.3836439744428,23.0690781871599,124.919051527875)) ;
#36514 = CARTESIAN_POINT('Ctrl Pts',(-19.1819671042923,23.2589571000963,124.596152765897)) ;
#36515 = CARTESIAN_POINT('Ctrl Pts',(-19.1251242692566,23.0789680196865,124.892233416158)) ;
#36516 = CARTESIAN_POINT('Ctrl Pts',(-18.9130557461595,23.2722550709057,124.5197923832)) ;
#36517 = CARTESIAN_POINT('Ctrl Pts',(-18.7890035336814,23.0922659904958,124.796782825509)) ;
#36518 = CARTESIAN_POINT('Ctrl Pts',(-18.6717587243513,23.2854534660148,124.376385706573)) ;
#36519 = CARTESIAN_POINT('Ctrl Pts',(-18.4874072190353,23.105464385605,124.617549791565)) ;
#36520 = CARTESIAN_POINT('Ctrl Pts',(-18.4752682237642,23.2988489082943,124.174730150354)) ;
#36521 = CARTESIAN_POINT('Ctrl Pts',(-18.2417519025622,23.1188598278845,124.365440343036)) ;
#36522 = CARTESIAN_POINT('Ctrl Pts',(-18.358218981122,23.3087247465333,124.00319866305)) ;
#36523 = CARTESIAN_POINT('Ctrl Pts',(-18.0954516813819,23.1287356661234,124.151032241579)) ;
#36524 = CARTESIAN_POINT('Ctrl Pts',(-18.2710692283596,23.318786149131,123.810502936059)) ;
#36525 = CARTESIAN_POINT('Ctrl Pts',(-17.9865146771472,23.1387970687212,123.91015878141)) ;
#36526 = CARTESIAN_POINT('Ctrl Pts',(-18.2196477196924,23.3286512060661,123.609550825009)) ;
#36527 = CARTESIAN_POINT('Ctrl Pts',(-17.9222404620335,23.1486621256563,123.658970587681)) ;
#36528 = CARTESIAN_POINT('Ctrl Pts',(-18.2032931252815,23.3386633020149,123.399733102314)) ;
#36529 = CARTESIAN_POINT('Ctrl Pts',(-17.9018022903817,23.1586742216051,123.396691351191)) ;
#36530 = CARTESIAN_POINT('Ctrl Pts',(-18.2303090879066,23.3519406111604,123.121854743172)) ;
#36531 = CARTESIAN_POINT('Ctrl Pts',(-17.9355630206945,23.1719515307505,123.049376976585)) ;
#36532 = CARTESIAN_POINT('Ctrl Pts',(-18.3537865412185,23.3685396366677,122.791280328664)) ;
#36533 = CARTESIAN_POINT('Ctrl Pts',(-18.0899419028063,23.1885505562579,122.636110521805)) ;
#36534 = CARTESIAN_POINT('Ctrl Pts',(-18.5826974213556,23.3851386847007,122.522589585536)) ;
#36535 = CARTESIAN_POINT('Ctrl Pts',(-18.37602583293,23.2051496042909,122.300311520371)) ;
#36536 = CARTESIAN_POINT('Ctrl Pts',(-18.8116870577227,23.3983820967316,122.364269542791)) ;
#36537 = CARTESIAN_POINT('Ctrl Pts',(-18.6623130733646,23.2183930163218,122.102367993651)) ;
#36538 = CARTESIAN_POINT('Ctrl Pts',(-19.0034183423248,23.4084195244201,122.276133501985)) ;
#36539 = CARTESIAN_POINT('Ctrl Pts',(-18.9019676656233,23.2284304440103,121.992209381393)) ;
#36540 = CARTESIAN_POINT('Ctrl Pts',(-19.2048395995662,23.4183238263757,122.223371608911)) ;
#36541 = CARTESIAN_POINT('Ctrl Pts',(-19.1537511180721,23.2383347459658,121.926257438572)) ;
#36542 = CARTESIAN_POINT('Ctrl Pts',(-19.4827891473364,23.4315906663508,122.19988920511)) ;
#36543 = CARTESIAN_POINT('Ctrl Pts',(-19.5011668383607,23.251601585941,121.896906682968)) ;
#36544 = CARTESIAN_POINT('Ctrl Pts',(-19.8307318849537,23.4482168644408,122.262263108639)) ;
#36545 = CARTESIAN_POINT('Ctrl Pts',(-19.9361152833233,23.2682277840309,121.97487577289)) ;
#36546 = CARTESIAN_POINT('Ctrl Pts',(-20.1971528166808,23.4681359798242,122.474678281948)) ;
#36547 = CARTESIAN_POINT('Ctrl Pts',(-20.3941427128654,23.2881468994144,122.24041645657)) ;
#36548 = CARTESIAN_POINT('Ctrl Pts',(-20.4241051193176,23.4847424029584,122.745236826327)) ;
#36549 = CARTESIAN_POINT('Ctrl Pts',(-20.6777956763703,23.3047533225486,122.578559316813)) ;
#36550 = CARTESIAN_POINT('Ctrl Pts',(-20.5421768965827,23.4980386234541,122.998554900509)) ;
#36551 = CARTESIAN_POINT('Ctrl Pts',(-20.8254141686422,23.3180495430443,122.895260367397)) ;
#36552 = CARTESIAN_POINT('Ctrl Pts',(-20.614959986531,23.5113074557956,123.267928258052)) ;
#36553 = CARTESIAN_POINT('Ctrl Pts',(-20.9163840286482,23.3313183753857,123.231954203328)) ;
#36554 = CARTESIAN_POINT('Ctrl Pts',(-20.6152647113257,23.5279987038287,123.622730942973)) ;
#36555 = CARTESIAN_POINT('Ctrl Pts',(-20.9167633042125,23.3480096234189,123.675476169149)) ;
#36556 = CARTESIAN_POINT('Ctrl Pts',(-20.4722994274042,23.5478084355015,124.018996186989)) ;
#36557 = CARTESIAN_POINT('Ctrl Pts',(-20.7380527826881,23.3678193550916,124.170798980332)) ;
#36558 = CARTESIAN_POINT('Ctrl Pts',(-20.2010981674225,23.56778604283,124.345907252259)) ;
#36559 = CARTESIAN_POINT('Ctrl Pts',(-20.39904878012,23.3877969624202,124.579436972795)) ;
#36560 = CARTESIAN_POINT('Ctrl Pts',(-19.8351962742171,23.5877123518879,124.559408382312)) ;
#36561 = CARTESIAN_POINT('Ctrl Pts',(-19.9416700356662,23.4077232714781,124.846309372942)) ;
#36562 = CARTESIAN_POINT('Ctrl Pts',(-19.4207969533748,23.6075292120526,124.636299831341)) ;
#36563 = CARTESIAN_POINT('Ctrl Pts',(-19.4236722805428,23.4275401316427,124.942420637925)) ;
#36564 = CARTESIAN_POINT('Ctrl Pts',(-18.9994637731957,23.6276290276466,124.565563992342)) ;
#36565 = CARTESIAN_POINT('Ctrl Pts',(-18.8970052108273,23.4476399472368,124.85399762063)) ;
#36566 = CARTESIAN_POINT('Ctrl Pts',(-18.6335253229913,23.6473859915291,124.358902751464)) ;
#36567 = CARTESIAN_POINT('Ctrl Pts',(-18.439585873165,23.4673969111193,124.595670036083)) ;
#36568 = CARTESIAN_POINT('Ctrl Pts',(-18.3557767431134,23.6674229175986,124.036039149984)) ;
#36569 = CARTESIAN_POINT('Ctrl Pts',(-18.092401477784,23.4874338371887,124.192088863954)) ;
#36570 = CARTESIAN_POINT('Ctrl Pts',(-18.2066700929233,23.6872924999801,123.640628669761)) ;
#36571 = CARTESIAN_POINT('Ctrl Pts',(-17.9060208621078,23.5073034195703,123.697826439098)) ;
#36572 = CARTESIAN_POINT('Ctrl Pts',(-18.20037309154,23.7071970717333,123.217532309015)) ;
#36573 = CARTESIAN_POINT('Ctrl Pts',(-17.898151051561,23.5272079913234,123.168957382095)) ;
#36574 = CARTESIAN_POINT('Ctrl Pts',(-18.3392583799834,23.7271496739318,122.816587599737)) ;
#36575 = CARTESIAN_POINT('Ctrl Pts',(-18.0717585757176,23.547160593522,122.667777463701)) ;
#36576 = CARTESIAN_POINT('Ctrl Pts',(-18.6060586541103,23.747059164902,122.488027614891)) ;
#36577 = CARTESIAN_POINT('Ctrl Pts',(-18.405258884035,23.5670700844922,122.25707925787)) ;
#36578 = CARTESIAN_POINT('Ctrl Pts',(-18.9674540788008,23.7669105336015,122.269754789477)) ;
#36579 = CARTESIAN_POINT('Ctrl Pts',(-18.8570010753388,23.5869214531917,121.98423938823)) ;
#36580 = CARTESIAN_POINT('Ctrl Pts',(-19.3863467957852,23.7869907297375,122.187619791407)) ;
#36581 = CARTESIAN_POINT('Ctrl Pts',(-19.3806182677783,23.6070016493277,121.881570519857)) ;
#36582 = CARTESIAN_POINT('Ctrl Pts',(-19.8024562321169,23.8067916733129,122.25247266476)) ;
#36583 = CARTESIAN_POINT('Ctrl Pts',(-19.9007519851845,23.6268025929031,121.962636023164)) ;
#36584 = CARTESIAN_POINT('Ctrl Pts',(-20.1751703809712,23.8267756498224,122.456380190659)) ;
#36585 = CARTESIAN_POINT('Ctrl Pts',(-20.3666450135569,23.6467865694126,122.217519362983)) ;
#36586 = CARTESIAN_POINT('Ctrl Pts',(-20.4545225997992,23.846691612798,122.774634398599)) ;
#36587 = CARTESIAN_POINT('Ctrl Pts',(-20.7158350928869,23.6667025323882,122.615335633033)) ;
#36588 = CARTESIAN_POINT('Ctrl Pts',(-20.6092694572912,23.8665620476199,123.167863522626)) ;
#36589 = CARTESIAN_POINT('Ctrl Pts',(-20.9092697535832,23.6865729672101,123.106869748177)) ;
#36590 = CARTESIAN_POINT('Ctrl Pts',(-20.6199224875745,23.886612332853,123.593929804403)) ;
#36591 = CARTESIAN_POINT('Ctrl Pts',(-20.922587690432,23.7066232524431,123.639453176965)) ;
#36592 = CARTESIAN_POINT('Ctrl Pts',(-20.4868864023955,23.9063863016123,123.992954670448)) ;
#36593 = CARTESIAN_POINT('Ctrl Pts',(-20.7562955196526,23.7263972212025,124.138232320096)) ;
#36594 = CARTESIAN_POINT('Ctrl Pts',(-20.2223831801166,23.9264427597318,124.327253105703)) ;
#36595 = CARTESIAN_POINT('Ctrl Pts',(-20.4256681461697,23.746453679322,124.556107455233)) ;
#36596 = CARTESIAN_POINT('Ctrl Pts',(-19.8640850949148,23.9462376427228,124.548331334748)) ;
#36597 = CARTESIAN_POINT('Ctrl Pts',(-19.9777988611874,23.766248562313,124.832456311701)) ;
#36598 = CARTESIAN_POINT('Ctrl Pts',(-19.448727810941,23.9662042980252,124.63574281183)) ;
#36599 = CARTESIAN_POINT('Ctrl Pts',(-19.458603262155,23.7862152176154,124.941723990057)) ;
#36600 = CARTESIAN_POINT('Ctrl Pts',(-19.0285651397822,23.9861632681017,124.575472295223)) ;
#36601 = CARTESIAN_POINT('Ctrl Pts',(-18.9333997951167,23.8061741876918,124.866389115845)) ;
#36602 = CARTESIAN_POINT('Ctrl Pts',(-18.6553168032142,24.0060593556918,124.376389568719)) ;
#36603 = CARTESIAN_POINT('Ctrl Pts',(-18.4668385535569,23.826070275282,124.617539311682)) ;
#36604 = CARTESIAN_POINT('Ctrl Pts',(-18.3720148561307,24.0259575256034,124.062201487962)) ;
#36605 = CARTESIAN_POINT('Ctrl Pts',(-18.1127087821961,23.8459684451936,124.224807490368)) ;
#36606 = CARTESIAN_POINT('Ctrl Pts',(-18.2124303919169,24.0458633609705,123.67015401321)) ;
#36607 = CARTESIAN_POINT('Ctrl Pts',(-17.9132245362544,23.8658742805607,123.734750368426)) ;
#36608 = CARTESIAN_POINT('Ctrl Pts',(-18.1961880168038,24.0658132859084,123.246313641307)) ;
#36609 = CARTESIAN_POINT('Ctrl Pts',(-17.8929172316188,23.8858242054986,123.204950398217)) ;
#36610 = CARTESIAN_POINT('Ctrl Pts',(-18.3247423088814,24.0856924758188,122.84360479257)) ;
#36611 = CARTESIAN_POINT('Ctrl Pts',(-18.0536055021763,23.905703395409,122.701563670967)) ;
#36612 = CARTESIAN_POINT('Ctrl Pts',(-18.5841033382921,24.1056738000994,122.507146079178)) ;
#36613 = CARTESIAN_POINT('Ctrl Pts',(-18.3778029519337,23.9256847196896,122.280987362642)) ;
#36614 = CARTESIAN_POINT('Ctrl Pts',(-18.942010615732,24.1256035843077,122.280096072877)) ;
#36615 = CARTESIAN_POINT('Ctrl Pts',(-18.8251843464283,23.9456145038979,121.997171158649)) ;
#36616 = CARTESIAN_POINT('Ctrl Pts',(-19.3555068623215,24.1455235736985,122.188809483554)) ;
#36617 = CARTESIAN_POINT('Ctrl Pts',(-19.3420527237454,23.9655344932887,121.88305758852)) ;
#36618 = CARTESIAN_POINT('Ctrl Pts',(-19.7742904831662,24.1653787690525,122.2430041829)) ;
#36619 = CARTESIAN_POINT('Ctrl Pts',(-19.8655341730097,23.9853896886427,121.950798016856)) ;
#36620 = CARTESIAN_POINT('Ctrl Pts',(-20.1526808934445,24.1854247707119,122.438992855019)) ;
#36621 = CARTESIAN_POINT('Ctrl Pts',(-20.3385180584814,24.005435690302,122.195770834765)) ;
#36622 = CARTESIAN_POINT('Ctrl Pts',(-20.3906070125325,24.2019245179217,122.696923893817)) ;
#36623 = CARTESIAN_POINT('Ctrl Pts',(-20.6359495242744,24.0219354375118,122.518207743298)) ;
#36624 = CARTESIAN_POINT('Ctrl Pts',(-20.5216768074671,24.2153131223698,122.945999721875)) ;
#36625 = CARTESIAN_POINT('Ctrl Pts',(-20.7997715921417,24.0353240419599,122.829526935815)) ;
#36626 = CARTESIAN_POINT('Ctrl Pts',(-20.5848955736062,24.2251749507047,123.143455647205)) ;
#36627 = CARTESIAN_POINT('Ctrl Pts',(-20.8788004514972,24.0451858702949,123.07635383237)) ;
#36628 = CARTESIAN_POINT('Ctrl Pts',(-20.6138199274551,24.2351410934622,123.350985731134)) ;
#36629 = CARTESIAN_POINT('Ctrl Pts',(-20.9149604444561,24.0551520130524,123.335751428968)) ;
#36630 = CARTESIAN_POINT('Ctrl Pts',(-20.6032002789081,24.2485028395872,123.631591883731)) ;
#36631 = CARTESIAN_POINT('Ctrl Pts',(-20.9016757193744,24.0685137591774,123.686576406625)) ;
#36632 = CARTESIAN_POINT('Ctrl Pts',(-20.5008787541352,24.2649571685423,123.966355059804)) ;
#36633 = CARTESIAN_POINT('Ctrl Pts',(-20.7738010339996,24.0849680881324,124.104947280298)) ;
#36634 = CARTESIAN_POINT('Ctrl Pts',(-20.2867198767303,24.2817244135906,124.2511417434)) ;
#36635 = CARTESIAN_POINT('Ctrl Pts',(-20.5060740059502,24.1017353331807,124.46098906877)) ;
#36636 = CARTESIAN_POINT('Ctrl Pts',(-20.068100156107,24.2949109788646,124.421823870107)) ;
#36637 = CARTESIAN_POINT('Ctrl Pts',(-20.2328267963753,24.1149218984548,124.67431188179)) ;
#36638 = CARTESIAN_POINT('Ctrl Pts',(-19.8829901974809,24.3049004376092,124.520886533694)) ;
#36639 = CARTESIAN_POINT('Ctrl Pts',(-20.0014355866931,24.1249113571994,124.798149276019)) ;
#36640 = CARTESIAN_POINT('Ctrl Pts',(-19.6841183586994,24.3148542100903,124.586142139234)) ;
#36641 = CARTESIAN_POINT('Ctrl Pts',(-19.7528479925911,24.1348651296805,124.879719694425)) ;
#36642 = CARTESIAN_POINT('Ctrl Pts',(-19.4750256631218,24.324902026623,124.61598118881)) ;
#36643 = CARTESIAN_POINT('Ctrl Pts',(-19.4914820582806,24.1449129462132,124.917021763286)) ;
#36644 = CARTESIAN_POINT('Ctrl Pts',(-19.2682080171776,24.3347435597455,124.609445253002)) ;
#36645 = CARTESIAN_POINT('Ctrl Pts',(-19.2329600579594,24.1547544793356,124.908854524418)) ;
#36646 = CARTESIAN_POINT('Ctrl Pts',(-19.0626517418926,24.3447298019652,124.566925901012)) ;
#36647 = CARTESIAN_POINT('Ctrl Pts',(-18.9760140363153,24.1647407215554,124.855708116938)) ;
#36648 = CARTESIAN_POINT('Ctrl Pts',(-18.8684666859137,24.3546664253901,124.489818172107)) ;
#36649 = CARTESIAN_POINT('Ctrl Pts',(-18.7332816198443,24.1746773449803,124.759326036372)) ;
#36650 = CARTESIAN_POINT('Ctrl Pts',(-18.688696650813,24.3647163027731,124.378854486706)) ;
#36651 = CARTESIAN_POINT('Ctrl Pts',(-18.5085675409844,24.1847272223632,124.620623799744)) ;
#36652 = CARTESIAN_POINT('Ctrl Pts',(-18.5339244507054,24.3745667415506,124.241242493615)) ;
#36653 = CARTESIAN_POINT('Ctrl Pts',(-18.31510033538,24.1945776611408,124.448610838054)) ;
#36654 = CARTESIAN_POINT('Ctrl Pts',(-18.4034080881523,24.3845387555194,124.077216087896)) ;
#36655 = CARTESIAN_POINT('Ctrl Pts',(-18.1519526132977,24.2045496751095,124.243579488849)) ;
#36656 = CARTESIAN_POINT('Ctrl Pts',(-18.3031188994434,24.3945339241455,123.892525344681)) ;
#36657 = CARTESIAN_POINT('Ctrl Pts',(-18.0265886283388,24.2145448437356,124.012717326588)) ;
#36658 = CARTESIAN_POINT('Ctrl Pts',(-18.2364182379383,24.4045678074067,123.692421879584)) ;
#36659 = CARTESIAN_POINT('Ctrl Pts',(-17.943210117293,24.2245787269968,123.762588848244)) ;
#36660 = CARTESIAN_POINT('Ctrl Pts',(-18.2057083821517,24.41442367747,123.487493870639)) ;
#36661 = CARTESIAN_POINT('Ctrl Pts',(-17.9048199952897,24.2344345970602,123.506429025604)) ;
#36662 = CARTESIAN_POINT('Ctrl Pts',(-18.2107882331578,24.4244212233872,123.277398137475)) ;
#36663 = CARTESIAN_POINT('Ctrl Pts',(-17.9111670276796,24.2444321429774,123.243809194856)) ;
#36664 = CARTESIAN_POINT('Ctrl Pts',(-18.2518400342972,24.4343293502864,123.073174907185)) ;
#36665 = CARTESIAN_POINT('Ctrl Pts',(-17.9624791058207,24.2543402698766,122.988529382355)) ;
#36666 = CARTESIAN_POINT('Ctrl Pts',(-18.3281714579042,24.4443397218086,122.877045008902)) ;
#36667 = CARTESIAN_POINT('Ctrl Pts',(-18.0578908531546,24.2643506413988,122.743365948053)) ;
#36668 = CARTESIAN_POINT('Ctrl Pts',(-18.438010301051,24.454370164556,122.69704745568)) ;
#36669 = CARTESIAN_POINT('Ctrl Pts',(-18.1951870356192,24.2743810841462,122.518367543311)) ;
#36670 = CARTESIAN_POINT('Ctrl Pts',(-18.5745495647584,24.4642181171093,122.541397741827)) ;
#36671 = CARTESIAN_POINT('Ctrl Pts',(-18.3658593160334,24.2842290366995,122.323803295481)) ;
#36672 = CARTESIAN_POINT('Ctrl Pts',(-18.7394306699372,24.4742807861303,122.408888682602)) ;
#36673 = CARTESIAN_POINT('Ctrl Pts',(-18.5719589573897,24.2942917057204,122.158164871413)) ;
#36674 = CARTESIAN_POINT('Ctrl Pts',(-18.9218207597135,24.4841751615942,122.308835807993)) ;
#36675 = CARTESIAN_POINT('Ctrl Pts',(-18.7999455381044,24.3041860811844,122.033096218189)) ;
#36676 = CARTESIAN_POINT('Ctrl Pts',(-19.119533784816,24.4941169599123,122.241135188269)) ;
#36677 = CARTESIAN_POINT('Ctrl Pts',(-19.0470862012613,24.3141278795025,121.948467825703)) ;
#36678 = CARTESIAN_POINT('Ctrl Pts',(-19.327299776132,24.5041194536396,122.208506614829)) ;
#36679 = CARTESIAN_POINT('Ctrl Pts',(-19.3067933605176,24.3241303732298,121.907679467722)) ;
#36680 = CARTESIAN_POINT('Ctrl Pts',(-19.5382060178291,24.5141542521466,122.212793291372)) ;
#36681 = CARTESIAN_POINT('Ctrl Pts',(-19.5704262020261,24.3341651717368,121.913035104039)) ;
#36682 = CARTESIAN_POINT('Ctrl Pts',(-19.741340693941,24.5239991361259,122.252526138907)) ;
#36683 = CARTESIAN_POINT('Ctrl Pts',(-19.8243456091052,24.3440100557161,121.962698661927)) ;
#36684 = CARTESIAN_POINT('Ctrl Pts',(-19.9373544726432,24.533984992944,122.327605162214)) ;
#36685 = CARTESIAN_POINT('Ctrl Pts',(-20.0693639138085,24.3539959125342,122.056545067765)) ;
#36686 = CARTESIAN_POINT('Ctrl Pts',(-20.1165728966918,24.5439198071187,122.434935896096)) ;
#36687 = CARTESIAN_POINT('Ctrl Pts',(-20.293388543739,24.3639307267089,122.190706447079)) ;
#36688 = CARTESIAN_POINT('Ctrl Pts',(-20.2762066027916,24.5539773069041,122.573540909043)) ;
#36689 = CARTESIAN_POINT('Ctrl Pts',(-20.4929322997867,24.3739882264943,122.363960667398)) ;
#36690 = CARTESIAN_POINT('Ctrl Pts',(-20.4065058320593,24.5637990653224,122.733750397852)) ;
#36691 = CARTESIAN_POINT('Ctrl Pts',(-20.6558088061763,24.3838099849125,122.564221525953)) ;
#36692 = CARTESIAN_POINT('Ctrl Pts',(-20.5097290699146,24.5738547231064,122.918217818253)) ;
#36693 = CARTESIAN_POINT('Ctrl Pts',(-20.7848399621109,24.3938656426965,122.794804495991)) ;
#36694 = CARTESIAN_POINT('Ctrl Pts',(-20.5782202375852,24.5837969052864,123.115704900593)) ;
#36695 = CARTESIAN_POINT('Ctrl Pts',(-20.8704564404007,24.4038078248766,123.041662828732)) ;
#36696 = CARTESIAN_POINT('Ctrl Pts',(-20.6118814894185,24.5937021139811,123.32120168517)) ;
#36697 = CARTESIAN_POINT('Ctrl Pts',(-20.9125354802017,24.4137130335713,123.298533937994)) ;
#36698 = CARTESIAN_POINT('Ctrl Pts',(-20.6092481539705,24.6037439049435,123.532291786237)) ;
#36699 = CARTESIAN_POINT('Ctrl Pts',(-20.9092462484332,24.4237548245337,123.562396507281)) ;
#36700 = CARTESIAN_POINT('Ctrl Pts',(-20.5705464706402,24.6136516794158,123.73696556278)) ;
#36701 = CARTESIAN_POINT('Ctrl Pts',(-20.8608714360001,24.433662599006,123.818239689854)) ;
#36702 = CARTESIAN_POINT('Ctrl Pts',(-20.4964883343986,24.6236631796434,123.933985160015)) ;
#36703 = CARTESIAN_POINT('Ctrl Pts',(-20.7683009427503,24.4436740992336,124.064515066645)) ;
#36704 = CARTESIAN_POINT('Ctrl Pts',(-20.388743463947,24.6336959400361,124.115308071487)) ;
#36705 = CARTESIAN_POINT('Ctrl Pts',(-20.6336219826215,24.4537068596262,124.291169915727)) ;
#36706 = CARTESIAN_POINT('Ctrl Pts',(-20.2539226961547,24.643546509171,124.272507133189)) ;
#36707 = CARTESIAN_POINT('Ctrl Pts',(-20.4650972756189,24.4635574287611,124.487670909618)) ;
#36708 = CARTESIAN_POINT('Ctrl Pts',(-20.0918811514129,24.6535351187009,124.406043156148)) ;
#36709 = CARTESIAN_POINT('Ctrl Pts',(-20.2625466477775,24.4735460382911,124.65459280721)) ;
#36710 = CARTESIAN_POINT('Ctrl Pts',(-19.9101907899771,24.663463774725,124.50880446125)) ;
#36711 = CARTESIAN_POINT('Ctrl Pts',(-20.0354343909246,24.4834746943151,124.783046651273)) ;
#36712 = CARTESIAN_POINT('Ctrl Pts',(-19.7123608153397,24.6734515209028,124.579209070927)) ;
#36713 = CARTESIAN_POINT('Ctrl Pts',(-19.7881474809578,24.4934624404929,124.871054527535)) ;
#36714 = CARTESIAN_POINT('Ctrl Pts',(-19.504271624768,24.6834875098385,124.614009588062)) ;
#36715 = CARTESIAN_POINT('Ctrl Pts',(-19.5280364526024,24.5034984294287,124.914557400137)) ;
#36716 = CARTESIAN_POINT('Ctrl Pts',(-19.2970799984549,24.6933423796521,124.612527488624)) ;
#36717 = CARTESIAN_POINT('Ctrl Pts',(-19.2690459880679,24.5133532992423,124.91270694931)) ;
#36718 = CARTESIAN_POINT('Ctrl Pts',(-19.090303135345,24.7033418208939,124.574834044645)) ;
#36719 = CARTESIAN_POINT('Ctrl Pts',(-19.0105743992128,24.5233527404841,124.865592193669)) ;
#36720 = CARTESIAN_POINT('Ctrl Pts',(-18.8951262772354,24.713236895074,124.502757695016)) ;
#36721 = CARTESIAN_POINT('Ctrl Pts',(-18.7666019328794,24.5332478146641,124.775498416495)) ;
#36722 = CARTESIAN_POINT('Ctrl Pts',(-18.7124871130711,24.7232975509137,124.396143715782)) ;
#36723 = CARTESIAN_POINT('Ctrl Pts',(-18.5383021509455,24.5433084705038,124.642232833869)) ;
#36724 = CARTESIAN_POINT('Ctrl Pts',(-18.5544214010454,24.7331464251093,124.262378682155)) ;
#36725 = CARTESIAN_POINT('Ctrl Pts',(-18.3407179160903,24.5531573446995,124.475027408932)) ;
#36726 = CARTESIAN_POINT('Ctrl Pts',(-18.4191678408928,24.7431751370725,124.100648450517)) ;
#36727 = CARTESIAN_POINT('Ctrl Pts',(-18.1716495640593,24.5631860566627,124.272865839521)) ;
#36728 = CARTESIAN_POINT('Ctrl Pts',(-18.3145372263734,24.7532045376556,123.917586468341)) ;
#36729 = CARTESIAN_POINT('Ctrl Pts',(-18.0408595711502,24.5732154572458,124.044039432709)) ;
#36730 = CARTESIAN_POINT('Ctrl Pts',(-18.2441926662311,24.7630447312725,123.723038994785)) ;
#36731 = CARTESIAN_POINT('Ctrl Pts',(-17.9529267053287,24.5830556508627,123.800854664301)) ;
#36732 = CARTESIAN_POINT('Ctrl Pts',(-18.2077279525062,24.7730481538477,123.515942344631)) ;
#36733 = CARTESIAN_POINT('Ctrl Pts',(-17.9073440509862,24.5930590734379,123.541984051111)) ;
#36734 = CARTESIAN_POINT('Ctrl Pts',(-18.2078442834315,24.7830336909408,123.305979629472)) ;
#36735 = CARTESIAN_POINT('Ctrl Pts',(-17.9074876719924,24.6030446105309,123.27953044781)) ;
#36736 = CARTESIAN_POINT('Ctrl Pts',(-18.244816810972,24.7930746954276,123.098169474309)) ;
#36737 = CARTESIAN_POINT('Ctrl Pts',(-17.9537014743121,24.6130856150177,123.019767558677)) ;
#36738 = CARTESIAN_POINT('Ctrl Pts',(-18.3156319158811,24.8029182343688,122.903704450163)) ;
#36739 = CARTESIAN_POINT('Ctrl Pts',(-18.0422190939803,24.622929153959,122.776684574522)) ;
#36740 = CARTESIAN_POINT('Ctrl Pts',(-18.4202205854455,24.8129032653596,122.721733922501)) ;
#36741 = CARTESIAN_POINT('Ctrl Pts',(-18.172953642186,24.6329141849498,122.549220386066)) ;
#36742 = CARTESIAN_POINT('Ctrl Pts',(-18.5541770056788,24.8228427278816,122.561322433432)) ;
#36743 = CARTESIAN_POINT('Ctrl Pts',(-18.3403982887931,24.6428536474717,122.348704582973)) ;
#36744 = CARTESIAN_POINT('Ctrl Pts',(-18.715558190906,24.8328824601054,122.425314061368)) ;
#36745 = CARTESIAN_POINT('Ctrl Pts',(-18.5421236161381,24.6528933796956,122.178692975318)) ;
#36746 = CARTESIAN_POINT('Ctrl Pts',(-18.8953205226514,24.8427706404226,122.320888321674)) ;
#36747 = CARTESIAN_POINT('Ctrl Pts',(-18.7668265323495,24.6627815600127,122.048158969727)) ;
#36748 = CARTESIAN_POINT('Ctrl Pts',(-19.0923303882549,24.8527601561251,122.248163396936)) ;
#36749 = CARTESIAN_POINT('Ctrl Pts',(-19.0130885634248,24.6727710757152,121.957251380522)) ;
#36750 = CARTESIAN_POINT('Ctrl Pts',(-19.298364039197,24.8627187067798,122.211026101757)) ;
#36751 = CARTESIAN_POINT('Ctrl Pts',(-19.2706307855843,24.68272962637,121.910828202556)) ;
#36752 = CARTESIAN_POINT('Ctrl Pts',(-19.5064905058478,24.8726181138848,122.209713205834)) ;
#36753 = CARTESIAN_POINT('Ctrl Pts',(-19.5307897392414,24.692629033475,121.909185754138)) ;
#36754 = CARTESIAN_POINT('Ctrl Pts',(-19.7147219092595,24.8826667003011,122.245162774326)) ;
#36755 = CARTESIAN_POINT('Ctrl Pts',(-19.7910790035735,24.7026776198912,121.953496342131)) ;
#36756 = CARTESIAN_POINT('Ctrl Pts',(-19.9106826139148,24.8925595192655,122.314960468538)) ;
#36757 = CARTESIAN_POINT('Ctrl Pts',(-20.0360311857211,24.7125704388557,122.040742561754)) ;
#36758 = CARTESIAN_POINT('Ctrl Pts',(-20.0946951962707,24.9026306367953,122.41960013013)) ;
#36759 = CARTESIAN_POINT('Ctrl Pts',(-20.2660472328495,24.7226415563855,122.171540812084)) ;
#36760 = CARTESIAN_POINT('Ctrl Pts',(-20.2538475997201,24.9124463307614,122.551014009269)) ;
#36761 = CARTESIAN_POINT('Ctrl Pts',(-20.4649896869085,24.7324572503516,122.335808206384)) ;
#36762 = CARTESIAN_POINT('Ctrl Pts',(-20.3913621573758,24.9225127082587,122.711814363181)) ;
#36763 = CARTESIAN_POINT('Ctrl Pts',(-20.6368834830803,24.7425236278489,122.536807653751)) ;
#36764 = CARTESIAN_POINT('Ctrl Pts',(-20.4970748886783,24.9324116943406,122.891133137665)) ;
#36765 = CARTESIAN_POINT('Ctrl Pts',(-20.7690258159977,24.7524226139307,122.760956322178)) ;
#36766 = CARTESIAN_POINT('Ctrl Pts',(-20.571232101278,24.9424658743341,123.089018879175)) ;
#36767 = CARTESIAN_POINT('Ctrl Pts',(-20.8617232643384,24.7624767939243,123.008312860286)) ;
#36768 = CARTESIAN_POINT('Ctrl Pts',(-20.6094160911567,24.9523366872668,123.293040667745)) ;
#36769 = CARTESIAN_POINT('Ctrl Pts',(-20.909454464959,24.772347606857,123.263341038954)) ;
#36770 = CARTESIAN_POINT('Ctrl Pts',(-20.6116329545151,24.9624105881206,123.504764653356)) ;
#36771 = CARTESIAN_POINT('Ctrl Pts',(-20.9122265610238,24.7824215077108,123.527995577723)) ;
#36772 = CARTESIAN_POINT('Ctrl Pts',(-20.5781600299015,24.9722307435072,123.708532107742)) ;
#36773 = CARTESIAN_POINT('Ctrl Pts',(-20.8703860649525,24.7922416630974,123.782706579773)) ;
#36774 = CARTESIAN_POINT('Ctrl Pts',(-20.508237892881,24.9823094504595,123.908493710654)) ;
#36775 = CARTESIAN_POINT('Ctrl Pts',(-20.7829843523963,24.8023203700497,124.032658419527)) ;
#36776 = CARTESIAN_POINT('Ctrl Pts',(-20.4070053264551,24.9921610389983,124.089234851178)) ;
#36777 = CARTESIAN_POINT('Ctrl Pts',(-20.6564437175052,24.8121719585885,124.258586397177)) ;
#36778 = CARTESIAN_POINT('Ctrl Pts',(-20.2731799394624,25.0022341555233,124.253310305418)) ;
#36779 = CARTESIAN_POINT('Ctrl Pts',(-20.489162844456,24.8222450751134,124.463680852366)) ;
#36780 = CARTESIAN_POINT('Ctrl Pts',(-20.1165044718704,25.0120766726191,124.388500704501)) ;
#36781 = CARTESIAN_POINT('Ctrl Pts',(-20.2933179390666,24.8320875922093,124.63267035684)) ;
#36782 = CARTESIAN_POINT('Ctrl Pts',(-19.936630039934,25.022057134173,124.496508778481)) ;
#36783 = CARTESIAN_POINT('Ctrl Pts',(-20.0684748873382,24.8420680537632,124.767681031744)) ;
#36784 = CARTESIAN_POINT('Ctrl Pts',(-19.7398406206067,25.0320753841638,124.571552225653)) ;
#36785 = CARTESIAN_POINT('Ctrl Pts',(-19.8224883547099,24.852086303754,124.861485946941)) ;
#36786 = CARTESIAN_POINT('Ctrl Pts',(-19.5358376882034,25.0419595443576,124.611179719753)) ;
#36787 = CARTESIAN_POINT('Ctrl Pts',(-19.5674837085311,24.8619704639478,124.911020996761)) ;
#36788 = CARTESIAN_POINT('Ctrl Pts',(-19.3242913071813,25.0520246913326,124.614802833866)) ;
#36789 = CARTESIAN_POINT('Ctrl Pts',(-19.3030511329989,24.8720356109227,124.915550386489)) ;
#36790 = CARTESIAN_POINT('Ctrl Pts',(-19.1199106240367,25.0618665149734,124.582483950528)) ;
#36791 = CARTESIAN_POINT('Ctrl Pts',(-19.0475737608412,24.8818774345635,124.875152002787)) ;
#36792 = CARTESIAN_POINT('Ctrl Pts',(-18.9203492375791,25.0718959874342,124.514427752027)) ;
#36793 = CARTESIAN_POINT('Ctrl Pts',(-18.7981220481648,24.8919069070244,124.790082006615)) ;
#36794 = CARTESIAN_POINT('Ctrl Pts',(-18.7359613362089,25.0819228426962,124.412260699821)) ;
#36795 = CARTESIAN_POINT('Ctrl Pts',(-18.5676370264937,24.9019337622864,124.662373648664)) ;
#36796 = CARTESIAN_POINT('Ctrl Pts',(-18.5748042640139,25.0917660928068,124.282445342146)) ;
#36797 = CARTESIAN_POINT('Ctrl Pts',(-18.3661893963052,24.9117770123969,124.500103756248)) ;
#36798 = CARTESIAN_POINT('Ctrl Pts',(-18.4355859909014,25.1018145323899,124.123567079919)) ;
#36799 = CARTESIAN_POINT('Ctrl Pts',(-18.1921666069549,24.9218254519801,124.301506228966)) ;
#36800 = CARTESIAN_POINT('Ctrl Pts',(-18.3274272880711,25.1117640266378,123.944530772977)) ;
#36801 = CARTESIAN_POINT('Ctrl Pts',(-18.0569676781465,24.931774946228,124.07771050016)) ;
#36802 = CARTESIAN_POINT('Ctrl Pts',(-18.2517272644222,25.1216718823638,123.750467023187)) ;
#36803 = CARTESIAN_POINT('Ctrl Pts',(-17.9623422827385,24.941682801954,123.835129981022)) ;
#36804 = CARTESIAN_POINT('Ctrl Pts',(-18.2104743970335,25.1317313590138,123.543070104516)) ;
#36805 = CARTESIAN_POINT('Ctrl Pts',(-17.9107761379944,24.9517422786039,123.575884197332)) ;
#36806 = CARTESIAN_POINT('Ctrl Pts',(-18.2056782190192,25.1415721684225,123.336215569633)) ;
#36807 = CARTESIAN_POINT('Ctrl Pts',(-17.9047808644397,24.9615830880126,123.317314560697)) ;
#36808 = CARTESIAN_POINT('Ctrl Pts',(-18.2373040930332,25.1516343187233,123.127077183961)) ;
#36809 = CARTESIAN_POINT('Ctrl Pts',(-17.944313237632,24.9716452383135,123.055891956655)) ;
#36810 = CARTESIAN_POINT('Ctrl Pts',(-18.3038712513499,25.1615314798458,122.929932299027)) ;
#36811 = CARTESIAN_POINT('Ctrl Pts',(-18.0275225051549,24.981542399436,122.809459900644)) ;
#36812 = CARTESIAN_POINT('Ctrl Pts',(-18.4033840340755,25.1714626542499,122.746394261675)) ;
#36813 = CARTESIAN_POINT('Ctrl Pts',(-18.1519140706744,24.9914735738401,122.580036852165)) ;
#36814 = CARTESIAN_POINT('Ctrl Pts',(-18.534887670248,25.1815048579749,122.581237562845)) ;
#36815 = CARTESIAN_POINT('Ctrl Pts',(-18.3162936299814,25.0015157775651,122.373591256338)) ;
#36816 = CARTESIAN_POINT('Ctrl Pts',(-18.690527647173,25.1913914404053,122.443467269935)) ;
#36817 = CARTESIAN_POINT('Ctrl Pts',(-18.5108445770274,25.0114023599955,122.201377852342)) ;
#36818 = CARTESIAN_POINT('Ctrl Pts',(-18.8694400895696,25.2013848761537,122.333355299341)) ;
#36819 = CARTESIAN_POINT('Ctrl Pts',(-18.7344855027251,25.0213957957439,122.063738108115)) ;
#36820 = CARTESIAN_POINT('Ctrl Pts',(-19.0638333349581,25.2113293445118,122.256415312659)) ;
#36821 = CARTESIAN_POINT('Ctrl Pts',(-18.9774777480987,25.031340264102,121.967563231997)) ;
#36822 = CARTESIAN_POINT('Ctrl Pts',(-19.2687117383254,25.2212811607574,122.213977770171)) ;
#36823 = CARTESIAN_POINT('Ctrl Pts',(-19.2335763972237,25.0412920803476,121.914516693605)) ;
#36824 = CARTESIAN_POINT('Ctrl Pts',(-19.4796320217027,25.2313185968719,122.207898426795)) ;
#36825 = CARTESIAN_POINT('Ctrl Pts',(-19.497226599863,25.0513295164621,121.906917954513)) ;
#36826 = CARTESIAN_POINT('Ctrl Pts',(-19.6852897576632,25.2412035560482,122.237873411144)) ;
#36827 = CARTESIAN_POINT('Ctrl Pts',(-19.7542997604655,25.0612144756384,121.944387345467)) ;
#36828 = CARTESIAN_POINT('Ctrl Pts',(-19.8849152260127,25.2512016742602,122.303598681316)) ;
#36829 = CARTESIAN_POINT('Ctrl Pts',(-20.0038315528592,25.0712125938503,122.026544562905)) ;
#36830 = CARTESIAN_POINT('Ctrl Pts',(-20.0687767747122,25.2611226067721,122.402114690331)) ;
#36831 = CARTESIAN_POINT('Ctrl Pts',(-20.2336588621187,25.0811335263623,122.149690526429)) ;
#36832 = CARTESIAN_POINT('Ctrl Pts',(-20.2347377539777,25.2711639069942,122.532559750854)) ;
#36833 = CARTESIAN_POINT('Ctrl Pts',(-20.441109523497,25.0911748265844,122.312747279653)) ;
#36834 = CARTESIAN_POINT('Ctrl Pts',(-20.3735985016344,25.2810708253842,122.687791031638)) ;
#36835 = CARTESIAN_POINT('Ctrl Pts',(-20.6146855653085,25.1010817449744,122.506787487655)) ;
#36836 = CARTESIAN_POINT('Ctrl Pts',(-20.4842246461165,25.2910066170932,122.864973861521)) ;
#36837 = CARTESIAN_POINT('Ctrl Pts',(-20.7529678400748,25.1110175366834,122.728267052346)) ;
#36838 = CARTESIAN_POINT('Ctrl Pts',(-20.5630324165797,25.3010475116711,123.060797396838)) ;
#36839 = CARTESIAN_POINT('Ctrl Pts',(-20.8514767359584,25.1210584312613,122.973046599263)) ;
#36840 = CARTESIAN_POINT('Ctrl Pts',(-20.6061255781903,25.310934713385,123.264152339049)) ;
#36841 = CARTESIAN_POINT('Ctrl Pts',(-20.9053425590563,25.1309456329752,123.227241473622)) ;
#36842 = CARTESIAN_POINT('Ctrl Pts',(-20.6136784836377,25.3209269811466,123.474070984614)) ;
#36843 = CARTESIAN_POINT('Ctrl Pts',(-20.9147827033074,25.1409379007368,123.489640019816)) ;
#36844 = CARTESIAN_POINT('Ctrl Pts',(-20.5847340091675,25.3308755021684,123.681219469277)) ;
#36845 = CARTESIAN_POINT('Ctrl Pts',(-20.8786010725956,25.1508864217586,123.74857602838)) ;
#36846 = CARTESIAN_POINT('Ctrl Pts',(-20.5206272668833,25.3408122757461,123.880023760585)) ;
#36847 = CARTESIAN_POINT('Ctrl Pts',(-20.7984664180072,25.1608231953363,123.997081667637)) ;
#36848 = CARTESIAN_POINT('Ctrl Pts',(-20.4227342551937,25.3507953238871,124.065699360491)) ;
#36849 = CARTESIAN_POINT('Ctrl Pts',(-20.6760989907046,25.1708062434773,124.229175844489)) ;
#36850 = CARTESIAN_POINT('Ctrl Pts',(-20.2930330978776,25.3608390314972,124.232290893968)) ;
#36851 = CARTESIAN_POINT('Ctrl Pts',(-20.5139718407588,25.1808499510873,124.437414474458)) ;
#36852 = CARTESIAN_POINT('Ctrl Pts',(-20.1400132496701,25.3706677246505,124.3711852769)) ;
#36853 = CARTESIAN_POINT('Ctrl Pts',(-20.3226951495679,25.1906786442406,124.611032523196)) ;
#36854 = CARTESIAN_POINT('Ctrl Pts',(-19.9609525577094,25.3807424737799,124.484253952446)) ;
#36855 = CARTESIAN_POINT('Ctrl Pts',(-20.098868954163,25.2007533933701,124.752367074703)) ;
#36856 = CARTESIAN_POINT('Ctrl Pts',(-19.7689867735879,25.3906077995755,124.56282261199)) ;
#36857 = CARTESIAN_POINT('Ctrl Pts',(-19.8589101906674,25.2106187191656,124.850577176183)) ;
#36858 = CARTESIAN_POINT('Ctrl Pts',(-19.5632165090055,25.4006299739324,124.608087313352)) ;
#36859 = CARTESIAN_POINT('Ctrl Pts',(-19.6016970937492,25.2206408935226,124.907156637962)) ;
#36860 = CARTESIAN_POINT('Ctrl Pts',(-19.3525876909076,25.4106560271393,124.616422421431)) ;
#36861 = CARTESIAN_POINT('Ctrl Pts',(-19.3384110920263,25.2306669467295,124.917574265038)) ;
#36862 = CARTESIAN_POINT('Ctrl Pts',(-19.147287360646,25.4205097239856,124.588883432483)) ;
#36863 = CARTESIAN_POINT('Ctrl Pts',(-19.0817846505266,25.2405206435758,124.883149004146)) ;
#36864 = CARTESIAN_POINT('Ctrl Pts',(-18.9475566685195,25.4304691287386,124.526036690547)) ;
#36865 = CARTESIAN_POINT('Ctrl Pts',(-18.8321213569648,25.2504800483288,124.804588928361)) ;
#36866 = CARTESIAN_POINT('Ctrl Pts',(-18.7604916580374,25.4405073744435,124.428375640314)) ;
#36867 = CARTESIAN_POINT('Ctrl Pts',(-18.5982908950079,25.2605182940336,124.682511380087)) ;
#36868 = CARTESIAN_POINT('Ctrl Pts',(-18.5957013870381,25.4503815586055,124.302092265061)) ;
#36869 = CARTESIAN_POINT('Ctrl Pts',(-18.3923032184269,25.2703924781957,124.524655280028)) ;
#36870 = CARTESIAN_POINT('Ctrl Pts',(-18.4526055536538,25.4604513417434,124.146119088409)) ;
#36871 = CARTESIAN_POINT('Ctrl Pts',(-18.2134348353702,25.2804622613336,124.329687992467)) ;
#36872 = CARTESIAN_POINT('Ctrl Pts',(-18.3413212778129,25.4702845967642,123.971882300025)) ;
#36873 = CARTESIAN_POINT('Ctrl Pts',(-18.0743301698289,25.2902955163544,124.111890051022)) ;
#36874 = CARTESIAN_POINT('Ctrl Pts',(-18.2598482943526,25.4803150228959,123.777393425404)) ;
#36875 = CARTESIAN_POINT('Ctrl Pts',(-17.9724906535457,25.300325942486,123.868778335206)) ;
#36876 = CARTESIAN_POINT('Ctrl Pts',(-18.2139714522043,25.4903466350829,123.571535696539)) ;
#36877 = CARTESIAN_POINT('Ctrl Pts',(-17.91514620018,25.3103575546731,123.611455902994)) ;
#36878 = CARTESIAN_POINT('Ctrl Pts',(-18.2042958256806,25.5001763319375,123.365125390913)) ;
#36879 = CARTESIAN_POINT('Ctrl Pts',(-17.9030533677923,25.3201872515277,123.353441667696)) ;
#36880 = CARTESIAN_POINT('Ctrl Pts',(-18.2304147172978,25.51016577384,123.156740327135)) ;
#36881 = CARTESIAN_POINT('Ctrl Pts',(-17.9357039465611,25.3301766934301,123.092960405567)) ;
#36882 = CARTESIAN_POINT('Ctrl Pts',(-18.2931661314917,25.5202096658556,122.955127632222)) ;
#36883 = CARTESIAN_POINT('Ctrl Pts',(-18.0141448809972,25.3402205854458,122.840945210774)) ;
#36884 = CARTESIAN_POINT('Ctrl Pts',(-18.3874495319765,25.5300312276249,122.771432509652)) ;
#36885 = CARTESIAN_POINT('Ctrl Pts',(-18.1320014122623,25.3500421472151,122.61132607428)) ;
#36886 = CARTESIAN_POINT('Ctrl Pts',(-18.5144967250623,25.5400667992491,122.60299121237)) ;
#36887 = CARTESIAN_POINT('Ctrl Pts',(-18.2908120041976,25.3600777188393,122.400775785522)) ;
#36888 = CARTESIAN_POINT('Ctrl Pts',(-18.669193308683,25.5500960735309,122.459723633636)) ;
#36889 = CARTESIAN_POINT('Ctrl Pts',(-18.4841839837609,25.370106993121,122.221692735546)) ;
#36890 = CARTESIAN_POINT('Ctrl Pts',(-18.8426660315161,25.5599299106495,122.34725013946)) ;
#36891 = CARTESIAN_POINT('Ctrl Pts',(-18.7010269360749,25.3799408302397,122.081101987124)) ;
#36892 = CARTESIAN_POINT('Ctrl Pts',(-19.0371487210636,25.5699823067377,122.26458450001)) ;
#36893 = CARTESIAN_POINT('Ctrl Pts',(-18.9441309444013,25.3899932263279,121.977771975158)) ;
#36894 = CARTESIAN_POINT('Ctrl Pts',(-19.2407432881081,25.5799190736882,122.217749926032)) ;
#36895 = CARTESIAN_POINT('Ctrl Pts',(-19.1986250892974,25.3999299932784,121.919230643836)) ;
#36896 = CARTESIAN_POINT('Ctrl Pts',(-19.4492836308601,25.5898533086675,122.206441411571)) ;
#36897 = CARTESIAN_POINT('Ctrl Pts',(-19.4593011285886,25.4098642282577,121.905097168165)) ;
#36898 = CARTESIAN_POINT('Ctrl Pts',(-19.6584731388207,25.5998770719943,122.231868584206)) ;
#36899 = CARTESIAN_POINT('Ctrl Pts',(-19.7207877370462,25.4198879915845,121.936883279479)) ;
#36900 = CARTESIAN_POINT('Ctrl Pts',(-19.8573510139272,25.6097634133789,122.292244191361)) ;
#36901 = CARTESIAN_POINT('Ctrl Pts',(-19.96938514331,25.4297743329691,122.012355109313)) ;
#36902 = CARTESIAN_POINT('Ctrl Pts',(-20.0448786077411,25.6197524621459,122.386778679778)) ;
#36903 = CARTESIAN_POINT('Ctrl Pts',(-20.2037937296908,25.4397633817361,122.13052536822)) ;
#36904 = CARTESIAN_POINT('Ctrl Pts',(-20.2137531182518,25.6297936828433,122.513441376923)) ;
#36905 = CARTESIAN_POINT('Ctrl Pts',(-20.4148854639399,25.4498046024334,122.288855457057)) ;
#36906 = CARTESIAN_POINT('Ctrl Pts',(-20.3553169833918,25.6396263230212,122.664067992544)) ;
#36907 = CARTESIAN_POINT('Ctrl Pts',(-20.5918392756483,25.4596372426114,122.47714100209)) ;
#36908 = CARTESIAN_POINT('Ctrl Pts',(-20.4709395710573,25.6496202523291,122.839494815761)) ;
#36909 = CARTESIAN_POINT('Ctrl Pts',(-20.7363655380305,25.4696311719193,122.696425976551)) ;
#36910 = CARTESIAN_POINT('Ctrl Pts',(-20.5542313166204,25.6596494600097,123.033193067616)) ;
#36911 = CARTESIAN_POINT('Ctrl Pts',(-20.8404780633485,25.4796603795999,122.938549694625)) ;
#36912 = CARTESIAN_POINT('Ctrl Pts',(-20.6022166705038,25.6695252717138,123.235204192602)) ;
#36913 = CARTESIAN_POINT('Ctrl Pts',(-20.9004575631495,25.489536191304,123.191064817274)) ;
#36914 = CARTESIAN_POINT('Ctrl Pts',(-20.6147777399099,25.6795244986852,123.445015641522)) ;
#36915 = CARTESIAN_POINT('Ctrl Pts',(-20.9161564442724,25.4995354182754,123.453329386863)) ;
#36916 = CARTESIAN_POINT('Ctrl Pts',(-20.5911250967984,25.6894339798409,123.652027739966)) ;
#36917 = CARTESIAN_POINT('Ctrl Pts',(-20.8865881010468,25.5094448994311,123.71209469823)) ;
#36918 = CARTESIAN_POINT('Ctrl Pts',(-20.531017224915,25.6994872101418,123.854627589131)) ;
#36919 = CARTESIAN_POINT('Ctrl Pts',(-20.8114508926531,25.519498129732,123.965343699731)) ;
#36920 = CARTESIAN_POINT('Ctrl Pts',(-20.4384325667578,25.7093578266928,124.040355450809)) ;
#36921 = CARTESIAN_POINT('Ctrl Pts',(-20.6957175422726,25.529368746283,124.197502953575)) ;
#36922 = CARTESIAN_POINT('Ctrl Pts',(-20.3135029459365,25.7193794884249,124.210003208649)) ;
#36923 = CARTESIAN_POINT('Ctrl Pts',(-20.5395534187426,25.539390408015,124.409561109436)) ;
#36924 = CARTESIAN_POINT('Ctrl Pts',(-20.1606542811385,25.729402301606,124.355058412312)) ;
#36925 = CARTESIAN_POINT('Ctrl Pts',(-20.3484908449699,25.5494132211962,124.590878299878)) ;
#36926 = CARTESIAN_POINT('Ctrl Pts',(-19.9878788008662,25.7392694660659,124.469843004655)) ;
#36927 = CARTESIAN_POINT('Ctrl Pts',(-20.1325195803548,25.5592803856561,124.734357216865)) ;
#36928 = CARTESIAN_POINT('Ctrl Pts',(-19.7955437673314,25.7492629082859,124.554394992238)) ;
#36929 = CARTESIAN_POINT('Ctrl Pts',(-19.8920996177398,25.569273827876,124.840044812228)) ;
#36930 = CARTESIAN_POINT('Ctrl Pts',(-19.5905777687678,25.7592945818862,124.604056660559)) ;
#36931 = CARTESIAN_POINT('Ctrl Pts',(-19.6358915111291,25.5793055014764,124.902119378394)) ;
#36932 = CARTESIAN_POINT('Ctrl Pts',(-19.3835799225067,25.7691610169992,124.617474520566)) ;
#36933 = CARTESIAN_POINT('Ctrl Pts',(-19.3771435134403,25.5891719365894,124.918889100864)) ;
#36934 = CARTESIAN_POINT('Ctrl Pts',(-19.1748644935385,25.7791484675323,124.594811648332)) ;
#36935 = CARTESIAN_POINT('Ctrl Pts',(-19.1162493957919,25.5991593871224,124.890557819101)) ;
#36936 = CARTESIAN_POINT('Ctrl Pts',(-18.9740276761385,25.7890933973602,124.536594188768)) ;
#36937 = CARTESIAN_POINT('Ctrl Pts',(-18.8652039002505,25.6091043169504,124.817783333107)) ;
#36938 = CARTESIAN_POINT('Ctrl Pts',(-18.7845612887665,25.7991382924153,124.443378041818)) ;
#36939 = CARTESIAN_POINT('Ctrl Pts',(-18.6283721225414,25.6191492120055,124.701260743768)) ;
#36940 = CARTESIAN_POINT('Ctrl Pts',(-18.6171242290503,25.8090003541012,124.321077049524)) ;
#36941 = CARTESIAN_POINT('Ctrl Pts',(-18.4190770494623,25.6290112736914,124.5483820594)) ;
#36942 = CARTESIAN_POINT('Ctrl Pts',(-18.4712964694787,25.818992076888,124.169910090686)) ;
#36943 = CARTESIAN_POINT('Ctrl Pts',(-18.2367942708483,25.6390029964782,124.359421375192)) ;
#36944 = CARTESIAN_POINT('Ctrl Pts',(-18.3546829235641,25.828924291128,123.996697923502)) ;
#36945 = CARTESIAN_POINT('Ctrl Pts',(-18.0910294951363,25.6489352107182,124.142904444587)) ;
#36946 = CARTESIAN_POINT('Ctrl Pts',(-18.269414013462,25.8388636096937,123.805925409421)) ;
#36947 = CARTESIAN_POINT('Ctrl Pts',(-17.9844458362776,25.6588745292839,123.904437503989)) ;
#36948 = CARTESIAN_POINT('Ctrl Pts',(-18.2182183799845,25.8489077844696,123.601068446955)) ;
#36949 = CARTESIAN_POINT('Ctrl Pts',(-17.9204539830974,25.6689187040598,123.648365609481)) ;
#36950 = CARTESIAN_POINT('Ctrl Pts',(-18.2035144290787,25.8587783385346,123.394080423168)) ;
#36951 = CARTESIAN_POINT('Ctrl Pts',(-17.9020768057529,25.6787892581248,123.389630116783)) ;
#36952 = CARTESIAN_POINT('Ctrl Pts',(-18.2245755858917,25.8687433208888,123.185646036697)) ;
#36953 = CARTESIAN_POINT('Ctrl Pts',(-17.9284060680504,25.6887542404789,123.129087322385)) ;
#36954 = CARTESIAN_POINT('Ctrl Pts',(-18.2821927216553,25.8787740237786,122.982799143705)) ;
#36955 = CARTESIAN_POINT('Ctrl Pts',(-18.0004301996435,25.6987849433688,122.875529417098)) ;
#36956 = CARTESIAN_POINT('Ctrl Pts',(-18.3726282398812,25.8886663638038,122.795495732635)) ;
#36957 = CARTESIAN_POINT('Ctrl Pts',(-18.113477198808,25.708677283394,122.641401239068)) ;
#36958 = CARTESIAN_POINT('Ctrl Pts',(-18.4961390189177,25.8987195969637,122.624026714153)) ;
#36959 = CARTESIAN_POINT('Ctrl Pts',(-18.2678679862783,25.7187305165539,122.427066576794)) ;
#36960 = CARTESIAN_POINT('Ctrl Pts',(-18.6449144456404,25.9086008414405,122.478993547401)) ;
#36961 = CARTESIAN_POINT('Ctrl Pts',(-18.4538393268048,25.7286117610307,122.245777047837)) ;
#36962 = CARTESIAN_POINT('Ctrl Pts',(-18.8191018734821,25.9186339623115,122.36011093306)) ;
#36963 = CARTESIAN_POINT('Ctrl Pts',(-18.6715752592843,25.7386448819017,122.097176077523)) ;
#36964 = CARTESIAN_POINT('Ctrl Pts',(-19.0083693285525,25.9285151725866,122.274392628594)) ;
#36965 = CARTESIAN_POINT('Ctrl Pts',(-18.9081608032802,25.7485260921767,121.990030737778)) ;
#36966 = CARTESIAN_POINT('Ctrl Pts',(-19.2132442732851,25.9385772483559,122.221858172896)) ;
#36967 = CARTESIAN_POINT('Ctrl Pts',(-19.1642552672719,25.7585881679461,121.924365385108)) ;
#36968 = CARTESIAN_POINT('Ctrl Pts',(-19.41988850403,25.9484343067377,122.205946244502)) ;
#36969 = CARTESIAN_POINT('Ctrl Pts',(-19.4225607860538,25.7684452263278,121.904478285309)) ;
#36970 = CARTESIAN_POINT('Ctrl Pts',(-19.6290114818218,25.9584288620267,122.226010291668)) ;
#36971 = CARTESIAN_POINT('Ctrl Pts',(-19.6839642883696,25.7784397816168,121.929561151794)) ;
#36972 = CARTESIAN_POINT('Ctrl Pts',(-19.8301627349406,25.9683547495622,122.281640275295)) ;
#36973 = CARTESIAN_POINT('Ctrl Pts',(-19.9354025959097,25.7883656691523,121.99910133033)) ;
#36974 = CARTESIAN_POINT('Ctrl Pts',(-20.0204672700362,25.9783797695574,122.372173587935)) ;
#36975 = CARTESIAN_POINT('Ctrl Pts',(-20.1732821454696,25.7983906891476,122.112270545076)) ;
#36976 = CARTESIAN_POINT('Ctrl Pts',(-20.1900359400144,25.9882771466611,122.492771224812)) ;
#36977 = CARTESIAN_POINT('Ctrl Pts',(-20.3852412940492,25.8082880662513,122.26301982618)) ;
#36978 = CARTESIAN_POINT('Ctrl Pts',(-20.3377857345997,25.998267383742,122.642047679255)) ;
#36979 = CARTESIAN_POINT('Ctrl Pts',(-20.5699265940413,25.8182783033321,122.449617357503)) ;
#36980 = CARTESIAN_POINT('Ctrl Pts',(-20.4575881124741,26.0083039965508,122.815736066675)) ;
#36981 = CARTESIAN_POINT('Ctrl Pts',(-20.7196773405348,25.828314916141,122.66672955988)) ;
#36982 = CARTESIAN_POINT('Ctrl Pts',(-20.5440893195705,26.0181538799688,123.003887825492)) ;
#36983 = CARTESIAN_POINT('Ctrl Pts',(-20.8278012350938,25.838164799559,122.901920139977)) ;
#36984 = CARTESIAN_POINT('Ctrl Pts',(-20.5978286138219,26.0281574968712,123.207191914562)) ;
#36985 = CARTESIAN_POINT('Ctrl Pts',(-20.8949727103814,25.8481684164614,123.156051177418)) ;
#36986 = CARTESIAN_POINT('Ctrl Pts',(-20.6153163617937,26.0381469086364,123.416505710601)) ;
#36987 = CARTESIAN_POINT('Ctrl Pts',(-20.9168297434184,25.8581578282265,123.417692998704)) ;
#36988 = CARTESIAN_POINT('Ctrl Pts',(-20.5960135788333,26.0481656699812,123.626222930686)) ;
#36989 = CARTESIAN_POINT('Ctrl Pts',(-20.8926982525925,25.8681765895714,123.679841956344)) ;
#36990 = CARTESIAN_POINT('Ctrl Pts',(-20.5232631932467,26.0613843453623,123.894483327193)) ;
#36991 = CARTESIAN_POINT('Ctrl Pts',(-20.8017581312265,25.8813952649524,124.015153473763)) ;
#36992 = CARTESIAN_POINT('Ctrl Pts',(-20.3813483402664,26.074694652607,124.13929149955)) ;
#36993 = CARTESIAN_POINT('Ctrl Pts',(-20.624392002949,25.8947055721972,124.32113343049)) ;
#36994 = CARTESIAN_POINT('Ctrl Pts',(-20.1842168943985,26.087932318833,124.335713981098)) ;
#36995 = CARTESIAN_POINT('Ctrl Pts',(-20.3779377393068,25.9079432384232,124.566705392329)) ;
#36996 = CARTESIAN_POINT('Ctrl Pts',(-20.0135494311699,26.0978520142437,124.455575991443)) ;
#36997 = CARTESIAN_POINT('Ctrl Pts',(-20.164609841779,25.9178629338339,124.716521317897)) ;
#36998 = CARTESIAN_POINT('Ctrl Pts',(-19.8220452045287,26.1079048812422,124.544939686849)) ;
#36999 = CARTESIAN_POINT('Ctrl Pts',(-19.9252257841206,25.9279158008324,124.828226044288)) ;
#37000 = CARTESIAN_POINT('Ctrl Pts',(-19.6219710853917,26.1177602895715,124.598853822715)) ;
#37001 = CARTESIAN_POINT('Ctrl Pts',(-19.675135063597,25.9377712091617,124.895616007235)) ;
#37002 = CARTESIAN_POINT('Ctrl Pts',(-19.4118059045154,26.1277989212481,124.617896062361)) ;
#37003 = CARTESIAN_POINT('Ctrl Pts',(-19.4124225556357,25.9478098408382,124.919414322687)) ;
#37004 = CARTESIAN_POINT('Ctrl Pts',(-19.1331380537758,26.1411011035151,124.594040851199)) ;
#37005 = CARTESIAN_POINT('Ctrl Pts',(-19.0641152659806,25.9611120231053,124.889602890064)) ;
#37006 = CARTESIAN_POINT('Ctrl Pts',(-18.8021064780862,26.157646116598,124.475037573678)) ;
#37007 = CARTESIAN_POINT('Ctrl Pts',(-18.6502847526596,25.9776570361881,124.74081980976)) ;
#37008 = CARTESIAN_POINT('Ctrl Pts',(-18.5297345481408,26.1742981326742,124.248799717429)) ;
#37009 = CARTESIAN_POINT('Ctrl Pts',(-18.3098802866358,25.9943090522644,124.458074394321)) ;
#37010 = CARTESIAN_POINT('Ctrl Pts',(-18.369098727454,26.1875212235794,124.021942776296)) ;
#37011 = CARTESIAN_POINT('Ctrl Pts',(-18.1090436807986,26.0075321431696,124.174455573263)) ;
#37012 = CARTESIAN_POINT('Ctrl Pts',(-18.2790691456165,26.1974821831388,123.832864887124)) ;
#37013 = CARTESIAN_POINT('Ctrl Pts',(-17.9965176539115,26.0174931027289,123.938117510203)) ;
#37014 = CARTESIAN_POINT('Ctrl Pts',(-18.2231373596907,26.2075069798899,123.629678729636)) ;
#37015 = CARTESIAN_POINT('Ctrl Pts',(-17.9266031350855,26.0275178994801,123.684128675008)) ;
#37016 = CARTESIAN_POINT('Ctrl Pts',(-18.19662185451,26.2207314272857,123.352884992182)) ;
#37017 = CARTESIAN_POINT('Ctrl Pts',(-17.8934600553599,26.0407423468759,123.338151922394)) ;
#37018 = CARTESIAN_POINT('Ctrl Pts',(-18.2547370627252,26.2373652119848,123.004073948381)) ;
#37019 = CARTESIAN_POINT('Ctrl Pts',(-17.966109897948,26.0573761315749,122.902122581891)) ;
#37020 = CARTESIAN_POINT('Ctrl Pts',(-18.4626485183739,26.2572678787097,122.635440004849)) ;
#37021 = CARTESIAN_POINT('Ctrl Pts',(-18.2260016701875,26.0772787982999,122.441338078441)) ;
#37022 = CARTESIAN_POINT('Ctrl Pts',(-18.7834207710504,26.2771681064916,122.359539756273)) ;
#37023 = CARTESIAN_POINT('Ctrl Pts',(-18.6269689740225,26.0971790260817,122.096464789872)) ;
#37024 = CARTESIAN_POINT('Ctrl Pts',(-19.1793519772945,26.2970855940231,122.209249706673)) ;
#37025 = CARTESIAN_POINT('Ctrl Pts',(-19.1218834344453,26.1170965136132,121.908606135726)) ;
#37026 = CARTESIAN_POINT('Ctrl Pts',(-19.60307943523,26.31701511984,122.202825724999)) ;
#37027 = CARTESIAN_POINT('Ctrl Pts',(-19.6515421009245,26.1370260394302,121.900579249944)) ;
#37028 = CARTESIAN_POINT('Ctrl Pts',(-20.004197714649,26.3369773877262,122.341686788595)) ;
#37029 = CARTESIAN_POINT('Ctrl Pts',(-20.152938612381,26.1569883073164,122.074158377554)) ;
#37030 = CARTESIAN_POINT('Ctrl Pts',(-20.3326211942537,26.3568675826784,122.608053388485)) ;
#37031 = CARTESIAN_POINT('Ctrl Pts',(-20.5634651728488,26.1768785022686,122.407118082676)) ;
#37032 = CARTESIAN_POINT('Ctrl Pts',(-20.5514266364284,26.3767578274247,122.970081973903)) ;
#37033 = CARTESIAN_POINT('Ctrl Pts',(-20.8369695351396,26.1967687470149,122.85965377227)) ;
#37034 = CARTESIAN_POINT('Ctrl Pts',(-20.6334217410706,26.3968321999872,123.388909430167)) ;
#37035 = CARTESIAN_POINT('Ctrl Pts',(-20.9394612389144,26.2168431195774,123.383189522099)) ;
#37036 = CARTESIAN_POINT('Ctrl Pts',(-20.5686369856693,26.4166175773475,123.804638740479)) ;
#37037 = CARTESIAN_POINT('Ctrl Pts',(-20.8584786210776,26.2366284969377,123.902848054714)) ;
#37038 = CARTESIAN_POINT('Ctrl Pts',(-20.3652722304398,26.4365794514146,124.177147234351)) ;
#37039 = CARTESIAN_POINT('Ctrl Pts',(-20.6042720421634,26.2565903710048,124.368482650249)) ;
#37040 = CARTESIAN_POINT('Ctrl Pts',(-20.0459994667024,26.4565594269051,124.457421972499)) ;
#37041 = CARTESIAN_POINT('Ctrl Pts',(-20.205180240238,26.2765703464953,124.71882479519)) ;
#37042 = CARTESIAN_POINT('Ctrl Pts',(-19.6538522670745,26.476371856783,124.611397902099)) ;
#37043 = CARTESIAN_POINT('Ctrl Pts',(-19.7149987089406,26.2963827763732,124.911292999906)) ;
#37044 = CARTESIAN_POINT('Ctrl Pts',(-19.2292568239862,26.4963519648733,124.622952036836)) ;
#37045 = CARTESIAN_POINT('Ctrl Pts',(-19.1842547999706,26.3163628844635,124.925735636697)) ;
#37046 = CARTESIAN_POINT('Ctrl Pts',(-18.8278291774401,26.5162463484706,124.489264756815)) ;
#37047 = CARTESIAN_POINT('Ctrl Pts',(-18.6824717518565,26.3362572680608,124.758627144379)) ;
#37048 = CARTESIAN_POINT('Ctrl Pts',(-18.4954865718006,26.5361732764478,124.226604674122)) ;
#37049 = CARTESIAN_POINT('Ctrl Pts',(-18.267043998799,26.356184196038,124.430303289981)) ;
#37050 = CARTESIAN_POINT('Ctrl Pts',(-18.2725029600721,26.556068133749,123.867014296754)) ;
#37051 = CARTESIAN_POINT('Ctrl Pts',(-17.9883141682821,26.3760790533392,123.98081722358)) ;
#37052 = CARTESIAN_POINT('Ctrl Pts',(-18.1854325985899,26.5761073273527,123.449960855483)) ;
#37053 = CARTESIAN_POINT('Ctrl Pts',(-17.8794749234903,26.3961182469429,123.459500138787)) ;
#37054 = CARTESIAN_POINT('Ctrl Pts',(-18.2454084367871,26.5959472952634,123.032350538864)) ;
#37055 = CARTESIAN_POINT('Ctrl Pts',(-17.9544430375699,26.4159582148536,122.937489228137)) ;
#37056 = CARTESIAN_POINT('Ctrl Pts',(-18.4440381416904,26.6158621122275,122.658424632547)) ;
#37057 = CARTESIAN_POINT('Ctrl Pts',(-18.2027276436478,26.4358730318177,122.470081707815)) ;
#37058 = CARTESIAN_POINT('Ctrl Pts',(-18.75897849637,26.6358043576238,122.374552553596)) ;
#37059 = CARTESIAN_POINT('Ctrl Pts',(-18.5964009950836,26.455815277214,122.11524037907)) ;
#37060 = CARTESIAN_POINT('Ctrl Pts',(-19.1503485290493,26.6556764057383,122.215041816388)) ;
#37061 = CARTESIAN_POINT('Ctrl Pts',(-19.0856111707596,26.4756873253285,121.915849802036)) ;
#37062 = CARTESIAN_POINT('Ctrl Pts',(-19.5753925439647,26.6756874706924,122.198865355149)) ;
#37063 = CARTESIAN_POINT('Ctrl Pts',(-19.616916168293,26.4956983902826,121.895626311557)) ;
#37064 = CARTESIAN_POINT('Ctrl Pts',(-19.9769190829482,26.695498994996,122.326876472295)) ;
#37065 = CARTESIAN_POINT('Ctrl Pts',(-20.118823655728,26.5155099145862,122.055636433921)) ;
#37066 = CARTESIAN_POINT('Ctrl Pts',(-20.3149929284387,26.7155942069594,122.58789233349)) ;
#37067 = CARTESIAN_POINT('Ctrl Pts',(-20.5414187887215,26.5356051265496,122.381904092587)) ;
#37068 = CARTESIAN_POINT('Ctrl Pts',(-20.5402392709743,26.7353749308792,122.943283604957)) ;
#37069 = CARTESIAN_POINT('Ctrl Pts',(-20.8229786363096,26.5553858504693,122.826139617784)) ;
#37070 = CARTESIAN_POINT('Ctrl Pts',(-20.6325355714334,26.755366006522,123.358044401428)) ;
#37071 = CARTESIAN_POINT('Ctrl Pts',(-20.9383530389169,26.5753769261122,123.344589665561)) ;
#37072 = CARTESIAN_POINT('Ctrl Pts',(-20.5777323731222,26.775247945565,123.777341421288)) ;
#37073 = CARTESIAN_POINT('Ctrl Pts',(-20.8698532062962,26.5952588651552,123.868710610719)) ;
#37074 = CARTESIAN_POINT('Ctrl Pts',(-20.3829509016501,26.7952005500682,124.154152656679)) ;
#37075 = CARTESIAN_POINT('Ctrl Pts',(-20.6263804834171,26.6152114696584,124.339726432441)) ;
#37076 = CARTESIAN_POINT('Ctrl Pts',(-20.0720296957647,26.8150994187989,124.441175273159)) ;
#37077 = CARTESIAN_POINT('Ctrl Pts',(-20.237732360991,26.6351103383891,124.69850747848)) ;
#37078 = CARTESIAN_POINT('Ctrl Pts',(-19.682246570693,26.8349928186085,124.605258451714)) ;
#37079 = CARTESIAN_POINT('Ctrl Pts',(-19.7505063847468,26.6550037381987,124.90361609291)) ;
#37080 = CARTESIAN_POINT('Ctrl Pts',(-19.2594063736317,26.8549019494485,124.627157490124)) ;
#37081 = CARTESIAN_POINT('Ctrl Pts',(-19.2219548120754,26.6749128690387,124.930993209618)) ;
#37082 = CARTESIAN_POINT('Ctrl Pts',(-18.8522665349481,26.8749340492121,124.502164719981)) ;
#37083 = CARTESIAN_POINT('Ctrl Pts',(-18.7130356341948,26.6949449688022,124.774763267503)) ;
#37084 = CARTESIAN_POINT('Ctrl Pts',(-18.5715001351461,26.8914661223815,124.290581364288)) ;
#37085 = CARTESIAN_POINT('Ctrl Pts',(-18.362052855483,26.7114770419717,124.510268121251)) ;
#37086 = CARTESIAN_POINT('Ctrl Pts',(-18.3986933822299,26.9048014629875,124.069844703011)) ;
#37087 = CARTESIAN_POINT('Ctrl Pts',(-18.1460617746842,26.7248123825776,124.234367496559)) ;
#37088 = CARTESIAN_POINT('Ctrl Pts',(-18.3010328118348,26.9146440215272,123.887397849221)) ;
#37089 = CARTESIAN_POINT('Ctrl Pts',(-18.0239800546403,26.7346549411174,124.006303612816)) ;
#37090 = CARTESIAN_POINT('Ctrl Pts',(-18.234968179349,26.9246959283771,123.68668524791)) ;
#37091 = CARTESIAN_POINT('Ctrl Pts',(-17.9413973813145,26.7447068479673,123.755428033615)) ;
#37092 = CARTESIAN_POINT('Ctrl Pts',(-18.1952008801186,26.937944442768,123.411026766241)) ;
#37093 = CARTESIAN_POINT('Ctrl Pts',(-17.8916861491589,26.7579553623582,123.410787353361)) ;
#37094 = CARTESIAN_POINT('Ctrl Pts',(-18.2364062598888,26.9545436177157,123.060472721167)) ;
#37095 = CARTESIAN_POINT('Ctrl Pts',(-17.9431815126831,26.7745545373059,122.972680824435)) ;
#37096 = CARTESIAN_POINT('Ctrl Pts',(-18.3945264788303,26.9711324035108,122.745229733751)) ;
#37097 = CARTESIAN_POINT('Ctrl Pts',(-18.1408483241841,26.791143323101,122.578566000218)) ;
#37098 = CARTESIAN_POINT('Ctrl Pts',(-18.5797786495349,26.9844082198528,122.536429267407)) ;
#37099 = CARTESIAN_POINT('Ctrl Pts',(-18.37239268425,26.8044191394429,122.31759864417)) ;
#37100 = CARTESIAN_POINT('Ctrl Pts',(-18.7438802886562,26.9943820706466,122.405894110244)) ;
#37101 = CARTESIAN_POINT('Ctrl Pts',(-18.5775216542412,26.8143929902368,122.154420338584)) ;
#37102 = CARTESIAN_POINT('Ctrl Pts',(-18.929271898675,27.004411102739,122.305482739616)) ;
#37103 = CARTESIAN_POINT('Ctrl Pts',(-18.8092589677478,26.8244220223292,122.028905565385)) ;
#37104 = CARTESIAN_POINT('Ctrl Pts',(-19.1264590553554,27.0143012282409,122.239497823847)) ;
#37105 = CARTESIAN_POINT('Ctrl Pts',(-19.0557421895027,26.834312147831,121.946421302881)) ;
#37106 = CARTESIAN_POINT('Ctrl Pts',(-19.3341576766828,27.0242937065124,122.208161049022)) ;
#37107 = CARTESIAN_POINT('Ctrl Pts',(-19.3153650354492,26.8443046261026,121.907247691333)) ;
#37108 = CARTESIAN_POINT('Ctrl Pts',(-19.5433352481452,27.0342449216098,122.213230891029)) ;
#37109 = CARTESIAN_POINT('Ctrl Pts',(-19.5768371046755,26.8542558412,121.913582155123)) ;
#37110 = CARTESIAN_POINT('Ctrl Pts',(-19.7503716423327,27.0442934233648,122.255105192578)) ;
#37111 = CARTESIAN_POINT('Ctrl Pts',(-19.8356332457504,26.864304342955,121.965922317527)) ;
#37112 = CARTESIAN_POINT('Ctrl Pts',(-19.9430662208723,27.0541347729816,122.330491998155)) ;
#37113 = CARTESIAN_POINT('Ctrl Pts',(-20.0765024472535,26.8741456925718,122.060153189974)) ;
#37114 = CARTESIAN_POINT('Ctrl Pts',(-20.1225333341149,27.0641210640018,122.439364927213)) ;
#37115 = CARTESIAN_POINT('Ctrl Pts',(-20.300837872544,26.884131983592,122.196241979988)) ;
#37116 = CARTESIAN_POINT('Ctrl Pts',(-20.2797057557656,27.0740576757304,122.57702448676)) ;
#37117 = CARTESIAN_POINT('Ctrl Pts',(-20.4973053063257,26.8940685953206,122.368314358349)) ;
#37118 = CARTESIAN_POINT('Ctrl Pts',(-20.4119625359954,27.084107551098,122.74176172172)) ;
#37119 = CARTESIAN_POINT('Ctrl Pts',(-20.6626285188084,26.9041184706882,122.574234184179)) ;
#37120 = CARTESIAN_POINT('Ctrl Pts',(-20.5117431177263,27.0939580096334,122.92324291587)) ;
#37121 = CARTESIAN_POINT('Ctrl Pts',(-20.787356768741,26.9139689292236,122.801084418364)) ;
#37122 = CARTESIAN_POINT('Ctrl Pts',(-20.579826322129,27.1039299465862,123.121493753205)) ;
#37123 = CARTESIAN_POINT('Ctrl Pts',(-20.8724634669846,26.9239408661763,123.048897162367)) ;
#37124 = CARTESIAN_POINT('Ctrl Pts',(-20.6125055315077,27.1139254035183,123.329105646214)) ;
#37125 = CARTESIAN_POINT('Ctrl Pts',(-20.9133152578659,26.9339363231085,123.308411671267)) ;
#37126 = CARTESIAN_POINT('Ctrl Pts',(-20.6083877682446,27.1239582105714,123.539972730989)) ;
#37127 = CARTESIAN_POINT('Ctrl Pts',(-20.9081708679843,26.9439691301615,123.571995622516)) ;
#37128 = CARTESIAN_POINT('Ctrl Pts',(-20.5686916631752,27.1338180971613,123.743433100123)) ;
#37129 = CARTESIAN_POINT('Ctrl Pts',(-20.8585534427994,26.9538290167515,123.826321841981)) ;
#37130 = CARTESIAN_POINT('Ctrl Pts',(-20.4936737353725,27.1438071777266,123.939559222509)) ;
#37131 = CARTESIAN_POINT('Ctrl Pts',(-20.7647835916082,26.9638180973167,124.07148059007)) ;
#37132 = CARTESIAN_POINT('Ctrl Pts',(-20.3863494619409,27.1537386569357,124.118661541936)) ;
#37133 = CARTESIAN_POINT('Ctrl Pts',(-20.6306305350596,26.9737495765259,124.295360078416)) ;
#37134 = CARTESIAN_POINT('Ctrl Pts',(-20.2490645865285,27.1637245163817,124.277504970353)) ;
#37135 = CARTESIAN_POINT('Ctrl Pts',(-20.459026445873,26.9837354359718,124.493916247304)) ;
#37136 = CARTESIAN_POINT('Ctrl Pts',(-20.0852193557923,27.1737626670289,124.410486117788)) ;
#37137 = CARTESIAN_POINT('Ctrl Pts',(-20.2542216594621,26.993773586619,124.660144844875)) ;
#37138 = CARTESIAN_POINT('Ctrl Pts',(-19.9044415797665,27.1836107575333,124.511442323854)) ;
#37139 = CARTESIAN_POINT('Ctrl Pts',(-20.0282504284542,27.0036216771234,124.786342691805)) ;
#37140 = CARTESIAN_POINT('Ctrl Pts',(-19.7047523070118,27.1936716660512,124.581101591854)) ;
#37141 = CARTESIAN_POINT('Ctrl Pts',(-19.7786397745588,27.0136825856414,124.873419336905)) ;
#37142 = CARTESIAN_POINT('Ctrl Pts',(-19.4993833052846,27.2035665132092,124.614334962714)) ;
#37143 = CARTESIAN_POINT('Ctrl Pts',(-19.5219286374302,27.0235774327994,124.914963808384)) ;
#37144 = CARTESIAN_POINT('Ctrl Pts',(-19.2904166566976,27.2135081852543,124.611948250234)) ;
#37145 = CARTESIAN_POINT('Ctrl Pts',(-19.2607200330017,27.0335191048444,124.91198309145)) ;
#37146 = CARTESIAN_POINT('Ctrl Pts',(-19.0837134685083,27.2235107123797,124.573148992734)) ;
#37147 = CARTESIAN_POINT('Ctrl Pts',(-19.0023404745317,27.0435216319699,124.863486618842)) ;
#37148 = CARTESIAN_POINT('Ctrl Pts',(-18.886408762246,27.2335455035672,124.49851245076)) ;
#37149 = CARTESIAN_POINT('Ctrl Pts',(-18.755708647679,27.0535564231574,124.770193481256)) ;
#37150 = CARTESIAN_POINT('Ctrl Pts',(-18.7082920067272,27.2433903834263,124.393076161983)) ;
#37151 = CARTESIAN_POINT('Ctrl Pts',(-18.5330608652643,27.0634013030165,124.638400122034)) ;
#37152 = CARTESIAN_POINT('Ctrl Pts',(-18.548717036597,27.2533762640448,124.256715634161)) ;
#37153 = CARTESIAN_POINT('Ctrl Pts',(-18.3335903392145,27.073387183635,124.467951336742)) ;
#37154 = CARTESIAN_POINT('Ctrl Pts',(-18.415763782662,27.263310987138,124.095588178805)) ;
#37155 = CARTESIAN_POINT('Ctrl Pts',(-18.1673965821036,27.0833219067282,124.266543402292)) ;
#37156 = CARTESIAN_POINT('Ctrl Pts',(-18.3117355785266,27.2733688274492,123.911537425513)) ;
#37157 = CARTESIAN_POINT('Ctrl Pts',(-18.0373591120352,27.0933797470393,124.036481345852)) ;
#37158 = CARTESIAN_POINT('Ctrl Pts',(-18.2425753593927,27.2831893148457,123.716980331988)) ;
#37159 = CARTESIAN_POINT('Ctrl Pts',(-17.9509061763895,27.1032002344359,123.793285094088)) ;
#37160 = CARTESIAN_POINT('Ctrl Pts',(-18.2070714729757,27.2932497161908,123.508505960271)) ;
#37161 = CARTESIAN_POINT('Ctrl Pts',(-17.9065238900958,27.113260635781,123.532692664092)) ;
#37162 = CARTESIAN_POINT('Ctrl Pts',(-18.2085717097183,27.3031806817437,123.299707474007)) ;
#37163 = CARTESIAN_POINT('Ctrl Pts',(-17.9083966529468,27.1231916013339,123.271694164599)) ;
#37164 = CARTESIAN_POINT('Ctrl Pts',(-18.2458677394489,27.3131195440802,123.094139009505)) ;
#37165 = CARTESIAN_POINT('Ctrl Pts',(-17.955014348972,27.1331304636704,123.014732779551)) ;
#37166 = CARTESIAN_POINT('Ctrl Pts',(-18.3185162099704,27.3231052750064,122.897153471792)) ;
#37167 = CARTESIAN_POINT('Ctrl Pts',(-18.0458227293061,27.1431161945965,122.768499870835)) ;
#37168 = CARTESIAN_POINT('Ctrl Pts',(-18.4248467767158,27.3331296604338,122.715218646708)) ;
#37169 = CARTESIAN_POINT('Ctrl Pts',(-18.1787338061825,27.153140580024,122.541080100804)) ;
#37170 = CARTESIAN_POINT('Ctrl Pts',(-18.5592899800235,27.3430329447871,122.556213400873)) ;
#37171 = CARTESIAN_POINT('Ctrl Pts',(-18.3467863406114,27.1630438643772,122.342321572966)) ;
#37172 = CARTESIAN_POINT('Ctrl Pts',(-18.7218362744338,27.3530929493651,122.42094597078)) ;
#37173 = CARTESIAN_POINT('Ctrl Pts',(-18.5499675317569,27.1731038689552,122.173235543867)) ;
#37174 = CARTESIAN_POINT('Ctrl Pts',(-18.9014128659292,27.3629362184342,122.3180699415)) ;
#37175 = CARTESIAN_POINT('Ctrl Pts',(-18.7744378364705,27.1829471380244,122.044638016487)) ;
#37176 = CARTESIAN_POINT('Ctrl Pts',(-19.0988286897178,27.3729267840419,122.246443873207)) ;
#37177 = CARTESIAN_POINT('Ctrl Pts',(-19.0212070083679,27.192937703632,121.955103241805)) ;
#37178 = CARTESIAN_POINT('Ctrl Pts',(-19.3044292359815,27.3828549158207,122.210437107956)) ;
#37179 = CARTESIAN_POINT('Ctrl Pts',(-19.2782077784746,27.2028658354109,121.910092465448)) ;
#37180 = CARTESIAN_POINT('Ctrl Pts',(-19.5144154098307,27.3928428029016,122.21031147887)) ;
#37181 = CARTESIAN_POINT('Ctrl Pts',(-19.5406906769482,27.2128537224918,121.909933250566)) ;
#37182 = CARTESIAN_POINT('Ctrl Pts',(-19.7221490194526,27.4028787524703,122.247173181467)) ;
#37183 = CARTESIAN_POINT('Ctrl Pts',(-19.800358000924,27.2228896720605,121.956008126959)) ;
#37184 = CARTESIAN_POINT('Ctrl Pts',(-19.916892573696,27.4127336388491,122.317923368138)) ;
#37185 = CARTESIAN_POINT('Ctrl Pts',(-20.0437890491304,27.2327445584393,122.044444124132)) ;
#37186 = CARTESIAN_POINT('Ctrl Pts',(-20.0991236220355,27.422733053197,122.422656802109)) ;
#37187 = CARTESIAN_POINT('Ctrl Pts',(-20.2715790260857,27.2427439727872,122.17535915605)) ;
#37188 = CARTESIAN_POINT('Ctrl Pts',(-20.2589164113812,27.4326282183875,122.555908904654)) ;
#37189 = CARTESIAN_POINT('Ctrl Pts',(-20.4713218816854,27.2526391379776,122.341923187098)) ;
#37190 = CARTESIAN_POINT('Ctrl Pts',(-20.3953279566597,27.4426885370794,122.71750152297)) ;
#37191 = CARTESIAN_POINT('Ctrl Pts',(-20.641837725394,27.2626994566696,122.543912452702)) ;
#37192 = CARTESIAN_POINT('Ctrl Pts',(-20.4995174983559,27.4525386688555,122.896483303571)) ;
#37193 = CARTESIAN_POINT('Ctrl Pts',(-20.7720769169052,27.2725495884457,122.767639568981)) ;
#37194 = CARTESIAN_POINT('Ctrl Pts',(-20.5728149864719,27.4625692393058,123.094198738288)) ;
#37195 = CARTESIAN_POINT('Ctrl Pts',(-20.8637005069511,27.282580158896,123.014783157518)) ;
#37196 = CARTESIAN_POINT('Ctrl Pts',(-20.6101494969086,27.4725833899786,123.301402871192)) ;
#37197 = CARTESIAN_POINT('Ctrl Pts',(-20.9103706253092,27.2925943095687,123.273787983247)) ;
#37198 = CARTESIAN_POINT('Ctrl Pts',(-20.6112662653975,27.482476323524,123.509383815082)) ;
#37199 = CARTESIAN_POINT('Ctrl Pts',(-20.9117684959154,27.3024872431142,123.533764947739)) ;
#37200 = CARTESIAN_POINT('Ctrl Pts',(-20.5761521288518,27.4924658375142,123.716418000998)) ;
#37201 = CARTESIAN_POINT('Ctrl Pts',(-20.8678776030597,27.3124767571044,123.792558185281)) ;
#37202 = CARTESIAN_POINT('Ctrl Pts',(-20.5059891635455,27.5024196081667,123.913596204343)) ;
#37203 = CARTESIAN_POINT('Ctrl Pts',(-20.7801754400908,27.3224305277569,124.039031948383)) ;
#37204 = CARTESIAN_POINT('Ctrl Pts',(-20.4015400398466,27.5124673768272,124.097177756809)) ;
#37205 = CARTESIAN_POINT('Ctrl Pts',(-20.6496157400561,27.3324782964174,124.268509637685)) ;
#37206 = CARTESIAN_POINT('Ctrl Pts',(-20.2697294375057,27.522309103267,124.256684479157)) ;
#37207 = CARTESIAN_POINT('Ctrl Pts',(-20.4848531001097,27.3423200228572,124.467895083778)) ;
#37208 = CARTESIAN_POINT('Ctrl Pts',(-20.1102592973178,27.5322946200898,124.393158289807)) ;
#37209 = CARTESIAN_POINT('Ctrl Pts',(-20.2855162963156,27.35230553968,124.638488743921)) ;
#37210 = CARTESIAN_POINT('Ctrl Pts',(-19.9303364745535,27.5422339517853,124.499474121132)) ;
#37211 = CARTESIAN_POINT('Ctrl Pts',(-20.0606131128691,27.3622448713755,124.771385186878)) ;
#37212 = CARTESIAN_POINT('Ctrl Pts',(-19.7327382041188,27.5522737214829,124.573617862549)) ;
#37213 = CARTESIAN_POINT('Ctrl Pts',(-19.813615980086,27.3722846410731,124.864066326377)) ;
#37214 = CARTESIAN_POINT('Ctrl Pts',(-19.5283912957834,27.5621618827317,124.611847447798)) ;
#37215 = CARTESIAN_POINT('Ctrl Pts',(-19.5581817302903,27.3821728023218,124.91185503281)) ;
#37216 = CARTESIAN_POINT('Ctrl Pts',(-19.3184025008245,27.5721514372341,124.614431043553)) ;
#37217 = CARTESIAN_POINT('Ctrl Pts',(-19.2956955404855,27.3921623568242,124.915085978985)) ;
#37218 = CARTESIAN_POINT('Ctrl Pts',(-19.1118246407992,27.5821098517577,124.580462400769)) ;
#37219 = CARTESIAN_POINT('Ctrl Pts',(-19.0374725439627,27.4021207713479,124.872626590883)) ;
#37220 = CARTESIAN_POINT('Ctrl Pts',(-18.9152594132557,27.5920097645871,124.512023957247)) ;
#37221 = CARTESIAN_POINT('Ctrl Pts',(-18.7917647458392,27.4120206841773,124.787079499409)) ;
#37222 = CARTESIAN_POINT('Ctrl Pts',(-18.7309264013132,27.602056464237,124.408951439022)) ;
#37223 = CARTESIAN_POINT('Ctrl Pts',(-18.5613480077175,27.4220673838271,124.658240132798)) ;
#37224 = CARTESIAN_POINT('Ctrl Pts',(-18.5695583676357,27.6119563245426,124.277459812412)) ;
#37225 = CARTESIAN_POINT('Ctrl Pts',(-18.3596364545729,27.4319672441327,124.493876043485)) ;
#37226 = CARTESIAN_POINT('Ctrl Pts',(-18.4313772500186,27.622007728748,124.117627545932)) ;
#37227 = CARTESIAN_POINT('Ctrl Pts',(-18.1869092530332,27.4420186483382,124.294086730382)) ;
#37228 = CARTESIAN_POINT('Ctrl Pts',(-18.3247881894919,27.6318887656692,123.939292964072)) ;
#37229 = CARTESIAN_POINT('Ctrl Pts',(-18.0536713290619,27.4518996852594,124.071168267652)) ;
#37230 = CARTESIAN_POINT('Ctrl Pts',(-18.2496492643862,27.6418885978467,123.742988738701)) ;
#37231 = CARTESIAN_POINT('Ctrl Pts',(-17.959746551278,27.4618995174369,123.825788262649)) ;
#37232 = CARTESIAN_POINT('Ctrl Pts',(-18.2098807597813,27.6518066008316,123.538271728212)) ;
#37233 = CARTESIAN_POINT('Ctrl Pts',(-17.91003471053,27.4718175204217,123.569891459498)) ;
#37234 = CARTESIAN_POINT('Ctrl Pts',(-18.2062837040758,27.6618579067061,123.327027887074)) ;
#37235 = CARTESIAN_POINT('Ctrl Pts',(-17.9055372819879,27.4818688262963,123.305836914711)) ;
#37236 = CARTESIAN_POINT('Ctrl Pts',(-18.2385839581239,27.6717277300977,123.122017781039)) ;
#37237 = CARTESIAN_POINT('Ctrl Pts',(-17.9459117764605,27.4917386496878,123.049572996313)) ;
#37238 = CARTESIAN_POINT('Ctrl Pts',(-18.307368702007,27.681801896148,122.921759006394)) ;
#37239 = CARTESIAN_POINT('Ctrl Pts',(-18.0318915985175,27.5018128157382,122.799249602939)) ;
#37240 = CARTESIAN_POINT('Ctrl Pts',(-18.4071173488075,27.6916219802896,122.74095235675)) ;
#37241 = CARTESIAN_POINT('Ctrl Pts',(-18.156577349418,27.5116328998798,122.573239483778)) ;
#37242 = CARTESIAN_POINT('Ctrl Pts',(-18.5399396605626,27.7017007070255,122.575930572394)) ;
#37243 = CARTESIAN_POINT('Ctrl Pts',(-18.3226042807451,27.5217116266156,122.366962086678)) ;
#37244 = CARTESIAN_POINT('Ctrl Pts',(-18.6958321778564,27.711552287675,122.439501623981)) ;
#37245 = CARTESIAN_POINT('Ctrl Pts',(-18.5174703779917,27.5315632072652,122.196424414274)) ;
#37246 = CARTESIAN_POINT('Ctrl Pts',(-18.8768591143373,27.7216254159734,122.329686829936)) ;
#37247 = CARTESIAN_POINT('Ctrl Pts',(-18.7437532834389,27.5416363355635,122.05915550408)) ;
#37248 = CARTESIAN_POINT('Ctrl Pts',(-19.069748360102,27.7314678938648,122.254738925638)) ;
#37249 = CARTESIAN_POINT('Ctrl Pts',(-18.9848658829464,27.551478813455,121.96546939627)) ;
#37250 = CARTESIAN_POINT('Ctrl Pts',(-19.275402729767,27.7414485004629,122.213172865234)) ;
#37251 = CARTESIAN_POINT('Ctrl Pts',(-19.2419340497861,27.561459420053,121.913511275043)) ;
#37252 = CARTESIAN_POINT('Ctrl Pts',(-19.4859500150315,27.7514662094817,122.208323768403)) ;
#37253 = CARTESIAN_POINT('Ctrl Pts',(-19.50511813664,27.5714771290719,121.907449255044)) ;
#37254 = CARTESIAN_POINT('Ctrl Pts',(-19.6914845982736,27.7613523885191,122.23929217762)) ;
#37255 = CARTESIAN_POINT('Ctrl Pts',(-19.7620374996912,27.5813633081093,121.946159440235)) ;
#37256 = CARTESIAN_POINT('Ctrl Pts',(-19.8919086335487,27.7714100010914,122.306601119756)) ;
#37257 = CARTESIAN_POINT('Ctrl Pts',(-20.0125674014289,27.5914209206816,122.030295059211)) ;
#37258 = CARTESIAN_POINT('Ctrl Pts',(-20.0742918881656,27.7812863944636,122.405862590949)) ;
#37259 = CARTESIAN_POINT('Ctrl Pts',(-20.2405477178928,27.6012973140538,122.154372035047)) ;
#37260 = CARTESIAN_POINT('Ctrl Pts',(-20.2389323043103,27.791281422614,122.536416615308)) ;
#37261 = CARTESIAN_POINT('Ctrl Pts',(-20.4463485473528,27.6112923422042,122.31756446123)) ;
#37262 = CARTESIAN_POINT('Ctrl Pts',(-20.3785025030073,27.80130216946,122.694229664895)) ;
#37263 = CARTESIAN_POINT('Ctrl Pts',(-20.6208115760538,27.6213130890502,122.514830465303)) ;
#37264 = CARTESIAN_POINT('Ctrl Pts',(-20.4874494476852,27.8112042381264,122.871614573746)) ;
#37265 = CARTESIAN_POINT('Ctrl Pts',(-20.7569960330967,27.6312151577166,122.736562250917)) ;
#37266 = CARTESIAN_POINT('Ctrl Pts',(-20.5649160847513,27.8211949779461,123.066844849364)) ;
#37267 = CARTESIAN_POINT('Ctrl Pts',(-20.8538296012272,27.6412058975363,122.980600241096)) ;
#37268 = CARTESIAN_POINT('Ctrl Pts',(-20.6070370985664,27.8311581741564,123.272013328294)) ;
#37269 = CARTESIAN_POINT('Ctrl Pts',(-20.9064812124733,27.6511690937465,123.237061229653)) ;
#37270 = CARTESIAN_POINT('Ctrl Pts',(-20.6133758883929,27.8410623584565,123.480152818403)) ;
#37271 = CARTESIAN_POINT('Ctrl Pts',(-20.9144047818511,27.6610732780467,123.497236530686)) ;
#37272 = CARTESIAN_POINT('Ctrl Pts',(-20.5828360532262,27.8511228188474,123.689412748153)) ;
#37273 = CARTESIAN_POINT('Ctrl Pts',(-20.8762301627314,27.6711337384376,123.758811110932)) ;
#37274 = CARTESIAN_POINT('Ctrl Pts',(-20.5181122383662,27.8609633647182,123.885935058997)) ;
#37275 = CARTESIAN_POINT('Ctrl Pts',(-20.7953249519899,27.6809742843083,124.004465402218)) ;
#37276 = CARTESIAN_POINT('Ctrl Pts',(-20.4183061486459,27.8710255854299,124.072424108861)) ;
#37277 = CARTESIAN_POINT('Ctrl Pts',(-20.6705674371675,27.6910365050201,124.237576347418)) ;
#37278 = CARTESIAN_POINT('Ctrl Pts',(-20.2895881644942,27.8809227284465,124.235913842461)) ;
#37279 = CARTESIAN_POINT('Ctrl Pts',(-20.5096693379548,27.7009336480366,124.441939302663)) ;
#37280 = CARTESIAN_POINT('Ctrl Pts',(-20.1343799700791,27.8908539048637,124.375554329111)) ;
#37281 = CARTESIAN_POINT('Ctrl Pts',(-20.3156583736033,27.7108648244538,124.616490187183)) ;
#37282 = CARTESIAN_POINT('Ctrl Pts',(-19.9551790503614,27.9008961186423,124.487164722517)) ;
#37283 = CARTESIAN_POINT('Ctrl Pts',(-20.0916573040226,27.7209070382324,124.756002912792)) ;
#37284 = CARTESIAN_POINT('Ctrl Pts',(-19.762401523415,27.910782658845,124.564891732212)) ;
#37285 = CARTESIAN_POINT('Ctrl Pts',(-19.8506842942857,27.7307935784352,124.853161854155)) ;
#37286 = CARTESIAN_POINT('Ctrl Pts',(-19.5569511425706,27.9207762534504,124.608757066638)) ;
#37287 = CARTESIAN_POINT('Ctrl Pts',(-19.59387104564,27.7407871730406,124.907993194493)) ;
#37288 = CARTESIAN_POINT('Ctrl Pts',(-19.3480204997779,27.930720128608,124.616215006894)) ;
#37289 = CARTESIAN_POINT('Ctrl Pts',(-19.3327071093506,27.7507310481981,124.917315275417)) ;
#37290 = CARTESIAN_POINT('Ctrl Pts',(-19.1406090152874,27.9406806647228,124.587509478741)) ;
#37291 = CARTESIAN_POINT('Ctrl Pts',(-19.0734423500344,27.760691584313,124.881432829673)) ;
#37292 = CARTESIAN_POINT('Ctrl Pts',(-18.9405381225761,27.9506772680455,124.523103824295)) ;
#37293 = CARTESIAN_POINT('Ctrl Pts',(-18.8233537498005,27.7706881876357,124.800925220458)) ;
#37294 = CARTESIAN_POINT('Ctrl Pts',(-18.7541744874109,27.960710351,124.424327030337)) ;
#37295 = CARTESIAN_POINT('Ctrl Pts',(-18.590399518169,27.7807212705902,124.677453935448)) ;
#37296 = CARTESIAN_POINT('Ctrl Pts',(-18.5906478671095,27.9705615197016,124.297248746626)) ;
#37297 = CARTESIAN_POINT('Ctrl Pts',(-18.3859904695605,27.7905724392918,124.518604840419)) ;
#37298 = CARTESIAN_POINT('Ctrl Pts',(-18.4496441002172,27.9805240104005,124.142390521308)) ;
#37299 = CARTESIAN_POINT('Ctrl Pts',(-18.2097360022232,27.8005349299906,124.325031213383)) ;
#37300 = CARTESIAN_POINT('Ctrl Pts',(-18.3371397750335,27.9905524388182,123.964073852674)) ;
#37301 = CARTESIAN_POINT('Ctrl Pts',(-18.0691061955959,27.8105633584084,124.102135115814)) ;
#37302 = CARTESIAN_POINT('Ctrl Pts',(-18.2581916508595,28.0004628061828,123.771274447575)) ;
#37303 = CARTESIAN_POINT('Ctrl Pts',(-17.970421329577,27.8204737257729,123.861134793035)) ;
#37304 = CARTESIAN_POINT('Ctrl Pts',(-18.2132715984884,28.0103976737979,123.567293786419)) ;
#37305 = CARTESIAN_POINT('Ctrl Pts',(-17.9142719851426,27.8304085933881,123.606158130972)) ;
#37306 = CARTESIAN_POINT('Ctrl Pts',(-18.2045541391692,28.0204388157769,123.356384171661)) ;
#37307 = CARTESIAN_POINT('Ctrl Pts',(-17.9033759752312,27.8404497353671,123.342521266575)) ;
#37308 = CARTESIAN_POINT('Ctrl Pts',(-18.2320173963766,28.0303259519801,123.150336225817)) ;
#37309 = CARTESIAN_POINT('Ctrl Pts',(-17.9377060395353,27.8503368715702,123.084960416977)) ;
#37310 = CARTESIAN_POINT('Ctrl Pts',(-18.2951662826154,28.0403182343835,122.949998669832)) ;
#37311 = CARTESIAN_POINT('Ctrl Pts',(-18.0166431581051,27.8603291539736,122.834538577191)) ;
#37312 = CARTESIAN_POINT('Ctrl Pts',(-18.3917805672602,28.0502667623487,122.764488512371)) ;
#37313 = CARTESIAN_POINT('Ctrl Pts',(-18.1374121264596,27.8702776819389,122.602650848171)) ;
#37314 = CARTESIAN_POINT('Ctrl Pts',(-18.5187344195011,28.0602034935108,122.598611319051)) ;
#37315 = CARTESIAN_POINT('Ctrl Pts',(-18.2961056898264,27.880214413101,122.395304507896)) ;
#37316 = CARTESIAN_POINT('Ctrl Pts',(-18.6731352153546,28.0701867043708,122.456413854557)) ;
#37317 = CARTESIAN_POINT('Ctrl Pts',(-18.4891076721337,27.890197623961,122.217558370884)) ;
#37318 = CARTESIAN_POINT('Ctrl Pts',(-18.8511053323271,28.0802298035207,122.342850389306)) ;
#37319 = CARTESIAN_POINT('Ctrl Pts',(-18.7115707176788,27.9002407231109,122.075605016145)) ;
#37320 = CARTESIAN_POINT('Ctrl Pts',(-19.0418370727349,28.0900607677956,122.26317827219)) ;
#37321 = CARTESIAN_POINT('Ctrl Pts',(-18.9499871891005,27.9100716873857,121.97601543362)) ;
#37322 = CARTESIAN_POINT('Ctrl Pts',(-19.2483766387023,28.1001336201815,122.216578929442)) ;
#37323 = CARTESIAN_POINT('Ctrl Pts',(-19.2081615249789,27.9201445397717,121.917767583911)) ;
#37324 = CARTESIAN_POINT('Ctrl Pts',(-19.4555437861215,28.1099977478933,122.206790899523)) ;
#37325 = CARTESIAN_POINT('Ctrl Pts',(-19.4671216625215,27.9300086674835,121.905533740813)) ;
#37326 = CARTESIAN_POINT('Ctrl Pts',(-19.6645948451265,28.1200199500282,122.233024086339)) ;
#37327 = CARTESIAN_POINT('Ctrl Pts',(-19.7284352632349,27.9400308696183,121.938326646728)) ;
#37328 = CARTESIAN_POINT('Ctrl Pts',(-19.8658877748029,28.1300471429966,122.295670934239)) ;
#37329 = CARTESIAN_POINT('Ctrl Pts',(-19.9800509846578,27.9500580625868,122.016636385293)) ;
#37330 = CARTESIAN_POINT('Ctrl Pts',(-20.0501626714237,28.1399027369636,122.39036087509)) ;
#37331 = CARTESIAN_POINT('Ctrl Pts',(-20.2103950643884,27.9599136565538,122.135000592718)) ;
#37332 = CARTESIAN_POINT('Ctrl Pts',(-20.2172929353047,28.1498599088289,122.516416762394)) ;
#37333 = CARTESIAN_POINT('Ctrl Pts',(-20.4193072749355,27.9698708284191,122.292571980772)) ;
#37334 = CARTESIAN_POINT('Ctrl Pts',(-20.36088775291,28.1598987528273,122.67106650366)) ;
#37335 = CARTESIAN_POINT('Ctrl Pts',(-20.5987996284772,27.9799096724175,122.485885053501)) ;
#37336 = CARTESIAN_POINT('Ctrl Pts',(-20.4738977645388,28.1697727767028,122.845224021032)) ;
#37337 = CARTESIAN_POINT('Ctrl Pts',(-20.7400613605659,27.989783696293,122.703583668391)) ;
#37338 = CARTESIAN_POINT('Ctrl Pts',(-20.5565305050554,28.1798426026932,123.040098786974)) ;
#37339 = CARTESIAN_POINT('Ctrl Pts',(-20.8433506854112,27.9998535222834,122.947177423927)) ;
#37340 = CARTESIAN_POINT('Ctrl Pts',(-20.603072347858,28.1896758465905,123.241534739974)) ;
#37341 = CARTESIAN_POINT('Ctrl Pts',(-20.9015266941118,28.0096867661807,123.198973980938)) ;
#37342 = CARTESIAN_POINT('Ctrl Pts',(-20.614743890259,28.1997062743635,123.452075818359)) ;
#37343 = CARTESIAN_POINT('Ctrl Pts',(-20.9161142995168,28.0197171939537,123.462150342136)) ;
#37344 = CARTESIAN_POINT('Ctrl Pts',(-20.5890670250738,28.2097378911087,123.661414868918)) ;
#37345 = CARTESIAN_POINT('Ctrl Pts',(-20.8840166201803,28.0297488106989,123.723823875487)) ;
#37346 = CARTESIAN_POINT('Ctrl Pts',(-20.5290926772713,28.2195675680894,123.859156375962)) ;
#37347 = CARTESIAN_POINT('Ctrl Pts',(-20.8090466299331,28.0395784876796,123.971001465178)) ;
#37348 = CARTESIAN_POINT('Ctrl Pts',(-20.4347263329766,28.2295570849293,124.046779224324)) ;
#37349 = CARTESIAN_POINT('Ctrl Pts',(-20.6910868707223,28.0495680045195,124.205529304488)) ;
#37350 = CARTESIAN_POINT('Ctrl Pts',(-20.308112533224,28.2396006970691,124.215750588149)) ;
#37351 = CARTESIAN_POINT('Ctrl Pts',(-20.5328182780255,28.0596116166593,124.416742316219)) ;
#37352 = CARTESIAN_POINT('Ctrl Pts',(-20.1577648900733,28.2494233034044,124.357312030463)) ;
#37353 = CARTESIAN_POINT('Ctrl Pts',(-20.3448814895042,28.0694342229946,124.593693576186)) ;
#37354 = CARTESIAN_POINT('Ctrl Pts',(-19.9816030750299,28.2594615333036,124.473500882314)) ;
#37355 = CARTESIAN_POINT('Ctrl Pts',(-20.1246781855413,28.0794724528938,124.738927845649)) ;
#37356 = CARTESIAN_POINT('Ctrl Pts',(-19.7882531660864,28.2694725680956,124.556669707045)) ;
#37357 = CARTESIAN_POINT('Ctrl Pts',(-19.8829899980737,28.0894834876857,124.84288713183)) ;
#37358 = CARTESIAN_POINT('Ctrl Pts',(-19.5858129110288,28.2793702990627,124.604775415822)) ;
#37359 = CARTESIAN_POINT('Ctrl Pts',(-19.629938496845,28.0993812186529,124.903017472002)) ;
#37360 = CARTESIAN_POINT('Ctrl Pts',(-19.376180880844,28.2893599269132,124.617388122946)) ;
#37361 = CARTESIAN_POINT('Ctrl Pts',(-19.3678981582477,28.1093708465034,124.9187812748)) ;
#37362 = CARTESIAN_POINT('Ctrl Pts',(-19.1682588404928,28.2993157173592,124.593418733339)) ;
#37363 = CARTESIAN_POINT('Ctrl Pts',(-19.1079954571201,28.1193266369494,124.88881743189)) ;
#37364 = CARTESIAN_POINT('Ctrl Pts',(-18.96810534998,28.3092431159212,124.534261318973)) ;
#37365 = CARTESIAN_POINT('Ctrl Pts',(-18.8578037171017,28.1292540355114,124.814868421529)) ;
#37366 = CARTESIAN_POINT('Ctrl Pts',(-18.7794564522439,28.3192687110311,124.440280835038)) ;
#37367 = CARTESIAN_POINT('Ctrl Pts',(-18.6219935808198,28.1392796306213,124.697390886219)) ;
#37368 = CARTESIAN_POINT('Ctrl Pts',(-18.6122710106145,28.3291545617007,124.31681671948)) ;
#37369 = CARTESIAN_POINT('Ctrl Pts',(-18.413012494955,28.1491654812909,124.543058534204)) ;
#37370 = CARTESIAN_POINT('Ctrl Pts',(-18.4672022044828,28.3391437415449,124.164964313106)) ;
#37371 = CARTESIAN_POINT('Ctrl Pts',(-18.2316780605687,28.1591546611351,124.353241304925)) ;
#37372 = CARTESIAN_POINT('Ctrl Pts',(-18.350468282265,28.3491849286484,123.98908060691)) ;
#37373 = CARTESIAN_POINT('Ctrl Pts',(-18.08576255543,28.1691958482386,124.133385523798)) ;
#37374 = CARTESIAN_POINT('Ctrl Pts',(-18.267489993905,28.3590175721244,123.799757295272)) ;
#37375 = CARTESIAN_POINT('Ctrl Pts',(-17.9820414176023,28.1790284917146,123.896729581329)) ;
#37376 = CARTESIAN_POINT('Ctrl Pts',(-18.2172586034104,28.3690115218339,123.595747330936)) ;
#37377 = CARTESIAN_POINT('Ctrl Pts',(-17.9192545217084,28.1890224414241,123.64171642404)) ;
#37378 = CARTESIAN_POINT('Ctrl Pts',(-18.2036074114145,28.3790406446104,123.385343767415)) ;
#37379 = CARTESIAN_POINT('Ctrl Pts',(-17.9021928664075,28.1990515642006,123.378711840275)) ;
#37380 = CARTESIAN_POINT('Ctrl Pts',(-18.2260142937554,28.3889167755291,123.178918899559)) ;
#37381 = CARTESIAN_POINT('Ctrl Pts',(-17.9302039421449,28.2089276951193,123.120680343529)) ;
#37382 = CARTESIAN_POINT('Ctrl Pts',(-18.2843913723889,28.3989148105461,122.977024252762)) ;
#37383 = CARTESIAN_POINT('Ctrl Pts',(-18.003177692541,28.2189257301363,122.868312611981)) ;
#37384 = CARTESIAN_POINT('Ctrl Pts',(-18.3760366799018,28.4088287403048,122.789803762381)) ;
#37385 = CARTESIAN_POINT('Ctrl Pts',(-18.1177367767747,28.228839659895,122.634287677153)) ;
#37386 = CARTESIAN_POINT('Ctrl Pts',(-18.500337734295,28.4188719280426,122.619151689602)) ;
#37387 = CARTESIAN_POINT('Ctrl Pts',(-18.2731150794014,28.2388828476328,122.420974122338)) ;
#37388 = CARTESIAN_POINT('Ctrl Pts',(-18.6502217855382,28.428771770183,122.474737172695)) ;
#37389 = CARTESIAN_POINT('Ctrl Pts',(-18.460472242702,28.2487826897731,122.240457435549)) ;
#37390 = CARTESIAN_POINT('Ctrl Pts',(-18.8242413063613,28.438763036991,122.357101788211)) ;
#37391 = CARTESIAN_POINT('Ctrl Pts',(-18.6779981948362,28.2587739565812,122.093415286222)) ;
#37392 = CARTESIAN_POINT('Ctrl Pts',(-19.0169763775656,28.4487951391229,122.271451770785)) ;
#37393 = CARTESIAN_POINT('Ctrl Pts',(-18.9189180448154,28.2688060587131,121.986355077161)) ;
#37394 = CARTESIAN_POINT('Ctrl Pts',(-19.2182110681717,28.4586620200777,122.221141613254)) ;
#37395 = CARTESIAN_POINT('Ctrl Pts',(-19.170462608238,28.2786729396679,121.923469734466)) ;
#37396 = CARTESIAN_POINT('Ctrl Pts',(-19.4277169110003,28.4686538113658,122.205851400272)) ;
#37397 = CARTESIAN_POINT('Ctrl Pts',(-19.4323452132242,28.288664730956,121.904359612278)) ;
#37398 = CARTESIAN_POINT('Ctrl Pts',(-19.6374921877922,28.4786859272774,122.227662227062)) ;
#37399 = CARTESIAN_POINT('Ctrl Pts',(-19.6945640397909,28.2986968468675,121.931625723093)) ;
#37400 = CARTESIAN_POINT('Ctrl Pts',(-19.8370378148064,28.4885522440774,122.284307432454)) ;
#37401 = CARTESIAN_POINT('Ctrl Pts',(-19.9439958523289,28.3085631636676,122.002434913223)) ;
#37402 = CARTESIAN_POINT('Ctrl Pts',(-20.0261278855234,28.498539725551,122.375526578932)) ;
#37403 = CARTESIAN_POINT('Ctrl Pts',(-20.1803573810045,28.3185506451412,122.116461326089)) ;
#37404 = CARTESIAN_POINT('Ctrl Pts',(-20.1958916606712,28.5084846499299,122.497612228053)) ;
#37405 = CARTESIAN_POINT('Ctrl Pts',(-20.3925607131748,28.3284955695201,122.269070719358)) ;
#37406 = CARTESIAN_POINT('Ctrl Pts',(-20.3432261236584,28.5185295358406,122.64887127178)) ;
#37407 = CARTESIAN_POINT('Ctrl Pts',(-20.5767268497532,28.3385404554308,122.458146387044)) ;
#37408 = CARTESIAN_POINT('Ctrl Pts',(-20.4600658639641,28.5283916395532,122.820164450749)) ;
#37409 = CARTESIAN_POINT('Ctrl Pts',(-20.7227745276949,28.3484025591434,122.672264744805)) ;
#37410 = CARTESIAN_POINT('Ctrl Pts',(-20.546882409536,28.5383832033776,123.011421338606)) ;
#37411 = CARTESIAN_POINT('Ctrl Pts',(-20.831292734905,28.3583941229678,122.911337082872)) ;
#37412 = CARTESIAN_POINT('Ctrl Pts',(-20.5987837541194,28.5483160114405,123.213686812683)) ;
#37413 = CARTESIAN_POINT('Ctrl Pts',(-20.8961668072617,28.3683269310307,123.164169825485)) ;
#37414 = CARTESIAN_POINT('Ctrl Pts',(-20.6152968104347,28.5582531136769,123.42195527368)) ;
#37415 = CARTESIAN_POINT('Ctrl Pts',(-20.9168053567252,28.3782640332671,123.424505796562)) ;
#37416 = CARTESIAN_POINT('Ctrl Pts',(-20.5948899082448,28.5683055599473,123.632285532663)) ;
#37417 = CARTESIAN_POINT('Ctrl Pts',(-20.891293966489,28.3883164795374,123.687418366496)) ;
#37418 = CARTESIAN_POINT('Ctrl Pts',(-20.5397117951602,28.5781516755289,123.831810652888)) ;
#37419 = CARTESIAN_POINT('Ctrl Pts',(-20.8223185569901,28.3981625951191,123.936824298413)) ;
#37420 = CARTESIAN_POINT('Ctrl Pts',(-20.4492135047243,28.5881996952438,124.022668210418)) ;
#37421 = CARTESIAN_POINT('Ctrl Pts',(-20.7091931472438,28.4082106148339,124.175395051992)) ;
#37422 = CARTESIAN_POINT('Ctrl Pts',(-20.3279884165152,28.5981416468727,124.192947955947)) ;
#37423 = CARTESIAN_POINT('Ctrl Pts',(-20.5576594224477,28.4181525664629,124.388243230792)) ;
#37424 = CARTESIAN_POINT('Ctrl Pts',(-20.1794561705445,28.6080804278718,124.339907298682)) ;
#37425 = CARTESIAN_POINT('Ctrl Pts',(-20.3719920554708,28.428091347462,124.571940487543)) ;
#37426 = CARTESIAN_POINT('Ctrl Pts',(-20.0060768723233,28.6181064765979,124.459748019633)) ;
#37427 = CARTESIAN_POINT('Ctrl Pts',(-20.1552662552199,28.438117396188,124.72173910567)) ;
#37428 = CARTESIAN_POINT('Ctrl Pts',(-19.8172567237363,28.6279933370061,124.546699844584)) ;
#37429 = CARTESIAN_POINT('Ctrl Pts',(-19.9192398618571,28.4480042565963,124.830426395239)) ;
#37430 = CARTESIAN_POINT('Ctrl Pts',(-19.6133539599856,28.6380246121379,124.600393761194)) ;
#37431 = CARTESIAN_POINT('Ctrl Pts',(-19.6643603212946,28.4580355317281,124.897541006025)) ;
#37432 = CARTESIAN_POINT('Ctrl Pts',(-19.4062711547036,28.6479075894383,124.617827169365)) ;
#37433 = CARTESIAN_POINT('Ctrl Pts',(-19.4055076350618,28.4679185090285,124.919330220235)) ;
#37434 = CARTESIAN_POINT('Ctrl Pts',(-19.1957631832706,28.6579644428455,124.598722627596)) ;
#37435 = CARTESIAN_POINT('Ctrl Pts',(-19.1423686472361,28.4779753624356,124.895445755613)) ;
#37436 = CARTESIAN_POINT('Ctrl Pts',(-18.9283731228152,28.6711326839214,124.526630695589)) ;
#37437 = CARTESIAN_POINT('Ctrl Pts',(-18.8081529113216,28.4911436035116,124.805332008943)) ;
#37438 = CARTESIAN_POINT('Ctrl Pts',(-18.6817983350219,28.6845337131479,124.384021538888)) ;
#37439 = CARTESIAN_POINT('Ctrl Pts',(-18.4999549681537,28.5045446327381,124.627092881271)) ;
#37440 = CARTESIAN_POINT('Ctrl Pts',(-18.4857344421306,28.6977466298788,124.187192207811)) ;
#37441 = CARTESIAN_POINT('Ctrl Pts',(-18.254834612915,28.5177575494689,124.381018273115)) ;
#37442 = CARTESIAN_POINT('Ctrl Pts',(-18.3657858162467,28.707675024332,124.016416499208)) ;
#37443 = CARTESIAN_POINT('Ctrl Pts',(-18.1049098191361,28.5276859439222,124.16755417654)) ;
#37444 = CARTESIAN_POINT('Ctrl Pts',(-18.2766712212058,28.7176565244601,123.826404589139)) ;
#37445 = CARTESIAN_POINT('Ctrl Pts',(-17.9935167508853,28.5376674440503,123.930036177119)) ;
#37446 = CARTESIAN_POINT('Ctrl Pts',(-18.2218707889986,28.7276970677302,123.622569483315)) ;
#37447 = CARTESIAN_POINT('Ctrl Pts',(-17.9250194852318,28.5477079873204,123.675241990124)) ;
#37448 = CARTESIAN_POINT('Ctrl Pts',(-18.2033757282844,28.7375463995133,123.416330418717)) ;
#37449 = CARTESIAN_POINT('Ctrl Pts',(-17.9019033242147,28.5575573191035,123.417442838969)) ;
#37450 = CARTESIAN_POINT('Ctrl Pts',(-18.2206940069242,28.747541803985,123.206912125949)) ;
#37451 = CARTESIAN_POINT('Ctrl Pts',(-17.9235537435517,28.5675527235752,123.155670875164)) ;
#37452 = CARTESIAN_POINT('Ctrl Pts',(-18.2745872662887,28.7575581314336,123.003350839589)) ;
#37453 = CARTESIAN_POINT('Ctrl Pts',(-17.990923682681,28.5775690510238,122.901217359039)) ;
#37454 = CARTESIAN_POINT('Ctrl Pts',(-18.3909335432918,28.7707817886001,122.750824717369)) ;
#37455 = CARTESIAN_POINT('Ctrl Pts',(-18.1363563321202,28.5907927081903,122.585573837996)) ;
#37456 = CARTESIAN_POINT('Ctrl Pts',(-18.5712652888683,28.7840760799895,122.533196711622)) ;
#37457 = CARTESIAN_POINT('Ctrl Pts',(-18.3617388881424,28.6040869995797,122.313564150159)) ;
#37458 = CARTESIAN_POINT('Ctrl Pts',(-18.799057046922,28.797360430921,122.371600064136)) ;
#37459 = CARTESIAN_POINT('Ctrl Pts',(-18.6465253994533,28.6173713505112,122.11153161396)) ;
#37460 = CARTESIAN_POINT('Ctrl Pts',(-18.9884277129976,28.8073328119828,122.281692967666)) ;
#37461 = CARTESIAN_POINT('Ctrl Pts',(-18.8832307222532,28.6273437315729,121.999158080015)) ;
#37462 = CARTESIAN_POINT('Ctrl Pts',(-19.1891836686621,28.8172411916084,122.226029840972)) ;
#37463 = CARTESIAN_POINT('Ctrl Pts',(-19.134178804972,28.6372521111986,121.929579826064)) ;
#37464 = CARTESIAN_POINT('Ctrl Pts',(-19.3995659070131,28.8272951903564,122.205875393867)) ;
#37465 = CARTESIAN_POINT('Ctrl Pts',(-19.3971551455216,28.6473061099466,121.904389073362)) ;
#37466 = CARTESIAN_POINT('Ctrl Pts',(-19.6062836932465,28.8371573874727,122.222079550303)) ;
#37467 = CARTESIAN_POINT('Ctrl Pts',(-19.6555567772923,28.6571683070629,121.924649710888)) ;
#37468 = CARTESIAN_POINT('Ctrl Pts',(-19.8780826757267,28.8505045138469,122.29182043757)) ;
#37469 = CARTESIAN_POINT('Ctrl Pts',(-19.995279830665,28.6705154334371,122.01181375835)) ;
#37470 = CARTESIAN_POINT('Ctrl Pts',(-20.1845000475927,28.8670414794883,122.464288153073)) ;
#37471 = CARTESIAN_POINT('Ctrl Pts',(-20.3783371558537,28.6870523990785,122.227433847965)) ;
#37472 = CARTESIAN_POINT('Ctrl Pts',(-20.4154369591003,28.8836760836622,122.732174044355)) ;
#37473 = CARTESIAN_POINT('Ctrl Pts',(-20.6669572706625,28.7036870032524,122.562229846331)) ;
#37474 = CARTESIAN_POINT('Ctrl Pts',(-20.5367399369156,28.8969658769049,122.98386445411)) ;
#37475 = CARTESIAN_POINT('Ctrl Pts',(-20.8186195037405,28.7169767964951,122.876897221758)) ;
#37476 = CARTESIAN_POINT('Ctrl Pts',(-20.5937434976173,28.9069185081643,123.1851719771)) ;
#37477 = CARTESIAN_POINT('Ctrl Pts',(-20.8898646072513,28.7269294277544,123.128520520416)) ;
#37478 = CARTESIAN_POINT('Ctrl Pts',(-20.6151704596498,28.916870475469,123.393312690541)) ;
#37479 = CARTESIAN_POINT('Ctrl Pts',(-20.9166469900547,28.7368813950591,123.388702342931)) ;
#37480 = CARTESIAN_POINT('Ctrl Pts',(-20.5948058201253,28.9302377339328,123.673577606172)) ;
#37481 = CARTESIAN_POINT('Ctrl Pts',(-20.8911927394043,28.750248653523,123.739016958584)) ;
#37482 = CARTESIAN_POINT('Ctrl Pts',(-20.4800520817175,28.9467545458819,124.005580786161)) ;
#37483 = CARTESIAN_POINT('Ctrl Pts',(-20.7477418811131,28.7667654654721,124.154036877194)) ;
#37484 = CARTESIAN_POINT('Ctrl Pts',(-20.2120144615373,28.9667804408883,124.336293100921)) ;
#37485 = CARTESIAN_POINT('Ctrl Pts',(-20.4126932065167,28.7867913604785,124.567418944553)) ;
#37486 = CARTESIAN_POINT('Ctrl Pts',(-19.8510301281953,28.9865911710184,124.553536596618)) ;
#37487 = CARTESIAN_POINT('Ctrl Pts',(-19.9614615275736,28.8066020906086,124.838970603428)) ;
#37488 = CARTESIAN_POINT('Ctrl Pts',(-19.4344012108349,29.0065683871483,124.636109825588)) ;
#37489 = CARTESIAN_POINT('Ctrl Pts',(-19.4406750274581,28.8265793067385,124.942183198425)) ;
#37490 = CARTESIAN_POINT('Ctrl Pts',(-19.0157681070412,29.0264952625436,124.57095034557)) ;
#37491 = CARTESIAN_POINT('Ctrl Pts',(-18.9173848458193,28.8465061821338,124.860730356199)) ;
#37492 = CARTESIAN_POINT('Ctrl Pts',(-18.6457374117665,29.0463167240198,124.369076668043)) ;
#37493 = CARTESIAN_POINT('Ctrl Pts',(-18.4548495375607,28.86632764361,124.608386573035)) ;
#37494 = CARTESIAN_POINT('Ctrl Pts',(-18.3635430708779,29.0663910418292,124.048922971134)) ;
#37495 = CARTESIAN_POINT('Ctrl Pts',(-18.1021082198749,28.8864019614194,124.208191902882)) ;
#37496 = CARTESIAN_POINT('Ctrl Pts',(-18.2096162661091,29.0862390108371,123.655849066001)) ;
#37497 = CARTESIAN_POINT('Ctrl Pts',(-17.9097030413974,28.9062499304272,123.716849978501)) ;
#37498 = CARTESIAN_POINT('Ctrl Pts',(-18.1981447189495,29.1061860449003,123.231968651957)) ;
#37499 = CARTESIAN_POINT('Ctrl Pts',(-17.8953659111602,28.9261969644905,123.187000088167)) ;
#37500 = CARTESIAN_POINT('Ctrl Pts',(-18.3318077694759,29.1260819958724,122.830562780161)) ;
#37501 = CARTESIAN_POINT('Ctrl Pts',(-18.0624463344444,28.9460929154626,122.685244684146)) ;
#37502 = CARTESIAN_POINT('Ctrl Pts',(-18.5938358537856,29.1459774754907,122.498483434728)) ;
#37503 = CARTESIAN_POINT('Ctrl Pts',(-18.3899816867549,28.9659883950809,122.270147568278)) ;
#37504 = CARTESIAN_POINT('Ctrl Pts',(-18.9545509966917,29.1659335864555,122.274963150452)) ;
#37505 = CARTESIAN_POINT('Ctrl Pts',(-18.8408757371955,28.9859445060457,121.99074852876)) ;
#37506 = CARTESIAN_POINT('Ctrl Pts',(-19.3687523473574,29.1858381344955,122.188317116435)) ;
#37507 = CARTESIAN_POINT('Ctrl Pts',(-19.3586261760536,29.0058490540857,121.882442313801)) ;
#37508 = CARTESIAN_POINT('Ctrl Pts',(-19.7873033294093,29.2057122588146,122.247090838418)) ;
#37509 = CARTESIAN_POINT('Ctrl Pts',(-19.8818129365683,29.0257231784047,121.955909174204)) ;
#37510 = CARTESIAN_POINT('Ctrl Pts',(-20.1636458920224,29.2257667888136,122.447434307739)) ;
#37511 = CARTESIAN_POINT('Ctrl Pts',(-20.352241834532,29.0457777084038,122.206339109626)) ;
#37512 = CARTESIAN_POINT('Ctrl Pts',(-20.4457143490153,29.2455743025736,122.760308780651)) ;
#37513 = CARTESIAN_POINT('Ctrl Pts',(-20.7048254925802,29.0655852221637,122.59742983607)) ;
#37514 = CARTESIAN_POINT('Ctrl Pts',(-20.6062625022629,29.2655576583413,123.153645694702)) ;
#37515 = CARTESIAN_POINT('Ctrl Pts',(-20.9055115950316,29.0855685779315,123.089100356968)) ;
#37516 = CARTESIAN_POINT('Ctrl Pts',(-20.6222571826096,29.2854759609252,123.57685578804)) ;
#37517 = CARTESIAN_POINT('Ctrl Pts',(-20.9255057422974,29.1054868805154,123.618111697488)) ;
#37518 = CARTESIAN_POINT('Ctrl Pts',(-20.4942524999631,29.305344176371,123.97953847386)) ;
#37519 = CARTESIAN_POINT('Ctrl Pts',(-20.7655021762752,29.1253550959612,124.121463964398)) ;
#37520 = CARTESIAN_POINT('Ctrl Pts',(-20.2337505644514,29.3253944931673,124.316857983923)) ;
#37521 = CARTESIAN_POINT('Ctrl Pts',(-20.4398756731865,29.1454054127574,124.543114839658)) ;
#37522 = CARTESIAN_POINT('Ctrl Pts',(-19.8787560188095,29.3451705550497,124.542547094781)) ;
#37523 = CARTESIAN_POINT('Ctrl Pts',(-19.9961359923374,29.1651814746399,124.825226575643)) ;
#37524 = CARTESIAN_POINT('Ctrl Pts',(-19.4626770517434,29.3652251607422,124.635063105545)) ;
#37525 = CARTESIAN_POINT('Ctrl Pts',(-19.4760372478576,29.1852360803324,124.940874254979)) ;
#37526 = CARTESIAN_POINT('Ctrl Pts',(-19.0452208405963,29.3850188498981,124.580591047788)) ;
#37527 = CARTESIAN_POINT('Ctrl Pts',(-18.9542188863965,29.2050297694883,124.872787108303)) ;
#37528 = CARTESIAN_POINT('Ctrl Pts',(-18.6678065643519,29.4049855414925,124.386372516553)) ;
#37529 = CARTESIAN_POINT('Ctrl Pts',(-18.4824497195232,29.2249964610827,124.630017164138)) ;
#37530 = CARTESIAN_POINT('Ctrl Pts',(-18.379791129464,29.4249455872434,124.074550900543)) ;
#37531 = CARTESIAN_POINT('Ctrl Pts',(-18.1224282620672,29.2449565068336,124.240242602024)) ;
#37532 = CARTESIAN_POINT('Ctrl Pts',(-18.2157634731263,29.4448438473937,123.684577273612)) ;
#37533 = CARTESIAN_POINT('Ctrl Pts',(-17.9173907833748,29.2648547669839,123.752777846952)) ;
#37534 = CARTESIAN_POINT('Ctrl Pts',(-18.1941500603982,29.4647387629429,123.262128718319)) ;
#37535 = CARTESIAN_POINT('Ctrl Pts',(-17.8903701259181,29.284749682533,123.224718223143)) ;
#37536 = CARTESIAN_POINT('Ctrl Pts',(-18.3177155519128,29.4846489433565,122.85722218228)) ;
#37537 = CARTESIAN_POINT('Ctrl Pts',(-18.0448227790929,29.3046598629467,122.718584462638)) ;
#37538 = CARTESIAN_POINT('Ctrl Pts',(-18.5722210885648,29.5045847424707,122.518222965031)) ;
#37539 = CARTESIAN_POINT('Ctrl Pts',(-18.3629508948928,29.3245956620609,122.294833096164)) ;
#37540 = CARTESIAN_POINT('Ctrl Pts',(-18.9271398359767,29.5245226041249,122.286384499788)) ;
#37541 = CARTESIAN_POINT('Ctrl Pts',(-18.806596664507,29.3445335237151,122.005031573902)) ;
#37542 = CARTESIAN_POINT('Ctrl Pts',(-19.3394465637527,29.5444416507625,122.189407632929)) ;
#37543 = CARTESIAN_POINT('Ctrl Pts',(-19.3219781329288,29.3644525703527,121.88380547974)) ;
#37544 = CARTESIAN_POINT('Ctrl Pts',(-19.7607048779396,29.5643905488167,122.23896191623)) ;
#37545 = CARTESIAN_POINT('Ctrl Pts',(-19.8485530096287,29.3844014684068,121.945745518178)) ;
#37546 = CARTESIAN_POINT('Ctrl Pts',(-20.1390238650554,29.5842963762597,122.428800132525)) ;
#37547 = CARTESIAN_POINT('Ctrl Pts',(-20.3214474198528,29.4043072958499,122.183031232966)) ;
#37548 = CARTESIAN_POINT('Ctrl Pts',(-20.381503088585,29.600879071625,122.684669772167)) ;
#37549 = CARTESIAN_POINT('Ctrl Pts',(-20.6245684185229,29.4208899912152,122.502888255903)) ;
#37550 = CARTESIAN_POINT('Ctrl Pts',(-20.5148467807965,29.6141532853487,122.929890317395)) ;
#37551 = CARTESIAN_POINT('Ctrl Pts',(-20.7912341810061,29.4341642049389,122.809390920686)) ;
#37552 = CARTESIAN_POINT('Ctrl Pts',(-20.5818729164079,29.624200004548,123.130156956782)) ;
#37553 = CARTESIAN_POINT('Ctrl Pts',(-20.875022085284,29.4442109241382,123.059731213221)) ;
#37554 = CARTESIAN_POINT('Ctrl Pts',(-20.6127109296286,29.6340440391937,123.334823989138)) ;
#37555 = CARTESIAN_POINT('Ctrl Pts',(-20.9135737768824,29.4540549587838,123.315549607636)) ;
#37556 = CARTESIAN_POINT('Ctrl Pts',(-20.6063479572666,29.6473784240982,123.615020683285)) ;
#37557 = CARTESIAN_POINT('Ctrl Pts',(-20.9056110533452,29.4673893436884,123.665862635862)) ;
#37558 = CARTESIAN_POINT('Ctrl Pts',(-20.5072137738658,29.663965641398,123.953603105851)) ;
#37559 = CARTESIAN_POINT('Ctrl Pts',(-20.7817183691732,29.4839765609882,124.08900812148)) ;
#37560 = CARTESIAN_POINT('Ctrl Pts',(-20.2982490380892,29.6805988534359,124.238824540592)) ;
#37561 = CARTESIAN_POINT('Ctrl Pts',(-20.5204871040538,29.500609773026,124.445591168516)) ;
#37562 = CARTESIAN_POINT('Ctrl Pts',(-20.0804621860381,29.6938812957081,124.413688383922)) ;
#37563 = CARTESIAN_POINT('Ctrl Pts',(-20.2482786095012,29.5138922152982,124.664142759383)) ;
#37564 = CARTESIAN_POINT('Ctrl Pts',(-19.8981216436981,29.7037871836223,124.514250466141)) ;
#37565 = CARTESIAN_POINT('Ctrl Pts',(-20.020349611139,29.5237981032124,124.78985389597)) ;
#37566 = CARTESIAN_POINT('Ctrl Pts',(-19.6995040700482,29.7137756017274,124.582447696612)) ;
#37567 = CARTESIAN_POINT('Ctrl Pts',(-19.7720804978003,29.5337865213176,124.875101645532)) ;
#37568 = CARTESIAN_POINT('Ctrl Pts',(-19.491307008318,29.7237990289661,124.615012952645)) ;
#37569 = CARTESIAN_POINT('Ctrl Pts',(-19.5118312861941,29.5438099485563,124.915810540178)) ;
#37570 = CARTESIAN_POINT('Ctrl Pts',(-19.2831262713956,29.7337034600831,124.611097510971)) ;
#37571 = CARTESIAN_POINT('Ctrl Pts',(-19.2516162816034,29.5537143796733,124.910922145077)) ;
#37572 = CARTESIAN_POINT('Ctrl Pts',(-19.0093558420609,29.7469666126936,124.55825582872)) ;
#37573 = CARTESIAN_POINT('Ctrl Pts',(-18.9093488133152,29.5669775322837,124.844857601272)) ;
#37574 = CARTESIAN_POINT('Ctrl Pts',(-18.7545952522591,29.7602915105975,124.434343951779)) ;
#37575 = CARTESIAN_POINT('Ctrl Pts',(-18.5909285364319,29.5803024301876,124.68997248973)) ;
#37576 = CARTESIAN_POINT('Ctrl Pts',(-18.5439553830956,29.7735472542131,124.251793494169)) ;
#37577 = CARTESIAN_POINT('Ctrl Pts',(-18.327641649914,29.5935581738033,124.461801734834)) ;
#37578 = CARTESIAN_POINT('Ctrl Pts',(-18.4117225992589,29.7835066276604,124.089495823393)) ;
#37579 = CARTESIAN_POINT('Ctrl Pts',(-18.1623453453475,29.6035175472506,124.258928464858)) ;
#37580 = CARTESIAN_POINT('Ctrl Pts',(-18.3095785405791,29.7934504515873,123.907068143892)) ;
#37581 = CARTESIAN_POINT('Ctrl Pts',(-18.034663608841,29.6134613711775,124.030895956601)) ;
#37582 = CARTESIAN_POINT('Ctrl Pts',(-18.2401254145393,29.8034983957346,123.707589819514)) ;
#37583 = CARTESIAN_POINT('Ctrl Pts',(-17.9478442965894,29.6235093153248,123.781548712631)) ;
#37584 = CARTESIAN_POINT('Ctrl Pts',(-18.2068401315693,29.8133493669528,123.503171166359)) ;
#37585 = CARTESIAN_POINT('Ctrl Pts',(-17.9062349536996,29.633360286543,123.526025793522)) ;
#37586 = CARTESIAN_POINT('Ctrl Pts',(-18.20904682234,29.8233211843949,123.293567779389)) ;
#37587 = CARTESIAN_POINT('Ctrl Pts',(-17.9089904953262,29.6433321039851,123.264021399706)) ;
#37588 = CARTESIAN_POINT('Ctrl Pts',(-18.2477491639959,29.833316606687,123.086997661394)) ;
#37589 = CARTESIAN_POINT('Ctrl Pts',(-17.9573656876307,29.6533275262772,123.005808163282)) ;
#37590 = CARTESIAN_POINT('Ctrl Pts',(-18.3222034367972,29.8433496718107,122.889655956978)) ;
#37591 = CARTESIAN_POINT('Ctrl Pts',(-18.0504309096525,29.6633605914008,122.759129997716)) ;
#37592 = CARTESIAN_POINT('Ctrl Pts',(-18.427820698995,29.8532150044759,122.711168026723)) ;
#37593 = CARTESIAN_POINT('Ctrl Pts',(-18.1824501819695,29.6732259240661,122.536018472137)) ;
#37594 = CARTESIAN_POINT('Ctrl Pts',(-18.5636657279792,29.8631755470735,122.551802567031)) ;
#37595 = CARTESIAN_POINT('Ctrl Pts',(-18.3522544607679,29.6831864666636,122.336809733976)) ;
#37596 = CARTESIAN_POINT('Ctrl Pts',(-18.7265192984171,29.8732092325752,122.41775022895)) ;
#37597 = CARTESIAN_POINT('Ctrl Pts',(-18.555819664676,29.6932201521654,122.169242143803)) ;
#37598 = CARTESIAN_POINT('Ctrl Pts',(-18.9073064956514,29.8830940645654,122.315216883983)) ;
#37599 = CARTESIAN_POINT('Ctrl Pts',(-18.7818025396758,29.7031049841556,122.041072921701)) ;
#37600 = CARTESIAN_POINT('Ctrl Pts',(-19.1067239041188,29.8931614913253,122.244413082228)) ;
#37601 = CARTESIAN_POINT('Ctrl Pts',(-19.0310733363966,29.7131724109154,121.952565569441)) ;
#37602 = CARTESIAN_POINT('Ctrl Pts',(-19.3106948006957,29.9029999804841,122.209895700099)) ;
#37603 = CARTESIAN_POINT('Ctrl Pts',(-19.2860369019706,29.7230109000743,121.90941606454)) ;
#37604 = CARTESIAN_POINT('Ctrl Pts',(-19.5222278617027,29.9130634616742,122.211069618084)) ;
#37605 = CARTESIAN_POINT('Ctrl Pts',(-19.5504531994804,29.7330743812644,121.910880737609)) ;
#37606 = CARTESIAN_POINT('Ctrl Pts',(-19.7268617704073,29.9229576194894,122.24850430312)) ;
#37607 = CARTESIAN_POINT('Ctrl Pts',(-19.8062464008492,29.7429685390795,121.957671456144)) ;
#37608 = CARTESIAN_POINT('Ctrl Pts',(-19.9229782407006,29.9328994762337,122.320699146715)) ;
#37609 = CARTESIAN_POINT('Ctrl Pts',(-20.0513931602356,29.7529103958238,122.047912589634)) ;
#37610 = CARTESIAN_POINT('Ctrl Pts',(-20.1047692037057,29.9429019539051,122.426450883275)) ;
#37611 = CARTESIAN_POINT('Ctrl Pts',(-20.2786332742653,29.7629128734952,122.18010000286)) ;
#37612 = CARTESIAN_POINT('Ctrl Pts',(-20.2657090613012,29.9529367582094,122.562825912537)) ;
#37613 = CARTESIAN_POINT('Ctrl Pts',(-20.4798098359989,29.7729476777996,122.350566712066)) ;
#37614 = CARTESIAN_POINT('Ctrl Pts',(-20.3982580149733,29.962781635055,122.72180138389)) ;
#37615 = CARTESIAN_POINT('Ctrl Pts',(-20.6454984301045,29.7827925546452,122.549284780263)) ;
#37616 = CARTESIAN_POINT('Ctrl Pts',(-20.5029831129388,29.9727675146106,122.903710362573)) ;
#37617 = CARTESIAN_POINT('Ctrl Pts',(-20.7764071388817,29.7927784342008,122.776669844113)) ;
#37618 = CARTESIAN_POINT('Ctrl Pts',(-20.5743335334042,29.9827022449691,123.100047335692)) ;
#37619 = CARTESIAN_POINT('Ctrl Pts',(-20.8655976910144,29.8027131645593,123.022090489165)) ;
#37620 = CARTESIAN_POINT('Ctrl Pts',(-20.6107482776223,29.992760057282,123.308299706397)) ;
#37621 = CARTESIAN_POINT('Ctrl Pts',(-20.9111186733623,29.8127709768721,123.282405386594)) ;
#37622 = CARTESIAN_POINT('Ctrl Pts',(-20.6108122645727,30.0025806494063,123.514793587701)) ;
#37623 = CARTESIAN_POINT('Ctrl Pts',(-20.9112011989826,29.8225915689965,123.540523528453)) ;
#37624 = CARTESIAN_POINT('Ctrl Pts',(-20.5743946708493,30.0126472350161,123.723224917904)) ;
#37625 = CARTESIAN_POINT('Ctrl Pts',(-20.8656816934945,29.8326581546063,123.801062971422)) ;
#37626 = CARTESIAN_POINT('Ctrl Pts',(-20.5034684423452,30.0225468155979,123.918938589695)) ;
#37627 = CARTESIAN_POINT('Ctrl Pts',(-20.7770260889006,29.8425577351881,124.0457063851)) ;
#37628 = CARTESIAN_POINT('Ctrl Pts',(-20.398156180313,30.0325984152762,124.102097749828)) ;
#37629 = CARTESIAN_POINT('Ctrl Pts',(-20.6453879764879,29.8526093348664,124.274656477353)) ;
#37630 = CARTESIAN_POINT('Ctrl Pts',(-20.2651035498594,30.0424726016932,124.261488906871)) ;
#37631 = CARTESIAN_POINT('Ctrl Pts',(-20.4790736606375,29.8624835212833,124.473897491977)) ;
#37632 = CARTESIAN_POINT('Ctrl Pts',(-20.1036145885846,30.0525290775741,124.397880998235)) ;
#37633 = CARTESIAN_POINT('Ctrl Pts',(-20.2772141278221,29.8725399971642,124.64438938029)) ;
#37634 = CARTESIAN_POINT('Ctrl Pts',(-19.9238362938821,30.0624220088767,124.502541628328)) ;
#37635 = CARTESIAN_POINT('Ctrl Pts',(-20.0524919644394,29.8824329284668,124.775217544971)) ;
#37636 = CARTESIAN_POINT('Ctrl Pts',(-19.7253526604774,30.0724847875893,124.575641997785)) ;
#37637 = CARTESIAN_POINT('Ctrl Pts',(-19.8043884253342,29.8924957071795,124.86659520155)) ;
#37638 = CARTESIAN_POINT('Ctrl Pts',(-19.5217089265332,30.0823273131705,124.612461273804)) ;
#37639 = CARTESIAN_POINT('Ctrl Pts',(-19.5498333322832,29.9023382327606,124.912621791189)) ;
#37640 = CARTESIAN_POINT('Ctrl Pts',(-19.3117032501177,30.0923180785953,124.613877366419)) ;
#37641 = CARTESIAN_POINT('Ctrl Pts',(-19.2873260770961,29.9123289981855,124.914394172903)) ;
#37642 = CARTESIAN_POINT('Ctrl Pts',(-19.1059111788541,30.1022461545934,124.578985148832)) ;
#37643 = CARTESIAN_POINT('Ctrl Pts',(-19.0300851291578,29.9222570741836,124.870781057803)) ;
#37644 = CARTESIAN_POINT('Ctrl Pts',(-18.9079961280173,30.1122340649804,124.508814514259)) ;
#37645 = CARTESIAN_POINT('Ctrl Pts',(-18.7826904157182,29.9322449845706,124.783069756835)) ;
#37646 = CARTESIAN_POINT('Ctrl Pts',(-18.7245848851423,30.1222699771053,124.404544827108)) ;
#37647 = CARTESIAN_POINT('Ctrl Pts',(-18.5534253143537,29.9422808966955,124.652734665158)) ;
#37648 = CARTESIAN_POINT('Ctrl Pts',(-18.5647574103382,30.132124989953,124.272686477183)) ;
#37649 = CARTESIAN_POINT('Ctrl Pts',(-18.3536388770695,29.9521359095432,124.487912827433)) ;
#37650 = CARTESIAN_POINT('Ctrl Pts',(-18.4280975268948,30.1421239358693,124.11300608856)) ;
#37651 = CARTESIAN_POINT('Ctrl Pts',(-18.1828123336162,29.9621348554594,124.288313606245)) ;
#37652 = CARTESIAN_POINT('Ctrl Pts',(-18.3221216583478,30.1520208483173,123.933916262018)) ;
#37653 = CARTESIAN_POINT('Ctrl Pts',(-18.0503403718205,29.9720317679075,124.064451745959)) ;
#37654 = CARTESIAN_POINT('Ctrl Pts',(-18.2476869675524,30.1620746464108,123.736121592027)) ;
#37655 = CARTESIAN_POINT('Ctrl Pts',(-17.9572951647784,29.9820855660009,123.817209301513)) ;
#37656 = CARTESIAN_POINT('Ctrl Pts',(-18.209328142363,30.1719555672375,123.531942530913)) ;
#37657 = CARTESIAN_POINT('Ctrl Pts',(-17.9093444926805,29.9919664868276,123.561985023858)) ;
#37658 = CARTESIAN_POINT('Ctrl Pts',(-18.2065963316718,30.1819600932352,123.321657997475)) ;
#37659 = CARTESIAN_POINT('Ctrl Pts',(-17.9059278138012,30.0019710128254,123.299129283871)) ;
#37660 = CARTESIAN_POINT('Ctrl Pts',(-18.2404207061427,30.1919440568527,123.114471153255)) ;
#37661 = CARTESIAN_POINT('Ctrl Pts',(-17.9482064112009,30.0119549764429,123.040145215729)) ;
#37662 = CARTESIAN_POINT('Ctrl Pts',(-18.31026366629,30.201983697404,122.915313410186)) ;
#37663 = CARTESIAN_POINT('Ctrl Pts',(-18.0355081866653,30.0219946169941,122.791197498852)) ;
#37664 = CARTESIAN_POINT('Ctrl Pts',(-18.4113981835528,30.2118277230187,122.734755075974)) ;
#37665 = CARTESIAN_POINT('Ctrl Pts',(-18.1619252128629,30.0318386426089,122.56549765769)) ;
#37666 = CARTESIAN_POINT('Ctrl Pts',(-18.5438338536838,30.221818728836,122.571724660386)) ;
#37667 = CARTESIAN_POINT('Ctrl Pts',(-18.327468580518,30.0418296484262,122.361708399331)) ;
#37668 = CARTESIAN_POINT('Ctrl Pts',(-18.7036229588605,30.2318565203682,122.433886669261)) ;
#37669 = CARTESIAN_POINT('Ctrl Pts',(-18.5272036339807,30.0518674399584,122.189409573073)) ;
#37670 = CARTESIAN_POINT('Ctrl Pts',(-18.8812446957364,30.2417009201566,122.327651393259)) ;
#37671 = CARTESIAN_POINT('Ctrl Pts',(-18.7492309039636,30.0617118397468,122.056613364002)) ;
#37672 = CARTESIAN_POINT('Ctrl Pts',(-19.0771915548651,30.2516857207133,122.252443734513)) ;
#37673 = CARTESIAN_POINT('Ctrl Pts',(-18.9941641262514,30.0716966403035,121.962602178219)) ;
#37674 = CARTESIAN_POINT('Ctrl Pts',(-19.2823241886974,30.2616252441245,122.212483119528)) ;
#37675 = CARTESIAN_POINT('Ctrl Pts',(-19.2505801464845,30.0816361637147,121.912649736789)) ;
#37676 = CARTESIAN_POINT('Ctrl Pts',(-19.4933414984696,30.2716649632255,122.20875992218)) ;
#37677 = CARTESIAN_POINT('Ctrl Pts',(-19.5143516088837,30.0916758828157,121.907994125339)) ;
#37678 = CARTESIAN_POINT('Ctrl Pts',(-19.698697204164,30.2815531351448,122.241136729093)) ;
#37679 = CARTESIAN_POINT('Ctrl Pts',(-19.7710473972824,30.101564054735,121.948463714457)) ;
#37680 = CARTESIAN_POINT('Ctrl Pts',(-19.8974368961156,30.2915426975618,122.308992544338)) ;
#37681 = CARTESIAN_POINT('Ctrl Pts',(-20.0194726828299,30.1115536171519,122.03328218097)) ;
#37682 = CARTESIAN_POINT('Ctrl Pts',(-20.0807289084001,30.3015010697565,122.410148468044)) ;
#37683 = CARTESIAN_POINT('Ctrl Pts',(-20.2485888049061,30.1215119893467,122.159725978193)) ;
#37684 = CARTESIAN_POINT('Ctrl Pts',(-20.2430415790186,30.3114011439872,122.540440637745)) ;
#37685 = CARTESIAN_POINT('Ctrl Pts',(-20.4514811555674,30.1314120635773,122.322590700171)) ;
#37686 = CARTESIAN_POINT('Ctrl Pts',(-20.3822575057102,30.3214472403608,122.699250508298)) ;
#37687 = CARTESIAN_POINT('Ctrl Pts',(-20.6255019414062,30.1414581599509,122.521102011008)) ;
#37688 = CARTESIAN_POINT('Ctrl Pts',(-20.4903053212277,30.3313558243579,122.877358635903)) ;
#37689 = CARTESIAN_POINT('Ctrl Pts',(-20.7605632741232,30.1513667439481,122.743737177672)) ;
#37690 = CARTESIAN_POINT('Ctrl Pts',(-20.56692385887,30.3413664029488,123.073373311009)) ;
#37691 = CARTESIAN_POINT('Ctrl Pts',(-20.8563375787793,30.1613773225389,122.988755129696)) ;
#37692 = CARTESIAN_POINT('Ctrl Pts',(-20.6080032804155,30.3513955610616,123.280185120993)) ;
#37693 = CARTESIAN_POINT('Ctrl Pts',(-20.9076881588151,30.1714064806518,123.247269528935)) ;
#37694 = CARTESIAN_POINT('Ctrl Pts',(-20.6127668223826,30.3612484428997,123.487255373469)) ;
#37695 = CARTESIAN_POINT('Ctrl Pts',(-20.9136438599794,30.1812593624898,123.506108579088)) ;
#37696 = CARTESIAN_POINT('Ctrl Pts',(-20.5818009833245,30.3712080040507,123.694340585296)) ;
#37697 = CARTESIAN_POINT('Ctrl Pts',(-20.8749374875064,30.1912189236409,123.764965708025)) ;
#37698 = CARTESIAN_POINT('Ctrl Pts',(-20.5144631349101,30.3812464386398,123.894334448527)) ;
#37699 = CARTESIAN_POINT('Ctrl Pts',(-20.7907663165275,30.2012573582299,124.014958246579)) ;
#37700 = CARTESIAN_POINT('Ctrl Pts',(-20.4154074111559,30.3911197108669,124.076778134823)) ;
#37701 = CARTESIAN_POINT('Ctrl Pts',(-20.6669470046952,30.211130630457,124.243014320162)) ;
#37702 = CARTESIAN_POINT('Ctrl Pts',(-20.283556385648,30.4011929528604,124.24244097245)) ;
#37703 = CARTESIAN_POINT('Ctrl Pts',(-20.5021342924087,30.2212038724506,124.450093173156)) ;
#37704 = CARTESIAN_POINT('Ctrl Pts',(-20.1290404897392,30.4110132843935,124.379433616432)) ;
#37705 = CARTESIAN_POINT('Ctrl Pts',(-20.3089888717368,30.2310242039837,124.621335698732)) ;
#37706 = CARTESIAN_POINT('Ctrl Pts',(-19.9486420914419,30.4210919456203,124.490474607517)) ;
#37707 = CARTESIAN_POINT('Ctrl Pts',(-20.0834917212071,30.2411028652105,124.760137415839)) ;
#37708 = CARTESIAN_POINT('Ctrl Pts',(-19.7560754413222,30.4309435409145,124.566851656652)) ;
#37709 = CARTESIAN_POINT('Ctrl Pts',(-19.8427824862029,30.2509544605047,124.855609977421)) ;
#37710 = CARTESIAN_POINT('Ctrl Pts',(-19.5487326187181,30.4410166761433,124.609735878305)) ;
#37711 = CARTESIAN_POINT('Ctrl Pts',(-19.5836045391688,30.2610275957335,124.909215904184)) ;
#37712 = CARTESIAN_POINT('Ctrl Pts',(-19.3418837703433,30.4508591116683,124.615794712703)) ;
#37713 = CARTESIAN_POINT('Ctrl Pts',(-19.325042085663,30.2708700312585,124.916790254911)) ;
#37714 = CARTESIAN_POINT('Ctrl Pts',(-19.1341767024053,30.4608398808017,124.586121780913)) ;
#37715 = CARTESIAN_POINT('Ctrl Pts',(-19.06540787512,30.2808508003919,124.879699535885)) ;
#37716 = CARTESIAN_POINT('Ctrl Pts',(-18.9341621364853,30.4708569820456,124.520222155215)) ;
#37717 = CARTESIAN_POINT('Ctrl Pts',(-18.8153894690944,30.2908679016358,124.797325621864)) ;
#37718 = CARTESIAN_POINT('Ctrl Pts',(-18.7508125062853,30.4807454296474,124.422211803213)) ;
#37719 = CARTESIAN_POINT('Ctrl Pts',(-18.5862012534793,30.3007563492376,124.674812609877)) ;
#37720 = CARTESIAN_POINT('Ctrl Pts',(-18.5845129446099,30.4908011438283,124.291721984471)) ;
#37721 = CARTESIAN_POINT('Ctrl Pts',(-18.3783267486682,30.3108120634185,124.511700910581)) ;
#37722 = CARTESIAN_POINT('Ctrl Pts',(-18.44588508889,30.5006763502421,124.137161226805)) ;
#37723 = CARTESIAN_POINT('Ctrl Pts',(-18.2050407984667,30.3206872698323,124.318499416567)) ;
#37724 = CARTESIAN_POINT('Ctrl Pts',(-18.3344500450704,30.5106714027149,123.959022928956)) ;
#37725 = CARTESIAN_POINT('Ctrl Pts',(-18.0657466674759,30.330682322305,124.095826539114)) ;
#37726 = CARTESIAN_POINT('Ctrl Pts',(-18.2557384460612,30.520693286677,123.763577906026)) ;
#37727 = CARTESIAN_POINT('Ctrl Pts',(-17.9673568014164,30.3407042062672,123.851520456644)) ;
#37728 = CARTESIAN_POINT('Ctrl Pts',(-18.2124447067718,30.5305972592063,123.559917806185)) ;
#37729 = CARTESIAN_POINT('Ctrl Pts',(-17.9132391132283,30.3506081787965,123.596944459878)) ;
#37730 = CARTESIAN_POINT('Ctrl Pts',(-18.204806352772,30.5405857558672,123.350065475818)) ;
#37731 = CARTESIAN_POINT('Ctrl Pts',(-17.9036909634777,30.3605966754573,123.334628818857)) ;
#37732 = CARTESIAN_POINT('Ctrl Pts',(-18.2337889801412,30.5505495531152,123.142620805064)) ;
#37733 = CARTESIAN_POINT('Ctrl Pts',(-17.9399190540349,30.3705604727053,123.075322497825)) ;
#37734 = CARTESIAN_POINT('Ctrl Pts',(-18.2974874686317,30.5604535764232,122.944369701572)) ;
#37735 = CARTESIAN_POINT('Ctrl Pts',(-18.0195424014085,30.3804644960134,122.827507706728)) ;
#37736 = CARTESIAN_POINT('Ctrl Pts',(-18.3963113380305,30.5705140797448,122.757403023843)) ;
#37737 = CARTESIAN_POINT('Ctrl Pts',(-18.1430719622908,30.390524999335,122.593799613833)) ;
#37738 = CARTESIAN_POINT('Ctrl Pts',(-18.5230838015688,30.5803546148847,122.593882778984)) ;
#37739 = CARTESIAN_POINT('Ctrl Pts',(-18.3015384279118,30.4003655344749,122.389398133956)) ;
#37740 = CARTESIAN_POINT('Ctrl Pts',(-18.6795561688118,30.5904168355893,122.451559837919)) ;
#37741 = CARTESIAN_POINT('Ctrl Pts',(-18.4971286723623,30.4104277551794,122.211494770996)) ;
#37742 = CARTESIAN_POINT('Ctrl Pts',(-18.8555743115362,30.6003139893655,122.340587366803)) ;
#37743 = CARTESIAN_POINT('Ctrl Pts',(-18.7171521979326,30.4203249089557,122.072778646535)) ;
#37744 = CARTESIAN_POINT('Ctrl Pts',(-19.0485703229917,30.610245122751,122.260955111829)) ;
#37745 = CARTESIAN_POINT('Ctrl Pts',(-18.9583979844266,30.4302560423412,121.973238308994)) ;
#37746 = CARTESIAN_POINT('Ctrl Pts',(-19.2547965608815,30.6202874978967,122.215768412004)) ;
#37747 = CARTESIAN_POINT('Ctrl Pts',(-19.2161806172609,30.4402984174869,121.916755158217)) ;
#37748 = CARTESIAN_POINT('Ctrl Pts',(-19.4624589820246,30.6301734356628,122.207050198295)) ;
#37749 = CARTESIAN_POINT('Ctrl Pts',(-19.4757597411962,30.450184355253,121.9058575907)) ;
#37750 = CARTESIAN_POINT('Ctrl Pts',(-19.6707860504758,30.6401692786477,122.234500227154)) ;
#37751 = CARTESIAN_POINT('Ctrl Pts',(-19.7361687240482,30.4601801982378,121.940170526938)) ;
#37752 = CARTESIAN_POINT('Ctrl Pts',(-19.8701217771489,30.6501112565263,122.297396578507)) ;
#37753 = CARTESIAN_POINT('Ctrl Pts',(-19.9853388632979,30.4701221761165,122.01879150235)) ;
#37754 = CARTESIAN_POINT('Ctrl Pts',(-20.0559439542631,30.6600706310073,122.393853881732)) ;
#37755 = CARTESIAN_POINT('Ctrl Pts',(-20.2176167859289,30.4800815505974,122.13936377116)) ;
#37756 = CARTESIAN_POINT('Ctrl Pts',(-20.2229095752647,30.6700672468411,122.521521564149)) ;
#37757 = CARTESIAN_POINT('Ctrl Pts',(-20.4263236161988,30.4900781664312,122.298948878798)) ;
#37758 = CARTESIAN_POINT('Ctrl Pts',(-20.3654814517331,30.6801014654146,122.676991794271)) ;
#37759 = CARTESIAN_POINT('Ctrl Pts',(-20.6045380696122,30.5001123850047,122.493286837785)) ;
#37760 = CARTESIAN_POINT('Ctrl Pts',(-20.4770590422529,30.6899545326252,122.851511404317)) ;
#37761 = CARTESIAN_POINT('Ctrl Pts',(-20.7440103711804,30.5099654522154,122.711437778159)) ;
#37762 = CARTESIAN_POINT('Ctrl Pts',(-20.5580675426808,30.6999147905028,123.044595067161)) ;
#37763 = CARTESIAN_POINT('Ctrl Pts',(-20.8452704863251,30.5199257100929,122.95279307228)) ;
#37764 = CARTESIAN_POINT('Ctrl Pts',(-20.6044003781511,30.7099438172084,123.250294695878)) ;
#37765 = CARTESIAN_POINT('Ctrl Pts',(-20.9031858778031,30.5299547367985,123.209917654141)) ;
#37766 = CARTESIAN_POINT('Ctrl Pts',(-20.6142563398137,30.7198540242428,123.458395760156)) ;
#37767 = CARTESIAN_POINT('Ctrl Pts',(-20.9155052004017,30.539864943833,123.47004489255)) ;
#37768 = CARTESIAN_POINT('Ctrl Pts',(-20.5883067682827,30.7297889348904,123.665646410074)) ;
#37769 = CARTESIAN_POINT('Ctrl Pts',(-20.8830672768475,30.5497998544806,123.729108751016)) ;
#37770 = CARTESIAN_POINT('Ctrl Pts',(-20.525923055177,30.7398300650696,123.867307187014)) ;
#37771 = CARTESIAN_POINT('Ctrl Pts',(-20.8050869197555,30.5598409846598,123.981184304472)) ;
#37772 = CARTESIAN_POINT('Ctrl Pts',(-20.4310732674177,30.7497172054396,124.052276123954)) ;
#37773 = CARTESIAN_POINT('Ctrl Pts',(-20.686523442515,30.5697281250298,124.212396007717)) ;
#37774 = CARTESIAN_POINT('Ctrl Pts',(-20.3045079136013,30.7597094829755,124.219919068454)) ;
#37775 = CARTESIAN_POINT('Ctrl Pts',(-20.5283158328831,30.5797204025657,124.421949250834)) ;
#37776 = CARTESIAN_POINT('Ctrl Pts',(-20.1513705963158,30.7696580262439,124.36238740214)) ;
#37777 = CARTESIAN_POINT('Ctrl Pts',(-20.3368931275414,30.589668945834,124.600034326039)) ;
#37778 = CARTESIAN_POINT('Ctrl Pts',(-19.97621673164,30.7795947010611,124.476202086606)) ;
#37779 = CARTESIAN_POINT('Ctrl Pts',(-20.117949669765,30.5996056206513,124.742302120587)) ;
#37780 = CARTESIAN_POINT('Ctrl Pts',(-19.7831216512904,30.7895781219974,124.558506793433)) ;
#37781 = CARTESIAN_POINT('Ctrl Pts',(-19.8765801266948,30.6095890415876,124.845182022311)) ;
#37782 = CARTESIAN_POINT('Ctrl Pts',(-19.577416346165,30.7996204371867,124.605973059919)) ;
#37783 = CARTESIAN_POINT('Ctrl Pts',(-19.6194484246189,30.6196313567769,124.904513792587)) ;
#37784 = CARTESIAN_POINT('Ctrl Pts',(-19.3708401231471,30.8094607546259,124.617114838702)) ;
#37785 = CARTESIAN_POINT('Ctrl Pts',(-19.3612267210276,30.6294716742161,124.918439915282)) ;
#37786 = CARTESIAN_POINT('Ctrl Pts',(-19.1614550331297,30.8194904586834,124.592230575313)) ;
#37787 = CARTESIAN_POINT('Ctrl Pts',(-19.0994956243857,30.6395013782735,124.887333257239)) ;
#37788 = CARTESIAN_POINT('Ctrl Pts',(-18.9599146448353,30.8295114154059,124.530878822072)) ;
#37789 = CARTESIAN_POINT('Ctrl Pts',(-18.8475705007407,30.6495223349961,124.810642476256)) ;
#37790 = CARTESIAN_POINT('Ctrl Pts',(-18.7747291699173,30.8393779577095,124.437402415365)) ;
#37791 = CARTESIAN_POINT('Ctrl Pts',(-18.6160882477123,30.6593888772996,124.693795263407)) ;
#37792 = CARTESIAN_POINT('Ctrl Pts',(-18.6051688450948,30.8494490576546,124.310638457262)) ;
#37793 = CARTESIAN_POINT('Ctrl Pts',(-18.404138945044,30.6694599772448,124.535339469845)) ;
#37794 = CARTESIAN_POINT('Ctrl Pts',(-18.4634769424933,30.8592911318322,124.159844576277)) ;
#37795 = CARTESIAN_POINT('Ctrl Pts',(-18.22702415179,30.6793020514224,124.346845255136)) ;
#37796 = CARTESIAN_POINT('Ctrl Pts',(-18.3481138935015,30.8692519264192,123.98508540905)) ;
#37797 = CARTESIAN_POINT('Ctrl Pts',(-18.0828214570225,30.6892628460094,124.128395071052)) ;
#37798 = CARTESIAN_POINT('Ctrl Pts',(-18.2645872120616,30.8792897993201,123.791299482673)) ;
#37799 = CARTESIAN_POINT('Ctrl Pts',(-17.9784145005969,30.6993007189103,123.886162207507)) ;
#37800 = CARTESIAN_POINT('Ctrl Pts',(-18.2163875155882,30.8891640848642,123.589358215528)) ;
#37801 = CARTESIAN_POINT('Ctrl Pts',(-17.9181661939487,30.7091750044543,123.633734267032)) ;
#37802 = CARTESIAN_POINT('Ctrl Pts',(-18.203753574643,30.8992338352781,123.378065938577)) ;
#37803 = CARTESIAN_POINT('Ctrl Pts',(-17.902375375643,30.7192447548683,123.369619175595)) ;
#37804 = CARTESIAN_POINT('Ctrl Pts',(-18.2273236827773,30.9090671198127,123.172670784879)) ;
#37805 = CARTESIAN_POINT('Ctrl Pts',(-17.9318397717287,30.7290780394029,123.112874144426)) ;
#37806 = CARTESIAN_POINT('Ctrl Pts',(-18.2867987026179,30.9190974606128,122.970368878916)) ;
#37807 = CARTESIAN_POINT('Ctrl Pts',(-18.0061852689319,30.739108380203,122.85999735939)) ;
#37808 = CARTESIAN_POINT('Ctrl Pts',(-18.3810728614528,30.9291293846124,122.781698599394)) ;
#37809 = CARTESIAN_POINT('Ctrl Pts',(-18.1240293774352,30.7491403042026,122.624160309283)) ;
#37810 = CARTESIAN_POINT('Ctrl Pts',(-18.50375518637,30.9389579195483,122.6154474201)) ;
#37811 = CARTESIAN_POINT('Ctrl Pts',(-18.2773844644473,30.7589688391385,122.416346355299)) ;
#37812 = CARTESIAN_POINT('Ctrl Pts',(-18.6555659033438,30.948951697313,122.470205569998)) ;
#37813 = CARTESIAN_POINT('Ctrl Pts',(-18.4671493140106,30.7689626169032,122.23479534461)) ;
#37814 = CARTESIAN_POINT('Ctrl Pts',(-18.8311197714127,30.9589794077985,122.353474256892)) ;
#37815 = CARTESIAN_POINT('Ctrl Pts',(-18.6865926220437,30.7789903273887,122.088882738847)) ;
#37816 = CARTESIAN_POINT('Ctrl Pts',(-19.021483587405,30.9688678186325,122.269936336135)) ;
#37817 = CARTESIAN_POINT('Ctrl Pts',(-18.9245489185177,30.7888787382227,121.984461740801)) ;
#37818 = CARTESIAN_POINT('Ctrl Pts',(-19.2251633873121,30.978844669168,122.219928658385)) ;
#37819 = CARTESIAN_POINT('Ctrl Pts',(-19.1791493957225,30.7988555887582,121.92195402928)) ;
#37820 = CARTESIAN_POINT('Ctrl Pts',(-19.4347905985392,30.9888364657185,122.206004671817)) ;
#37821 = CARTESIAN_POINT('Ctrl Pts',(-19.4411836962551,30.8088473853087,121.904551040797)) ;
#37822 = CARTESIAN_POINT('Ctrl Pts',(-19.6445006365015,30.9988724718122,122.229041741586)) ;
#37823 = CARTESIAN_POINT('Ctrl Pts',(-19.7033209422689,30.8188833914023,121.933349289117)) ;
#37824 = CARTESIAN_POINT('Ctrl Pts',(-19.8434060708219,31.008723206075,122.286751984525)) ;
#37825 = CARTESIAN_POINT('Ctrl Pts',(-19.9519531581961,30.8287341256652,122.005489324645)) ;
#37826 = CARTESIAN_POINT('Ctrl Pts',(-20.0320403039582,31.0187144646032,122.379080702505)) ;
#37827 = CARTESIAN_POINT('Ctrl Pts',(-20.1877451627324,30.8387253841934,122.120902211043)) ;
#37828 = CARTESIAN_POINT('Ctrl Pts',(-20.2006501988176,31.0286323595064,122.501784715894)) ;
#37829 = CARTESIAN_POINT('Ctrl Pts',(-20.3985067246946,30.8486432790966,122.274284311922)) ;
#37830 = CARTESIAN_POINT('Ctrl Pts',(-20.3470107237814,31.0386605011694,122.65350091565)) ;
#37831 = CARTESIAN_POINT('Ctrl Pts',(-20.58145578964,30.8586714207596,122.463931047344)) ;
#37832 = CARTESIAN_POINT('Ctrl Pts',(-20.4632104004851,31.0485456692853,122.825802329779)) ;
#37833 = CARTESIAN_POINT('Ctrl Pts',(-20.7267039760268,30.8685565888754,122.679309656384)) ;
#37834 = CARTESIAN_POINT('Ctrl Pts',(-20.5490845959354,31.0585350327913,123.017454794976)) ;
#37835 = CARTESIAN_POINT('Ctrl Pts',(-20.8340446604861,30.8785459523814,122.918876333031)) ;
#37836 = CARTESIAN_POINT('Ctrl Pts',(-20.6002096975552,31.0685761678013,123.22226668955)) ;
#37837 = CARTESIAN_POINT('Ctrl Pts',(-20.8979488652551,30.8885870873915,123.17489164825)) ;
#37838 = CARTESIAN_POINT('Ctrl Pts',(-20.615028805326,31.0784088359894,123.42844428818)) ;
#37839 = CARTESIAN_POINT('Ctrl Pts',(-20.9164705231376,30.8984197555796,123.43261476882)) ;
#37840 = CARTESIAN_POINT('Ctrl Pts',(-20.5940744638475,31.0884027389439,123.637499008543)) ;
#37841 = CARTESIAN_POINT('Ctrl Pts',(-20.8902751542732,30.908413658534,123.69393304665)) ;
#37842 = CARTESIAN_POINT('Ctrl Pts',(-20.5365069814263,31.0984320240284,123.840336990073)) ;
#37843 = CARTESIAN_POINT('Ctrl Pts',(-20.8183135578926,30.9184429436185,123.94747986394)) ;
#37844 = CARTESIAN_POINT('Ctrl Pts',(-20.446304755453,31.1083075524703,124.027344707869)) ;
#37845 = CARTESIAN_POINT('Ctrl Pts',(-20.7055583075016,30.9283184720605,124.181239071711)) ;
#37846 = CARTESIAN_POINT('Ctrl Pts',(-20.3236808566818,31.1183078350863,124.198085320137)) ;
#37847 = CARTESIAN_POINT('Ctrl Pts',(-20.5522763631696,30.9383187546765,124.394663488977)) ;
#37848 = CARTESIAN_POINT('Ctrl Pts',(-20.1746825112907,31.1282198511434,124.343800205569)) ;
#37849 = CARTESIAN_POINT('Ctrl Pts',(-20.3660263502504,30.9482307707336,124.576805637023)) ;
#37850 = CARTESIAN_POINT('Ctrl Pts',(-20.0004530429304,31.1382619264824,124.46299621068)) ;
#37851 = CARTESIAN_POINT('Ctrl Pts',(-20.1482381590655,30.9582728460726,124.72579853176)) ;
#37852 = CARTESIAN_POINT('Ctrl Pts',(-19.8108716546696,31.1481617591385,124.548900830841)) ;
#37853 = CARTESIAN_POINT('Ctrl Pts',(-19.9112599341411,30.9681726787286,124.833177229077)) ;
#37854 = CARTESIAN_POINT('Ctrl Pts',(-19.6074951368638,31.1581541597165,124.601515467069)) ;
#37855 = CARTESIAN_POINT('Ctrl Pts',(-19.6570385216624,30.9781650793067,124.898943043769)) ;
#37856 = CARTESIAN_POINT('Ctrl Pts',(-19.3971675954827,31.1681881814759,124.617712800031)) ;
#37857 = CARTESIAN_POINT('Ctrl Pts',(-19.3941289164033,30.988199101066,124.919187191748)) ;
#37858 = CARTESIAN_POINT('Ctrl Pts',(-19.1907487982186,31.1780527923171,124.59775750716)) ;
#37859 = CARTESIAN_POINT('Ctrl Pts',(-19.1361050769599,30.9980637119073,124.894240456092)) ;
#37860 = CARTESIAN_POINT('Ctrl Pts',(-18.9881977091377,31.1880451917782,124.542038359077)) ;
#37861 = CARTESIAN_POINT('Ctrl Pts',(-18.8829168165826,31.0080561113684,124.824588928415)) ;
#37862 = CARTESIAN_POINT('Ctrl Pts',(-18.7978278631162,31.1980771451111,124.451266994197)) ;
#37863 = CARTESIAN_POINT('Ctrl Pts',(-18.6449556256529,31.0180880647013,124.711122383889)) ;
#37864 = CARTESIAN_POINT('Ctrl Pts',(-18.6287533564004,31.2079435040528,124.331095273272)) ;
#37865 = CARTESIAN_POINT('Ctrl Pts',(-18.4336135989421,31.027954423643,124.56090527818)) ;
#37866 = CARTESIAN_POINT('Ctrl Pts',(-18.4811055178957,31.2179309795386,124.181843664757)) ;
#37867 = CARTESIAN_POINT('Ctrl Pts',(-18.2490556294544,31.0379418991288,124.374338785547)) ;
#37868 = CARTESIAN_POINT('Ctrl Pts',(-18.3620004505735,31.2278758857271,124.009975732587)) ;
#37869 = CARTESIAN_POINT('Ctrl Pts',(-18.1001763826334,31.0478868053173,124.159502137158)) ;
#37870 = CARTESIAN_POINT('Ctrl Pts',(-18.2737974644408,31.2379208503873,123.81812345337)) ;
#37871 = CARTESIAN_POINT('Ctrl Pts',(-17.9899251036458,31.0579317699775,123.919685682754)) ;
#37872 = CARTESIAN_POINT('Ctrl Pts',(-18.2210312867946,31.2477826572922,123.617606509006)) ;
#37873 = CARTESIAN_POINT('Ctrl Pts',(-17.923969894662,31.0677935768823,123.669038395276)) ;
#37874 = CARTESIAN_POINT('Ctrl Pts',(-18.2032568478729,31.2577753295979,123.408304026805)) ;
#37875 = CARTESIAN_POINT('Ctrl Pts',(-17.9017545883621,31.0777862491881,123.407409964502)) ;
#37876 = CARTESIAN_POINT('Ctrl Pts',(-18.222001276921,31.2677040005433,123.200401767921)) ;
#37877 = CARTESIAN_POINT('Ctrl Pts',(-17.9251878867363,31.0877149201334,123.147532162206)) ;
#37878 = CARTESIAN_POINT('Ctrl Pts',(-18.2763524420486,31.2776565427686,122.998365459932)) ;
#37879 = CARTESIAN_POINT('Ctrl Pts',(-17.9931295755883,31.0976674623588,122.894987346487)) ;
#37880 = CARTESIAN_POINT('Ctrl Pts',(-18.3653072061262,31.2876578987645,122.807825356539)) ;
#37881 = CARTESIAN_POINT('Ctrl Pts',(-18.1043255908687,31.1076688183546,122.656813330309)) ;
#37882 = CARTESIAN_POINT('Ctrl Pts',(-18.4865417491966,31.2976865110392,122.635347065935)) ;
#37883 = CARTESIAN_POINT('Ctrl Pts',(-18.2558710625167,31.1176974306294,122.441217023583)) ;
#37884 = CARTESIAN_POINT('Ctrl Pts',(-18.6332380965549,31.3075508455887,122.488744885021)) ;
#37885 = CARTESIAN_POINT('Ctrl Pts',(-18.4392436559593,31.1275617651789,122.257966085738)) ;
#37886 = CARTESIAN_POINT('Ctrl Pts',(-18.8051439882642,31.3175431696653,122.36805505233)) ;
#37887 = CARTESIAN_POINT('Ctrl Pts',(-18.6541277020342,31.1375540892555,122.107106052704)) ;
#37888 = CARTESIAN_POINT('Ctrl Pts',(-18.9941591698767,31.3274706620311,122.279486435379)) ;
#37889 = CARTESIAN_POINT('Ctrl Pts',(-18.8903979931556,31.1474815816213,121.996397771836)) ;
#37890 = CARTESIAN_POINT('Ctrl Pts',(-19.1976565576999,31.337498020582,122.224557944539)) ;
#37891 = CARTESIAN_POINT('Ctrl Pts',(-19.1447705223737,31.1575089401722,121.927739862288)) ;
#37892 = CARTESIAN_POINT('Ctrl Pts',(-19.4046860684407,31.3473844386331,122.205835676361)) ;
#37893 = CARTESIAN_POINT('Ctrl Pts',(-19.4035577854677,31.1673953582233,121.904339822877)) ;
#37894 = CARTESIAN_POINT('Ctrl Pts',(-19.6148093834641,31.3574161733685,122.223490530873)) ;
#37895 = CARTESIAN_POINT('Ctrl Pts',(-19.6662117594047,31.1774270929587,121.926411212901)) ;
#37896 = CARTESIAN_POINT('Ctrl Pts',(-19.8157458443054,31.3672977546117,122.27637611023)) ;
#37897 = CARTESIAN_POINT('Ctrl Pts',(-19.9173816828767,31.1873086742019,121.992520931591)) ;
#37898 = CARTESIAN_POINT('Ctrl Pts',(-20.0078493459752,31.3773597326441,122.364859285606)) ;
#37899 = CARTESIAN_POINT('Ctrl Pts',(-20.1575099537051,31.1973706522342,122.103127502603)) ;
#37900 = CARTESIAN_POINT('Ctrl Pts',(-20.1782249889718,31.3872168110058,122.482873113296)) ;
#37901 = CARTESIAN_POINT('Ctrl Pts',(-20.3704779129066,31.207227730596,122.250647114484)) ;
#37902 = CARTESIAN_POINT('Ctrl Pts',(-20.3278279199944,31.3972113841118,122.630365681166)) ;
#37903 = CARTESIAN_POINT('Ctrl Pts',(-20.5574796354709,31.217222303702,122.435014859844)) ;
#37904 = CARTESIAN_POINT('Ctrl Pts',(-20.4488094488748,31.4071371803994,122.800422727047)) ;
#37905 = CARTESIAN_POINT('Ctrl Pts',(-20.7087042531186,31.2271480999896,122.647587798047)) ;
#37906 = CARTESIAN_POINT('Ctrl Pts',(-20.5393550256187,31.4171625475691,122.990728200173)) ;
#37907 = CARTESIAN_POINT('Ctrl Pts',(-20.8218837392503,31.2371734671593,122.885470873047)) ;
#37908 = CARTESIAN_POINT('Ctrl Pts',(-20.5948502492867,31.427058627223,123.191245455736)) ;
#37909 = CARTESIAN_POINT('Ctrl Pts',(-20.8912500206814,31.2470695468132,123.136118325627)) ;
#37910 = CARTESIAN_POINT('Ctrl Pts',(-20.6153065851422,31.4370537069285,123.400378513475)) ;
#37911 = CARTESIAN_POINT('Ctrl Pts',(-20.9168177978967,31.2570646265187,123.397534145114)) ;
#37912 = CARTESIAN_POINT('Ctrl Pts',(-20.5987327650594,31.4470787947444,123.610482201889)) ;
#37913 = CARTESIAN_POINT('Ctrl Pts',(-20.8960973228118,31.2670897143346,123.66016667256)) ;
#37914 = CARTESIAN_POINT('Ctrl Pts',(-20.5297708945593,31.4602626171116,123.878943016611)) ;
#37915 = CARTESIAN_POINT('Ctrl Pts',(-20.8098934767171,31.2802735367018,123.995726533584)) ;
#37916 = CARTESIAN_POINT('Ctrl Pts',(-20.3913865952829,31.4735847352576,124.126114166337)) ;
#37917 = CARTESIAN_POINT('Ctrl Pts',(-20.6369390480792,31.2935956548477,124.304662239596)) ;
#37918 = CARTESIAN_POINT('Ctrl Pts',(-20.1945187909929,31.4869639448852,124.327003652239)) ;
#37919 = CARTESIAN_POINT('Ctrl Pts',(-20.3908148582796,31.3069748644754,124.555818133177)) ;
#37920 = CARTESIAN_POINT('Ctrl Pts',(-20.0266170027822,31.4968021821294,124.447815006563)) ;
#37921 = CARTESIAN_POINT('Ctrl Pts',(-20.1809438415155,31.3168131017196,124.706820601869)) ;
#37922 = CARTESIAN_POINT('Ctrl Pts',(-19.8359227028424,31.5068751053881,124.539840727089)) ;
#37923 = CARTESIAN_POINT('Ctrl Pts',(-19.9425721440024,31.3268860249783,124.821852782607)) ;
#37924 = CARTESIAN_POINT('Ctrl Pts',(-19.6364695609574,31.5167317468432,124.596111822066)) ;
#37925 = CARTESIAN_POINT('Ctrl Pts',(-19.6932575438863,31.3367426664334,124.892188886097)) ;
#37926 = CARTESIAN_POINT('Ctrl Pts',(-19.4276732492853,31.5267171223493,124.617725780505)) ;
#37927 = CARTESIAN_POINT('Ctrl Pts',(-19.4322556852205,31.3467280419395,124.919201640544)) ;
#37928 = CARTESIAN_POINT('Ctrl Pts',(-19.1491517758467,31.5400011538097,124.597557778909)) ;
#37929 = CARTESIAN_POINT('Ctrl Pts',(-19.0841345591843,31.3600120733999,124.89399942422)) ;
#37930 = CARTESIAN_POINT('Ctrl Pts',(-18.8168268265356,31.55651994568,124.4835998274)) ;
#37931 = CARTESIAN_POINT('Ctrl Pts',(-18.6686831094872,31.3765308652702,124.751522351266)) ;
#37932 = CARTESIAN_POINT('Ctrl Pts',(-18.5395236647983,31.5733056626867,124.258964597931)) ;
#37933 = CARTESIAN_POINT('Ctrl Pts',(-18.3221176258068,31.3933165822769,124.470780415022)) ;
#37934 = CARTESIAN_POINT('Ctrl Pts',(-18.3774782260285,31.5864188111957,124.035919217362)) ;
#37935 = CARTESIAN_POINT('Ctrl Pts',(-18.11951716402,31.4064297307859,124.19192546982)) ;
#37936 = CARTESIAN_POINT('Ctrl Pts',(-18.2842368170373,31.5964543602758,123.846684019974)) ;
#37937 = CARTESIAN_POINT('Ctrl Pts',(-18.0029767277988,31.416465279866,123.955390640445)) ;
#37938 = CARTESIAN_POINT('Ctrl Pts',(-18.2259601248409,31.6064704164553,123.644318949324)) ;
#37939 = CARTESIAN_POINT('Ctrl Pts',(-17.9301311612178,31.4264813360454,123.702427282668)) ;
#37940 = CARTESIAN_POINT('Ctrl Pts',(-18.1960923933868,31.6196484523213,123.368912551157)) ;
#37941 = CARTESIAN_POINT('Ctrl Pts',(-17.8927981854037,31.4396593719114,123.358188928684)) ;
#37942 = CARTESIAN_POINT('Ctrl Pts',(-18.2490034102453,31.6362503295084,123.019854463279)) ;
#37943 = CARTESIAN_POINT('Ctrl Pts',(-17.958942776027,31.4562612490985,122.921846253588)) ;
#37944 = CARTESIAN_POINT('Ctrl Pts',(-18.4541225555357,31.6563134741243,122.64582032832)) ;
#37945 = CARTESIAN_POINT('Ctrl Pts',(-18.2153452936245,31.4763243937144,122.454312103311)) ;
#37946 = CARTESIAN_POINT('Ctrl Pts',(-18.7702542503997,31.676114364208,122.367683074125)) ;
#37947 = CARTESIAN_POINT('Ctrl Pts',(-18.6105119795109,31.4961252837982,122.106643007556)) ;
#37948 = CARTESIAN_POINT('Ctrl Pts',(-19.1646379113021,31.6960574894867,122.212071616699)) ;
#37949 = CARTESIAN_POINT('Ctrl Pts',(-19.1034924936839,31.5160684090769,121.912133008528)) ;
#37950 = CARTESIAN_POINT('Ctrl Pts',(-19.5875617432602,31.7159555346063,122.200691268626)) ;
#37951 = CARTESIAN_POINT('Ctrl Pts',(-19.632146534188,31.5359664541965,121.897911371851)) ;
#37952 = CARTESIAN_POINT('Ctrl Pts',(-19.9891315337937,31.735841294233,122.333252820407)) ;
#37953 = CARTESIAN_POINT('Ctrl Pts',(-20.1341066883762,31.5558522138232,122.063616102394)) ;
#37954 = CARTESIAN_POINT('Ctrl Pts',(-20.3238700828937,31.7559064694129,122.597717645849)) ;
#37955 = CARTESIAN_POINT('Ctrl Pts',(-20.5525283111151,31.5759173890031,122.394200252116)) ;
#37956 = CARTESIAN_POINT('Ctrl Pts',(-20.5455304831707,31.7757331125157,122.956392108189)) ;
#37957 = CARTESIAN_POINT('Ctrl Pts',(-20.8296000416623,31.5957440321059,122.84254361494)) ;
#37958 = CARTESIAN_POINT('Ctrl Pts',(-20.6329476537698,31.7956418219641,123.370466525032)) ;
#37959 = CARTESIAN_POINT('Ctrl Pts',(-20.938868749629,31.6156527415543,123.360136077139)) ;
#37960 = CARTESIAN_POINT('Ctrl Pts',(-20.5737577153688,31.8155936589959,123.790666742913)) ;
#37961 = CARTESIAN_POINT('Ctrl Pts',(-20.8648791196571,31.635604578586,123.885385533436)) ;
#37962 = CARTESIAN_POINT('Ctrl Pts',(-20.3736372597136,31.835602133699,124.166043131573)) ;
#37963 = CARTESIAN_POINT('Ctrl Pts',(-20.61472624886,31.6556130532892,124.354604941033)) ;
#37964 = CARTESIAN_POINT('Ctrl Pts',(-20.0609970576513,31.8554035924605,124.448061776785)) ;
#37965 = CARTESIAN_POINT('Ctrl Pts',(-20.2239265792677,31.6754145120507,124.707125000018)) ;
#37966 = CARTESIAN_POINT('Ctrl Pts',(-19.6682512234286,31.8753604806964,124.608723454266)) ;
#37967 = CARTESIAN_POINT('Ctrl Pts',(-19.7329944592296,31.6953714002866,124.907950847029)) ;
#37968 = CARTESIAN_POINT('Ctrl Pts',(-19.2436603324159,31.8953443181105,124.624778169694)) ;
#37969 = CARTESIAN_POINT('Ctrl Pts',(-19.2022559885515,31.7153552377007,124.928017723772)) ;
#37970 = CARTESIAN_POINT('Ctrl Pts',(-18.8422996219988,31.9151527573315,124.496909348728)) ;
#37971 = CARTESIAN_POINT('Ctrl Pts',(-18.7005580952359,31.7351636769217,124.7681819531)) ;
#37972 = CARTESIAN_POINT('Ctrl Pts',(-18.5055590914568,31.9351384667117,124.237910045326)) ;
#37973 = CARTESIAN_POINT('Ctrl Pts',(-18.279632753258,31.7551493863019,124.444432947337)) ;
#37974 = CARTESIAN_POINT('Ctrl Pts',(-18.2784623208037,31.955007989727,123.881451590909)) ;
#37975 = CARTESIAN_POINT('Ctrl Pts',(-17.9957625955385,31.7750189093172,123.998861683827)) ;
#37976 = CARTESIAN_POINT('Ctrl Pts',(-18.1861815675504,31.9750287288442,123.466043557042)) ;
#37977 = CARTESIAN_POINT('Ctrl Pts',(-17.8804111930081,31.7950396484344,123.479601508634)) ;
#37978 = CARTESIAN_POINT('Ctrl Pts',(-18.2401047055373,31.9948327938211,123.04826047757)) ;
#37979 = CARTESIAN_POINT('Ctrl Pts',(-17.9478137324898,31.8148437134113,122.957375358407)) ;
#37980 = CARTESIAN_POINT('Ctrl Pts',(-18.4356159524676,32.0148947575519,122.669266623573)) ;
#37981 = CARTESIAN_POINT('Ctrl Pts',(-18.1922019497026,31.8349056771421,122.483631625213)) ;
#37982 = CARTESIAN_POINT('Ctrl Pts',(-18.7455928392011,32.0347279378404,122.383198650126)) ;
#37983 = CARTESIAN_POINT('Ctrl Pts',(-18.5796705035048,31.8547388574305,122.126047237361)) ;
#37984 = CARTESIAN_POINT('Ctrl Pts',(-19.1356511664417,32.0546471351664,122.218343920433)) ;
#37985 = CARTESIAN_POINT('Ctrl Pts',(-19.0672415406951,31.8746580547566,121.919977102757)) ;
#37986 = CARTESIAN_POINT('Ctrl Pts',(-19.5590376558123,32.0745851602798,122.196738769831)) ;
#37987 = CARTESIAN_POINT('Ctrl Pts',(-19.5964737982828,31.8945960798699,121.892968380633)) ;
#37988 = CARTESIAN_POINT('Ctrl Pts',(-19.9633771695477,32.0944632063358,122.319975235754)) ;
#37989 = CARTESIAN_POINT('Ctrl Pts',(-20.101897742519,31.914474125926,122.04701086148)) ;
#37990 = CARTESIAN_POINT('Ctrl Pts',(-20.3031500801308,32.1144479406239,122.575069386705)) ;
#37991 = CARTESIAN_POINT('Ctrl Pts',(-20.5266155989979,31.9344588602141,122.365876034271)) ;
#37992 = CARTESIAN_POINT('Ctrl Pts',(-20.5347790537855,32.1343587573024,122.929588130013)) ;
#37993 = CARTESIAN_POINT('Ctrl Pts',(-20.8161540517075,31.9543696768926,122.809022005438)) ;
#37994 = CARTESIAN_POINT('Ctrl Pts',(-20.6316344190319,32.1543577328211,123.343539091195)) ;
#37995 = CARTESIAN_POINT('Ctrl Pts',(-20.9372264314163,31.9743686524113,123.326459903435)) ;
#37996 = CARTESIAN_POINT('Ctrl Pts',(-20.5824108030896,32.1741626534663,123.761844882659)) ;
#37997 = CARTESIAN_POINT('Ctrl Pts',(-20.8757007543039,31.9941735730565,123.84934083429)) ;
#37998 = CARTESIAN_POINT('Ctrl Pts',(-20.3923321685515,32.1941466137575,124.141760103579)) ;
#37999 = CARTESIAN_POINT('Ctrl Pts',(-20.638106149318,32.0141575333477,124.324236585246)) ;
#38000 = CARTESIAN_POINT('Ctrl Pts',(-20.0852664590449,32.2140328174815,124.432569654713)) ;
#38001 = CARTESIAN_POINT('Ctrl Pts',(-20.2542774845591,32.0340437370717,124.687750970739)) ;
#38002 = CARTESIAN_POINT('Ctrl Pts',(-19.6964684402798,32.2339819958047,124.602063783456)) ;
#38003 = CARTESIAN_POINT('Ctrl Pts',(-19.7682819396378,32.0539929153948,124.899622390198)) ;
#38004 = CARTESIAN_POINT('Ctrl Pts',(-19.2741435561821,32.2538837950442,124.628548088097)) ;
#38005 = CARTESIAN_POINT('Ctrl Pts',(-19.2403770539428,32.0738947146344,124.932732853873)) ;
#38006 = CARTESIAN_POINT('Ctrl Pts',(-18.8683229480946,32.2737624000966,124.51031319366)) ;
#38007 = CARTESIAN_POINT('Ctrl Pts',(-18.733099358732,32.0937733196867,124.784941726055)) ;
#38008 = CARTESIAN_POINT('Ctrl Pts',(-18.5246822894204,32.2937947598223,124.258593479938)) ;
#38009 = CARTESIAN_POINT('Ctrl Pts',(-18.3035498467092,32.1138056794125,124.470304693614)) ;
#38010 = CARTESIAN_POINT('Ctrl Pts',(-18.3288903417923,32.3103764857783,123.965395680415)) ;
#38011 = CARTESIAN_POINT('Ctrl Pts',(-18.0587930610625,32.1303874053685,124.103782576925)) ;
#38012 = CARTESIAN_POINT('Ctrl Pts',(-18.2389994739994,32.3235706560763,123.702969811419)) ;
#38013 = CARTESIAN_POINT('Ctrl Pts',(-17.9464384609931,32.1435815756664,123.775785395654)) ;
#38014 = CARTESIAN_POINT('Ctrl Pts',(-18.1952099825185,32.3368828341695,123.426608876342)) ;
#38015 = CARTESIAN_POINT('Ctrl Pts',(-17.8916962163373,32.1568937537597,123.430264324838)) ;
#38016 = CARTESIAN_POINT('Ctrl Pts',(-18.2318513898389,32.3534490137628,123.076189005305)) ;
#38017 = CARTESIAN_POINT('Ctrl Pts',(-17.9374894752917,32.173459933353,122.992325212218)) ;
#38018 = CARTESIAN_POINT('Ctrl Pts',(-18.3860665926035,32.370077208623,122.758138167499)) ;
#38019 = CARTESIAN_POINT('Ctrl Pts',(-18.1302718088157,32.1900881282131,122.59470355935)) ;
#38020 = CARTESIAN_POINT('Ctrl Pts',(-18.5689151454784,32.3833657903327,122.546824011485)) ;
#38021 = CARTESIAN_POINT('Ctrl Pts',(-18.35881410566,32.2033767099229,122.330591540725)) ;
#38022 = CARTESIAN_POINT('Ctrl Pts',(-18.7313456924468,32.3933340384363,122.414447869079)) ;
#38023 = CARTESIAN_POINT('Ctrl Pts',(-18.5618539277507,32.2133449580265,122.165112713806)) ;
#38024 = CARTESIAN_POINT('Ctrl Pts',(-18.9132084253142,32.4032487946925,122.312590576436)) ;
#38025 = CARTESIAN_POINT('Ctrl Pts',(-18.7891790717672,32.2232597142826,122.037790375952)) ;
#38026 = CARTESIAN_POINT('Ctrl Pts',(-19.1118736333332,32.4132619453437,122.242954847394)) ;
#38027 = CARTESIAN_POINT('Ctrl Pts',(-19.0375135912556,32.2332728649338,121.950743279244)) ;
#38028 = CARTESIAN_POINT('Ctrl Pts',(-19.3196522724763,32.4232746525457,122.209207410282)) ;
#38029 = CARTESIAN_POINT('Ctrl Pts',(-19.2972230251733,32.2432855721359,121.90855387345)) ;
#38030 = CARTESIAN_POINT('Ctrl Pts',(-19.5975327146755,32.436493941237,122.212420867369)) ;
#38031 = CARTESIAN_POINT('Ctrl Pts',(-19.6446403660518,32.2565048608272,121.912579552322)) ;
#38032 = CARTESIAN_POINT('Ctrl Pts',(-19.9378232247677,32.453112622235,122.307507172536)) ;
#38033 = CARTESIAN_POINT('Ctrl Pts',(-20.0699198327453,32.2731235418252,122.031411460311)) ;
#38034 = CARTESIAN_POINT('Ctrl Pts',(-20.2246076543759,32.4696775300085,122.512015826499)) ;
#38035 = CARTESIAN_POINT('Ctrl Pts',(-20.4284615240683,32.2896884495986,122.287076388231)) ;
#38036 = CARTESIAN_POINT('Ctrl Pts',(-20.4036500534061,32.4830760016193,122.729503286316)) ;
#38037 = CARTESIAN_POINT('Ctrl Pts',(-20.6522321703865,32.3030869212095,122.558907212875)) ;
#38038 = CARTESIAN_POINT('Ctrl Pts',(-20.5055910328036,32.4929172571063,122.909552354167)) ;
#38039 = CARTESIAN_POINT('Ctrl Pts',(-20.779667910958,32.3129281766964,122.78397239338)) ;
#38040 = CARTESIAN_POINT('Ctrl Pts',(-20.5761633681093,32.5029035726945,123.10724493237)) ;
#38041 = CARTESIAN_POINT('Ctrl Pts',(-20.8678841148918,32.3229144922846,123.031085830955)) ;
#38042 = CARTESIAN_POINT('Ctrl Pts',(-20.6112720105989,32.5128401802809,123.313207381497)) ;
#38043 = CARTESIAN_POINT('Ctrl Pts',(-20.9117732133803,32.3328510998711,123.288538866808)) ;
#38044 = CARTESIAN_POINT('Ctrl Pts',(-20.6099679457665,32.5228900476492,123.524461765722)) ;
#38045 = CARTESIAN_POINT('Ctrl Pts',(-20.9101458154303,32.3429009672394,123.552606824045)) ;
#38046 = CARTESIAN_POINT('Ctrl Pts',(-20.5729021146074,32.532740542324,123.728221890654)) ;
#38047 = CARTESIAN_POINT('Ctrl Pts',(-20.8638163143474,32.3527514619142,123.807307622457)) ;
#38048 = CARTESIAN_POINT('Ctrl Pts',(-20.5006629810764,32.5427123427185,123.924992058864)) ;
#38049 = CARTESIAN_POINT('Ctrl Pts',(-20.7735199835642,32.3627232623086,124.053271401058)) ;
#38050 = CARTESIAN_POINT('Ctrl Pts',(-20.3950484487511,32.5527083097443,124.106711975887)) ;
#38051 = CARTESIAN_POINT('Ctrl Pts',(-20.6415042016584,32.3727192293345,124.280422776286)) ;
#38052 = CARTESIAN_POINT('Ctrl Pts',(-20.2587392018978,32.5627457691255,124.267771847846)) ;
#38053 = CARTESIAN_POINT('Ctrl Pts',(-20.4711197707365,32.3827566887157,124.481749462208)) ;
#38054 = CARTESIAN_POINT('Ctrl Pts',(-20.0999386935785,32.5725864700262,124.400395451585)) ;
#38055 = CARTESIAN_POINT('Ctrl Pts',(-20.2726207382354,32.3925973896164,124.647531272465)) ;
#38056 = CARTESIAN_POINT('Ctrl Pts',(-19.9169195431235,32.5826344912936,124.505860717618)) ;
#38057 = CARTESIAN_POINT('Ctrl Pts',(-20.043848162919,32.4026454108838,124.779365278016)) ;
#38058 = CARTESIAN_POINT('Ctrl Pts',(-19.7202317170747,32.5925818843763,124.576913026863)) ;
#38059 = CARTESIAN_POINT('Ctrl Pts',(-19.797989200882,32.4125928039664,124.868183348223)) ;
#38060 = CARTESIAN_POINT('Ctrl Pts',(-19.5150675447947,32.6024920304227,124.613229581171)) ;
#38061 = CARTESIAN_POINT('Ctrl Pts',(-19.5415342218472,32.4225029500128,124.913581797446)) ;
#38062 = CARTESIAN_POINT('Ctrl Pts',(-19.3036192781191,32.6125509442723,124.613134139564)) ;
#38063 = CARTESIAN_POINT('Ctrl Pts',(-19.2772239183681,32.4325618638625,124.913465271253)) ;
#38064 = CARTESIAN_POINT('Ctrl Pts',(-19.0998162930448,32.6223917145616,124.5774017769)) ;
#38065 = CARTESIAN_POINT('Ctrl Pts',(-19.0224693115229,32.4424026341518,124.868802452582)) ;
#38066 = CARTESIAN_POINT('Ctrl Pts',(-18.9008906926549,32.6324545841402,124.505484176666)) ;
#38067 = CARTESIAN_POINT('Ctrl Pts',(-18.7738114255995,32.4524655037304,124.778908029385)) ;
#38068 = CARTESIAN_POINT('Ctrl Pts',(-18.7205888208704,32.6423489072707,124.401712674565)) ;
#38069 = CARTESIAN_POINT('Ctrl Pts',(-18.5484324346337,32.4623598268608,124.649195864333)) ;
#38070 = CARTESIAN_POINT('Ctrl Pts',(-18.5599523550071,32.6522907143652,124.268035857057)) ;
#38071 = CARTESIAN_POINT('Ctrl Pts',(-18.3476349379479,32.4723016339554,124.482101731638)) ;
#38072 = CARTESIAN_POINT('Ctrl Pts',(-18.4240467284614,32.6622932253205,124.107533030312)) ;
#38073 = CARTESIAN_POINT('Ctrl Pts',(-18.177750820169,32.4823041449107,124.281474853477)) ;
#38074 = CARTESIAN_POINT('Ctrl Pts',(-18.3180393506076,32.6723279461389,123.925154810979)) ;
#38075 = CARTESIAN_POINT('Ctrl Pts',(-18.0452392632556,32.492338865729,124.053503454167)) ;
#38076 = CARTESIAN_POINT('Ctrl Pts',(-18.2463535071879,32.6821731236446,123.730976061633)) ;
#38077 = CARTESIAN_POINT('Ctrl Pts',(-17.955629269533,32.5021840432348,123.810780412373)) ;
#38078 = CARTESIAN_POINT('Ctrl Pts',(-18.2085503842841,32.6921578840457,123.524527153024)) ;
#38079 = CARTESIAN_POINT('Ctrl Pts',(-17.9083727783056,32.5121688036358,123.552719582541)) ;
#38080 = CARTESIAN_POINT('Ctrl Pts',(-18.2070734509099,32.7020967903621,123.315553842166)) ;
#38081 = CARTESIAN_POINT('Ctrl Pts',(-17.9065240318063,32.5221077099522,123.291502653979)) ;
#38082 = CARTESIAN_POINT('Ctrl Pts',(-18.2423288903742,32.7121390179978,123.107420822376)) ;
#38083 = CARTESIAN_POINT('Ctrl Pts',(-17.9505907656903,32.532149937588,123.031335993572)) ;
#38084 = CARTESIAN_POINT('Ctrl Pts',(-18.3119535046348,32.7220242295822,122.91158798625)) ;
#38085 = CARTESIAN_POINT('Ctrl Pts',(-18.0376192935989,32.5420351491723,122.786543593537)) ;
#38086 = CARTESIAN_POINT('Ctrl Pts',(-18.4154411859655,32.7320231597841,122.728653020651)) ;
#38087 = CARTESIAN_POINT('Ctrl Pts',(-18.1669767555534,32.5520340793743,122.557873550003)) ;
#38088 = CARTESIAN_POINT('Ctrl Pts',(-18.5479494903237,32.7419405826945,122.567636304584)) ;
#38089 = CARTESIAN_POINT('Ctrl Pts',(-18.3326104946067,32.5619515022847,122.356600741691)) ;
#38090 = CARTESIAN_POINT('Ctrl Pts',(-18.7084645463627,32.7519885147733,122.430363552934)) ;
#38091 = CARTESIAN_POINT('Ctrl Pts',(-18.5332526173414,32.5719994343634,122.18500796692)) ;
#38092 = CARTESIAN_POINT('Ctrl Pts',(-18.8872415852668,32.7618658905827,122.324659315536)) ;
#38093 = CARTESIAN_POINT('Ctrl Pts',(-18.7567232186998,32.5818768101728,122.052875232576)) ;
#38094 = CARTESIAN_POINT('Ctrl Pts',(-19.0850258483024,32.7719197837506,122.25022120339)) ;
#38095 = CARTESIAN_POINT('Ctrl Pts',(-19.0039525695747,32.5919307033408,121.959825361335)) ;
#38096 = CARTESIAN_POINT('Ctrl Pts',(-19.2894783129814,32.7818134070039,122.211767437767)) ;
#38097 = CARTESIAN_POINT('Ctrl Pts',(-19.2595182815771,32.601824326594,121.91175567857)) ;
#38098 = CARTESIAN_POINT('Ctrl Pts',(-19.5009779859704,32.7918760006269,122.209324968633)) ;
#38099 = CARTESIAN_POINT('Ctrl Pts',(-19.5238926627114,32.611886920217,121.908700188331)) ;
#38100 = CARTESIAN_POINT('Ctrl Pts',(-19.7051996408792,32.8017185746159,122.242795102334)) ;
#38101 = CARTESIAN_POINT('Ctrl Pts',(-19.7791709674266,32.6217294942061,121.950535647237)) ;
#38102 = CARTESIAN_POINT('Ctrl Pts',(-19.9035645751163,32.8117093314989,122.311756543246)) ;
#38103 = CARTESIAN_POINT('Ctrl Pts',(-20.0271280441741,32.631720251089,122.036735366564)) ;
#38104 = CARTESIAN_POINT('Ctrl Pts',(-20.0858058022882,32.8216373932568,122.41352070292)) ;
#38105 = CARTESIAN_POINT('Ctrl Pts',(-20.2549311094076,32.641648312847,122.163938821272)) ;
#38106 = CARTESIAN_POINT('Ctrl Pts',(-20.2488151784822,32.831625369146,122.545893277075)) ;
#38107 = CARTESIAN_POINT('Ctrl Pts',(-20.4586943445839,32.6516362887362,122.329402962542)) ;
#38108 = CARTESIAN_POINT('Ctrl Pts',(-20.3867446811956,32.8416610335024,122.705536508051)) ;
#38109 = CARTESIAN_POINT('Ctrl Pts',(-20.6311078852377,32.6616719530926,122.528955452301)) ;
#38110 = CARTESIAN_POINT('Ctrl Pts',(-20.4932113035389,32.8515169719221,122.883306696087)) ;
#38111 = CARTESIAN_POINT('Ctrl Pts',(-20.7641935054107,32.6715278915122,122.751167847441)) ;
#38112 = CARTESIAN_POINT('Ctrl Pts',(-20.5685516723176,32.861512463319,123.079449372689)) ;
#38113 = CARTESIAN_POINT('Ctrl Pts',(-20.8583709771004,32.6815233829091,122.996345583819)) ;
#38114 = CARTESIAN_POINT('Ctrl Pts',(-20.6084146945894,32.8714222682724,123.283945522481)) ;
#38115 = CARTESIAN_POINT('Ctrl Pts',(-20.9082019159702,32.6914331878626,123.251966021341)) ;
#38116 = CARTESIAN_POINT('Ctrl Pts',(-20.6125455527865,32.8814344905392,123.494398317047)) ;
#38117 = CARTESIAN_POINT('Ctrl Pts',(-20.9133674663854,32.7014454101294,123.515032024861)) ;
#38118 = CARTESIAN_POINT('Ctrl Pts',(-20.5796147863066,32.891462371232,123.702629937833)) ;
#38119 = CARTESIAN_POINT('Ctrl Pts',(-20.8722060910086,32.7114732908222,123.775321815861)) ;
#38120 = CARTESIAN_POINT('Ctrl Pts',(-20.512536676068,32.9013187672146,123.898683038546)) ;
#38121 = CARTESIAN_POINT('Ctrl Pts',(-20.7883600168508,32.7213296868048,124.020389778682)) ;
#38122 = CARTESIAN_POINT('Ctrl Pts',(-20.4111096637263,32.9113435643946,124.083427639594)) ;
#38123 = CARTESIAN_POINT('Ctrl Pts',(-20.6615779008466,32.7313544839848,124.251321404654)) ;
#38124 = CARTESIAN_POINT('Ctrl Pts',(-20.2786586384408,32.9213744943784,124.247533456191)) ;
#38125 = CARTESIAN_POINT('Ctrl Pts',(-20.496015737572,32.7413854139686,124.456454889793)) ;
#38126 = CARTESIAN_POINT('Ctrl Pts',(-20.1229354505894,32.931219096887,124.38384374608)) ;
#38127 = CARTESIAN_POINT('Ctrl Pts',(-20.3013621684874,32.7512300164772,124.626844922509)) ;
#38128 = CARTESIAN_POINT('Ctrl Pts',(-19.9435638207466,32.9412099481111,124.493133513568)) ;
#38129 = CARTESIAN_POINT('Ctrl Pts',(-20.0771483651053,32.7612208677013,124.763458712238)) ;
#38130 = CARTESIAN_POINT('Ctrl Pts',(-19.7468547735515,32.9512477811224,124.569535084003)) ;
#38131 = CARTESIAN_POINT('Ctrl Pts',(-19.8312628601303,32.7712587007126,124.858962378783)) ;
#38132 = CARTESIAN_POINT('Ctrl Pts',(-19.5439187927745,32.9610921695878,124.610185963789)) ;
#38133 = CARTESIAN_POINT('Ctrl Pts',(-19.5775920832563,32.781103089178,124.90977793786)) ;
#38134 = CARTESIAN_POINT('Ctrl Pts',(-19.3341011134292,32.9710769739574,124.615465585142)) ;
#38135 = CARTESIAN_POINT('Ctrl Pts',(-19.3153197757282,32.7910878935475,124.916379101502)) ;
#38136 = CARTESIAN_POINT('Ctrl Pts',(-19.1274257911367,32.9810164934402,124.584456615172)) ;
#38137 = CARTESIAN_POINT('Ctrl Pts',(-19.0569748481589,32.8010274130304,124.87761938897)) ;
#38138 = CARTESIAN_POINT('Ctrl Pts',(-18.927334989013,32.9910562244416,124.517330597724)) ;
#38139 = CARTESIAN_POINT('Ctrl Pts',(-18.8068609697221,32.8110671440317,124.793713447286)) ;
#38140 = CARTESIAN_POINT('Ctrl Pts',(-18.7446634407344,33.0009443526879,124.418083254216)) ;
#38141 = CARTESIAN_POINT('Ctrl Pts',(-18.5785199696403,32.820955272278,124.669655218492)) ;
#38142 = CARTESIAN_POINT('Ctrl Pts',(-18.5801005857967,33.0109340778964,124.28761411625)) ;
#38143 = CARTESIAN_POINT('Ctrl Pts',(-18.3728153330227,32.8309449974866,124.506569798972)) ;
#38144 = CARTESIAN_POINT('Ctrl Pts',(-18.4412469443852,33.0208918425979,124.130951753119)) ;
#38145 = CARTESIAN_POINT('Ctrl Pts',(-18.1992468677695,32.8409027621881,124.3107425181)) ;
#38146 = CARTESIAN_POINT('Ctrl Pts',(-18.3318926647563,33.0307941840099,123.9538000731)) ;
#38147 = CARTESIAN_POINT('Ctrl Pts',(-18.0625524287455,32.8508051036001,124.089302873822)) ;
#38148 = CARTESIAN_POINT('Ctrl Pts',(-18.2538818671851,33.0408383797163,123.757588934328)) ;
#38149 = CARTESIAN_POINT('Ctrl Pts',(-17.9650377613025,32.8608492993064,123.844039624729)) ;
#38150 = CARTESIAN_POINT('Ctrl Pts',(-18.2116804220347,33.0507457804755,123.553613209322)) ;
#38151 = CARTESIAN_POINT('Ctrl Pts',(-17.9122844842021,32.8707567000657,123.589069438269)) ;
#38152 = CARTESIAN_POINT('Ctrl Pts',(-18.2051029806548,33.0607563803499,123.343258587515)) ;
#38153 = CARTESIAN_POINT('Ctrl Pts',(-17.9040614840554,32.8807672999401,123.326126151245)) ;
#38154 = CARTESIAN_POINT('Ctrl Pts',(-18.2356129749223,33.0707866762621,123.134602723717)) ;
#38155 = CARTESIAN_POINT('Ctrl Pts',(-17.942197627279,32.8907975958523,123.0653062275)) ;
#38156 = CARTESIAN_POINT('Ctrl Pts',(-18.300450441629,33.0806414559118,122.937844780199)) ;
#38157 = CARTESIAN_POINT('Ctrl Pts',(-18.0232436734784,32.900652375502,122.819357208216)) ;
#38158 = CARTESIAN_POINT('Ctrl Pts',(-18.3989330999902,33.0905987841293,122.753115564655)) ;
#38159 = CARTESIAN_POINT('Ctrl Pts',(-18.146346329286,32.9106097037195,122.588444800314)) ;
#38160 = CARTESIAN_POINT('Ctrl Pts',(-18.5293347628917,33.1006378170362,122.587186806717)) ;
#38161 = CARTESIAN_POINT('Ctrl Pts',(-18.3093474041902,32.9206487366264,122.381033273933)) ;
#38162 = CARTESIAN_POINT('Ctrl Pts',(-18.6837449458525,33.1105109289255,122.44842798728)) ;
#38163 = CARTESIAN_POINT('Ctrl Pts',(-18.5023603004439,32.9305218485156,122.207583253735)) ;
#38164 = CARTESIAN_POINT('Ctrl Pts',(-18.8634428506156,33.1205842139526,122.336455552253)) ;
#38165 = CARTESIAN_POINT('Ctrl Pts',(-18.7269817759112,32.9405951335427,122.067617063603)) ;
#38166 = CARTESIAN_POINT('Ctrl Pts',(-19.0549009830223,33.1304045336893,122.259087158195)) ;
#38167 = CARTESIAN_POINT('Ctrl Pts',(-18.9663055363754,32.9504154532795,121.970905134064)) ;
#38168 = CARTESIAN_POINT('Ctrl Pts',(-19.2620617743464,33.1404831990678,122.214836805238)) ;
#38169 = CARTESIAN_POINT('Ctrl Pts',(-19.2252558871438,32.960494118658,121.915591458539)) ;
#38170 = CARTESIAN_POINT('Ctrl Pts',(-19.4690858066591,33.1503347895516,122.207323763932)) ;
#38171 = CARTESIAN_POINT('Ctrl Pts',(-19.4840372151906,32.9703457091417,121.906199287726)) ;
#38172 = CARTESIAN_POINT('Ctrl Pts',(-19.6788221961635,33.1604079398705,122.236318117315)) ;
#38173 = CARTESIAN_POINT('Ctrl Pts',(-19.7462073717057,32.9804188594607,121.942441422223)) ;
#38174 = CARTESIAN_POINT('Ctrl Pts',(-19.8757676666468,33.1702503198455,122.29984587334)) ;
#38175 = CARTESIAN_POINT('Ctrl Pts',(-19.9923907934108,32.9902612394357,122.021850824129)) ;
#38176 = CARTESIAN_POINT('Ctrl Pts',(-20.0615568423931,33.1802312960886,122.397340048121)) ;
#38177 = CARTESIAN_POINT('Ctrl Pts',(-20.2246277641861,33.0002422156788,122.14371824194)) ;
#38178 = CARTESIAN_POINT('Ctrl Pts',(-20.2279876372291,33.1902476244439,122.526364012805)) ;
#38179 = CARTESIAN_POINT('Ctrl Pts',(-20.4326666594607,33.010258544034,122.304997705709)) ;
#38180 = CARTESIAN_POINT('Ctrl Pts',(-20.3679958704936,33.200145421435,122.680288715959)) ;
#38181 = CARTESIAN_POINT('Ctrl Pts',(-20.6076780089527,33.0201563410252,122.497403957901)) ;
#38182 = CARTESIAN_POINT('Ctrl Pts',(-20.4807568430483,33.2101579781671,122.858052147058)) ;
#38183 = CARTESIAN_POINT('Ctrl Pts',(-20.748629570093,33.0301688977572,122.719608055102)) ;
#38184 = CARTESIAN_POINT('Ctrl Pts',(-20.5606237614743,33.2201900130135,123.053239269694)) ;
#38185 = CARTESIAN_POINT('Ctrl Pts',(-20.8484637131668,33.0402009326037,122.963591613867)) ;
#38186 = CARTESIAN_POINT('Ctrl Pts',(-20.6050359521563,33.230029413829,123.255287016282)) ;
#38187 = CARTESIAN_POINT('Ctrl Pts',(-20.9039796444684,33.0500403334192,123.216152649284)) ;
#38188 = CARTESIAN_POINT('Ctrl Pts',(-20.614049092095,33.2400951994806,123.466685199039)) ;
#38189 = CARTESIAN_POINT('Ctrl Pts',(-20.915246377554,33.0601061190708,123.480399984262)) ;
#38190 = CARTESIAN_POINT('Ctrl Pts',(-20.5866016199623,33.2499856545952,123.672815882505)) ;
#38191 = CARTESIAN_POINT('Ctrl Pts',(-20.8809372576275,33.0699965741854,123.738064421182)) ;
#38192 = CARTESIAN_POINT('Ctrl Pts',(-20.5235744358789,33.2599777732309,123.873192435292)) ;
#38193 = CARTESIAN_POINT('Ctrl Pts',(-20.8021533890581,33.0799886928211,123.98853537264)) ;
#38194 = CARTESIAN_POINT('Ctrl Pts',(-20.4268201921986,33.269940599994,124.058949341531)) ;
#38195 = CARTESIAN_POINT('Ctrl Pts',(-20.6812106073912,33.0899515195842,124.22073203139)) ;
#38196 = CARTESIAN_POINT('Ctrl Pts',(-20.3004366840512,33.2798448832669,124.224447351388)) ;
#38197 = CARTESIAN_POINT('Ctrl Pts',(-20.5232306933869,33.0998558028571,124.427605321888)) ;
#38198 = CARTESIAN_POINT('Ctrl Pts',(-20.1447295418141,33.289905317214,124.36754765931)) ;
#38199 = CARTESIAN_POINT('Ctrl Pts',(-20.3285971107934,33.1099162368042,124.60648055999)) ;
#38200 = CARTESIAN_POINT('Ctrl Pts',(-19.9705348461401,33.2997458698872,124.479200573106)) ;
#38201 = CARTESIAN_POINT('Ctrl Pts',(-20.1108525131873,33.1197567894774,124.746047511575)) ;
#38202 = CARTESIAN_POINT('Ctrl Pts',(-19.7754486620415,33.3098080898329,124.560937015525)) ;
#38203 = CARTESIAN_POINT('Ctrl Pts',(-19.8669950901553,33.129819009423,124.848217841125)) ;
#38204 = CARTESIAN_POINT('Ctrl Pts',(-19.57243885132,33.3197052291114,124.606588971433)) ;
#38205 = CARTESIAN_POINT('Ctrl Pts',(-19.613231849326,33.1397161487016,124.905283007281)) ;
#38206 = CARTESIAN_POINT('Ctrl Pts',(-19.3639189425878,33.3296364212465,124.61702574814)) ;
#38207 = CARTESIAN_POINT('Ctrl Pts',(-19.3525812289546,33.1496473408367,124.918328736753)) ;
#38208 = CARTESIAN_POINT('Ctrl Pts',(-19.1544701914488,33.3396785758916,124.5905747195)) ;
#38209 = CARTESIAN_POINT('Ctrl Pts',(-19.0907705220103,33.1596894954817,124.885264797478)) ;
#38210 = CARTESIAN_POINT('Ctrl Pts',(-18.9558448503062,33.3495653369109,124.529280922673)) ;
#38211 = CARTESIAN_POINT('Ctrl Pts',(-18.8424878708844,33.169576256501,124.808646986512)) ;
#38212 = CARTESIAN_POINT('Ctrl Pts',(-18.7686911463768,33.3595646386281,124.433610207421)) ;
#38213 = CARTESIAN_POINT('Ctrl Pts',(-18.6085457634683,33.1795755582183,124.689058201109)) ;
#38214 = CARTESIAN_POINT('Ctrl Pts',(-18.6021783660485,33.3694854367949,124.307970432937)) ;
#38215 = CARTESIAN_POINT('Ctrl Pts',(-18.4004044123942,33.189496356385,124.532007686326)) ;
#38216 = CARTESIAN_POINT('Ctrl Pts',(-18.4584063019832,33.3795194903916,124.153637802788)) ;
#38217 = CARTESIAN_POINT('Ctrl Pts',(-18.2206897369565,33.1995304099818,124.339091715011)) ;
#38218 = CARTESIAN_POINT('Ctrl Pts',(-18.3447487639094,33.389442607958,123.978664957015)) ;
#38219 = CARTESIAN_POINT('Ctrl Pts',(-18.0786177880048,33.2094535275481,124.120374761403)) ;
#38220 = CARTESIAN_POINT('Ctrl Pts',(-18.262168874499,33.3994987314571,123.784072019688)) ;
#38221 = CARTESIAN_POINT('Ctrl Pts',(-17.9753934549704,33.2195096510473,123.877133689794)) ;
#38222 = CARTESIAN_POINT('Ctrl Pts',(-18.2155327305873,33.4093441731119,123.582403847225)) ;
#38223 = CARTESIAN_POINT('Ctrl Pts',(-17.9170984303187,33.2293550927021,123.625046988964)) ;
#38224 = CARTESIAN_POINT('Ctrl Pts',(-18.203805100798,33.4193064742361,123.373306871914)) ;
#38225 = CARTESIAN_POINT('Ctrl Pts',(-17.9024396208833,33.2393173938262,123.36367527573)) ;
#38226 = CARTESIAN_POINT('Ctrl Pts',(-18.2290055597389,33.4293349535112,123.163973793253)) ;
#38227 = CARTESIAN_POINT('Ctrl Pts',(-17.9339408231796,33.2493458731014,123.102009100118)) ;
#38228 = CARTESIAN_POINT('Ctrl Pts',(-18.289374518782,33.4392453070209,122.96457571185)) ;
#38229 = CARTESIAN_POINT('Ctrl Pts',(-18.0094029196339,33.2592562266111,122.852760854064)) ;
#38230 = CARTESIAN_POINT('Ctrl Pts',(-18.3832010117499,33.4491801791981,122.777967476055)) ;
#38231 = CARTESIAN_POINT('Ctrl Pts',(-18.1266871223005,33.2691910987883,122.619500365628)) ;
#38232 = CARTESIAN_POINT('Ctrl Pts',(-18.5094881208649,33.4592213167838,122.60882144455)) ;
#38233 = CARTESIAN_POINT('Ctrl Pts',(-18.2845465433312,33.2792322363739,122.408068459488)) ;
#38234 = CARTESIAN_POINT('Ctrl Pts',(-18.6607816210844,33.4691084659983,122.466272054033)) ;
#38235 = CARTESIAN_POINT('Ctrl Pts',(-18.4736647675595,33.2891193855885,122.229881635871)) ;
#38236 = CARTESIAN_POINT('Ctrl Pts',(-18.8361603645087,33.4791007007494,122.350665197575)) ;
#38237 = CARTESIAN_POINT('Ctrl Pts',(-18.6928889148364,33.2991116203396,122.085373784638)) ;
#38238 = CARTESIAN_POINT('Ctrl Pts',(-19.0281558133508,33.4890494063124,122.267675696057)) ;
#38239 = CARTESIAN_POINT('Ctrl Pts',(-18.9328841091026,33.3090603259026,121.981637584329)) ;
#38240 = CARTESIAN_POINT('Ctrl Pts',(-19.2312903333038,33.4989854747361,122.219054749115)) ;
#38241 = CARTESIAN_POINT('Ctrl Pts',(-19.1868031331722,33.3189963943262,121.920862306475)) ;
#38242 = CARTESIAN_POINT('Ctrl Pts',(-19.4408438884127,33.5089711589519,122.206138288306)) ;
#38243 = CARTESIAN_POINT('Ctrl Pts',(-19.4487454010875,33.328982078542,121.904717887732)) ;
#38244 = CARTESIAN_POINT('Ctrl Pts',(-19.6505310611523,33.5190115855205,122.230262302281)) ;
#38245 = CARTESIAN_POINT('Ctrl Pts',(-19.7108540776714,33.3390225051107,121.934873930114)) ;
#38246 = CARTESIAN_POINT('Ctrl Pts',(-19.8489000133317,33.5288506989843,122.288894555747)) ;
#38247 = CARTESIAN_POINT('Ctrl Pts',(-19.958816242514,33.3488616185744,122.008165761132)) ;
#38248 = CARTESIAN_POINT('Ctrl Pts',(-20.0378734404374,33.5388804331601,122.382439401842)) ;
#38249 = CARTESIAN_POINT('Ctrl Pts',(-20.1950323308035,33.3588913527503,122.125097981802)) ;
#38250 = CARTESIAN_POINT('Ctrl Pts',(-20.2072755150805,33.548902532666,122.50771918548)) ;
#38251 = CARTESIAN_POINT('Ctrl Pts',(-20.4067842186,33.3689134522561,122.281698617099)) ;
#38252 = CARTESIAN_POINT('Ctrl Pts',(-20.3505163323491,33.5587709725594,122.657820476515)) ;
#38253 = CARTESIAN_POINT('Ctrl Pts',(-20.5858350553215,33.3787818921496,122.469326974314)) ;
#38254 = CARTESIAN_POINT('Ctrl Pts',(-20.467830910548,33.568839837245,122.833994863383)) ;
#38255 = CARTESIAN_POINT('Ctrl Pts',(-20.732476955255,33.3888507568352,122.689545385332)) ;
#38256 = CARTESIAN_POINT('Ctrl Pts',(-20.5508822742983,33.5786825103436,123.023527927505)) ;
#38257 = CARTESIAN_POINT('Ctrl Pts',(-20.8362904560679,33.3986934299338,122.926463443112)) ;
#38258 = CARTESIAN_POINT('Ctrl Pts',(-20.6010906324588,33.5886431445061,123.226819066084)) ;
#38259 = CARTESIAN_POINT('Ctrl Pts',(-20.8990494416422,33.4086540640963,123.180578146972)) ;
#38260 = CARTESIAN_POINT('Ctrl Pts',(-20.6149332523502,33.5986810601842,123.437385843915)) ;
#38261 = CARTESIAN_POINT('Ctrl Pts',(-20.9163512491307,33.4186919797744,123.443786581485)) ;
#38262 = CARTESIAN_POINT('Ctrl Pts',(-20.5927561143563,33.6085553350436,123.64381161214)) ;
#38263 = CARTESIAN_POINT('Ctrl Pts',(-20.8886281344134,33.4285662546338,123.701819630234)) ;
#38264 = CARTESIAN_POINT('Ctrl Pts',(-20.5339350999099,33.6186250854188,123.847144174352)) ;
#38265 = CARTESIAN_POINT('Ctrl Pts',(-20.8151004365059,33.438636005009,123.955984554738)) ;
#38266 = CARTESIAN_POINT('Ctrl Pts',(-20.4429721196494,33.6284583807933,124.032801166583)) ;
#38267 = CARTESIAN_POINT('Ctrl Pts',(-20.7013946873049,33.4484693003834,124.188056231811)) ;
#38268 = CARTESIAN_POINT('Ctrl Pts',(-20.3192120120837,33.6384886782729,124.203524561785)) ;
#38269 = CARTESIAN_POINT('Ctrl Pts',(-20.546693129782,33.4584995978631,124.401459336324)) ;
#38270 = CARTESIAN_POINT('Ctrl Pts',(-20.1672189301495,33.6485207647143,124.34975537749)) ;
#38271 = CARTESIAN_POINT('Ctrl Pts',(-20.3567007162812,33.4685316843045,124.584246630781)) ;
#38272 = CARTESIAN_POINT('Ctrl Pts',(-19.9959765672418,33.6583486932033,124.465347265226)) ;
#38273 = CARTESIAN_POINT('Ctrl Pts',(-20.1426457143596,33.4783596127934,124.728735741581)) ;
#38274 = CARTESIAN_POINT('Ctrl Pts',(-19.8042599262361,33.668344734314,124.551406477392)) ;
#38275 = CARTESIAN_POINT('Ctrl Pts',(-19.9029989792724,33.4883556539042,124.836308043076)) ;
#38276 = CARTESIAN_POINT('Ctrl Pts',(-19.5997986838968,33.6783705464153,124.602630095532)) ;
#38277 = CARTESIAN_POINT('Ctrl Pts',(-19.6474220237425,33.4983814660054,124.900335793368)) ;
#38278 = CARTESIAN_POINT('Ctrl Pts',(-19.3924774849365,33.6882577813101,124.617636375072)) ;
#38279 = CARTESIAN_POINT('Ctrl Pts',(-19.3882695560043,33.5082687009003,124.919091810122)) ;
#38280 = CARTESIAN_POINT('Ctrl Pts',(-19.1838086719246,33.6982346475211,124.59657238943)) ;
#38281 = CARTESIAN_POINT('Ctrl Pts',(-19.1274334857546,33.5182455671113,124.892759807701)) ;
#38282 = CARTESIAN_POINT('Ctrl Pts',(-18.9815887866603,33.7082275913929,124.539527650244)) ;
#38283 = CARTESIAN_POINT('Ctrl Pts',(-18.8746590268062,33.5282385109831,124.82145190794)) ;
#38284 = CARTESIAN_POINT('Ctrl Pts',(-18.7916507877663,33.7182655140643,124.447604623788)) ;
#38285 = CARTESIAN_POINT('Ctrl Pts',(-18.6372374521319,33.5382764336545,124.706546424566)) ;
#38286 = CARTESIAN_POINT('Ctrl Pts',(-18.6235800416685,33.728113978326,124.326664479328)) ;
#38287 = CARTESIAN_POINT('Ctrl Pts',(-18.4271493677477,33.5481248979162,124.555368999673)) ;
#38288 = CARTESIAN_POINT('Ctrl Pts',(-18.4767212967357,33.73810584507,124.17651438228)) ;
#38289 = CARTESIAN_POINT('Ctrl Pts',(-18.2435773438857,33.5581167646602,124.367679767464)) ;
#38290 = CARTESIAN_POINT('Ctrl Pts',(-18.3589139649517,33.7480235771112,124.004451145981)) ;
#38291 = CARTESIAN_POINT('Ctrl Pts',(-18.0963196368505,33.5680344967013,124.152599028202)) ;
#38292 = CARTESIAN_POINT('Ctrl Pts',(-18.2717798858509,33.7580517620064,123.812495005014)) ;
#38293 = CARTESIAN_POINT('Ctrl Pts',(-17.9874040347647,33.5780626815966,123.91265298461)) ;
#38294 = CARTESIAN_POINT('Ctrl Pts',(-18.2199583948153,33.7679369200553,123.611237430731)) ;
#38295 = CARTESIAN_POINT('Ctrl Pts',(-17.9226291155183,33.5879478396455,123.661079753406)) ;
#38296 = CARTESIAN_POINT('Ctrl Pts',(-18.2031899992664,33.777926280597,123.401895935145)) ;
#38297 = CARTESIAN_POINT('Ctrl Pts',(-17.9016709287032,33.5979372001872,123.399402541443)) ;
#38298 = CARTESIAN_POINT('Ctrl Pts',(-18.2235716353926,33.7879674375313,123.191785549963)) ;
#38299 = CARTESIAN_POINT('Ctrl Pts',(-17.9271501703905,33.6079783571215,123.136764865885)) ;
#38300 = CARTESIAN_POINT('Ctrl Pts',(-18.2786200114163,33.7978000209865,122.992541931651)) ;
#38301 = CARTESIAN_POINT('Ctrl Pts',(-17.9959631146124,33.6178109405767,122.887710030795)) ;
#38302 = CARTESIAN_POINT('Ctrl Pts',(-18.3683487595105,33.8077942409485,122.802558224902)) ;
#38303 = CARTESIAN_POINT('Ctrl Pts',(-18.1081263092471,33.6278051605386,122.650231330514)) ;
#38304 = CARTESIAN_POINT('Ctrl Pts',(-18.4904696258343,33.8178223427358,122.63070110739)) ;
#38305 = CARTESIAN_POINT('Ctrl Pts',(-18.2607792874673,33.6378332623259,122.435411305437)) ;
#38306 = CARTESIAN_POINT('Ctrl Pts',(-18.6381482308556,33.8277022873588,122.484636845884)) ;
#38307 = CARTESIAN_POINT('Ctrl Pts',(-18.4453797141008,33.647713206949,122.252832221306)) ;
#38308 = CARTESIAN_POINT('Ctrl Pts',(-18.8106558657306,33.8376926139159,122.364855145629)) ;
#38309 = CARTESIAN_POINT('Ctrl Pts',(-18.6610157890735,33.6577035335061,122.103107051282)) ;
#38310 = CARTESIAN_POINT('Ctrl Pts',(-19.0004133748142,33.8476335455702,122.277272733612)) ;
#38311 = CARTESIAN_POINT('Ctrl Pts',(-18.8982140304838,33.6676444651604,121.993631136428)) ;
#38312 = CARTESIAN_POINT('Ctrl Pts',(-19.2033679275045,33.8576206640731,122.223428561579)) ;
#38313 = CARTESIAN_POINT('Ctrl Pts',(-19.1519080089665,33.6776315836633,121.926328336062)) ;
#38314 = CARTESIAN_POINT('Ctrl Pts',(-19.413555239702,33.8676539969703,122.205893497392)) ;
#38315 = CARTESIAN_POINT('Ctrl Pts',(-19.4146423301782,33.6876649165604,121.90441196927)) ;
#38316 = CARTESIAN_POINT('Ctrl Pts',(-19.6201683892138,33.877520101415,122.224398460952)) ;
#38317 = CARTESIAN_POINT('Ctrl Pts',(-19.6729091690193,33.6975310210052,121.927545767078)) ;
#38318 = CARTESIAN_POINT('Ctrl Pts',(-19.824456202544,33.8875862152953,122.279533485596)) ;
#38319 = CARTESIAN_POINT('Ctrl Pts',(-19.928268124028,33.7075971348855,121.996466980222)) ;
#38320 = CARTESIAN_POINT('Ctrl Pts',(-20.0121077833752,33.8974422270637,122.367434002635)) ;
#38321 = CARTESIAN_POINT('Ctrl Pts',(-20.1628320829967,33.7174531466539,122.106345209842)) ;
#38322 = CARTESIAN_POINT('Ctrl Pts',(-20.1843716366312,33.9074369306951,122.487738822849)) ;
#38323 = CARTESIAN_POINT('Ctrl Pts',(-20.3781604556109,33.7274478502852,122.256728476935)) ;
#38324 = CARTESIAN_POINT('Ctrl Pts',(-20.3333627134761,33.9174682664199,122.63699684848)) ;
#38325 = CARTESIAN_POINT('Ctrl Pts',(-20.5643974693721,33.7374791860101,122.443302838749)) ;
#38326 = CARTESIAN_POINT('Ctrl Pts',(-20.4524620397036,33.9273347916236,122.806830884017)) ;
#38327 = CARTESIAN_POINT('Ctrl Pts',(-20.71326976199,33.7473457112138,122.655597325684)) ;
#38328 = CARTESIAN_POINT('Ctrl Pts',(-20.5416324218957,33.9373222196694,122.996895065908)) ;
#38329 = CARTESIAN_POINT('Ctrl Pts',(-20.8247303533293,33.7573331392596,122.8931788086)) ;
#38330 = CARTESIAN_POINT('Ctrl Pts',(-20.5963371639424,33.9472671493558,123.198716985131)) ;
#38331 = CARTESIAN_POINT('Ctrl Pts',(-20.893108733767,33.767278068946,123.145457142125)) ;
#38332 = CARTESIAN_POINT('Ctrl Pts',(-20.615233404167,33.9573120674643,123.409025558996)) ;
#38333 = CARTESIAN_POINT('Ctrl Pts',(-20.9167263519212,33.7773229870545,123.408343079754)) ;
#38334 = CARTESIAN_POINT('Ctrl Pts',(-20.5978343581406,33.9671740370782,123.615640699636)) ;
#38335 = CARTESIAN_POINT('Ctrl Pts',(-20.8949748057221,33.7871849566684,123.666612207496)) ;
#38336 = CARTESIAN_POINT('Ctrl Pts',(-20.5445304522243,33.9771661050995,123.818808413641)) ;
#38337 = CARTESIAN_POINT('Ctrl Pts',(-20.8283422293849,33.7971770246896,123.920571241205)) ;
#38338 = CARTESIAN_POINT('Ctrl Pts',(-20.4572488945019,33.987097030474,124.008482314326)) ;
#38339 = CARTESIAN_POINT('Ctrl Pts',(-20.7192376865888,33.8071079500642,124.157662672226)) ;
#38340 = CARTESIAN_POINT('Ctrl Pts',(-20.3384279441806,33.9970476586975,124.180637038288)) ;
#38341 = CARTESIAN_POINT('Ctrl Pts',(-20.5707091130327,33.8170585782876,124.372854625931)) ;
#38342 = CARTESIAN_POINT('Ctrl Pts',(-20.1908473350017,34.0070478977566,124.330400148074)) ;
#38343 = CARTESIAN_POINT('Ctrl Pts',(-20.3862313186924,33.8270588173468,124.560056609372)) ;
#38344 = CARTESIAN_POINT('Ctrl Pts',(-20.0188703479351,34.0170763531258,124.452341161375)) ;
#38345 = CARTESIAN_POINT('Ctrl Pts',(-20.1712584195918,33.837087272716,124.712480635238)) ;
#38346 = CARTESIAN_POINT('Ctrl Pts',(-19.8315368351169,34.026942387709,124.541398156012)) ;
#38347 = CARTESIAN_POINT('Ctrl Pts',(-19.9370901885527,33.8469533072992,124.823799494595)) ;
#38348 = CARTESIAN_POINT('Ctrl Pts',(-19.6291473919891,34.0369347094565,124.597606613349)) ;
#38349 = CARTESIAN_POINT('Ctrl Pts',(-19.6841021964564,33.8569456290466,124.894057285031)) ;
#38350 = CARTESIAN_POINT('Ctrl Pts',(-19.4212948778569,34.0468669991335,124.617735601843)) ;
#38351 = CARTESIAN_POINT('Ctrl Pts',(-19.4242874903847,33.8668779187237,124.919216071778)) ;
#38352 = CARTESIAN_POINT('Ctrl Pts',(-19.2116608547725,34.0568686441042,124.601562538898)) ;
#38353 = CARTESIAN_POINT('Ctrl Pts',(-19.1622401128743,33.8768795636944,124.89899567107)) ;
#38354 = CARTESIAN_POINT('Ctrl Pts',(-18.9405917318877,34.0701812775203,124.531785628182)) ;
#38355 = CARTESIAN_POINT('Ctrl Pts',(-18.8234293921044,33.8901921971104,124.811777112325)) ;
#38356 = CARTESIAN_POINT('Ctrl Pts',(-18.6953484784507,34.0834130269018,124.393891815293)) ;
#38357 = CARTESIAN_POINT('Ctrl Pts',(-18.5168908225007,33.903423946492,124.639429121333)) ;
#38358 = CARTESIAN_POINT('Ctrl Pts',(-18.4950002821873,34.0967362917189,124.198208396693)) ;
#38359 = CARTESIAN_POINT('Ctrl Pts',(-18.2664169529744,33.9167472113091,124.394788919325)) ;
#38360 = CARTESIAN_POINT('Ctrl Pts',(-18.3736497757206,34.1066119979366,124.029725845387)) ;
#38361 = CARTESIAN_POINT('Ctrl Pts',(-18.1147393756413,33.9266229175268,124.184190734475)) ;
#38362 = CARTESIAN_POINT('Ctrl Pts',(-18.2821299159748,34.1166015890366,123.840730802708)) ;
#38363 = CARTESIAN_POINT('Ctrl Pts',(-18.0003398463221,33.9366125086268,123.947943873765)) ;
#38364 = CARTESIAN_POINT('Ctrl Pts',(-18.2250270269363,34.126528685492,123.639969576889)) ;
#38365 = CARTESIAN_POINT('Ctrl Pts',(-17.9289645287867,33.9465396050822,123.696992065045)) ;
#38366 = CARTESIAN_POINT('Ctrl Pts',(-18.2034190105843,34.1365538339966,123.430338906527)) ;
#38367 = CARTESIAN_POINT('Ctrl Pts',(-17.9019571310987,33.9565647535868,123.434953214905)) ;
#38368 = CARTESIAN_POINT('Ctrl Pts',(-18.2182165399645,34.1464494881433,123.22280972338)) ;
#38369 = CARTESIAN_POINT('Ctrl Pts',(-17.9204568678603,33.9664604077335,123.17554205704)) ;
#38370 = CARTESIAN_POINT('Ctrl Pts',(-18.2690763393294,34.1564530225215,123.018767205604)) ;
#38371 = CARTESIAN_POINT('Ctrl Pts',(-17.9840343131373,33.9764639421116,122.920489516551)) ;
#38372 = CARTESIAN_POINT('Ctrl Pts',(-18.3544753384947,34.1664381609615,122.826969229147)) ;
#38373 = CARTESIAN_POINT('Ctrl Pts',(-18.090785614711,33.9864490805517,122.680743142439)) ;
#38374 = CARTESIAN_POINT('Ctrl Pts',(-18.472628068217,34.1764740855569,122.652181840679)) ;
#38375 = CARTESIAN_POINT('Ctrl Pts',(-18.2384789184534,33.9964850051471,122.462260358668)) ;
#38376 = CARTESIAN_POINT('Ctrl Pts',(-18.6164655673293,34.1863253609846,122.503176356432)) ;
#38377 = CARTESIAN_POINT('Ctrl Pts',(-18.4182776202501,34.0063362805748,122.276005602342)) ;
#38378 = CARTESIAN_POINT('Ctrl Pts',(-18.7860413391488,34.1963176221459,122.379176678945)) ;
#38379 = CARTESIAN_POINT('Ctrl Pts',(-18.6302489537786,34.0163285417361,122.121008186934)) ;
#38380 = CARTESIAN_POINT('Ctrl Pts',(-18.9756890039157,34.2063575061635,122.28655058311)) ;
#38381 = CARTESIAN_POINT('Ctrl Pts',(-18.8673098715095,34.0263684257537,122.005227980677)) ;
#38382 = CARTESIAN_POINT('Ctrl Pts',(-19.1742841833314,34.216192280666,122.228937175601)) ;
#38383 = CARTESIAN_POINT('Ctrl Pts',(-19.115554348172,34.0362032002561,121.933213929696)) ;
#38384 = CARTESIAN_POINT('Ctrl Pts',(-19.3848491923498,34.2262686616863,122.206064095347)) ;
#38385 = CARTESIAN_POINT('Ctrl Pts',(-19.378760644143,34.0462795812764,121.904625237275)) ;
#38386 = CARTESIAN_POINT('Ctrl Pts',(-19.5914235484233,34.2361149348369,122.219725589952)) ;
#38387 = CARTESIAN_POINT('Ctrl Pts',(-19.6369799649449,34.0561258544271,121.921704730761)) ;
#38388 = CARTESIAN_POINT('Ctrl Pts',(-19.8644290889112,34.2494794561221,122.286150104752)) ;
#38389 = CARTESIAN_POINT('Ctrl Pts',(-19.9782262367298,34.0694903757123,122.004738916852)) ;
#38390 = CARTESIAN_POINT('Ctrl Pts',(-20.1107333011822,34.2626857005566,122.421054667692)) ;
#38391 = CARTESIAN_POINT('Ctrl Pts',(-20.2860725516043,34.0826966201467,122.173341752831)) ;
#38392 = CARTESIAN_POINT('Ctrl Pts',(-20.3128900283233,34.2759506552338,122.613069418679)) ;
#38393 = CARTESIAN_POINT('Ctrl Pts',(-20.5388137927401,34.095961574824,122.41339891427)) ;
#38394 = CARTESIAN_POINT('Ctrl Pts',(-20.438205183774,34.2859829357855,122.782731790521)) ;
#38395 = CARTESIAN_POINT('Ctrl Pts',(-20.6954462285067,34.1059938553757,122.625471146466)) ;
#38396 = CARTESIAN_POINT('Ctrl Pts',(-20.5310032145783,34.2958916693034,122.96922602419)) ;
#38397 = CARTESIAN_POINT('Ctrl Pts',(-20.811443835106,34.1159025888936,122.858591933843)) ;
#38398 = CARTESIAN_POINT('Ctrl Pts',(-20.5907085275571,34.3058292201709,123.169440553708)) ;
#38399 = CARTESIAN_POINT('Ctrl Pts',(-20.8860726330652,34.1258401397611,123.108858926541)) ;
#38400 = CARTESIAN_POINT('Ctrl Pts',(-20.6147885837747,34.3158590677648,123.378897155107)) ;
#38401 = CARTESIAN_POINT('Ctrl Pts',(-20.9161696355362,34.135869987355,123.370684085344)) ;
#38402 = CARTESIAN_POINT('Ctrl Pts',(-20.5984660377212,34.3290942076852,123.656745178139)) ;
#38403 = CARTESIAN_POINT('Ctrl Pts',(-20.8957675551439,34.1491051272754,123.717974610687)) ;
#38404 = CARTESIAN_POINT('Ctrl Pts',(-20.4868736795983,34.3457626720564,123.993002939098)) ;
#38405 = CARTESIAN_POINT('Ctrl Pts',(-20.7562726268959,34.1657735916466,124.138314956039)) ;
#38406 = CARTESIAN_POINT('Ctrl Pts',(-20.2251415994005,34.3656336839303,124.324854114814)) ;
#38407 = CARTESIAN_POINT('Ctrl Pts',(-20.429086179161,34.1856446035205,124.553127465657)) ;
#38408 = CARTESIAN_POINT('Ctrl Pts',(-19.9231542481283,34.3823407683133,124.511841033235)) ;
#38409 = CARTESIAN_POINT('Ctrl Pts',(-20.0516612998158,34.2023516879034,124.786832185084)) ;
#38410 = CARTESIAN_POINT('Ctrl Pts',(-19.657904162901,34.3955180496239,124.591763757733)) ;
#38411 = CARTESIAN_POINT('Ctrl Pts',(-19.7200431655588,34.215528969214,124.886756209317)) ;
#38412 = CARTESIAN_POINT('Ctrl Pts',(-19.3810401547888,34.408785510138,124.625633782009)) ;
#38413 = CARTESIAN_POINT('Ctrl Pts',(-19.3739840223189,34.2287964297281,124.929088135759)) ;
#38414 = CARTESIAN_POINT('Ctrl Pts',(-19.0312401721135,34.4253994008252,124.576410369976)) ;
#38415 = CARTESIAN_POINT('Ctrl Pts',(-18.9367200239934,34.2454103204153,124.867555179956)) ;
#38416 = CARTESIAN_POINT('Ctrl Pts',(-18.6565409852236,34.4453482002526,124.377526322459)) ;
#38417 = CARTESIAN_POINT('Ctrl Pts',(-18.4683529488441,34.2653591198428,124.618947214289)) ;
#38418 = CARTESIAN_POINT('Ctrl Pts',(-18.372722975046,34.4652693117834,124.063178650212)) ;
#38419 = CARTESIAN_POINT('Ctrl Pts',(-18.1135823384901,34.2852802313736,124.226010700045)) ;
#38420 = CARTESIAN_POINT('Ctrl Pts',(-18.2127872385282,34.4851357599563,123.672140863886)) ;
#38421 = CARTESIAN_POINT('Ctrl Pts',(-17.9136663304717,34.3051466795465,123.737213595572)) ;
#38422 = CARTESIAN_POINT('Ctrl Pts',(-18.1960174572984,34.5051621065734,123.246703868946)) ;
#38423 = CARTESIAN_POINT('Ctrl Pts',(-17.8927069830595,34.3251730261636,123.205416904753)) ;
#38424 = CARTESIAN_POINT('Ctrl Pts',(-18.3244861075331,34.525024150963,122.844320049915)) ;
#38425 = CARTESIAN_POINT('Ctrl Pts',(-18.0532950836651,34.3450350705532,122.702439446639)) ;
#38426 = CARTESIAN_POINT('Ctrl Pts',(-18.5830265246617,34.5449694536441,122.508225439242)) ;
#38427 = CARTESIAN_POINT('Ctrl Pts',(-18.3764719974308,34.3649803732343,122.282323158673)) ;
#38428 = CARTESIAN_POINT('Ctrl Pts',(-18.9399371008137,34.564864760703,122.281121704416)) ;
#38429 = CARTESIAN_POINT('Ctrl Pts',(-18.8226102498353,34.3848756802931,121.998446004873)) ;
#38430 = CARTESIAN_POINT('Ctrl Pts',(-19.3527127164133,34.5847580308706,122.188711680669)) ;
#38431 = CARTESIAN_POINT('Ctrl Pts',(-19.3385786404535,34.4047689504608,121.882935209687)) ;
#38432 = CARTESIAN_POINT('Ctrl Pts',(-19.7737254388914,34.604723623551,122.242987808738)) ;
#38433 = CARTESIAN_POINT('Ctrl Pts',(-19.8648438727178,34.4247345431412,121.950781567491)) ;
#38434 = CARTESIAN_POINT('Ctrl Pts',(-20.1494199931143,34.6245989472359,122.436554500858)) ;
#38435 = CARTESIAN_POINT('Ctrl Pts',(-20.3344600161098,34.444609866826,122.19273979903)) ;
#38436 = CARTESIAN_POINT('Ctrl Pts',(-20.4382613496929,34.6445740098108,122.747966146561)) ;
#38437 = CARTESIAN_POINT('Ctrl Pts',(-20.6955112754872,34.464584929401,122.582004291028)) ;
#38438 = CARTESIAN_POINT('Ctrl Pts',(-20.6027074825129,34.6645264194419,123.139039458747)) ;
#38439 = CARTESIAN_POINT('Ctrl Pts',(-20.90106819709,34.4845373390321,123.07084543129)) ;
#38440 = CARTESIAN_POINT('Ctrl Pts',(-20.6245230947549,34.684362473678,123.560242571632)) ;
#38441 = CARTESIAN_POINT('Ctrl Pts',(-20.9283379624116,34.5043733932682,123.597346656972)) ;
#38442 = CARTESIAN_POINT('Ctrl Pts',(-20.5008638045205,34.7043403850956,123.9666287374)) ;
#38443 = CARTESIAN_POINT('Ctrl Pts',(-20.7737648834349,34.5243513046858,124.105329355259)) ;
#38444 = CARTESIAN_POINT('Ctrl Pts',(-20.2463289326715,34.7242584345991,124.305081206645)) ;
#38445 = CARTESIAN_POINT('Ctrl Pts',(-20.4555977349915,34.5442693541892,124.528394482455)) ;
#38446 = CARTESIAN_POINT('Ctrl Pts',(-19.8929765679083,34.7441265783672,124.53677216459)) ;
#38447 = CARTESIAN_POINT('Ctrl Pts',(-20.0139097342073,34.5641374979573,124.818008765384)) ;
#38448 = CARTESIAN_POINT('Ctrl Pts',(-19.4780285765812,34.7641774349545,124.634188159113)) ;
#38449 = CARTESIAN_POINT('Ctrl Pts',(-19.4952245291037,34.5841883545447,124.939780508344)) ;
#38450 = CARTESIAN_POINT('Ctrl Pts',(-19.060179710771,34.7839578714104,124.585251419341)) ;
#38451 = CARTESIAN_POINT('Ctrl Pts',(-18.9729159061635,34.6039687910005,124.878612004272)) ;
#38452 = CARTESIAN_POINT('Ctrl Pts',(-18.6792558296266,34.8039879270882,124.394988896057)) ;
#38453 = CARTESIAN_POINT('Ctrl Pts',(-18.4967594861514,34.6239988466783,124.640786108543)) ;
#38454 = CARTESIAN_POINT('Ctrl Pts',(-18.3887123278353,34.823869032263,124.087835513571)) ;
#38455 = CARTESIAN_POINT('Ctrl Pts',(-18.1335792137184,34.6438799518531,124.256847057507)) ;
#38456 = CARTESIAN_POINT('Ctrl Pts',(-18.2193821090019,34.8437494946307,123.70056629443)) ;
#38457 = CARTESIAN_POINT('Ctrl Pts',(-17.921913909552,34.6637604142209,123.772762991372)) ;
#38458 = CARTESIAN_POINT('Ctrl Pts',(-18.1923412672095,34.8637346417751,123.276475566402)) ;
#38459 = CARTESIAN_POINT('Ctrl Pts',(-17.8881094854383,34.6837455613653,123.242649910953)) ;
#38460 = CARTESIAN_POINT('Ctrl Pts',(-18.3111763931638,34.8836252203115,122.870576698358)) ;
#38461 = CARTESIAN_POINT('Ctrl Pts',(-18.0366497414932,34.7036361399017,122.735276316427)) ;
#38462 = CARTESIAN_POINT('Ctrl Pts',(-18.5608208396316,34.9035192401859,122.529106310762)) ;
#38463 = CARTESIAN_POINT('Ctrl Pts',(-18.34870157791,34.7235301597761,122.30843669083)) ;
#38464 = CARTESIAN_POINT('Ctrl Pts',(-18.9123762892436,34.9234406849123,122.292940920012)) ;
#38465 = CARTESIAN_POINT('Ctrl Pts',(-18.7881430602203,34.7434516045024,122.013226846823)) ;
#38466 = CARTESIAN_POINT('Ctrl Pts',(-19.322937407292,34.9433388229677,122.190263489512)) ;
#38467 = CARTESIAN_POINT('Ctrl Pts',(-19.3013427498068,34.7633497425579,121.884875817317)) ;
#38468 = CARTESIAN_POINT('Ctrl Pts',(-19.7472655180878,34.9634095781838,122.235024621243)) ;
#38469 = CARTESIAN_POINT('Ctrl Pts',(-19.831753866014,34.783420497774,121.940822959817)) ;
#38470 = CARTESIAN_POINT('Ctrl Pts',(-20.1256368241744,34.983195128235,122.419137958029)) ;
#38471 = CARTESIAN_POINT('Ctrl Pts',(-20.304718807225,34.8032060478252,122.170959918771)) ;
#38472 = CARTESIAN_POINT('Ctrl Pts',(-20.4220114238497,35.0031782031124,122.723491321835)) ;
#38473 = CARTESIAN_POINT('Ctrl Pts',(-20.6751904640784,34.8231891227026,122.551398320175)) ;
#38474 = CARTESIAN_POINT('Ctrl Pts',(-20.5955208583163,35.0230872857583,123.109625284551)) ;
#38475 = CARTESIAN_POINT('Ctrl Pts',(-20.8920819874043,34.8430982053485,123.034062768694)) ;
#38476 = CARTESIAN_POINT('Ctrl Pts',(-20.6279870536071,35.0429458448811,123.530675885179)) ;
#38477 = CARTESIAN_POINT('Ctrl Pts',(-20.9326680571387,34.8629567644712,123.560377307956)) ;
#38478 = CARTESIAN_POINT('Ctrl Pts',(-20.5133192729208,35.0629892887198,123.941055703616)) ;
#38479 = CARTESIAN_POINT('Ctrl Pts',(-20.7893451367236,34.88300020831,124.07334538232)) ;
#38480 = CARTESIAN_POINT('Ctrl Pts',(-20.3093835063598,35.079489353449,124.226623757706)) ;
#38481 = CARTESIAN_POINT('Ctrl Pts',(-20.5344079581164,34.8995002730392,124.430333478013)) ;
#38482 = CARTESIAN_POINT('Ctrl Pts',(-20.092268777163,35.0928790932979,124.405758678577)) ;
#38483 = CARTESIAN_POINT('Ctrl Pts',(-20.2630356080209,34.912890012888,124.654232063072)) ;
#38484 = CARTESIAN_POINT('Ctrl Pts',(-19.9119702886458,35.1027359945063,124.507953316112)) ;
#38485 = CARTESIAN_POINT('Ctrl Pts',(-20.0376601532966,34.9227469140964,124.78198202428)) ;
#38486 = CARTESIAN_POINT('Ctrl Pts',(-19.7141970013292,35.1127275203528,124.578624517524)) ;
#38487 = CARTESIAN_POINT('Ctrl Pts',(-19.7904462532024,34.9327384399429,124.870322609991)) ;
#38488 = CARTESIAN_POINT('Ctrl Pts',(-19.5084940721676,35.1226522008037,124.613732527868)) ;
#38489 = CARTESIAN_POINT('Ctrl Pts',(-19.5333148830191,34.9426631203939,124.914209741569)) ;
#38490 = CARTESIAN_POINT('Ctrl Pts',(-19.2980655867416,35.1326627908481,124.612658643822)) ;
#38491 = CARTESIAN_POINT('Ctrl Pts',(-19.2702905171921,34.9526737104383,124.912873328906)) ;
#38492 = CARTESIAN_POINT('Ctrl Pts',(-19.0237133873326,35.1459220515518,124.563175266845)) ;
#38493 = CARTESIAN_POINT('Ctrl Pts',(-18.9272936377621,34.965932971142,124.85100643063)) ;
#38494 = CARTESIAN_POINT('Ctrl Pts',(-18.7669990026085,35.1592731267021,124.442141475141)) ;
#38495 = CARTESIAN_POINT('Ctrl Pts',(-18.6064360058231,34.9792840462923,124.699721053727)) ;
#38496 = CARTESIAN_POINT('Ctrl Pts',(-18.5548922307535,35.1724794359369,124.262885149978)) ;
#38497 = CARTESIAN_POINT('Ctrl Pts',(-18.3413122765089,34.9924903555271,124.475665673897)) ;
#38498 = CARTESIAN_POINT('Ctrl Pts',(-18.4202016194479,35.1824662695272,124.101878407724)) ;
#38499 = CARTESIAN_POINT('Ctrl Pts',(-18.1729444099788,35.0024771891173,124.274406568273)) ;
#38500 = CARTESIAN_POINT('Ctrl Pts',(-18.3157421931826,35.1924189970233,123.920538588917)) ;
#38501 = CARTESIAN_POINT('Ctrl Pts',(-18.0423683361374,35.0124299166134,124.047733829705)) ;
#38502 = CARTESIAN_POINT('Ctrl Pts',(-18.243859696856,35.2024670938648,123.721927113406)) ;
#38503 = CARTESIAN_POINT('Ctrl Pts',(-17.9525123754885,35.022478013455,123.799470169286)) ;
#38504 = CARTESIAN_POINT('Ctrl Pts',(-18.2080532676477,35.2123085507367,123.518130094329)) ;
#38505 = CARTESIAN_POINT('Ctrl Pts',(-17.9077516293332,35.0323194703268,123.544724476249)) ;
#38506 = CARTESIAN_POINT('Ctrl Pts',(-18.2077298878391,35.2222948176502,123.308221872427)) ;
#38507 = CARTESIAN_POINT('Ctrl Pts',(-17.9073445683003,35.0423057372403,123.28233910936)) ;
#38508 = CARTESIAN_POINT('Ctrl Pts',(-18.2435874649064,35.2322314185506,123.102388357164)) ;
#38509 = CARTESIAN_POINT('Ctrl Pts',(-17.9521637826458,35.0522423381408,123.025046666894)) ;
#38510 = CARTESIAN_POINT('Ctrl Pts',(-18.3155310783834,35.2422813613376,122.903755486322)) ;
#38511 = CARTESIAN_POINT('Ctrl Pts',(-18.0420906679153,35.0622922809278,122.776754559709)) ;
#38512 = CARTESIAN_POINT('Ctrl Pts',(-18.4186601658913,35.2521315610234,122.724163217864)) ;
#38513 = CARTESIAN_POINT('Ctrl Pts',(-18.1709996405976,35.0721424806135,122.552262724079)) ;
#38514 = CARTESIAN_POINT('Ctrl Pts',(-18.5526102972871,35.2621044659555,122.562900255392)) ;
#38515 = CARTESIAN_POINT('Ctrl Pts',(-18.3384352196135,35.0821153855456,122.350682137538)) ;
#38516 = CARTESIAN_POINT('Ctrl Pts',(-18.7130161190752,35.2721028404351,122.427018538122)) ;
#38517 = CARTESIAN_POINT('Ctrl Pts',(-18.5389407429499,35.0921137600253,122.180827804049)) ;
#38518 = CARTESIAN_POINT('Ctrl Pts',(-18.8950233937213,35.2821230143051,122.320968913956)) ;
#38519 = CARTESIAN_POINT('Ctrl Pts',(-18.7664484679587,35.1021339338953,122.048263316503)) ;
#38520 = CARTESIAN_POINT('Ctrl Pts',(-19.0902785173193,35.2920240582471,122.248825467389)) ;
#38521 = CARTESIAN_POINT('Ctrl Pts',(-19.0105165623508,35.1120349778372,121.958081319007)) ;
#38522 = CARTESIAN_POINT('Ctrl Pts',(-19.2968437850745,35.3020128619714,122.211027115049)) ;
#38523 = CARTESIAN_POINT('Ctrl Pts',(-19.2687227454452,35.1220237815616,121.91083061917)) ;
#38524 = CARTESIAN_POINT('Ctrl Pts',(-19.5063361205008,35.3119783288032,122.209821899411)) ;
#38525 = CARTESIAN_POINT('Ctrl Pts',(-19.5305882706749,35.1319892483934,121.909321300871)) ;
#38526 = CARTESIAN_POINT('Ctrl Pts',(-19.7116863669934,35.3218818910762,122.244299443621)) ;
#38527 = CARTESIAN_POINT('Ctrl Pts',(-19.7872767838553,35.1418928106663,121.952415553916)) ;
#38528 = CARTESIAN_POINT('Ctrl Pts',(-19.9109411377999,35.3319425689542,122.31516138068)) ;
#38529 = CARTESIAN_POINT('Ctrl Pts',(-20.0363461470048,35.1519534885443,122.040990349763)) ;
#38530 = CARTESIAN_POINT('Ctrl Pts',(-20.0910169677187,35.3417828669036,122.417053554877)) ;
#38531 = CARTESIAN_POINT('Ctrl Pts',(-20.2614426416731,35.1617937864938,122.168353377838)) ;
#38532 = CARTESIAN_POINT('Ctrl Pts',(-20.2543967354931,35.3518458618131,122.551408724914)) ;
#38533 = CARTESIAN_POINT('Ctrl Pts',(-20.4656690482837,35.1718567814032,122.336295208353)) ;
#38534 = CARTESIAN_POINT('Ctrl Pts',(-20.389561216917,35.3617401559602,122.709546984576)) ;
#38535 = CARTESIAN_POINT('Ctrl Pts',(-20.6346269467012,35.1817510755504,122.533966500699)) ;
#38536 = CARTESIAN_POINT('Ctrl Pts',(-20.4961856714635,35.3716819536571,122.889282267769)) ;
#38537 = CARTESIAN_POINT('Ctrl Pts',(-20.7679099511317,35.1916928732473,122.758634465318)) ;
#38538 = CARTESIAN_POINT('Ctrl Pts',(-20.5705249428159,35.3816845311862,123.08601924968)) ;
#38539 = CARTESIAN_POINT('Ctrl Pts',(-20.8608365588949,35.2016954507764,123.004554830553)) ;
#38540 = CARTESIAN_POINT('Ctrl Pts',(-20.6093729379891,35.3917189951073,123.293356771096)) ;
#38541 = CARTESIAN_POINT('Ctrl Pts',(-20.9093992124096,35.2117299146974,123.263726218805)) ;
#38542 = CARTESIAN_POINT('Ctrl Pts',(-20.6119121965854,35.4015651336283,123.500344351237)) ;
#38543 = CARTESIAN_POINT('Ctrl Pts',(-20.9125759543074,35.2215760532185,123.522461220012)) ;
#38544 = CARTESIAN_POINT('Ctrl Pts',(-20.5784797869807,35.4115463068653,123.707482594867)) ;
#38545 = CARTESIAN_POINT('Ctrl Pts',(-20.8707879749445,35.2315572264555,123.781384610277)) ;
#38546 = CARTESIAN_POINT('Ctrl Pts',(-20.5097340551168,35.4214986008226,123.905101498051)) ;
#38547 = CARTESIAN_POINT('Ctrl Pts',(-20.7848581741981,35.2415095204127,124.02840934673)) ;
#38548 = CARTESIAN_POINT('Ctrl Pts',(-20.4074763823881,35.4314973959572,124.088777449656)) ;
#38549 = CARTESIAN_POINT('Ctrl Pts',(-20.6570382604002,35.2515083155473,124.258005618695)) ;
#38550 = CARTESIAN_POINT('Ctrl Pts',(-20.2740486464451,35.441536504218,124.252287560575)) ;
#38551 = CARTESIAN_POINT('Ctrl Pts',(-20.4902556613288,35.2615474238082,124.46239487073)) ;
#38552 = CARTESIAN_POINT('Ctrl Pts',(-20.1179375824698,35.4513614456571,124.387557243279)) ;
#38553 = CARTESIAN_POINT('Ctrl Pts',(-20.2951179161425,35.2713723652473,124.631484396913)) ;
#38554 = CARTESIAN_POINT('Ctrl Pts',(-19.9367669407761,35.4614161327315,124.496432561187)) ;
#38555 = CARTESIAN_POINT('Ctrl Pts',(-20.0686559822172,35.2814270523217,124.767580615246)) ;
#38556 = CARTESIAN_POINT('Ctrl Pts',(-19.7414940311369,35.4713589376717,124.571026731004)) ;
#38557 = CARTESIAN_POINT('Ctrl Pts',(-19.8245654449481,35.2913698572619,124.860825828443)) ;
#38558 = CARTESIAN_POINT('Ctrl Pts',(-19.5371642498936,35.4812627236682,124.611053711609)) ;
#38559 = CARTESIAN_POINT('Ctrl Pts',(-19.569153162575,35.3012736432584,124.910862029664)) ;
#38560 = CARTESIAN_POINT('Ctrl Pts',(-19.3260021505189,35.491309540233,124.614922626693)) ;
#38561 = CARTESIAN_POINT('Ctrl Pts',(-19.3052006854383,35.3113204598231,124.915700617932)) ;
#38562 = CARTESIAN_POINT('Ctrl Pts',(-19.1204374563193,35.5012050597117,124.582740242867)) ;
#38563 = CARTESIAN_POINT('Ctrl Pts',(-19.0482438727932,35.3212159793018,124.875474923226)) ;
#38564 = CARTESIAN_POINT('Ctrl Pts',(-18.9203301984494,35.5112671450361,124.514241085289)) ;
#38565 = CARTESIAN_POINT('Ctrl Pts',(-18.7981091918195,35.3312780646263,124.78985331279)) ;
#38566 = CARTESIAN_POINT('Ctrl Pts',(-18.7390904234207,35.521109855994,124.414343573593)) ;
#38567 = CARTESIAN_POINT('Ctrl Pts',(-18.5715575696293,35.3411207755842,124.664983089967)) ;
#38568 = CARTESIAN_POINT('Ctrl Pts',(-18.575252732091,35.5311005733001,124.282960921875)) ;
#38569 = CARTESIAN_POINT('Ctrl Pts',(-18.3667589019596,35.3511114928903,124.500756432861)) ;
#38570 = CARTESIAN_POINT('Ctrl Pts',(-18.4375879398549,35.5410286563966,124.126065100434)) ;
#38571 = CARTESIAN_POINT('Ctrl Pts',(-18.1946758846968,35.3610395759868,124.304637787701)) ;
#38572 = CARTESIAN_POINT('Ctrl Pts',(-18.3282912493656,35.5510165865084,123.94676509158)) ;
#38573 = CARTESIAN_POINT('Ctrl Pts',(-18.0580530663617,35.3710275060986,124.080513755033)) ;
#38574 = CARTESIAN_POINT('Ctrl Pts',(-18.2517565825726,35.5610524126357,123.750158377981)) ;
#38575 = CARTESIAN_POINT('Ctrl Pts',(-17.9623826479832,35.3810633322259,123.834756266212)) ;
#38576 = CARTESIAN_POINT('Ctrl Pts',(-18.2109351619,35.5709077497493,123.547017923555)) ;
#38577 = CARTESIAN_POINT('Ctrl Pts',(-17.9113535513551,35.3909186693395,123.580830234508)) ;
#38578 = CARTESIAN_POINT('Ctrl Pts',(-18.2056029932862,35.5809054845995,123.336924382834)) ;
#38579 = CARTESIAN_POINT('Ctrl Pts',(-17.9046862414438,35.4009164041897,123.318213209576)) ;
#38580 = CARTESIAN_POINT('Ctrl Pts',(-18.2364854342571,35.5908133885839,123.130921758617)) ;
#38581 = CARTESIAN_POINT('Ctrl Pts',(-17.9432873404419,35.4108243081741,123.060708970224)) ;
#38582 = CARTESIAN_POINT('Ctrl Pts',(-18.3030212952615,35.6008244631324,122.931244855466)) ;
#38583 = CARTESIAN_POINT('Ctrl Pts',(-18.0264553067541,35.4208353827226,122.811112169796)) ;
#38584 = CARTESIAN_POINT('Ctrl Pts',(-18.4037616999809,35.610852318668,122.746053058714)) ;
#38585 = CARTESIAN_POINT('Ctrl Pts',(-18.152378938914,35.4308632382582,122.579621476775)) ;
#38586 = CARTESIAN_POINT('Ctrl Pts',(-18.532602474964,35.6207099125732,122.583737923954)) ;
#38587 = CARTESIAN_POINT('Ctrl Pts',(-18.3134289649953,35.4407208321634,122.376725539673)) ;
#38588 = CARTESIAN_POINT('Ctrl Pts',(-18.6900489868914,35.6307365994113,122.443575063873)) ;
#38589 = CARTESIAN_POINT('Ctrl Pts',(-18.5102358432647,35.4507475190015,122.201520587854)) ;
#38590 = CARTESIAN_POINT('Ctrl Pts',(-18.8697550672844,35.6407652685651,122.333303125857)) ;
#38591 = CARTESIAN_POINT('Ctrl Pts',(-18.7348673255347,35.4607761881552,122.063678979637)) ;
#38592 = CARTESIAN_POINT('Ctrl Pts',(-19.0621320904684,35.6506104768465,122.256973154102)) ;
#38593 = CARTESIAN_POINT('Ctrl Pts',(-18.9753389391847,35.4706213964366,121.968264330537)) ;
#38594 = CARTESIAN_POINT('Ctrl Pts',(-19.2677365853568,35.6606011658096,122.214031607131)) ;
#38595 = CARTESIAN_POINT('Ctrl Pts',(-19.2323443952297,35.4806120853998,121.914585661978)) ;
#38596 = CARTESIAN_POINT('Ctrl Pts',(-19.4786728867515,35.6706390420919,122.207881553144)) ;
#38597 = CARTESIAN_POINT('Ctrl Pts',(-19.4960145845465,35.4906499616821,121.906896220125)) ;
#38598 = CARTESIAN_POINT('Ctrl Pts',(-19.6835091491884,35.6804834197341,122.237505000338)) ;
#38599 = CARTESIAN_POINT('Ctrl Pts',(-19.7520613231503,35.5004943393243,121.943923950891)) ;
#38600 = CARTESIAN_POINT('Ctrl Pts',(-19.8829904576665,35.6904682241255,122.302762495252)) ;
#38601 = CARTESIAN_POINT('Ctrl Pts',(-20.0014137030145,35.5104791437157,122.025494346752)) ;
#38602 = CARTESIAN_POINT('Ctrl Pts',(-20.0673637367163,35.7004077543441,122.401163727744)) ;
#38603 = CARTESIAN_POINT('Ctrl Pts',(-20.2318815339164,35.5204186739343,122.148494733282)) ;
#38604 = CARTESIAN_POINT('Ctrl Pts',(-20.2334425789832,35.710447442381,122.531393346306)) ;
#38605 = CARTESIAN_POINT('Ctrl Pts',(-20.4394809697668,35.5304583619711,122.311280393295)) ;
#38606 = CARTESIAN_POINT('Ctrl Pts',(-20.3723559056366,35.7203357317493,122.686064760268)) ;
#38607 = CARTESIAN_POINT('Ctrl Pts',(-20.6131244207702,35.5403466513395,122.504619288764)) ;
#38608 = CARTESIAN_POINT('Ctrl Pts',(-20.4837508188583,35.7303248554341,122.864079606437)) ;
#38609 = CARTESIAN_POINT('Ctrl Pts',(-20.7523694042622,35.5503357750242,122.727137258845)) ;
#38610 = CARTESIAN_POINT('Ctrl Pts',(-20.5621646542934,35.7402848651087,123.058229679049)) ;
#38611 = CARTESIAN_POINT('Ctrl Pts',(-20.850388256129,35.5602957846989,122.969824688624)) ;
#38612 = CARTESIAN_POINT('Ctrl Pts',(-20.6059033424676,35.7501852948129,123.261726613465)) ;
#38613 = CARTESIAN_POINT('Ctrl Pts',(-20.9050630990468,35.5701962144031,123.224196430438)) ;
#38614 = CARTESIAN_POINT('Ctrl Pts',(-20.6137449772283,35.7602283762197,123.472709317713)) ;
#38615 = CARTESIAN_POINT('Ctrl Pts',(-20.9148664710667,35.5802392958098,123.487924566712)) ;
#38616 = CARTESIAN_POINT('Ctrl Pts',(-20.5852260061574,35.7701357701273,123.67904320518)) ;
#38617 = CARTESIAN_POINT('Ctrl Pts',(-20.8792189655505,35.5901466897175,123.745842918038)) ;
#38618 = CARTESIAN_POINT('Ctrl Pts',(-20.5210141564566,35.7801475011165,123.879489186249)) ;
#38619 = CARTESIAN_POINT('Ctrl Pts',(-20.7989552796093,35.6001584207067,123.996400804907)) ;
#38620 = CARTESIAN_POINT('Ctrl Pts',(-20.4224008662751,35.7901797188313,124.06593183367)) ;
#38621 = CARTESIAN_POINT('Ctrl Pts',(-20.6756899073962,35.6101906384214,124.229454654576)) ;
#38622 = CARTESIAN_POINT('Ctrl Pts',(-20.2954649937383,35.8000322280774,124.229594024067)) ;
#38623 = CARTESIAN_POINT('Ctrl Pts',(-20.5170202760373,35.6200431476676,124.434034154128)) ;
#38624 = CARTESIAN_POINT('Ctrl Pts',(-20.1408226833668,35.8099901646204,124.370712894289)) ;
#38625 = CARTESIAN_POINT('Ctrl Pts',(-20.3237177194056,35.6300010842106,124.610433802468)) ;
#38626 = CARTESIAN_POINT('Ctrl Pts',(-19.9624034194556,35.8200290346287,124.483417161163)) ;
#38627 = CARTESIAN_POINT('Ctrl Pts',(-20.1006943915222,35.6400399542189,124.751315017592)) ;
#38628 = CARTESIAN_POINT('Ctrl Pts',(-19.7704532057316,35.829902189787,124.56248627394)) ;
#38629 = CARTESIAN_POINT('Ctrl Pts',(-19.8607559657589,35.6499131093772,124.850152762087)) ;
#38630 = CARTESIAN_POINT('Ctrl Pts',(-19.5636408193586,35.8399754646367,124.607848543225)) ;
#38631 = CARTESIAN_POINT('Ctrl Pts',(-19.6022411196916,35.6599863842269,124.906856510857)) ;
#38632 = CARTESIAN_POINT('Ctrl Pts',(-19.3573296065172,35.8497957818141,124.616666849155)) ;
#38633 = CARTESIAN_POINT('Ctrl Pts',(-19.3443505908439,35.6698067014042,124.917880380805)) ;
#38634 = CARTESIAN_POINT('Ctrl Pts',(-19.1473070231254,35.8598744676076,124.58902082137)) ;
#38635 = CARTESIAN_POINT('Ctrl Pts',(-19.0818227173848,35.6798853871977,124.883323751805)) ;
#38636 = CARTESIAN_POINT('Ctrl Pts',(-18.9497113689918,35.8697259789907,124.526804413324)) ;
#38637 = CARTESIAN_POINT('Ctrl Pts',(-18.8348266453124,35.6897368985808,124.805553629487)) ;
#38638 = CARTESIAN_POINT('Ctrl Pts',(-18.7617765756378,35.8797994252973,124.429271647714)) ;
#38639 = CARTESIAN_POINT('Ctrl Pts',(-18.5999081950483,35.6998103448875,124.683638544775)) ;
#38640 = CARTESIAN_POINT('Ctrl Pts',(-18.597467101793,35.889640700422,124.303505365942)) ;
#38641 = CARTESIAN_POINT('Ctrl Pts',(-18.3945197611564,35.7096516200122,124.526430434766)) ;
#38642 = CARTESIAN_POINT('Ctrl Pts',(-18.4549920931084,35.8996258000788,124.149368497595)) ;
#38643 = CARTESIAN_POINT('Ctrl Pts',(-18.2164254320206,35.7196367196689,124.333759479589)) ;
#38644 = CARTESIAN_POINT('Ctrl Pts',(-18.3414173666157,35.9096332762131,123.972250384681)) ;
#38645 = CARTESIAN_POINT('Ctrl Pts',(-18.0744564632935,35.7296441958033,124.11236211311)) ;
#38646 = CARTESIAN_POINT('Ctrl Pts',(-18.2608430560108,35.919555863922,123.779847146659)) ;
#38647 = CARTESIAN_POINT('Ctrl Pts',(-17.9737377683904,35.7395667835122,123.871857563542)) ;
#38648 = CARTESIAN_POINT('Ctrl Pts',(-18.2142645919712,35.9295424681954,123.575109420464)) ;
#38649 = CARTESIAN_POINT('Ctrl Pts',(-17.9155142333491,35.7495533877855,123.615935266931)) ;
#38650 = CARTESIAN_POINT('Ctrl Pts',(-18.2042845382939,35.9395825965295,123.364287204911)) ;
#38651 = CARTESIAN_POINT('Ctrl Pts',(-17.9030386019391,35.7595935161196,123.352407710943)) ;
#38652 = CARTESIAN_POINT('Ctrl Pts',(-18.2300836682839,35.9494220310629,123.159025741679)) ;
#38653 = CARTESIAN_POINT('Ctrl Pts',(-17.9352873093069,35.7694329506531,123.095829360988)) ;
#38654 = CARTESIAN_POINT('Ctrl Pts',(-18.2923429640459,35.9594860855539,122.956842133847)) ;
#38655 = CARTESIAN_POINT('Ctrl Pts',(-18.0131110082293,35.779497005144,122.843100123042)) ;
#38656 = CARTESIAN_POINT('Ctrl Pts',(-18.3872080620054,35.969377004791,122.771780131143)) ;
#38657 = CARTESIAN_POINT('Ctrl Pts',(-18.1316925351678,35.7893879243812,122.61177152467)) ;
#38658 = CARTESIAN_POINT('Ctrl Pts',(-18.5136711614344,35.9793689980971,122.604062443733)) ;
#38659 = CARTESIAN_POINT('Ctrl Pts',(-18.2897713916433,35.7993799176872,122.402124132934)) ;
#38660 = CARTESIAN_POINT('Ctrl Pts',(-18.6670229740416,35.9893318620564,122.461407293779)) ;
#38661 = CARTESIAN_POINT('Ctrl Pts',(-18.4814613117937,35.8093427816465,122.2238046921)) ;
#38662 = CARTESIAN_POINT('Ctrl Pts',(-18.8415130358515,35.9992361218741,122.347760866079)) ;
#38663 = CARTESIAN_POINT('Ctrl Pts',(-18.6995746479516,35.8192470414643,122.081746101309)) ;
#38664 = CARTESIAN_POINT('Ctrl Pts',(-19.0361390397703,36.0092966124456,122.26503638611)) ;
#38665 = CARTESIAN_POINT('Ctrl Pts',(-18.9428567780689,35.8293075320357,121.978340523803)) ;
#38666 = CARTESIAN_POINT('Ctrl Pts',(-19.2376557259542,36.0191369620766,122.218129994328)) ;
#38667 = CARTESIAN_POINT('Ctrl Pts',(-19.1947540651951,35.8391478816668,121.919707183681)) ;
#38668 = CARTESIAN_POINT('Ctrl Pts',(-19.4488594057997,36.0291999375666,122.206420949229)) ;
#38669 = CARTESIAN_POINT('Ctrl Pts',(-19.4587582959339,35.8492108571568,121.905070980608)) ;
#38670 = CARTESIAN_POINT('Ctrl Pts',(-19.6553963029658,36.03909425771,122.231316246705)) ;
#38671 = CARTESIAN_POINT('Ctrl Pts',(-19.716930430741,35.8591051773002,121.936190237878)) ;
#38672 = CARTESIAN_POINT('Ctrl Pts',(-19.8555419191766,36.0490359708416,122.291429452583)) ;
#38673 = CARTESIAN_POINT('Ctrl Pts',(-19.9671129942115,35.8690468904317,122.011332156025)) ;
#38674 = CARTESIAN_POINT('Ctrl Pts',(-20.0434534803591,36.0590388606357,122.385905221195)) ;
#38675 = CARTESIAN_POINT('Ctrl Pts',(-20.2020024297715,35.8790497802259,122.129427167132)) ;
#38676 = CARTESIAN_POINT('Ctrl Pts',(-20.2124564475029,36.0690787177962,122.512316557016)) ;
#38677 = CARTESIAN_POINT('Ctrl Pts',(-20.4132559197918,35.8890896373864,122.287441324551)) ;
#38678 = CARTESIAN_POINT('Ctrl Pts',(-20.3542066989014,36.0789028986338,122.662550738687)) ;
#38679 = CARTESIAN_POINT('Ctrl Pts',(-20.5904446049979,35.898913818224,122.475235421975)) ;
#38680 = CARTESIAN_POINT('Ctrl Pts',(-20.4706332696789,36.088959872137,122.839015977808)) ;
#38681 = CARTESIAN_POINT('Ctrl Pts',(-20.7359772784727,35.9089707917272,122.695816923805)) ;
#38682 = CARTESIAN_POINT('Ctrl Pts',(-20.5533425088199,36.0988879963241,123.030662056921)) ;
#38683 = CARTESIAN_POINT('Ctrl Pts',(-20.8393638310025,35.9188989159142,122.935375322658)) ;
#38684 = CARTESIAN_POINT('Ctrl Pts',(-20.6021853906492,36.1088416913975,123.234141443748)) ;
#38685 = CARTESIAN_POINT('Ctrl Pts',(-20.9004170384747,35.9288526109877,123.189725205671)) ;
#38686 = CARTESIAN_POINT('Ctrl Pts',(-20.6147732903502,36.1188878849728,123.444966785403)) ;
#38687 = CARTESIAN_POINT('Ctrl Pts',(-20.9161514804583,35.9388988045629,123.453256665998)) ;
#38688 = CARTESIAN_POINT('Ctrl Pts',(-20.5912389874168,36.1287359873327,123.65066140107)) ;
#38689 = CARTESIAN_POINT('Ctrl Pts',(-20.8867329497479,35.9487469069229,123.710376268583)) ;
#38690 = CARTESIAN_POINT('Ctrl Pts',(-20.5322920817203,36.1386975755603,123.851608665551)) ;
#38691 = CARTESIAN_POINT('Ctrl Pts',(-20.8130484687253,35.9587084951504,123.961560575072)) ;
#38692 = CARTESIAN_POINT('Ctrl Pts',(-20.4384766708263,36.1487262457165,124.040434185181)) ;
#38693 = CARTESIAN_POINT('Ctrl Pts',(-20.6957786699468,35.9687371653067,124.19759210039)) ;
#38694 = CARTESIAN_POINT('Ctrl Pts',(-20.3148448154568,36.1586365485983,124.208121309133)) ;
#38695 = CARTESIAN_POINT('Ctrl Pts',(-20.5412377893626,35.9786474681884,124.407201312271)) ;
#38696 = CARTESIAN_POINT('Ctrl Pts',(-20.1639673049378,36.1685714324062,124.352558297041)) ;
#38697 = CARTESIAN_POINT('Ctrl Pts',(-20.3526398125577,35.9885823519964,124.587747365934)) ;
#38698 = CARTESIAN_POINT('Ctrl Pts',(-19.9883464931502,36.1786125740968,124.4696744726)) ;
#38699 = CARTESIAN_POINT('Ctrl Pts',(-20.1331135059833,35.998623493687,124.734141809711)) ;
#38700 = CARTESIAN_POINT('Ctrl Pts',(-19.7980654386768,36.1884996952608,124.553357993941)) ;
#38701 = CARTESIAN_POINT('Ctrl Pts',(-19.8952608882238,36.008510614851,124.83874584046)) ;
#38702 = CARTESIAN_POINT('Ctrl Pts',(-19.5941039539844,36.1984920381093,124.603590833534)) ;
#38703 = CARTESIAN_POINT('Ctrl Pts',(-19.6403085962597,36.0185029576995,124.901535971486)) ;
#38704 = CARTESIAN_POINT('Ctrl Pts',(-19.3854139464057,36.2084403393333,124.617526696654)) ;
#38705 = CARTESIAN_POINT('Ctrl Pts',(-19.3794454821453,36.0284512589234,124.918954868262)) ;
#38706 = CARTESIAN_POINT('Ctrl Pts',(-19.1776885830865,36.2183779170154,124.595344537768)) ;
#38707 = CARTESIAN_POINT('Ctrl Pts',(-19.1197882532183,36.0383888366056,124.891226019477)) ;
#38708 = CARTESIAN_POINT('Ctrl Pts',(-18.9758949839322,36.228364491466,124.537343966283)) ;
#38709 = CARTESIAN_POINT('Ctrl Pts',(-18.8675463523615,36.0483754110561,124.818724120337)) ;
#38710 = CARTESIAN_POINT('Ctrl Pts',(-18.7865605948736,36.2383933013744,124.444585421192)) ;
#38711 = CARTESIAN_POINT('Ctrl Pts',(-18.6308789215962,36.0584042209646,124.702775017939)) ;
#38712 = CARTESIAN_POINT('Ctrl Pts',(-18.6186460163788,36.2482716226812,124.322389246568)) ;
#38713 = CARTESIAN_POINT('Ctrl Pts',(-18.4209855121362,36.0682825422714,124.550028242174)) ;
#38714 = CARTESIAN_POINT('Ctrl Pts',(-18.4724839475725,36.2582632700286,124.171514768616)) ;
#38715 = CARTESIAN_POINT('Ctrl Pts',(-18.2382837455573,36.0782741896188,124.361434085775)) ;
#38716 = CARTESIAN_POINT('Ctrl Pts',(-18.3546005152364,36.2682977934664,123.996579143374)) ;
#38717 = CARTESIAN_POINT('Ctrl Pts',(-18.0909304836931,36.0883087130566,124.14276398916)) ;
#38718 = CARTESIAN_POINT('Ctrl Pts',(-18.2699376189153,36.278161150345,123.80726784102)) ;
#38719 = CARTESIAN_POINT('Ctrl Pts',(-17.985102604673,36.0981720699351,123.906123266349)) ;
#38720 = CARTESIAN_POINT('Ctrl Pts',(-18.2183426275422,36.2882313770253,123.601966412164)) ;
#38721 = CARTESIAN_POINT('Ctrl Pts',(-17.9206102594322,36.1082422966155,123.649496524014)) ;
#38722 = CARTESIAN_POINT('Ctrl Pts',(-18.2035300755518,36.2980736851599,123.395572554759)) ;
#38723 = CARTESIAN_POINT('Ctrl Pts',(-17.9020958098303,36.1180846047501,123.391502808903)) ;
#38724 = CARTESIAN_POINT('Ctrl Pts',(-18.2242647172834,36.3080344171834,123.187200743274)) ;
#38725 = CARTESIAN_POINT('Ctrl Pts',(-17.9280157513934,36.1280453367736,123.13103779863)) ;
#38726 = CARTESIAN_POINT('Ctrl Pts',(-18.2817044009816,36.3180723063815,122.984147670972)) ;
#38727 = CARTESIAN_POINT('Ctrl Pts',(-17.9998167260215,36.1380832259716,122.877221984958)) ;
#38728 = CARTESIAN_POINT('Ctrl Pts',(-18.3716994134048,36.3279465893003,122.797053220826)) ;
#38729 = CARTESIAN_POINT('Ctrl Pts',(-18.1123123668166,36.1479575088905,122.643353698626)) ;
#38730 = CARTESIAN_POINT('Ctrl Pts',(-18.4951890966193,36.3380163339178,122.625139380423)) ;
#38731 = CARTESIAN_POINT('Ctrl Pts',(-18.2666755577788,36.158027253508,122.428462610137)) ;
#38732 = CARTESIAN_POINT('Ctrl Pts',(-18.6430502592492,36.3478496442634,122.480641003559)) ;
#38733 = CARTESIAN_POINT('Ctrl Pts',(-18.4515040640522,36.1678605638536,122.247839904788)) ;
#38734 = CARTESIAN_POINT('Ctrl Pts',(-18.8168167962975,36.3578798876161,122.361190643597)) ;
#38735 = CARTESIAN_POINT('Ctrl Pts',(-18.6687131962047,36.1778908072062,122.098528505447)) ;
#38736 = CARTESIAN_POINT('Ctrl Pts',(-19.0089931407264,36.3679121755945,122.274279269825)) ;
#38737 = CARTESIAN_POINT('Ctrl Pts',(-18.9089342116868,36.1879230951846,121.989890796005)) ;
#38738 = CARTESIAN_POINT('Ctrl Pts',(-19.2090377913951,36.3777393520626,122.222649776035)) ;
#38739 = CARTESIAN_POINT('Ctrl Pts',(-19.1589917224772,36.1977502716528,121.925355327171)) ;
#38740 = CARTESIAN_POINT('Ctrl Pts',(-19.4186819898018,36.3877447349294,122.205814654101)) ;
#38741 = CARTESIAN_POINT('Ctrl Pts',(-19.4210472098024,36.2077556545196,121.904313326914)) ;
#38742 = CARTESIAN_POINT('Ctrl Pts',(-19.6276479448215,36.3977273739222,122.225666562334)) ;
#38743 = CARTESIAN_POINT('Ctrl Pts',(-19.6822546897999,36.2177382935123,121.929130109928)) ;
#38744 = CARTESIAN_POINT('Ctrl Pts',(-19.831109521622,36.4077714410588,122.282077039624)) ;
#38745 = CARTESIAN_POINT('Ctrl Pts',(-19.9365810272127,36.2277823606489,121.99964491067)) ;
#38746 = CARTESIAN_POINT('Ctrl Pts',(-20.0176363662993,36.4175926598628,122.370629532132)) ;
#38747 = CARTESIAN_POINT('Ctrl Pts',(-20.1697398906733,36.237603579453,122.110337795511)) ;
#38748 = CARTESIAN_POINT('Ctrl Pts',(-20.1899535608722,36.4276294988008,122.49240362926)) ;
#38749 = CARTESIAN_POINT('Ctrl Pts',(-20.3851350978056,36.247640418391,122.262557053021)) ;
#38750 = CARTESIAN_POINT('Ctrl Pts',(-20.3379053809418,36.4376539108986,122.642492380833)) ;
#38751 = CARTESIAN_POINT('Ctrl Pts',(-20.57007350028,36.2576648304888,122.450169309944)) ;
#38752 = CARTESIAN_POINT('Ctrl Pts',(-20.4558677797191,36.4475059953039,122.812743968213)) ;
#38753 = CARTESIAN_POINT('Ctrl Pts',(-20.7175254013576,36.267516914894,122.662985785886)) ;
#38754 = CARTESIAN_POINT('Ctrl Pts',(-20.5439760773838,36.457496892047,123.003382833653)) ;
#38755 = CARTESIAN_POINT('Ctrl Pts',(-20.827658912921,36.2775078116372,122.901285416347)) ;
#38756 = CARTESIAN_POINT('Ctrl Pts',(-20.5973974591388,36.467414883948,123.20495630849)) ;
#38757 = CARTESIAN_POINT('Ctrl Pts',(-20.8944336982195,36.2874258035382,123.153253367659)) ;
#38758 = CARTESIAN_POINT('Ctrl Pts',(-20.6152498950623,36.477442999405,123.415005149614)) ;
#38759 = CARTESIAN_POINT('Ctrl Pts',(-20.9167470715242,36.2974539189952,123.415814568148)) ;
#38760 = CARTESIAN_POINT('Ctrl Pts',(-20.5967150299844,36.4873281753471,123.621999291059)) ;
#38761 = CARTESIAN_POINT('Ctrl Pts',(-20.8935762348369,36.3073390949373,123.674557784491)) ;
#38762 = CARTESIAN_POINT('Ctrl Pts',(-20.5424427129043,36.497317533754,123.824877571005)) ;
#38763 = CARTESIAN_POINT('Ctrl Pts',(-20.8257335493315,36.3173284533442,123.928155184721)) ;
#38764 = CARTESIAN_POINT('Ctrl Pts',(-20.4529063543909,36.5073586813343,124.016044649924)) ;
#38765 = CARTESIAN_POINT('Ctrl Pts',(-20.7138111339089,36.3273696009244,124.167113009854)) ;
#38766 = CARTESIAN_POINT('Ctrl Pts',(-20.3343398025796,36.5171913043407,124.185369576253)) ;
#38767 = CARTESIAN_POINT('Ctrl Pts',(-20.5656005076425,36.3372022239309,124.378768633735)) ;
#38768 = CARTESIAN_POINT('Ctrl Pts',(-20.1861956020173,36.5271853754515,124.334353336419)) ;
#38769 = CARTESIAN_POINT('Ctrl Pts',(-20.3804184421246,36.3471962950417,124.564996698396)) ;
#38770 = CARTESIAN_POINT('Ctrl Pts',(-20.013585956424,36.5372140330923,124.455438892729)) ;
#38771 = CARTESIAN_POINT('Ctrl Pts',(-20.1646550508687,36.3572249526825,124.716351716275)) ;
#38772 = CARTESIAN_POINT('Ctrl Pts',(-19.8254390215131,36.5470983592851,124.543627316343)) ;
#38773 = CARTESIAN_POINT('Ctrl Pts',(-19.9294697799038,36.3671092788753,124.826585348524)) ;
#38774 = CARTESIAN_POINT('Ctrl Pts',(-19.6233034874049,36.5570641027758,124.598757212987)) ;
#38775 = CARTESIAN_POINT('Ctrl Pts',(-19.6767994745844,36.3770750223659,124.895495364901)) ;
#38776 = CARTESIAN_POINT('Ctrl Pts',(-19.4133432163963,36.567092481907,124.617767958151)) ;
#38777 = CARTESIAN_POINT('Ctrl Pts',(-19.4143489319627,36.3871034014971,124.919256362249)) ;
#38778 = CARTESIAN_POINT('Ctrl Pts',(-19.2058808015427,36.5769933281139,124.600571301318)) ;
#38779 = CARTESIAN_POINT('Ctrl Pts',(-19.1550206095312,36.397004247704,124.897758003424)) ;
#38780 = CARTESIAN_POINT('Ctrl Pts',(-19.0014191299385,36.587051985531,124.546729537717)) ;
#38781 = CARTESIAN_POINT('Ctrl Pts',(-18.8994442732489,36.4070629051212,124.830453416139)) ;
#38782 = CARTESIAN_POINT('Ctrl Pts',(-18.813096638073,36.5969095483129,124.460143866391)) ;
#38783 = CARTESIAN_POINT('Ctrl Pts',(-18.664041621049,36.416920467903,124.722218749331)) ;
#38784 = CARTESIAN_POINT('Ctrl Pts',(-18.6390013358373,36.6069779508661,124.339804591474)) ;
#38785 = CARTESIAN_POINT('Ctrl Pts',(-18.446424079418,36.4269888704563,124.571792635171)) ;
#38786 = CARTESIAN_POINT('Ctrl Pts',(-18.4916105941839,36.6168333496057,124.194162637956)) ;
#38787 = CARTESIAN_POINT('Ctrl Pts',(-18.2621870023976,36.4368442691958,124.389737932102)) ;
#38788 = CARTESIAN_POINT('Ctrl Pts',(-18.3695504756262,36.6268282166796,124.023135375574)) ;
#38789 = CARTESIAN_POINT('Ctrl Pts',(-18.109613965784,36.4468391362698,124.175952224947)) ;
#38790 = CARTESIAN_POINT('Ctrl Pts',(-18.2791165716848,36.636859511663,123.832615497264)) ;
#38791 = CARTESIAN_POINT('Ctrl Pts',(-17.9965739247964,36.4568704312532,123.937801266172)) ;
#38792 = CARTESIAN_POINT('Ctrl Pts',(-18.2237360833858,36.6467260363896,123.632712396887)) ;
#38793 = CARTESIAN_POINT('Ctrl Pts',(-17.9273507222651,36.4667369559798,123.687921184564)) ;
#38794 = CARTESIAN_POINT('Ctrl Pts',(-18.2033310226805,36.6567135070853,123.423763661605)) ;
#38795 = CARTESIAN_POINT('Ctrl Pts',(-17.9018470653367,36.4767244266755,123.426734881174)) ;
#38796 = CARTESIAN_POINT('Ctrl Pts',(-18.2193352845113,36.6666582666492,123.215274762374)) ;
#38797 = CARTESIAN_POINT('Ctrl Pts',(-17.9218551057962,36.4866691862394,123.166123729033)) ;
#38798 = CARTESIAN_POINT('Ctrl Pts',(-18.2719370323567,36.676703822598,123.010765439361)) ;
#38799 = CARTESIAN_POINT('Ctrl Pts',(-17.9876098910879,36.4967147421882,122.910487765903)) ;
#38800 = CARTESIAN_POINT('Ctrl Pts',(-18.3574522060071,36.6865634109731,122.82192143973)) ;
#38801 = CARTESIAN_POINT('Ctrl Pts',(-18.0945065088877,36.5065743305633,122.674433491179)) ;
#38802 = CARTESIAN_POINT('Ctrl Pts',(-18.4758403465642,36.6965643661092,122.648211025078)) ;
#38803 = CARTESIAN_POINT('Ctrl Pts',(-18.2424940101629,36.5165752856994,122.457296954306)) ;
#38804 = CARTESIAN_POINT('Ctrl Pts',(-18.6211027599908,36.7064685933867,122.49899007134)) ;
#38805 = CARTESIAN_POINT('Ctrl Pts',(-18.4240741922452,36.5264795129769,122.270772499989)) ;
#38806 = CARTESIAN_POINT('Ctrl Pts',(-18.7923364863628,36.7165106702819,122.37555164078)) ;
#38807 = CARTESIAN_POINT('Ctrl Pts',(-18.6381179776892,36.5365215898721,122.116476705883)) ;
#38808 = CARTESIAN_POINT('Ctrl Pts',(-18.9798717838469,36.726418282968,122.28482859885)) ;
#38809 = CARTESIAN_POINT('Ctrl Pts',(-18.8725385168202,36.5464292025582,122.003075302524)) ;
#38810 = CARTESIAN_POINT('Ctrl Pts',(-19.1832128493394,36.7364728135838,122.227207958605)) ;
#38811 = CARTESIAN_POINT('Ctrl Pts',(-19.1267156102727,36.556483733174,121.931052177894)) ;
#38812 = CARTESIAN_POINT('Ctrl Pts',(-19.3894625931079,36.7463336001326,122.206055828831)) ;
#38813 = CARTESIAN_POINT('Ctrl Pts',(-19.3845283469654,36.5663445197228,121.904614760516)) ;
#38814 = CARTESIAN_POINT('Ctrl Pts',(-19.5990077419193,36.7563273552037,122.220846428092)) ;
#38815 = CARTESIAN_POINT('Ctrl Pts',(-19.6464596606134,36.5763382747939,121.923105823605)) ;
#38816 = CARTESIAN_POINT('Ctrl Pts',(-19.8014959540694,36.7662527154437,122.271364787942)) ;
#38817 = CARTESIAN_POINT('Ctrl Pts',(-19.8995693751414,36.5862636350339,121.9862565339)) ;
#38818 = CARTESIAN_POINT('Ctrl Pts',(-19.9940544316431,36.776280644839,122.357120402506)) ;
#38819 = CARTESIAN_POINT('Ctrl Pts',(-20.1402663825866,36.5962915644292,122.093453651189)) ;
#38820 = CARTESIAN_POINT('Ctrl Pts',(-20.1664982335649,36.7861669116383,122.473197134529)) ;
#38821 = CARTESIAN_POINT('Ctrl Pts',(-20.3558196617757,36.6061778312285,122.238551973219)) ;
#38822 = CARTESIAN_POINT('Ctrl Pts',(-20.3183982755101,36.7961986805365,122.619450743956)) ;
#38823 = CARTESIAN_POINT('Ctrl Pts',(-20.5456928031765,36.6162096001267,122.421371062142)) ;
#38824 = CARTESIAN_POINT('Ctrl Pts',(-20.4409436536401,36.8060802763801,122.787245264454)) ;
#38825 = CARTESIAN_POINT('Ctrl Pts',(-20.6988722846578,36.6260911959703,122.631115950186)) ;
#38826 = CARTESIAN_POINT('Ctrl Pts',(-20.5341804059787,36.8161421618481,122.977086052336)) ;
#38827 = CARTESIAN_POINT('Ctrl Pts',(-20.8154157384353,36.6361530814383,122.868418182674)) ;
#38828 = CARTESIAN_POINT('Ctrl Pts',(-20.5919244424178,36.825999595867,123.176140531021)) ;
#38829 = CARTESIAN_POINT('Ctrl Pts',(-20.8875930299572,36.6460105154571,123.117237354215)) ;
#38830 = CARTESIAN_POINT('Ctrl Pts',(-20.6149712049277,36.8359928389089,123.384935530242)) ;
#38831 = CARTESIAN_POINT('Ctrl Pts',(-20.9163988743964,36.6560037584991,123.378230437878)) ;
#38832 = CARTESIAN_POINT('Ctrl Pts',(-20.6015124206239,36.8459235997953,123.593287168939)) ;
#38833 = CARTESIAN_POINT('Ctrl Pts',(-20.8995719079285,36.6659345193854,123.638673612043)) ;
#38834 = CARTESIAN_POINT('Ctrl Pts',(-20.5353308402502,36.8592725919925,123.866051377186)) ;
#38835 = CARTESIAN_POINT('Ctrl Pts',(-20.816844696695,36.6792835115826,123.979609103894)) ;
#38836 = CARTESIAN_POINT('Ctrl Pts',(-20.3999609319661,36.8725409648089,124.11357862058)) ;
#38837 = CARTESIAN_POINT('Ctrl Pts',(-20.6476556409082,36.6925518843991,124.288994177513)) ;
#38838 = CARTESIAN_POINT('Ctrl Pts',(-20.2075188150344,36.8858239061933,124.315902403528)) ;
#38839 = CARTESIAN_POINT('Ctrl Pts',(-20.4070652076919,36.7058348257834,124.541941671603)) ;
#38840 = CARTESIAN_POINT('Ctrl Pts',(-20.0375727801162,36.8958666920355,124.441171046121)) ;
#38841 = CARTESIAN_POINT('Ctrl Pts',(-20.1946380685307,36.7158776116257,124.698516250098)) ;
#38842 = CARTESIAN_POINT('Ctrl Pts',(-19.8521787979742,36.9057166345876,124.533432305183)) ;
#38843 = CARTESIAN_POINT('Ctrl Pts',(-19.9628921815121,36.7257275541777,124.813842499305)) ;
#38844 = CARTESIAN_POINT('Ctrl Pts',(-19.6507731123258,36.9157138675065,124.593480412264)) ;
#38845 = CARTESIAN_POINT('Ctrl Pts',(-19.711136668814,36.7357247870967,124.888900023819)) ;
#38846 = CARTESIAN_POINT('Ctrl Pts',(-19.4415809415258,36.9257287628411,124.617367629168)) ;
#38847 = CARTESIAN_POINT('Ctrl Pts',(-19.4496388355462,36.7457396824312,124.918754107252)) ;
#38848 = CARTESIAN_POINT('Ctrl Pts',(-19.1637149095619,36.9389684394793,124.600711262707)) ;
#38849 = CARTESIAN_POINT('Ctrl Pts',(-19.1023419164325,36.7589793590695,124.897941856182)) ;
#38850 = CARTESIAN_POINT('Ctrl Pts',(-18.8297170296114,36.9555156638846,124.490312279794)) ;
#38851 = CARTESIAN_POINT('Ctrl Pts',(-18.6847931249535,36.7755265834747,124.759912522022)) ;
#38852 = CARTESIAN_POINT('Ctrl Pts',(-18.5515569849989,36.9721631010157,124.271299498721)) ;
#38853 = CARTESIAN_POINT('Ctrl Pts',(-18.3371603329955,36.7921740206059,124.486198909342)) ;
#38854 = CARTESIAN_POINT('Ctrl Pts',(-18.3844875359923,36.9854525984939,124.047410122767)) ;
#38855 = CARTESIAN_POINT('Ctrl Pts',(-18.12827768874,36.8054635180841,124.206288377177)) ;
#38856 = CARTESIAN_POINT('Ctrl Pts',(-18.2905524045651,36.9953260063163,123.862298699992)) ;
#38857 = CARTESIAN_POINT('Ctrl Pts',(-18.0108710101384,36.8153369259064,123.974907927286)) ;
#38858 = CARTESIAN_POINT('Ctrl Pts',(-18.2290667315247,37.005378383909,123.660120832007)) ;
#38859 = CARTESIAN_POINT('Ctrl Pts',(-17.9340138083653,36.8253893034992,123.722181735782)) ;
#38860 = CARTESIAN_POINT('Ctrl Pts',(-18.2040801154488,37.0152820374499,123.45340205248)) ;
#38861 = CARTESIAN_POINT('Ctrl Pts',(-17.9027830694493,36.8352929570401,123.463785283057)) ;
#38862 = CARTESIAN_POINT('Ctrl Pts',(-18.214904553946,37.0252263064452,123.244652571559)) ;
#38863 = CARTESIAN_POINT('Ctrl Pts',(-17.9163185740289,36.8452372260354,123.20284412537)) ;
#38864 = CARTESIAN_POINT('Ctrl Pts',(-18.2776834319682,37.0385573147779,122.97143393021)) ;
#38865 = CARTESIAN_POINT('Ctrl Pts',(-17.9947816308902,36.858568234368,122.861344091151)) ;
#38866 = CARTESIAN_POINT('Ctrl Pts',(-18.4435275534842,37.0551788953021,122.659444683358)) ;
#38867 = CARTESIAN_POINT('Ctrl Pts',(-18.2021201495305,36.8751898148923,122.471324046432)) ;
#38868 = CARTESIAN_POINT('Ctrl Pts',(-18.704290384894,37.0717215660005,122.423272162924)) ;
#38869 = CARTESIAN_POINT('Ctrl Pts',(-18.5280140337885,36.8917324855907,122.176159129559)) ;
#38870 = CARTESIAN_POINT('Ctrl Pts',(-18.9539020590981,37.0850707255635,122.295120923871)) ;
#38871 = CARTESIAN_POINT('Ctrl Pts',(-18.8400831149199,36.9050816451537,122.015936356895)) ;
#38872 = CARTESIAN_POINT('Ctrl Pts',(-19.2195445907984,37.098298875723,122.212649877143)) ;
#38873 = CARTESIAN_POINT('Ctrl Pts',(-19.1721122727265,36.9183097953132,121.912858361349)) ;
#38874 = CARTESIAN_POINT('Ctrl Pts',(-19.5728022237674,37.1149295528605,122.198387297674)) ;
#38875 = CARTESIAN_POINT('Ctrl Pts',(-19.6137036972976,36.9349404724507,121.895030598784)) ;
#38876 = CARTESIAN_POINT('Ctrl Pts',(-19.9761409789066,37.1348324921486,122.326670598827)) ;
#38877 = CARTESIAN_POINT('Ctrl Pts',(-20.1178689308349,36.9548434117388,122.055389405925)) ;
#38878 = CARTESIAN_POINT('Ctrl Pts',(-20.3116476022959,37.1547353587518,122.584460179412)) ;
#38879 = CARTESIAN_POINT('Ctrl Pts',(-20.5372508618849,36.974746278342,122.377628584665)) ;
#38880 = CARTESIAN_POINT('Ctrl Pts',(-20.539804233534,37.1746485238567,122.941249904607)) ;
#38881 = CARTESIAN_POINT('Ctrl Pts',(-20.8224429653255,36.9946594434469,122.823616943163)) ;
#38882 = CARTESIAN_POINT('Ctrl Pts',(-20.6323994014347,37.194684352998,123.35701958835)) ;
#38883 = CARTESIAN_POINT('Ctrl Pts',(-20.9381837030193,37.0146952725882,123.343330198134)) ;
#38884 = CARTESIAN_POINT('Ctrl Pts',(-20.5783831690263,37.2145029278761,123.775043446031)) ;
#38885 = CARTESIAN_POINT('Ctrl Pts',(-20.8706604307742,37.0345138474663,123.86585779173)) ;
#38886 = CARTESIAN_POINT('Ctrl Pts',(-20.3841900567002,37.2344732289181,124.152499639715)) ;
#38887 = CARTESIAN_POINT('Ctrl Pts',(-20.6279168053661,37.0544841485082,124.337676429596)) ;
#38888 = CARTESIAN_POINT('Ctrl Pts',(-20.0739514395831,37.2543647612826,124.440192864302)) ;
#38889 = CARTESIAN_POINT('Ctrl Pts',(-20.2401177850966,37.0743756808728,124.6972903502)) ;
#38890 = CARTESIAN_POINT('Ctrl Pts',(-19.6816910451499,37.2743878590991,124.605446609559)) ;
#38891 = CARTESIAN_POINT('Ctrl Pts',(-19.7497910668665,37.0943987786893,124.903855399338)) ;
#38892 = CARTESIAN_POINT('Ctrl Pts',(-19.2612575086077,37.2941846120191,124.626987367423)) ;
#38893 = CARTESIAN_POINT('Ctrl Pts',(-19.2242516782376,37.1141955316092,124.930779156433)) ;
#38894 = CARTESIAN_POINT('Ctrl Pts',(-18.8551235164096,37.3141457005079,124.503854762639)) ;
#38895 = CARTESIAN_POINT('Ctrl Pts',(-18.7165851062423,37.134156620098,124.776862536651)) ;
#38896 = CARTESIAN_POINT('Ctrl Pts',(-18.5155691321444,37.33412396944,124.248549659237)) ;
#38897 = CARTESIAN_POINT('Ctrl Pts',(-18.2921431805253,37.1541348890302,124.457730120123)) ;
#38898 = CARTESIAN_POINT('Ctrl Pts',(-18.2848840893229,37.353943984231,123.895912818502)) ;
#38899 = CARTESIAN_POINT('Ctrl Pts',(-18.0037890981004,37.1739549038212,124.016935959748)) ;
#38900 = CARTESIAN_POINT('Ctrl Pts',(-18.1867266757181,37.3738823934829,123.483465881593)) ;
#38901 = CARTESIAN_POINT('Ctrl Pts',(-17.8810922819459,37.193893313073,123.501378325244)) ;
#38902 = CARTESIAN_POINT('Ctrl Pts',(-18.2364290835758,37.3939295108753,123.060063699983)) ;
#38903 = CARTESIAN_POINT('Ctrl Pts',(-17.9432206010294,37.2139404304655,122.972124751347)) ;
#38904 = CARTESIAN_POINT('Ctrl Pts',(-18.425848548575,37.4137757567091,122.683031202947)) ;
#38905 = CARTESIAN_POINT('Ctrl Pts',(-18.1799938361584,37.2337866762993,122.50083649183)) ;
#38906 = CARTESIAN_POINT('Ctrl Pts',(-18.7315064002048,37.4336247252212,122.391977885503)) ;
#38907 = CARTESIAN_POINT('Ctrl Pts',(-18.5620635940809,37.2536356448114,122.137020325859)) ;
#38908 = CARTESIAN_POINT('Ctrl Pts',(-19.1222176535589,37.4536750275325,122.221508253603)) ;
#38909 = CARTESIAN_POINT('Ctrl Pts',(-19.0504528465685,37.2736859471226,121.923931865061)) ;
#38910 = CARTESIAN_POINT('Ctrl Pts',(-19.5432296563708,37.4735099499637,122.194969642124)) ;
#38911 = CARTESIAN_POINT('Ctrl Pts',(-19.5767155011181,37.2935208695539,121.890757345923)) ;
#38912 = CARTESIAN_POINT('Ctrl Pts',(-19.9499494548822,37.4934403511896,122.313396694246)) ;
#38913 = CARTESIAN_POINT('Ctrl Pts',(-20.0851149441252,37.3134512707798,122.038788804376)) ;
#38914 = CARTESIAN_POINT('Ctrl Pts',(-20.2916433860762,37.5133252965484,122.562694249305)) ;
#38915 = CARTESIAN_POINT('Ctrl Pts',(-20.5122328950724,37.3333362161386,122.350407887825)) ;
#38916 = CARTESIAN_POINT('Ctrl Pts',(-20.5292680047328,37.5333979046998,122.917125700607)) ;
#38917 = CARTESIAN_POINT('Ctrl Pts',(-20.8092661803388,37.35340882429,122.793446550303)) ;
#38918 = CARTESIAN_POINT('Ctrl Pts',(-20.6303478789093,37.5531892210279,123.325688691572)) ;
#38919 = CARTESIAN_POINT('Ctrl Pts',(-20.9356180405514,37.3732001406181,123.304147384371)) ;
#38920 = CARTESIAN_POINT('Ctrl Pts',(-20.5868633210281,37.5731540107952,123.747925395275)) ;
#38921 = CARTESIAN_POINT('Ctrl Pts',(-20.8812658706994,37.3931649303854,123.831943312422)) ;
#38922 = CARTESIAN_POINT('Ctrl Pts',(-20.400758322157,37.5931369665455,124.129898349839)) ;
#38923 = CARTESIAN_POINT('Ctrl Pts',(-20.6486375256377,37.4131478861357,124.309410738595)) ;
#38924 = CARTESIAN_POINT('Ctrl Pts',(-20.0987238949301,37.6129454885216,124.423499457933)) ;
#38925 = CARTESIAN_POINT('Ctrl Pts',(-20.2710983170849,37.4329564081118,124.676413569075)) ;
#38926 = CARTESIAN_POINT('Ctrl Pts',(-19.7115115108839,37.6329310632575,124.598340112043)) ;
#38927 = CARTESIAN_POINT('Ctrl Pts',(-19.7870846026181,37.4529419828477,124.894968051446)) ;
#38928 = CARTESIAN_POINT('Ctrl Pts',(-19.2898630183284,37.6528137033259,124.630311193854)) ;
#38929 = CARTESIAN_POINT('Ctrl Pts',(-19.2600251516801,37.4728246229161,124.934935958252)) ;
#38930 = CARTESIAN_POINT('Ctrl Pts',(-18.8812143689227,37.6727690154578,124.516434264361)) ;
#38931 = CARTESIAN_POINT('Ctrl Pts',(-18.7492134555488,37.492779935048,124.792594096321)) ;
#38932 = CARTESIAN_POINT('Ctrl Pts',(-18.5370718720123,37.6926433720656,124.271071448135)) ;
#38933 = CARTESIAN_POINT('Ctrl Pts',(-18.3190332544941,37.5126542916557,124.485894779844)) ;
#38934 = CARTESIAN_POINT('Ctrl Pts',(-18.295856749821,37.7126255789266,123.921365626854)) ;
#38935 = CARTESIAN_POINT('Ctrl Pts',(-18.0175106059338,37.5326364985168,124.048765115421)) ;
#38936 = CARTESIAN_POINT('Ctrl Pts',(-18.1889170459794,37.7325566568766,123.511199159604)) ;
#38937 = CARTESIAN_POINT('Ctrl Pts',(-17.8838308617146,37.5525675764668,123.536059048155)) ;
#38938 = CARTESIAN_POINT('Ctrl Pts',(-18.2282802535352,37.7524836317316,123.089417927906)) ;
#38939 = CARTESIAN_POINT('Ctrl Pts',(-17.9330320753594,37.5724945513218,123.008830581994)) ;
#38940 = CARTESIAN_POINT('Ctrl Pts',(-18.4076686429173,37.7723160906805,122.707716966432)) ;
#38941 = CARTESIAN_POINT('Ctrl Pts',(-18.1572546227827,37.5923270102706,122.5317096236)) ;
#38942 = CARTESIAN_POINT('Ctrl Pts',(-18.6583803627313,37.7889737748557,122.457695839393)) ;
#38943 = CARTESIAN_POINT('Ctrl Pts',(-18.4706659457607,37.6089846944459,122.219158783992)) ;
#38944 = CARTESIAN_POINT('Ctrl Pts',(-18.8998510224225,37.8022229987628,122.318670298478)) ;
#38945 = CARTESIAN_POINT('Ctrl Pts',(-18.7724796761742,37.622233918353,122.045392670277)) ;
#38946 = CARTESIAN_POINT('Ctrl Pts',(-19.0983967328829,37.812272020214,122.246576703272)) ;
#38947 = CARTESIAN_POINT('Ctrl Pts',(-19.0206690088964,37.6322829398042,121.955269929657)) ;
#38948 = CARTESIAN_POINT('Ctrl Pts',(-19.3025665370279,37.8221320284445,122.210682156202)) ;
#38949 = CARTESIAN_POINT('Ctrl Pts',(-19.2758657648951,37.6421429480347,121.910397904095)) ;
#38950 = CARTESIAN_POINT('Ctrl Pts',(-19.5818034711638,37.8354155416691,122.209888694931)) ;
#38951 = CARTESIAN_POINT('Ctrl Pts',(-19.6249794284408,37.6554264612593,121.909413584205)) ;
#38952 = CARTESIAN_POINT('Ctrl Pts',(-19.9238580353541,37.8520614606699,122.300927522182)) ;
#38953 = CARTESIAN_POINT('Ctrl Pts',(-20.0524638778984,37.6720723802601,122.023188295544)) ;
#38954 = CARTESIAN_POINT('Ctrl Pts',(-20.2129442647701,37.868615438486,122.501691868279)) ;
#38955 = CARTESIAN_POINT('Ctrl Pts',(-20.4138807769964,37.6886263580762,122.274169668355)) ;
#38956 = CARTESIAN_POINT('Ctrl Pts',(-20.3943636779236,37.8819751674576,122.716138212852)) ;
#38957 = CARTESIAN_POINT('Ctrl Pts',(-20.6406243713775,37.7019860870478,122.542201540459)) ;
#38958 = CARTESIAN_POINT('Ctrl Pts',(-20.4992200878676,37.8918682192543,122.895764414402)) ;
#38959 = CARTESIAN_POINT('Ctrl Pts',(-20.7717039791491,37.7118791388445,122.766737576654)) ;
#38960 = CARTESIAN_POINT('Ctrl Pts',(-20.5722587350757,37.9018581845353,123.092651468805)) ;
#38961 = CARTESIAN_POINT('Ctrl Pts',(-20.863003128302,37.7218691041255,123.012844193448)) ;
#38962 = CARTESIAN_POINT('Ctrl Pts',(-20.6099889776979,37.9118100653962,123.298474001835)) ;
#38963 = CARTESIAN_POINT('Ctrl Pts',(-20.9101691765869,37.7318209849863,123.270122215442)) ;
#38964 = CARTESIAN_POINT('Ctrl Pts',(-20.6112435236213,37.921858417088,123.509695858603)) ;
#38965 = CARTESIAN_POINT('Ctrl Pts',(-20.9117400295887,37.7418693366781,123.534149528091)) ;
#38966 = CARTESIAN_POINT('Ctrl Pts',(-20.5767689441837,37.9316997011942,123.713719442)) ;
#38967 = CARTESIAN_POINT('Ctrl Pts',(-20.8686496158708,37.7517106207844,123.789179451351)) ;
#38968 = CARTESIAN_POINT('Ctrl Pts',(-20.5068028273446,37.9416864043198,123.911631328625)) ;
#38969 = CARTESIAN_POINT('Ctrl Pts',(-20.7811945959471,37.76169732391,124.036570320632)) ;
#38970 = CARTESIAN_POINT('Ctrl Pts',(-20.4041443174755,37.9516214331373,124.093573751061)) ;
#38971 = CARTESIAN_POINT('Ctrl Pts',(-20.6528738764456,37.7716323527274,124.263999794923)) ;
#38972 = CARTESIAN_POINT('Ctrl Pts',(-20.2697516088806,37.9616772280442,124.256720400925)) ;
#38973 = CARTESIAN_POINT('Ctrl Pts',(-20.4848851322736,37.7816881476343,124.467934944168)) ;
#38974 = CARTESIAN_POINT('Ctrl Pts',(-20.112868940614,37.9715055913335,124.391230410189)) ;
#38975 = CARTESIAN_POINT('Ctrl Pts',(-20.2887835293131,37.7915165109236,124.636074676851)) ;
#38976 = CARTESIAN_POINT('Ctrl Pts',(-19.9310077930652,37.9815665612314,124.499176168369)) ;
#38977 = CARTESIAN_POINT('Ctrl Pts',(-20.0614584856312,37.8015774808215,124.771009318102)) ;
#38978 = CARTESIAN_POINT('Ctrl Pts',(-19.7359423603849,37.9914808401212,124.572672275179)) ;
#38979 = CARTESIAN_POINT('Ctrl Pts',(-19.8176275658796,37.8114917597113,124.862882128351)) ;
#38980 = CARTESIAN_POINT('Ctrl Pts',(-19.5292180654532,38.0014898345894,124.611953243679)) ;
#38981 = CARTESIAN_POINT('Ctrl Pts',(-19.5592226441378,37.8215007541796,124.911986102297)) ;
#38982 = CARTESIAN_POINT('Ctrl Pts',(-19.3183758075429,38.0115196691532,124.614317888065)) ;
#38983 = CARTESIAN_POINT('Ctrl Pts',(-19.2956698137469,37.8315305887433,124.914944725323)) ;
#38984 = CARTESIAN_POINT('Ctrl Pts',(-19.1138048120896,38.0213778992254,124.581009867866)) ;
#38985 = CARTESIAN_POINT('Ctrl Pts',(-19.039955392314,37.8413888188156,124.873312424848)) ;
#38986 = CARTESIAN_POINT('Ctrl Pts',(-18.9152985830758,38.0313766049678,124.51196923972)) ;
#38987 = CARTESIAN_POINT('Ctrl Pts',(-18.7918216048149,37.851387524558,124.787014243673)) ;
#38988 = CARTESIAN_POINT('Ctrl Pts',(-18.7335213440721,38.0412712608866,124.410757402581)) ;
#38989 = CARTESIAN_POINT('Ctrl Pts',(-18.5645984860239,37.8612821804768,124.660501733437)) ;
#38990 = CARTESIAN_POINT('Ctrl Pts',(-18.5694307222782,38.0513343252705,124.27728255479)) ;
#38991 = CARTESIAN_POINT('Ctrl Pts',(-18.3594834847506,37.8713452448607,124.493660346737)) ;
#38992 = CARTESIAN_POINT('Ctrl Pts',(-18.4338627813113,38.0611739835504,124.120992090027)) ;
#38993 = CARTESIAN_POINT('Ctrl Pts',(-18.190021216124,37.8811849031406,124.298298757622)) ;
#38994 = CARTESIAN_POINT('Ctrl Pts',(-18.3248772146404,38.0712371506323,123.939698712811)) ;
#38995 = CARTESIAN_POINT('Ctrl Pts',(-18.0537869453048,37.8912480702225,124.071683477149)) ;
#38996 = CARTESIAN_POINT('Ctrl Pts',(-18.2504447417178,38.0811313957594,123.745439174698)) ;
#38997 = CARTESIAN_POINT('Ctrl Pts',(-17.960743677064,37.9011423153496,123.828859729591)) ;
#38998 = CARTESIAN_POINT('Ctrl Pts',(-18.2101341066762,38.091073217364,123.54038139259)) ;
#38999 = CARTESIAN_POINT('Ctrl Pts',(-17.9103527061802,37.9110841369542,123.572537760111)) ;
#39000 = CARTESIAN_POINT('Ctrl Pts',(-18.2059368471232,38.1010757482821,123.330110491768)) ;
#39001 = CARTESIAN_POINT('Ctrl Pts',(-17.9051034698684,37.9210866678723,123.309699103463)) ;
#39002 = CARTESIAN_POINT('Ctrl Pts',(-18.238734440385,38.1111103747396,123.12172723179)) ;
#39003 = CARTESIAN_POINT('Ctrl Pts',(-17.9460977833977,37.9311212943298,123.049219622121)) ;
#39004 = CARTESIAN_POINT('Ctrl Pts',(-18.305619068495,38.120955909726,122.925840042337)) ;
#39005 = CARTESIAN_POINT('Ctrl Pts',(-18.0297012300199,37.9409668293162,122.804359246447)) ;
#39006 = CARTESIAN_POINT('Ctrl Pts',(-18.4064882596098,38.130939334565,122.74180463094)) ;
#39007 = CARTESIAN_POINT('Ctrl Pts',(-18.155785528009,37.9509502541552,122.574313582094)) ;
#39008 = CARTESIAN_POINT('Ctrl Pts',(-18.537392601509,38.1408897249301,122.578629160492)) ;
#39009 = CARTESIAN_POINT('Ctrl Pts',(-18.3194140987467,37.9609006445203,122.370342409451)) ;
#39010 = CARTESIAN_POINT('Ctrl Pts',(-18.6952097088462,38.1508873652272,122.439785210272)) ;
#39011 = CARTESIAN_POINT('Ctrl Pts',(-18.5166838775073,37.9708982848174,122.196785487639)) ;
#39012 = CARTESIAN_POINT('Ctrl Pts',(-18.8756765943063,38.1609264457904,122.330377777602)) ;
#39013 = CARTESIAN_POINT('Ctrl Pts',(-18.7422660731798,37.9809373653805,122.060023983212)) ;
#39014 = CARTESIAN_POINT('Ctrl Pts',(-19.0680799590173,38.1707525965595,122.255148656096)) ;
#39015 = CARTESIAN_POINT('Ctrl Pts',(-18.9827700674424,37.9907635161496,121.965984935023)) ;
#39016 = CARTESIAN_POINT('Ctrl Pts',(-19.2752831931946,38.1808091714886,122.213190167837)) ;
#39017 = CARTESIAN_POINT('Ctrl Pts',(-19.2417735141218,38.0008200910788,121.913534414726)) ;
#39018 = CARTESIAN_POINT('Ctrl Pts',(-19.4842136350837,38.1907497108689,122.208272468333)) ;
#39019 = CARTESIAN_POINT('Ctrl Pts',(-19.5029368385438,38.010760630459,121.907384733484)) ;
#39020 = CARTESIAN_POINT('Ctrl Pts',(-19.6901672000189,38.2006541038453,122.238947693484)) ;
#39021 = CARTESIAN_POINT('Ctrl Pts',(-19.7603796759011,38.0206650234355,121.945726450794)) ;
#39022 = CARTESIAN_POINT('Ctrl Pts',(-19.8904397603091,38.2107007580502,122.305985318567)) ;
#39023 = CARTESIAN_POINT('Ctrl Pts',(-20.0107210558976,38.0307116776404,122.029521129551)) ;
#39024 = CARTESIAN_POINT('Ctrl Pts',(-20.073374575685,38.2205963199886,122.405120062079)) ;
#39025 = CARTESIAN_POINT('Ctrl Pts',(-20.2393912303879,38.0406072395788,122.153437721964)) ;
#39026 = CARTESIAN_POINT('Ctrl Pts',(-20.239009195266,38.2306583978341,122.536650134801)) ;
#39027 = CARTESIAN_POINT('Ctrl Pts',(-20.4464358605155,38.0506693174243,122.317848314832)) ;
#39028 = CARTESIAN_POINT('Ctrl Pts',(-20.3763552173519,38.2405010962479,122.691451330782)) ;
#39029 = CARTESIAN_POINT('Ctrl Pts',(-20.6181207396149,38.0605120158381,122.511348876355)) ;
#39030 = CARTESIAN_POINT('Ctrl Pts',(-20.4867630860936,38.2504918712094,122.870097720652)) ;
#39031 = CARTESIAN_POINT('Ctrl Pts',(-20.7561325944184,38.0705027907995,122.734655821547)) ;
#39032 = CARTESIAN_POINT('Ctrl Pts',(-20.5639707241842,38.2604197362285,123.064019607399)) ;
#39033 = CARTESIAN_POINT('Ctrl Pts',(-20.8526444302955,38.0804306558186,122.97705779297)) ;
#39034 = CARTESIAN_POINT('Ctrl Pts',(-20.606936524891,38.2704084809947,123.269576207478)) ;
#39035 = CARTESIAN_POINT('Ctrl Pts',(-20.9063538532472,38.0904194005849,123.234003272372)) ;
#39036 = CARTESIAN_POINT('Ctrl Pts',(-20.6132774081827,38.2804412665816,123.480405040988)) ;
#39037 = CARTESIAN_POINT('Ctrl Pts',(-20.9142822163388,38.1004521861718,123.497539173059)) ;
#39038 = CARTESIAN_POINT('Ctrl Pts',(-20.5836278378137,38.2903079512023,123.685696146507)) ;
#39039 = CARTESIAN_POINT('Ctrl Pts',(-20.8772223147978,38.1103188707925,123.754154223946)) ;
#39040 = CARTESIAN_POINT('Ctrl Pts',(-20.5187275010846,38.3002698433654,123.884820325634)) ;
#39041 = CARTESIAN_POINT('Ctrl Pts',(-20.796098729083,38.1202807629555,124.00306041156)) ;
#39042 = CARTESIAN_POINT('Ctrl Pts',(-20.4192419119231,38.310303320278,124.070811287122)) ;
#39043 = CARTESIAN_POINT('Ctrl Pts',(-20.6717436693402,38.1303142398682,124.235550043446)) ;
#39044 = CARTESIAN_POINT('Ctrl Pts',(-20.2911476331738,38.3201876615263,124.234467456338)) ;
#39045 = CARTESIAN_POINT('Ctrl Pts',(-20.5116269404507,38.1401985811165,124.440122137417)) ;
#39046 = CARTESIAN_POINT('Ctrl Pts',(-20.1338310125617,38.3302506036474,124.375873737008)) ;
#39047 = CARTESIAN_POINT('Ctrl Pts',(-20.314982722804,38.1502615232376,124.616881340086)) ;
#39048 = CARTESIAN_POINT('Ctrl Pts',(-19.9581597878484,38.340101005267,124.485559805927)) ;
#39049 = CARTESIAN_POINT('Ctrl Pts',(-20.0953938753125,38.1601119248572,124.75399118934)) ;
#39050 = CARTESIAN_POINT('Ctrl Pts',(-19.7628910644464,38.3501278940566,124.564952690496)) ;
#39051 = CARTESIAN_POINT('Ctrl Pts',(-19.8513087068657,38.1701388136468,124.853234002118)) ;
#39052 = CARTESIAN_POINT('Ctrl Pts',(-19.5566368100917,38.3601565090128,124.608705273283)) ;
#39053 = CARTESIAN_POINT('Ctrl Pts',(-19.5934913762966,38.180167428603,124.907926696721)) ;
#39054 = CARTESIAN_POINT('Ctrl Pts',(-19.3498081641325,38.3700017321329,124.616238591243)) ;
#39055 = CARTESIAN_POINT('Ctrl Pts',(-19.3349545228512,38.1900126517231,124.917345289644)) ;
#39056 = CARTESIAN_POINT('Ctrl Pts',(-19.1416901454092,38.3799924159389,124.587880295423)) ;
#39057 = CARTESIAN_POINT('Ctrl Pts',(-19.0748065717791,38.200003335529,124.881899109287)) ;
#39058 = CARTESIAN_POINT('Ctrl Pts',(-18.9408634995236,38.3900302980113,124.52306847004)) ;
#39059 = CARTESIAN_POINT('Ctrl Pts',(-18.8237728136587,38.2100412176015,124.800886156502)) ;
#39060 = CARTESIAN_POINT('Ctrl Pts',(-18.7577593662331,38.3998746576501,124.426589014127)) ;
#39061 = CARTESIAN_POINT('Ctrl Pts',(-18.5948907895903,38.2198855772403,124.680287851549)) ;
#39062 = CARTESIAN_POINT('Ctrl Pts',(-18.5916294729954,38.4098595282649,124.298321906934)) ;
#39063 = CARTESIAN_POINT('Ctrl Pts',(-18.3872272286313,38.2298704478551,124.519955106636)) ;
#39064 = CARTESIAN_POINT('Ctrl Pts',(-18.4508291327248,38.4197988115935,124.14388654102)) ;
#39065 = CARTESIAN_POINT('Ctrl Pts',(-18.2112252563258,38.2398097311837,124.326911572876)) ;
#39066 = CARTESIAN_POINT('Ctrl Pts',(-18.3379263587694,38.4298394209667,123.965558708293)) ;
#39067 = CARTESIAN_POINT('Ctrl Pts',(-18.0700954991663,38.2498503405568,124.104002776389)) ;
#39068 = CARTESIAN_POINT('Ctrl Pts',(-18.2587866795904,38.4397242718799,123.77338134412)) ;
#39069 = CARTESIAN_POINT('Ctrl Pts',(-17.9711690913836,38.2597351914701,123.863780801311)) ;
#39070 = CARTESIAN_POINT('Ctrl Pts',(-18.2134543934735,38.4497262280487,123.568085773831)) ;
#39071 = CARTESIAN_POINT('Ctrl Pts',(-17.9145022539085,38.2697371476389,123.607161518805)) ;
#39072 = CARTESIAN_POINT('Ctrl Pts',(-18.2043619080485,38.4596448247692,123.359731016795)) ;
#39073 = CARTESIAN_POINT('Ctrl Pts',(-17.9031351939058,38.2796557443593,123.346717419447)) ;
#39074 = CARTESIAN_POINT('Ctrl Pts',(-18.2319694185159,38.469691646845,123.150356999405)) ;
#39075 = CARTESIAN_POINT('Ctrl Pts',(-17.9376431227028,38.2897025664352,123.084999919359)) ;
#39076 = CARTESIAN_POINT('Ctrl Pts',(-18.2942537247054,38.4795659279577,122.952295745254)) ;
#39077 = CARTESIAN_POINT('Ctrl Pts',(-18.0154975115809,38.2995768475479,122.837421943635)) ;
#39078 = CARTESIAN_POINT('Ctrl Pts',(-18.3915795652772,38.4896201280023,122.764705800279)) ;
#39079 = CARTESIAN_POINT('Ctrl Pts',(-18.137153510748,38.3096310475925,122.6029341291)) ;
#39080 = CARTESIAN_POINT('Ctrl Pts',(-18.517948341089,38.4995155576375,122.599403244728)) ;
#39081 = CARTESIAN_POINT('Ctrl Pts',(-18.295114007529,38.3195264772277,122.396304412865)) ;
#39082 = CARTESIAN_POINT('Ctrl Pts',(-18.6735897291934,38.5095771859549,122.456195028724)) ;
#39083 = CARTESIAN_POINT('Ctrl Pts',(-18.489664633959,38.329588105545,122.217293421635)) ;
#39084 = CARTESIAN_POINT('Ctrl Pts',(-18.8479034008404,38.5194218147848,122.344605396143)) ;
#39085 = CARTESIAN_POINT('Ctrl Pts',(-18.7075571482526,38.3394327343749,122.077804596449)) ;
#39086 = CARTESIAN_POINT('Ctrl Pts',(-19.0408840506454,38.5293818623904,122.263352848004)) ;
#39087 = CARTESIAN_POINT('Ctrl Pts',(-18.9487829946341,38.3493927819806,121.976237815582)) ;
#39088 = CARTESIAN_POINT('Ctrl Pts',(-19.2467307026046,38.5394201685644,122.216882947286)) ;
#39089 = CARTESIAN_POINT('Ctrl Pts',(-19.2060908983503,38.3594310881546,121.918149353358)) ;
#39090 = CARTESIAN_POINT('Ctrl Pts',(-19.4540764654965,38.5492934679971,122.206624033393)) ;
#39091 = CARTESIAN_POINT('Ctrl Pts',(-19.4652741750453,38.3693043875873,121.905324657116)) ;
#39092 = CARTESIAN_POINT('Ctrl Pts',(-19.6641424754752,38.5593667295834,122.233106532609)) ;
#39093 = CARTESIAN_POINT('Ctrl Pts',(-19.727856392787,38.3793776491735,121.938426707884)) ;
#39094 = CARTESIAN_POINT('Ctrl Pts',(-19.8615036156616,38.5691869555401,122.293853612687)) ;
#39095 = CARTESIAN_POINT('Ctrl Pts',(-19.9745595743233,38.3891978751303,122.014360134758)) ;
#39096 = CARTESIAN_POINT('Ctrl Pts',(-20.0501587943975,38.5792660194796,122.390213788691)) ;
#39097 = CARTESIAN_POINT('Ctrl Pts',(-20.2103785147043,38.3992769390698,122.13480937885)) ;
#39098 = CARTESIAN_POINT('Ctrl Pts',(-20.2155221291384,38.5891161094994,122.514954133078)) ;
#39099 = CARTESIAN_POINT('Ctrl Pts',(-20.4170842341613,38.4091270290896,122.290734959932)) ;
#39100 = CARTESIAN_POINT('Ctrl Pts',(-20.3599977542973,38.5991948631132,122.669874910187)) ;
#39101 = CARTESIAN_POINT('Ctrl Pts',(-20.5976790050337,38.4192057827034,122.484385049219)) ;
#39102 = CARTESIAN_POINT('Ctrl Pts',(-20.4726208048676,38.6090163303726,122.842988026387)) ;
#39103 = CARTESIAN_POINT('Ctrl Pts',(-20.7384592822056,38.4290272499628,122.700777392745)) ;
#39104 = CARTESIAN_POINT('Ctrl Pts',(-20.5557471903728,38.6190819287303,123.037535696826)) ;
#39105 = CARTESIAN_POINT('Ctrl Pts',(-20.8423676550526,38.4390928483204,122.943961403753)) ;
#39106 = CARTESIAN_POINT('Ctrl Pts',(-20.6030203243983,38.628984584505,123.240335099083)) ;
#39107 = CARTESIAN_POINT('Ctrl Pts',(-20.9014598752685,38.4489955040952,123.197461404654)) ;
#39108 = CARTESIAN_POINT('Ctrl Pts',(-20.6145926696744,38.6390354103346,123.451275235179)) ;
#39109 = CARTESIAN_POINT('Ctrl Pts',(-20.9159258762497,38.4590463299248,123.461136272489)) ;
#39110 = CARTESIAN_POINT('Ctrl Pts',(-20.5899961792857,38.6489096146735,123.657445196275)) ;
#39111 = CARTESIAN_POINT('Ctrl Pts',(-20.8851806309727,38.4689205342637,123.718849938171)) ;
#39112 = CARTESIAN_POINT('Ctrl Pts',(-20.5288093864204,38.6589820647126,123.860120703039)) ;
#39113 = CARTESIAN_POINT('Ctrl Pts',(-20.808697747112,38.4789929843028,123.972194060063)) ;
#39114 = CARTESIAN_POINT('Ctrl Pts',(-20.4358076287803,38.6688110814861,124.044689523101)) ;
#39115 = CARTESIAN_POINT('Ctrl Pts',(-20.6924452330698,38.4888220010763,124.202906653786)) ;
#39116 = CARTESIAN_POINT('Ctrl Pts',(-20.3094581014981,38.6788779274009,124.214427563999)) ;
#39117 = CARTESIAN_POINT('Ctrl Pts',(-20.5345088117852,38.4988888469911,124.415079071693)) ;
#39118 = CARTESIAN_POINT('Ctrl Pts',(-20.1581204946843,38.6887680987027,124.357044093307)) ;
#39119 = CARTESIAN_POINT('Ctrl Pts',(-20.3453362910771,38.5087790182928,124.593350718239)) ;
#39120 = CARTESIAN_POINT('Ctrl Pts',(-19.9828118483022,38.6987602923265,124.472759650499)) ;
#39121 = CARTESIAN_POINT('Ctrl Pts',(-20.1262004053529,38.5187712119167,124.737995435584)) ;
#39122 = CARTESIAN_POINT('Ctrl Pts',(-19.7905552310231,38.7087231029499,124.555852659848)) ;
#39123 = CARTESIAN_POINT('Ctrl Pts',(-19.8858793197605,38.5287340225401,124.841862120284)) ;
#39124 = CARTESIAN_POINT('Ctrl Pts',(-19.5880898351678,38.7186273757934,124.604536143381)) ;
#39125 = CARTESIAN_POINT('Ctrl Pts',(-19.6327966736639,38.5386382953835,124.902716744678)) ;
#39126 = CARTESIAN_POINT('Ctrl Pts',(-19.3770005006573,38.728687867598,124.617340881454)) ;
#39127 = CARTESIAN_POINT('Ctrl Pts',(-19.3689353661854,38.5486987871882,124.918722771534)) ;
#39128 = CARTESIAN_POINT('Ctrl Pts',(-19.1714080286777,38.7385281992703,124.594087546926)) ;
#39129 = CARTESIAN_POINT('Ctrl Pts',(-19.111943312049,38.5585391188605,124.889655955277)) ;
#39130 = CARTESIAN_POINT('Ctrl Pts',(-18.9684668170041,38.7485912453621,124.53442387862)) ;
#39131 = CARTESIAN_POINT('Ctrl Pts',(-18.8582671795693,38.5686021649523,124.81507639537)) ;
#39132 = CARTESIAN_POINT('Ctrl Pts',(-18.7821841412429,38.7584853010572,124.441832669131)) ;
#39133 = CARTESIAN_POINT('Ctrl Pts',(-18.6254129262144,38.5784962206474,124.699336919399)) ;
#39134 = CARTESIAN_POINT('Ctrl Pts',(-18.613681541493,38.7684280013801,124.318182967995)) ;
#39135 = CARTESIAN_POINT('Ctrl Pts',(-18.4147842987737,38.5884389209703,124.544774213957)) ;
#39136 = CARTESIAN_POINT('Ctrl Pts',(-18.4682304496749,38.7784337423077,124.166191909922)) ;
#39137 = CARTESIAN_POINT('Ctrl Pts',(-18.2329705622682,38.5984446618979,124.354785151185)) ;
#39138 = CARTESIAN_POINT('Ctrl Pts',(-18.3514150571057,38.7884546528233,123.990879578772)) ;
#39139 = CARTESIAN_POINT('Ctrl Pts',(-18.086951476035,38.6084655724134,124.135644682237)) ;
#39140 = CARTESIAN_POINT('Ctrl Pts',(-18.2676887679517,38.7983453882732,123.800540045983)) ;
#39141 = CARTESIAN_POINT('Ctrl Pts',(-17.9822934308171,38.6183563078634,123.89771920694)) ;
#39142 = CARTESIAN_POINT('Ctrl Pts',(-18.2174815072807,38.8083369290021,123.596583556656)) ;
#39143 = CARTESIAN_POINT('Ctrl Pts',(-17.919534669745,38.6283478485923,123.642773296605)) ;
#39144 = CARTESIAN_POINT('Ctrl Pts',(-18.2035708832846,38.8182847894237,123.387913191954)) ;
#39145 = CARTESIAN_POINT('Ctrl Pts',(-17.9021467019561,38.6382957090139,123.381934725882)) ;
#39146 = CARTESIAN_POINT('Ctrl Pts',(-18.2256918881132,38.8282314586101,123.17996466364)) ;
#39147 = CARTESIAN_POINT('Ctrl Pts',(-17.9297985345698,38.6482423782002,123.121998548206)) ;
#39148 = CARTESIAN_POINT('Ctrl Pts',(-18.2843906460259,38.8382795347457,122.977049468211)) ;
#39149 = CARTESIAN_POINT('Ctrl Pts',(-18.0031723205418,38.6582904543359,122.868354913006)) ;
#39150 = CARTESIAN_POINT('Ctrl Pts',(-18.3754224094433,38.8481271327513,122.79110855479)) ;
#39151 = CARTESIAN_POINT('Ctrl Pts',(-18.1169630845175,38.6681380523415,122.635927730697)) ;
#39152 = CARTESIAN_POINT('Ctrl Pts',(-18.4982316363328,38.8580888558358,122.621481919964)) ;
#39153 = CARTESIAN_POINT('Ctrl Pts',(-18.2704754939208,38.6780997754259,122.423894509183)) ;
#39154 = CARTESIAN_POINT('Ctrl Pts',(-18.6498412742199,38.8681174909188,122.474952850286)) ;
#39155 = CARTESIAN_POINT('Ctrl Pts',(-18.4599879202385,38.6881284105089,122.240733703657)) ;
#39156 = CARTESIAN_POINT('Ctrl Pts',(-18.822471332867,38.8780277992368,122.358322296909)) ;
#39157 = CARTESIAN_POINT('Ctrl Pts',(-18.6757765964576,38.698038718827,122.094945578036)) ;
#39158 = CARTESIAN_POINT('Ctrl Pts',(-19.0129931752722,38.8879626963727,122.272721130062)) ;
#39159 = CARTESIAN_POINT('Ctrl Pts',(-18.9139298646376,38.7079736159628,121.987944654612)) ;
#39160 = CARTESIAN_POINT('Ctrl Pts',(-19.2176845439249,38.8980037793153,122.221146163374)) ;
#39161 = CARTESIAN_POINT('Ctrl Pts',(-19.1697940908781,38.7180146989054,121.923476774972)) ;
#39162 = CARTESIAN_POINT('Ctrl Pts',(-19.4250041735291,38.9078911221435,122.205985759555)) ;
#39163 = CARTESIAN_POINT('Ctrl Pts',(-19.4289447281895,38.7279020417337,121.904527054384)) ;
#39164 = CARTESIAN_POINT('Ctrl Pts',(-19.6340005528841,38.9178826370828,122.22691350164)) ;
#39165 = CARTESIAN_POINT('Ctrl Pts',(-19.6901903067316,38.737893556673,121.930687744882)) ;
#39166 = CARTESIAN_POINT('Ctrl Pts',(-19.8353682152375,38.9278340282793,122.283672510292)) ;
#39167 = CARTESIAN_POINT('Ctrl Pts',(-19.9419001392647,38.7478449478695,122.001637581094)) ;
#39168 = CARTESIAN_POINT('Ctrl Pts',(-20.0236163341247,38.9377665616119,122.374032890848)) ;
#39169 = CARTESIAN_POINT('Ctrl Pts',(-20.1772104092454,38.7577774812021,122.114589337073)) ;
#39170 = CARTESIAN_POINT('Ctrl Pts',(-20.1944626039504,38.9477637195114,122.496427038679)) ;
#39171 = CARTESIAN_POINT('Ctrl Pts',(-20.3907677133097,38.7677746391016,122.267583026832)) ;
#39172 = CARTESIAN_POINT('Ctrl Pts',(-20.3413685794426,38.9577487296749,122.646417878081)) ;
#39173 = CARTESIAN_POINT('Ctrl Pts',(-20.5743995161531,38.7777596492651,122.455072551168)) ;
#39174 = CARTESIAN_POINT('Ctrl Pts',(-20.46039600103,38.9677915562447,122.820765432393)) ;
#39175 = CARTESIAN_POINT('Ctrl Pts',(-20.723182830776,38.7878024758349,122.673007430782)) ;
#39176 = CARTESIAN_POINT('Ctrl Pts',(-20.5459597437265,38.9776217905496,123.00891851305)) ;
#39177 = CARTESIAN_POINT('Ctrl Pts',(-20.830136998743,38.7976327101398,122.908200598541)) ;
#39178 = CARTESIAN_POINT('Ctrl Pts',(-20.5989170245634,38.9876978157843,123.213977187539)) ;
#39179 = CARTESIAN_POINT('Ctrl Pts',(-20.8963322765034,38.8077087353745,123.164523836738)) ;
#39180 = CARTESIAN_POINT('Ctrl Pts',(-20.6152120888322,38.9975500522752,123.42050479598)) ;
#39181 = CARTESIAN_POINT('Ctrl Pts',(-20.9166999185625,38.8175609718654,123.422684680524)) ;
#39182 = CARTESIAN_POINT('Ctrl Pts',(-20.5951407332866,39.0076232587093,123.631287792169)) ;
#39183 = CARTESIAN_POINT('Ctrl Pts',(-20.8916094133679,38.8276341782995,123.686162896896)) ;
#39184 = CARTESIAN_POINT('Ctrl Pts',(-20.5400039210857,39.0174647682165,123.830719200316)) ;
#39185 = CARTESIAN_POINT('Ctrl Pts',(-20.8226867660567,38.8374756878066,123.935453060499)) ;
#39186 = CARTESIAN_POINT('Ctrl Pts',(-20.4507189099979,39.0274257149963,124.020134101284)) ;
#39187 = CARTESIAN_POINT('Ctrl Pts',(-20.711078874203,38.8474366345865,124.172221368171)) ;
#39188 = CARTESIAN_POINT('Ctrl Pts',(-20.3286238637453,39.0374635437963,124.192245807622)) ;
#39189 = CARTESIAN_POINT('Ctrl Pts',(-20.558458951946,38.8574744633865,124.387360046593)) ;
#39190 = CARTESIAN_POINT('Ctrl Pts',(-20.1811938017144,39.0473378535508,124.338423480837)) ;
#39191 = CARTESIAN_POINT('Ctrl Pts',(-20.3741695323941,38.867348773141,124.570081721037)) ;
#39192 = CARTESIAN_POINT('Ctrl Pts',(-20.0072836350948,39.0574075512239,124.45908427213)) ;
#39193 = CARTESIAN_POINT('Ctrl Pts',(-20.1567812055982,38.8774184708141,124.720906204258)) ;
#39194 = CARTESIAN_POINT('Ctrl Pts',(-19.8195805182457,39.0672410225113,124.545752922959)) ;
#39195 = CARTESIAN_POINT('Ctrl Pts',(-19.9221504639086,38.8872519421015,124.829241080154)) ;
#39196 = CARTESIAN_POINT('Ctrl Pts',(-19.6158666766055,39.0772706690413,124.600148476529)) ;
#39197 = CARTESIAN_POINT('Ctrl Pts',(-19.6675077755465,38.8972815886314,124.897233739446)) ;
#39198 = CARTESIAN_POINT('Ctrl Pts',(-19.4056375158977,39.0873051833686,124.617714671404)) ;
#39199 = CARTESIAN_POINT('Ctrl Pts',(-19.4047212779263,38.9073161029588,124.919189866016)) ;
#39200 = CARTESIAN_POINT('Ctrl Pts',(-19.1998910206002,39.0971304688395,124.599407552797)) ;
#39201 = CARTESIAN_POINT('Ctrl Pts',(-19.1475370274875,38.9171413884297,124.896304082201)) ;
#39202 = CARTESIAN_POINT('Ctrl Pts',(-18.9967244321837,39.1071347103881,124.545112550832)) ;
#39203 = CARTESIAN_POINT('Ctrl Pts',(-18.8935792031273,38.9271456299783,124.828433457383)) ;
#39204 = CARTESIAN_POINT('Ctrl Pts',(-18.8064617759764,39.1171173554672,124.456450033526)) ;
#39205 = CARTESIAN_POINT('Ctrl Pts',(-18.6557514840538,38.9371282750574,124.717603510454)) ;
#39206 = CARTESIAN_POINT('Ctrl Pts',(-18.6335954547731,39.1271625525587,124.335184104469)) ;
#39207 = CARTESIAN_POINT('Ctrl Pts',(-18.4396697499404,38.9471734721488,124.566019705059)) ;
#39208 = CARTESIAN_POINT('Ctrl Pts',(-18.4874417294713,39.1369856683188,124.189274410091)) ;
#39209 = CARTESIAN_POINT('Ctrl Pts',(-18.2569780632048,38.956996587909,124.383630345481)) ;
#39210 = CARTESIAN_POINT('Ctrl Pts',(-18.3658597551784,39.1470202801191,124.016878296206)) ;
#39211 = CARTESIAN_POINT('Ctrl Pts',(-18.105002354756,38.9670311997093,124.16813409238)) ;
#39212 = CARTESIAN_POINT('Ctrl Pts',(-18.2766733676231,39.1570452888922,123.825914539901)) ;
#39213 = CARTESIAN_POINT('Ctrl Pts',(-17.9935211047734,38.9770562084824,123.929428614869)) ;
#39214 = CARTESIAN_POINT('Ctrl Pts',(-18.2225068331294,39.1668972137338,123.626000802301)) ;
#39215 = CARTESIAN_POINT('Ctrl Pts',(-17.9258146374258,38.986908133324,123.679534933415)) ;
#39216 = CARTESIAN_POINT('Ctrl Pts',(-18.2032934378515,39.1768881520565,123.416865948046)) ;
#39217 = CARTESIAN_POINT('Ctrl Pts',(-17.9017999975466,38.9968990716467,123.418116000194)) ;
#39218 = CARTESIAN_POINT('Ctrl Pts',(-18.2204270850265,39.186806137203,123.209038883101)) ;
#39219 = CARTESIAN_POINT('Ctrl Pts',(-17.9232192571751,39.0068170567931,123.158331775169)) ;
#39220 = CARTESIAN_POINT('Ctrl Pts',(-18.2739141189626,39.1968342380985,123.005131243804)) ;
#39221 = CARTESIAN_POINT('Ctrl Pts',(-17.9900801458931,39.0168451576887,122.903447812463)) ;
#39222 = CARTESIAN_POINT('Ctrl Pts',(-18.3606686893931,39.2067194790411,122.816282003128)) ;
#39223 = CARTESIAN_POINT('Ctrl Pts',(-18.0985256645182,39.0267303986312,122.667386508151)) ;
#39224 = CARTESIAN_POINT('Ctrl Pts',(-18.4797149154803,39.2167085920077,122.643274137874)) ;
#39225 = CARTESIAN_POINT('Ctrl Pts',(-18.2473354546327,39.0367195115979,122.451127866557)) ;
#39226 = CARTESIAN_POINT('Ctrl Pts',(-18.6280950699641,39.2267506563485,122.493104045599)) ;
#39227 = CARTESIAN_POINT('Ctrl Pts',(-18.4328121554454,39.0467615759387,122.263416874348)) ;
#39228 = CARTESIAN_POINT('Ctrl Pts',(-18.7964289728388,39.236579857753,122.37324034441)) ;
#39229 = CARTESIAN_POINT('Ctrl Pts',(-18.6432316642318,39.0565907773432,122.1135885661)) ;
#39230 = CARTESIAN_POINT('Ctrl Pts',(-18.9861633069281,39.2465866985112,122.282419196658)) ;
#39231 = CARTESIAN_POINT('Ctrl Pts',(-18.8804006959782,39.0665976181013,122.000064282173)) ;
#39232 = CARTESIAN_POINT('Ctrl Pts',(-19.1884846108807,39.2565742227031,122.226135721448)) ;
#39233 = CARTESIAN_POINT('Ctrl Pts',(-19.1333031196134,39.0765851422933,121.929712194774)) ;
#39234 = CARTESIAN_POINT('Ctrl Pts',(-19.3983474426324,39.2666038685117,122.205902107928)) ;
#39235 = CARTESIAN_POINT('Ctrl Pts',(-19.3956318554849,39.0866147881019,121.904422523762)) ;
#39236 = CARTESIAN_POINT('Ctrl Pts',(-19.6053336272935,39.2764778992504,122.221912828081)) ;
#39237 = CARTESIAN_POINT('Ctrl Pts',(-19.6543650766662,39.0964888188406,121.924438378647)) ;
#39238 = CARTESIAN_POINT('Ctrl Pts',(-19.8089581741731,39.2864772221145,122.274010548513)) ;
#39239 = CARTESIAN_POINT('Ctrl Pts',(-19.908895255935,39.1064881417047,121.989562946807)) ;
#39240 = CARTESIAN_POINT('Ctrl Pts',(-19.9988971817539,39.2963880576901,122.359747483072)) ;
#39241 = CARTESIAN_POINT('Ctrl Pts',(-20.1463184204501,39.1163989772803,122.096736593736)) ;
#39242 = CARTESIAN_POINT('Ctrl Pts',(-20.173454632489,39.3064423056642,122.478884560245)) ;
#39243 = CARTESIAN_POINT('Ctrl Pts',(-20.3645137351281,39.1264532252543,122.245659936817)) ;
#39244 = CARTESIAN_POINT('Ctrl Pts',(-20.321953767156,39.3163010499269,122.623523272663)) ;
#39245 = CARTESIAN_POINT('Ctrl Pts',(-20.5501363523846,39.136311969517,122.426460600521)) ;
#39246 = CARTESIAN_POINT('Ctrl Pts',(-20.4457184725392,39.3263691359999,122.79519306141)) ;
#39247 = CARTESIAN_POINT('Ctrl Pts',(-20.7048400637397,39.1463800555901,122.641049209718)) ;
#39248 = CARTESIAN_POINT('Ctrl Pts',(-20.5358574260446,39.3362246191794,122.981770543194)) ;
#39249 = CARTESIAN_POINT('Ctrl Pts',(-20.8175117264018,39.1562355387696,122.874272740712)) ;
#39250 = CARTESIAN_POINT('Ctrl Pts',(-20.593627567202,39.3462194649736,123.183789054105)) ;
#39251 = CARTESIAN_POINT('Ctrl Pts',(-20.8897218677833,39.1662303845638,123.126796707749)) ;
#39252 = CARTESIAN_POINT('Ctrl Pts',(-20.6150717947813,39.3562507606361,123.393589597854)) ;
#39253 = CARTESIAN_POINT('Ctrl Pts',(-20.9165245763785,39.1762616802263,123.38904765132)) ;
#39254 = CARTESIAN_POINT('Ctrl Pts',(-20.6003432400617,39.366117303926,123.600498782211)) ;
#39255 = CARTESIAN_POINT('Ctrl Pts',(-20.8981112103202,39.1861282235162,123.647684462336)) ;
#39256 = CARTESIAN_POINT('Ctrl Pts',(-20.5496307755805,39.3761046996894,123.804223422372)) ;
#39257 = CARTESIAN_POINT('Ctrl Pts',(-20.8347179860478,39.1961156192796,123.902339731303)) ;
#39258 = CARTESIAN_POINT('Ctrl Pts',(-20.4647567854182,39.3860497404194,123.995331104397)) ;
#39259 = CARTESIAN_POINT('Ctrl Pts',(-20.7286229324539,39.2060606600095,124.141223452018)) ;
#39260 = CARTESIAN_POINT('Ctrl Pts',(-20.3467526330684,39.3960942466361,124.170424565575)) ;
#39261 = CARTESIAN_POINT('Ctrl Pts',(-20.5811155220778,39.2161051662263,124.360088757651)) ;
#39262 = CARTESIAN_POINT('Ctrl Pts',(-20.2028876578197,39.4059577527734,124.31979097255)) ;
#39263 = CARTESIAN_POINT('Ctrl Pts',(-20.4012820502174,39.2259686723636,124.546795194505)) ;
#39264 = CARTESIAN_POINT('Ctrl Pts',(-20.0333359133557,39.4159506136095,124.443780975724)) ;
#39265 = CARTESIAN_POINT('Ctrl Pts',(-20.1893406640015,39.2359615331996,124.701780528512)) ;
#39266 = CARTESIAN_POINT('Ctrl Pts',(-19.8460776642137,39.4258768073284,124.535944097192)) ;
#39267 = CARTESIAN_POINT('Ctrl Pts',(-19.9552664329301,39.2458877269186,124.81698205313)) ;
#39268 = CARTESIAN_POINT('Ctrl Pts',(-19.6438526109254,39.435895733361,124.594760442334)) ;
#39269 = CARTESIAN_POINT('Ctrl Pts',(-19.7024842949492,39.2559066529511,124.890499840272)) ;
#39270 = CARTESIAN_POINT('Ctrl Pts',(-19.4366243471817,39.4458107327286,124.617535468965)) ;
#39271 = CARTESIAN_POINT('Ctrl Pts',(-19.4434484431306,39.2658216523187,124.918965884145)) ;
#39272 = CARTESIAN_POINT('Ctrl Pts',(-19.2257177733582,39.4558655042859,124.603751642872)) ;
#39273 = CARTESIAN_POINT('Ctrl Pts',(-19.1798154010416,39.275876423876,124.901733325826)) ;
#39274 = CARTESIAN_POINT('Ctrl Pts',(-19.024324659477,39.4657244665834,124.554651862093)) ;
#39275 = CARTESIAN_POINT('Ctrl Pts',(-18.9280744033363,39.2857353861736,124.840355827258)) ;
#39276 = CARTESIAN_POINT('Ctrl Pts',(-18.8318078658274,39.4757187104213,124.47057126686)) ;
#39277 = CARTESIAN_POINT('Ctrl Pts',(-18.6874294683432,39.2957296300115,124.73525247238)) ;
#39278 = CARTESIAN_POINT('Ctrl Pts',(-18.6579134178425,39.4856439398455,124.355188357993)) ;
#39279 = CARTESIAN_POINT('Ctrl Pts',(-18.4700628512776,39.3056548594357,124.591021419494)) ;
#39280 = CARTESIAN_POINT('Ctrl Pts',(-18.505167355136,39.495671903737,124.209924117878)) ;
#39281 = CARTESIAN_POINT('Ctrl Pts',(-18.2791321697384,39.3156828233272,124.409439034556)) ;
#39282 = CARTESIAN_POINT('Ctrl Pts',(-18.3815260589152,39.5055581633674,124.042821017598)) ;
#39283 = CARTESIAN_POINT('Ctrl Pts',(-18.1245827426847,39.3255690829575,124.200558385434)) ;
#39284 = CARTESIAN_POINT('Ctrl Pts',(-18.2873441788241,39.5155899264452,123.854158630485)) ;
#39285 = CARTESIAN_POINT('Ctrl Pts',(-18.0068578912932,39.3356008460354,123.96472907927)) ;
#39286 = CARTESIAN_POINT('Ctrl Pts',(-18.2280346546859,39.5254715527393,123.655023225739)) ;
#39287 = CARTESIAN_POINT('Ctrl Pts',(-17.9327236697007,39.3454824723295,123.715808953647)) ;
#39288 = CARTESIAN_POINT('Ctrl Pts',(-18.2037205041182,39.5355333222255,123.444926394971)) ;
#39289 = CARTESIAN_POINT('Ctrl Pts',(-17.9023337792081,39.3555442418157,123.453187507277)) ;
#39290 = CARTESIAN_POINT('Ctrl Pts',(-18.2159436021786,39.545391189721,123.238018443075)) ;
#39291 = CARTESIAN_POINT('Ctrl Pts',(-17.9176154684793,39.3654021093111,123.194552719104)) ;
#39292 = CARTESIAN_POINT('Ctrl Pts',(-18.2640935145991,39.5553828148383,123.033581530344)) ;
#39293 = CARTESIAN_POINT('Ctrl Pts',(-17.977805608363,39.3753937344285,122.939007178542)) ;
#39294 = CARTESIAN_POINT('Ctrl Pts',(-18.346604236998,39.5653196139466,122.841649932194)) ;
#39295 = CARTESIAN_POINT('Ctrl Pts',(-18.080946592247,39.3853305335367,122.699093789384)) ;
#39296 = CARTESIAN_POINT('Ctrl Pts',(-18.4615503978526,39.5753104435039,122.665852839243)) ;
#39297 = CARTESIAN_POINT('Ctrl Pts',(-18.2246316582035,39.3953213630941,122.479348914354)) ;
#39298 = CARTESIAN_POINT('Ctrl Pts',(-18.6059214023956,39.5853336792171,122.512353088395)) ;
#39299 = CARTESIAN_POINT('Ctrl Pts',(-18.4050975253552,39.4053445988073,122.287476075937)) ;
#39300 = CARTESIAN_POINT('Ctrl Pts',(-18.7725024087154,39.5952300272463,122.38771377753)) ;
#39301 = CARTESIAN_POINT('Ctrl Pts',(-18.6133254066548,39.4152409468365,122.131679228694)) ;
#39302 = CARTESIAN_POINT('Ctrl Pts',(-18.9597546314449,39.6052195897488,122.292601295741)) ;
#39303 = CARTESIAN_POINT('Ctrl Pts',(-18.847391914281,39.4252305093389,122.012791074243)) ;
#39304 = CARTESIAN_POINT('Ctrl Pts',(-19.1618012116734,39.6152598974333,122.231549580434)) ;
#39305 = CARTESIAN_POINT('Ctrl Pts',(-19.0999512728401,39.4352708170235,121.936479082137)) ;
#39306 = CARTESIAN_POINT('Ctrl Pts',(-19.367227076232,39.6251022007805,122.206604242828)) ;
#39307 = CARTESIAN_POINT('Ctrl Pts',(-19.3567329848068,39.4451131203707,121.905300141078)) ;
#39308 = CARTESIAN_POINT('Ctrl Pts',(-19.5776342598679,39.6351259090596,122.217627035733)) ;
#39309 = CARTESIAN_POINT('Ctrl Pts',(-19.6197445019945,39.4551368286498,121.919081532406)) ;
#39310 = CARTESIAN_POINT('Ctrl Pts',(-19.8485635991152,39.6483480865273,122.280050363964)) ;
#39311 = CARTESIAN_POINT('Ctrl Pts',(-19.9583923044569,39.4683590061174,121.997113385138)) ;
#39312 = CARTESIAN_POINT('Ctrl Pts',(-20.0983757230061,39.6616406715866,122.4121455033)) ;
#39313 = CARTESIAN_POINT('Ctrl Pts',(-20.2706261181755,39.4816515911767,122.162206025438)) ;
#39314 = CARTESIAN_POINT('Ctrl Pts',(-20.3030677190675,39.6749255275082,122.602175666116)) ;
#39315 = CARTESIAN_POINT('Ctrl Pts',(-20.5265366200898,39.4949364470983,122.399782063026)) ;
#39316 = CARTESIAN_POINT('Ctrl Pts',(-20.4297258307919,39.684897754681,122.76921101663)) ;
#39317 = CARTESIAN_POINT('Ctrl Pts',(-20.6848475062814,39.5049086742711,122.608570519068)) ;
#39318 = CARTESIAN_POINT('Ctrl Pts',(-20.5251856164806,39.69480637112,122.95438797765)) ;
#39319 = CARTESIAN_POINT('Ctrl Pts',(-20.8041722375958,39.5148172907101,122.8400449268)) ;
#39320 = CARTESIAN_POINT('Ctrl Pts',(-20.587851626912,39.7048595765037,123.156213626947)) ;
#39321 = CARTESIAN_POINT('Ctrl Pts',(-20.8825021975675,39.5248704960938,123.092326029343)) ;
#39322 = CARTESIAN_POINT('Ctrl Pts',(-20.6141617899061,39.714724710264,123.361949025928)) ;
#39323 = CARTESIAN_POINT('Ctrl Pts',(-20.9153854641388,39.5347356298541,123.349500706132)) ;
#39324 = CARTESIAN_POINT('Ctrl Pts',(-20.6014061829563,39.7280637678903,123.642094545317)) ;
#39325 = CARTESIAN_POINT('Ctrl Pts',(-20.8994475639115,39.5480746874805,123.699654940687)) ;
#39326 = CARTESIAN_POINT('Ctrl Pts',(-20.4948803150655,39.7446329552234,123.977922234663)) ;
#39327 = CARTESIAN_POINT('Ctrl Pts',(-20.766262621046,39.5646438748136,124.119481950591)) ;
#39328 = CARTESIAN_POINT('Ctrl Pts',(-20.279368944222,39.7612780950745,124.258669320355)) ;
#39329 = CARTESIAN_POINT('Ctrl Pts',(-20.4969232973437,39.5812890146646,124.4703529915)) ;
#39330 = CARTESIAN_POINT('Ctrl Pts',(-20.057952056873,39.7745503975479,124.428460036515)) ;
#39331 = CARTESIAN_POINT('Ctrl Pts',(-20.220105563722,39.5945613171381,124.682635504539)) ;
#39332 = CARTESIAN_POINT('Ctrl Pts',(-19.8719346516173,39.7845313609955,124.525525802343)) ;
#39333 = CARTESIAN_POINT('Ctrl Pts',(-19.987592650646,39.6045422805857,124.803956293418)) ;
#39334 = CARTESIAN_POINT('Ctrl Pts',(-19.6726840160093,39.7944731930648,124.588696431075)) ;
#39335 = CARTESIAN_POINT('Ctrl Pts',(-19.7385233068457,39.614484112655,124.882919421842)) ;
#39336 = CARTESIAN_POINT('Ctrl Pts',(-19.3951538397195,39.8077927622802,124.625793701431)) ;
#39337 = CARTESIAN_POINT('Ctrl Pts',(-19.3916274184832,39.6278036818704,124.929289096375)) ;
#39338 = CARTESIAN_POINT('Ctrl Pts',(-19.0464383279096,39.824322917213,124.581253491284)) ;
#39339 = CARTESIAN_POINT('Ctrl Pts',(-18.9557155359745,39.6443338368031,124.87360860491)) ;
#39340 = CARTESIAN_POINT('Ctrl Pts',(-18.668086969949,39.8443446427051,124.386327800272)) ;
#39341 = CARTESIAN_POINT('Ctrl Pts',(-18.4827841914454,39.6643555622952,124.629948165765)) ;
#39342 = CARTESIAN_POINT('Ctrl Pts',(-18.3816863058028,39.8641560393119,124.077284990008)) ;
#39343 = CARTESIAN_POINT('Ctrl Pts',(-18.1247857375312,39.6841669589021,124.243642886359)) ;
#39344 = CARTESIAN_POINT('Ctrl Pts',(-18.2159257669221,39.8841412880207,123.686114821925)) ;
#39345 = CARTESIAN_POINT('Ctrl Pts',(-17.9175888920775,39.7041522076109,123.754678947972)) ;
#39346 = CARTESIAN_POINT('Ctrl Pts',(-18.1939835367103,39.9040353506567,123.263614550275)) ;
#39347 = CARTESIAN_POINT('Ctrl Pts',(-17.8901646193541,39.7240462702468,123.226554358743)) ;
#39348 = CARTESIAN_POINT('Ctrl Pts',(-18.317143757237,39.9239670298303,122.858111488064)) ;
#39349 = CARTESIAN_POINT('Ctrl Pts',(-18.04411771938,39.7439779494204,122.719677099865)) ;
#39350 = CARTESIAN_POINT('Ctrl Pts',(-18.5719284249735,39.9439310843023,122.518586193573)) ;
#39351 = CARTESIAN_POINT('Ctrl Pts',(-18.3626008286058,39.7639420038924,122.295272619699)) ;
#39352 = CARTESIAN_POINT('Ctrl Pts',(-18.9256419898356,39.9638119860652,122.287076377155)) ;
#39353 = CARTESIAN_POINT('Ctrl Pts',(-18.8047431637994,39.7838229056553,122.005888410371)) ;
#39354 = CARTESIAN_POINT('Ctrl Pts',(-19.3381892305123,39.9837506476736,122.189510079094)) ;
#39355 = CARTESIAN_POINT('Ctrl Pts',(-19.3204270314269,39.8037615672637,121.883932996497)) ;
#39356 = CARTESIAN_POINT('Ctrl Pts',(-19.7583997067115,40.0036471729289,122.23841409713)) ;
#39357 = CARTESIAN_POINT('Ctrl Pts',(-19.8456885699693,39.8236580925191,121.945064977798)) ;
#39358 = CARTESIAN_POINT('Ctrl Pts',(-20.1370001314726,40.0235422113832,122.427152769696)) ;
#39359 = CARTESIAN_POINT('Ctrl Pts',(-20.3189371294042,39.8435531309734,122.180988955617)) ;
#39360 = CARTESIAN_POINT('Ctrl Pts',(-20.4293996902846,40.0435060346893,122.734826780891)) ;
#39361 = CARTESIAN_POINT('Ctrl Pts',(-20.6844353023525,39.8635169542794,122.565581974884)) ;
#39362 = CARTESIAN_POINT('Ctrl Pts',(-20.598804014177,40.0633801588183,123.121996946429)) ;
#39363 = CARTESIAN_POINT('Ctrl Pts',(-20.896189201181,39.8833910784085,123.049543285413)) ;
#39364 = CARTESIAN_POINT('Ctrl Pts',(-20.6264486511241,40.0833552345456,123.545839265876)) ;
#39365 = CARTESIAN_POINT('Ctrl Pts',(-20.9307446999829,39.9033661541358,123.579345858912)) ;
#39366 = CARTESIAN_POINT('Ctrl Pts',(-20.5073509704462,40.1033088039022,123.953040176851)) ;
#39367 = CARTESIAN_POINT('Ctrl Pts',(-20.7818723369442,39.9233197234924,124.088346140081)) ;
#39368 = CARTESIAN_POINT('Ctrl Pts',(-20.2585393963816,40.12314671409,124.293652583633)) ;
#39369 = CARTESIAN_POINT('Ctrl Pts',(-20.4708597449385,39.9431576336802,124.514109737986)) ;
#39370 = CARTESIAN_POINT('Ctrl Pts',(-19.9062499760645,40.143122542661,124.530920991778)) ;
#39371 = CARTESIAN_POINT('Ctrl Pts',(-20.0304987771177,39.9631334622511,124.810695893645)) ;
#39372 = CARTESIAN_POINT('Ctrl Pts',(-19.4952472081866,40.1630405873712,124.63297354376)) ;
#39373 = CARTESIAN_POINT('Ctrl Pts',(-19.5167467255033,39.9830515069614,124.938262136375)) ;
#39374 = CARTESIAN_POINT('Ctrl Pts',(-19.0748749833404,40.1829108331589,124.58981024594)) ;
#39375 = CARTESIAN_POINT('Ctrl Pts',(-18.9912829799655,40.0029217527491,124.884310017426)) ;
#39376 = CARTESIAN_POINT('Ctrl Pts',(-18.6914968706604,40.2029598362585,124.403647517381)) ;
#39377 = CARTESIAN_POINT('Ctrl Pts',(-18.5120590676542,40.0229707558487,124.651607827886)) ;
#39378 = CARTESIAN_POINT('Ctrl Pts',(-18.3981552231749,40.2227390774993,124.10210693945)) ;
#39379 = CARTESIAN_POINT('Ctrl Pts',(-18.1453823899239,40.0427499970895,124.274685535376)) ;
#39380 = CARTESIAN_POINT('Ctrl Pts',(-18.2226350296879,40.2427691412082,123.714169214818)) ;
#39381 = CARTESIAN_POINT('Ctrl Pts',(-17.9259795061212,40.0627800607984,123.789764142182)) ;
#39382 = CARTESIAN_POINT('Ctrl Pts',(-18.1909445920671,40.2626514261102,123.292541082987)) ;
#39383 = CARTESIAN_POINT('Ctrl Pts',(-17.8863640755037,40.0826623457003,123.262730489932)) ;
#39384 = CARTESIAN_POINT('Ctrl Pts',(-18.3038777435817,40.2825337270031,122.885191709277)) ;
#39385 = CARTESIAN_POINT('Ctrl Pts',(-18.0275270007158,40.1025446465933,122.753544083074)) ;
#39386 = CARTESIAN_POINT('Ctrl Pts',(-18.5504210038991,40.3025168366215,122.539129314307)) ;
#39387 = CARTESIAN_POINT('Ctrl Pts',(-18.3357032517793,40.1225277562117,122.320964219428)) ;
#39388 = CARTESIAN_POINT('Ctrl Pts',(-18.8986806428871,40.3224072319994,122.29912255241)) ;
#39389 = CARTESIAN_POINT('Ctrl Pts',(-18.7710249751716,40.1424181515896,122.02095345069)) ;
#39390 = CARTESIAN_POINT('Ctrl Pts',(-19.3078266805979,40.3423040220336,122.191737778741)) ;
#39391 = CARTESIAN_POINT('Ctrl Pts',(-19.2824556627303,40.1623149416238,121.886718883262)) ;
#39392 = CARTESIAN_POINT('Ctrl Pts',(-19.7296085524883,40.3622210759752,122.230003374302)) ;
#39393 = CARTESIAN_POINT('Ctrl Pts',(-19.8096827929728,40.1822319955654,121.934546603933)) ;
#39394 = CARTESIAN_POINT('Ctrl Pts',(-20.1146489811739,40.3822246241788,122.410827144587)) ;
#39395 = CARTESIAN_POINT('Ctrl Pts',(-20.290985297795,40.2022355437689,122.160572440188)) ;
#39396 = CARTESIAN_POINT('Ctrl Pts',(-20.4133927271247,40.4021629178314,122.711596083807)) ;
#39397 = CARTESIAN_POINT('Ctrl Pts',(-20.6644175476842,40.2221738374216,122.536530476468)) ;
#39398 = CARTESIAN_POINT('Ctrl Pts',(-20.5914685302538,40.4219844052643,123.093592798811)) ;
#39399 = CARTESIAN_POINT('Ctrl Pts',(-20.887016493454,40.2419953248545,123.014022848791)) ;
#39400 = CARTESIAN_POINT('Ctrl Pts',(-20.6292190379642,40.4419627982552,123.516656820411)) ;
#39401 = CARTESIAN_POINT('Ctrl Pts',(-20.9342078754109,40.2619737178453,123.542854403197)) ;
#39402 = CARTESIAN_POINT('Ctrl Pts',(-20.5204888317716,40.4618611798689,123.925614309865)) ;
#39403 = CARTESIAN_POINT('Ctrl Pts',(-20.7983060144044,40.2818720994591,124.054044528047)) ;
#39404 = CARTESIAN_POINT('Ctrl Pts',(-20.3195216622248,40.4784441105988,124.215207938259)) ;
#39405 = CARTESIAN_POINT('Ctrl Pts',(-20.5470819881122,40.2984550301889,124.4160621592)) ;
#39406 = CARTESIAN_POINT('Ctrl Pts',(-20.1066630617855,40.4917183461876,124.395787910796)) ;
#39407 = CARTESIAN_POINT('Ctrl Pts',(-20.2810284413274,40.3117292657778,124.641768863656)) ;
#39408 = CARTESIAN_POINT('Ctrl Pts',(-19.9242973164539,40.5017647636438,124.502269830301)) ;
#39409 = CARTESIAN_POINT('Ctrl Pts',(-20.0530654837858,40.321775683234,124.774877815185)) ;
#39410 = CARTESIAN_POINT('Ctrl Pts',(-19.7302037187856,40.5116099888631,124.57423387795)) ;
#39411 = CARTESIAN_POINT('Ctrl Pts',(-19.8104644040159,40.3316209084532,124.864833820597)) ;
#39412 = CARTESIAN_POINT('Ctrl Pts',(-19.4546005991835,40.5249449599025,124.625166757655)) ;
#39413 = CARTESIAN_POINT('Ctrl Pts',(-19.4658929191253,40.3449558794926,124.928504806304)) ;
#39414 = CARTESIAN_POINT('Ctrl Pts',(-19.102968767351,40.5415278166951,124.597279021719)) ;
#39415 = CARTESIAN_POINT('Ctrl Pts',(-19.0264390688112,40.3615387362853,124.893652813631)) ;
#39416 = CARTESIAN_POINT('Ctrl Pts',(-18.7810021390429,40.5581708190445,124.450732297002)) ;
#39417 = CARTESIAN_POINT('Ctrl Pts',(-18.6239205040099,40.3781817386347,124.710456066607)) ;
#39418 = CARTESIAN_POINT('Ctrl Pts',(-18.5658420171576,40.5714145500762,124.273876479058)) ;
#39419 = CARTESIAN_POINT('Ctrl Pts',(-18.3550031410249,40.3914254696664,124.489405088458)) ;
#39420 = CARTESIAN_POINT('Ctrl Pts',(-18.428371398618,40.5814689447508,124.113372164029)) ;
#39421 = CARTESIAN_POINT('Ctrl Pts',(-18.1831556506219,40.401479864341,124.288773158627)) ;
#39422 = CARTESIAN_POINT('Ctrl Pts',(-18.322862621758,40.5913100061393,123.935361777761)) ;
#39423 = CARTESIAN_POINT('Ctrl Pts',(-18.051269318921,40.4113209257295,124.066262657629)) ;
#39424 = CARTESIAN_POINT('Ctrl Pts',(-18.2480294467794,40.6013762304958,123.737449279801)) ;
#39425 = CARTESIAN_POINT('Ctrl Pts',(-17.9577246776694,40.421387150086,123.81887262292)) ;
#39426 = CARTESIAN_POINT('Ctrl Pts',(-18.2094701938353,40.6112568434155,123.533303511753)) ;
#39427 = CARTESIAN_POINT('Ctrl Pts',(-17.9095230456685,40.4312677630057,123.563691114029)) ;
#39428 = CARTESIAN_POINT('Ctrl Pts',(-18.206516541867,40.6212501365751,123.323267667439)) ;
#39429 = CARTESIAN_POINT('Ctrl Pts',(-17.9058281377945,40.4412610561653,123.301146268744)) ;
#39430 = CARTESIAN_POINT('Ctrl Pts',(-18.2398673386455,40.6312011447987,123.11670429861)) ;
#39431 = CARTESIAN_POINT('Ctrl Pts',(-17.9475138798417,40.4512120643889,123.042941598597)) ;
#39432 = CARTESIAN_POINT('Ctrl Pts',(-18.3093839574438,40.6412496591607,122.917243416711)) ;
#39433 = CARTESIAN_POINT('Ctrl Pts',(-18.0344070396887,40.4612605787509,122.79361447851)) ;
#39434 = CARTESIAN_POINT('Ctrl Pts',(-18.4101694123091,40.6510911652234,122.736528533016)) ;
#39435 = CARTESIAN_POINT('Ctrl Pts',(-18.1603863835786,40.4711020848136,122.567719550019)) ;
#39436 = CARTESIAN_POINT('Ctrl Pts',(-18.542325109746,40.6610768178531,122.573458997662)) ;
#39437 = CARTESIAN_POINT('Ctrl Pts',(-18.3255788629678,40.4810877374433,122.363880789435)) ;
#39438 = CARTESIAN_POINT('Ctrl Pts',(-18.7000440263116,40.671015826698,122.436353330348)) ;
#39439 = CARTESIAN_POINT('Ctrl Pts',(-18.5227257140417,40.4910267462881,122.192496536493)) ;
#39440 = CARTESIAN_POINT('Ctrl Pts',(-18.8809941836839,40.681056751991,122.327685783444)) ;
#39441 = CARTESIAN_POINT('Ctrl Pts',(-18.7489120153054,40.5010676715811,122.056659651351)) ;
#39442 = CARTESIAN_POINT('Ctrl Pts',(-19.0750989997885,40.6909470737459,122.253093211541)) ;
#39443 = CARTESIAN_POINT('Ctrl Pts',(-18.9915421154264,40.510957993336,121.963416273377)) ;
#39444 = CARTESIAN_POINT('Ctrl Pts',(-19.2812929576741,40.7009430470793,122.212614380291)) ;
#39445 = CARTESIAN_POINT('Ctrl Pts',(-19.2492841014226,40.5209539666695,121.912814957427)) ;
#39446 = CARTESIAN_POINT('Ctrl Pts',(-19.4900519469436,40.7108744466613,122.208562124172)) ;
#39447 = CARTESIAN_POINT('Ctrl Pts',(-19.5102329048688,40.5308853662515,121.907746825815)) ;
#39448 = CARTESIAN_POINT('Ctrl Pts',(-19.6979309739298,40.7208799871384,122.240764687343)) ;
#39449 = CARTESIAN_POINT('Ctrl Pts',(-19.7700821946182,40.5408909067286,121.947997275282)) ;
#39450 = CARTESIAN_POINT('Ctrl Pts',(-19.8974653853249,40.7309129710697,122.30911862514)) ;
#39451 = CARTESIAN_POINT('Ctrl Pts',(-20.0195011591116,40.5509238906599,122.033437044864)) ;
#39452 = CARTESIAN_POINT('Ctrl Pts',(-20.0790342263548,40.7407686018965,122.40896792997)) ;
#39453 = CARTESIAN_POINT('Ctrl Pts',(-20.2464637604677,40.5607795214867,122.158246335516)) ;
#39454 = CARTESIAN_POINT('Ctrl Pts',(-20.2429931194927,40.7507680040897,122.540475873946)) ;
#39455 = CARTESIAN_POINT('Ctrl Pts',(-20.4514141920233,40.5707789236799,122.322629146691)) ;
#39456 = CARTESIAN_POINT('Ctrl Pts',(-20.3804016988981,40.7606624734508,122.696694794566)) ;
#39457 = CARTESIAN_POINT('Ctrl Pts',(-20.6231771610024,40.5806733930409,122.517901168741)) ;
#39458 = CARTESIAN_POINT('Ctrl Pts',(-20.4903492131892,40.770725587615,122.877396553859)) ;
#39459 = CARTESIAN_POINT('Ctrl Pts',(-20.7606139058303,40.5907365072052,122.74377689725)) ;
#39460 = CARTESIAN_POINT('Ctrl Pts',(-20.565781026169,40.7805652333314,123.070050005765)) ;
#39461 = CARTESIAN_POINT('Ctrl Pts',(-20.8549063787126,40.6005761529215,122.984593090439)) ;
#39462 = CARTESIAN_POINT('Ctrl Pts',(-20.6077950411033,40.7906284008871,123.277366104284)) ;
#39463 = CARTESIAN_POINT('Ctrl Pts',(-20.9074265588259,40.6106393204773,123.243737629729)) ;
#39464 = CARTESIAN_POINT('Ctrl Pts',(-20.6129087024178,40.800522656682,123.485334552873)) ;
#39465 = CARTESIAN_POINT('Ctrl Pts',(-20.9138213840981,40.6205335762722,123.503698450434)) ;
#39466 = CARTESIAN_POINT('Ctrl Pts',(-20.5822552704826,40.8104644351417,123.692055896881)) ;
#39467 = CARTESIAN_POINT('Ctrl Pts',(-20.8755072032349,40.6304753547318,123.762100783277)) ;
#39468 = CARTESIAN_POINT('Ctrl Pts',(-20.5158234904619,40.8204671279719,123.891604227127)) ;
#39469 = CARTESIAN_POINT('Ctrl Pts',(-20.7924699763018,40.640478047562,124.011537115985)) ;
#39470 = CARTESIAN_POINT('Ctrl Pts',(-20.4151748597048,40.8305011499257,124.076979654914)) ;
#39471 = CARTESIAN_POINT('Ctrl Pts',(-20.6666615752948,40.6505120695159,124.24325767995)) ;
#39472 = CARTESIAN_POINT('Ctrl Pts',(-20.2865434555371,40.8403489410147,124.239210149898)) ;
#39473 = CARTESIAN_POINT('Ctrl Pts',(-20.5058740591631,40.6603598606049,124.446047890663)) ;
#39474 = CARTESIAN_POINT('Ctrl Pts',(-20.1299205089068,40.8503304655638,124.378837643327)) ;
#39475 = CARTESIAN_POINT('Ctrl Pts',(-20.3100969714377,40.6703413851539,124.620584309746)) ;
#39476 = CARTESIAN_POINT('Ctrl Pts',(-19.951972487446,40.8602796890547,124.488778577698)) ;
#39477 = CARTESIAN_POINT('Ctrl Pts',(-20.0876630799847,40.6802906086448,124.75801282766)) ;
#39478 = CARTESIAN_POINT('Ctrl Pts',(-19.7567802099133,40.8702773452713,124.566778486158)) ;
#39479 = CARTESIAN_POINT('Ctrl Pts',(-19.8436735817006,40.6902882648614,124.855515120225)) ;
#39480 = CARTESIAN_POINT('Ctrl Pts',(-19.5500818247868,40.8803175583263,124.609481079621)) ;
#39481 = CARTESIAN_POINT('Ctrl Pts',(-19.5853011891649,40.7003284779165,124.908895920556)) ;
#39482 = CARTESIAN_POINT('Ctrl Pts',(-19.3435554371878,40.8901456056026,124.615967681651)) ;
#39483 = CARTESIAN_POINT('Ctrl Pts',(-19.3271425182184,40.7101565251927,124.917006738084)) ;
#39484 = CARTESIAN_POINT('Ctrl Pts',(-19.1343072045349,40.9001999526349,124.586146876164)) ;
#39485 = CARTESIAN_POINT('Ctrl Pts',(-19.0655819825026,40.7202108722251,124.879733201106)) ;
#39486 = CARTESIAN_POINT('Ctrl Pts',(-18.9357705406544,40.9101410889635,124.520845573056)) ;
#39487 = CARTESIAN_POINT('Ctrl Pts',(-18.8174100403861,40.7301520085537,124.798108890676)) ;
#39488 = CARTESIAN_POINT('Ctrl Pts',(-18.7519690818306,40.9200453220432,124.423000581694)) ;
#39489 = CARTESIAN_POINT('Ctrl Pts',(-18.5876566118976,40.7400562416334,124.675804537105)) ;
#39490 = CARTESIAN_POINT('Ctrl Pts',(-18.585688282195,40.9300920188868,124.292792552293)) ;
#39491 = CARTESIAN_POINT('Ctrl Pts',(-18.3798041844337,40.750102938477,124.513046489753)) ;
#39492 = CARTESIAN_POINT('Ctrl Pts',(-18.4464901568893,40.9399875701671,124.138142420818)) ;
#39493 = CARTESIAN_POINT('Ctrl Pts',(-18.2058043531238,40.7599984897572,124.319735002342)) ;
#39494 = CARTESIAN_POINT('Ctrl Pts',(-18.3344376414912,40.9500496480066,123.958756744201)) ;
#39495 = CARTESIAN_POINT('Ctrl Pts',(-18.0657367626223,40.7700605675967,124.095504335567)) ;
#39496 = CARTESIAN_POINT('Ctrl Pts',(-18.2568316622771,40.9598923571026,123.766911195192)) ;
#39497 = CARTESIAN_POINT('Ctrl Pts',(-17.9687267603037,40.7799032766928,123.85569749179)) ;
#39498 = CARTESIAN_POINT('Ctrl Pts',(-18.2125910584586,40.9698830893411,123.561614077019)) ;
#39499 = CARTESIAN_POINT('Ctrl Pts',(-17.9134237542837,40.7898940089313,123.599076400328)) ;
#39500 = CARTESIAN_POINT('Ctrl Pts',(-18.204750664211,40.9798111145698,123.353032026553)) ;
#39501 = CARTESIAN_POINT('Ctrl Pts',(-17.9036209756427,40.79982203416,123.338348435946)) ;
#39502 = CARTESIAN_POINT('Ctrl Pts',(-18.2330639112473,40.9897992612204,123.14496244916)) ;
#39503 = CARTESIAN_POINT('Ctrl Pts',(-17.9390103971516,40.8098101808106,123.078260992333)) ;
#39504 = CARTESIAN_POINT('Ctrl Pts',(-18.297681746232,40.9998342790604,122.944131359391)) ;
#39505 = CARTESIAN_POINT('Ctrl Pts',(-18.0197805146049,40.8198451986505,122.827221506628)) ;
#39506 = CARTESIAN_POINT('Ctrl Pts',(-18.3943201381265,41.0096990761655,122.760643431724)) ;
#39507 = CARTESIAN_POINT('Ctrl Pts',(-18.1405769535564,40.8297099957557,122.597859805784)) ;
#39508 = CARTESIAN_POINT('Ctrl Pts',(-18.5221077214792,41.0196598085217,122.594742227815)) ;
#39509 = CARTESIAN_POINT('Ctrl Pts',(-18.3003100261573,40.8396707281118,122.3904817787)) ;
#39510 = CARTESIAN_POINT('Ctrl Pts',(-18.6781171729852,41.0296932709187,122.452788170327)) ;
#39511 = CARTESIAN_POINT('Ctrl Pts',(-18.4953203364259,40.8497041905088,122.213037685438)) ;
#39512 = CARTESIAN_POINT('Ctrl Pts',(-18.8536177054508,41.0395788051301,122.341428905828)) ;
#39513 = CARTESIAN_POINT('Ctrl Pts',(-18.7146955767599,40.8595897247203,122.073836456168)) ;
#39514 = CARTESIAN_POINT('Ctrl Pts',(-19.0492301850846,41.0496436458101,122.260823818413)) ;
#39515 = CARTESIAN_POINT('Ctrl Pts',(-18.959210160501,40.8696545654002,121.97307830108)) ;
#39516 = CARTESIAN_POINT('Ctrl Pts',(-19.2514386207072,41.0594917775389,122.216286024392)) ;
#39517 = CARTESIAN_POINT('Ctrl Pts',(-19.2119712899372,40.8795026971291,121.917403865037)) ;
#39518 = CARTESIAN_POINT('Ctrl Pts',(-19.4620301676676,41.0695192745291,122.206830853245)) ;
#39519 = CARTESIAN_POINT('Ctrl Pts',(-19.4752106016356,40.8895301941192,121.905583046099)) ;
#39520 = CARTESIAN_POINT('Ctrl Pts',(-19.6710285196364,41.0795477265741,122.234643377154)) ;
#39521 = CARTESIAN_POINT('Ctrl Pts',(-19.7364587404742,40.8995586461643,121.940346685174)) ;
#39522 = CARTESIAN_POINT('Ctrl Pts',(-19.8684484239612,41.0893929931382,122.29677641338)) ;
#39523 = CARTESIAN_POINT('Ctrl Pts',(-19.9832352577445,40.9094039127284,122.018011497332)) ;
#39524 = CARTESIAN_POINT('Ctrl Pts',(-20.05506817094,41.0993836660792,122.39316265703)) ;
#39525 = CARTESIAN_POINT('Ctrl Pts',(-20.216510909968,40.9193945856693,122.138492853091)) ;
#39526 = CARTESIAN_POINT('Ctrl Pts',(-20.2226153017789,41.1094215481676,122.521458694971)) ;
#39527 = CARTESIAN_POINT('Ctrl Pts',(-20.4259458604825,40.9294324677578,122.298861327962)) ;
#39528 = CARTESIAN_POINT('Ctrl Pts',(-20.3628619913098,41.1192659186073,122.673663617627)) ;
#39529 = CARTESIAN_POINT('Ctrl Pts',(-20.6012563124349,40.9392768381975,122.489117146643)) ;
#39530 = CARTESIAN_POINT('Ctrl Pts',(-20.4764734479912,41.1292507460027,122.850139489613)) ;
#39531 = CARTESIAN_POINT('Ctrl Pts',(-20.7432721400765,40.9492616655929,122.709711313063)) ;
#39532 = CARTESIAN_POINT('Ctrl Pts',(-20.5574566491448,41.139190191408,123.042799763275)) ;
#39533 = CARTESIAN_POINT('Ctrl Pts',(-20.8445028247559,40.9592011109982,122.950536538192)) ;
#39534 = CARTESIAN_POINT('Ctrl Pts',(-20.6041559807991,41.1492301956939,123.248619953668)) ;
#39535 = CARTESIAN_POINT('Ctrl Pts',(-20.9028785374185,40.9692411152841,123.20781127081)) ;
#39536 = CARTESIAN_POINT('Ctrl Pts',(-20.6143967382331,41.1591173048795,123.456249137288)) ;
#39537 = CARTESIAN_POINT('Ctrl Pts',(-20.9156810986657,40.9791282244697,123.467348610192)) ;
#39538 = CARTESIAN_POINT('Ctrl Pts',(-20.5883994319064,41.169117364782,123.664835776685)) ;
#39539 = CARTESIAN_POINT('Ctrl Pts',(-20.8831859203431,40.9891282843722,123.728082234678)) ;
#39540 = CARTESIAN_POINT('Ctrl Pts',(-20.5272409128475,41.1790347806967,123.864195390867)) ;
#39541 = CARTESIAN_POINT('Ctrl Pts',(-20.8067389221257,40.9990457002868,123.977282854294)) ;
#39542 = CARTESIAN_POINT('Ctrl Pts',(-20.4311340846493,41.1890815954375,124.052246102088)) ;
#39543 = CARTESIAN_POINT('Ctrl Pts',(-20.6866067691322,41.0090925150276,124.212346711467)) ;
#39544 = CARTESIAN_POINT('Ctrl Pts',(-20.3061390393343,41.1989570726341,124.218058301868)) ;
#39545 = CARTESIAN_POINT('Ctrl Pts',(-20.5303634280542,41.0189679922243,124.419613620492)) ;
#39546 = CARTESIAN_POINT('Ctrl Pts',(-20.1516052416653,41.2090131683554,124.362275980325)) ;
#39547 = CARTESIAN_POINT('Ctrl Pts',(-20.337197279219,41.0290240879456,124.59988651574)) ;
#39548 = CARTESIAN_POINT('Ctrl Pts',(-19.977229302393,41.2189063303704,124.475710615594)) ;
#39549 = CARTESIAN_POINT('Ctrl Pts',(-20.1192272912167,41.0389172499606,124.741681401937)) ;
#39550 = CARTESIAN_POINT('Ctrl Pts',(-19.782620580465,41.228968566393,124.558568223159)) ;
#39551 = CARTESIAN_POINT('Ctrl Pts',(-19.8759671921911,41.0489794859832,124.845254462192)) ;
#39552 = CARTESIAN_POINT('Ctrl Pts',(-19.5810123835409,41.238813032022,124.605369966311)) ;
#39553 = CARTESIAN_POINT('Ctrl Pts',(-19.6239559484713,41.0588239516122,124.903758180458)) ;
#39554 = CARTESIAN_POINT('Ctrl Pts',(-19.3719656317782,41.2487731247261,124.617339157751)) ;
#39555 = CARTESIAN_POINT('Ctrl Pts',(-19.3626471098538,41.0687840443163,124.918720690841)) ;
#39556 = CARTESIAN_POINT('Ctrl Pts',(-19.1624388090685,41.2588114137072,124.592224884282)) ;
#39557 = CARTESIAN_POINT('Ctrl Pts',(-19.1007386053402,41.0788223332973,124.887329010264)) ;
#39558 = CARTESIAN_POINT('Ctrl Pts',(-18.9636200217074,41.2686847368134,124.532486383853)) ;
#39559 = CARTESIAN_POINT('Ctrl Pts',(-18.8522137572245,41.0886956564036,124.812656518807)) ;
#39560 = CARTESIAN_POINT('Ctrl Pts',(-18.7745367667636,41.2787579208985,124.437217363327)) ;
#39561 = CARTESIAN_POINT('Ctrl Pts',(-18.6158596069145,41.0987688404886,124.693571352433)) ;
#39562 = CARTESIAN_POINT('Ctrl Pts',(-18.6088938849064,41.2885784331864,124.313905580801)) ;
#39563 = CARTESIAN_POINT('Ctrl Pts',(-18.4088042083413,41.1085893527766,124.539431437852)) ;
#39564 = CARTESIAN_POINT('Ctrl Pts',(-18.4633794200554,41.2986564293022,124.159977351109)) ;
#39565 = CARTESIAN_POINT('Ctrl Pts',(-18.2269108302381,41.1186673488924,124.34702207149)) ;
#39566 = CARTESIAN_POINT('Ctrl Pts',(-18.34929862132,41.3085105042855,123.986997787861)) ;
#39567 = CARTESIAN_POINT('Ctrl Pts',(-18.0843084262806,41.1285214238756,124.130796993376)) ;
#39568 = CARTESIAN_POINT('Ctrl Pts',(-18.2650562986397,41.3185743858692,123.79296185912)) ;
#39569 = CARTESIAN_POINT('Ctrl Pts',(-17.9790049811193,41.1385853054594,123.888252695301)) ;
#39570 = CARTESIAN_POINT('Ctrl Pts',(-18.2166879254847,41.3284578118429,123.590852828316)) ;
#39571 = CARTESIAN_POINT('Ctrl Pts',(-17.9185435300632,41.1484687314331,123.635615538462)) ;
#39572 = CARTESIAN_POINT('Ctrl Pts',(-18.2036681221716,41.338458415764,123.381049020955)) ;
#39573 = CARTESIAN_POINT('Ctrl Pts',(-17.9022681371012,41.1584693353541,123.373360677128)) ;
#39574 = CARTESIAN_POINT('Ctrl Pts',(-18.2269611110855,41.3483782001018,123.173770725139)) ;
#39575 = CARTESIAN_POINT('Ctrl Pts',(-17.9313838879789,41.168389119692,123.114261971912)) ;
#39576 = CARTESIAN_POINT('Ctrl Pts',(-18.2866756180986,41.3584255504587,122.971196494413)) ;
#39577 = CARTESIAN_POINT('Ctrl Pts',(-18.006026378471,41.1784364700489,122.861044240418)) ;
#39578 = CARTESIAN_POINT('Ctrl Pts',(-18.3788795710986,41.368302892693,122.785091205517)) ;
#39579 = CARTESIAN_POINT('Ctrl Pts',(-18.1212813811311,41.1883138122831,122.628411371789)) ;
#39580 = CARTESIAN_POINT('Ctrl Pts',(-18.5043585823623,41.3783727737676,122.614637642039)) ;
#39581 = CARTESIAN_POINT('Ctrl Pts',(-18.2781294850694,41.1983836933578,122.415344458244)) ;
#39582 = CARTESIAN_POINT('Ctrl Pts',(-18.6537818292948,41.3882024789693,122.471833456278)) ;
#39583 = CARTESIAN_POINT('Ctrl Pts',(-18.464909367622,41.2082133985595,122.236837854642)) ;
#39584 = CARTESIAN_POINT('Ctrl Pts',(-18.8296579695578,41.3982691401357,122.35418375427)) ;
#39585 = CARTESIAN_POINT('Ctrl Pts',(-18.6847540386552,41.2182800597259,122.089775689202)) ;
#39586 = CARTESIAN_POINT('Ctrl Pts',(-19.0200041203782,41.408159362003,122.270450878119)) ;
#39587 = CARTESIAN_POINT('Ctrl Pts',(-18.9226875395076,41.2281702815932,121.985108837404)) ;
#39588 = CARTESIAN_POINT('Ctrl Pts',(-19.2239333482095,41.4181515381132,122.220092117685)) ;
#39589 = CARTESIAN_POINT('Ctrl Pts',(-19.1775992382412,41.2381624577033,121.922160157679)) ;
#39590 = CARTESIAN_POINT('Ctrl Pts',(-19.432913401362,41.4281143682258,122.206147099919)) ;
#39591 = CARTESIAN_POINT('Ctrl Pts',(-19.4388247420812,41.248125287816,121.904728591828)) ;
#39592 = CARTESIAN_POINT('Ctrl Pts',(-19.6399945794,41.4380185806261,122.228042536446)) ;
#39593 = CARTESIAN_POINT('Ctrl Pts',(-19.6976771545736,41.2580295002163,121.932097935287)) ;
#39594 = CARTESIAN_POINT('Ctrl Pts',(-19.84319524037,41.448079294714,122.286638879611)) ;
#39595 = CARTESIAN_POINT('Ctrl Pts',(-19.9516776747538,41.2680902143041,122.005343143333)) ;
#39596 = CARTESIAN_POINT('Ctrl Pts',(-20.0291359735094,41.4579187976968,122.377353855789)) ;
#39597 = CARTESIAN_POINT('Ctrl Pts',(-20.1841049253303,41.277929717287,122.118737500437)) ;
#39598 = CARTESIAN_POINT('Ctrl Pts',(-20.2004294013988,41.4679849362632,122.501563731977)) ;
#39599 = CARTESIAN_POINT('Ctrl Pts',(-20.398221343626,41.2879958558534,122.273999666792)) ;
#39600 = CARTESIAN_POINT('Ctrl Pts',(-20.3448588998162,41.4778674507492,122.650955267273)) ;
#39601 = CARTESIAN_POINT('Ctrl Pts',(-20.5787589736022,41.2978783703394,122.460739928053)) ;
#39602 = CARTESIAN_POINT('Ctrl Pts',(-20.4627539040108,41.4878597501047,122.824784252551)) ;
#39603 = CARTESIAN_POINT('Ctrl Pts',(-20.726127681702,41.3078706696949,122.678026456286)) ;
#39604 = CARTESIAN_POINT('Ctrl Pts',(-20.5484123348916,41.4978128170581,123.01572690911)) ;
#39605 = CARTESIAN_POINT('Ctrl Pts',(-20.8332007283989,41.3178237366483,122.916705335821)) ;
#39606 = CARTESIAN_POINT('Ctrl Pts',(-20.5999387117747,41.5078475252634,123.220282510794)) ;
#39607 = CARTESIAN_POINT('Ctrl Pts',(-20.8976084793922,41.3278584448536,123.172399737511)) ;
#39608 = CARTESIAN_POINT('Ctrl Pts',(-20.6150963668154,41.5177357461675,123.42762288197)) ;
#39609 = CARTESIAN_POINT('Ctrl Pts',(-20.9165553817882,41.3377466657577,123.431576287924)) ;
#39610 = CARTESIAN_POINT('Ctrl Pts',(-20.5941420991674,41.527730169198,123.636678083396)) ;
#39611 = CARTESIAN_POINT('Ctrl Pts',(-20.8903621465551,41.3477410887881,123.692895458751)) ;
#39612 = CARTESIAN_POINT('Ctrl Pts',(-20.5374038460003,41.5376755086441,123.837915099807)) ;
#39613 = CARTESIAN_POINT('Ctrl Pts',(-20.8194388312566,41.3576864282343,123.944442205992)) ;
#39614 = CARTESIAN_POINT('Ctrl Pts',(-20.4469513423603,41.5476228532555,124.026477171833)) ;
#39615 = CARTESIAN_POINT('Ctrl Pts',(-20.7063724849258,41.3676337728457,124.180145089971)) ;
#39616 = CARTESIAN_POINT('Ctrl Pts',(-20.3237166893896,41.5576707486665,124.198034788354)) ;
#39617 = CARTESIAN_POINT('Ctrl Pts',(-20.5523289699453,41.3776816682566,124.394591659051)) ;
#39618 = CARTESIAN_POINT('Ctrl Pts',(-20.1756958626887,41.5675183941458,124.342779195868)) ;
#39619 = CARTESIAN_POINT('Ctrl Pts',(-20.3673015896702,41.387529313736,124.575522794195)) ;
#39620 = CARTESIAN_POINT('Ctrl Pts',(-20.0031915988338,41.5774801080598,124.461512163313)) ;
#39621 = CARTESIAN_POINT('Ctrl Pts',(-20.1516704587089,41.39749102765,124.72393864251)) ;
#39622 = CARTESIAN_POINT('Ctrl Pts',(-19.8112800553437,41.5875087323508,124.548840187101)) ;
#39623 = CARTESIAN_POINT('Ctrl Pts',(-19.9117808501252,41.407519651941,124.833098044419)) ;
#39624 = CARTESIAN_POINT('Ctrl Pts',(-19.6095677146579,41.5974190930075,124.600957112613)) ;
#39625 = CARTESIAN_POINT('Ctrl Pts',(-19.6596394073154,41.4174300125977,124.898243770092)) ;
#39626 = CARTESIAN_POINT('Ctrl Pts',(-19.4013858198479,41.6073537915808,124.617849546448)) ;
#39627 = CARTESIAN_POINT('Ctrl Pts',(-19.3994113076563,41.4273647111709,124.919358484118)) ;
#39628 = CARTESIAN_POINT('Ctrl Pts',(-19.1912280423145,41.617395616435,124.597921301321)) ;
#39629 = CARTESIAN_POINT('Ctrl Pts',(-19.1367143515036,41.4374065360251,124.894447395095)) ;
#39630 = CARTESIAN_POINT('Ctrl Pts',(-18.990832747362,41.6272801901794,124.542852864692)) ;
#39631 = CARTESIAN_POINT('Ctrl Pts',(-18.8862194476492,41.4472911097696,124.825610729132)) ;
#39632 = CARTESIAN_POINT('Ctrl Pts',(-18.8007506253046,41.6372820395426,124.453017154148)) ;
#39633 = CARTESIAN_POINT('Ctrl Pts',(-18.6486170761849,41.4572929591327,124.713315149786)) ;
#39634 = CARTESIAN_POINT('Ctrl Pts',(-18.6304363747329,41.6472013411166,124.332637276004)) ;
#39635 = CARTESIAN_POINT('Ctrl Pts',(-18.4357242322811,41.4672122607068,124.562839022711)) ;
#39636 = CARTESIAN_POINT('Ctrl Pts',(-18.4817919543754,41.6572454494619,124.182685192246)) ;
#39637 = CARTESIAN_POINT('Ctrl Pts',(-18.2499195837337,41.4772563690521,124.375398347037)) ;
#39638 = CARTESIAN_POINT('Ctrl Pts',(-18.3632889695078,41.6671298729041,124.011973794938)) ;
#39639 = CARTESIAN_POINT('Ctrl Pts',(-18.101791128682,41.4871407924943,124.162007655871)) ;
#39640 = CARTESIAN_POINT('Ctrl Pts',(-18.2746407632442,41.6771462348136,123.820958583722)) ;
#39641 = CARTESIAN_POINT('Ctrl Pts',(-17.9909819761394,41.4971571544038,123.923238127111)) ;
#39642 = CARTESIAN_POINT('Ctrl Pts',(-18.2209377342613,41.687182890319,123.616916772057)) ;
#39643 = CARTESIAN_POINT('Ctrl Pts',(-17.923854202781,41.5071938099091,123.668185724593)) ;
#39644 = CARTESIAN_POINT('Ctrl Pts',(-18.2032737429254,41.6970130205083,123.410988166114)) ;
#39645 = CARTESIAN_POINT('Ctrl Pts',(-17.9017753133352,41.5170239400985,123.410773438911)) ;
#39646 = CARTESIAN_POINT('Ctrl Pts',(-18.2220155993058,41.7070890735982,123.200029060193)) ;
#39647 = CARTESIAN_POINT('Ctrl Pts',(-17.9252038428082,41.5270999931883,123.147075094829)) ;
#39648 = CARTESIAN_POINT('Ctrl Pts',(-18.2757906963554,41.716941302784,122.999961670963)) ;
#39649 = CARTESIAN_POINT('Ctrl Pts',(-17.9924242808848,41.5369522223742,122.896990000654)) ;
#39650 = CARTESIAN_POINT('Ctrl Pts',(-18.3652603008448,41.7270145105833,122.808056320445)) ;
#39651 = CARTESIAN_POINT('Ctrl Pts',(-18.104262344417,41.5470254301734,122.657109249367)) ;
#39652 = CARTESIAN_POINT('Ctrl Pts',(-18.4839724624689,41.7368560219347,122.638585553312)) ;
#39653 = CARTESIAN_POINT('Ctrl Pts',(-18.2526543868077,41.5568669415249,122.445270485512)) ;
#39654 = CARTESIAN_POINT('Ctrl Pts',(-18.6315099791709,41.7468169599722,122.489983799293)) ;
#39655 = CARTESIAN_POINT('Ctrl Pts',(-18.4370777101602,41.5668278795624,122.259519138092)) ;
#39656 = CARTESIAN_POINT('Ctrl Pts',(-18.8041736856207,41.7568548218972,122.368670001095)) ;
#39657 = CARTESIAN_POINT('Ctrl Pts',(-18.6529080737504,41.5768657414874,122.107878162764)) ;
#39658 = CARTESIAN_POINT('Ctrl Pts',(-18.9920269431984,41.7667290078943,122.280273355514)) ;
#39659 = CARTESIAN_POINT('Ctrl Pts',(-18.8877262423415,41.5867399274844,121.997383365616)) ;
#39660 = CARTESIAN_POINT('Ctrl Pts',(-19.1963027713809,41.7767991674721,122.224790072043)) ;
#39661 = CARTESIAN_POINT('Ctrl Pts',(-19.1430711045698,41.5968100870623,121.928030886466)) ;
#39662 = CARTESIAN_POINT('Ctrl Pts',(-19.4021553537775,41.786630914898,122.205937341071)) ;
#39663 = CARTESIAN_POINT('Ctrl Pts',(-19.4003882644738,41.6066418344882,121.90446647736)) ;
#39664 = CARTESIAN_POINT('Ctrl Pts',(-19.6124500007053,41.7966669949693,122.222921105174)) ;
#39665 = CARTESIAN_POINT('Ctrl Pts',(-19.6632563157886,41.6166779145595,121.925697979443)) ;
#39666 = CARTESIAN_POINT('Ctrl Pts',(-19.8161003455475,41.8066840418218,122.27657994795)) ;
#39667 = CARTESIAN_POINT('Ctrl Pts',(-19.9178188413612,41.626694961412,121.992773118828)) ;
#39668 = CARTESIAN_POINT('Ctrl Pts',(-20.004923629097,41.8165662999884,122.363238250864)) ;
#39669 = CARTESIAN_POINT('Ctrl Pts',(-20.1538480382327,41.6365772195785,122.101097977742)) ;
#39670 = CARTESIAN_POINT('Ctrl Pts',(-20.1777719329602,41.8265539827847,122.482413681147)) ;
#39671 = CARTESIAN_POINT('Ctrl Pts',(-20.3699075386574,41.6465649023749,122.250068895557)) ;
#39672 = CARTESIAN_POINT('Ctrl Pts',(-20.326844928488,41.8365006395015,122.629102840794)) ;
#39673 = CARTESIAN_POINT('Ctrl Pts',(-20.5562477856128,41.6565115590916,122.433432011436)) ;
#39674 = CARTESIAN_POINT('Ctrl Pts',(-20.4493206526294,41.8465576975816,122.801419365625)) ;
#39675 = CARTESIAN_POINT('Ctrl Pts',(-20.70934082782,41.6665686171718,122.648828544802)) ;
#39676 = CARTESIAN_POINT('Ctrl Pts',(-20.5381348768749,41.8563758771311,122.98775540366)) ;
#39677 = CARTESIAN_POINT('Ctrl Pts',(-20.8203574276799,41.6763867967212,122.8817505594)) ;
#39678 = CARTESIAN_POINT('Ctrl Pts',(-20.5950148919747,41.86641181157,123.190925085264)) ;
#39679 = CARTESIAN_POINT('Ctrl Pts',(-20.8914554134342,41.6864227311602,123.135713115913)) ;
#39680 = CARTESIAN_POINT('Ctrl Pts',(-20.615129903165,41.876436465999,123.400720653862)) ;
#39681 = CARTESIAN_POINT('Ctrl Pts',(-20.9165972821223,41.6964473855892,123.397957733957)) ;
#39682 = CARTESIAN_POINT('Ctrl Pts',(-20.5992555683587,41.8862884855786,123.607234834638)) ;
#39683 = CARTESIAN_POINT('Ctrl Pts',(-20.8967522554503,41.7062994051687,123.656101312772)) ;
#39684 = CARTESIAN_POINT('Ctrl Pts',(-20.5473561444667,41.8962793992935,123.810736345392)) ;
#39685 = CARTESIAN_POINT('Ctrl Pts',(-20.8318758705057,41.7162903188837,123.910477841252)) ;
#39686 = CARTESIAN_POINT('Ctrl Pts',(-20.4616446993946,41.9061973881331,124.000839502752)) ;
#39687 = CARTESIAN_POINT('Ctrl Pts',(-20.7247343586045,41.7262083077233,124.14810642243)) ;
#39688 = CARTESIAN_POINT('Ctrl Pts',(-20.3429884977472,41.9162254988639,124.175080591613)) ;
#39689 = CARTESIAN_POINT('Ctrl Pts',(-20.576412327472,41.7362364184541,124.365906529222)) ;
#39690 = CARTESIAN_POINT('Ctrl Pts',(-20.1980255650348,41.9261106967723,124.323996156688)) ;
#39691 = CARTESIAN_POINT('Ctrl Pts',(-20.3952065715185,41.7461216163624,124.552049981511)) ;
#39692 = CARTESIAN_POINT('Ctrl Pts',(-20.0279320557978,41.9360999720403,124.447175593972)) ;
#39693 = CARTESIAN_POINT('Ctrl Pts',(-20.1825881915895,41.7561108916304,124.706022484773)) ;
#39694 = CARTESIAN_POINT('Ctrl Pts',(-19.837857448319,41.9461414302098,124.539013945011)) ;
#39695 = CARTESIAN_POINT('Ctrl Pts',(-19.9449940548439,41.7661523498,124.820818389539)) ;
#39696 = CARTESIAN_POINT('Ctrl Pts',(-19.6390644945786,41.9559728939981,124.595621547206)) ;
#39697 = CARTESIAN_POINT('Ctrl Pts',(-19.6965012965353,41.7759838135883,124.8915759365)) ;
#39698 = CARTESIAN_POINT('Ctrl Pts',(-19.4299150619604,41.965977826302,124.617688613248)) ;
#39699 = CARTESIAN_POINT('Ctrl Pts',(-19.4350641759106,41.7859887458922,124.919157369888)) ;
#39700 = CARTESIAN_POINT('Ctrl Pts',(-19.2204473086949,41.9759641901967,124.603013545437)) ;
#39701 = CARTESIAN_POINT('Ctrl Pts',(-19.173229491633,41.7959751097869,124.900811143263)) ;
#39702 = CARTESIAN_POINT('Ctrl Pts',(-19.0159203877433,41.9859938190826,124.551823701844)) ;
#39703 = CARTESIAN_POINT('Ctrl Pts',(-18.9175714408516,41.8060047386728,124.836821562525)) ;
#39704 = CARTESIAN_POINT('Ctrl Pts',(-18.8262081647961,41.995869041191,124.467451255716)) ;
#39705 = CARTESIAN_POINT('Ctrl Pts',(-18.6804315219081,41.8158799607811,124.731353527427)) ;
#39706 = CARTESIAN_POINT('Ctrl Pts',(-18.6517356024177,42.0058702535881,124.350176231649)) ;
#39707 = CARTESIAN_POINT('Ctrl Pts',(-18.4623421035924,41.8258811731783,124.58475763756)) ;
#39708 = CARTESIAN_POINT('Ctrl Pts',(-18.5014918306554,42.0157788328236,124.205833220851)) ;
#39709 = CARTESIAN_POINT('Ctrl Pts',(-18.2745387789703,41.8357897524138,124.40432673796)) ;
#39710 = CARTESIAN_POINT('Ctrl Pts',(-18.376872413352,42.0258336853796,124.035131663706)) ;
#39711 = CARTESIAN_POINT('Ctrl Pts',(-18.1187665880274,41.8458446049698,124.190948411638)) ;
#39712 = CARTESIAN_POINT('Ctrl Pts',(-18.285357700117,42.0356922676544,123.849131188738)) ;
#39713 = CARTESIAN_POINT('Ctrl Pts',(-18.0043751833933,41.8557031872446,123.958446111425)) ;
#39714 = CARTESIAN_POINT('Ctrl Pts',(-18.2261951447151,42.0457603970971,123.645935941914)) ;
#39715 = CARTESIAN_POINT('Ctrl Pts',(-17.9304244939929,41.8657713166872,123.704451485335)) ;
#39716 = CARTESIAN_POINT('Ctrl Pts',(-18.2037096295155,42.0556158687862,123.439949227679)) ;
#39717 = CARTESIAN_POINT('Ctrl Pts',(-17.9023200740901,41.8756267883763,123.446967189867)) ;
#39718 = CARTESIAN_POINT('Ctrl Pts',(-18.2168940215252,42.0656107171724,123.230246957662)) ;
#39719 = CARTESIAN_POINT('Ctrl Pts',(-17.9188032302144,41.8856216367626,123.184839420301)) ;
#39720 = CARTESIAN_POINT('Ctrl Pts',(-18.2669137943528,42.0756420139569,123.025370929616)) ;
#39721 = CARTESIAN_POINT('Ctrl Pts',(-17.9813304618854,41.8956529335471,122.928744998812)) ;
#39722 = CARTESIAN_POINT('Ctrl Pts',(-18.3500517364716,42.085508550167,122.835328127626)) ;
#39723 = CARTESIAN_POINT('Ctrl Pts',(-18.085255518592,41.9055194697571,122.691192079441)) ;
#39724 = CARTESIAN_POINT('Ctrl Pts',(-18.4660321364788,42.0954959731278,122.660329302149)) ;
#39725 = CARTESIAN_POINT('Ctrl Pts',(-18.2302333322314,41.915506892718,122.472444933133)) ;
#39726 = CARTESIAN_POINT('Ctrl Pts',(-18.6099789814412,42.1054409121476,122.508661371675)) ;
#39727 = CARTESIAN_POINT('Ctrl Pts',(-18.4101690100721,41.9254518317378,122.282861709765)) ;
#39728 = CARTESIAN_POINT('Ctrl Pts',(-18.7797885338698,42.1154857980076,122.383148139199)) ;
#39729 = CARTESIAN_POINT('Ctrl Pts',(-18.6224325373826,41.9354967175978,122.125972345767)) ;
#39730 = CARTESIAN_POINT('Ctrl Pts',(-18.9654610961427,42.1253543330938,122.290568762634)) ;
#39731 = CARTESIAN_POINT('Ctrl Pts',(-18.8545248231333,41.945365252684,122.010250360276)) ;
#39732 = CARTESIAN_POINT('Ctrl Pts',(-19.1661696006187,42.1353202011005,122.230497998175)) ;
#39733 = CARTESIAN_POINT('Ctrl Pts',(-19.1054113849809,41.9553311206907,121.935164518656)) ;
#39734 = CARTESIAN_POINT('Ctrl Pts',(-19.3754959713858,42.145342848553,122.206283829226)) ;
#39735 = CARTESIAN_POINT('Ctrl Pts',(-19.3670697024501,41.9653537681432,121.904899528169)) ;
#39736 = CARTESIAN_POINT('Ctrl Pts',(-19.5837472933625,42.1552664875606,122.218600651272)) ;
#39737 = CARTESIAN_POINT('Ctrl Pts',(-19.6273839317771,41.9752774071507,121.920298317291)) ;
#39738 = CARTESIAN_POINT('Ctrl Pts',(-19.7872248880091,42.1652092125663,122.266499710306)) ;
#39739 = CARTESIAN_POINT('Ctrl Pts',(-19.8817304497054,41.9852201321565,121.980174899342)) ;
#39740 = CARTESIAN_POINT('Ctrl Pts',(-19.98116015884,42.1752548186182,122.350078644094)) ;
#39741 = CARTESIAN_POINT('Ctrl Pts',(-20.1241484577125,41.9952657382084,122.084651122063)) ;
#39742 = CARTESIAN_POINT('Ctrl Pts',(-20.1545514692075,42.1851162411393,122.463760650406)) ;
#39743 = CARTESIAN_POINT('Ctrl Pts',(-20.3408862917472,42.0051271607295,122.226756112428)) ;
#39744 = CARTESIAN_POINT('Ctrl Pts',(-20.3078045675298,42.1951098095885,122.607431591005)) ;
#39745 = CARTESIAN_POINT('Ctrl Pts',(-20.5324507968352,42.0151207291787,122.406346888333)) ;
#39746 = CARTESIAN_POINT('Ctrl Pts',(-20.4330485966864,42.2050352803438,122.774367875557)) ;
#39747 = CARTESIAN_POINT('Ctrl Pts',(-20.689003659768,42.025046199934,122.61501906144)) ;
#39748 = CARTESIAN_POINT('Ctrl Pts',(-20.528359134433,42.2150629542996,122.96237648736)) ;
#39749 = CARTESIAN_POINT('Ctrl Pts',(-20.808139363891,42.0350738738898,122.850031069937)) ;
#39750 = CARTESIAN_POINT('Ctrl Pts',(-20.5889282022475,42.2249501323413,123.161244468246)) ;
#39751 = CARTESIAN_POINT('Ctrl Pts',(-20.8838479742396,42.0449610519315,123.098617303738)) ;
#39752 = CARTESIAN_POINT('Ctrl Pts',(-20.6145455202288,42.2349785117095,123.370482821943)) ;
#39753 = CARTESIAN_POINT('Ctrl Pts',(-20.9158670632357,42.0549894312997,123.360164459765)) ;
#39754 = CARTESIAN_POINT('Ctrl Pts',(-20.6037026584376,42.244872754431,123.57823145244)) ;
#39755 = CARTESIAN_POINT('Ctrl Pts',(-20.9023097752642,42.0648836740212,123.619854631493)) ;
#39756 = CARTESIAN_POINT('Ctrl Pts',(-20.5408518696117,42.2582256710819,123.851819040007)) ;
#39757 = CARTESIAN_POINT('Ctrl Pts',(-20.8237470249791,42.078236590672,123.961816174776)) ;
#39758 = CARTESIAN_POINT('Ctrl Pts',(-20.4095172303577,42.2714281888286,124.099989933585)) ;
#39759 = CARTESIAN_POINT('Ctrl Pts',(-20.6595997815487,42.0914391084188,124.272009590698)) ;
#39760 = CARTESIAN_POINT('Ctrl Pts',(-20.2186534632653,42.2847840941096,124.305832996325)) ;
#39761 = CARTESIAN_POINT('Ctrl Pts',(-20.4209837963246,42.1047950136997,124.529355053703)) ;
#39762 = CARTESIAN_POINT('Ctrl Pts',(-20.0529351292621,42.2946807427474,124.431692913237)) ;
#39763 = CARTESIAN_POINT('Ctrl Pts',(-20.2138409515124,42.1146916623376,124.686668821031)) ;
#39764 = CARTESIAN_POINT('Ctrl Pts',(-19.8651277354385,42.3047288807999,124.528356903845)) ;
#39765 = CARTESIAN_POINT('Ctrl Pts',(-19.9790784983031,42.12473980039,124.807498749115)) ;
#39766 = CARTESIAN_POINT('Ctrl Pts',(-19.6665158493402,42.3146198409776,124.58996703809)) ;
#39767 = CARTESIAN_POINT('Ctrl Pts',(-19.7308134332354,42.1346307605678,124.884508093011)) ;
#39768 = CARTESIAN_POINT('Ctrl Pts',(-19.4581683197363,42.3246126768544,124.616948547445)) ;
#39769 = CARTESIAN_POINT('Ctrl Pts',(-19.4703782998124,42.1446235964446,124.918232356499)) ;
#39770 = CARTESIAN_POINT('Ctrl Pts',(-19.2473681600248,42.334651771856,124.606814985885)) ;
#39771 = CARTESIAN_POINT('Ctrl Pts',(-19.2068788945303,42.1546626914461,124.905562766007)) ;
#39772 = CARTESIAN_POINT('Ctrl Pts',(-19.0455307327722,42.3444891277071,124.561634051858)) ;
#39773 = CARTESIAN_POINT('Ctrl Pts',(-18.9545800921751,42.1645000472973,124.849083179749)) ;
#39774 = CARTESIAN_POINT('Ctrl Pts',(-18.7855849758638,42.3578820756379,124.453519111834)) ;
#39775 = CARTESIAN_POINT('Ctrl Pts',(-18.6296634518403,42.177892995228,124.713940021427)) ;
#39776 = CARTESIAN_POINT('Ctrl Pts',(-18.5635083695273,42.3710487520648,124.282885771656)) ;
#39777 = CARTESIAN_POINT('Ctrl Pts',(-18.3520925364805,42.191059671655,124.500678451759)) ;
#39778 = CARTESIAN_POINT('Ctrl Pts',(-18.392149943478,42.3844335334716,124.059804324477)) ;
#39779 = CARTESIAN_POINT('Ctrl Pts',(-18.1378563759375,42.2044444530618,124.221781306331)) ;
#39780 = CARTESIAN_POINT('Ctrl Pts',(-18.2962255678194,42.3942953161154,123.875955923581)) ;
#39781 = CARTESIAN_POINT('Ctrl Pts',(-18.0179616237047,42.2143062357056,123.991978653558)) ;
#39782 = CARTESIAN_POINT('Ctrl Pts',(-18.2325120769393,42.4042944640685,123.675676595792)) ;
#39783 = CARTESIAN_POINT('Ctrl Pts',(-17.9383202715921,42.2243053836587,123.741625973952)) ;
#39784 = CARTESIAN_POINT('Ctrl Pts',(-18.2046075101168,42.4141972566856,123.469320833634)) ;
#39785 = CARTESIAN_POINT('Ctrl Pts',(-17.9034419631951,42.2342081762757,123.483683307467)) ;
#39786 = CARTESIAN_POINT('Ctrl Pts',(-18.2131324921205,42.4242468365765,123.258275057059)) ;
#39787 = CARTESIAN_POINT('Ctrl Pts',(-17.9141036163892,42.2442577561667,123.21987047092)) ;
#39788 = CARTESIAN_POINT('Ctrl Pts',(-18.271742279274,42.437433910386,122.987181315059)) ;
#39789 = CARTESIAN_POINT('Ctrl Pts',(-17.9873542557703,42.2574448299761,122.881031053138)) ;
#39790 = CARTESIAN_POINT('Ctrl Pts',(-18.4346521343874,42.4541867003572,122.670610361465)) ;
#39791 = CARTESIAN_POINT('Ctrl Pts',(-18.1910268971843,42.2741976199474,122.485278257372)) ;
#39792 = CARTESIAN_POINT('Ctrl Pts',(-18.6920409930995,42.4706753524519,122.432258546102)) ;
#39793 = CARTESIAN_POINT('Ctrl Pts',(-18.5127023286891,42.2906862720421,122.187393477303)) ;
#39794 = CARTESIAN_POINT('Ctrl Pts',(-18.9400618332129,42.4840321786353,122.300845882537)) ;
#39795 = CARTESIAN_POINT('Ctrl Pts',(-18.8227825349373,42.3040430982254,122.02309131617)) ;
#39796 = CARTESIAN_POINT('Ctrl Pts',(-19.1380453310715,42.4939285635132,122.236723926044)) ;
#39797 = CARTESIAN_POINT('Ctrl Pts',(-19.0702507618839,42.3139394831034,121.942948929618)) ;
#39798 = CARTESIAN_POINT('Ctrl Pts',(-19.346318954824,42.5039350780337,122.2075435774)) ;
#39799 = CARTESIAN_POINT('Ctrl Pts',(-19.3305991664971,42.3239459976239,121.906474651772)) ;
#39800 = CARTESIAN_POINT('Ctrl Pts',(-19.623580125889,42.5171252015501,122.216652416966)) ;
#39801 = CARTESIAN_POINT('Ctrl Pts',(-19.6771578660566,42.3371361211402,121.917859655093)) ;
#39802 = CARTESIAN_POINT('Ctrl Pts',(-19.9644761073968,42.5338917626996,122.32049383106)) ;
#39803 = CARTESIAN_POINT('Ctrl Pts',(-20.1032957575769,42.3539026822898,122.047670197604)) ;
#39804 = CARTESIAN_POINT('Ctrl Pts',(-20.3009572251947,42.5536762514077,122.573177848514)) ;
#39805 = CARTESIAN_POINT('Ctrl Pts',(-20.5238873611749,42.3736871709978,122.363526340952)) ;
#39806 = CARTESIAN_POINT('Ctrl Pts',(-20.5338536920251,42.5736216990041,122.927472083475)) ;
#39807 = CARTESIAN_POINT('Ctrl Pts',(-20.8150059841299,42.3936326185943,122.806396279315)) ;
#39808 = CARTESIAN_POINT('Ctrl Pts',(-20.6313376491033,42.5935333611601,123.339481760479)) ;
#39809 = CARTESIAN_POINT('Ctrl Pts',(-20.936856534069,42.4135442807503,123.321408446945)) ;
#39810 = CARTESIAN_POINT('Ctrl Pts',(-20.5833429972544,42.6134255531789,123.75977761235)) ;
#39811 = CARTESIAN_POINT('Ctrl Pts',(-20.8768601174768,42.4334364727691,123.846776921261)) ;
#39812 = CARTESIAN_POINT('Ctrl Pts',(-20.3928775516324,42.6334666837336,124.140904242147)) ;
#39813 = CARTESIAN_POINT('Ctrl Pts',(-20.6387749465304,42.4534776033238,124.323184054262)) ;
#39814 = CARTESIAN_POINT('Ctrl Pts',(-20.0872595412336,42.6532850183492,124.431171962633)) ;
#39815 = CARTESIAN_POINT('Ctrl Pts',(-20.2567515624384,42.4732959379394,124.686015098772)) ;
#39816 = CARTESIAN_POINT('Ctrl Pts',(-19.6984277741902,42.6732575835688,124.601563615224)) ;
#39817 = CARTESIAN_POINT('Ctrl Pts',(-19.7707111217322,42.4932685031589,124.899002007954)) ;
#39818 = CARTESIAN_POINT('Ctrl Pts',(-19.2762631710593,42.6931467997404,124.629052850656)) ;
#39819 = CARTESIAN_POINT('Ctrl Pts',(-19.2430064355519,42.5131577193306,124.933361057045)) ;
#39820 = CARTESIAN_POINT('Ctrl Pts',(-18.8676531896362,42.7131703740631,124.5098269493)) ;
#39821 = CARTESIAN_POINT('Ctrl Pts',(-18.7322443545609,42.5331812936533,124.784326245824)) ;
#39822 = CARTESIAN_POINT('Ctrl Pts',(-18.5278123839697,42.7329675371513,124.26130431907)) ;
#39823 = CARTESIAN_POINT('Ctrl Pts',(-18.3074466868531,42.5529784567415,124.473672881687)) ;
#39824 = CARTESIAN_POINT('Ctrl Pts',(-18.2904261749242,42.7529330309751,123.909466884417)) ;
#39825 = CARTESIAN_POINT('Ctrl Pts',(-18.0107152100322,42.5729439505653,124.033875901422)) ;
#39826 = CARTESIAN_POINT('Ctrl Pts',(-18.187872486649,42.7728867387165,123.49766130319)) ;
#39827 = CARTESIAN_POINT('Ctrl Pts',(-17.8825244705075,42.5928976583067,123.519119143686)) ;
#39828 = CARTESIAN_POINT('Ctrl Pts',(-18.2318581554824,42.7927941154431,123.076763552661)) ;
#39829 = CARTESIAN_POINT('Ctrl Pts',(-17.937507467377,42.6128050350333,122.992998485327)) ;
#39830 = CARTESIAN_POINT('Ctrl Pts',(-18.4153780545509,42.8126463269917,122.696553693905)) ;
#39831 = CARTESIAN_POINT('Ctrl Pts',(-18.1669062691419,42.6326572465818,122.517738273544)) ;
#39832 = CARTESIAN_POINT('Ctrl Pts',(-18.7212077898556,42.8327187139374,122.398884993394)) ;
#39833 = CARTESIAN_POINT('Ctrl Pts',(-18.5491943142901,42.6527296335276,122.145651577416)) ;
#39834 = CARTESIAN_POINT('Ctrl Pts',(-19.1059608983857,42.8525565835777,122.225998547386)) ;
#39835 = CARTESIAN_POINT('Ctrl Pts',(-19.030133332195,42.6725675031678,121.929544757025)) ;
#39836 = CARTESIAN_POINT('Ctrl Pts',(-19.526741490911,42.8724072381308,122.192939772244)) ;
#39837 = CARTESIAN_POINT('Ctrl Pts',(-19.5561067931741,42.692418157721,121.888220022681)) ;
#39838 = CARTESIAN_POINT('Ctrl Pts',(-19.9374721598721,42.8924591724712,122.307188454904)) ;
#39839 = CARTESIAN_POINT('Ctrl Pts',(-20.0695211678487,42.7124700920614,122.031029897326)) ;
#39840 = CARTESIAN_POINT('Ctrl Pts',(-20.2808472333612,42.9122923600373,122.552162407161)) ;
#39841 = CARTESIAN_POINT('Ctrl Pts',(-20.4987389792861,42.7323032796275,122.337244880604)) ;
#39842 = CARTESIAN_POINT('Ctrl Pts',(-20.5217209474624,42.932221572268,122.90060218186)) ;
#39843 = CARTESIAN_POINT('Ctrl Pts',(-20.7998323715724,42.7522324918582,122.772792578449)) ;
#39844 = CARTESIAN_POINT('Ctrl Pts',(-20.6295592118292,42.9521065374824,123.309594803802)) ;
#39845 = CARTESIAN_POINT('Ctrl Pts',(-20.9346324232029,42.7721174570725,123.284031475308)) ;
#39846 = CARTESIAN_POINT('Ctrl Pts',(-20.5903609500711,42.972180278627,123.734525663825)) ;
#39847 = CARTESIAN_POINT('Ctrl Pts',(-20.8856369562463,42.7921911982171,123.815196128972)) ;
#39848 = CARTESIAN_POINT('Ctrl Pts',(-20.4110322867297,42.9919734604074,124.115338189697)) ;
#39849 = CARTESIAN_POINT('Ctrl Pts',(-20.6614795251778,42.8119843799976,124.29121080534)) ;
#39850 = CARTESIAN_POINT('Ctrl Pts',(-20.1109437575518,43.0119361684101,124.415478901693)) ;
#39851 = CARTESIAN_POINT('Ctrl Pts',(-20.2863715696401,42.8319470880002,124.66638895846)) ;
#39852 = CARTESIAN_POINT('Ctrl Pts',(-19.7255846738428,43.0319191201525,124.594466908089)) ;
#39853 = CARTESIAN_POINT('Ctrl Pts',(-19.8046741907644,42.8519300397427,124.89012675408)) ;
#39854 = CARTESIAN_POINT('Ctrl Pts',(-19.3059710828873,43.0517297399247,124.631722413805)) ;
#39855 = CARTESIAN_POINT('Ctrl Pts',(-19.2801592562406,42.8717406595148,124.936699673611)) ;
#39856 = CARTESIAN_POINT('Ctrl Pts',(-18.8952733972345,43.0717134559576,124.523123476909)) ;
#39857 = CARTESIAN_POINT('Ctrl Pts',(-18.7667862152557,42.8917243755477,124.800954951292)) ;
#39858 = CARTESIAN_POINT('Ctrl Pts',(-18.547948160276,43.0915949198549,124.281962291053)) ;
#39859 = CARTESIAN_POINT('Ctrl Pts',(-18.3326279856104,42.9116058394451,124.499507379854)) ;
#39860 = CARTESIAN_POINT('Ctrl Pts',(-18.3027271825646,43.1115502496993,123.935800002761)) ;
#39861 = CARTESIAN_POINT('Ctrl Pts',(-18.0260984755264,42.9315611692895,124.06680718518)) ;
#39862 = CARTESIAN_POINT('Ctrl Pts',(-18.1904651269619,43.1314257105047,123.528307608364)) ;
#39863 = CARTESIAN_POINT('Ctrl Pts',(-17.8857662259609,42.9514366300949,123.557444062355)) ;
#39864 = CARTESIAN_POINT('Ctrl Pts',(-18.2239197601607,43.1514100305563,123.104753802092)) ;
#39865 = CARTESIAN_POINT('Ctrl Pts',(-17.9275815085421,42.9714209501464,123.027999899629)) ;
#39866 = CARTESIAN_POINT('Ctrl Pts',(-18.3996847638181,43.1713380633459,122.719094804955)) ;
#39867 = CARTESIAN_POINT('Ctrl Pts',(-18.1472767537008,42.9913489829361,122.545930346228)) ;
#39868 = CARTESIAN_POINT('Ctrl Pts',(-18.646890943322,43.1879468252857,122.467036487721)) ;
#39869 = CARTESIAN_POINT('Ctrl Pts',(-18.4563016259039,43.0079577448759,122.230836526312)) ;
#39870 = CARTESIAN_POINT('Ctrl Pts',(-18.8854093868125,43.2011344639758,122.325626761766)) ;
#39871 = CARTESIAN_POINT('Ctrl Pts',(-18.754428778719,43.021145383566,122.054087877061)) ;
#39872 = CARTESIAN_POINT('Ctrl Pts',(-19.0816631258239,43.2111208983359,122.25109404408)) ;
#39873 = CARTESIAN_POINT('Ctrl Pts',(-18.9997521034585,43.0311318179261,121.960916807057)) ;
#39874 = CARTESIAN_POINT('Ctrl Pts',(-19.2884287473412,43.2211302722953,122.211885729769)) ;
#39875 = CARTESIAN_POINT('Ctrl Pts',(-19.2581944108734,43.0411411918854,121.911902702799)) ;
#39876 = CARTESIAN_POINT('Ctrl Pts',(-19.5677559979308,43.2344203058605,122.208091123803)) ;
#39877 = CARTESIAN_POINT('Ctrl Pts',(-19.6074202778516,43.0544312254507,121.907165841885)) ;
#39878 = CARTESIAN_POINT('Ctrl Pts',(-19.9099408495608,43.251014293523,122.294450351363)) ;
#39879 = CARTESIAN_POINT('Ctrl Pts',(-20.035068776761,43.0710252131132,122.015093622718)) ;
#39880 = CARTESIAN_POINT('Ctrl Pts',(-20.2026638187543,43.2676465487985,122.492780810066)) ;
#39881 = CARTESIAN_POINT('Ctrl Pts',(-20.4010277794192,43.0876574683887,122.26302842481)) ;
#39882 = CARTESIAN_POINT('Ctrl Pts',(-20.3849853860425,43.2808889324664,122.703218028358)) ;
#39883 = CARTESIAN_POINT('Ctrl Pts',(-20.6289019817708,43.1008998520566,122.526052209326)) ;
#39884 = CARTESIAN_POINT('Ctrl Pts',(-20.4925880976511,43.2908031406938,122.881725152075)) ;
#39885 = CARTESIAN_POINT('Ctrl Pts',(-20.7634137016277,43.110814060284,122.74918883152)) ;
#39886 = CARTESIAN_POINT('Ctrl Pts',(-20.5684111030146,43.3008597799655,123.079068387712)) ;
#39887 = CARTESIAN_POINT('Ctrl Pts',(-20.8581936478077,43.1208706995557,122.995865179675)) ;
#39888 = CARTESIAN_POINT('Ctrl Pts',(-20.6082199665284,43.3107055863856,123.282209920598)) ;
#39889 = CARTESIAN_POINT('Ctrl Pts',(-20.9079570488716,43.1307165059758,123.249794573019)) ;
#39890 = CARTESIAN_POINT('Ctrl Pts',(-20.6125910585015,43.3207505860188,123.493341268355)) ;
#39891 = CARTESIAN_POINT('Ctrl Pts',(-20.9134264775724,43.140761505609,123.513697714183)) ;
#39892 = CARTESIAN_POINT('Ctrl Pts',(-20.569416287465,43.3340316083915,123.769136883137)) ;
#39893 = CARTESIAN_POINT('Ctrl Pts',(-20.8594473357506,43.1540425279817,123.858497845356)) ;
#39894 = CARTESIAN_POINT('Ctrl Pts',(-20.4566616002104,43.3472290549162,124.026134355986)) ;
#39895 = CARTESIAN_POINT('Ctrl Pts',(-20.7185081963273,43.1672399745064,124.17971260663)) ;
#39896 = CARTESIAN_POINT('Ctrl Pts',(-20.2801208783856,43.3606433527231,124.246084172849)) ;
#39897 = CARTESIAN_POINT('Ctrl Pts',(-20.4978485963145,43.1806542723133,124.454637161289)) ;
#39898 = CARTESIAN_POINT('Ctrl Pts',(-20.1246767207839,43.3704824181259,124.382563644853)) ;
#39899 = CARTESIAN_POINT('Ctrl Pts',(-20.3035425807925,43.1904933377161,124.625241624107)) ;
#39900 = CARTESIAN_POINT('Ctrl Pts',(-19.9456198245211,43.3804656244036,124.492010358693)) ;
#39901 = CARTESIAN_POINT('Ctrl Pts',(-20.0797235876793,43.2004765439937,124.762051652088)) ;
#39902 = CARTESIAN_POINT('Ctrl Pts',(-19.7508481450483,43.3904168593164,124.568404517536)) ;
#39903 = CARTESIAN_POINT('Ctrl Pts',(-19.8362597617157,43.2104277789065,124.857547214576)) ;
#39904 = CARTESIAN_POINT('Ctrl Pts',(-19.5447971219931,43.400417859018,124.610275376094)) ;
#39905 = CARTESIAN_POINT('Ctrl Pts',(-19.5786965198852,43.2204287786082,124.909888505261)) ;
#39906 = CARTESIAN_POINT('Ctrl Pts',(-19.3339717832248,43.4104492048053,124.615418235309)) ;
#39907 = CARTESIAN_POINT('Ctrl Pts',(-19.3151648430012,43.2304601243955,124.916319914213)) ;
#39908 = CARTESIAN_POINT('Ctrl Pts',(-19.1290970717957,43.4203029695104,124.584716305653)) ;
#39909 = CARTESIAN_POINT('Ctrl Pts',(-19.0590709276803,43.2403138891005,124.877945266939)) ;
#39910 = CARTESIAN_POINT('Ctrl Pts',(-18.9302029392523,43.4302736231787,124.518609768227)) ;
#39911 = CARTESIAN_POINT('Ctrl Pts',(-18.8104522662842,43.2502845427688,124.795314724082)) ;
#39912 = CARTESIAN_POINT('Ctrl Pts',(-18.7452726680142,43.4402708668359,124.418674434814)) ;
#39913 = CARTESIAN_POINT('Ctrl Pts',(-18.579288025875,43.2602817864261,124.670397983548)) ;
#39914 = CARTESIAN_POINT('Ctrl Pts',(-18.5801137359114,43.4503043227801,124.28749236113)) ;
#39915 = CARTESIAN_POINT('Ctrl Pts',(-18.3728375783014,43.2703152423702,124.506422572579)) ;
#39916 = CARTESIAN_POINT('Ctrl Pts',(-18.4424457993828,43.4601598270805,124.132620980022)) ;
#39917 = CARTESIAN_POINT('Ctrl Pts',(-18.2007504133427,43.2801707466707,124.312835032827)) ;
#39918 = CARTESIAN_POINT('Ctrl Pts',(-18.3319639426538,43.4701592633666,123.953818397867)) ;
#39919 = CARTESIAN_POINT('Ctrl Pts',(-18.0626456728445,43.2901701829567,124.089333194089)) ;
#39920 = CARTESIAN_POINT('Ctrl Pts',(-18.2547737206712,43.4800537228825,123.760615819088)) ;
#39921 = CARTESIAN_POINT('Ctrl Pts',(-17.9661552349322,43.3000646424727,123.847830754012)) ;
#39922 = CARTESIAN_POINT('Ctrl Pts',(-18.2116553133487,43.4901168423341,123.553535266331)) ;
#39923 = CARTESIAN_POINT('Ctrl Pts',(-17.912254517231,43.3101277619243,123.58898066156)) ;
#39924 = CARTESIAN_POINT('Ctrl Pts',(-18.2050619663453,43.4999564767461,123.346745963906)) ;
#39925 = CARTESIAN_POINT('Ctrl Pts',(-17.9040100748789,43.3199673963363,123.330493713349)) ;
#39926 = CARTESIAN_POINT('Ctrl Pts',(-18.23486765756,43.5100196842319,123.137325469672)) ;
#39927 = CARTESIAN_POINT('Ctrl Pts',(-17.9412644854558,43.3300306038221,123.068717754893)) ;
#39928 = CARTESIAN_POINT('Ctrl Pts',(-18.2996597954055,43.5199137916111,122.939643533093)) ;
#39929 = CARTESIAN_POINT('Ctrl Pts',(-18.0222521550485,43.3399247112013,122.821614169034)) ;
#39930 = CARTESIAN_POINT('Ctrl Pts',(-18.3977518129424,43.5298561238035,122.755103321263)) ;
#39931 = CARTESIAN_POINT('Ctrl Pts',(-18.1448649356919,43.3498670433936,122.590937416145)) ;
#39932 = CARTESIAN_POINT('Ctrl Pts',(-18.5271067731501,43.5398567501185,122.589320233305)) ;
#39933 = CARTESIAN_POINT('Ctrl Pts',(-18.3065565945631,43.3598676697087,122.383706851655)) ;
#39934 = CARTESIAN_POINT('Ctrl Pts',(-18.6841488510847,43.5498984844004,122.448264779539)) ;
#39935 = CARTESIAN_POINT('Ctrl Pts',(-18.5028573530052,43.3699094039905,122.207385535519)) ;
#39936 = CARTESIAN_POINT('Ctrl Pts',(-18.8592239504986,43.5597239103495,122.33861707734)) ;
#39937 = CARTESIAN_POINT('Ctrl Pts',(-18.7217003533582,43.3797348299397,122.070323331538)) ;
#39938 = CARTESIAN_POINT('Ctrl Pts',(-19.0550398152044,43.5697807368771,122.258927424476)) ;
#39939 = CARTESIAN_POINT('Ctrl Pts',(-18.9664691272674,43.3897916564673,121.9707088847)) ;
#39940 = CARTESIAN_POINT('Ctrl Pts',(-19.2591461901148,43.5797081699987,122.215302018421)) ;
#39941 = CARTESIAN_POINT('Ctrl Pts',(-19.221601860933,43.3997190895889,121.916174469937)) ;
#39942 = CARTESIAN_POINT('Ctrl Pts',(-19.4681756382475,43.5896581624049,122.207163663793)) ;
#39943 = CARTESIAN_POINT('Ctrl Pts',(-19.482888856262,43.4096690819951,121.905998966788)) ;
#39944 = CARTESIAN_POINT('Ctrl Pts',(-19.6775616742312,43.5997133634789,122.236109466576)) ;
#39945 = CARTESIAN_POINT('Ctrl Pts',(-19.7446216548222,43.4197242830691,121.94217861372)) ;
#39946 = CARTESIAN_POINT('Ctrl Pts',(-19.874223881596,43.6095356375312,122.299123887037)) ;
#39947 = CARTESIAN_POINT('Ctrl Pts',(-19.990450932251,43.4295465571214,122.020944452107)) ;
#39948 = CARTESIAN_POINT('Ctrl Pts',(-20.0614519230175,43.6195915314905,122.397267586826)) ;
#39949 = CARTESIAN_POINT('Ctrl Pts',(-20.2244870381209,43.4396024510806,122.1436218314)) ;
#39950 = CARTESIAN_POINT('Ctrl Pts',(-20.2266685259505,43.6295322533356,122.525258130833)) ;
#39951 = CARTESIAN_POINT('Ctrl Pts',(-20.4310096168691,43.4495431729258,122.303608199014)) ;
#39952 = CARTESIAN_POINT('Ctrl Pts',(-20.3671176125788,43.6394365974222,122.678983059671)) ;
#39953 = CARTESIAN_POINT('Ctrl Pts',(-20.6065731184641,43.4594475170124,122.495763120435)) ;
#39954 = CARTESIAN_POINT('Ctrl Pts',(-20.4802208408433,43.6494832647217,122.857339300403)) ;
#39955 = CARTESIAN_POINT('Ctrl Pts',(-20.7479541653206,43.4694941843119,122.718707024685)) ;
#39956 = CARTESIAN_POINT('Ctrl Pts',(-20.5596229425746,43.6593788231716,123.049662217343)) ;
#39957 = CARTESIAN_POINT('Ctrl Pts',(-20.8472092356636,43.4793897427618,122.959110289746)) ;
#39958 = CARTESIAN_POINT('Ctrl Pts',(-20.6051653987093,43.6694409018763,123.256207404328)) ;
#39959 = CARTESIAN_POINT('Ctrl Pts',(-20.904139618106,43.4894518214665,123.217291078414)) ;
#39960 = CARTESIAN_POINT('Ctrl Pts',(-20.614077706757,43.6792836003421,123.462962817774)) ;
#39961 = CARTESIAN_POINT('Ctrl Pts',(-20.9152824167308,43.4992945199322,123.475736104281)) ;
#39962 = CARTESIAN_POINT('Ctrl Pts',(-20.587046897207,43.6892743742365,123.671227339976)) ;
#39963 = CARTESIAN_POINT('Ctrl Pts',(-20.8814961281011,43.5092852938267,123.736067222358)) ;
#39964 = CARTESIAN_POINT('Ctrl Pts',(-20.5246153399661,43.6992022434715,123.870395640026)) ;
#39965 = CARTESIAN_POINT('Ctrl Pts',(-20.8034587033773,43.5192131630616,123.985028739418)) ;
#39966 = CARTESIAN_POINT('Ctrl Pts',(-20.4282901507528,43.7091909724413,124.0570066794)) ;
#39967 = CARTESIAN_POINT('Ctrl Pts',(-20.6830540647479,43.5292018920315,124.218293703529)) ;
#39968 = CARTESIAN_POINT('Ctrl Pts',(-20.300083088921,43.7192303744251,124.224651641945)) ;
#39969 = CARTESIAN_POINT('Ctrl Pts',(-20.5227971111526,43.5392412940152,124.427851205547)) ;
#39970 = CARTESIAN_POINT('Ctrl Pts',(-20.1480587442798,43.7290705421618,124.364969335422)) ;
#39971 = CARTESIAN_POINT('Ctrl Pts',(-20.3327674227831,43.549081461752,124.603250592151)) ;
#39972 = CARTESIAN_POINT('Ctrl Pts',(-19.9704841404498,43.7391187525363,124.479372090359)) ;
#39973 = CARTESIAN_POINT('Ctrl Pts',(-20.1108004287788,43.5591296721265,124.746255706774)) ;
#39974 = CARTESIAN_POINT('Ctrl Pts',(-19.7775615457972,43.7490659228241,124.560080673461)) ;
#39975 = CARTESIAN_POINT('Ctrl Pts',(-19.8696476489061,43.5690768424143,124.847143607125)) ;
#39976 = CARTESIAN_POINT('Ctrl Pts',(-19.5744358323149,43.7589767710792,124.606507407475)) ;
#39977 = CARTESIAN_POINT('Ctrl Pts',(-19.6157403076498,43.5789876906694,124.905179129391)) ;
#39978 = CARTESIAN_POINT('Ctrl Pts',(-19.3632888752703,43.7690330987569,124.616913341482)) ;
#39979 = CARTESIAN_POINT('Ctrl Pts',(-19.3518069355722,43.5890440183471,124.918188595458)) ;
#39980 = CARTESIAN_POINT('Ctrl Pts',(-19.1577934192907,43.7788835115255,124.591215482131)) ;
#39981 = CARTESIAN_POINT('Ctrl Pts',(-19.0949363387269,43.5988944311156,124.886068138091)) ;
#39982 = CARTESIAN_POINT('Ctrl Pts',(-18.9561968908211,43.7889103973592,124.529628376844)) ;
#39983 = CARTESIAN_POINT('Ctrl Pts',(-18.8429401698884,43.6089213169493,124.809086046487)) ;
#39984 = CARTESIAN_POINT('Ctrl Pts',(-18.7685615510423,43.79893901299,124.433463237905)) ;
#39985 = CARTESIAN_POINT('Ctrl Pts',(-18.6083951336162,43.6189499325802,124.688881455455)) ;
#39986 = CARTESIAN_POINT('Ctrl Pts',(-18.6033288718835,43.8087842363675,124.30883132978)) ;
#39987 = CARTESIAN_POINT('Ctrl Pts',(-18.4018522456161,43.6287951559577,124.533092420039)) ;
#39988 = CARTESIAN_POINT('Ctrl Pts',(-18.4597378892454,43.8187749184691,124.155537858628)) ;
#39989 = CARTESIAN_POINT('Ctrl Pts',(-18.222362119769,43.6387858380593,124.341476622119)) ;
#39990 = CARTESIAN_POINT('Ctrl Pts',(-18.3448008532577,43.8288128071015,123.978559187435)) ;
#39991 = CARTESIAN_POINT('Ctrl Pts',(-18.0786893212489,43.6488237266917,124.120254417856)) ;
#39992 = CARTESIAN_POINT('Ctrl Pts',(-18.2635921715876,43.8386571422047,123.78819018194)) ;
#39993 = CARTESIAN_POINT('Ctrl Pts',(-17.9771763876503,43.6586680617949,123.882292776762)) ;
#39994 = CARTESIAN_POINT('Ctrl Pts',(-18.2156072803135,43.8486421044022,123.583862375105)) ;
#39995 = CARTESIAN_POINT('Ctrl Pts',(-17.9171936283301,43.6686530239924,123.626883148395)) ;
#39996 = CARTESIAN_POINT('Ctrl Pts',(-18.2037829776996,43.8585810459356,123.375218987753)) ;
#39997 = CARTESIAN_POINT('Ctrl Pts',(-17.9024116243898,43.6785919655257,123.366078461574)) ;
#39998 = CARTESIAN_POINT('Ctrl Pts',(-18.2286806326614,43.868622930907,123.165600430253)) ;
#39999 = CARTESIAN_POINT('Ctrl Pts',(-17.9335320665927,43.6886338504972,123.104055220475)) ;
#40000 = CARTESIAN_POINT('Ctrl Pts',(-18.2885381500914,43.8785094788153,122.96653880576)) ;
#40001 = CARTESIAN_POINT('Ctrl Pts',(-18.008352723636,43.6985203984054,122.855226846707)) ;
#40002 = CARTESIAN_POINT('Ctrl Pts',(-18.3827677761836,43.8885034043153,122.778780845212)) ;
#40003 = CARTESIAN_POINT('Ctrl Pts',(-18.1261385187885,43.7085143239054,122.62052857553)) ;
#40004 = CARTESIAN_POINT('Ctrl Pts',(-18.507397260208,43.8984394954417,122.611106118602)) ;
#40005 = CARTESIAN_POINT('Ctrl Pts',(-18.2819245676368,43.7184504150319,122.410933845999)) ;
#40006 = CARTESIAN_POINT('Ctrl Pts',(-18.6606561201383,43.9084687644217,122.466343302757)) ;
#40007 = CARTESIAN_POINT('Ctrl Pts',(-18.4734970875325,43.7284796840119,122.229979319917)) ;
#40008 = CARTESIAN_POINT('Ctrl Pts',(-18.8340470507955,43.918351146981,122.351835718989)) ;
#40009 = CARTESIAN_POINT('Ctrl Pts',(-18.690235843168,43.7383620665712,122.08684314791)) ;
#40010 = CARTESIAN_POINT('Ctrl Pts',(-19.0278824329128,43.9284036640689,122.267711760247)) ;
#40011 = CARTESIAN_POINT('Ctrl Pts',(-18.9325293092755,43.748414583659,121.981687073704)) ;
#40012 = CARTESIAN_POINT('Ctrl Pts',(-19.2301849856646,43.9382977848928,122.219177390576)) ;
#40013 = CARTESIAN_POINT('Ctrl Pts',(-19.1854080916238,43.7583087044829,121.92101763461)) ;
#40014 = CARTESIAN_POINT('Ctrl Pts',(-19.441298301709,43.9483597643132,122.206244667768)) ;
#40015 = CARTESIAN_POINT('Ctrl Pts',(-19.4492993318435,43.7683706839034,121.904850471497)) ;
#40016 = CARTESIAN_POINT('Ctrl Pts',(-19.6469435683342,43.9582042975421,122.229626514128)) ;
#40017 = CARTESIAN_POINT('Ctrl Pts',(-19.7063573702786,43.7782152171323,121.934076662978)) ;
#40018 = CARTESIAN_POINT('Ctrl Pts',(-19.8479372841435,43.9681643764484,122.288322728641)) ;
#40019 = CARTESIAN_POINT('Ctrl Pts',(-19.9576002327709,43.7881752960385,122.007446102403)) ;
#40020 = CARTESIAN_POINT('Ctrl Pts',(-20.0369708079469,43.978202653021,122.38212312448)) ;
#40021 = CARTESIAN_POINT('Ctrl Pts',(-20.1938925037077,43.7982135726111,122.124695495062)) ;
#40022 = CARTESIAN_POINT('Ctrl Pts',(-20.2043238205213,43.9880760395588,122.504967849574)) ;
#40023 = CARTESIAN_POINT('Ctrl Pts',(-20.4030852669938,43.808086959149,122.27825126005)) ;
#40024 = CARTESIAN_POINT('Ctrl Pts',(-20.3506106823668,43.9981489823259,122.658028324524)) ;
#40025 = CARTESIAN_POINT('Ctrl Pts',(-20.5859442922176,43.8181599019161,122.469575837345)) ;
#40026 = CARTESIAN_POINT('Ctrl Pts',(-20.465419038605,44.0079703964542,122.82969122843)) ;
#40027 = CARTESIAN_POINT('Ctrl Pts',(-20.7294563689263,43.8279813160444,122.684155238278)) ;
#40028 = CARTESIAN_POINT('Ctrl Pts',(-20.5510249351871,44.0180450265265,123.023378752783)) ;
#40029 = CARTESIAN_POINT('Ctrl Pts',(-20.836464323358,43.8380559461167,122.926263897457)) ;
#40030 = CARTESIAN_POINT('Ctrl Pts',(-20.6005844279953,44.0279116638434,123.224825343159)) ;
#40031 = CARTESIAN_POINT('Ctrl Pts',(-20.8984148213761,43.8479225834336,123.178073112057)) ;
#40032 = CARTESIAN_POINT('Ctrl Pts',(-20.6151706977744,44.0379352092152,123.435036739168)) ;
#40033 = CARTESIAN_POINT('Ctrl Pts',(-20.9166483133652,43.8579461288053,123.440837266539)) ;
#40034 = CARTESIAN_POINT('Ctrl Pts',(-20.5925229977775,44.0479609607324,123.644602262895)) ;
#40035 = CARTESIAN_POINT('Ctrl Pts',(-20.8883395524588,43.8679718803225,123.702794177779)) ;
#40036 = CARTESIAN_POINT('Ctrl Pts',(-20.5351790535078,44.0578145477417,123.843648615532)) ;
#40037 = CARTESIAN_POINT('Ctrl Pts',(-20.8166599480238,43.8778254673319,123.951603594753)) ;
#40038 = CARTESIAN_POINT('Ctrl Pts',(-20.4434995838773,44.0677915079697,124.032303037785)) ;
#40039 = CARTESIAN_POINT('Ctrl Pts',(-20.7020609237205,43.8878024275598,124.187422142882)) ;
#40040 = CARTESIAN_POINT('Ctrl Pts',(-20.3196315257472,44.0778126509981,124.202704231129)) ;
#40041 = CARTESIAN_POINT('Ctrl Pts',(-20.5472263848323,43.8978235705883,124.400424003593)) ;
#40042 = CARTESIAN_POINT('Ctrl Pts',(-20.1704166426939,44.0876952570181,124.347313905858)) ;
#40043 = CARTESIAN_POINT('Ctrl Pts',(-20.3607073266123,43.9077061766083,124.581187205832)) ;
#40044 = CARTESIAN_POINT('Ctrl Pts',(-19.9951290913081,44.0977637276508,124.465904961827)) ;
#40045 = CARTESIAN_POINT('Ctrl Pts',(-20.1415985165623,43.9177746472409,124.729426223208)) ;
#40046 = CARTESIAN_POINT('Ctrl Pts',(-19.8065219734023,44.1075938108345,124.550461991308)) ;
#40047 = CARTESIAN_POINT('Ctrl Pts',(-19.9058383855196,43.9276047304247,124.835123522577)) ;
#40048 = CARTESIAN_POINT('Ctrl Pts',(-19.6014110884651,44.1176603705148,124.602451546472)) ;
#40049 = CARTESIAN_POINT('Ctrl Pts',(-19.6494502413874,43.937671290105,124.900110672146)) ;
#40050 = CARTESIAN_POINT('Ctrl Pts',(-19.3940171097119,44.1275506203441,124.617639758843)) ;
#40051 = CARTESIAN_POINT('Ctrl Pts',(-19.3902067493434,43.9475615399342,124.919096378377)) ;
#40052 = CARTESIAN_POINT('Ctrl Pts',(-19.1849952546928,44.1375427860929,124.596831802444)) ;
#40053 = CARTESIAN_POINT('Ctrl Pts',(-19.1289291993342,43.957553705683,124.893086594039)) ;
#40054 = CARTESIAN_POINT('Ctrl Pts',(-18.9834025895948,44.147505629689,124.540019916616)) ;
#40055 = CARTESIAN_POINT('Ctrl Pts',(-18.8769378575114,43.9675165492791,124.822071867024)) ;
#40056 = CARTESIAN_POINT('Ctrl Pts',(-18.7955966982782,44.1574097985167,124.450071701931)) ;
#40057 = CARTESIAN_POINT('Ctrl Pts',(-18.6421796236428,43.9774207181069,124.709636239005)) ;
#40058 = CARTESIAN_POINT('Ctrl Pts',(-18.6237306354897,44.1674706734111,124.326834768521)) ;
#40059 = CARTESIAN_POINT('Ctrl Pts',(-18.427347259584,43.9874815930013,124.555590382831)) ;
#40060 = CARTESIAN_POINT('Ctrl Pts',(-18.4788866563946,44.1773095767404,124.179124043168)) ;
#40061 = CARTESIAN_POINT('Ctrl Pts',(-18.246291241733,43.9973204963306,124.370950929474)) ;
#40062 = CARTESIAN_POINT('Ctrl Pts',(-18.3590318669185,44.1873779531143,124.004699120229)) ;
#40063 = CARTESIAN_POINT('Ctrl Pts',(-18.0964730403445,44.0073888727045,124.152920066844)) ;
#40064 = CARTESIAN_POINT('Ctrl Pts',(-18.2729573990922,44.197258569747,123.815617005926)) ;
#40065 = CARTESIAN_POINT('Ctrl Pts',(-17.9888795242081,44.0172694893372,123.916566377158)) ;
#40066 = CARTESIAN_POINT('Ctrl Pts',(-18.2200454094595,44.207249729976,123.612376766819)) ;
#40067 = CARTESIAN_POINT('Ctrl Pts',(-17.9227396808908,44.0272606495662,123.662515814655)) ;
#40068 = CARTESIAN_POINT('Ctrl Pts',(-18.2032518304312,44.2172028034081,123.403775478978)) ;
#40069 = CARTESIAN_POINT('Ctrl Pts',(-17.901747886527,44.0372137229982,123.40176367561)) ;
#40070 = CARTESIAN_POINT('Ctrl Pts',(-18.2231612060629,44.2272386390207,123.19374932302)) ;
#40071 = CARTESIAN_POINT('Ctrl Pts',(-17.9266347799098,44.0472495586109,123.139231148723)) ;
#40072 = CARTESIAN_POINT('Ctrl Pts',(-18.2782926365655,44.2371287657509,122.993256824972)) ;
#40073 = CARTESIAN_POINT('Ctrl Pts',(-17.9955495885847,44.0571396853411,122.888614558042)) ;
#40074 = CARTESIAN_POINT('Ctrl Pts',(-18.368002893643,44.2471209475202,122.803320931818)) ;
#40075 = CARTESIAN_POINT('Ctrl Pts',(-18.1076878439649,44.0671318671104,122.651194666608)) ;
#40076 = CARTESIAN_POINT('Ctrl Pts',(-18.4888319440295,44.2570668874946,122.632672480447)) ;
#40077 = CARTESIAN_POINT('Ctrl Pts',(-18.2587247866169,44.0770778070848,122.437883820096)) ;
#40078 = CARTESIAN_POINT('Ctrl Pts',(-18.6371833756394,44.2670140712541,122.485268515715)) ;
#40079 = CARTESIAN_POINT('Ctrl Pts',(-18.4441648499468,44.0870249908443,122.253628827134)) ;
#40080 = CARTESIAN_POINT('Ctrl Pts',(-18.810735082372,44.2770620095444,122.364857154366)) ;
#40081 = CARTESIAN_POINT('Ctrl Pts',(-18.6611045195104,44.0970729291346,122.1031151175)) ;
#40082 = CARTESIAN_POINT('Ctrl Pts',(-18.9986676053786,44.286909644358,122.278010090229)) ;
#40083 = CARTESIAN_POINT('Ctrl Pts',(-18.8960216519276,44.1069205639482,121.994556148526)) ;
#40084 = CARTESIAN_POINT('Ctrl Pts',(-19.2009643648431,44.296871358056,122.223868979964)) ;
#40085 = CARTESIAN_POINT('Ctrl Pts',(-19.1488932353509,44.1168822776461,121.92688036903)) ;
#40086 = CARTESIAN_POINT('Ctrl Pts',(-19.4110368321455,44.3068999938771,122.205817721847)) ;
#40087 = CARTESIAN_POINT('Ctrl Pts',(-19.4114837782063,44.1269109134673,121.90431694798)) ;
#40088 = CARTESIAN_POINT('Ctrl Pts',(-19.6185576126464,44.3168103086289,122.224226084689)) ;
#40089 = CARTESIAN_POINT('Ctrl Pts',(-19.6708855677845,44.1368212282191,121.927328148296)) ;
#40090 = CARTESIAN_POINT('Ctrl Pts',(-19.8203871123028,44.3267451792916,122.277995841482)) ;
#40091 = CARTESIAN_POINT('Ctrl Pts',(-19.9231728540548,44.1467560988817,121.994541369451)) ;
#40092 = CARTESIAN_POINT('Ctrl Pts',(-20.0117417687553,44.3367863616933,122.367111250582)) ;
#40093 = CARTESIAN_POINT('Ctrl Pts',(-20.1623656623035,44.1567972812835,122.105936279565)) ;
#40094 = CARTESIAN_POINT('Ctrl Pts',(-20.182178194294,44.3466733331581,122.48611803753)) ;
#40095 = CARTESIAN_POINT('Ctrl Pts',(-20.3754115588307,44.1666842527482,122.254696080768)) ;
#40096 = CARTESIAN_POINT('Ctrl Pts',(-20.3311931711049,44.3566727654207,122.634359060664)) ;
#40097 = CARTESIAN_POINT('Ctrl Pts',(-20.5616797006855,44.1766836850109,122.439998156189)) ;
#40098 = CARTESIAN_POINT('Ctrl Pts',(-20.4513895888392,44.3665928306773,122.804819406772)) ;
#40099 = CARTESIAN_POINT('Ctrl Pts',(-20.7119248210621,44.1866037502675,122.653074789984)) ;
#40100 = CARTESIAN_POINT('Ctrl Pts',(-20.5412304164301,44.3766296832615,122.995731464311)) ;
#40101 = CARTESIAN_POINT('Ctrl Pts',(-20.8242248480823,44.1966406028516,122.891715161763)) ;
#40102 = CARTESIAN_POINT('Ctrl Pts',(-20.5958716500195,44.3865423426014,123.196839523156)) ;
#40103 = CARTESIAN_POINT('Ctrl Pts',(-20.8925256089118,44.2065532621916,123.143101297564)) ;
#40104 = CARTESIAN_POINT('Ctrl Pts',(-20.6153694128764,44.3965335545164,123.405991946571)) ;
#40105 = CARTESIAN_POINT('Ctrl Pts',(-20.9168966358172,44.2165444741065,123.404542148438)) ;
#40106 = CARTESIAN_POINT('Ctrl Pts',(-20.5976979683511,44.4065751959195,123.616341273831)) ;
#40107 = CARTESIAN_POINT('Ctrl Pts',(-20.8948063198031,44.2265861155096,123.667478543091)) ;
#40108 = CARTESIAN_POINT('Ctrl Pts',(-20.54540602134,44.4164039901265,123.816275966712)) ;
#40109 = CARTESIAN_POINT('Ctrl Pts',(-20.8294398408102,44.2364149097167,123.917397996008)) ;
#40110 = CARTESIAN_POINT('Ctrl Pts',(-20.4571322193429,44.4264804012478,124.008799381337)) ;
#40111 = CARTESIAN_POINT('Ctrl Pts',(-20.7190966285522,44.2464913208379,124.158051348359)) ;
#40112 = CARTESIAN_POINT('Ctrl Pts',(-20.3394898621036,44.4363325342902,124.179323371872)) ;
#40113 = CARTESIAN_POINT('Ctrl Pts',(-20.5720419187285,44.2563434538804,124.371206621311)) ;
#40114 = CARTESIAN_POINT('Ctrl Pts',(-20.1909447204641,44.4464057686315,124.330210550994)) ;
#40115 = CARTESIAN_POINT('Ctrl Pts',(-20.3863598083337,44.2664166882217,124.559814357992)) ;
#40116 = CARTESIAN_POINT('Ctrl Pts',(-20.0223534222565,44.4562472699582,124.450168274092)) ;
#40117 = CARTESIAN_POINT('Ctrl Pts',(-20.1756188493181,44.2762581895484,124.709761183262)) ;
#40118 = CARTESIAN_POINT('Ctrl Pts',(-19.8335848822427,44.466208221553,124.540812132209)) ;
#40119 = CARTESIAN_POINT('Ctrl Pts',(-19.9396571120526,44.2862191411431,124.823064731711)) ;
#40120 = CARTESIAN_POINT('Ctrl Pts',(-19.6302748014164,44.4762460392736,124.597332076024)) ;
#40121 = CARTESIAN_POINT('Ctrl Pts',(-19.6855192485498,44.2962569588638,124.893713217943)) ;
#40122 = CARTESIAN_POINT('Ctrl Pts',(-19.4236658402343,44.4861203885307,124.617747552604)) ;
#40123 = CARTESIAN_POINT('Ctrl Pts',(-19.4272568805924,44.3061313081208,124.919231077628)) ;
#40124 = CARTESIAN_POINT('Ctrl Pts',(-19.2126136916866,44.4961899392729,124.601657803566)) ;
#40125 = CARTESIAN_POINT('Ctrl Pts',(-19.163442166299,44.316200858863,124.899117334213)) ;
#40126 = CARTESIAN_POINT('Ctrl Pts',(-19.0122816584332,44.5060239587815,124.550498030164)) ;
#40127 = CARTESIAN_POINT('Ctrl Pts',(-18.9130262792638,44.3260348783717,124.835165719993)) ;
#40128 = CARTESIAN_POINT('Ctrl Pts',(-18.8198408604291,44.516058113361,124.464118183293)) ;
#40129 = CARTESIAN_POINT('Ctrl Pts',(-18.6724761255708,44.3360690329512,124.727189304503)) ;
#40130 = CARTESIAN_POINT('Ctrl Pts',(-18.6459125382961,44.5260740391835,124.345407050209)) ;
#40131 = CARTESIAN_POINT('Ctrl Pts',(-18.4550666358209,44.3460849587737,124.578799029754)) ;
#40132 = CARTESIAN_POINT('Ctrl Pts',(-18.4969953236926,44.5359562943777,124.200536328678)) ;
#40133 = CARTESIAN_POINT('Ctrl Pts',(-18.2689206933838,44.3559672139679,124.397708730876)) ;
#40134 = CARTESIAN_POINT('Ctrl Pts',(-18.3739888329453,44.5459451008887,124.030365635577)) ;
#40135 = CARTESIAN_POINT('Ctrl Pts',(-18.1151639541636,44.3659560204788,124.184994122612)) ;
#40136 = CARTESIAN_POINT('Ctrl Pts',(-18.2825994603111,44.5558936681514,123.842202089097)) ;
#40137 = CARTESIAN_POINT('Ctrl Pts',(-18.0009287363938,44.3759045877415,123.949788453005)) ;
#40138 = CARTESIAN_POINT('Ctrl Pts',(-18.2248894304791,44.5659484734534,123.638872201841)) ;
#40139 = CARTESIAN_POINT('Ctrl Pts',(-17.9287930123435,44.3859593930436,123.695625807399)) ;
#40140 = CARTESIAN_POINT('Ctrl Pts',(-18.2035656681982,44.575767256717,123.433544830677)) ;
#40141 = CARTESIAN_POINT('Ctrl Pts',(-17.9021400803731,44.3957781763071,123.438965134923)) ;
#40142 = CARTESIAN_POINT('Ctrl Pts',(-18.2179757066852,44.5858030290775,123.223058832807)) ;
#40143 = CARTESIAN_POINT('Ctrl Pts',(-17.9201546964338,44.4058139486677,123.175857889866)) ;
#40144 = CARTESIAN_POINT('Ctrl Pts',(-18.2692459499617,44.5958277281062,123.018631696878)) ;
#40145 = CARTESIAN_POINT('Ctrl Pts',(-17.9842443391472,44.4158386476964,122.920324456144)) ;
#40146 = CARTESIAN_POINT('Ctrl Pts',(-18.3533314311282,44.6056797313652,122.829344467355)) ;
#40147 = CARTESIAN_POINT('Ctrl Pts',(-18.0893534626568,44.4256906509554,122.683715321266)) ;
#40148 = CARTESIAN_POINT('Ctrl Pts',(-18.4703557315628,44.6156706657625,122.65495463514)) ;
#40149 = CARTESIAN_POINT('Ctrl Pts',(-18.2356357012521,44.4356815853526,122.465729074821)) ;
#40150 = CARTESIAN_POINT('Ctrl Pts',(-18.6147549951052,44.6255885881936,122.504508089155)) ;
#40151 = CARTESIAN_POINT('Ctrl Pts',(-18.4161367370382,44.4455995077838,122.27767197509)) ;
#40152 = CARTESIAN_POINT('Ctrl Pts',(-18.7848954850902,44.6356169438759,122.380036959605)) ;
#40153 = CARTESIAN_POINT('Ctrl Pts',(-18.6288136046969,44.4556278634661,122.122084840431)) ;
#40154 = CARTESIAN_POINT('Ctrl Pts',(-18.9713236852492,44.6455012283865,122.288233366533)) ;
#40155 = CARTESIAN_POINT('Ctrl Pts',(-18.8618504935947,44.4655121479767,122.00733199544)) ;
#40156 = CARTESIAN_POINT('Ctrl Pts',(-19.1729084480282,44.6554939122944,122.229103541019)) ;
#40157 = CARTESIAN_POINT('Ctrl Pts',(-19.1138322342579,44.4755048318845,121.93342190107)) ;
#40158 = CARTESIAN_POINT('Ctrl Pts',(-19.382493485015,44.6655226493021,122.206156839358)) ;
#40159 = CARTESIAN_POINT('Ctrl Pts',(-19.3758137501486,44.4855335688923,121.904740742788)) ;
#40160 = CARTESIAN_POINT('Ctrl Pts',(-19.5898954585969,44.675408045931,122.219478540037)) ;
#40161 = CARTESIAN_POINT('Ctrl Pts',(-19.635066763445,44.4954189655212,121.921395205992)) ;
#40162 = CARTESIAN_POINT('Ctrl Pts',(-19.793970597842,44.6853959313449,122.268821405339)) ;
#40163 = CARTESIAN_POINT('Ctrl Pts',(-19.8901602888194,44.505406850935,121.983076126972)) ;
#40164 = CARTESIAN_POINT('Ctrl Pts',(-19.9857471745296,44.6953466340055,122.352468749605)) ;
#40165 = CARTESIAN_POINT('Ctrl Pts',(-20.1298803582972,44.5153575535956,122.08763762812)) ;
#40166 = CARTESIAN_POINT('Ctrl Pts',(-20.1615504334524,44.7053869521029,122.469253001426)) ;
#40167 = CARTESIAN_POINT('Ctrl Pts',(-20.3496330624208,44.525397871693,122.233619868596)) ;
#40168 = CARTESIAN_POINT('Ctrl Pts',(-20.3120561281735,44.7152615174361,122.612267502799)) ;
#40169 = CARTESIAN_POINT('Ctrl Pts',(-20.5377640234827,44.5352724370263,122.412390214777)) ;
#40170 = CARTESIAN_POINT('Ctrl Pts',(-20.4371874370457,44.7252611774972,122.78115208881)) ;
#40171 = CARTESIAN_POINT('Ctrl Pts',(-20.6941762400881,44.5452720970874,122.623497503529)) ;
#40172 = CARTESIAN_POINT('Ctrl Pts',(-20.5304535414409,44.7351701726649,122.967466993672)) ;
#40173 = CARTESIAN_POINT('Ctrl Pts',(-20.8107568463989,44.5551810922551,122.856392682667)) ;
#40174 = CARTESIAN_POINT('Ctrl Pts',(-20.5907433449701,44.7452249138281,123.170033529265)) ;
#40175 = CARTESIAN_POINT('Ctrl Pts',(-20.8861166780626,44.5652358334183,123.109601455846)) ;
#40176 = CARTESIAN_POINT('Ctrl Pts',(-20.6147190095158,44.7550835257419,123.375937676543)) ;
#40177 = CARTESIAN_POINT('Ctrl Pts',(-20.9160838152845,44.5750944453321,123.366982582958)) ;
#40178 = CARTESIAN_POINT('Ctrl Pts',(-20.60245263379,44.7651516480213,123.587214744072)) ;
#40179 = CARTESIAN_POINT('Ctrl Pts',(-20.9007482952773,44.5851625676115,123.631078613725)) ;
#40180 = CARTESIAN_POINT('Ctrl Pts',(-20.5546908139825,44.7750071187245,123.788845425538)) ;
#40181 = CARTESIAN_POINT('Ctrl Pts',(-20.8410433869933,44.5950180383147,123.883116988004)) ;
#40182 = CARTESIAN_POINT('Ctrl Pts',(-20.4720727117349,44.7850019782178,123.9820375159)) ;
#40183 = CARTESIAN_POINT('Ctrl Pts',(-20.7377682696153,44.605012897808,124.124606144485)) ;
#40184 = CARTESIAN_POINT('Ctrl Pts',(-20.3563607572283,44.7950332315598,124.158351468293)) ;
#40185 = CARTESIAN_POINT('Ctrl Pts',(-20.593126161349,44.61504415115,124.34499716475)) ;
#40186 = CARTESIAN_POINT('Ctrl Pts',(-20.2144020973158,44.8048999304329,124.309603441992)) ;
#40187 = CARTESIAN_POINT('Ctrl Pts',(-20.4156755542351,44.624910850023,124.534060702325)) ;
#40188 = CARTESIAN_POINT('Ctrl Pts',(-20.0465467747764,44.8148867461841,124.435681086058)) ;
#40189 = CARTESIAN_POINT('Ctrl Pts',(-20.2058546847312,44.6348976657742,124.691655677505)) ;
#40190 = CARTESIAN_POINT('Ctrl Pts',(-19.8600899400834,44.8248339513795,124.530430266587)) ;
#40191 = CARTESIAN_POINT('Ctrl Pts',(-19.9727822075315,44.6448448709697,124.810089850154)) ;
#40192 = CARTESIAN_POINT('Ctrl Pts',(-19.6581014765466,44.8348769395058,124.591850093754)) ;
#40193 = CARTESIAN_POINT('Ctrl Pts',(-19.7202958616574,44.654887859096,124.886862052419)) ;
#40194 = CARTESIAN_POINT('Ctrl Pts',(-19.4521749099809,44.8447442941273,124.616945312236)) ;
#40195 = CARTESIAN_POINT('Ctrl Pts',(-19.4628869098963,44.6647552137175,124.918228439738)) ;
#40196 = CARTESIAN_POINT('Ctrl Pts',(-19.242936933169,44.8547101874254,124.606358445387)) ;
#40197 = CARTESIAN_POINT('Ctrl Pts',(-19.2013394365001,44.6747211070155,124.904992081286)) ;
#40198 = CARTESIAN_POINT('Ctrl Pts',(-19.0375566117157,44.8647339648015,124.559112347747)) ;
#40199 = CARTESIAN_POINT('Ctrl Pts',(-18.9446146116766,44.6847448843916,124.845931776664)) ;
#40200 = CARTESIAN_POINT('Ctrl Pts',(-18.8454040569223,44.8746595127332,124.477781348015)) ;
#40201 = CARTESIAN_POINT('Ctrl Pts',(-18.7044247703593,44.6946704323233,124.744265398485)) ;
#40202 = CARTESIAN_POINT('Ctrl Pts',(-18.6697413624025,44.8845999891542,124.364553604711)) ;
#40203 = CARTESIAN_POINT('Ctrl Pts',(-18.4848477731796,44.7046109087444,124.602728280035)) ;
#40204 = CARTESIAN_POINT('Ctrl Pts',(-18.5149584063942,44.8946461988171,124.220874734381)) ;
#40205 = CARTESIAN_POINT('Ctrl Pts',(-18.2913709520565,44.7146571184072,124.423127645195)) ;
#40206 = CARTESIAN_POINT('Ctrl Pts',(-18.3896255165691,44.9045074554789,124.055712470621)) ;
#40207 = CARTESIAN_POINT('Ctrl Pts',(-18.1347068985663,44.7245183750691,124.216672914179)) ;
#40208 = CARTESIAN_POINT('Ctrl Pts',(-18.2933036607311,44.9145010837542,123.869030082729)) ;
#40209 = CARTESIAN_POINT('Ctrl Pts',(-18.014307045051,44.7345120033443,123.983318570119)) ;
#40210 = CARTESIAN_POINT('Ctrl Pts',(-18.2311629194592,44.9244264810644,123.669801758037)) ;
#40211 = CARTESIAN_POINT('Ctrl Pts',(-17.9366337629122,44.7444374006545,123.734282199361)) ;
#40212 = CARTESIAN_POINT('Ctrl Pts',(-18.2042856489682,44.9344543889746,123.46073131352)) ;
#40213 = CARTESIAN_POINT('Ctrl Pts',(-17.9030399616873,44.7544653085648,123.472943722702)) ;
#40214 = CARTESIAN_POINT('Ctrl Pts',(-18.2137679240456,44.9443407046438,123.253075539075)) ;
#40215 = CARTESIAN_POINT('Ctrl Pts',(-17.9148956262802,44.764351624234,123.213374011932)) ;
#40216 = CARTESIAN_POINT('Ctrl Pts',(-18.2597049737886,44.9543722995476,123.047278072271)) ;
#40217 = CARTESIAN_POINT('Ctrl Pts',(-17.9723197113406,44.7743832191377,122.956127728826)) ;
#40218 = CARTESIAN_POINT('Ctrl Pts',(-18.339321156955,44.9642545424993,122.855346311805)) ;
#40219 = CARTESIAN_POINT('Ctrl Pts',(-18.0718425713176,44.7842654620895,122.716214046149)) ;
#40220 = CARTESIAN_POINT('Ctrl Pts',(-18.4529511231331,44.9743140135291,122.677012970206)) ;
#40221 = CARTESIAN_POINT('Ctrl Pts',(-18.2138824565309,44.7943249331193,122.493298818383)) ;
#40222 = CARTESIAN_POINT('Ctrl Pts',(-18.5931221037197,44.9841804581923,122.524103073492)) ;
#40223 = CARTESIAN_POINT('Ctrl Pts',(-18.3890982743492,44.8041913777825,122.302163339067)) ;
#40224 = CARTESIAN_POINT('Ctrl Pts',(-18.7589604520614,44.994146582641,122.3960648915)) ;
#40225 = CARTESIAN_POINT('Ctrl Pts',(-18.5963979569231,44.8141575022311,122.142117824545)) ;
#40226 = CARTESIAN_POINT('Ctrl Pts',(-18.9458650964473,45.0041768260321,122.298439068355)) ;
#40227 = CARTESIAN_POINT('Ctrl Pts',(-18.8300300927148,44.8241877456223,122.020087986047)) ;
#40228 = CARTESIAN_POINT('Ctrl Pts',(-19.1440629077566,45.0140698609852,122.235330723378)) ;
#40229 = CARTESIAN_POINT('Ctrl Pts',(-19.0777784030941,44.8340807805753,121.941205272845)) ;
#40230 = CARTESIAN_POINT('Ctrl Pts',(-19.3534531145185,45.024120775222,122.207100463021)) ;
#40231 = CARTESIAN_POINT('Ctrl Pts',(-19.3395157430268,44.8441316948122,121.905920090601)) ;
#40232 = CARTESIAN_POINT('Ctrl Pts',(-19.5612049836232,45.0340106014466,122.215495999718)) ;
#40233 = CARTESIAN_POINT('Ctrl Pts',(-19.5992088007516,44.8540215210367,121.916417743539)) ;
#40234 = CARTESIAN_POINT('Ctrl Pts',(-19.8352568409963,45.0473454164935,122.274745540189)) ;
#40235 = CARTESIAN_POINT('Ctrl Pts',(-19.9417558495627,44.8673563360837,121.990481112077)) ;
#40236 = CARTESIAN_POINT('Ctrl Pts',(-20.0861970248156,45.060622507665,122.404050574181)) ;
#40237 = CARTESIAN_POINT('Ctrl Pts',(-20.2554040576393,44.8806334272551,122.152088557829)) ;
#40238 = CARTESIAN_POINT('Ctrl Pts',(-20.2927670242742,45.0738707962633,122.590851363296)) ;
#40239 = CARTESIAN_POINT('Ctrl Pts',(-20.5136611156459,44.8938817158535,122.385626670175)) ;
#40240 = CARTESIAN_POINT('Ctrl Pts',(-20.4224319151714,45.0839256377574,122.757766119149)) ;
#40241 = CARTESIAN_POINT('Ctrl Pts',(-20.6757307464125,44.9039365573475,122.594264917547)) ;
#40242 = CARTESIAN_POINT('Ctrl Pts',(-20.5192820589709,45.0937566270649,122.940386196395)) ;
#40243 = CARTESIAN_POINT('Ctrl Pts',(-20.7967932246685,44.9137675466551,122.822543238492)) ;
#40244 = CARTESIAN_POINT('Ctrl Pts',(-20.584670046844,45.1038331913881,123.141847213542)) ;
#40245 = CARTESIAN_POINT('Ctrl Pts',(-20.8785256179564,44.9238441109783,123.07436836546)) ;
#40246 = CARTESIAN_POINT('Ctrl Pts',(-20.6134250008506,45.1136825165221,123.34692196347)) ;
#40247 = CARTESIAN_POINT('Ctrl Pts',(-20.9144646605094,44.9336934361122,123.330718388818)) ;
#40248 = CARTESIAN_POINT('Ctrl Pts',(-20.6042179421268,45.1270305161593,123.627426871071)) ;
#40249 = CARTESIAN_POINT('Ctrl Pts',(-20.9029627809531,44.9470414357495,123.681317025958)) ;
#40250 = CARTESIAN_POINT('Ctrl Pts',(-20.501477245052,45.1436152756959,123.964696954444)) ;
#40251 = CARTESIAN_POINT('Ctrl Pts',(-20.7745082952535,44.9636261952861,124.102953255056)) ;
#40252 = CARTESIAN_POINT('Ctrl Pts',(-20.2906509977138,45.160183827044,124.247002494003)) ;
#40253 = CARTESIAN_POINT('Ctrl Pts',(-20.5110259010541,44.9801947466342,124.455768261857)) ;
#40254 = CARTESIAN_POINT('Ctrl Pts',(-20.0699761701848,45.173543651863,124.420705346495)) ;
#40255 = CARTESIAN_POINT('Ctrl Pts',(-20.2351348039326,44.9935545714532,124.672943272152)) ;
#40256 = CARTESIAN_POINT('Ctrl Pts',(-19.8865323634229,45.1834490606937,124.519294728282)) ;
#40257 = CARTESIAN_POINT('Ctrl Pts',(-20.0058393288529,45.0034599802838,124.796167835436)) ;
#40258 = CARTESIAN_POINT('Ctrl Pts',(-19.6878012033677,45.1934090872777,124.585169308581)) ;
#40259 = CARTESIAN_POINT('Ctrl Pts',(-19.7574184008702,45.0134200068679,124.878510971873)) ;
#40260 = CARTESIAN_POINT('Ctrl Pts',(-19.4120405401479,45.206666671463,124.625957687893)) ;
#40261 = CARTESIAN_POINT('Ctrl Pts',(-19.4127381950799,45.0266775910532,124.929494089097)) ;
#40262 = CARTESIAN_POINT('Ctrl Pts',(-19.0603261711488,45.2233178829577,124.585513512105)) ;
#40263 = CARTESIAN_POINT('Ctrl Pts',(-18.9730728854601,45.0433288025479,124.87893348785)) ;
#40264 = CARTESIAN_POINT('Ctrl Pts',(-18.6814904591991,45.243236097068,124.396215063051)) ;
#40265 = CARTESIAN_POINT('Ctrl Pts',(-18.4995381186074,45.0632470166581,124.642306903912)) ;
#40266 = CARTESIAN_POINT('Ctrl Pts',(-18.3898754544286,45.2631138602888,124.090194523484)) ;
#40267 = CARTESIAN_POINT('Ctrl Pts',(-18.1350210819203,45.083124779879,124.259778759183)) ;
#40268 = CARTESIAN_POINT('Ctrl Pts',(-18.2194472690857,45.283126528076,123.70037612657)) ;
#40269 = CARTESIAN_POINT('Ctrl Pts',(-17.9219902773801,45.1031374476661,123.772503946096)) ;
#40270 = CARTESIAN_POINT('Ctrl Pts',(-18.1921410054773,45.3029390507426,123.279913832054)) ;
#40271 = CARTESIAN_POINT('Ctrl Pts',(-17.8878614142663,45.1229499703327,123.246927329165)) ;
#40272 = CARTESIAN_POINT('Ctrl Pts',(-18.3102817888919,45.3229223507425,122.871855648759)) ;
#40273 = CARTESIAN_POINT('Ctrl Pts',(-18.0355408684249,45.1429332703326,122.736855760761)) ;
#40274 = CARTESIAN_POINT('Ctrl Pts',(-18.5597996288413,45.3428166278438,122.530199318799)) ;
#40275 = CARTESIAN_POINT('Ctrl Pts',(-18.3474404946202,45.162827547434,122.30978822878)) ;
#40276 = CARTESIAN_POINT('Ctrl Pts',(-18.9111760068349,45.3627493896015,122.293234594438)) ;
#40277 = CARTESIAN_POINT('Ctrl Pts',(-18.7866621497905,45.1827603091917,122.013585300627)) ;
#40278 = CARTESIAN_POINT('Ctrl Pts',(-19.3230940340298,45.3827153953663,122.190513539357)) ;
#40279 = CARTESIAN_POINT('Ctrl Pts',(-19.301560104668,45.2027263149564,121.885187082608)) ;
#40280 = CARTESIAN_POINT('Ctrl Pts',(-19.7435470242779,45.4025939275311,122.234031106994)) ;
#40281 = CARTESIAN_POINT('Ctrl Pts',(-19.8271247058166,45.2226048471213,121.939586650909)) ;
#40282 = CARTESIAN_POINT('Ctrl Pts',(-20.1251936183417,45.4225335941915,122.418585683632)) ;
#40283 = CARTESIAN_POINT('Ctrl Pts',(-20.3041812490241,45.2425445137817,122.170281678223)) ;
#40284 = CARTESIAN_POINT('Ctrl Pts',(-20.4204383603451,45.4424284688368,122.721592637798)) ;
#40285 = CARTESIAN_POINT('Ctrl Pts',(-20.673234757287,45.262439388427,122.549040856851)) ;
#40286 = CARTESIAN_POINT('Ctrl Pts',(-20.5949902534563,45.4623356081302,123.107099332329)) ;
#40287 = CARTESIAN_POINT('Ctrl Pts',(-20.8914226003614,45.2823465277204,123.03092366851)) ;
#40288 = CARTESIAN_POINT('Ctrl Pts',(-20.6282585414511,45.4822461562087,123.529280154733)) ;
#40289 = CARTESIAN_POINT('Ctrl Pts',(-20.9330069949025,45.3022570757988,123.558648564274)) ;
#40290 = CARTESIAN_POINT('Ctrl Pts',(-20.5136884964889,45.5023147415659,123.940226483196)) ;
#40291 = CARTESIAN_POINT('Ctrl Pts',(-20.7897928711764,45.322325661156,124.072332126793)) ;
#40292 = CARTESIAN_POINT('Ctrl Pts',(-20.2695153225536,45.5220965388806,124.282881980283)) ;
#40293 = CARTESIAN_POINT('Ctrl Pts',(-20.4845776582098,45.3421074584708,124.500648372622)) ;
#40294 = CARTESIAN_POINT('Ctrl Pts',(-19.9197219519249,45.5421040858251,124.52470903084)) ;
#40295 = CARTESIAN_POINT('Ctrl Pts',(-20.0473359397497,45.3621150054153,124.802932073831)) ;
#40296 = CARTESIAN_POINT('Ctrl Pts',(-19.5119563590964,45.561925824128,124.631740685911)) ;
#40297 = CARTESIAN_POINT('Ctrl Pts',(-19.5376317009482,45.3819367437181,124.936721152297)) ;
#40298 = CARTESIAN_POINT('Ctrl Pts',(-19.0888978513631,45.5819058440321,124.593677351388)) ;
#40299 = CARTESIAN_POINT('Ctrl Pts',(-19.008808761564,45.4019167636223,124.889143040462)) ;
#40300 = CARTESIAN_POINT('Ctrl Pts',(-18.7055922778892,45.6018232952944,124.413561871822)) ;
#40301 = CARTESIAN_POINT('Ctrl Pts',(-18.5296775435037,45.4218342148845,124.664000015281)) ;
#40302 = CARTESIAN_POINT('Ctrl Pts',(-18.4066895135121,45.6216982164671,124.114786478611)) ;
#40303 = CARTESIAN_POINT('Ctrl Pts',(-18.1560490204871,45.4417091360573,124.290533223546)) ;
#40304 = CARTESIAN_POINT('Ctrl Pts',(-18.2266120856884,45.6417225850179,123.729001322783)) ;
#40305 = CARTESIAN_POINT('Ctrl Pts',(-17.9309504550063,45.4617335046081,123.808302209961)) ;
#40306 = CARTESIAN_POINT('Ctrl Pts',(-18.1894029579917,45.6615892693914,123.308154855926)) ;
#40307 = CARTESIAN_POINT('Ctrl Pts',(-17.8844372684627,45.4816001889816,123.282245957204)) ;
#40308 = CARTESIAN_POINT('Ctrl Pts',(-18.2977756961196,45.6815330912376,122.898226280014)) ;
#40309 = CARTESIAN_POINT('Ctrl Pts',(-18.0199005694617,45.5015440108278,122.769835234254)) ;
#40310 = CARTESIAN_POINT('Ctrl Pts',(-18.5392315029753,45.7014404604891,122.55056181091)) ;
#40311 = CARTESIAN_POINT('Ctrl Pts',(-18.3217175474318,45.5214513800793,122.335254029411)) ;
#40312 = CARTESIAN_POINT('Ctrl Pts',(-18.8838051537408,45.7213151582358,122.30592410139)) ;
#40313 = CARTESIAN_POINT('Ctrl Pts',(-18.7524316861254,45.541326077826,122.029454998102)) ;
#40314 = CARTESIAN_POINT('Ctrl Pts',(-19.2933757524993,45.7412971007575,122.192842071119)) ;
#40315 = CARTESIAN_POINT('Ctrl Pts',(-19.2643939100307,45.5613080203477,121.888099189158)) ;
#40316 = CARTESIAN_POINT('Ctrl Pts',(-19.7151717006801,45.7611997676684,122.226529361424)) ;
#40317 = CARTESIAN_POINT('Ctrl Pts',(-19.7916381676722,45.5812106872585,121.930204794617)) ;
#40318 = CARTESIAN_POINT('Ctrl Pts',(-20.0998523433655,45.7810551252071,122.400620470514)) ;
#40319 = CARTESIAN_POINT('Ctrl Pts',(-20.2724895989513,45.6010660447972,122.14781446257)) ;
#40320 = CARTESIAN_POINT('Ctrl Pts',(-20.4047844549801,45.8011191639231,122.698883119931)) ;
#40321 = CARTESIAN_POINT('Ctrl Pts',(-20.6536580200365,45.6211300835133,122.520640262286)) ;
#40322 = CARTESIAN_POINT('Ctrl Pts',(-20.5876495556406,45.8209743436481,123.079572690105)) ;
#40323 = CARTESIAN_POINT('Ctrl Pts',(-20.8822424651836,45.6409852632383,122.996499598283)) ;
#40324 = CARTESIAN_POINT('Ctrl Pts',(-20.6301960454336,45.8409544483126,123.502103273831)) ;
#40325 = CARTESIAN_POINT('Ctrl Pts',(-20.9354305274522,45.6609653679027,123.524661889093)) ;
#40326 = CARTESIAN_POINT('Ctrl Pts',(-20.5273174567824,45.8607635534824,123.910665052776)) ;
#40327 = CARTESIAN_POINT('Ctrl Pts',(-20.8068347568446,45.6807744730725,124.035365380698)) ;
#40328 = CARTESIAN_POINT('Ctrl Pts',(-20.2894986913643,45.8807561738231,124.262859185796)) ;
#40329 = CARTESIAN_POINT('Ctrl Pts',(-20.509573914599,45.7007670934133,124.475605981079)) ;
#40330 = CARTESIAN_POINT('Ctrl Pts',(-20.0050296007185,45.8972956563272,124.469758288625)) ;
#40331 = CARTESIAN_POINT('Ctrl Pts',(-20.1539637829623,45.7173065759173,124.734247767435)) ;
#40332 = CARTESIAN_POINT('Ctrl Pts',(-19.7428533033287,45.9106599743914,124.570733072106)) ;
#40333 = CARTESIAN_POINT('Ctrl Pts',(-19.8262766968498,45.7306708939816,124.860455779967)) ;
#40334 = CARTESIAN_POINT('Ctrl Pts',(-19.4702042971827,45.9238775768929,124.624395490945)) ;
#40335 = CARTESIAN_POINT('Ctrl Pts',(-19.4853999049145,45.7438884964831,124.927543476364)) ;
#40336 = CARTESIAN_POINT('Ctrl Pts',(-19.1168393550171,45.9405351711707,124.600762737389)) ;
#40337 = CARTESIAN_POINT('Ctrl Pts',(-19.0437646821561,45.7605460907609,124.897999792961)) ;
#40338 = CARTESIAN_POINT('Ctrl Pts',(-18.7301975068277,45.9604008732124,124.430507653493)) ;
#40339 = CARTESIAN_POINT('Ctrl Pts',(-18.5604443553071,45.7804117928026,124.685196121314)) ;
#40340 = CARTESIAN_POINT('Ctrl Pts',(-18.4743625889817,45.9770305999024,124.186562575314)) ;
#40341 = CARTESIAN_POINT('Ctrl Pts',(-18.24063059039,45.7970415194926,124.380241225742)) ;
#40342 = CARTESIAN_POINT('Ctrl Pts',(-18.3289929824002,45.9903197150403,123.947896155844)) ;
#40343 = CARTESIAN_POINT('Ctrl Pts',(-18.0589348453774,45.8103306346304,124.081934291381)) ;
#40344 = CARTESIAN_POINT('Ctrl Pts',(-18.2525232753599,46.0002840620174,123.752891385966)) ;
#40345 = CARTESIAN_POINT('Ctrl Pts',(-17.9633418368629,45.8202949816076,123.838171148534)) ;
#40346 = CARTESIAN_POINT('Ctrl Pts',(-18.2110838319254,46.0102124300189,123.548318215047)) ;
#40347 = CARTESIAN_POINT('Ctrl Pts',(-17.9115389080793,45.8302233496091,123.582470100108)) ;
#40348 = CARTESIAN_POINT('Ctrl Pts',(-18.2034517091304,46.0234958631076,123.269181346863)) ;
#40349 = CARTESIAN_POINT('Ctrl Pts',(-17.9020047413627,45.8435067826978,123.233481404812)) ;
#40350 = CARTESIAN_POINT('Ctrl Pts',(-18.2859373810871,46.0401479408479,122.924806830037)) ;
#40351 = CARTESIAN_POINT('Ctrl Pts',(-18.0050894428753,45.8601588604381,122.803097863818)) ;
#40352 = CARTESIAN_POINT('Ctrl Pts',(-18.479608382182,46.0566993101488,122.631034753051)) ;
#40353 = CARTESIAN_POINT('Ctrl Pts',(-18.247204245024,45.8767102297389,122.43582128981)) ;
#40354 = CARTESIAN_POINT('Ctrl Pts',(-18.6881326465127,46.0699867382977,122.445080340454)) ;
#40355 = CARTESIAN_POINT('Ctrl Pts',(-18.5078328375025,45.8899976578879,122.203411111206)) ;
#40356 = CARTESIAN_POINT('Ctrl Pts',(-18.8678435030827,46.0800312779978,122.334231053414)) ;
#40357 = CARTESIAN_POINT('Ctrl Pts',(-18.7324749006749,45.900042197588,122.064839903959)) ;
#40358 = CARTESIAN_POINT('Ctrl Pts',(-19.060066473483,46.0898741198217,122.257583029304)) ;
#40359 = CARTESIAN_POINT('Ctrl Pts',(-18.9727512213938,45.9098850394119,121.969029204028)) ;
#40360 = CARTESIAN_POINT('Ctrl Pts',(-19.2654570004802,46.0998584040686,122.214404145467)) ;
#40361 = CARTESIAN_POINT('Ctrl Pts',(-19.2294892302729,45.9198693236588,121.915052304712)) ;
#40362 = CARTESIAN_POINT('Ctrl Pts',(-19.474529222648,46.1098080494678,122.207609739844)) ;
#40363 = CARTESIAN_POINT('Ctrl Pts',(-19.4908293876559,45.9298189690579,121.906556619417)) ;
#40364 = CARTESIAN_POINT('Ctrl Pts',(-19.6826867659275,46.1198078111562,122.237114286998)) ;
#40365 = CARTESIAN_POINT('Ctrl Pts',(-19.7510268140422,45.9398187307464,121.943434488451)) ;
#40366 = CARTESIAN_POINT('Ctrl Pts',(-19.8830689863678,46.1298391571151,122.30284594859)) ;
#40367 = CARTESIAN_POINT('Ctrl Pts',(-20.0015055167164,45.9498500767053,122.025596415267)) ;
#40368 = CARTESIAN_POINT('Ctrl Pts',(-20.0658738233849,46.1396941115922,122.400357303943)) ;
#40369 = CARTESIAN_POINT('Ctrl Pts',(-20.2300129909118,45.9597050311824,122.147483174529)) ;
#40370 = CARTESIAN_POINT('Ctrl Pts',(-20.2311978485199,46.1496666495927,122.529251790254)) ;
#40371 = CARTESIAN_POINT('Ctrl Pts',(-20.436669839149,45.9696775691829,122.308599139471)) ;
#40372 = CARTESIAN_POINT('Ctrl Pts',(-20.371971249445,46.1596616433277,122.68529494029)) ;
#40373 = CARTESIAN_POINT('Ctrl Pts',(-20.6126387230333,45.9796725629179,122.503651259924)) ;
#40374 = CARTESIAN_POINT('Ctrl Pts',(-20.4837019140822,46.1696957021218,122.864201377535)) ;
#40375 = CARTESIAN_POINT('Ctrl Pts',(-20.7523044635287,45.989706621712,122.727282847783)) ;
#40376 = CARTESIAN_POINT('Ctrl Pts',(-20.5615851923955,46.1795510449448,123.056218498459)) ;
#40377 = CARTESIAN_POINT('Ctrl Pts',(-20.8496612408274,45.999561964535,122.967303410846)) ;
#40378 = CARTESIAN_POINT('Ctrl Pts',(-20.6058435319962,46.1895505242904,123.261688930267)) ;
#40379 = CARTESIAN_POINT('Ctrl Pts',(-20.9049869102636,46.0095614438806,123.224140951686)) ;
#40380 = CARTESIAN_POINT('Ctrl Pts',(-20.613909648338,46.1994449730457,123.469584195291)) ;
#40381 = CARTESIAN_POINT('Ctrl Pts',(-20.9150723248819,46.0194558926359,123.484010185293)) ;
#40382 = CARTESIAN_POINT('Ctrl Pts',(-20.5852243576683,46.2095080924802,123.679152099285)) ;
#40383 = CARTESIAN_POINT('Ctrl Pts',(-20.8792184641812,46.0295190120704,123.745970407951)) ;
#40384 = CARTESIAN_POINT('Ctrl Pts',(-20.5222181496825,46.2193477377214,123.87621952154)) ;
#40385 = CARTESIAN_POINT('Ctrl Pts',(-20.8004631964892,46.0393586573116,123.992305910874)) ;
#40386 = CARTESIAN_POINT('Ctrl Pts',(-20.4240329883721,46.2294109019075,124.06358200029)) ;
#40387 = CARTESIAN_POINT('Ctrl Pts',(-20.6777341783053,46.0494218214976,124.22651023524)) ;
#40388 = CARTESIAN_POINT('Ctrl Pts',(-20.2968048807207,46.2393051716563,124.228173665467)) ;
#40389 = CARTESIAN_POINT('Ctrl Pts',(-20.5187010120896,46.0593160912465,124.432251752414)) ;
#40390 = CARTESIAN_POINT('Ctrl Pts',(-20.1426117795388,46.2492468976701,124.369228950053)) ;
#40391 = CARTESIAN_POINT('Ctrl Pts',(-20.3259612494257,46.0692578172603,124.608573010478)) ;
#40392 = CARTESIAN_POINT('Ctrl Pts',(-19.9651819070724,46.2592497863295,124.482167683482)) ;
#40393 = CARTESIAN_POINT('Ctrl Pts',(-20.1041752621222,46.0792607059197,124.749748717366)) ;
#40394 = CARTESIAN_POINT('Ctrl Pts',(-19.7700203195679,46.2692896351235,124.562503209581)) ;
#40395 = CARTESIAN_POINT('Ctrl Pts',(-19.8602243414152,46.0893005547136,124.850170623669)) ;
#40396 = CARTESIAN_POINT('Ctrl Pts',(-19.5683677612482,46.2791138505843,124.607227073809)) ;
#40397 = CARTESIAN_POINT('Ctrl Pts',(-19.6081586045718,46.0991247701745,124.906078173835)) ;
#40398 = CARTESIAN_POINT('Ctrl Pts',(-19.3571724462641,46.2891706940779,124.61676513193)) ;
#40399 = CARTESIAN_POINT('Ctrl Pts',(-19.3441646598622,46.109181613668,124.91800334369)) ;
#40400 = CARTESIAN_POINT('Ctrl Pts',(-19.1502130268079,46.2990993034739,124.589560068272)) ;
#40401 = CARTESIAN_POINT('Ctrl Pts',(-19.0854647176611,46.119110223064,124.883999596973)) ;
#40402 = CARTESIAN_POINT('Ctrl Pts',(-18.9504791865377,46.3090511875118,124.527247497498)) ;
#40403 = CARTESIAN_POINT('Ctrl Pts',(-18.8357963857366,46.129062107102,124.806111234184)) ;
#40404 = CARTESIAN_POINT('Ctrl Pts',(-18.7629062407361,46.3191041403194,124.429897592764)) ;
#40405 = CARTESIAN_POINT('Ctrl Pts',(-18.6013290922815,46.1391150599095,124.684426224034)) ;
#40406 = CARTESIAN_POINT('Ctrl Pts',(-18.5986696134654,46.3289270167856,124.304685324782)) ;
#40407 = CARTESIAN_POINT('Ctrl Pts',(-18.3960311453645,46.1489379363757,124.527912442019)) ;
#40408 = CARTESIAN_POINT('Ctrl Pts',(-18.4550971880899,46.3389827493557,124.149533035185)) ;
#40409 = CARTESIAN_POINT('Ctrl Pts',(-18.2165638687555,46.1589936689459,124.333973843057)) ;
#40410 = CARTESIAN_POINT('Ctrl Pts',(-18.34225300586,46.3489235143433,123.973622295558)) ;
#40411 = CARTESIAN_POINT('Ctrl Pts',(-18.0755063144971,46.1689344339335,124.114086515465)) ;
#40412 = CARTESIAN_POINT('Ctrl Pts',(-18.2613628141207,46.358827847249,123.78175251306)) ;
#40413 = CARTESIAN_POINT('Ctrl Pts',(-17.9743911402147,46.1788387668392,123.874249738022)) ;
#40414 = CARTESIAN_POINT('Ctrl Pts',(-18.2144855602519,46.3688745161297,123.575825795225)) ;
#40415 = CARTESIAN_POINT('Ctrl Pts',(-17.915792209874,46.1888854357199,123.616841983507)) ;
#40416 = CARTESIAN_POINT('Ctrl Pts',(-18.2040405773316,46.3787700794355,123.368018792122)) ;
#40417 = CARTESIAN_POINT('Ctrl Pts',(-17.9027335514431,46.1987809990257,123.357082770934)) ;
#40418 = CARTESIAN_POINT('Ctrl Pts',(-18.2302623333417,46.3888321371358,123.158144461646)) ;
#40419 = CARTESIAN_POINT('Ctrl Pts',(-17.9355083347954,46.2088430567259,123.094739738862)) ;
#40420 = CARTESIAN_POINT('Ctrl Pts',(-18.2910726090505,46.3986749147633,122.960331021879)) ;
#40421 = CARTESIAN_POINT('Ctrl Pts',(-18.0115191596007,46.2186858343534,122.84747141581)) ;
#40422 = CARTESIAN_POINT('Ctrl Pts',(-18.3862537401612,46.4086653930151,122.773135377991)) ;
#40423 = CARTESIAN_POINT('Ctrl Pts',(-18.1304936326188,46.2286763126053,122.613475678905)) ;
#40424 = CARTESIAN_POINT('Ctrl Pts',(-18.5117634998611,46.4185943656587,122.606329099744)) ;
#40425 = CARTESIAN_POINT('Ctrl Pts',(-18.2873793151944,46.2386052852488,122.404966075786)) ;
#40426 = CARTESIAN_POINT('Ctrl Pts',(-18.6650531697513,46.4285855025382,122.462726172881)) ;
#40427 = CARTESIAN_POINT('Ctrl Pts',(-18.4789900283412,46.2485964221284,122.225460708886)) ;
#40428 = CARTESIAN_POINT('Ctrl Pts',(-18.8416348523983,46.4386076200272,122.347776529069)) ;
#40429 = CARTESIAN_POINT('Ctrl Pts',(-18.6997158872506,46.2586185396174,122.081771774916)) ;
#40430 = CARTESIAN_POINT('Ctrl Pts',(-19.033062714252,46.4485081304294,122.266054468037)) ;
#40431 = CARTESIAN_POINT('Ctrl Pts',(-18.9390004515554,46.2685190500195,121.979616917405)) ;
#40432 = CARTESIAN_POINT('Ctrl Pts',(-19.2375063165582,46.4584971231755,122.218070769825)) ;
#40433 = CARTESIAN_POINT('Ctrl Pts',(-19.1945546489637,46.2785080427657,121.919635191625)) ;
#40434 = CARTESIAN_POINT('Ctrl Pts',(-19.4466780664343,46.4684623672261,122.206487877889)) ;
#40435 = CARTESIAN_POINT('Ctrl Pts',(-19.4560195398853,46.2884732868162,121.905154403396)) ;
#40436 = CARTESIAN_POINT('Ctrl Pts',(-19.6534929917255,46.4783666317393,122.230762789135)) ;
#40437 = CARTESIAN_POINT('Ctrl Pts',(-19.7145391120735,46.2983775513295,121.935496118743)) ;
#40438 = CARTESIAN_POINT('Ctrl Pts',(-19.8559786184111,46.4884247234375,122.291626495888)) ;
#40439 = CARTESIAN_POINT('Ctrl Pts',(-19.9676465194211,46.3084356430277,122.01157371518)) ;
#40440 = CARTESIAN_POINT('Ctrl Pts',(-20.0410082512781,46.4982746638659,122.384630025382)) ;
#40441 = CARTESIAN_POINT('Ctrl Pts',(-20.1989353902654,46.3182855834561,122.127826794812)) ;
#40442 = CARTESIAN_POINT('Ctrl Pts',(-20.2103627890321,46.5083016750394,122.510144547104)) ;
#40443 = CARTESIAN_POINT('Ctrl Pts',(-20.4106296401111,46.3283125946296,122.28471843049)) ;
#40444 = CARTESIAN_POINT('Ctrl Pts',(-20.354983799268,46.5183302616515,122.66357001132)) ;
#40445 = CARTESIAN_POINT('Ctrl Pts',(-20.5914073283371,46.3383411812416,122.476498822168)) ;
#40446 = CARTESIAN_POINT('Ctrl Pts',(-20.4689669278839,46.5281754757642,122.836320633626)) ;
#40447 = CARTESIAN_POINT('Ctrl Pts',(-20.7338884448632,46.3481863953544,122.692436981953)) ;
#40448 = CARTESIAN_POINT('Ctrl Pts',(-20.5529614777016,46.5381662239437,123.028836720587)) ;
#40449 = CARTESIAN_POINT('Ctrl Pts',(-20.8388832978075,46.3581771435339,122.933081577191)) ;
#40450 = CARTESIAN_POINT('Ctrl Pts',(-20.6020311758152,46.5482038575292,123.234075060244)) ;
#40451 = CARTESIAN_POINT('Ctrl Pts',(-20.9002222160661,46.3682147771194,123.189628936888)) ;
#40452 = CARTESIAN_POINT('Ctrl Pts',(-20.6148200501619,46.5580491467421,123.440660845129)) ;
#40453 = CARTESIAN_POINT('Ctrl Pts',(-20.9162101456028,46.3780600663322,123.447862222643)) ;
#40454 = CARTESIAN_POINT('Ctrl Pts',(-20.5916887931145,46.568030547548,123.649206343481)) ;
#40455 = CARTESIAN_POINT('Ctrl Pts',(-20.8872976540817,46.3880414671381,123.708544539152)) ;
#40456 = CARTESIAN_POINT('Ctrl Pts',(-20.5328161463453,46.5779827805379,123.849986028359)) ;
#40457 = CARTESIAN_POINT('Ctrl Pts',(-20.8137082786471,46.3979937001281,123.959520057997)) ;
#40458 = CARTESIAN_POINT('Ctrl Pts',(-20.4397820483577,46.5879815919945,124.038501912924)) ;
#40459 = CARTESIAN_POINT('Ctrl Pts',(-20.6974169784286,46.4079925115847,124.195165716558)) ;
#40460 = CARTESIAN_POINT('Ctrl Pts',(-20.3146171869605,46.5980206959252,124.208420179491)) ;
#40461 = CARTESIAN_POINT('Ctrl Pts',(-20.5409623496544,46.4180316155154,124.407564420315)) ;
#40462 = CARTESIAN_POINT('Ctrl Pts',(-20.1653985323656,46.6078456383445,124.351256112857)) ;
#40463 = CARTESIAN_POINT('Ctrl Pts',(-20.3544390960166,46.4278565579347,124.586111387975)) ;
#40464 = CARTESIAN_POINT('Ctrl Pts',(-19.989843192052,46.6179003258204,124.468971674532)) ;
#40465 = CARTESIAN_POINT('Ctrl Pts',(-20.1349959199088,46.4379112454106,124.733256870645)) ;
#40466 = CARTESIAN_POINT('Ctrl Pts',(-19.7985051156906,46.6278431281773,124.553146705472)) ;
#40467 = CARTESIAN_POINT('Ctrl Pts',(-19.8958234362886,46.4478540477674,124.838477290349)) ;
#40468 = CARTESIAN_POINT('Ctrl Pts',(-19.5964092228832,46.637746924117,124.603245253759)) ;
#40469 = CARTESIAN_POINT('Ctrl Pts',(-19.6432030628743,46.4577578437072,124.901101950922)) ;
#40470 = CARTESIAN_POINT('Ctrl Pts',(-19.3856978448509,46.6477937034921,124.617570281629)) ;
#40471 = CARTESIAN_POINT('Ctrl Pts',(-19.3798141419752,46.4678046230822,124.919009575236)) ;
#40472 = CARTESIAN_POINT('Ctrl Pts',(-19.1787922985653,46.6576893617867,124.595604702868)) ;
#40473 = CARTESIAN_POINT('Ctrl Pts',(-19.1211811679107,46.4777002813768,124.891553789265)) ;
#40474 = CARTESIAN_POINT('Ctrl Pts',(-18.9755356634845,46.6677509290373,124.537120494577)) ;
#40475 = CARTESIAN_POINT('Ctrl Pts',(-18.8671103311034,46.4877618486275,124.818449853057)) ;
#40476 = CARTESIAN_POINT('Ctrl Pts',(-18.7895780705822,46.6775955734746,124.446252644844)) ;
#40477 = CARTESIAN_POINT('Ctrl Pts',(-18.6346615957994,46.4976064930648,124.704865605412)) ;
#40478 = CARTESIAN_POINT('Ctrl Pts',(-18.6198270026623,46.6875556197173,124.323663154049)) ;
#40479 = CARTESIAN_POINT('Ctrl Pts',(-18.4224718069729,46.5075665393075,124.551629282705)) ;
#40480 = CARTESIAN_POINT('Ctrl Pts',(-18.4730960397559,46.6975939157357,124.171998085648)) ;
#40481 = CARTESIAN_POINT('Ctrl Pts',(-18.2390573894133,46.5176048353258,124.362048863157)) ;
#40482 = CARTESIAN_POINT('Ctrl Pts',(-18.3565170418454,46.707467257154,124.0002223481)) ;
#40483 = CARTESIAN_POINT('Ctrl Pts',(-18.0933321835111,46.5274781767442,124.147328823176)) ;
#40484 = CARTESIAN_POINT('Ctrl Pts',(-18.2699035021467,46.7175403609533,123.807021171241)) ;
#40485 = CARTESIAN_POINT('Ctrl Pts',(-17.9850644965826,46.5375512805435,123.90582815991)) ;
#40486 = CARTESIAN_POINT('Ctrl Pts',(-18.2191778694931,46.7273611760722,123.606843477145)) ;
#40487 = CARTESIAN_POINT('Ctrl Pts',(-17.9216561766036,46.5473720956623,123.655604769704)) ;
#40488 = CARTESIAN_POINT('Ctrl Pts',(-18.2033482281936,46.7374380411502,123.395627154277)) ;
#40489 = CARTESIAN_POINT('Ctrl Pts',(-17.9018683249847,46.5574489607404,123.391584873683)) ;
#40490 = CARTESIAN_POINT('Ctrl Pts',(-18.2240747598041,46.7473027808054,123.189252605334)) ;
#40491 = CARTESIAN_POINT('Ctrl Pts',(-17.9277757498325,46.5673137003956,123.133615388433)) ;
#40492 = CARTESIAN_POINT('Ctrl Pts',(-18.2806784571676,46.7573251840468,122.986304105928)) ;
#40493 = CARTESIAN_POINT('Ctrl Pts',(-17.9985297243312,46.5773361036369,122.879929630488)) ;
#40494 = CARTESIAN_POINT('Ctrl Pts',(-18.3721757227985,46.7673509083353,122.796412957651)) ;
#40495 = CARTESIAN_POINT('Ctrl Pts',(-18.112900494446,46.5873618279254,122.642565399485)) ;
#40496 = CARTESIAN_POINT('Ctrl Pts',(-18.4928445279093,46.7772056913566,122.628018609058)) ;
#40497 = CARTESIAN_POINT('Ctrl Pts',(-18.263736687569,46.5972166109468,122.432070963877)) ;
#40498 = CARTESIAN_POINT('Ctrl Pts',(-18.6424131075352,46.7871845350798,122.480907272402)) ;
#40499 = CARTESIAN_POINT('Ctrl Pts',(-18.4506972916497,46.60719545467,122.2481811978)) ;
#40500 = CARTESIAN_POINT('Ctrl Pts',(-18.8161403685394,46.7972034273165,122.361831711629)) ;
#40501 = CARTESIAN_POINT('Ctrl Pts',(-18.6678559884492,46.6172143469067,122.099336220599)) ;
#40502 = CARTESIAN_POINT('Ctrl Pts',(-19.0051621248725,46.8070866363575,122.275502154482)) ;
#40503 = CARTESIAN_POINT('Ctrl Pts',(-18.9041339832158,46.6270975559476,121.991423381357)) ;
#40504 = CARTESIAN_POINT('Ctrl Pts',(-19.210031702073,46.8171549456977,122.222428926557)) ;
#40505 = CARTESIAN_POINT('Ctrl Pts',(-19.1602204279104,46.6371658652879,121.925081449828)) ;
#40506 = CARTESIAN_POINT('Ctrl Pts',(-19.4160633040709,46.8269850710304,122.205881850251)) ;
#40507 = CARTESIAN_POINT('Ctrl Pts',(-19.4177614318247,46.6469959906205,121.904397063285)) ;
#40508 = CARTESIAN_POINT('Ctrl Pts',(-19.6267444353502,46.8370516234074,122.22554880192)) ;
#40509 = CARTESIAN_POINT('Ctrl Pts',(-19.681112479363,46.6570625429976,121.928980404432)) ;
#40510 = CARTESIAN_POINT('Ctrl Pts',(-19.8272585672866,46.8469418603011,122.280657735595)) ;
#40511 = CARTESIAN_POINT('Ctrl Pts',(-19.9317562516672,46.6669527798912,121.997866497252)) ;
#40512 = CARTESIAN_POINT('Ctrl Pts',(-20.0172576560397,46.8569340850951,122.370232887069)) ;
#40513 = CARTESIAN_POINT('Ctrl Pts',(-20.1692553844412,46.6769450046852,122.109835361728)) ;
#40514 = CARTESIAN_POINT('Ctrl Pts',(-20.1882040593248,46.866896705446,122.491242308474)) ;
#40515 = CARTESIAN_POINT('Ctrl Pts',(-20.3829389131925,46.6869076250362,122.261097188101)) ;
#40516 = CARTESIAN_POINT('Ctrl Pts',(-20.3350687567512,46.8768017082092,122.638883740388)) ;
#40517 = CARTESIAN_POINT('Ctrl Pts',(-20.5665204840061,46.6968126277993,122.445649602408)) ;
#40518 = CARTESIAN_POINT('Ctrl Pts',(-20.4557645798383,46.8868594706073,122.812475638472)) ;
#40519 = CARTESIAN_POINT('Ctrl Pts',(-20.717390165257,46.7068703901975,122.662639131552)) ;
#40520 = CARTESIAN_POINT('Ctrl Pts',(-20.5428264939987,46.8967099899861,123.000391779581)) ;
#40521 = CARTESIAN_POINT('Ctrl Pts',(-20.8262181895513,46.7167209095763,122.897535565363)) ;
#40522 = CARTESIAN_POINT('Ctrl Pts',(-20.5973539637941,46.9067415669843,123.204102169364)) ;
#40523 = CARTESIAN_POINT('Ctrl Pts',(-20.8943773618828,46.7267524865744,123.152173475016)) ;
#40524 = CARTESIAN_POINT('Ctrl Pts',(-20.6152416325616,46.9167513020892,123.413800001265)) ;
#40525 = CARTESIAN_POINT('Ctrl Pts',(-20.9167369791309,46.7367622216794,123.414295804395)) ;
#40526 = CARTESIAN_POINT('Ctrl Pts',(-20.5968220041765,46.9266608787155,123.621296181329)) ;
#40527 = CARTESIAN_POINT('Ctrl Pts',(-20.8937123153828,46.7466717983056,123.673666920651)) ;
#40528 = CARTESIAN_POINT('Ctrl Pts',(-20.5430662397492,46.9365882645721,123.822968750851)) ;
#40529 = CARTESIAN_POINT('Ctrl Pts',(-20.8265171674888,46.7565991841623,123.925758286635)) ;
#40530 = CARTESIAN_POINT('Ctrl Pts',(-20.4539206450829,46.9466331990624,124.014396648142)) ;
#40531 = CARTESIAN_POINT('Ctrl Pts',(-20.7150850922939,46.7666441186526,124.165042884017)) ;
#40532 = CARTESIAN_POINT('Ctrl Pts',(-20.3348959674513,46.9565191312504,124.184787009017)) ;
#40533 = CARTESIAN_POINT('Ctrl Pts',(-20.5663034238084,46.7765300508405,124.378031588632)) ;
#40534 = CARTESIAN_POINT('Ctrl Pts',(-20.1867731077761,46.9665124372034,124.333759281434)) ;
#40535 = CARTESIAN_POINT('Ctrl Pts',(-20.3811494336944,46.7865233567936,124.56424680327)) ;
#40536 = CARTESIAN_POINT('Ctrl Pts',(-20.0157955120954,46.9764580749853,124.454112395529)) ;
#40537 = CARTESIAN_POINT('Ctrl Pts',(-20.1674267507565,46.7964689945755,124.714688252235)) ;
#40538 = CARTESIAN_POINT('Ctrl Pts',(-19.8266604007549,46.9864053433312,124.543356690271)) ;
#40539 = CARTESIAN_POINT('Ctrl Pts',(-19.9310071201498,46.8064162629214,124.826243396282)) ;
#40540 = CARTESIAN_POINT('Ctrl Pts',(-19.6228151224958,46.9964532454683,124.598728489148)) ;
#40541 = CARTESIAN_POINT('Ctrl Pts',(-19.6762006528728,46.8164641650585,124.895457669086)) ;
#40542 = CARTESIAN_POINT('Ctrl Pts',(-19.4166526981356,47.0063009403085,124.617657767281)) ;
#40543 = CARTESIAN_POINT('Ctrl Pts',(-19.4184961828362,46.8263118598987,124.919118902968)) ;
#40544 = CARTESIAN_POINT('Ctrl Pts',(-19.2079050762096,47.0162624500529,124.600964149911)) ;
#40545 = CARTESIAN_POINT('Ctrl Pts',(-19.1575612606984,46.8362733696431,124.898251094287)) ;
#40546 = CARTESIAN_POINT('Ctrl Pts',(-19.0039009099091,47.0262918416617,124.54764239375)) ;
#40547 = CARTESIAN_POINT('Ctrl Pts',(-18.9025563129706,46.8463027612519,124.83159830442)) ;
#40548 = CARTESIAN_POINT('Ctrl Pts',(-18.8145419924307,47.0361993372165,124.460883485285)) ;
#40549 = CARTESIAN_POINT('Ctrl Pts',(-18.6658571373516,46.8562102568067,124.723148672064)) ;
#40550 = CARTESIAN_POINT('Ctrl Pts',(-18.642246189298,47.0461447288795,124.342465094977)) ;
#40551 = CARTESIAN_POINT('Ctrl Pts',(-18.4504873824493,46.8661556484697,124.575124657346)) ;
#40552 = CARTESIAN_POINT('Ctrl Pts',(-18.4921614871914,47.0561466464769,124.1951532533)) ;
#40553 = CARTESIAN_POINT('Ctrl Pts',(-18.2628820412351,46.876157566067,124.390984128051)) ;
#40554 = CARTESIAN_POINT('Ctrl Pts',(-18.3698136381604,47.0661867140291,124.023179183361)) ;
#40555 = CARTESIAN_POINT('Ctrl Pts',(-18.1099479380349,46.8861976336192,124.176016249367)) ;
#40556 = CARTESIAN_POINT('Ctrl Pts',(-18.2806928887342,47.0760110254689,123.836839708192)) ;
#40557 = CARTESIAN_POINT('Ctrl Pts',(-17.9985471751424,46.896021945059,123.943090129872)) ;
#40558 = CARTESIAN_POINT('Ctrl Pts',(-18.2237020979738,47.086067266625,123.633273731581)) ;
#40559 = CARTESIAN_POINT('Ctrl Pts',(-17.9273097684418,46.9060781862152,123.688632681339)) ;
#40560 = CARTESIAN_POINT('Ctrl Pts',(-18.203421628533,47.0959981883606,123.425458332389)) ;
#40561 = CARTESIAN_POINT('Ctrl Pts',(-17.9019600483901,46.9160091079508,123.428862667501)) ;
#40562 = CARTESIAN_POINT('Ctrl Pts',(-18.2191232760878,47.1059414244368,123.217037662918)) ;
#40563 = CARTESIAN_POINT('Ctrl Pts',(-17.92158824873,46.925952344027,123.168336310524)) ;
#40564 = CARTESIAN_POINT('Ctrl Pts',(-18.2707913644975,47.1159227084493,123.013627488194)) ;
#40565 = CARTESIAN_POINT('Ctrl Pts',(-17.9861745622981,46.9359336280395,122.914073624289)) ;
#40566 = CARTESIAN_POINT('Ctrl Pts',(-18.3578456878256,47.125967010075,122.821273166394)) ;
#40567 = CARTESIAN_POINT('Ctrl Pts',(-18.094993333607,46.9459779296651,122.67363132512)) ;
#40568 = CARTESIAN_POINT('Ctrl Pts',(-18.4740478321358,47.1357950912944,122.650390408871)) ;
#40569 = CARTESIAN_POINT('Ctrl Pts',(-18.2402478329173,46.9558060108846,122.460027367122)) ;
#40570 = CARTESIAN_POINT('Ctrl Pts',(-18.6216725538285,47.1458716941436,122.498517159224)) ;
#40571 = CARTESIAN_POINT('Ctrl Pts',(-18.4247793330905,46.9658826137337,122.270186990545)) ;
#40572 = CARTESIAN_POINT('Ctrl Pts',(-18.789608451275,47.1557237732621,122.377209771896)) ;
#40573 = CARTESIAN_POINT('Ctrl Pts',(-18.6347009617325,46.9757346928523,122.118553077967)) ;
#40574 = CARTESIAN_POINT('Ctrl Pts',(-18.980091407923,47.165797031571,122.284749398737)) ;
#40575 = CARTESIAN_POINT('Ctrl Pts',(-18.8728048872748,46.9858079511612,122.002979006132)) ;
#40576 = CARTESIAN_POINT('Ctrl Pts',(-19.1791102852178,47.1756384909513,122.228144087822)) ;
#40577 = CARTESIAN_POINT('Ctrl Pts',(-19.1215801045006,46.9956494105415,121.932223291973)) ;
#40578 = CARTESIAN_POINT('Ctrl Pts',(-19.3873332175923,47.1855995863637,122.205917819797)) ;
#40579 = CARTESIAN_POINT('Ctrl Pts',(-19.3818593433925,47.0056105059539,121.904442012437)) ;
#40580 = CARTESIAN_POINT('Ctrl Pts',(-19.5978250311267,47.1956368707604,122.220705841968)) ;
#40581 = CARTESIAN_POINT('Ctrl Pts',(-19.6449738783017,47.0156477903506,121.922928491148)) ;
#40582 = CARTESIAN_POINT('Ctrl Pts',(-19.7993828425593,47.2055132094957,122.270652196407)) ;
#40583 = CARTESIAN_POINT('Ctrl Pts',(-19.8969217299494,47.0255241290858,121.985363214228)) ;
#40584 = CARTESIAN_POINT('Ctrl Pts',(-19.9927485786675,47.2155753356489,122.356364369119)) ;
#40585 = CARTESIAN_POINT('Ctrl Pts',(-20.1386279884398,47.0355862552391,122.092504779717)) ;
#40586 = CARTESIAN_POINT('Ctrl Pts',(-20.1649812697198,47.2254435096255,122.472061623222)) ;
#40587 = CARTESIAN_POINT('Ctrl Pts',(-20.353918813109,47.0454544292157,122.237128269976)) ;
#40588 = CARTESIAN_POINT('Ctrl Pts',(-20.3168466409141,47.2354490581293,122.61756598711)) ;
#40589 = CARTESIAN_POINT('Ctrl Pts',(-20.5437493741257,47.0554599777195,122.419010050807)) ;
#40590 = CARTESIAN_POINT('Ctrl Pts',(-20.4408371920724,47.2454316900249,122.7869363998)) ;
#40591 = CARTESIAN_POINT('Ctrl Pts',(-20.698736298612,47.065442609615,122.63072426996)) ;
#40592 = CARTESIAN_POINT('Ctrl Pts',(-20.5338834735868,47.2554756324466,122.976466219455)) ;
#40593 = CARTESIAN_POINT('Ctrl Pts',(-20.8150425910065,47.0754865520368,122.867637130204)) ;
#40594 = CARTESIAN_POINT('Ctrl Pts',(-20.5916167588128,47.2653037804738,123.17485450326)) ;
#40595 = CARTESIAN_POINT('Ctrl Pts',(-20.8872078792665,47.085314700064,123.115624213274)) ;
#40596 = CARTESIAN_POINT('Ctrl Pts',(-20.6150653225155,47.2752936478482,123.383560571913)) ;
#40597 = CARTESIAN_POINT('Ctrl Pts',(-20.9165166535545,47.0953045674384,123.376507189918)) ;
#40598 = CARTESIAN_POINT('Ctrl Pts',(-20.601300740418,47.2853373868037,123.594262445601)) ;
#40599 = CARTESIAN_POINT('Ctrl Pts',(-20.89930914947,47.1053483063939,123.639884268213)) ;
#40600 = CARTESIAN_POINT('Ctrl Pts',(-20.552687444503,47.2951591353416,123.794940800993)) ;
#40601 = CARTESIAN_POINT('Ctrl Pts',(-20.8385403651115,47.1151700549318,123.890732974472)) ;
#40602 = CARTESIAN_POINT('Ctrl Pts',(-20.4686462395042,47.3051941129514,123.988445576631)) ;
#40603 = CARTESIAN_POINT('Ctrl Pts',(-20.7334869966669,47.1252050325415,124.132613019334)) ;
#40604 = CARTESIAN_POINT('Ctrl Pts',(-20.3519069360569,47.3152190257091,124.163922378538)) ;
#40605 = CARTESIAN_POINT('Ctrl Pts',(-20.5875612970063,47.1352299452993,124.351957946724)) ;
#40606 = CARTESIAN_POINT('Ctrl Pts',(-20.2093112218679,47.3250709688029,124.314143088258)) ;
#40607 = CARTESIAN_POINT('Ctrl Pts',(-20.4093144806354,47.1450818883931,124.539733166046)) ;
#40608 = CARTESIAN_POINT('Ctrl Pts',(-20.0406636984681,47.335061930132,124.439301449808)) ;
#40609 = CARTESIAN_POINT('Ctrl Pts',(-20.198503670169,47.1550728497222,124.696179510647)) ;
#40610 = CARTESIAN_POINT('Ctrl Pts',(-19.8542359453285,47.3449798050004,124.532734343896)) ;
#40611 = CARTESIAN_POINT('Ctrl Pts',(-19.9654674976821,47.1649907245906,124.812968953149)) ;
#40612 = CARTESIAN_POINT('Ctrl Pts',(-19.6522424998238,47.3550083240017,124.593072966075)) ;
#40613 = CARTESIAN_POINT('Ctrl Pts',(-19.7129751029458,47.1750192435918,124.888390135927)) ;
#40614 = CARTESIAN_POINT('Ctrl Pts',(-19.4458515602898,47.3648920027995,124.617180149755)) ;
#40615 = CARTESIAN_POINT('Ctrl Pts',(-19.4549854354242,47.1849029223897,124.918522015766)) ;
#40616 = CARTESIAN_POINT('Ctrl Pts',(-19.2360564520279,47.3748869462393,124.605411359256)) ;
#40617 = CARTESIAN_POINT('Ctrl Pts',(-19.1927415406331,47.1948978658294,124.903808702295)) ;
#40618 = CARTESIAN_POINT('Ctrl Pts',(-19.0309200127824,47.3849138000617,124.556888090555)) ;
#40619 = CARTESIAN_POINT('Ctrl Pts',(-18.9363215273334,47.2049247196518,124.843152452607)) ;
#40620 = CARTESIAN_POINT('Ctrl Pts',(-18.8399600132762,47.3947979644006,124.474930121574)) ;
#40621 = CARTESIAN_POINT('Ctrl Pts',(-18.6976217950218,47.2148088839908,124.740702605939)) ;
#40622 = CARTESIAN_POINT('Ctrl Pts',(-18.6641751096275,47.404786062443,124.360112233341)) ;
#40623 = CARTESIAN_POINT('Ctrl Pts',(-18.4778918250727,47.2247969820332,124.597178175562)) ;
#40624 = CARTESIAN_POINT('Ctrl Pts',(-18.5114500487226,47.4147371689001,124.217101265402)) ;
#40625 = CARTESIAN_POINT('Ctrl Pts',(-18.2869868869879,47.2347480884902,124.41841249346)) ;
#40626 = CARTESIAN_POINT('Ctrl Pts',(-18.3848081572941,47.4247822200682,124.048124629567)) ;
#40627 = CARTESIAN_POINT('Ctrl Pts',(-18.1286864682483,47.2447931396584,124.207190353559)) ;
#40628 = CARTESIAN_POINT('Ctrl Pts',(-18.2910618402465,47.4346439804265,123.86320370385)) ;
#40629 = CARTESIAN_POINT('Ctrl Pts',(-18.0115053674307,47.2546549000167,123.976037450249)) ;
#40630 = CARTESIAN_POINT('Ctrl Pts',(-18.2296126467464,47.4446067972569,123.662969790822)) ;
#40631 = CARTESIAN_POINT('Ctrl Pts',(-17.9346962186419,47.2646177168471,123.725744078464)) ;
#40632 = CARTESIAN_POINT('Ctrl Pts',(-18.2040389740413,47.4546414785377,123.45357433271)) ;
#40633 = CARTESIAN_POINT('Ctrl Pts',(-17.9027315658583,47.2746523981279,123.4639994927)) ;
#40634 = CARTESIAN_POINT('Ctrl Pts',(-18.2146920724958,47.4645265083184,123.246004580245)) ;
#40635 = CARTESIAN_POINT('Ctrl Pts',(-17.9160504866388,47.2845374279086,123.204536864784)) ;
#40636 = CARTESIAN_POINT('Ctrl Pts',(-18.2621069746344,47.4745921017164,123.039809498366)) ;
#40637 = CARTESIAN_POINT('Ctrl Pts',(-17.9753215325258,47.2946030213066,122.946793722873)) ;
#40638 = CARTESIAN_POINT('Ctrl Pts',(-18.3425816794122,47.4844312700779,122.849220328905)) ;
#40639 = CARTESIAN_POINT('Ctrl Pts',(-18.0759175401619,47.3044421896681,122.708557598434)) ;
#40640 = CARTESIAN_POINT('Ctrl Pts',(-18.457201944164,47.4944938678194,122.671444955583)) ;
#40641 = CARTESIAN_POINT('Ctrl Pts',(-18.2191949883695,47.3145047874096,122.486339905926)) ;
#40642 = CARTESIAN_POINT('Ctrl Pts',(-18.5987718864396,47.5043908802264,122.518950167232)) ;
#40643 = CARTESIAN_POINT('Ctrl Pts',(-18.3961596154612,47.3244017998165,122.295722821645)) ;
#40644 = CARTESIAN_POINT('Ctrl Pts',(-18.7648105631557,47.514322202052,122.392374159236)) ;
#40645 = CARTESIAN_POINT('Ctrl Pts',(-18.6037098264128,47.3343331216421,122.137504758637)) ;
#40646 = CARTESIAN_POINT('Ctrl Pts',(-18.9524743880465,47.5243639648065,122.295687498941)) ;
#40647 = CARTESIAN_POINT('Ctrl Pts',(-18.8382907890094,47.3443748843966,122.016648795415)) ;
#40648 = CARTESIAN_POINT('Ctrl Pts',(-19.1509626646768,47.5342521636972,122.233865751707)) ;
#40649 = CARTESIAN_POINT('Ctrl Pts',(-19.0864023365474,47.3542630832873,121.939374027892)) ;
#40650 = CARTESIAN_POINT('Ctrl Pts',(-19.3593042021687,47.544246102297,122.206837954189)) ;
#40651 = CARTESIAN_POINT('Ctrl Pts',(-19.3468297085814,47.3642570218872,121.905591956096)) ;
#40652 = CARTESIAN_POINT('Ctrl Pts',(-19.5680879347369,47.5541869233339,122.216359937286)) ;
#40653 = CARTESIAN_POINT('Ctrl Pts',(-19.6078094898801,47.3741978429241,121.917497147555)) ;
#40654 = CARTESIAN_POINT('Ctrl Pts',(-19.7724614957895,47.5641463056221,122.26180879175)) ;
#40655 = CARTESIAN_POINT('Ctrl Pts',(-19.8632760201086,47.3841572252123,121.974310927334)) ;
#40656 = CARTESIAN_POINT('Ctrl Pts',(-19.966662779158,47.5741440652745,122.342257817906)) ;
#40657 = CARTESIAN_POINT('Ctrl Pts',(-20.106026651874,47.3941549848646,122.074874782369)) ;
#40658 = CARTESIAN_POINT('Ctrl Pts',(-20.1444477349424,47.5841802014768,122.455869269298)) ;
#40659 = CARTESIAN_POINT('Ctrl Pts',(-20.3282563986767,47.4041911210669,122.21689139883)) ;
#40660 = CARTESIAN_POINT('Ctrl Pts',(-20.2971040279646,47.5940309989677,122.595810595244)) ;
#40661 = CARTESIAN_POINT('Ctrl Pts',(-20.5190752000147,47.4140419185579,122.391820347665)) ;
#40662 = CARTESIAN_POINT('Ctrl Pts',(-20.425042108738,47.603991864044,122.761583938118)) ;
#40663 = CARTESIAN_POINT('Ctrl Pts',(-20.6789956607741,47.4240027836341,122.599038838979)) ;
#40664 = CARTESIAN_POINT('Ctrl Pts',(-20.5226996631887,47.6140207316744,122.948455189612)) ;
#40665 = CARTESIAN_POINT('Ctrl Pts',(-20.8010651624345,47.4340316512646,122.832629226819)) ;
#40666 = CARTESIAN_POINT('Ctrl Pts',(-20.5857281504088,47.6239309678108,123.147028040722)) ;
#40667 = CARTESIAN_POINT('Ctrl Pts',(-20.8798481804422,47.443941887401,123.080846336927)) ;
#40668 = CARTESIAN_POINT('Ctrl Pts',(-20.6139336283943,47.6338659211253,123.353984814139)) ;
#40669 = CARTESIAN_POINT('Ctrl Pts',(-20.9151022555058,47.4538768407155,123.339542816452)) ;
#40670 = CARTESIAN_POINT('Ctrl Pts',(-20.605496943485,47.6439068515349,123.564903134672)) ;
#40671 = CARTESIAN_POINT('Ctrl Pts',(-20.9045535939889,47.4639177711251,123.603190650001)) ;
#40672 = CARTESIAN_POINT('Ctrl Pts',(-20.5613779871071,47.6537947483165,123.768050424334)) ;
#40673 = CARTESIAN_POINT('Ctrl Pts',(-20.8494021157821,47.4738056679067,123.85712432545)) ;
#40674 = CARTESIAN_POINT('Ctrl Pts',(-20.4822143423052,47.6637841999752,123.962563095657)) ;
#40675 = CARTESIAN_POINT('Ctrl Pts',(-20.7504449184819,47.4837951195654,124.100264163636)) ;
#40676 = CARTESIAN_POINT('Ctrl Pts',(-20.370678012507,47.6737432903405,124.139744915088)) ;
#40677 = CARTESIAN_POINT('Ctrl Pts',(-20.6110220669894,47.4937542099307,124.321740017051)) ;
#40678 = CARTESIAN_POINT('Ctrl Pts',(-20.2313246232406,47.6836406026468,124.294278132182)) ;
#40679 = CARTESIAN_POINT('Ctrl Pts',(-20.4368281965644,47.503651522237,124.514904688162)) ;
#40680 = CARTESIAN_POINT('Ctrl Pts',(-20.0645809253998,47.6936970285471,124.424226886793)) ;
#40681 = CARTESIAN_POINT('Ctrl Pts',(-20.2283967744632,47.5137079481373,124.677338457661)) ;
#40682 = CARTESIAN_POINT('Ctrl Pts',(-19.8812864921283,47.7035670311368,124.521524514142)) ;
#40683 = CARTESIAN_POINT('Ctrl Pts',(-19.9992773799841,47.523577950727,124.798958001581)) ;
#40684 = CARTESIAN_POINT('Ctrl Pts',(-19.6813729094116,47.7135709643141,124.586772503536)) ;
#40685 = CARTESIAN_POINT('Ctrl Pts',(-19.7493845402338,47.5335818839042,124.880515352812)) ;
#40686 = CARTESIAN_POINT('Ctrl Pts',(-19.4734437265146,47.723558224778,124.616166289177)) ;
#40687 = CARTESIAN_POINT('Ctrl Pts',(-19.489472364039,47.5435691443681,124.917254732938)) ;
#40688 = CARTESIAN_POINT('Ctrl Pts',(-19.2627853496724,47.7335852763637,124.608859964159)) ;
#40689 = CARTESIAN_POINT('Ctrl Pts',(-19.2261503134939,47.5535961959539,124.908119290027)) ;
#40690 = CARTESIAN_POINT('Ctrl Pts',(-19.0593193011781,47.7434763661898,124.565875611357)) ;
#40691 = CARTESIAN_POINT('Ctrl Pts',(-18.9718149570736,47.5634872857799,124.854385043572)) ;
#40692 = CARTESIAN_POINT('Ctrl Pts',(-18.7998791514015,47.7567741209708,124.46180634869)) ;
#40693 = CARTESIAN_POINT('Ctrl Pts',(-18.6475331408363,47.576785040561,124.72430028687)) ;
#40694 = CARTESIAN_POINT('Ctrl Pts',(-18.5749055156603,47.769972180579,124.293953042302)) ;
#40695 = CARTESIAN_POINT('Ctrl Pts',(-18.3663382798693,47.5899831001692,124.514511431448)) ;
#40696 = CARTESIAN_POINT('Ctrl Pts',(-18.4005844763,47.7833689211482,124.072822952987)) ;
#40697 = CARTESIAN_POINT('Ctrl Pts',(-18.1483991887815,47.6033798407383,124.23805464201)) ;
#40698 = CARTESIAN_POINT('Ctrl Pts',(-18.3021342969201,47.7932398332216,123.890089252221)) ;
#40699 = CARTESIAN_POINT('Ctrl Pts',(-18.0253471436318,47.6132507528118,124.009644853033)) ;
#40700 = CARTESIAN_POINT('Ctrl Pts',(-18.2356106700847,47.8033133949897,123.689082460906)) ;
#40701 = CARTESIAN_POINT('Ctrl Pts',(-17.9421929510955,47.6233243145799,123.758382877835)) ;
#40702 = CARTESIAN_POINT('Ctrl Pts',(-18.2055029737511,47.8131348075781,123.484761908509)) ;
#40703 = CARTESIAN_POINT('Ctrl Pts',(-17.9045616883092,47.6331457271682,123.502983370992)) ;
#40704 = CARTESIAN_POINT('Ctrl Pts',(-18.2112771538204,47.8232088248091,123.273106955294)) ;
#40705 = CARTESIAN_POINT('Ctrl Pts',(-17.9117818429639,47.6432197443993,123.238412336135)) ;
#40706 = CARTESIAN_POINT('Ctrl Pts',(-18.2665340735366,47.8363676117737,123.001975829454)) ;
#40707 = CARTESIAN_POINT('Ctrl Pts',(-17.9808569614188,47.6563785313638,122.899509564603)) ;
#40708 = CARTESIAN_POINT('Ctrl Pts',(-18.3927847313785,47.8497337148678,122.747421002799)) ;
#40709 = CARTESIAN_POINT('Ctrl Pts',(-18.138643663301,47.669744634458,122.581350825169)) ;
#40710 = CARTESIAN_POINT('Ctrl Pts',(-18.5783616406369,47.8630476497569,122.537834672679)) ;
#40711 = CARTESIAN_POINT('Ctrl Pts',(-18.3706523157878,47.6830585693471,122.319320691022)) ;
#40712 = CARTESIAN_POINT('Ctrl Pts',(-18.7409869953793,47.8729476892044,122.407978701696)) ;
#40713 = CARTESIAN_POINT('Ctrl Pts',(-18.5739282398192,47.6929586087946,122.157012936073)) ;
#40714 = CARTESIAN_POINT('Ctrl Pts',(-18.924736336014,47.8829120923389,122.307361857159)) ;
#40715 = CARTESIAN_POINT('Ctrl Pts',(-18.803618171693,47.7029230119291,122.031241515274)) ;
#40716 = CARTESIAN_POINT('Ctrl Pts',(-19.124525129965,47.89294205946,122.239917422604)) ;
#40717 = CARTESIAN_POINT('Ctrl Pts',(-19.053353575871,47.7129529790502,121.946938831244)) ;
#40718 = CARTESIAN_POINT('Ctrl Pts',(-19.3303060797298,47.9028443360691,122.20850438304)) ;
#40719 = CARTESIAN_POINT('Ctrl Pts',(-19.310583887986,47.7228552556593,121.907675661844)) ;
#40720 = CARTESIAN_POINT('Ctrl Pts',(-19.6091875472562,47.9161102652382,122.214220010693)) ;
#40721 = CARTESIAN_POINT('Ctrl Pts',(-19.6591650885783,47.7361211848284,121.914819682734)) ;
#40722 = CARTESIAN_POINT('Ctrl Pts',(-19.9485239198388,47.9327317963447,122.312705470027)) ;
#40723 = CARTESIAN_POINT('Ctrl Pts',(-20.0833550247986,47.7527427159348,122.03793050963)) ;
#40724 = CARTESIAN_POINT('Ctrl Pts',(-20.2902037781463,47.9526066249893,122.561462918073)) ;
#40725 = CARTESIAN_POINT('Ctrl Pts',(-20.5104537296024,47.7726175445795,122.348898696979)) ;
#40726 = CARTESIAN_POINT('Ctrl Pts',(-20.4884640691053,47.9692798330912,122.855376240776)) ;
#40727 = CARTESIAN_POINT('Ctrl Pts',(-20.7582479358971,47.7892907526814,122.716231896323)) ;
#40728 = CARTESIAN_POINT('Ctrl Pts',(-20.5789910924744,47.9825309580725,123.118806998675)) ;
#40729 = CARTESIAN_POINT('Ctrl Pts',(-20.8714295869676,47.8025418776626,123.045575912821)) ;
#40730 = CARTESIAN_POINT('Ctrl Pts',(-20.6233964771784,47.9957732768933,123.393706926206)) ;
#40731 = CARTESIAN_POINT('Ctrl Pts',(-20.9269298435313,47.8157841964835,123.38917831621)) ;
#40732 = CARTESIAN_POINT('Ctrl Pts',(-20.5867718231029,48.0125065172328,123.747531507057)) ;
#40733 = CARTESIAN_POINT('Ctrl Pts',(-20.8811455204018,47.8325174368229,123.83147612068)) ;
#40734 = CARTESIAN_POINT('Ctrl Pts',(-20.4028036698389,48.0323356654207,124.126994342041)) ;
#40735 = CARTESIAN_POINT('Ctrl Pts',(-20.6511822087016,47.8523465850109,124.305796219688)) ;
#40736 = CARTESIAN_POINT('Ctrl Pts',(-20.0997742547527,48.0522603605214,124.422927439283)) ;
#40737 = CARTESIAN_POINT('Ctrl Pts',(-20.2723934902677,47.8722712801115,124.67571100162)) ;
#40738 = CARTESIAN_POINT('Ctrl Pts',(-19.7138146747958,48.0721835891048,124.597703149849)) ;
#40739 = CARTESIAN_POINT('Ctrl Pts',(-19.789943257648,47.892194508695,124.894176873647)) ;
#40740 = CARTESIAN_POINT('Ctrl Pts',(-19.2914240334227,48.0921107282309,124.630406193651)) ;
#40741 = CARTESIAN_POINT('Ctrl Pts',(-19.2619554888024,47.9121216478211,124.935052545487)) ;
#40742 = CARTESIAN_POINT('Ctrl Pts',(-18.8840463674362,48.1119871908466,124.517801066557)) ;
#40743 = CARTESIAN_POINT('Ctrl Pts',(-18.7527354696234,47.9319981104368,124.794293876261)) ;
#40744 = CARTESIAN_POINT('Ctrl Pts',(-18.5376979877752,48.1319644194519,124.271899046843)) ;
#40745 = CARTESIAN_POINT('Ctrl Pts',(-18.3198015892521,47.9519753390421,124.486914551097)) ;
#40746 = CARTESIAN_POINT('Ctrl Pts',(-18.2968188645784,48.1518992774256,123.923081812922)) ;
#40747 = CARTESIAN_POINT('Ctrl Pts',(-18.0187050937589,47.9719101970158,124.050892286843)) ;
#40748 = CARTESIAN_POINT('Ctrl Pts',(-18.1892385120565,48.1717957263564,123.513969714441)) ;
#40749 = CARTESIAN_POINT('Ctrl Pts',(-17.8842318765128,47.9918066459466,123.539502996673)) ;
#40750 = CARTESIAN_POINT('Ctrl Pts',(-18.2273051805781,48.191717010423,123.092084857011)) ;
#40751 = CARTESIAN_POINT('Ctrl Pts',(-17.931816529744,48.0117279300131,123.01214812022)) ;
#40752 = CARTESIAN_POINT('Ctrl Pts',(-18.4074959386059,48.2116736600939,122.707887148316)) ;
#40753 = CARTESIAN_POINT('Ctrl Pts',(-18.1570558911113,48.0316845796841,122.531902035384)) ;
#40754 = CARTESIAN_POINT('Ctrl Pts',(-18.7066336703321,48.2315509532055,122.409391624937)) ;
#40755 = CARTESIAN_POINT('Ctrl Pts',(-18.5309774064704,48.0515618727957,122.158784664418)) ;
#40756 = CARTESIAN_POINT('Ctrl Pts',(-19.0894690754,48.251437425434,122.229752123671)) ;
#40757 = CARTESIAN_POINT('Ctrl Pts',(-19.0095199143014,48.0714483450242,121.934235959728)) ;
#40758 = CARTESIAN_POINT('Ctrl Pts',(-19.5143590700572,48.271498991358,122.191844649005)) ;
#40759 = CARTESIAN_POINT('Ctrl Pts',(-19.5406334938979,48.0915099109482,121.886851609372)) ;
#40760 = CARTESIAN_POINT('Ctrl Pts',(-19.9220000869853,48.2913393988987,122.300380775824)) ;
#40761 = CARTESIAN_POINT('Ctrl Pts',(-20.0501821768605,48.1113503184889,122.022521216155)) ;
#40762 = CARTESIAN_POINT('Ctrl Pts',(-20.2693591113835,48.3111907228717,122.540208509566)) ;
#40763 = CARTESIAN_POINT('Ctrl Pts',(-20.484379980263,48.1312016424618,122.322303458177)) ;
#40764 = CARTESIAN_POINT('Ctrl Pts',(-20.515946924029,48.3312439928231,122.887990451022)) ;
#40765 = CARTESIAN_POINT('Ctrl Pts',(-20.7926161665068,48.1512549124133,122.757030819411)) ;
#40766 = CARTESIAN_POINT('Ctrl Pts',(-20.6278740447954,48.3510646502064,123.29441743572)) ;
#40767 = CARTESIAN_POINT('Ctrl Pts',(-20.9325258350394,48.1710755697966,123.265061844728)) ;
#40768 = CARTESIAN_POINT('Ctrl Pts',(-20.594840913384,48.3710360715369,123.717637162342)) ;
#40769 = CARTESIAN_POINT('Ctrl Pts',(-20.8912365983852,48.1910469911271,123.794086280591)) ;
#40770 = CARTESIAN_POINT('Ctrl Pts',(-20.4200275936189,48.3909295639006,124.102979449163)) ;
#40771 = CARTESIAN_POINT('Ctrl Pts',(-20.6727225903165,48.2109404834908,124.275764014149)) ;
#40772 = CARTESIAN_POINT('Ctrl Pts',(-20.1222338289871,48.4109536501417,124.407148329069)) ;
#40773 = CARTESIAN_POINT('Ctrl Pts',(-20.3004819425232,48.2309645697319,124.655976968118)) ;
#40774 = CARTESIAN_POINT('Ctrl Pts',(-19.7426972067717,48.4307585292546,124.589684508702)) ;
#40775 = CARTESIAN_POINT('Ctrl Pts',(-19.8260643109715,48.2507694488447,124.884148701438)) ;
#40776 = CARTESIAN_POINT('Ctrl Pts',(-19.3205665484207,48.4507175449524,124.633213336041)) ;
#40777 = CARTESIAN_POINT('Ctrl Pts',(-19.2984016894082,48.2707284645426,124.938563164656)) ;
#40778 = CARTESIAN_POINT('Ctrl Pts',(-18.9085978348677,48.4707035685815,124.528976750497)) ;
#40779 = CARTESIAN_POINT('Ctrl Pts',(-18.7834401752253,48.2907144881717,124.808270536244)) ;
#40780 = CARTESIAN_POINT('Ctrl Pts',(-18.5595521592662,48.490512064342,124.293192736646)) ;
#40781 = CARTESIAN_POINT('Ctrl Pts',(-18.347132448287,48.3105229839322,124.513544556364)) ;
#40782 = CARTESIAN_POINT('Ctrl Pts',(-18.3093912570992,48.5104947034476,123.949871011709)) ;
#40783 = CARTESIAN_POINT('Ctrl Pts',(-18.0344280932118,48.3305056230378,124.084394876758)) ;
#40784 = CARTESIAN_POINT('Ctrl Pts',(-18.1920511017376,48.5303761512416,123.543638375906)) ;
#40785 = CARTESIAN_POINT('Ctrl Pts',(-17.8877491678814,48.3503870708318,123.576606049557)) ;
#40786 = CARTESIAN_POINT('Ctrl Pts',(-18.2201380169056,48.5503326179791,123.120331661826)) ;
#40787 = CARTESIAN_POINT('Ctrl Pts',(-17.9228534216477,48.3703435375693,123.047472668658)) ;
#40788 = CARTESIAN_POINT('Ctrl Pts',(-18.3901149333137,48.5702100149347,122.733295429989)) ;
#40789 = CARTESIAN_POINT('Ctrl Pts',(-18.135320026782,48.3902209345249,122.563676201038)) ;
#40790 = CARTESIAN_POINT('Ctrl Pts',(-18.6832494392057,48.59019196111,122.425805232135)) ;
#40791 = CARTESIAN_POINT('Ctrl Pts',(-18.5017348374679,48.4102028807002,122.179310317694)) ;
#40792 = CARTESIAN_POINT('Ctrl Pts',(-19.0629244099466,48.6101210601467,122.237437305555)) ;
#40793 = CARTESIAN_POINT('Ctrl Pts',(-18.9763255338621,48.4301319797369,121.943845821866)) ;
#40794 = CARTESIAN_POINT('Ctrl Pts',(-19.483901793505,48.6300496833594,122.189890024133)) ;
#40795 = CARTESIAN_POINT('Ctrl Pts',(-19.5025485758223,48.4500606029495,121.88440856262)) ;
#40796 = CARTESIAN_POINT('Ctrl Pts',(-19.8941924839498,48.6498840074658,122.2876543526)) ;
#40797 = CARTESIAN_POINT('Ctrl Pts',(-20.0154041734729,48.469894927056,122.006602474258)) ;
#40798 = CARTESIAN_POINT('Ctrl Pts',(-20.1900657132766,48.6665362948492,122.481970833508)) ;
#40799 = CARTESIAN_POINT('Ctrl Pts',(-20.3852740340887,48.4865472144393,122.249514009175)) ;
#40800 = CARTESIAN_POINT('Ctrl Pts',(-20.375507427574,48.6797967958714,122.690222552236)) ;
#40801 = CARTESIAN_POINT('Ctrl Pts',(-20.6170557320591,48.4998077154616,122.509808729573)) ;
#40802 = CARTESIAN_POINT('Ctrl Pts',(-20.4862754015006,48.6897982730727,122.868932780703)) ;
#40803 = CARTESIAN_POINT('Ctrl Pts',(-20.7555225669934,48.5098091926629,122.733198872914)) ;
#40804 = CARTESIAN_POINT('Ctrl Pts',(-20.5642475378503,48.6998302939322,123.064902655755)) ;
#40805 = CARTESIAN_POINT('Ctrl Pts',(-20.8529891979542,48.5198412135224,122.978158629143)) ;
#40806 = CARTESIAN_POINT('Ctrl Pts',(-20.6065360548538,48.7096938376577,123.267899186555)) ;
#40807 = CARTESIAN_POINT('Ctrl Pts',(-20.905851938362,48.5297047572479,123.231906669107)) ;
#40808 = CARTESIAN_POINT('Ctrl Pts',(-20.6135560240591,48.7196625513279,123.477368148513)) ;
#40809 = CARTESIAN_POINT('Ctrl Pts',(-20.9146324102644,48.539673470918,123.493731289985)) ;
#40810 = CARTESIAN_POINT('Ctrl Pts',(-20.5737423786962,48.7330082987316,123.755033330118)) ;
#40811 = CARTESIAN_POINT('Ctrl Pts',(-20.8648547232343,48.5530192183217,123.840870176968)) ;
#40812 = CARTESIAN_POINT('Ctrl Pts',(-20.4644055794944,48.7461588538042,124.012444095883)) ;
#40813 = CARTESIAN_POINT('Ctrl Pts',(-20.7281894338914,48.5661697733944,124.16259745945)) ;
#40814 = CARTESIAN_POINT('Ctrl Pts',(-20.2913023971137,48.7595442343541,124.234297005858)) ;
#40815 = CARTESIAN_POINT('Ctrl Pts',(-20.5118249049467,48.5795551539443,124.43990359673)) ;
#40816 = CARTESIAN_POINT('Ctrl Pts',(-20.1368920609285,48.7694321703469,124.373504586034)) ;
#40817 = CARTESIAN_POINT('Ctrl Pts',(-20.3188115906688,48.5894430899371,124.613917552895)) ;
#40818 = CARTESIAN_POINT('Ctrl Pts',(-19.9590459239484,48.7794233601596,124.485212508452)) ;
#40819 = CARTESIAN_POINT('Ctrl Pts',(-20.0965059872055,48.5994342797498,124.753554193892)) ;
#40820 = CARTESIAN_POINT('Ctrl Pts',(-19.7652457599506,48.7893754586979,124.564139501548)) ;
#40821 = CARTESIAN_POINT('Ctrl Pts',(-19.8542566549594,48.6093863782881,124.852215716906)) ;
#40822 = CARTESIAN_POINT('Ctrl Pts',(-19.5587662011907,48.7994217151483,124.608490141116)) ;
#40823 = CARTESIAN_POINT('Ctrl Pts',(-19.5961577410674,48.6194326347385,124.907656726874)) ;
#40824 = CARTESIAN_POINT('Ctrl Pts',(-19.3518437628438,48.8092711625425,124.616313912249)) ;
#40825 = CARTESIAN_POINT('Ctrl Pts',(-19.3375048370033,48.6292820821327,124.917439257237)) ;
#40826 = CARTESIAN_POINT('Ctrl Pts',(-19.1442698754285,48.8192338150376,124.588420325865)) ;
#40827 = CARTESIAN_POINT('Ctrl Pts',(-19.0780370222547,48.6392447346278,124.882575057836)) ;
#40828 = CARTESIAN_POINT('Ctrl Pts',(-18.9435612342431,48.8292569006798,124.52425240661)) ;
#40829 = CARTESIAN_POINT('Ctrl Pts',(-18.8271502999085,48.64926782027,124.802367820809)) ;
#40830 = CARTESIAN_POINT('Ctrl Pts',(-18.7587343657275,48.8391820164367,124.427368142674)) ;
#40831 = CARTESIAN_POINT('Ctrl Pts',(-18.5961153422088,48.6591929360269,124.681264951372)) ;
#40832 = CARTESIAN_POINT('Ctrl Pts',(-18.5915035853904,48.8492344948365,124.298186724899)) ;
#40833 = CARTESIAN_POINT('Ctrl Pts',(-18.3870750955286,48.6692454144267,124.519790373275)) ;
#40834 = CARTESIAN_POINT('Ctrl Pts',(-18.4519608110317,48.8590859935392,124.14512278795)) ;
#40835 = CARTESIAN_POINT('Ctrl Pts',(-18.2126444693524,48.6790969131294,124.328462267101)) ;
#40836 = CARTESIAN_POINT('Ctrl Pts',(-18.3393227852187,48.8690577327418,123.968347894014)) ;
#40837 = CARTESIAN_POINT('Ctrl Pts',(-18.0718445075034,48.6890686523319,124.107495060941)) ;
#40838 = CARTESIAN_POINT('Ctrl Pts',(-18.2589016789919,48.8790529405074,123.774178747308)) ;
#40839 = CARTESIAN_POINT('Ctrl Pts',(-17.9713155068526,48.6990638600976,123.864784625914)) ;
#40840 = CARTESIAN_POINT('Ctrl Pts',(-18.2135023400313,48.8890869419765,123.568194672117)) ;
#40841 = CARTESIAN_POINT('Ctrl Pts',(-17.9145635741689,48.7090978615667,123.60730509988)) ;
#40842 = CARTESIAN_POINT('Ctrl Pts',(-18.2043860504649,48.8989423000689,123.361183900461)) ;
#40843 = CARTESIAN_POINT('Ctrl Pts',(-17.9031654068382,48.7189532196591,123.348541528171)) ;
#40844 = CARTESIAN_POINT('Ctrl Pts',(-18.2314583491406,48.9089417756622,123.152751792762)) ;
#40845 = CARTESIAN_POINT('Ctrl Pts',(-17.9370030265892,48.7289526952524,123.08800094487)) ;
#40846 = CARTESIAN_POINT('Ctrl Pts',(-18.2934466731116,48.9188362241573,122.954149298326)) ;
#40847 = CARTESIAN_POINT('Ctrl Pts',(-18.0144858730906,48.7388471437475,122.839746756347)) ;
#40848 = CARTESIAN_POINT('Ctrl Pts',(-18.3906263668652,48.928899348385,122.766272454152)) ;
#40849 = CARTESIAN_POINT('Ctrl Pts',(-18.1359580111579,48.7489102679752,122.604899456837)) ;
#40850 = CARTESIAN_POINT('Ctrl Pts',(-18.5159623132325,48.9387389747136,122.601663674346)) ;
#40851 = CARTESIAN_POINT('Ctrl Pts',(-18.2926260056049,48.7587498943038,122.399136493394)) ;
#40852 = CARTESIAN_POINT('Ctrl Pts',(-18.6712011618515,48.9488022097566,122.457974021879)) ;
#40853 = CARTESIAN_POINT('Ctrl Pts',(-18.4866726839384,48.7688131293468,122.219522458064)) ;
#40854 = CARTESIAN_POINT('Ctrl Pts',(-18.8461785268419,48.9586962149906,122.345468773217)) ;
#40855 = CARTESIAN_POINT('Ctrl Pts',(-18.7053931822767,48.7787071345808,122.078888414261)) ;
#40856 = CARTESIAN_POINT('Ctrl Pts',(-19.038712835581,48.9686389282064,122.264147456417)) ;
#40857 = CARTESIAN_POINT('Ctrl Pts',(-18.9460602718155,48.7886498477966,121.977234200154)) ;
#40858 = CARTESIAN_POINT('Ctrl Pts',(-19.2437694434536,48.9786446680046,122.217145600225)) ;
#40859 = CARTESIAN_POINT('Ctrl Pts',(-19.2023805081948,48.7986555875947,121.918479266263)) ;
#40860 = CARTESIAN_POINT('Ctrl Pts',(-19.4541758562915,48.988665570151,122.206684633886)) ;
#40861 = CARTESIAN_POINT('Ctrl Pts',(-19.4653884139516,48.8086764897411,121.905400359925)) ;
#40862 = CARTESIAN_POINT('Ctrl Pts',(-19.6605286713295,48.9985563401998,122.232339508242)) ;
#40863 = CARTESIAN_POINT('Ctrl Pts',(-19.7233301714407,48.81856725979,121.937466358533)) ;
#40864 = CARTESIAN_POINT('Ctrl Pts',(-19.8613941607014,49.0085477509796,122.29375208743)) ;
#40865 = CARTESIAN_POINT('Ctrl Pts',(-19.9744129235996,48.8285586705698,122.014229612628)) ;
#40866 = CARTESIAN_POINT('Ctrl Pts',(-20.0477097453618,49.0184960966441,122.388760410401)) ;
#40867 = CARTESIAN_POINT('Ctrl Pts',(-20.207308842741,48.8385070162342,122.132987793713)) ;
#40868 = CARTESIAN_POINT('Ctrl Pts',(-20.2149235430791,49.0284409547052,122.514293134598)) ;
#40869 = CARTESIAN_POINT('Ctrl Pts',(-20.4163278634492,48.8484518742954,122.28990183288)) ;
#40870 = CARTESIAN_POINT('Ctrl Pts',(-20.3591274679965,49.0384957900982,122.668825290875)) ;
#40871 = CARTESIAN_POINT('Ctrl Pts',(-20.596584606347,48.8585067096884,122.483065165186)) ;
#40872 = CARTESIAN_POINT('Ctrl Pts',(-20.4719672533018,49.0483181621996,122.841786669687)) ;
#40873 = CARTESIAN_POINT('Ctrl Pts',(-20.7376368969184,48.8683290817898,122.699266149555)) ;
#40874 = CARTESIAN_POINT('Ctrl Pts',(-20.5553257636715,49.0583740296434,123.036047834246)) ;
#40875 = CARTESIAN_POINT('Ctrl Pts',(-20.841837268975,48.8783849492335,122.942091527924)) ;
#40876 = CARTESIAN_POINT('Ctrl Pts',(-20.6027766814193,49.0683147595013,123.239583217983)) ;
#40877 = CARTESIAN_POINT('Ctrl Pts',(-20.901153475683,48.8883256790915,123.196510502695)) ;
#40878 = CARTESIAN_POINT('Ctrl Pts',(-20.6147759350692,49.0782190980524,123.447461236143)) ;
#40879 = CARTESIAN_POINT('Ctrl Pts',(-20.9161549877404,48.8982300176426,123.456358415648)) ;
#40880 = CARTESIAN_POINT('Ctrl Pts',(-20.5900184388483,49.0882657794809,123.657200174385)) ;
#40881 = CARTESIAN_POINT('Ctrl Pts',(-20.8852105593399,48.9082766990711,123.718532273729)) ;
#40882 = CARTESIAN_POINT('Ctrl Pts',(-20.5303023151086,49.0981612869501,123.856515276786)) ;
#40883 = CARTESIAN_POINT('Ctrl Pts',(-20.8105675406621,48.9181722065403,123.967677397278)) ;
#40884 = CARTESIAN_POINT('Ctrl Pts',(-20.4353377015861,49.1082235554488,124.045507278438)) ;
#40885 = CARTESIAN_POINT('Ctrl Pts',(-20.6918640067606,48.9282344750389,124.203918318758)) ;
#40886 = CARTESIAN_POINT('Ctrl Pts',(-20.3118353609742,49.1180655457194,124.211547456422)) ;
#40887 = CARTESIAN_POINT('Ctrl Pts',(-20.5374874733273,48.9380764653096,124.411470652652)) ;
#40888 = CARTESIAN_POINT('Ctrl Pts',(-20.1594306056428,49.1280589626003,124.356110189049)) ;
#40889 = CARTESIAN_POINT('Ctrl Pts',(-20.3469829663969,48.9480698821905,124.592175832541)) ;
#40890 = CARTESIAN_POINT('Ctrl Pts',(-19.9854133922224,49.1379834504525,124.471260343078)) ;
#40891 = CARTESIAN_POINT('Ctrl Pts',(-20.1294622772361,48.9579943700427,124.736115686186)) ;
#40892 = CARTESIAN_POINT('Ctrl Pts',(-19.7927208813877,49.147983084361,124.555263507083)) ;
#40893 = CARTESIAN_POINT('Ctrl Pts',(-19.8885974147737,48.9679940039512,124.841121711995)) ;
#40894 = CARTESIAN_POINT('Ctrl Pts',(-19.5886002486788,49.1579691946177,124.604484612063)) ;
#40895 = CARTESIAN_POINT('Ctrl Pts',(-19.6334469697775,48.9779801142079,124.902650275678)) ;
#40896 = CARTESIAN_POINT('Ctrl Pts',(-19.3780258214189,49.1680051458049,124.617357030462)) ;
#40897 = CARTESIAN_POINT('Ctrl Pts',(-19.3702291570115,48.9880160653951,124.918743054882)) ;
#40898 = CARTESIAN_POINT('Ctrl Pts',(-19.1720854488287,49.1778617841397,124.594203709604)) ;
#40899 = CARTESIAN_POINT('Ctrl Pts',(-19.1128025382684,48.9978727037298,124.889803469865)) ;
#40900 = CARTESIAN_POINT('Ctrl Pts',(-18.9703969120688,49.1878607442177,124.535088681931)) ;
#40901 = CARTESIAN_POINT('Ctrl Pts',(-18.8606911455378,49.0078716638079,124.815911669499)) ;
#40902 = CARTESIAN_POINT('Ctrl Pts',(-18.7838271969103,49.1977559745315,124.442990126703)) ;
#40903 = CARTESIAN_POINT('Ctrl Pts',(-18.6274774419771,49.0177668941216,124.700789980543)) ;
#40904 = CARTESIAN_POINT('Ctrl Pts',(-18.6133446048038,49.2078164870001,124.317858094273)) ;
#40905 = CARTESIAN_POINT('Ctrl Pts',(-18.4143731817595,49.0278274065903,124.544376734634)) ;
#40906 = CARTESIAN_POINT('Ctrl Pts',(-18.470133520923,49.2176657785463,124.168284568055)) ;
#40907 = CARTESIAN_POINT('Ctrl Pts',(-18.235357152959,49.0376766981364,124.35741046968)) ;
#40908 = CARTESIAN_POINT('Ctrl Pts',(-18.3525585485733,49.2276929644785,123.993322107595)) ;
#40909 = CARTESIAN_POINT('Ctrl Pts',(-18.0883869154399,49.0477038840687,124.138708462397)) ;
#40910 = CARTESIAN_POINT('Ctrl Pts',(-18.2676375468135,49.2377215009378,123.800338049473)) ;
#40911 = CARTESIAN_POINT('Ctrl Pts',(-17.9822338382252,49.057732420528,123.897479268206)) ;
#40912 = CARTESIAN_POINT('Ctrl Pts',(-18.2180547672955,49.2475667409028,123.599398819481)) ;
#40913 = CARTESIAN_POINT('Ctrl Pts',(-17.920253245843,49.067577660493,123.646304603667)) ;
#40914 = CARTESIAN_POINT('Ctrl Pts',(-18.2033462478986,49.257557435826,123.389873464327)) ;
#40915 = CARTESIAN_POINT('Ctrl Pts',(-17.9018658551687,49.0775683554161,123.384397836006)) ;
#40916 = CARTESIAN_POINT('Ctrl Pts',(-18.2258094823577,49.2675952565846,123.180046491113)) ;
#40917 = CARTESIAN_POINT('Ctrl Pts',(-17.9299430169483,49.0876061761748,123.122114050763)) ;
#40918 = CARTESIAN_POINT('Ctrl Pts',(-18.282899951332,49.2774398503615,122.981108060184)) ;
#40919 = CARTESIAN_POINT('Ctrl Pts',(-18.0013047262226,49.0974507699517,122.873439403383)) ;
#40920 = CARTESIAN_POINT('Ctrl Pts',(-18.3745381888825,49.2874238457376,122.792294663389)) ;
#40921 = CARTESIAN_POINT('Ctrl Pts',(-18.1158511804097,49.1074347653277,122.637421711122)) ;
#40922 = CARTESIAN_POINT('Ctrl Pts',(-18.4971732872616,49.297372894299,122.622845943854)) ;
#40923 = CARTESIAN_POINT('Ctrl Pts',(-18.2691440174717,49.1173838138892,122.42560946912)) ;
#40924 = CARTESIAN_POINT('Ctrl Pts',(-18.6480139790816,49.3073753332735,122.476322024514)) ;
#40925 = CARTESIAN_POINT('Ctrl Pts',(-18.4576938725273,49.1273862528637,122.242453382351)) ;
#40926 = CARTESIAN_POINT('Ctrl Pts',(-18.8224872342568,49.3173965745699,122.358233047741)) ;
#40927 = CARTESIAN_POINT('Ctrl Pts',(-18.6757844900772,49.1374074941601,122.09484081394)) ;
#40928 = CARTESIAN_POINT('Ctrl Pts',(-19.0122435632454,49.3272892530094,122.273107300004)) ;
#40929 = CARTESIAN_POINT('Ctrl Pts',(-18.9129800736581,49.1473001725995,121.988431832864)) ;
#40930 = CARTESIAN_POINT('Ctrl Pts',(-19.2157981994734,49.337279306957,122.221395750134)) ;
#40931 = CARTESIAN_POINT('Ctrl Pts',(-19.1674232251386,49.1572902265472,121.92379093172)) ;
#40932 = CARTESIAN_POINT('Ctrl Pts',(-19.4245809336143,49.3472376681055,122.206012139912)) ;
#40933 = CARTESIAN_POINT('Ctrl Pts',(-19.4284019621505,49.1672485876957,121.904559887183)) ;
#40934 = CARTESIAN_POINT('Ctrl Pts',(-19.6317061321161,49.3571372949903,122.226481358477)) ;
#40935 = CARTESIAN_POINT('Ctrl Pts',(-19.6873094647,49.1771482145805,121.930145178701)) ;
#40936 = CARTESIAN_POINT('Ctrl Pts',(-19.8350793181158,49.3671851917937,122.283506518214)) ;
#40937 = CARTESIAN_POINT('Ctrl Pts',(-19.9415261026208,49.1871961113839,122.001425268256)) ;
#40938 = CARTESIAN_POINT('Ctrl Pts',(-20.0226907344885,49.3770805494297,122.373464971147)) ;
#40939 = CARTESIAN_POINT('Ctrl Pts',(-20.1760417540459,49.1970914690199,122.113872563155)) ;
#40940 = CARTESIAN_POINT('Ctrl Pts',(-20.1946471925884,49.3871422018863,122.496611414451)) ;
#40941 = CARTESIAN_POINT('Ctrl Pts',(-20.390987809778,49.2071531214765,122.267804384086)) ;
#40942 = CARTESIAN_POINT('Ctrl Pts',(-20.3394609229976,49.3969868061583,122.644483147191)) ;
#40943 = CARTESIAN_POINT('Ctrl Pts',(-20.5720068054178,49.2169977257485,122.452644101935)) ;
#40944 = CARTESIAN_POINT('Ctrl Pts',(-20.4583844624104,49.4069469278563,122.816823206098)) ;
#40945 = CARTESIAN_POINT('Ctrl Pts',(-20.7206623097911,49.2269578474465,122.668068984901)) ;
#40946 = CARTESIAN_POINT('Ctrl Pts',(-20.5458863827844,49.4169849622188,123.008849967238)) ;
#40947 = CARTESIAN_POINT('Ctrl Pts',(-20.8300406887317,49.236995881809,122.908101813683)) ;
#40948 = CARTESIAN_POINT('Ctrl Pts',(-20.5982321140661,49.4268592748053,123.209757190274)) ;
#40949 = CARTESIAN_POINT('Ctrl Pts',(-20.8954741072966,49.2468701943954,123.159236671897)) ;
#40950 = CARTESIAN_POINT('Ctrl Pts',(-20.6152137828225,49.436928755588,123.420738615319)) ;
#40951 = CARTESIAN_POINT('Ctrl Pts',(-20.9167021697112,49.2569396751782,123.422962968095)) ;
#40952 = CARTESIAN_POINT('Ctrl Pts',(-20.5958761668654,49.4467630916051,123.62659808383)) ;
#40953 = CARTESIAN_POINT('Ctrl Pts',(-20.8925309749188,49.2667740111952,123.680288852966)) ;
#40954 = CARTESIAN_POINT('Ctrl Pts',(-20.540545363407,49.4567960493333,123.83012921168)) ;
#40955 = CARTESIAN_POINT('Ctrl Pts',(-20.8233682240622,49.2768069689235,123.934702843871)) ;
#40956 = CARTESIAN_POINT('Ctrl Pts',(-20.4502978778667,49.4668164479085,124.020482337261)) ;
#40957 = CARTESIAN_POINT('Ctrl Pts',(-20.7105597645197,49.2868273674987,124.17264463345)) ;
#40958 = CARTESIAN_POINT('Ctrl Pts',(-20.3306741561224,49.4766820216797,124.189933002317)) ;
#40959 = CARTESIAN_POINT('Ctrl Pts',(-20.5610300421518,49.2966929412699,124.3844593966)) ;
#40960 = CARTESIAN_POINT('Ctrl Pts',(-20.1804401966572,49.4867508963358,124.339026315722)) ;
#40961 = CARTESIAN_POINT('Ctrl Pts',(-20.3732384290745,49.306761815926,124.570826297065)) ;
#40962 = CARTESIAN_POINT('Ctrl Pts',(-20.0104505357021,49.4965963272413,124.45713399561)) ;
#40963 = CARTESIAN_POINT('Ctrl Pts',(-20.1607506292754,49.3166072468315,124.718462326093)) ;
#40964 = CARTESIAN_POINT('Ctrl Pts',(-19.8202741615974,49.506575952112,124.545721379773)) ;
#40965 = CARTESIAN_POINT('Ctrl Pts',(-19.9230300882305,49.3265868717022,124.82919713631)) ;
#40966 = CARTESIAN_POINT('Ctrl Pts',(-19.6167083846425,49.5165946350261,124.599768391812)) ;
#40967 = CARTESIAN_POINT('Ctrl Pts',(-19.6685730451503,49.3366055546162,124.896756529941)) ;
#40968 = CARTESIAN_POINT('Ctrl Pts',(-19.4096938931667,49.5264779002099,124.617848281754)) ;
#40969 = CARTESIAN_POINT('Ctrl Pts',(-19.4098038796016,49.3464888198001,124.919356964581)) ;
#40970 = CARTESIAN_POINT('Ctrl Pts',(-19.198877107358,49.5365461943013,124.599282994167)) ;
#40971 = CARTESIAN_POINT('Ctrl Pts',(-19.1462832607575,49.3565571138914,124.896150905587)) ;
#40972 = CARTESIAN_POINT('Ctrl Pts',(-18.9991919639653,49.5463763244866,124.54591031217)) ;
#40973 = CARTESIAN_POINT('Ctrl Pts',(-18.8966752356314,49.3663872440768,124.829435060351)) ;
#40974 = CARTESIAN_POINT('Ctrl Pts',(-18.8072474578189,49.5564428727018,124.456856220617)) ;
#40975 = CARTESIAN_POINT('Ctrl Pts',(-18.6567448317127,49.3764537922919,124.71811789698)) ;
#40976 = CARTESIAN_POINT('Ctrl Pts',(-18.6367469946914,49.5663331213904,124.337807634366)) ;
#40977 = CARTESIAN_POINT('Ctrl Pts',(-18.4436181844435,49.3863440409805,124.569306863468)) ;
#40978 = CARTESIAN_POINT('Ctrl Pts',(-18.4876920453678,49.5763253031664,124.189801919102)) ;
#40979 = CARTESIAN_POINT('Ctrl Pts',(-18.2572992165768,49.3963362227566,124.384299698953)) ;
#40980 = CARTESIAN_POINT('Ctrl Pts',(-18.3671123398386,49.5862880837942,124.018548544852)) ;
#40981 = CARTESIAN_POINT('Ctrl Pts',(-18.1065741068912,49.4062990033844,124.170232758751)) ;
#40982 = CARTESIAN_POINT('Ctrl Pts',(-18.2781412601889,49.5961924884679,123.830276313694)) ;
#40983 = CARTESIAN_POINT('Ctrl Pts',(-17.9953598076436,49.4162034080581,123.934891647495)) ;
#40984 = CARTESIAN_POINT('Ctrl Pts',(-18.222510202651,49.606252482947,123.626250710745)) ;
#40985 = CARTESIAN_POINT('Ctrl Pts',(-17.9258209626991,49.4262634025372,123.67985999985)) ;
#40986 = CARTESIAN_POINT('Ctrl Pts',(-18.203376410996,49.6161011049168,123.420072742586)) ;
#40987 = CARTESIAN_POINT('Ctrl Pts',(-17.9019035488752,49.436112024507,123.422136143484)) ;
#40988 = CARTESIAN_POINT('Ctrl Pts',(-18.2201708403545,49.6261315443286,123.209883238116)) ;
#40989 = CARTESIAN_POINT('Ctrl Pts',(-17.9228967150364,49.4461424639188,123.159399391349)) ;
#40990 = CARTESIAN_POINT('Ctrl Pts',(-18.2735161472999,49.6361412599634,123.00629722832)) ;
#40991 = CARTESIAN_POINT('Ctrl Pts',(-17.9895783324889,49.4561521795535,122.904916831254)) ;
#40992 = CARTESIAN_POINT('Ctrl Pts',(-18.3603293584098,49.646052012656,122.816911028997)) ;
#40993 = CARTESIAN_POINT('Ctrl Pts',(-18.0980952654857,49.4660629322462,122.66818328543)) ;
#40994 = CARTESIAN_POINT('Ctrl Pts',(-18.4785136980993,49.6559812856024,122.644833121426)) ;
#40995 = CARTESIAN_POINT('Ctrl Pts',(-18.2458263260203,49.4759922051926,122.453085432512)) ;
#40996 = CARTESIAN_POINT('Ctrl Pts',(-18.6265668723548,49.666023976995,122.494326841967)) ;
#40997 = CARTESIAN_POINT('Ctrl Pts',(-18.4308927790362,49.4860348965852,122.264952869132)) ;
#40998 = CARTESIAN_POINT('Ctrl Pts',(-18.7957677209067,49.6759105102126,122.373596637961)) ;
#40999 = CARTESIAN_POINT('Ctrl Pts',(-18.6423948660531,49.4959214298028,122.114039679002)) ;
#41000 = CARTESIAN_POINT('Ctrl Pts',(-18.985209711551,49.6859036551446,122.282802300609)) ;
#41001 = CARTESIAN_POINT('Ctrl Pts',(-18.8791977037607,49.5059145747348,122.00054701503)) ;
#41002 = CARTESIAN_POINT('Ctrl Pts',(-19.1866107318813,49.6958493359811,122.226622842635)) ;
#41003 = CARTESIAN_POINT('Ctrl Pts',(-19.1309496466669,49.5158602555713,121.93032286987)) ;
#41004 = CARTESIAN_POINT('Ctrl Pts',(-19.3947080629283,49.7057965931296,122.205836498686)) ;
#41005 = CARTESIAN_POINT('Ctrl Pts',(-19.391071934028,49.5258075127198,121.904340399556)) ;
#41006 = CARTESIAN_POINT('Ctrl Pts',(-19.6053289184389,49.7158444970016,122.221892340969)) ;
#41007 = CARTESIAN_POINT('Ctrl Pts',(-19.6543477211371,49.5358554165918,121.924410607044)) ;
#41008 = CARTESIAN_POINT('Ctrl Pts',(-19.8059348665026,49.7256921960996,122.273064256038)) ;
#41009 = CARTESIAN_POINT('Ctrl Pts',(-19.9051063909885,49.5457031156897,121.988376325606)) ;
#41010 = CARTESIAN_POINT('Ctrl Pts',(-19.9970522744167,49.7356536870782,122.358669039494)) ;
#41011 = CARTESIAN_POINT('Ctrl Pts',(-20.1440032594168,49.5556646066684,122.09538317843)) ;
#41012 = CARTESIAN_POINT('Ctrl Pts',(-20.1714411232963,49.7456831494922,122.477202699067)) ;
#41013 = CARTESIAN_POINT('Ctrl Pts',(-20.3619888763229,49.5656940690824,122.243550726911)) ;
#41014 = CARTESIAN_POINT('Ctrl Pts',(-20.3208300958534,49.7555903805921,122.622336917083)) ;
#41015 = CARTESIAN_POINT('Ctrl Pts',(-20.5487252566321,49.5756013001823,122.424969612964)) ;
#41016 = CARTESIAN_POINT('Ctrl Pts',(-20.4435688894129,49.7655367592695,122.791613197818)) ;
#41017 = CARTESIAN_POINT('Ctrl Pts',(-20.7021484058093,49.5855476788597,122.636565942027)) ;
#41018 = CARTESIAN_POINT('Ctrl Pts',(-20.5356692060204,49.7755415280784,122.980728511161)) ;
#41019 = CARTESIAN_POINT('Ctrl Pts',(-20.8172730521425,49.5955524476686,122.872960551579)) ;
#41020 = CARTESIAN_POINT('Ctrl Pts',(-20.5933907296624,49.7855626490986,123.183338291841)) ;
#41021 = CARTESIAN_POINT('Ctrl Pts',(-20.8894241945807,49.6055735686887,123.126222955813)) ;
#41022 = CARTESIAN_POINT('Ctrl Pts',(-20.615012812427,49.7954535149512,123.390155066676)) ;
#41023 = CARTESIAN_POINT('Ctrl Pts',(-20.9164510303949,49.6154644345414,123.384745011976)) ;
#41024 = CARTESIAN_POINT('Ctrl Pts',(-20.6005593145487,49.8054443237105,123.599683369761)) ;
#41025 = CARTESIAN_POINT('Ctrl Pts',(-20.8983831555145,49.6254552433007,123.646655535342)) ;
#41026 = CARTESIAN_POINT('Ctrl Pts',(-20.5501038609146,49.8153949818908,123.802712023402)) ;
#41027 = CARTESIAN_POINT('Ctrl Pts',(-20.8353127629609,49.635405901481,123.900441641749)) ;
#41028 = CARTESIAN_POINT('Ctrl Pts',(-20.4655527395291,49.8253311915329,123.993707680392)) ;
#41029 = CARTESIAN_POINT('Ctrl Pts',(-20.729622612963,49.6453421111231,124.139186358995)) ;
#41030 = CARTESIAN_POINT('Ctrl Pts',(-20.3487747189752,49.8353143582578,124.168128009877)) ;
#41031 = CARTESIAN_POINT('Ctrl Pts',(-20.5836489641355,49.655325277848,124.357211327717)) ;
#41032 = CARTESIAN_POINT('Ctrl Pts',(-20.2023558449378,49.8453581554681,124.320235724213)) ;
#41033 = CARTESIAN_POINT('Ctrl Pts',(-20.4006247563996,49.6653690750583,124.547345114795)) ;
#41034 = CARTESIAN_POINT('Ctrl Pts',(-20.0356569177011,49.8551863716364,124.442367095108)) ;
#41035 = CARTESIAN_POINT('Ctrl Pts',(-20.1922492122614,49.6751972912265,124.700009200447)) ;
#41036 = CARTESIAN_POINT('Ctrl Pts',(-19.8457113842319,49.8652629391056,124.536063834955)) ;
#41037 = CARTESIAN_POINT('Ctrl Pts',(-19.9548171286906,49.6852738586958,124.817128808166)) ;
#41038 = CARTESIAN_POINT('Ctrl Pts',(-19.6468577220022,49.875115024795,124.594160167334)) ;
#41039 = CARTESIAN_POINT('Ctrl Pts',(-19.7062485030575,49.6951259443852,124.889748332489)) ;
#41040 = CARTESIAN_POINT('Ctrl Pts',(-19.4364134670954,49.8851882922004,124.617525881756)) ;
#41041 = CARTESIAN_POINT('Ctrl Pts',(-19.4431934347675,49.7051992117906,124.918954084467)) ;
#41042 = CARTESIAN_POINT('Ctrl Pts',(-19.2299283765432,49.895029708624,124.604248514442)) ;
#41043 = CARTESIAN_POINT('Ctrl Pts',(-19.1850858539065,49.7150406282141,124.902355961702)) ;
#41044 = CARTESIAN_POINT('Ctrl Pts',(-19.0262747705676,49.9049909667667,124.55549141664)) ;
#41045 = CARTESIAN_POINT('Ctrl Pts',(-18.930518826785,49.7250018863569,124.841407931726)) ;
#41046 = CARTESIAN_POINT('Ctrl Pts',(-18.8328848698317,49.9150276431986,124.471106946337)) ;
#41047 = CARTESIAN_POINT('Ctrl Pts',(-18.6887821551141,49.7350385627888,124.735926054281)) ;
#41048 = CARTESIAN_POINT('Ctrl Pts',(-18.6596380225063,49.9249062510625,124.35654118208)) ;
#41049 = CARTESIAN_POINT('Ctrl Pts',(-18.4722236385822,49.7449171706527,124.592716974751)) ;
#41050 = CARTESIAN_POINT('Ctrl Pts',(-18.5061473019625,49.9349664797013,124.211075267504)) ;
#41051 = CARTESIAN_POINT('Ctrl Pts',(-18.2803615485747,49.7549773992915,124.410883615261)) ;
#41052 = CARTESIAN_POINT('Ctrl Pts',(-18.3825837811286,49.9448334638621,124.044425289918)) ;
#41053 = CARTESIAN_POINT('Ctrl Pts',(-18.1259078276159,49.7648443834522,124.202569344541)) ;
#41054 = CARTESIAN_POINT('Ctrl Pts',(-18.2881916231086,49.9548390301148,123.856476139896)) ;
#41055 = CARTESIAN_POINT('Ctrl Pts',(-18.0079191605339,49.774849949705,123.967632043621)) ;
#41056 = CARTESIAN_POINT('Ctrl Pts',(-18.2280312076151,49.9648228185294,123.655353475487)) ;
#41057 = CARTESIAN_POINT('Ctrl Pts',(-17.9327202356011,49.7848337381195,123.716228002362)) ;
#41058 = CARTESIAN_POINT('Ctrl Pts',(-18.2037899064989,49.974868675332,123.445570734123)) ;
#41059 = CARTESIAN_POINT('Ctrl Pts',(-17.9024202751132,49.7948795949222,123.45399954575)) ;
#41060 = CARTESIAN_POINT('Ctrl Pts',(-18.2157993043397,49.984694552548,123.239349234005)) ;
#41061 = CARTESIAN_POINT('Ctrl Pts',(-17.9174338427827,49.8047054721381,123.196221483271)) ;
#41062 = CARTESIAN_POINT('Ctrl Pts',(-18.2635625382729,49.9946850283893,123.034820965476)) ;
#41063 = CARTESIAN_POINT('Ctrl Pts',(-17.9771398351089,49.8146959479795,122.94056142547)) ;
#41064 = CARTESIAN_POINT('Ctrl Pts',(-18.3470621028792,50.0047286042881,122.840884623417)) ;
#41065 = CARTESIAN_POINT('Ctrl Pts',(-18.0815158765175,49.8247395238783,122.698141841132)) ;
#41066 = CARTESIAN_POINT('Ctrl Pts',(-18.4600443984035,50.0145503965861,122.668054220945)) ;
#41067 = CARTESIAN_POINT('Ctrl Pts',(-18.2227460406052,49.8345613161763,122.482103844495)) ;
#41068 = CARTESIAN_POINT('Ctrl Pts',(-18.604009794299,50.024585362212,122.513843576675)) ;
#41069 = CARTESIAN_POINT('Ctrl Pts',(-18.402704230727,49.8445962818022,122.289342033842)) ;
#41070 = CARTESIAN_POINT('Ctrl Pts',(-18.7727524722638,50.034610279145,122.387565767662)) ;
#41071 = CARTESIAN_POINT('Ctrl Pts',(-18.6136336980981,49.8546211987352,122.131496311186)) ;
#41072 = CARTESIAN_POINT('Ctrl Pts',(-18.957405994649,50.0444622175212,122.293741975346)) ;
#41073 = CARTESIAN_POINT('Ctrl Pts',(-18.8444524258335,49.8644731371114,122.014217927742)) ;
#41074 = CARTESIAN_POINT('Ctrl Pts',(-19.1582192780616,50.0544531935459,122.23225581094)) ;
#41075 = CARTESIAN_POINT('Ctrl Pts',(-19.0954698169748,49.8744641131361,121.937362207326)) ;
#41076 = CARTESIAN_POINT('Ctrl Pts',(-19.3651677350279,50.0643710143496,122.206614010036)) ;
#41077 = CARTESIAN_POINT('Ctrl Pts',(-19.3541562238225,49.8843819339398,121.905312031282)) ;
#41078 = CARTESIAN_POINT('Ctrl Pts',(-19.5757056924692,50.0743997349142,122.217377366657)) ;
#41079 = CARTESIAN_POINT('Ctrl Pts',(-19.6173285206094,49.8944106545043,121.918768394754)) ;
#41080 = CARTESIAN_POINT('Ctrl Pts',(-19.7782617157918,50.0842826615234,122.263718063625)) ;
#41081 = CARTESIAN_POINT('Ctrl Pts',(-19.8705237928477,49.9042935811135,121.97669658887)) ;
#41082 = CARTESIAN_POINT('Ctrl Pts',(-19.9721356284537,50.0942869466428,122.345192272109)) ;
#41083 = CARTESIAN_POINT('Ctrl Pts',(-20.1128653759059,49.914297866233,122.07854150103)) ;
#41084 = CARTESIAN_POINT('Ctrl Pts',(-20.1485909447356,50.1042706278507,122.458909425641)) ;
#41085 = CARTESIAN_POINT('Ctrl Pts',(-20.3334334359749,49.9242815474409,122.220689960758)) ;
#41086 = CARTESIAN_POINT('Ctrl Pts',(-20.3033028222086,50.1143116265806,122.602499485329)) ;
#41087 = CARTESIAN_POINT('Ctrl Pts',(-20.5268216964148,49.9343225461708,122.400179102823)) ;
#41088 = CARTESIAN_POINT('Ctrl Pts',(-20.4283285557546,50.1241440714477,122.767114268604)) ;
#41089 = CARTESIAN_POINT('Ctrl Pts',(-20.6831026136784,49.9441549910379,122.605949735481)) ;
#41090 = CARTESIAN_POINT('Ctrl Pts',(-20.5249823851883,50.1341390698781,122.95368511086)) ;
#41091 = CARTESIAN_POINT('Ctrl Pts',(-20.803917788404,49.9541499894682,122.839164524144)) ;
#41092 = CARTESIAN_POINT('Ctrl Pts',(-20.5875768112403,50.1441706186277,123.155088324659)) ;
#41093 = CARTESIAN_POINT('Ctrl Pts',(-20.8821585763182,49.9641815382179,123.090919199745)) ;
#41094 = CARTESIAN_POINT('Ctrl Pts',(-20.6140645488152,50.1540359969332,123.360779768465)) ;
#41095 = CARTESIAN_POINT('Ctrl Pts',(-20.915265961447,49.9740469165233,123.348034537655)) ;
#41096 = CARTESIAN_POINT('Ctrl Pts',(-20.6049313505838,50.1639978443934,123.570016308224)) ;
#41097 = CARTESIAN_POINT('Ctrl Pts',(-20.9038469303257,49.9840087639836,123.609580355005)) ;
#41098 = CARTESIAN_POINT('Ctrl Pts',(-20.5589419047173,50.1740327852077,123.775896953256)) ;
#41099 = CARTESIAN_POINT('Ctrl Pts',(-20.8463577367152,49.9940437047979,123.866930592324)) ;
#41100 = CARTESIAN_POINT('Ctrl Pts',(-20.4794221936391,50.1839177462248,123.967925666986)) ;
#41101 = CARTESIAN_POINT('Ctrl Pts',(-20.746955550935,50.003928665815,124.106966044007)) ;
#41102 = CARTESIAN_POINT('Ctrl Pts',(-20.3657227466916,50.1939833551437,124.146355086132)) ;
#41103 = CARTESIAN_POINT('Ctrl Pts',(-20.6048292012877,50.0139942747339,124.330001338976)) ;
#41104 = CARTESIAN_POINT('Ctrl Pts',(-20.2260937776423,50.2038225301854,124.299012275186)) ;
#41105 = CARTESIAN_POINT('Ctrl Pts',(-20.4302906277836,50.0238334497756,124.520821628154)) ;
#41106 = CARTESIAN_POINT('Ctrl Pts',(-20.0585794048684,50.2138850856853,124.428165424389)) ;
#41107 = CARTESIAN_POINT('Ctrl Pts',(-20.2208961768648,50.0338960052755,124.682260919723)) ;
#41108 = CARTESIAN_POINT('Ctrl Pts',(-19.8741279084005,50.2237822603782,124.524475108692)) ;
#41109 = CARTESIAN_POINT('Ctrl Pts',(-19.9903302029033,50.0437931799684,124.802645968582)) ;
#41110 = CARTESIAN_POINT('Ctrl Pts',(-19.675310997847,50.2337129753016,124.588171794171)) ;
#41111 = CARTESIAN_POINT('Ctrl Pts',(-19.741807958997,50.0537238948917,124.882264366588)) ;
#41112 = CARTESIAN_POINT('Ctrl Pts',(-19.4660617887297,50.2437570033792,124.616460712568)) ;
#41113 = CARTESIAN_POINT('Ctrl Pts',(-19.4802461248296,50.0637679229693,124.917622892758)) ;
#41114 = CARTESIAN_POINT('Ctrl Pts',(-19.2583695225843,50.2536432052325,124.608282274617)) ;
#41115 = CARTESIAN_POINT('Ctrl Pts',(-19.2206304688788,50.0736541248226,124.90739716592)) ;
#41116 = CARTESIAN_POINT('Ctrl Pts',(-19.0530229072309,50.2636363716993,124.564006896081)) ;
#41117 = CARTESIAN_POINT('Ctrl Pts',(-18.9639476699282,50.0836472912895,124.852050273557)) ;
#41118 = CARTESIAN_POINT('Ctrl Pts',(-18.8594602487142,50.2735758426865,124.485214042851)) ;
#41119 = CARTESIAN_POINT('Ctrl Pts',(-18.7219951492105,50.0935867622767,124.753556604805)) ;
#41120 = CARTESIAN_POINT('Ctrl Pts',(-18.6811659538875,50.2835923570407,124.373207861046)) ;
#41121 = CARTESIAN_POINT('Ctrl Pts',(-18.4991286839154,50.1036032766309,124.613546547517)) ;
#41122 = CARTESIAN_POINT('Ctrl Pts',(-18.5262199735624,50.2935223835175,124.233262173088)) ;
#41123 = CARTESIAN_POINT('Ctrl Pts',(-18.3054478577974,50.1135333031077,124.438612238889)) ;
#41124 = CARTESIAN_POINT('Ctrl Pts',(-18.3964464306137,50.303574919027,124.066486390739)) ;
#41125 = CARTESIAN_POINT('Ctrl Pts',(-18.1432330981543,50.1235858386171,124.230140853432)) ;
#41126 = CARTESIAN_POINT('Ctrl Pts',(-18.2995125290276,50.3134213222466,123.883574583666)) ;
#41127 = CARTESIAN_POINT('Ctrl Pts',(-18.0220679537271,50.1334322418368,124.001499451912)) ;
#41128 = CARTESIAN_POINT('Ctrl Pts',(-18.2344247285052,50.3233833651007,123.684524259499)) ;
#41129 = CARTESIAN_POINT('Ctrl Pts',(-17.9407108290362,50.1433942846909,123.752685556901)) ;
#41130 = CARTESIAN_POINT('Ctrl Pts',(-18.204957703029,50.3334119158914,123.475747879046)) ;
#41131 = CARTESIAN_POINT('Ctrl Pts',(-17.9038797901194,50.1534228354815,123.491714650902)) ;
#41132 = CARTESIAN_POINT('Ctrl Pts',(-18.2120324651509,50.343322241609,123.267531291762)) ;
#41133 = CARTESIAN_POINT('Ctrl Pts',(-17.9127260346725,50.1633331611992,123.23144379836)) ;
#41134 = CARTESIAN_POINT('Ctrl Pts',(-18.2547290771079,50.3532571534386,123.063072199955)) ;
#41135 = CARTESIAN_POINT('Ctrl Pts',(-17.9660995837992,50.1732680730287,122.975870378425)) ;
#41136 = CARTESIAN_POINT('Ctrl Pts',(-18.3332815125372,50.3632981602067,122.867144842082)) ;
#41137 = CARTESIAN_POINT('Ctrl Pts',(-18.064292748785,50.1833090797968,122.730962183321)) ;
#41138 = CARTESIAN_POINT('Ctrl Pts',(-18.4428498626735,50.3731857930389,122.69048500063)) ;
#41139 = CARTESIAN_POINT('Ctrl Pts',(-18.2012556639799,50.193196712629,122.510138724669)) ;
#41140 = CARTESIAN_POINT('Ctrl Pts',(-18.5825766741435,50.3831762241369,122.533689688026)) ;
#41141 = CARTESIAN_POINT('Ctrl Pts',(-18.3759163266947,50.2031871437271,122.314146410312)) ;
#41142 = CARTESIAN_POINT('Ctrl Pts',(-18.7469116188207,50.3931316606941,122.404071107336)) ;
#41143 = CARTESIAN_POINT('Ctrl Pts',(-18.5813368509821,50.2131425802843,122.152125343419)) ;
#41144 = CARTESIAN_POINT('Ctrl Pts',(-18.930235657484,50.4030426087935,122.305070551018)) ;
#41145 = CARTESIAN_POINT('Ctrl Pts',(-18.8104932141382,50.2230535283836,122.028377092492)) ;
#41146 = CARTESIAN_POINT('Ctrl Pts',(-19.1299354241263,50.4130546848912,122.238492971298)) ;
#41147 = CARTESIAN_POINT('Ctrl Pts',(-19.0601191774132,50.2330656044813,121.945157820118)) ;
#41148 = CARTESIAN_POINT('Ctrl Pts',(-19.3385035067007,50.4230820069661,122.207980233689)) ;
#41149 = CARTESIAN_POINT('Ctrl Pts',(-19.3208286510876,50.2430929265563,121.907019503195)) ;
#41150 = CARTESIAN_POINT('Ctrl Pts',(-19.5457289876827,50.4329407819203,122.213520699819)) ;
#41151 = CARTESIAN_POINT('Ctrl Pts',(-19.5798646279498,50.2529517015105,121.913948569408)) ;
#41152 = CARTESIAN_POINT('Ctrl Pts',(-19.822185156653,50.4463669747327,122.270169175991)) ;
#41153 = CARTESIAN_POINT('Ctrl Pts',(-19.9254133373787,50.2663778943229,121.984759551883)) ;
#41154 = CARTESIAN_POINT('Ctrl Pts',(-20.0713938613618,50.4594509905141,122.394125106127)) ;
#41155 = CARTESIAN_POINT('Ctrl Pts',(-20.2369013110958,50.2794619101043,122.139682808974)) ;
#41156 = CARTESIAN_POINT('Ctrl Pts',(-20.2838339244026,50.4729244392694,122.581328585295)) ;
#41157 = CARTESIAN_POINT('Ctrl Pts',(-20.5024950622099,50.2929353588595,122.373723117141)) ;
#41158 = CARTESIAN_POINT('Ctrl Pts',(-20.4126445774875,50.4827573970752,122.743055891855)) ;
#41159 = CARTESIAN_POINT('Ctrl Pts',(-20.66349684116,50.3027683166654,122.575877232231)) ;
#41160 = CARTESIAN_POINT('Ctrl Pts',(-20.5134783735398,50.4927206705259,122.926629074294)) ;
#41161 = CARTESIAN_POINT('Ctrl Pts',(-20.7895391336707,50.3127315901161,122.805346777451)) ;
#41162 = CARTESIAN_POINT('Ctrl Pts',(-20.5809791036652,50.5027577443438,123.126549900042)) ;
#41163 = CARTESIAN_POINT('Ctrl Pts',(-20.8739118056106,50.322768663934,123.055248323622)) ;
#41164 = CARTESIAN_POINT('Ctrl Pts',(-20.6126206713393,50.5126327473555,123.331753130747)) ;
#41165 = CARTESIAN_POINT('Ctrl Pts',(-20.913461175216,50.3326436669457,123.311752830496)) ;
#41166 = CARTESIAN_POINT('Ctrl Pts',(-20.608057270493,50.5227004269817,123.543329168377)) ;
#41167 = CARTESIAN_POINT('Ctrl Pts',(-20.9077542262007,50.3427113465718,123.576222416547)) ;
#41168 = CARTESIAN_POINT('Ctrl Pts',(-20.5678626540345,50.5325412771994,123.746296518726)) ;
#41169 = CARTESIAN_POINT('Ctrl Pts',(-20.8575080096766,50.3525521967896,123.829932935533)) ;
#41170 = CARTESIAN_POINT('Ctrl Pts',(-20.4670213376231,50.5458774756753,124.007888589382)) ;
#41171 = CARTESIAN_POINT('Ctrl Pts',(-20.7314548292168,50.3658883952655,124.156910684375)) ;
#41172 = CARTESIAN_POINT('Ctrl Pts',(-20.3015547858526,50.5590949994898,124.235123685654)) ;
#41173 = CARTESIAN_POINT('Ctrl Pts',(-20.5246530684262,50.3791059190799,124.440925618339)) ;
#41174 = CARTESIAN_POINT('Ctrl Pts',(-20.0837840031638,50.572429925981,124.411566237074)) ;
#41175 = CARTESIAN_POINT('Ctrl Pts',(-20.252395006767,50.3924408455712,124.661518807846)) ;
#41176 = CARTESIAN_POINT('Ctrl Pts',(-19.9002502528585,50.5824130265756,124.513455062962)) ;
#41177 = CARTESIAN_POINT('Ctrl Pts',(-20.0229851843153,50.4024239461658,124.788869046828)) ;
#41178 = CARTESIAN_POINT('Ctrl Pts',(-19.7005468923068,50.5924578024753,124.582032085012)) ;
#41179 = CARTESIAN_POINT('Ctrl Pts',(-19.7733522297918,50.4124687220654,124.874590001688)) ;
#41180 = CARTESIAN_POINT('Ctrl Pts',(-19.4967087425705,50.6022757256612,124.614562625887)) ;
#41181 = CARTESIAN_POINT('Ctrl Pts',(-19.5185568926569,50.4222866452513,124.915250650711)) ;
#41182 = CARTESIAN_POINT('Ctrl Pts',(-19.2854718592234,50.6123250396165,124.611560869832)) ;
#41183 = CARTESIAN_POINT('Ctrl Pts',(-19.2545052235501,50.4323359592067,124.911493375644)) ;
#41184 = CARTESIAN_POINT('Ctrl Pts',(-19.0108573397302,50.6256287802391,124.558525690301)) ;
#41185 = CARTESIAN_POINT('Ctrl Pts',(-18.9112636455779,50.4456396998293,124.845209773886)) ;
#41186 = CARTESIAN_POINT('Ctrl Pts',(-18.6949673472923,50.6421189757157,124.406294928456)) ;
#41187 = CARTESIAN_POINT('Ctrl Pts',(-18.516363618277,50.4621298953059,124.654888417468)) ;
#41188 = CARTESIAN_POINT('Ctrl Pts',(-18.4467378433555,50.6588381406404,124.151872297138)) ;
#41189 = CARTESIAN_POINT('Ctrl Pts',(-18.2061311341632,50.4788490602306,124.336917792482)) ;
#41190 = CARTESIAN_POINT('Ctrl Pts',(-18.311368251597,50.6719991343105,123.910554451692)) ;
#41191 = CARTESIAN_POINT('Ctrl Pts',(-18.0368827272088,50.4920100539007,124.035219084642)) ;
#41192 = CARTESIAN_POINT('Ctrl Pts',(-18.2412163964924,50.6819953564158,123.7124638999)) ;
#41193 = CARTESIAN_POINT('Ctrl Pts',(-17.9492027071772,50.502006276006,123.787616040882)) ;
#41194 = CARTESIAN_POINT('Ctrl Pts',(-18.2069016120642,50.6920191959495,123.504545752087)) ;
#41195 = CARTESIAN_POINT('Ctrl Pts',(-17.9063100732853,50.5120301155397,123.527712476813)) ;
#41196 = CARTESIAN_POINT('Ctrl Pts',(-18.209328291179,50.7052125179428,123.227157565911)) ;
#41197 = CARTESIAN_POINT('Ctrl Pts',(-17.9093431972847,50.5252234375329,123.180991999686)) ;
#41198 = CARTESIAN_POINT('Ctrl Pts',(-18.3035425854847,50.7218716897201,122.88574552881)) ;
#41199 = CARTESIAN_POINT('Ctrl Pts',(-18.0271182837049,50.5418826093103,122.754212984413)) ;
#41200 = CARTESIAN_POINT('Ctrl Pts',(-18.5489966287471,50.7417818652058,122.540800163354)) ;
#41201 = CARTESIAN_POINT('Ctrl Pts',(-18.3339375616829,50.561792784796,122.323039035069)) ;
#41202 = CARTESIAN_POINT('Ctrl Pts',(-18.8965967981805,50.7616718530502,122.299823800529)) ;
#41203 = CARTESIAN_POINT('Ctrl Pts',(-18.768439392141,50.5816827726403,122.021820822847)) ;
#41204 = CARTESIAN_POINT('Ctrl Pts',(-19.3079195621711,50.781677301065,122.191706071761)) ;
#41205 = CARTESIAN_POINT('Ctrl Pts',(-19.2825937715337,50.6016882206552,121.886677539516)) ;
#41206 = CARTESIAN_POINT('Ctrl Pts',(-19.728095167199,50.8015136950923,122.229696970735)) ;
#41207 = CARTESIAN_POINT('Ctrl Pts',(-19.8078113963471,50.6215246146825,121.934169205289)) ;
#41208 = CARTESIAN_POINT('Ctrl Pts',(-20.1132481010553,50.821521488989,122.410089592141)) ;
#41209 = CARTESIAN_POINT('Ctrl Pts',(-20.2892513212944,50.6415324085791,122.159662815693)) ;
#41210 = CARTESIAN_POINT('Ctrl Pts',(-20.4112416238867,50.8413481252829,122.708392112376)) ;
#41211 = CARTESIAN_POINT('Ctrl Pts',(-20.6617398848394,50.6613590448731,122.532541564625)) ;
#41212 = CARTESIAN_POINT('Ctrl Pts',(-20.5915810372585,50.8613270682368,123.093001610394)) ;
#41213 = CARTESIAN_POINT('Ctrl Pts',(-20.8871620270303,50.6813379878269,123.013304098407)) ;
#41214 = CARTESIAN_POINT('Ctrl Pts',(-20.6290028587678,50.8812588701058,123.51509334654)) ;
#41215 = CARTESIAN_POINT('Ctrl Pts',(-20.9339369379652,50.701269789696,123.540918150511)) ;
#41216 = CARTESIAN_POINT('Ctrl Pts',(-20.5220534572003,50.9010831706034,123.922954659986)) ;
#41217 = CARTESIAN_POINT('Ctrl Pts',(-20.8002489893683,50.7210940901936,124.050742162829)) ;
#41218 = CARTESIAN_POINT('Ctrl Pts',(-20.2786120446289,50.9211791719433,124.273908281155)) ;
#41219 = CARTESIAN_POINT('Ctrl Pts',(-20.4959470938252,50.7411900915334,124.48943444645)) ;
#41220 = CARTESIAN_POINT('Ctrl Pts',(-19.9357982920383,50.9409375880472,124.517186763173)) ;
#41221 = CARTESIAN_POINT('Ctrl Pts',(-20.0674250455344,50.7609485076374,124.793529199936)) ;
#41222 = CARTESIAN_POINT('Ctrl Pts',(-19.5241716085477,50.9610312809313,124.630773509642)) ;
#41223 = CARTESIAN_POINT('Ctrl Pts',(-19.5529196248106,50.7810422005214,124.935512899824)) ;
#41224 = CARTESIAN_POINT('Ctrl Pts',(-19.2461442415946,50.9741422468379,124.608669218602)) ;
#41225 = CARTESIAN_POINT('Ctrl Pts',(-19.2053312340935,50.7941531664281,124.907880339423)) ;
#41226 = CARTESIAN_POINT('Ctrl Pts',(-19.1099467513572,50.9808556216258,124.573813086965)) ;
#41227 = CARTESIAN_POINT('Ctrl Pts',(-19.0351174388764,50.800866541216,124.86431206241)) ;
#41228 = CARTESIAN_POINT('',(-20.8890752031254,12.1693713464509,123.166987767337)) ;
#41229 = CARTESIAN_POINT('Ctrl Pts',(-20.8890752032057,12.1693713464047,123.166987767343)) ;
#41230 = CARTESIAN_POINT('Ctrl Pts',(-20.8610687220169,12.1854956519226,123.164917450078)) ;
#41231 = CARTESIAN_POINT('Ctrl Pts',(-20.8327633568022,12.2014611086523,123.160624756444)) ;
#41232 = CARTESIAN_POINT('Ctrl Pts',(-20.7745996966326,12.2331206623017,123.145633809153)) ;
#41233 = CARTESIAN_POINT('Ctrl Pts',(-20.7441110801631,12.24905051571,123.134145565635)) ;
#41234 = CARTESIAN_POINT('Ctrl Pts',(-20.6955669569155,12.272204921772,123.1064423772)) ;
#41235 = CARTESIAN_POINT('Ctrl Pts',(-20.6762675979802,12.2807112212954,123.092474606893)) ;
#41236 = CARTESIAN_POINT('Ctrl Pts',(-20.6467890442397,12.2917621876962,123.063862344896)) ;
#41237 = CARTESIAN_POINT('Ctrl Pts',(-20.635672579296,12.295300396613,123.050723734153)) ;
#41238 = CARTESIAN_POINT('Ctrl Pts',(-20.619631838715,12.2989553934292,123.026534454028)) ;
#41239 = CARTESIAN_POINT('Ctrl Pts',(-20.6139434300127,12.2998015796369,123.016333414216)) ;
#41240 = CARTESIAN_POINT('Ctrl Pts',(-20.6070335810964,12.3000406423084,123.001098589481)) ;
#41241 = CARTESIAN_POINT('Ctrl Pts',(-20.6051280525899,12.2999881147679,122.996469969497)) ;
#41242 = CARTESIAN_POINT('Ctrl Pts',(-20.6030890986318,12.2997791002204,122.990964267602)) ;
#41243 = CARTESIAN_POINT('Ctrl Pts',(-20.6027932190504,12.2997444866016,122.990149815383)) ;
#41244 = CARTESIAN_POINT('Ctrl Pts',(-20.6024894319963,12.2997043922845,122.989297097151)) ;
#41245 = CARTESIAN_POINT('Ctrl Pts',(-20.6024764105458,12.2997026647784,122.989260514172)) ;
#41246 = CARTESIAN_POINT('Ctrl Pts',(-20.6024544471701,12.2996997359228,122.989198754854)) ;
#41247 = CARTESIAN_POINT('Ctrl Pts',(-20.6024454997488,12.2996985385416,122.989173580088)) ;
#41248 = CARTESIAN_POINT('Ctrl Pts',(-20.6024308468241,12.2996965706967,122.989132327026)) ;
#41249 = CARTESIAN_POINT('Ctrl Pts',(-20.6024251384176,12.2996958023491,122.989116249634)) ;
#41250 = CARTESIAN_POINT('Ctrl Pts',(-20.6024162524072,12.2996946036105,122.989091212972)) ;
#41251 = CARTESIAN_POINT('Ctrl Pts',(-20.6024130734271,12.2996941742243,122.989082254137)) ;
#41252 = CARTESIAN_POINT('Ctrl Pts',(-20.6024072279404,12.299693383686,122.989065777121)) ;
#41253 = CARTESIAN_POINT('Ctrl Pts',(-20.6024045612302,12.2996930226649,122.989058258941)) ;
#41254 = CARTESIAN_POINT('Ctrl Pts',(-20.6023987642738,12.2996922370477,122.989041912772)) ;
#41255 = CARTESIAN_POINT('Ctrl Pts',(-20.6023956342093,12.2996918123332,122.989033084778)) ;
#41256 = CARTESIAN_POINT('Ctrl Pts',(-20.6023869166592,12.2996906280087,122.989008492654)) ;
#41257 = CARTESIAN_POINT('Ctrl Pts',(-20.6023813304886,12.2996898674372,122.988992728105)) ;
#41258 = CARTESIAN_POINT('Ctrl Pts',(-20.6023507307001,12.299685692091,122.988906340457)) ;
#41259 = CARTESIAN_POINT('Ctrl Pts',(-20.602325753627,12.2996822506058,122.988835705718)) ;
#41260 = CARTESIAN_POINT('Ctrl Pts',(-20.6022559538207,12.2996725396693,122.988637974298)) ;
#41261 = CARTESIAN_POINT('Ctrl Pts',(-20.6022112171852,12.2996662073738,122.988510850483)) ;
#41262 = CARTESIAN_POINT('Ctrl Pts',(-20.5998442084474,12.2993254047404,122.981763874573)) ;
#41263 = CARTESIAN_POINT('Ctrl Pts',(-20.5978658821419,12.2987454066201,122.975055792179)) ;
#41264 = CARTESIAN_POINT('Ctrl Pts',(-20.5933548407168,12.2964747990813,122.956304836256)) ;
#41265 = CARTESIAN_POINT('Ctrl Pts',(-20.5915905482467,12.2942918311834,122.944252818362)) ;
#41266 = CARTESIAN_POINT('Ctrl Pts',(-20.5898591383132,12.2873891660181,122.914933679065)) ;
#41267 = CARTESIAN_POINT('Ctrl Pts',(-20.5910205314854,12.2820577513669,122.8979913349)) ;
#41268 = CARTESIAN_POINT('Ctrl Pts',(-20.5980947263798,12.2670202296296,122.858409784169)) ;
#41269 = CARTESIAN_POINT('Ctrl Pts',(-20.6057336956224,12.2565042285035,122.83652182479)) ;
#41270 = CARTESIAN_POINT('Ctrl Pts',(-20.6376705328441,12.2199530300488,122.770754536439)) ;
#41271 = CARTESIAN_POINT('Ctrl Pts',(-20.673969475726,12.1873876374,122.72708632587)) ;
#41272 = CARTESIAN_POINT('Ctrl Pts',(-20.7227191491784,12.149892972702,122.68753928804)) ;
#41273 = CARTESIAN_POINT('Ctrl Pts',(-17.9353686288931,11.9999999994367,123.599289317261)) ;
#41274 = CARTESIAN_POINT('Ctrl Pts',(-17.9738189265565,12.0242028233619,123.58612699736)) ;
#41275 = CARTESIAN_POINT('Ctrl Pts',(-18.0134459580924,12.0487813737637,123.575656459509)) ;
#41276 = CARTESIAN_POINT('Ctrl Pts',(-18.0909257937832,12.0961326415371,123.561717397006)) ;
#41277 = CARTESIAN_POINT('Ctrl Pts',(-18.129448015999,12.1193588332732,123.557760132541)) ;
#41278 = CARTESIAN_POINT('Ctrl Pts',(-18.1677926267253,12.1420303856096,123.557513873554)) ;
#41279 = CARTESIAN_POINT('Ctrl Pts',(-20.8890752031254,12.1693713464509,123.166987767337)) ;
#41280 = CARTESIAN_POINT('Ctrl Pts',(-20.8921168691093,12.1700845612802,123.185411053998)) ;
#41281 = CARTESIAN_POINT('Ctrl Pts',(-20.9073190645084,12.174105036101,123.289588099265)) ;
#41282 = CARTESIAN_POINT('Ctrl Pts',(-20.9152054113298,12.1814863726884,123.483408955597)) ;
#41283 = CARTESIAN_POINT('Ctrl Pts',(-20.8794802827671,12.1915186409522,123.744603500789)) ;
#41284 = CARTESIAN_POINT('Ctrl Pts',(-20.8008139737887,12.2013826029581,123.991621606298)) ;
#41285 = CARTESIAN_POINT('Ctrl Pts',(-20.678002189668,12.211452664303,124.225997440401)) ;
#41286 = CARTESIAN_POINT('Ctrl Pts',(-20.5199833626838,12.2212950286517,124.430776031763)) ;
#41287 = CARTESIAN_POINT('Ctrl Pts',(-20.327174746647,12.2312557011542,124.607803018266)) ;
#41288 = CARTESIAN_POINT('Ctrl Pts',(-20.1045650508631,12.241293772222,124.749310160051)) ;
#41289 = CARTESIAN_POINT('Ctrl Pts',(-19.8649051459857,12.2511673871824,124.84884392232)) ;
#41290 = CARTESIAN_POINT('Ctrl Pts',(-19.6065797304044,12.2612396217637,124.906300997495)) ;
#41291 = CARTESIAN_POINT('Ctrl Pts',(-19.3486297183306,12.2710636402125,124.918040759663)) ;
#41292 = CARTESIAN_POINT('Ctrl Pts',(-19.0863456687476,12.2811285611885,124.884353810211)) ;
#41293 = CARTESIAN_POINT('Ctrl Pts',(-18.7548496615759,12.2943388594833,124.781008020348)) ;
#41294 = CARTESIAN_POINT('Ctrl Pts',(-18.4555083325038,12.3076543062152,124.592460114452)) ;
#41295 = CARTESIAN_POINT('Ctrl Pts',(-18.2182158984291,12.3209445514825,124.336043204847)) ;
#41296 = CARTESIAN_POINT('Ctrl Pts',(-18.0753697674858,12.3309953010896,124.113946532571)) ;
#41297 = CARTESIAN_POINT('Ctrl Pts',(-17.9751686262583,12.3408079080718,123.876303265546)) ;
#41298 = CARTESIAN_POINT('Ctrl Pts',(-17.9159132713503,12.3508790060661,123.61839959421)) ;
#41299 = CARTESIAN_POINT('Ctrl Pts',(-17.9028470180164,12.360768578841,123.358821518713)) ;
#41300 = CARTESIAN_POINT('Ctrl Pts',(-17.9449900324593,12.3740386856443,123.012644489447)) ;
#41301 = CARTESIAN_POINT('Ctrl Pts',(-18.1100382420715,12.3906553725668,122.603018959482)) ;
#41302 = CARTESIAN_POINT('Ctrl Pts',(-18.403953809166,12.407229415883,122.274921978595)) ;
#41303 = CARTESIAN_POINT('Ctrl Pts',(-18.6963080999561,12.4205259833148,122.083501484983)) ;
#41304 = CARTESIAN_POINT('Ctrl Pts',(-18.9385791929077,12.4305560468922,121.979673523522)) ;
#41305 = CARTESIAN_POINT('Ctrl Pts',(-19.1916818709481,12.4404499387415,121.920281628208)) ;
#41306 = CARTESIAN_POINT('Ctrl Pts',(-19.5394009792638,12.453702694527,121.899549493621)) ;
#41307 = CARTESIAN_POINT('Ctrl Pts',(-19.9747293753154,12.4704307995194,121.989564308867)) ;
#41308 = CARTESIAN_POINT('Ctrl Pts',(-20.423556659189,12.4902616359979,122.266069036656)) ;
#41309 = CARTESIAN_POINT('Ctrl Pts',(-20.7535327226879,12.5101870278881,122.680135635484)) ;
#41310 = CARTESIAN_POINT('Ctrl Pts',(-20.9224041261076,12.5301122412401,123.18215712058)) ;
#41311 = CARTESIAN_POINT('Ctrl Pts',(-20.9099617273115,12.5500372547252,123.711523704258)) ;
#41312 = CARTESIAN_POINT('Ctrl Pts',(-20.7187360422604,12.5699137264252,124.204018044716)) ;
#41313 = CARTESIAN_POINT('Ctrl Pts',(-20.3693300643289,12.5898930443341,124.603877601687)) ;
#41314 = CARTESIAN_POINT('Ctrl Pts',(-19.9052905888142,12.6098260479101,124.859582769263)) ;
#41315 = CARTESIAN_POINT('Ctrl Pts',(-19.3829989743676,12.6297213179378,124.941977004567)) ;
#41316 = CARTESIAN_POINT('Ctrl Pts',(-18.8631060156455,12.6496426558436,124.841587523865)) ;
#41317 = CARTESIAN_POINT('Ctrl Pts',(-18.4079042835162,12.6696002791098,124.569214868981)) ;
#41318 = CARTESIAN_POINT('Ctrl Pts',(-18.0742532724176,12.689480111067,124.15962015315)) ;
#41319 = CARTESIAN_POINT('Ctrl Pts',(-17.8989480657597,12.7093619623639,123.661012507451)) ;
#41320 = CARTESIAN_POINT('Ctrl Pts',(-17.9053743363839,12.7294329794677,123.127663535506)) ;
#41321 = CARTESIAN_POINT('Ctrl Pts',(-18.0909224032866,12.7492402032208,122.634900991628)) ;
#41322 = CARTESIAN_POINT('Ctrl Pts',(-18.4354537167374,12.7692213387896,122.230824135122)) ;
#41323 = CARTESIAN_POINT('Ctrl Pts',(-18.8964641846084,12.7891488321288,121.970176160961)) ;
#41324 = CARTESIAN_POINT('Ctrl Pts',(-19.415834432645,12.8089694934866,121.881151656097)) ;
#41325 = CARTESIAN_POINT('Ctrl Pts',(-19.9411566590932,12.8290666827084,121.976780870031)) ;
#41326 = CARTESIAN_POINT('Ctrl Pts',(-20.3952240684518,12.8488303617167,122.241384544964)) ;
#41327 = CARTESIAN_POINT('Ctrl Pts',(-20.7368987004041,12.8688876403898,122.650278783027)) ;
#41328 = CARTESIAN_POINT('Ctrl Pts',(-20.915999998585,12.8886830641372,123.145136393717)) ;
#41329 = CARTESIAN_POINT('Ctrl Pts',(-20.9171224626081,12.9086467088648,123.675675466344)) ;
#41330 = CARTESIAN_POINT('Ctrl Pts',(-20.7357148689362,12.9286302001389,124.174870580485)) ;
#41331 = CARTESIAN_POINT('Ctrl Pts',(-20.3986521463145,12.9484376952882,124.579332558867)) ;
#41332 = CARTESIAN_POINT('Ctrl Pts',(-19.9402235763069,12.9684202860083,124.847283742868)) ;
#41333 = CARTESIAN_POINT('Ctrl Pts',(-19.4202416053834,12.9883029399995,124.942191223807)) ;
#41334 = CARTESIAN_POINT('Ctrl Pts',(-18.8972653738817,13.0082611848626,124.854056149815)) ;
#41335 = CARTESIAN_POINT('Ctrl Pts',(-18.4373467193133,13.0281367719042,124.594021898923)) ;
#41336 = CARTESIAN_POINT('Ctrl Pts',(-18.0917408140289,13.0481176600395,124.190855292359)) ;
#41337 = CARTESIAN_POINT('Ctrl Pts',(-17.9052414355018,13.0680528011505,123.694844185524)) ;
#41338 = CARTESIAN_POINT('Ctrl Pts',(-17.8988271166947,13.0879648191615,123.165702838927)) ;
#41339 = CARTESIAN_POINT('Ctrl Pts',(-18.072637630343,13.1078530374051,122.666485551976)) ;
#41340 = CARTESIAN_POINT('Ctrl Pts',(-18.3508356377982,13.124451341252,122.324166060085)) ;
#41341 = CARTESIAN_POINT('Ctrl Pts',(-18.6332461345771,13.1377239311548,122.119417599801)) ;
#41342 = CARTESIAN_POINT('Ctrl Pts',(-18.8696106143661,13.1477313461057,122.004127651261)) ;
#41343 = CARTESIAN_POINT('Ctrl Pts',(-19.1224757065835,13.1577386928383,121.931849416177)) ;
#41344 = CARTESIAN_POINT('Ctrl Pts',(-19.4692111889447,13.1710050526399,121.895476582139)) ;
#41345 = CARTESIAN_POINT('Ctrl Pts',(-19.9027886653172,13.1875197102629,121.963391453896)) ;
#41346 = CARTESIAN_POINT('Ctrl Pts',(-20.2896179416635,13.2041171435055,122.175375538865)) ;
#41347 = CARTESIAN_POINT('Ctrl Pts',(-20.5428541366256,13.2174651406505,122.418153018463)) ;
#41348 = CARTESIAN_POINT('Ctrl Pts',(-20.6967627804406,13.2273608950021,122.62776755716)) ;
#41349 = CARTESIAN_POINT('Ctrl Pts',(-20.8132896637095,13.2373488489335,122.862934128972)) ;
#41350 = CARTESIAN_POINT('Ctrl Pts',(-20.8871117690639,13.2473060726382,123.114002366625)) ;
#41351 = CARTESIAN_POINT('Ctrl Pts',(-20.9163194697392,13.2573416191949,123.376085199788)) ;
#41352 = CARTESIAN_POINT('Ctrl Pts',(-20.9000197111728,13.267228730471,123.635413520908)) ;
#41353 = CARTESIAN_POINT('Ctrl Pts',(-20.8387093067046,13.2772201355718,123.890705618829)) ;
#41354 = CARTESIAN_POINT('Ctrl Pts',(-20.7344045824693,13.2871657567866,124.130350209159)) ;
#41355 = CARTESIAN_POINT('Ctrl Pts',(-20.5904556480587,13.2971150050549,124.348628887742)) ;
#41356 = CARTESIAN_POINT('Ctrl Pts',(-20.4088310489179,13.3071615002235,124.540222615066)) ;
#41357 = CARTESIAN_POINT('Ctrl Pts',(-20.2009526790891,13.3170128430151,124.69453910851)) ;
#41358 = CARTESIAN_POINT('Ctrl Pts',(-19.9669434550335,13.3269846231424,124.812406349802)) ;
#41359 = CARTESIAN_POINT('Ctrl Pts',(-19.7153564891379,13.3369798231201,124.888022808457)) ;
#41360 = CARTESIAN_POINT('Ctrl Pts',(-19.4534753611638,13.3470138148161,124.918598821052)) ;
#41361 = CARTESIAN_POINT('Ctrl Pts',(-19.1948766730221,13.3568692197886,124.903920505576)) ;
#41362 = CARTESIAN_POINT('Ctrl Pts',(-18.9390603846793,13.3668685176344,124.844062381727)) ;
#41363 = CARTESIAN_POINT('Ctrl Pts',(-18.6998481883594,13.3767636302396,124.741995186928)) ;
#41364 = CARTESIAN_POINT('Ctrl Pts',(-18.4784292945889,13.3868242757746,124.597585675323)) ;
#41365 = CARTESIAN_POINT('Ctrl Pts',(-18.2893688821215,13.3966731527638,124.420799145494)) ;
#41366 = CARTESIAN_POINT('Ctrl Pts',(-18.1305208053495,13.4067018638574,124.210511784196)) ;
#41367 = CARTESIAN_POINT('Ctrl Pts',(-18.0112247910287,13.4167312651135,123.975488167396)) ;
#41368 = CARTESIAN_POINT('Ctrl Pts',(-17.9354445009214,13.4265714569095,123.72824647118)) ;
#41369 = CARTESIAN_POINT('Ctrl Pts',(-17.9027395319079,13.4365748861025,123.467435684465)) ;
#41370 = CARTESIAN_POINT('Ctrl Pts',(-17.9158814573718,13.4465603985687,123.205311390375)) ;
#41371 = CARTESIAN_POINT('Ctrl Pts',(-17.9749065837832,13.4566014949527,122.948155155583)) ;
#41372 = CARTESIAN_POINT('Ctrl Pts',(-18.0753470360815,13.4664446909037,122.709757985454)) ;
#41373 = CARTESIAN_POINT('Ctrl Pts',(-18.217218281521,13.4764310019581,122.489035231126)) ;
#41374 = CARTESIAN_POINT('Ctrl Pts',(-18.3942732512551,13.4863656872158,122.297106419642)) ;
#41375 = CARTESIAN_POINT('Ctrl Pts',(-18.6046031877743,13.4964232484328,122.137116873894)) ;
#41376 = CARTESIAN_POINT('Ctrl Pts',(-18.8338850495127,13.5062448900415,122.018535713195)) ;
#41377 = CARTESIAN_POINT('Ctrl Pts',(-19.0859583258846,13.5163009536324,121.939273611562)) ;
#41378 = CARTESIAN_POINT('Ctrl Pts',(-19.3450516698222,13.5262416293942,121.905839973782)) ;
#41379 = CARTESIAN_POINT('Ctrl Pts',(-19.6050909750196,13.5361459881825,121.917041144644)) ;
#41380 = CARTESIAN_POINT('Ctrl Pts',(-19.862825851585,13.5461926427583,121.97418792217)) ;
#41381 = CARTESIAN_POINT('Ctrl Pts',(-20.1031997643857,13.5560882374012,122.073508487898)) ;
#41382 = CARTESIAN_POINT('Ctrl Pts',(-20.3263218440362,13.5661501840581,122.215343672236)) ;
#41383 = CARTESIAN_POINT('Ctrl Pts',(-20.5173749645332,13.5759998079902,122.38999462014)) ;
#41384 = CARTESIAN_POINT('Ctrl Pts',(-20.6776884554839,13.5859630470201,122.596980439567)) ;
#41385 = CARTESIAN_POINT('Ctrl Pts',(-20.8000704181908,13.5959876217959,122.830280403309)) ;
#41386 = CARTESIAN_POINT('Ctrl Pts',(-20.8793920083737,13.6059061844836,123.07855998187)) ;
#41387 = CARTESIAN_POINT('Ctrl Pts',(-20.9151199375489,13.6158983712076,123.338717822216)) ;
#41388 = CARTESIAN_POINT('Ctrl Pts',(-20.9046168525977,13.6259331697918,123.6022019633)) ;
#41389 = CARTESIAN_POINT('Ctrl Pts',(-20.8499556627768,13.6357883604655,123.855372966742)) ;
#41390 = CARTESIAN_POINT('Ctrl Pts',(-20.7510855573927,13.6457877086185,124.098788324435)) ;
#41391 = CARTESIAN_POINT('Ctrl Pts',(-20.6130996723433,13.6556828342936,124.319242233489)) ;
#41392 = CARTESIAN_POINT('Ctrl Pts',(-20.4360519660016,13.6657433772417,124.515540628893)) ;
#41393 = CARTESIAN_POINT('Ctrl Pts',(-20.232034145686,13.6755926515086,124.674850714962)) ;
#41394 = CARTESIAN_POINT('Ctrl Pts',(-19.9996623311131,13.6856198760785,124.799086161189)) ;
#41395 = CARTESIAN_POINT('Ctrl Pts',(-19.7489854254844,13.6956482752663,124.880448501815)) ;
#41396 = CARTESIAN_POINT('Ctrl Pts',(-19.4928401900497,13.7054940256798,124.916853671087)) ;
#41397 = CARTESIAN_POINT('Ctrl Pts',(-19.230454887784,13.7154828160805,124.908839488335)) ;
#41398 = CARTESIAN_POINT('Ctrl Pts',(-18.9721627761797,13.7255277444802,124.854438840815)) ;
#41399 = CARTESIAN_POINT('Ctrl Pts',(-18.7323658376547,13.7353522292692,124.758724681303)) ;
#41400 = CARTESIAN_POINT('Ctrl Pts',(-18.507457139982,13.7454096268104,124.619951807237)) ;
#41401 = CARTESIAN_POINT('Ctrl Pts',(-18.3128349524813,13.7553357183966,124.44624656969)) ;
#41402 = CARTESIAN_POINT('Ctrl Pts',(-18.1503452309715,13.7652905035412,124.241231958245)) ;
#41403 = CARTESIAN_POINT('Ctrl Pts',(-18.0251465109341,13.7753278731988,124.009068223143)) ;
#41404 = CARTESIAN_POINT('Ctrl Pts',(-17.9431959784106,13.7852166833204,123.762452941019)) ;
#41405 = CARTESIAN_POINT('Ctrl Pts',(-17.9044614031139,13.7952060423715,123.502822293364)) ;
#41406 = CARTESIAN_POINT('Ctrl Pts',(-17.9115693386521,13.8051645898276,123.241226463732)) ;
#41407 = CARTESIAN_POINT('Ctrl Pts',(-17.9630567197968,13.8150641663786,122.986205100608)) ;
#41408 = CARTESIAN_POINT('Ctrl Pts',(-18.0595361492998,13.8251120782093,122.740443216478)) ;
#41409 = CARTESIAN_POINT('Ctrl Pts',(-18.1949930036132,13.8350074260699,122.518422190268)) ;
#41410 = CARTESIAN_POINT('Ctrl Pts',(-18.3697572977927,13.845069102601,122.320042659935)) ;
#41411 = CARTESIAN_POINT('Ctrl Pts',(-18.5718588198519,13.8549136203502,122.158525512922)) ;
#41412 = CARTESIAN_POINT('Ctrl Pts',(-18.8011469810602,13.864874064065,122.032284729829)) ;
#41413 = CARTESIAN_POINT('Ctrl Pts',(-19.0509301231226,13.8749108968832,121.947590007007)) ;
#41414 = CARTESIAN_POINT('Ctrl Pts',(-19.3074865101994,13.88478969363,121.907757156992)) ;
#41415 = CARTESIAN_POINT('Ctrl Pts',(-19.5717537455678,13.8948490097584,121.91308802529)) ;
#41416 = CARTESIAN_POINT('Ctrl Pts',(-19.8262549511952,13.9047194565116,121.963266910915)) ;
#41417 = CARTESIAN_POINT('Ctrl Pts',(-20.0714142577279,13.9147120947696,122.057363864517)) ;
#41418 = CARTESIAN_POINT('Ctrl Pts',(-20.2970965036502,13.9247441103175,122.193613633218)) ;
#41419 = CARTESIAN_POINT('Ctrl Pts',(-20.4928009018349,13.9346099666241,122.363706237578)) ;
#41420 = CARTESIAN_POINT('Ctrl Pts',(-20.6593476164435,13.9446792560932,122.569291069351)) ;
#41421 = CARTESIAN_POINT('Ctrl Pts',(-20.7848399902421,13.9545228136445,122.795508554596)) ;
#41422 = CARTESIAN_POINT('Ctrl Pts',(-20.871120064522,13.9645029404323,123.043168459414)) ;
#41423 = CARTESIAN_POINT('Ctrl Pts',(-20.9127502836893,13.9745214890323,123.303126129535)) ;
#41424 = CARTESIAN_POINT('Ctrl Pts',(-20.9092186327094,13.9844047895555,123.562857078074)) ;
#41425 = CARTESIAN_POINT('Ctrl Pts',(-20.8668755026365,13.9930026771793,123.784759348932)) ;
#41426 = CARTESIAN_POINT('Ctrl Pts',(-20.8240292246658,13.9981476378102,123.912638068403)) ;
#41427 = CARTESIAN_POINT('Ctrl Pts',(-20.8063667317783,14.0000000000496,123.957804304199)) ;
#41428 = CARTESIAN_POINT('Origin',(-20.3808735729049,12.,126.250122109236)) ;
#41429 = CARTESIAN_POINT('',(-18.3583806245238,12.,124.088665030377)) ;
#41430 = CARTESIAN_POINT('',(-18.1677493372133,12.,124.153922001841)) ;
#41431 = CARTESIAN_POINT('Origin',(-19.4092722359532,12.,123.411814366564)) ;
#41432 = CARTESIAN_POINT('Origin',(-19.4092722359532,-13.9601742359176,123.411814366564)) ;
#41433 = CARTESIAN_POINT('',(-20.5919010016347,-12.5498814819081,123.006982052377)) ;
#41434 = CARTESIAN_POINT('Ctrl Pts',(-18.2266423654683,-12.3699164408135,
123.816643453356)) ;
#41435 = CARTESIAN_POINT('Ctrl Pts',(-18.2493742613449,-12.3731350315633,
123.883050290101)) ;
#41436 = CARTESIAN_POINT('Ctrl Pts',(-18.2776599920336,-12.3763218616224,
123.947414117214)) ;
#41437 = CARTESIAN_POINT('Ctrl Pts',(-18.3111475606552,-12.3795367049563,
124.008992897305)) ;
#41438 = CARTESIAN_POINT('Ctrl Pts',(-18.3133023878075,-12.3797435707274,
124.012955311801)) ;
#41439 = CARTESIAN_POINT('Ctrl Pts',(-18.3154787380571,-12.3799505524888,
124.016906203678)) ;
#41440 = CARTESIAN_POINT('Ctrl Pts',(-18.3176765111433,-12.3801576661661,
124.020845378626)) ;
#41441 = CARTESIAN_POINT('Ctrl Pts',(-18.3624711373787,-12.3843790208745,
124.101132952698)) ;
#41442 = CARTESIAN_POINT('Ctrl Pts',(-18.4158874627463,-12.3885782982683,
124.176062257801)) ;
#41443 = CARTESIAN_POINT('Ctrl Pts',(-18.4768889137241,-12.3927747089667,
124.244377481592)) ;
#41444 = CARTESIAN_POINT('Ctrl Pts',(-18.5122948246434,-12.3952103517423,
124.284028386435)) ;
#41445 = CARTESIAN_POINT('Ctrl Pts',(-18.5502576072234,-12.3976450287944,
124.321452073109)) ;
#41446 = CARTESIAN_POINT('Ctrl Pts',(-18.5905771630734,-12.4000824963187,
124.356398072605)) ;
#41447 = CARTESIAN_POINT('Ctrl Pts',(-18.6720599780286,-12.4050084363757,
124.42702133098)) ;
#41448 = CARTESIAN_POINT('Ctrl Pts',(-18.762391466541,-12.4099534088704,124.486846557586)) ;
#41449 = CARTESIAN_POINT('Ctrl Pts',(-18.8593143846845,-12.4148934429917,
124.53433223364)) ;
#41450 = CARTESIAN_POINT('Ctrl Pts',(-18.8925082975444,-12.4165852932299,
124.5505950064)) ;
#41451 = CARTESIAN_POINT('Ctrl Pts',(-18.9264384731065,-12.4182785416309,
124.565389349838)) ;
#41452 = CARTESIAN_POINT('Ctrl Pts',(-18.9609092505901,-12.4199790179757,
124.578635104052)) ;
#41453 = CARTESIAN_POINT('Ctrl Pts',(-19.0479270417047,-12.4242716886425,
124.612072593934)) ;
#41454 = CARTESIAN_POINT('Ctrl Pts',(-19.1382300374287,-12.428523931692,124.635603002896)) ;
#41455 = CARTESIAN_POINT('Ctrl Pts',(-19.2301289024319,-12.4327743159446,
124.64891083254)) ;
#41456 = CARTESIAN_POINT('Ctrl Pts',(-19.2817154738864,-12.4351602295351,
124.656381058694)) ;
#41457 = CARTESIAN_POINT('Ctrl Pts',(-19.3338065523741,-12.4375455574124,
124.660630085422)) ;
#41458 = CARTESIAN_POINT('Ctrl Pts',(-19.3861021450717,-12.4399371216425,
124.661599606901)) ;
#41459 = CARTESIAN_POINT('Ctrl Pts',(-19.5313727356904,-12.4465805868045,
124.664292815845)) ;
#41460 = CARTESIAN_POINT('Ctrl Pts',(-19.6760004365552,-12.4532079500155,
124.64163824834)) ;
#41461 = CARTESIAN_POINT('Ctrl Pts',(-19.8134891857048,-12.4598668438148,
124.594653602306)) ;
#41462 = CARTESIAN_POINT('Ctrl Pts',(-19.8136929095394,-12.4598767106249,
124.594583982847)) ;
#41463 = CARTESIAN_POINT('Ctrl Pts',(-19.8138971253372,-12.4598866034866,
124.594514136294)) ;
#41464 = CARTESIAN_POINT('Ctrl Pts',(-19.8141008161599,-12.4598964712907,
124.594444410459)) ;
#41465 = CARTESIAN_POINT('Ctrl Pts',(-19.9512603591532,-12.4665411667972,
124.547493038525)) ;
#41466 = CARTESIAN_POINT('Ctrl Pts',(-20.079206290757,-12.4731348095734,124.47703975085)) ;
#41467 = CARTESIAN_POINT('Ctrl Pts',(-20.1922170357684,-12.4797820389184,
124.386235959366)) ;
#41468 = CARTESIAN_POINT('Ctrl Pts',(-20.2724857565317,-12.4845034005562,
124.321740285241)) ;
#41469 = CARTESIAN_POINT('Ctrl Pts',(-20.3443508215252,-12.4891911037781,
124.247678939301)) ;
#41470 = CARTESIAN_POINT('Ctrl Pts',(-20.4062803455442,-12.4938975845992,
124.165787064668)) ;
#41471 = CARTESIAN_POINT('Ctrl Pts',(-20.4317492598245,-12.4958331550479,
124.132108505558)) ;
#41472 = CARTESIAN_POINT('Ctrl Pts',(-20.4555379658399,-12.4977719013865,
124.097104804527)) ;
#41473 = CARTESIAN_POINT('Ctrl Pts',(-20.477537722934,-12.4997174708836,124.060897450153)) ;
#41474 = CARTESIAN_POINT('Ctrl Pts',(-20.4970770533415,-12.5014454502005,
124.02873948326)) ;
#41475 = CARTESIAN_POINT('Ctrl Pts',(-20.5151876206594,-12.5031867191234,
123.995654919809)) ;
#41476 = CARTESIAN_POINT('Ctrl Pts',(-20.5317606313249,-12.5049236383535,
123.961832368389)) ;
#41477 = CARTESIAN_POINT('Ctrl Pts',(-20.5790398477391,-12.5098786934024,
123.865343941481)) ;
#41478 = CARTESIAN_POINT('Ctrl Pts',(-20.6136630444319,-12.5147321491143,
123.76319238016)) ;
#41479 = CARTESIAN_POINT('Ctrl Pts',(-20.6348005037812,-12.5196443197352,
123.657945357767)) ;
#41480 = CARTESIAN_POINT('Ctrl Pts',(-20.6530044812983,-12.5238747734556,
123.567304642735)) ;
#41481 = CARTESIAN_POINT('Ctrl Pts',(-20.6610621663733,-12.5281007098675,
123.475112747438)) ;
#41482 = CARTESIAN_POINT('Ctrl Pts',(-20.6589406533506,-12.5323257106508,
123.383024669876)) ;
#41483 = CARTESIAN_POINT('Ctrl Pts',(-20.6577323804436,-12.5347319904727,
123.330577417381)) ;
#41484 = CARTESIAN_POINT('Ctrl Pts',(-20.6532216458869,-12.5371379668062,
123.278162196879)) ;
#41485 = CARTESIAN_POINT('Ctrl Pts',(-20.6453973814328,-12.5395443013262,
123.2260870805)) ;
#41486 = CARTESIAN_POINT('Ctrl Pts',(-20.6348831474355,-12.5427779297865,
123.156108622811)) ;
#41487 = CARTESIAN_POINT('Ctrl Pts',(-20.6184302716024,-12.5460210114688,
123.087076547404)) ;
#41488 = CARTESIAN_POINT('Ctrl Pts',(-20.5962158993244,-12.5492621658114,
123.019813422613)) ;
#41489 = CARTESIAN_POINT('Ctrl Pts',(-20.5948009399898,-12.5494686133101,
123.015529052787)) ;
#41490 = CARTESIAN_POINT('Ctrl Pts',(-20.5933626230645,-12.5496750529894,
123.011251858573)) ;
#41491 = CARTESIAN_POINT('Ctrl Pts',(-20.5919010016528,-12.5498814819081,
123.00698205237)) ;
#41492 = CARTESIAN_POINT('Ctrl Pts',(-20.591901001653,-12.5498814819195,123.006982052371)) ;
#41493 = CARTESIAN_POINT('Ctrl Pts',(-20.5823589431143,-12.5512291337733,
122.979107022349)) ;
#41494 = CARTESIAN_POINT('Ctrl Pts',(-20.5718380184699,-12.5525754721182,
122.951587396436)) ;
#41495 = CARTESIAN_POINT('Ctrl Pts',(-20.5566068789105,-12.554364799924,122.915613370786)) ;
#41496 = CARTESIAN_POINT('Ctrl Pts',(-20.5527611641633,-12.5548048764859,
122.906814087733)) ;
#41497 = CARTESIAN_POINT('Ctrl Pts',(-20.5450459304218,-12.5556659701827,
122.889701173019)) ;
#41498 = CARTESIAN_POINT('Ctrl Pts',(-20.5411855614764,-12.5560869246646,
122.881384074547)) ;
#41499 = CARTESIAN_POINT('Ctrl Pts',(-20.5325850560412,-12.5570042627748,
122.863375967916)) ;
#41500 = CARTESIAN_POINT('Ctrl Pts',(-20.5278102677573,-12.5575008059757,
122.853702336013)) ;
#41501 = CARTESIAN_POINT('Ctrl Pts',(-20.5099171526103,-12.5593178066816,
122.818603391076)) ;
#41502 = CARTESIAN_POINT('Ctrl Pts',(-20.4960524227534,-12.5606460879697,
122.793569051698)) ;
#41503 = CARTESIAN_POINT('Ctrl Pts',(-20.4689003040132,-12.563103295292,122.748283142712)) ;
#41504 = CARTESIAN_POINT('Ctrl Pts',(-20.4558595340843,-12.5642297729607,
122.727898901248)) ;
#41505 = CARTESIAN_POINT('Ctrl Pts',(-20.4302918678698,-12.5663368883533,
122.690379167524)) ;
#41506 = CARTESIAN_POINT('Ctrl Pts',(-20.4179041026958,-12.5673180750482,
122.67315909667)) ;
#41507 = CARTESIAN_POINT('Ctrl Pts',(-20.4021421413916,-12.5685190263038,
122.652384948628)) ;
#41508 = CARTESIAN_POINT('Ctrl Pts',(-20.399177560185,-12.5687429472497,122.648524684188)) ;
#41509 = CARTESIAN_POINT('Ctrl Pts',(-20.3938451328287,-12.5691422581575,
122.641664500751)) ;
#41510 = CARTESIAN_POINT('Ctrl Pts',(-20.3914859348972,-12.5693177379361,
122.638657943332)) ;
#41511 = CARTESIAN_POINT('Ctrl Pts',(-20.3866874495288,-12.5696722825805,
122.632600172743)) ;
#41512 = CARTESIAN_POINT('Ctrl Pts',(-20.3842475723445,-12.56985133876,122.629549479762)) ;
#41513 = CARTESIAN_POINT('Ctrl Pts',(-20.3793277569038,-12.5702099774409,
122.623456776567)) ;
#41514 = CARTESIAN_POINT('Ctrl Pts',(-20.3768477118311,-12.5703895564525,
122.620414908624)) ;
#41515 = CARTESIAN_POINT('Ctrl Pts',(-20.3697971849743,-12.5708967125171,
122.611849857049)) ;
#41516 = CARTESIAN_POINT('Ctrl Pts',(-20.3651934473058,-12.5712239111852,
122.606354229413)) ;
#41517 = CARTESIAN_POINT('Ctrl Pts',(-20.3398192354273,-12.5730063449014,
122.57658821007)) ;
#41518 = CARTESIAN_POINT('Ctrl Pts',(-20.3181713921682,-12.5744508679129,
122.553081106076)) ;
#41519 = CARTESIAN_POINT('Ctrl Pts',(-20.2713672340028,-12.5774452618565,
122.506012022865)) ;
#41520 = CARTESIAN_POINT('Ctrl Pts',(-20.2460895006122,-12.5789942678939,
122.482609041878)) ;
#41521 = CARTESIAN_POINT('Ctrl Pts',(-20.205190152754,-12.5814291326774,122.447767194467)) ;
#41522 = CARTESIAN_POINT('Ctrl Pts',(-20.1902149311921,-12.5823059052257,
122.435596778385)) ;
#41523 = CARTESIAN_POINT('Ctrl Pts',(-20.1638910135029,-12.5838226693699,
122.415196710945)) ;
#41524 = CARTESIAN_POINT('Ctrl Pts',(-20.1526744831753,-12.5844616261347,
122.406802253454)) ;
#41525 = CARTESIAN_POINT('Ctrl Pts',(-20.1314495042424,-12.5856575004875,
122.391467241805)) ;
#41526 = CARTESIAN_POINT('Ctrl Pts',(-20.1214760949646,-12.5862141527252,
122.384480962141)) ;
#41527 = CARTESIAN_POINT('Ctrl Pts',(-20.1011791499057,-12.587336753662,122.37070077624)) ;
#41528 = CARTESIAN_POINT('Ctrl Pts',(-20.0908537279533,-12.5879026562735,
122.363912007451)) ;
#41529 = CARTESIAN_POINT('Ctrl Pts',(-20.0670701829121,-12.5891948400098,
122.3487750351)) ;
#41530 = CARTESIAN_POINT('Ctrl Pts',(-20.0535506550379,-12.5899212991964,
122.340527254705)) ;
#41531 = CARTESIAN_POINT('Ctrl Pts',(-20.019016799078,-12.5917579196349,122.320349601424)) ;
#41532 = CARTESIAN_POINT('Ctrl Pts',(-19.9978065224073,-12.5928685898015,
122.308768060688)) ;
#41533 = CARTESIAN_POINT('Ctrl Pts',(-19.93325379259,-12.5962035556881,122.275912295499)) ;
#41534 = CARTESIAN_POINT('Ctrl Pts',(-19.8890016377507,-12.5984314623645,
122.25652660003)) ;
#41535 = CARTESIAN_POINT('Ctrl Pts',(-19.8175637829835,-12.6019633799019,
122.230045627904)) ;
#41536 = CARTESIAN_POINT('Ctrl Pts',(-19.7910698527825,-12.6032577175856,
122.221222105843)) ;
#41537 = CARTESIAN_POINT('Ctrl Pts',(-19.7479684467081,-12.6053351370545,
122.208454446933)) ;
#41538 = CARTESIAN_POINT('Ctrl Pts',(-19.7315369229615,-12.6061207124371,
122.203950261288)) ;
#41539 = CARTESIAN_POINT('Ctrl Pts',(-19.7147727171071,-12.6069159056836,
122.199721333712)) ;
#41540 = CARTESIAN_POINT('Ctrl Pts',(-19.7145270194464,-12.6069275587511,
122.199659433633)) ;
#41541 = CARTESIAN_POINT('Ctrl Pts',(-19.7140600882535,-12.6069497020197,
122.19954194784)) ;
#41542 = CARTESIAN_POINT('Ctrl Pts',(-19.7138388583028,-12.6069601923071,
122.199486347973)) ;
#41543 = CARTESIAN_POINT('Ctrl Pts',(-19.7134183934058,-12.6069801278413,
122.199380798416)) ;
#41544 = CARTESIAN_POINT('Ctrl Pts',(-19.7132191613582,-12.6069895731578,
122.199330837273)) ;
#41545 = CARTESIAN_POINT('Ctrl Pts',(-19.7128404665971,-12.6070075248681,
122.19923597172)) ;
#41546 = CARTESIAN_POINT('Ctrl Pts',(-19.7126610062194,-12.6070160313187,
122.19919105804)) ;
#41547 = CARTESIAN_POINT('Ctrl Pts',(-19.7123198520826,-12.607032200713,122.199105757619)) ;
#41548 = CARTESIAN_POINT('Ctrl Pts',(-19.7121581602287,-12.6070398637017,
122.199065363379)) ;
#41549 = CARTESIAN_POINT('Ctrl Pts',(-19.7118507434955,-12.6070544318554,
122.198988629121)) ;
#41550 = CARTESIAN_POINT('Ctrl Pts',(-19.7117050201375,-12.6070613370577,
122.198952283027)) ;
#41551 = CARTESIAN_POINT('Ctrl Pts',(-19.7114279248196,-12.6070744665121,
122.198883223387)) ;
#41552 = CARTESIAN_POINT('Ctrl Pts',(-19.7112965539404,-12.6070806908015,
122.198850504881)) ;
#41553 = CARTESIAN_POINT('Ctrl Pts',(-19.7110467140566,-12.6070925273652,
122.198788324245)) ;
#41554 = CARTESIAN_POINT('Ctrl Pts',(-19.7109282459476,-12.6070981396689,
122.198758858101)) ;
#41555 = CARTESIAN_POINT('Ctrl Pts',(-19.710702911402,-12.6071088140654,122.198702846505)) ;
#41556 = CARTESIAN_POINT('Ctrl Pts',(-19.7105960459328,-12.6071138761706,
122.19867629786)) ;
#41557 = CARTESIAN_POINT('Ctrl Pts',(-19.7103927509742,-12.6071235055567,
122.198625821704)) ;
#41558 = CARTESIAN_POINT('Ctrl Pts',(-19.7102963222004,-12.6071280728509,
122.198601891585)) ;
#41559 = CARTESIAN_POINT('Ctrl Pts',(-19.7101128553429,-12.6071367622617,
122.198556384995)) ;
#41560 = CARTESIAN_POINT('Ctrl Pts',(-19.7100258179597,-12.6071408843834,
122.198534806435)) ;
#41561 = CARTESIAN_POINT('Ctrl Pts',(-19.709860196494,-12.6071487279555,122.198493764)) ;
#41562 = CARTESIAN_POINT('Ctrl Pts',(-19.709781612976,-12.6071524494102,122.198474298425)) ;
#41563 = CARTESIAN_POINT('Ctrl Pts',(-19.7096320586394,-12.6071595315467,
122.198437268405)) ;
#41564 = CARTESIAN_POINT('Ctrl Pts',(-19.7095610879269,-12.6071628922488,
122.198419702491)) ;
#41565 = CARTESIAN_POINT('Ctrl Pts',(-19.7094260047425,-12.6071692886795,
122.198386280719)) ;
#41566 = CARTESIAN_POINT('Ctrl Pts',(-19.7093618923431,-12.6071723244254,
122.198370423662)) ;
#41567 = CARTESIAN_POINT('Ctrl Pts',(-19.7092398482187,-12.6071781030863,
122.198340248493)) ;
#41568 = CARTESIAN_POINT('Ctrl Pts',(-19.7091819168212,-12.6071808460027,
122.198325929471)) ;
#41569 = CARTESIAN_POINT('Ctrl Pts',(-19.7090716261686,-12.607186067866,122.198298677086)) ;
#41570 = CARTESIAN_POINT('Ctrl Pts',(-19.7090192673479,-12.6071885468059,
122.198285743023)) ;
#41571 = CARTESIAN_POINT('Ctrl Pts',(-19.7089195754003,-12.6071932666276,
122.198261123227)) ;
#41572 = CARTESIAN_POINT('Ctrl Pts',(-19.7088722423718,-12.6071955075157,
122.198249436861)) ;
#41573 = CARTESIAN_POINT('Ctrl Pts',(-19.7086621076391,-12.6072054557069,
122.198197568342)) ;
#41574 = CARTESIAN_POINT('Ctrl Pts',(-19.7084992986925,-12.6072131628154,
122.19815741622)) ;
#41575 = CARTESIAN_POINT('Ctrl Pts',(-19.708179391157,-12.6072283055615,122.198078588555)) ;
#41576 = CARTESIAN_POINT('Ctrl Pts',(-19.7080222928393,-12.6072357412268,
122.198039910678)) ;
#41577 = CARTESIAN_POINT('Ctrl Pts',(-19.7077135496704,-12.6072503533658,
122.197963961149)) ;
#41578 = CARTESIAN_POINT('Ctrl Pts',(-19.7075619055399,-12.6072575298429,
122.197926687461)) ;
#41579 = CARTESIAN_POINT('Ctrl Pts',(-19.7072638259343,-12.6072716353024,
122.197853479587)) ;
#41580 = CARTESIAN_POINT('Ctrl Pts',(-19.7071173905713,-12.6072785643139,
122.197817543388)) ;
#41581 = CARTESIAN_POINT('Ctrl Pts',(-19.7042389243756,-12.6074147579478,
122.197111701068)) ;
#41582 = CARTESIAN_POINT('Ctrl Pts',(-19.7015046439169,-12.6075439648712,
122.196450991845)) ;
#41583 = CARTESIAN_POINT('Ctrl Pts',(-19.6987043805034,-12.607676123953,122.195784334832)) ;
#41584 = CARTESIAN_POINT('Ctrl Pts',(-19.6986406059296,-12.6076791337209,
122.195769157359)) ;
#41585 = CARTESIAN_POINT('Ctrl Pts',(-19.698514362601,-12.6076850914561,122.195739123674)) ;
#41586 = CARTESIAN_POINT('Ctrl Pts',(-19.6984518936512,-12.6076880394362,
122.1957242672)) ;
#41587 = CARTESIAN_POINT('Ctrl Pts',(-19.6983282031066,-12.6076938763653,
122.195694860969)) ;
#41588 = CARTESIAN_POINT('Ctrl Pts',(-19.6982669812627,-12.6076967653295,
122.195680310952)) ;
#41589 = CARTESIAN_POINT('Ctrl Pts',(-19.6981457281189,-12.6077024869176,
122.195651503537)) ;
#41590 = CARTESIAN_POINT('Ctrl Pts',(-19.6980856973534,-12.6077053195195,
122.195637246077)) ;
#41591 = CARTESIAN_POINT('Ctrl Pts',(-19.6979667723343,-12.6077109309419,
122.195609010383)) ;
#41592 = CARTESIAN_POINT('Ctrl Pts',(-19.6979078780992,-12.6077137097645,
122.195595031978)) ;
#41593 = CARTESIAN_POINT('Ctrl Pts',(-19.6977911743134,-12.6077192160826,
122.195567341568)) ;
#41594 = CARTESIAN_POINT('Ctrl Pts',(-19.6977333646325,-12.6077219435868,
122.195553629367)) ;
#41595 = CARTESIAN_POINT('Ctrl Pts',(-19.6976187794936,-12.6077273496572,
122.195526458909)) ;
#41596 = CARTESIAN_POINT('Ctrl Pts',(-19.6975620044722,-12.6077300282052,
122.1955130006)) ;
#41597 = CARTESIAN_POINT('Ctrl Pts',(-19.697449440663,-12.6077353386347,122.195486326088)) ;
#41598 = CARTESIAN_POINT('Ctrl Pts',(-19.6973936515213,-12.6077379705353,
122.195473109657)) ;
#41599 = CARTESIAN_POINT('Ctrl Pts',(-19.6972830127344,-12.607743189882,122.195446907401)) ;
#41600 = CARTESIAN_POINT('Ctrl Pts',(-19.6972281633212,-12.6077457773194,
122.195433921495)) ;
#41601 = CARTESIAN_POINT('Ctrl Pts',(-19.6971193589717,-12.6077509098701,
122.195408169227)) ;
#41602 = CARTESIAN_POINT('Ctrl Pts',(-19.6970654040202,-12.6077534549862,
122.195395402735)) ;
#41603 = CARTESIAN_POINT('Ctrl Pts',(-19.6969583450318,-12.6077585049555,
122.19537007861)) ;
#41604 = CARTESIAN_POINT('Ctrl Pts',(-19.6969052412423,-12.607761009799,122.195357520917)) ;
#41605 = CARTESIAN_POINT('Ctrl Pts',(-19.6967998427331,-12.6077659812027,
122.195332604143)) ;
#41606 = CARTESIAN_POINT('Ctrl Pts',(-19.6967475478354,-12.6077684477731,
122.195320244909)) ;
#41607 = CARTESIAN_POINT('Ctrl Pts',(-19.6966437264461,-12.6077733445542,
122.195295715112)) ;
#41608 = CARTESIAN_POINT('Ctrl Pts',(-19.6965921998974,-12.6077757747692,
122.195283544432)) ;
#41609 = CARTESIAN_POINT('Ctrl Pts',(-19.6964898757104,-12.6077806007074,
122.195259382105)) ;
#41610 = CARTESIAN_POINT('Ctrl Pts',(-19.6964390779954,-12.6077829964357,
122.195247390343)) ;
#41611 = CARTESIAN_POINT('Ctrl Pts',(-19.6963381731068,-12.6077877552149,
122.195223576507)) ;
#41612 = CARTESIAN_POINT('Ctrl Pts',(-19.6962880659664,-12.6077901182656,
122.195211754349)) ;
#41613 = CARTESIAN_POINT('Ctrl Pts',(-19.6961885047292,-12.6077948134625,
122.195188270605)) ;
#41614 = CARTESIAN_POINT('Ctrl Pts',(-19.6961390510113,-12.6077971455921,
122.195176609023)) ;
#41615 = CARTESIAN_POINT('Ctrl Pts',(-19.6960407609794,-12.6078017806316,
122.195153437773)) ;
#41616 = CARTESIAN_POINT('Ctrl Pts',(-19.6959919240049,-12.6078040835739,
122.195141927871)) ;
#41617 = CARTESIAN_POINT('Ctrl Pts',(-19.6958948320165,-12.6078086619139,
122.195119051393)) ;
#41618 = CARTESIAN_POINT('Ctrl Pts',(-19.6958465770502,-12.6078109373106,
122.195107684755)) ;
#41619 = CARTESIAN_POINT('Ctrl Pts',(-19.6957506146551,-12.6078154621864,
122.19508508648)) ;
#41620 = CARTESIAN_POINT('Ctrl Pts',(-19.6957029068916,-12.6078177116823,
122.195073854695)) ;
#41621 = CARTESIAN_POINT('Ctrl Pts',(-19.6956080047544,-12.6078221863699,
122.195051517883)) ;
#41622 = CARTESIAN_POINT('Ctrl Pts',(-19.6955608109201,-12.6078244115372,
122.195040412919)) ;
#41623 = CARTESIAN_POINT('Ctrl Pts',(-19.6903983371163,-12.6080678145502,
122.193825971945)) ;
#41624 = CARTESIAN_POINT('Ctrl Pts',(-19.6852755117442,-12.6083087869214,
122.192654899501)) ;
#41625 = CARTESIAN_POINT('Ctrl Pts',(-19.6750393244738,-12.6087892085501,
122.190382742671)) ;
#41626 = CARTESIAN_POINT('Ctrl Pts',(-19.6699261315132,-12.6090286549086,
122.189281379645)) ;
#41627 = CARTESIAN_POINT('Ctrl Pts',(-19.6576159234169,-12.609603906466,122.186710547548)) ;
#41628 = CARTESIAN_POINT('Ctrl Pts',(-19.6504125670521,-12.6099395127285,
122.185272359259)) ;
#41629 = CARTESIAN_POINT('Ctrl Pts',(-19.6186345223002,-12.6114160073915,
122.179218471343)) ;
#41630 = CARTESIAN_POINT('Ctrl Pts',(-19.5939371351516,-12.612552702159,122.175277227788)) ;
#41631 = CARTESIAN_POINT('Ctrl Pts',(-19.5429227890274,-12.6148881231595,
122.168698845769)) ;
#41632 = CARTESIAN_POINT('Ctrl Pts',(-19.5166069563132,-12.6160860748548,
122.166150720282)) ;
#41633 = CARTESIAN_POINT('Ctrl Pts',(-19.4774895783422,-12.617868798666,122.163611898003)) ;
#41634 = CARTESIAN_POINT('Ctrl Pts',(-19.4647370547848,-12.6184503341318,
122.162980246681)) ;
#41635 = CARTESIAN_POINT('Ctrl Pts',(-19.4481949718653,-12.6192065964796,
122.162414773797)) ;
#41636 = CARTESIAN_POINT('Ctrl Pts',(-19.4444122264889,-12.6193796709886,
122.162302660851)) ;
#41637 = CARTESIAN_POINT('Ctrl Pts',(-19.4370994027916,-12.6197145334933,
122.162119157728)) ;
#41638 = CARTESIAN_POINT('Ctrl Pts',(-19.4335694201136,-12.6198762945393,
122.162045542757)) ;
#41639 = CARTESIAN_POINT('Ctrl Pts',(-19.4273966833207,-12.6201593496691,
122.161942977503)) ;
#41640 = CARTESIAN_POINT('Ctrl Pts',(-19.4247540579576,-12.6202805900396,
122.161907450853)) ;
#41641 = CARTESIAN_POINT('Ctrl Pts',(-19.4158363722518,-12.620689914162,122.161815849925)) ;
#41642 = CARTESIAN_POINT('Ctrl Pts',(-19.4095610187109,-12.6209782745147,
122.161798648365)) ;
#41643 = CARTESIAN_POINT('Ctrl Pts',(-19.3763857784635,-12.6225041419926,
122.161957530909)) ;
#41644 = CARTESIAN_POINT('Ctrl Pts',(-19.3494969871598,-12.6237456414186,
122.162954670679)) ;
#41645 = CARTESIAN_POINT('Ctrl Pts',(-19.3030391145788,-12.6258943829398,
122.16618142812)) ;
#41646 = CARTESIAN_POINT('Ctrl Pts',(-19.2834516409819,-12.6268015222898,
122.16800727749)) ;
#41647 = CARTESIAN_POINT('Ctrl Pts',(-19.2535954058591,-12.6281856795908,
122.17150283852)) ;
#41648 = CARTESIAN_POINT('Ctrl Pts',(-19.2432908679898,-12.6286636822435,
122.172839730654)) ;
#41649 = CARTESIAN_POINT('Ctrl Pts',(-19.2328541455855,-12.6291481394445,
122.174326313922)) ;
#41650 = CARTESIAN_POINT('Ctrl Pts',(-19.2327041180626,-12.6291551035688,
122.174347711342)) ;
#41651 = CARTESIAN_POINT('Ctrl Pts',(-19.2320853257231,-12.6291838275611,
122.17443608037)) ;
#41652 = CARTESIAN_POINT('Ctrl Pts',(-19.2316165951017,-12.6292055864462,
122.174503291056)) ;
#41653 = CARTESIAN_POINT('Ctrl Pts',(-19.2307133962872,-12.6292475150354,
122.174633323401)) ;
#41654 = CARTESIAN_POINT('Ctrl Pts',(-19.2302789227293,-12.6292676848928,
122.174696107623)) ;
#41655 = CARTESIAN_POINT('Ctrl Pts',(-19.2294408644839,-12.6293065917713,
122.174817663155)) ;
#41656 = CARTESIAN_POINT('Ctrl Pts',(-19.229037275287,-12.6293253289209,122.174876403138)) ;
#41657 = CARTESIAN_POINT('Ctrl Pts',(-19.2282579490958,-12.6293615111381,
122.174990218902)) ;
#41658 = CARTESIAN_POINT('Ctrl Pts',(-19.2278822083674,-12.6293789563107,
122.175045268398)) ;
#41659 = CARTESIAN_POINT('Ctrl Pts',(-19.2271558456986,-12.6294126812908,
122.175152025387)) ;
#41660 = CARTESIAN_POINT('Ctrl Pts',(-19.2268052205377,-12.6294289611899,
122.175203710792)) ;
#41661 = CARTESIAN_POINT('Ctrl Pts',(-19.2261266277404,-12.6294604697388,
122.175304036564)) ;
#41662 = CARTESIAN_POINT('Ctrl Pts',(-19.2257986573805,-12.6294756984659,
122.175352658314)) ;
#41663 = CARTESIAN_POINT('Ctrl Pts',(-19.2251631568053,-12.6295052074923,
122.175447129968)) ;
#41664 = CARTESIAN_POINT('Ctrl Pts',(-19.224855624276,-12.629519487857,122.175492964141)) ;
#41665 = CARTESIAN_POINT('Ctrl Pts',(-19.2242590000135,-12.6295471928808,
122.175582111665)) ;
#41666 = CARTESIAN_POINT('Ctrl Pts',(-19.2239699064247,-12.6295606175903,
122.175625411672)) ;
#41667 = CARTESIAN_POINT('Ctrl Pts',(-19.2234083555449,-12.6295866949983,
122.175709721338)) ;
#41668 = CARTESIAN_POINT('Ctrl Pts',(-19.2231358964744,-12.629599347749,122.175750719693)) ;
#41669 = CARTESIAN_POINT('Ctrl Pts',(-19.2226059834077,-12.6296239569056,
122.175830637693)) ;
#41670 = CARTESIAN_POINT('Ctrl Pts',(-19.2223485279447,-12.6296359133535,
122.175869547708)) ;
#41671 = CARTESIAN_POINT('Ctrl Pts',(-19.2218471448554,-12.6296591984346,
122.175945483481)) ;
#41672 = CARTESIAN_POINT('Ctrl Pts',(-19.2216032160826,-12.6296705270986,
122.175982501006)) ;
#41673 = CARTESIAN_POINT('Ctrl Pts',(-19.2211275459536,-12.6296926188009,
122.17605483063)) ;
#41674 = CARTESIAN_POINT('Ctrl Pts',(-19.2208958034993,-12.6297033818708,
122.176090135709)) ;
#41675 = CARTESIAN_POINT('Ctrl Pts',(-19.2204432864389,-12.629724398972,122.17615920521)) ;
#41676 = CARTESIAN_POINT('Ctrl Pts',(-19.2202225108943,-12.6297346530301,
122.176192963621)) ;
#41677 = CARTESIAN_POINT('Ctrl Pts',(-19.2197908145895,-12.6297547037577,
122.176259091973)) ;
#41678 = CARTESIAN_POINT('Ctrl Pts',(-19.2195798930826,-12.6297645004474,
122.176291456753)) ;
#41679 = CARTESIAN_POINT('Ctrl Pts',(-19.219166885471,-12.6297836837448,122.176354938821)) ;
#41680 = CARTESIAN_POINT('Ctrl Pts',(-19.2189647987147,-12.6297930703704,
122.176386051681)) ;
#41681 = CARTESIAN_POINT('Ctrl Pts',(-19.2185685230648,-12.6298114770519,
122.176447161003)) ;
#41682 = CARTESIAN_POINT('Ctrl Pts',(-19.2183743335841,-12.6298204971244,
122.176477153672)) ;
#41683 = CARTESIAN_POINT('Ctrl Pts',(-19.2179929859661,-12.6298382109194,
122.176536145082)) ;
#41684 = CARTESIAN_POINT('Ctrl Pts',(-19.2178058273476,-12.6298469046551,
122.17656514057)) ;
#41685 = CARTESIAN_POINT('Ctrl Pts',(-19.2174377361236,-12.6298640031592,
122.176622252649)) ;
#41686 = CARTESIAN_POINT('Ctrl Pts',(-19.217256803013,-12.6298724079432,122.176650366475)) ;
#41687 = CARTESIAN_POINT('Ctrl Pts',(-19.21690040926,-12.6298889635257,122.176705824004)) ;
#41688 = CARTESIAN_POINT('Ctrl Pts',(-19.2167249482493,-12.6298971143347,
122.176733165344)) ;
#41689 = CARTESIAN_POINT('Ctrl Pts',(-19.2163787882633,-12.6299131949506,
122.176787181534)) ;
#41690 = CARTESIAN_POINT('Ctrl Pts',(-19.2162080890678,-12.6299211247621,
122.176813854373)) ;
#41691 = CARTESIAN_POINT('Ctrl Pts',(-19.2158707773977,-12.6299367947389,
122.176866633117)) ;
#41692 = CARTESIAN_POINT('Ctrl Pts',(-19.2157041645138,-12.6299445349184,
122.176892737376)) ;
#41693 = CARTESIAN_POINT('Ctrl Pts',(-19.215374376648,-12.6299598557597,122.176944475638)) ;
#41694 = CARTESIAN_POINT('Ctrl Pts',(-19.2152112016524,-12.6299674364181,
122.176970108237)) ;
#41695 = CARTESIAN_POINT('Ctrl Pts',(-19.214887659885,-12.6299824674594,122.177020998013)) ;
#41696 = CARTESIAN_POINT('Ctrl Pts',(-19.2147272926278,-12.6299899178617,
122.177046254141)) ;
#41697 = CARTESIAN_POINT('Ctrl Pts',(-19.2144087467008,-12.6300047171697,
122.177096485315)) ;
#41698 = CARTESIAN_POINT('Ctrl Pts',(-19.2142505681731,-12.6300120660663,
122.177121459475)) ;
#41699 = CARTESIAN_POINT('Ctrl Pts',(-19.2139357821194,-12.6300266910494,
122.177171221757)) ;
#41700 = CARTESIAN_POINT('Ctrl Pts',(-19.2137791745908,-12.6300339671342,
122.177196009267)) ;
#41701 = CARTESIAN_POINT('Ctrl Pts',(-19.2134669057242,-12.6300484755186,
122.177245495431)) ;
#41702 = CARTESIAN_POINT('Ctrl Pts',(-19.2133112441929,-12.6300557078261,
122.177270193752)) ;
#41703 = CARTESIAN_POINT('Ctrl Pts',(-19.2057079430292,-12.6304089747836,
122.178478059654)) ;
#41704 = CARTESIAN_POINT('Ctrl Pts',(-19.1982711444168,-12.6307547041646,
122.179728571221)) ;
#41705 = CARTESIAN_POINT('Ctrl Pts',(-19.1834408532855,-12.6314446406511,
122.182360523757)) ;
#41706 = CARTESIAN_POINT('Ctrl Pts',(-19.1760476010201,-12.6317888352755,
122.183741553141)) ;
#41707 = CARTESIAN_POINT('Ctrl Pts',(-19.1551189992639,-12.6327640416747,
122.187846740422)) ;
#41708 = CARTESIAN_POINT('Ctrl Pts',(-19.1416156682069,-12.6333942802176,
122.190728545803)) ;
#41709 = CARTESIAN_POINT('Ctrl Pts',(-19.0661340313394,-12.636925871898,122.208149672345)) ;
#41710 = CARTESIAN_POINT('Ctrl Pts',(-19.0052893743557,-12.6398087058573,
122.227183451971)) ;
#41711 = CARTESIAN_POINT('Ctrl Pts',(-18.9149366045977,-12.6442413311643,
122.263222930508)) ;
#41712 = CARTESIAN_POINT('Ctrl Pts',(-18.8842284343812,-12.6457738995312,
122.27693155338)) ;
#41713 = CARTESIAN_POINT('Ctrl Pts',(-18.8391459719155,-12.6480717008126,
122.299278974222)) ;
#41714 = CARTESIAN_POINT('Ctrl Pts',(-18.824331823361,-12.6488348427199,122.30699597971)) ;
#41715 = CARTESIAN_POINT('Ctrl Pts',(-18.7999530658644,-12.6501057378032,
122.32032320454)) ;
#41716 = CARTESIAN_POINT('Ctrl Pts',(-18.7903004680454,-12.6506129655805,
122.32576797826)) ;
#41717 = CARTESIAN_POINT('Ctrl Pts',(-18.7783091002417,-12.6512485272351,
122.33274378916)) ;
#41718 = CARTESIAN_POINT('Ctrl Pts',(-18.7759013432938,-12.6513764198403,
122.33415528227)) ;
#41719 = CARTESIAN_POINT('Ctrl Pts',(-18.7670487639839,-12.6518476839976,
122.339384823345)) ;
#41720 = CARTESIAN_POINT('Ctrl Pts',(-18.7606335807206,-12.6521912364205,
122.343252712879)) ;
#41721 = CARTESIAN_POINT('Ctrl Pts',(-18.7464048898659,-12.6529580188698,
122.352006930493)) ;
#41722 = CARTESIAN_POINT('Ctrl Pts',(-18.7386098729769,-12.6533813616417,
122.356922469633)) ;
#41723 = CARTESIAN_POINT('Ctrl Pts',(-18.7182237799422,-12.6544976850978,
122.370095243963)) ;
#41724 = CARTESIAN_POINT('Ctrl Pts',(-18.7057263480336,-12.655191387144,122.378494532999)) ;
#41725 = CARTESIAN_POINT('Ctrl Pts',(-18.661383944203,-12.6576898506211,122.409473661028)) ;
#41726 = CARTESIAN_POINT('Ctrl Pts',(-18.630449572009,-12.6595074050684,122.433316059771)) ;
#41727 = CARTESIAN_POINT('Ctrl Pts',(-18.5761658949485,-12.6628381702742,
122.479362045516)) ;
#41728 = CARTESIAN_POINT('Ctrl Pts',(-18.5524608573029,-12.6643427238562,
122.501096074152)) ;
#41729 = CARTESIAN_POINT('Ctrl Pts',(-18.5214989868315,-12.6663677019011,
122.531763624268)) ;
#41730 = CARTESIAN_POINT('Ctrl Pts',(-18.5134887348652,-12.6668974640506,
122.539918401899)) ;
#41731 = CARTESIAN_POINT('Ctrl Pts',(-18.5014977361161,-12.667699428476,122.552465447875)) ;
#41732 = CARTESIAN_POINT('Ctrl Pts',(-18.4974345599665,-12.6679727817489,
122.556778016611)) ;
#41733 = CARTESIAN_POINT('Ctrl Pts',(-18.4901635195785,-12.668464873343,122.564606119295)) ;
#41734 = CARTESIAN_POINT('Ctrl Pts',(-18.4869447827434,-12.6686837672033,
122.56811138798)) ;
#41735 = CARTESIAN_POINT('Ctrl Pts',(-18.4815131203139,-12.6690549693455,
122.574094806925)) ;
#41736 = CARTESIAN_POINT('Ctrl Pts',(-18.4792899194231,-12.6692074283339,
122.576563548974)) ;
#41737 = CARTESIAN_POINT('Ctrl Pts',(-18.4750700222158,-12.6694978250517,
122.581287247649)) ;
#41738 = CARTESIAN_POINT('Ctrl Pts',(-18.4730715829044,-12.6696357878119,
122.583540614292)) ;
#41739 = CARTESIAN_POINT('Ctrl Pts',(-18.4684621772687,-12.6699550260662,
122.588776006018)) ;
#41740 = CARTESIAN_POINT('Ctrl Pts',(-18.4658572084882,-12.6701362118605,
122.591763273304)) ;
#41741 = CARTESIAN_POINT('Ctrl Pts',(-18.4577135960731,-12.6707050992548,
122.601192182458)) ;
#41742 = CARTESIAN_POINT('Ctrl Pts',(-18.4522263678402,-12.6710920427928,
122.607677948871)) ;
#41743 = CARTESIAN_POINT('Ctrl Pts',(-18.42261589974,-12.6732008171969,122.643409215233)) ;
#41744 = CARTESIAN_POINT('Ctrl Pts',(-18.3997664505841,-12.6749032551716,
122.673684744541)) ;
#41745 = CARTESIAN_POINT('Ctrl Pts',(-18.3538817853352,-12.6785388722717,
122.740606617841)) ;
#41746 = CARTESIAN_POINT('Ctrl Pts',(-18.3313019093948,-12.6804754585744,
122.77750466779)) ;
#41747 = CARTESIAN_POINT('Ctrl Pts',(-18.3014044680669,-12.6833092522263,
122.832584729281)) ;
#41748 = CARTESIAN_POINT('Ctrl Pts',(-18.2925298800675,-12.6841907254495,
122.849885131158)) ;
#41749 = CARTESIAN_POINT('Ctrl Pts',(-18.2792955763098,-12.6855724906585,
122.877237398557)) ;
#41750 = CARTESIAN_POINT('Ctrl Pts',(-18.2746583098953,-12.6860709525609,
122.887151595537)) ;
#41751 = CARTESIAN_POINT('Ctrl Pts',(-18.267106157034,-12.6869076388084,122.903866177355)) ;
#41752 = CARTESIAN_POINT('Ctrl Pts',(-18.2641203595118,-12.6872454130824,
122.910633865986)) ;
#41753 = CARTESIAN_POINT('Ctrl Pts',(-18.2587962826136,-12.6878607690106,
122.922997572714)) ;
#41754 = CARTESIAN_POINT('Ctrl Pts',(-18.2564383210447,-12.6881382245845,
122.92858487498)) ;
#41755 = CARTESIAN_POINT('Ctrl Pts',(-18.251730558928,-12.6887024069194,122.93997073982)) ;
#41756 = CARTESIAN_POINT('Ctrl Pts',(-18.2493834459303,-12.6889891411828,
122.945770230628)) ;
#41757 = CARTESIAN_POINT('Ctrl Pts',(-18.2443071692216,-12.6896215946021,
122.958589135016)) ;
#41758 = CARTESIAN_POINT('Ctrl Pts',(-18.2415977053822,-12.6899674154144,
122.965616083993)) ;
#41759 = CARTESIAN_POINT('Ctrl Pts',(-18.2343375333888,-12.6909173795375,
122.984964323006)) ;
#41760 = CARTESIAN_POINT('Ctrl Pts',(-18.2299172780155,-12.6915222193984,
122.997333491861)) ;
#41761 = CARTESIAN_POINT('Ctrl Pts',(-18.2093085207767,-12.694478434943,123.058003660494)) ;
#41762 = CARTESIAN_POINT('Ctrl Pts',(-18.1958882779016,-12.6968431854278,
123.107193023935)) ;
#41763 = CARTESIAN_POINT('Ctrl Pts',(-18.1774542858308,-12.7010750666826,
123.195745579125)) ;
#41764 = CARTESIAN_POINT('Ctrl Pts',(-18.1712402661295,-12.7029291714922,
123.23478869457)) ;
#41765 = CARTESIAN_POINT('Ctrl Pts',(-18.1654539819847,-12.7053718894351,
123.286974583963)) ;
#41766 = CARTESIAN_POINT('Ctrl Pts',(-18.1642235341705,-12.7059746615582,
123.299910144494)) ;
#41767 = CARTESIAN_POINT('Ctrl Pts',(-18.1626765950558,-12.7068782140379,
123.319390404262)) ;
#41768 = CARTESIAN_POINT('Ctrl Pts',(-18.1622095214984,-12.7071804742072,
123.325922180861)) ;
#41769 = CARTESIAN_POINT('Ctrl Pts',(-18.1615327254344,-12.7076716790464,
123.336561296873)) ;
#41770 = CARTESIAN_POINT('Ctrl Pts',(-18.1612919099343,-12.7078609439941,
123.340666516006)) ;
#41771 = CARTESIAN_POINT('Ctrl Pts',(-18.1608750310765,-12.7082182780589,
123.34842810391)) ;
#41772 = CARTESIAN_POINT('Ctrl Pts',(-18.1606947626094,-12.7083863898857,
123.352084201567)) ;
#41773 = CARTESIAN_POINT('Ctrl Pts',(-18.1603887097239,-12.7086994042937,
123.35889993839)) ;
#41774 = CARTESIAN_POINT('Ctrl Pts',(-18.1602588499147,-12.7088443489854,
123.362059363132)) ;
#41775 = CARTESIAN_POINT('Ctrl Pts',(-18.1600049796484,-12.7091562594369,
123.368865168655)) ;
#41776 = CARTESIAN_POINT('Ctrl Pts',(-18.1598849423355,-12.7093231816509,
123.372511670275)) ;
#41777 = CARTESIAN_POINT('Ctrl Pts',(-18.1596045888525,-12.709772398752,123.382336161789)) ;
#41778 = CARTESIAN_POINT('Ctrl Pts',(-18.159474120741,-12.7100543749281,123.38851491354)) ;
#41779 = CARTESIAN_POINT('Ctrl Pts',(-18.1590117737733,-12.7115921273386,
123.422269624332)) ;
#41780 = CARTESIAN_POINT('Ctrl Pts',(-18.1595467225219,-12.7128384326479,
123.449850025637)) ;
#41781 = CARTESIAN_POINT('Ctrl Pts',(-18.1611750874062,-12.7142357117041,
123.480846876769)) ;
#41782 = CARTESIAN_POINT('Ctrl Pts',(-18.1613710178504,-12.7143914426241,
123.484302500605)) ;
#41783 = CARTESIAN_POINT('Ctrl Pts',(-18.1617139215948,-12.7146452921126,
123.489936179065)) ;
#41784 = CARTESIAN_POINT('Ctrl Pts',(-18.1618522523349,-12.7147434473181,
123.492114738866)) ;
#41785 = CARTESIAN_POINT('Ctrl Pts',(-18.1644289779936,-12.7164990055125,
123.531081082994)) ;
#41786 = CARTESIAN_POINT('Ctrl Pts',(-18.1684880122812,-12.7181494619589,
123.567743186609)) ;
#41787 = CARTESIAN_POINT('Ctrl Pts',(-18.1769816217963,-12.7206445999397,
123.622279720628)) ;
#41788 = CARTESIAN_POINT('Ctrl Pts',(-18.1801994938702,-12.7214758827103,
123.640322592031)) ;
#41789 = CARTESIAN_POINT('Ctrl Pts',(-18.1862202536776,-12.7228648724916,
123.670257618892)) ;
#41790 = CARTESIAN_POINT('Ctrl Pts',(-18.1888028923239,-12.7234212188363,
123.682191224482)) ;
#41791 = CARTESIAN_POINT('Ctrl Pts',(-18.1937585235136,-12.7244227162455,
123.703569758564)) ;
#41792 = CARTESIAN_POINT('Ctrl Pts',(-18.196067855581,-12.724867531529,123.713028450735)) ;
#41793 = CARTESIAN_POINT('Ctrl Pts',(-18.2009245696807,-12.7257612735697,
123.731958223253)) ;
#41794 = CARTESIAN_POINT('Ctrl Pts',(-18.2034733879766,-12.7262101759464,
123.741428245317)) ;
#41795 = CARTESIAN_POINT('Ctrl Pts',(-18.208547693183,-12.7270672430795,123.759434561359)) ;
#41796 = CARTESIAN_POINT('Ctrl Pts',(-18.2110534508749,-12.7274753170839,
123.767975804784)) ;
#41797 = CARTESIAN_POINT('Ctrl Pts',(-18.2177465313335,-12.7285278005071,
123.78991970147)) ;
#41798 = CARTESIAN_POINT('Ctrl Pts',(-18.222068836222,-12.729172528345,123.803279863462)) ;
#41799 = CARTESIAN_POINT('Ctrl Pts',(-18.226624312154,-12.7298190838978,123.816590711209)) ;
#41800 = CARTESIAN_POINT('Ctrl Pts',(-18.2266333383706,-12.7298203648599,
123.816617082436)) ;
#41801 = CARTESIAN_POINT('Ctrl Pts',(-18.2266423654683,-12.7298216458232,
123.816643453356)) ;
#41802 = CARTESIAN_POINT('',(-20.5919009558702,-12.4898128815389,123.006981918687)) ;
#41803 = CARTESIAN_POINT('Ctrl Pts',(-18.2266423654705,-12.6697781342469,
123.816643453362)) ;
#41804 = CARTESIAN_POINT('Ctrl Pts',(-18.2222198725711,-12.6691526626378,
123.803723995805)) ;
#41805 = CARTESIAN_POINT('Ctrl Pts',(-18.2180093556767,-12.6685278300723,
123.790732860964)) ;
#41806 = CARTESIAN_POINT('Ctrl Pts',(-18.2086322522418,-12.6670628909818,
123.760098065799)) ;
#41807 = CARTESIAN_POINT('Ctrl Pts',(-18.2036403657761,-12.6662233326266,
123.742404295056)) ;
#41808 = CARTESIAN_POINT('Ctrl Pts',(-18.19298079256,-12.6642778060177,123.701161126861)) ;
#41809 = CARTESIAN_POINT('Ctrl Pts',(-18.1876036952942,-12.6631723117401,
123.677544292641)) ;
#41810 = CARTESIAN_POINT('Ctrl Pts',(-18.1816338847035,-12.6617606659644,
123.647288244401)) ;
#41811 = CARTESIAN_POINT('Ctrl Pts',(-18.1804034253215,-12.6614572806127,
123.640780116299)) ;
#41812 = CARTESIAN_POINT('Ctrl Pts',(-18.1792049658555,-12.6611485008418,
123.634153124928)) ;
#41813 = CARTESIAN_POINT('Ctrl Pts',(-18.1791851952805,-12.6611434031646,
123.634043718373)) ;
#41814 = CARTESIAN_POINT('Ctrl Pts',(-18.1791518820801,-12.6611348071483,
123.633859228886)) ;
#41815 = CARTESIAN_POINT('Ctrl Pts',(-18.1791383317286,-12.6611313088524,
123.633784147331)) ;
#41816 = CARTESIAN_POINT('Ctrl Pts',(-18.1791126313361,-12.6611246703369,
123.633641668613)) ;
#41817 = CARTESIAN_POINT('Ctrl Pts',(-18.1791004799697,-12.6611215301275,
123.633574271746)) ;
#41818 = CARTESIAN_POINT('Ctrl Pts',(-18.1790774318414,-12.6611155711528,
123.633446376416)) ;
#41819 = CARTESIAN_POINT('Ctrl Pts',(-18.1790665339962,-12.6611127523918,
123.633385878106)) ;
#41820 = CARTESIAN_POINT('Ctrl Pts',(-18.1790458624592,-12.6611074033964,
123.633271073575)) ;
#41821 = CARTESIAN_POINT('Ctrl Pts',(-18.1790360878958,-12.6611048731659,
123.633216767484)) ;
#41822 = CARTESIAN_POINT('Ctrl Pts',(-18.179017546121,-12.661100071661,123.633113712869)) ;
#41823 = CARTESIAN_POINT('Ctrl Pts',(-18.1790087782331,-12.6610978003963,
123.633064964592)) ;
#41824 = CARTESIAN_POINT('Ctrl Pts',(-18.1789928277888,-12.6610936671406,
123.632976252003)) ;
#41825 = CARTESIAN_POINT('Ctrl Pts',(-18.1789856442511,-12.661091805147,123.632936287691)) ;
#41826 = CARTESIAN_POINT('Ctrl Pts',(-18.1789714724399,-12.6610881307546,
123.632857423312)) ;
#41827 = CARTESIAN_POINT('Ctrl Pts',(-18.1789644840787,-12.6610863183602,
123.632818523347)) ;
#41828 = CARTESIAN_POINT('Ctrl Pts',(-18.1789506970924,-12.6610827418132,
123.632741758643)) ;
#41829 = CARTESIAN_POINT('Ctrl Pts',(-18.1789438983696,-12.661080977661,123.632703893917)) ;
#41830 = CARTESIAN_POINT('Ctrl Pts',(-18.1789304853164,-12.6610774962882,
123.632629171589)) ;
#41831 = CARTESIAN_POINT('Ctrl Pts',(-18.1789238708723,-12.6610757790624,
123.63259231388)) ;
#41832 = CARTESIAN_POINT('Ctrl Pts',(-18.1789108211518,-12.6610723902585,
123.63251957804)) ;
#41833 = CARTESIAN_POINT('Ctrl Pts',(-18.1789043858028,-12.6610707186845,
123.632483700004)) ;
#41834 = CARTESIAN_POINT('Ctrl Pts',(-18.1788916892156,-12.6610674199392,
123.632412896805)) ;
#41835 = CARTESIAN_POINT('Ctrl Pts',(-18.1788854278926,-12.6610657927677,
123.632377971642)) ;
#41836 = CARTESIAN_POINT('Ctrl Pts',(-18.1788730744341,-12.6610625816129,
123.632309048137)) ;
#41837 = CARTESIAN_POINT('Ctrl Pts',(-18.1788669822482,-12.6610609976372,
123.632275049961)) ;
#41838 = CARTESIAN_POINT('Ctrl Pts',(-18.1788549623318,-12.6610578717051,
123.632207955356)) ;
#41839 = CARTESIAN_POINT('Ctrl Pts',(-18.1788490344895,-12.6610563297393,
123.632174858727)) ;
#41840 = CARTESIAN_POINT('Ctrl Pts',(-18.1788373386141,-12.6610532866768,
123.632109542538)) ;
#41841 = CARTESIAN_POINT('Ctrl Pts',(-18.1788315705353,-12.6610517855868,
123.632077323125)) ;
#41842 = CARTESIAN_POINT('Ctrl Pts',(-18.178820189713,-12.6610488231668,123.632013737577)) ;
#41843 = CARTESIAN_POINT('Ctrl Pts',(-18.1788145768701,-12.6610473618286,
123.631982371267)) ;
#41844 = CARTESIAN_POINT('Ctrl Pts',(-18.1788035021421,-12.6610444778248,
123.631920468596)) ;
#41845 = CARTESIAN_POINT('Ctrl Pts',(-18.178798040216,-12.6610430551653,123.631889932366)) ;
#41846 = CARTESIAN_POINT('Ctrl Pts',(-18.1787872630764,-12.6610402474628,
123.631829667196)) ;
#41847 = CARTESIAN_POINT('Ctrl Pts',(-18.1787819478163,-12.6610388624234,
123.631799938338)) ;
#41848 = CARTESIAN_POINT('Ctrl Pts',(-18.1787714599335,-12.6610361289464,
123.631741266135)) ;
#41849 = CARTESIAN_POINT('Ctrl Pts',(-18.1787662872217,-12.6610347805005,
123.631712322618)) ;
#41850 = CARTESIAN_POINT('Ctrl Pts',(-18.1787560804207,-12.6610321192082,
123.631655199598)) ;
#41851 = CARTESIAN_POINT('Ctrl Pts',(-18.1787510463077,-12.6610308063697,
123.631627020268)) ;
#41852 = CARTESIAN_POINT('Ctrl Pts',(-18.1787411128303,-12.6610282153243,
123.631571404855)) ;
#41853 = CARTESIAN_POINT('Ctrl Pts',(-18.1787362134164,-12.6610269371179,
123.631543968784)) ;
#41854 = CARTESIAN_POINT('Ctrl Pts',(-18.1787265455952,-12.6610244144002,
123.631489819798)) ;
#41855 = CARTESIAN_POINT('Ctrl Pts',(-18.178721777131,-12.6610231698868,123.631463106839)) ;
#41856 = CARTESIAN_POINT('Ctrl Pts',(-18.1787123675407,-12.6610207136356,
123.631410384348)) ;
#41857 = CARTESIAN_POINT('Ctrl Pts',(-18.1787077263944,-12.6610195019045,
123.631384374963)) ;
#41858 = CARTESIAN_POINT('Ctrl Pts',(-18.1786985679346,-12.6610171103388,
123.631333040751)) ;
#41859 = CARTESIAN_POINT('Ctrl Pts',(-18.1786940505312,-12.6610159304921,
123.631307715668)) ;
#41860 = CARTESIAN_POINT('Ctrl Pts',(-18.1786851360851,-12.6610136018221,
123.631257731334)) ;
#41861 = CARTESIAN_POINT('Ctrl Pts',(-18.1786807390407,-12.6610124530092,
123.631233072307)) ;
#41862 = CARTESIAN_POINT('Ctrl Pts',(-18.1786720619454,-12.6610101855594,
123.631184401898)) ;
#41863 = CARTESIAN_POINT('Ctrl Pts',(-18.1786677818952,-12.6610090669329,
123.631160390743)) ;
#41864 = CARTESIAN_POINT('Ctrl Pts',(-18.1786593355864,-12.6610068590496,
123.631112998777)) ;
#41865 = CARTESIAN_POINT('Ctrl Pts',(-18.1786551692717,-12.6610057697879,
123.631089617863)) ;
#41866 = CARTESIAN_POINT('Ctrl Pts',(-18.1786474529009,-12.6610037520521,
123.631046307264)) ;
#41867 = CARTESIAN_POINT('Ctrl Pts',(-18.1786439026348,-12.6610028235718,
123.631026377457)) ;
#41868 = CARTESIAN_POINT('Ctrl Pts',(-18.1786368277849,-12.6610009730697,
123.630986656424)) ;
#41869 = CARTESIAN_POINT('Ctrl Pts',(-18.1786333031354,-12.6610000510325,
123.630966864868)) ;
#41870 = CARTESIAN_POINT('Ctrl Pts',(-18.1786262792059,-12.6609982133402,
123.630927418699)) ;
#41871 = CARTESIAN_POINT('Ctrl Pts',(-18.1786227800154,-12.6609972977102,
123.630907764626)) ;
#41872 = CARTESIAN_POINT('Ctrl Pts',(-18.1786158068435,-12.6609954727955,
123.630868592636)) ;
#41873 = CARTESIAN_POINT('Ctrl Pts',(-18.1786123327889,-12.6609945634934,
123.630849074345)) ;
#41874 = CARTESIAN_POINT('Ctrl Pts',(-18.1786054096866,-12.6609927511868,
123.630810172895)) ;
#41875 = CARTESIAN_POINT('Ctrl Pts',(-18.1786019606267,-12.6609918481809,
123.630790789704)) ;
#41876 = CARTESIAN_POINT('Ctrl Pts',(-18.1785950872891,-12.6609900484128,
123.630752157304)) ;
#41877 = CARTESIAN_POINT('Ctrl Pts',(-18.1785916629856,-12.6609891516457,
123.630732907986)) ;
#41878 = CARTESIAN_POINT('Ctrl Pts',(-18.1785848389233,-12.6609873642982,
123.630694542104)) ;
#41879 = CARTESIAN_POINT('Ctrl Pts',(-18.1785814391846,-12.6609864737247,
123.63067542569)) ;
#41880 = CARTESIAN_POINT('Ctrl Pts',(-18.1785746640443,-12.6609846987152,
123.630637324558)) ;
#41881 = CARTESIAN_POINT('Ctrl Pts',(-18.1785712886371,-12.6609838142793,
123.630618339843)) ;
#41882 = CARTESIAN_POINT('Ctrl Pts',(-18.1785645619599,-12.6609820514973,
123.630580501093)) ;
#41883 = CARTESIAN_POINT('Ctrl Pts',(-18.1785612106855,-12.6609811731517,
123.630561647066)) ;
#41884 = CARTESIAN_POINT('Ctrl Pts',(-18.1785545320595,-12.6609794224991,
123.63052406859)) ;
#41885 = CARTESIAN_POINT('Ctrl Pts',(-18.178551204716,-12.6609785501958,123.63050534422)) ;
#41886 = CARTESIAN_POINT('Ctrl Pts',(-18.1785445737538,-12.6609768115805,
123.630468024045)) ;
#41887 = CARTESIAN_POINT('Ctrl Pts',(-18.1785412701285,-12.6609759452684,
123.630449428237)) ;
#41888 = CARTESIAN_POINT('Ctrl Pts',(-18.178534686392,-12.660974218585,123.630412364102)) ;
#41889 = CARTESIAN_POINT('Ctrl Pts',(-18.178531406295,-12.660973358219,123.630393895889)) ;
#41890 = CARTESIAN_POINT('Ctrl Pts',(-18.1785248694447,-12.6609716433877,
123.630357086084)) ;
#41891 = CARTESIAN_POINT('Ctrl Pts',(-18.1785216126508,-12.6609707889133,
123.630338744297)) ;
#41892 = CARTESIAN_POINT('Ctrl Pts',(-18.1785151221673,-12.660969085807,123.630302186095)) ;
#41893 = CARTESIAN_POINT('Ctrl Pts',(-18.1785118885266,-12.6609682371894,
123.630283969988)) ;
#41894 = CARTESIAN_POINT('Ctrl Pts',(-18.1785054441989,-12.6609665457617,
123.630247662396)) ;
#41895 = CARTESIAN_POINT('Ctrl Pts',(-18.1785022334477,-12.6609657029363,
123.630229570582)) ;
#41896 = CARTESIAN_POINT('Ctrl Pts',(-18.1784958346946,-12.6609640230436,
123.630193510517)) ;
#41897 = CARTESIAN_POINT('Ctrl Pts',(-18.1784926467002,-12.6609631859798,
123.630175542342)) ;
#41898 = CARTESIAN_POINT('Ctrl Pts',(-18.1784862932401,-12.6609615175568,
123.630139728408)) ;
#41899 = CARTESIAN_POINT('Ctrl Pts',(-18.1784831277879,-12.6609606862027,
123.630121882756)) ;
#41900 = CARTESIAN_POINT('Ctrl Pts',(-18.1784768192196,-12.6609590291528,
123.630086312877)) ;
#41901 = CARTESIAN_POINT('Ctrl Pts',(-18.1784736761173,-12.6609582034621,
123.630068588759)) ;
#41902 = CARTESIAN_POINT('Ctrl Pts',(-18.1784674120955,-12.660956557703,123.630033261172)) ;
#41903 = CARTESIAN_POINT('Ctrl Pts',(-18.1784642911362,-12.6609557376256,
123.630015657511)) ;
#41904 = CARTESIAN_POINT('Ctrl Pts',(-18.1784580712099,-12.6609541030473,
123.629980569855)) ;
#41905 = CARTESIAN_POINT('Ctrl Pts',(-18.1784549722345,-12.6609532885455,
123.629963085843)) ;
#41906 = CARTESIAN_POINT('Ctrl Pts',(-18.1784487960732,-12.6609516650692,
123.629928236432)) ;
#41907 = CARTESIAN_POINT('Ctrl Pts',(-18.1784457188897,-12.6609508560967,
123.629910871075)) ;
#41908 = CARTESIAN_POINT('Ctrl Pts',(-18.1784395861508,-12.6609492436407,
123.629876258152)) ;
#41909 = CARTESIAN_POINT('Ctrl Pts',(-18.1784365305591,-12.6609484401489,
123.629859010409)) ;
#41910 = CARTESIAN_POINT('Ctrl Pts',(-18.1784304408045,-12.6609468386058,
123.629824631675)) ;
#41911 = CARTESIAN_POINT('Ctrl Pts',(-18.1784274066506,-12.6609460405582,
123.629807500762)) ;
#41912 = CARTESIAN_POINT('Ctrl Pts',(-18.1784213595656,-12.6609444498532,
123.629773354611)) ;
#41913 = CARTESIAN_POINT('Ctrl Pts',(-18.1784183466596,-12.6609436572038,
123.629756339541)) ;
#41914 = CARTESIAN_POINT('Ctrl Pts',(-18.178412341923,-12.6609420772603,123.629722424328)) ;
#41915 = CARTESIAN_POINT('Ctrl Pts',(-18.1784093500629,-12.6609412899597,
123.629705524045)) ;
#41916 = CARTESIAN_POINT('Ctrl Pts',(-18.178403387222,-12.6609397206661,123.629671837378)) ;
#41917 = CARTESIAN_POINT('Ctrl Pts',(-18.178400416268,-12.6609389386814,123.629655051174)) ;
#41918 = CARTESIAN_POINT('Ctrl Pts',(-18.1783944951202,-12.6609373799921,
123.629621592074)) ;
#41919 = CARTESIAN_POINT('Ctrl Pts',(-18.1783915448412,-12.6609366032662,
123.629604918724)) ;
#41920 = CARTESIAN_POINT('Ctrl Pts',(-18.1783856648063,-12.6609350550358,
123.629571684074)) ;
#41921 = CARTESIAN_POINT('Ctrl Pts',(-18.178382735116,-12.6609342835497,123.62955512317)) ;
#41922 = CARTESIAN_POINT('Ctrl Pts',(-18.1783768960917,-12.6609327457586,
123.629522112549)) ;
#41923 = CARTESIAN_POINT('Ctrl Pts',(-18.1783739867411,-12.6609319794504,
123.629505662764)) ;
#41924 = CARTESIAN_POINT('Ctrl Pts',(-18.1783681882437,-12.6609304519784,
123.629472873596)) ;
#41925 = CARTESIAN_POINT('Ctrl Pts',(-18.1783652990943,-12.6609296908152,
123.629456534224)) ;
#41926 = CARTESIAN_POINT('Ctrl Pts',(-18.1783595408339,-12.6609281735932,
123.629423965023)) ;
#41927 = CARTESIAN_POINT('Ctrl Pts',(-18.1783566717088,-12.6609274175319,
123.62940773514)) ;
#41928 = CARTESIAN_POINT('Ctrl Pts',(-18.1783509532808,-12.6609259104603,
123.629375383771)) ;
#41929 = CARTESIAN_POINT('Ctrl Pts',(-18.1783481040431,-12.6609251594683,
123.629359262678)) ;
#41930 = CARTESIAN_POINT('Ctrl Pts',(-18.1783424252856,-12.6609236625113,
123.629327128374)) ;
#41931 = CARTESIAN_POINT('Ctrl Pts',(-18.1783395957,-12.6609229165301,123.629311114814)) ;
#41932 = CARTESIAN_POINT('Ctrl Pts',(-18.1783339560997,-12.6609214295592,
123.629279194819)) ;
#41933 = CARTESIAN_POINT('Ctrl Pts',(-18.178331146059,-12.6609206885638,123.62926328826)) ;
#41934 = CARTESIAN_POINT('Ctrl Pts',(-18.1783255453141,-12.6609192115063,
123.629231581011)) ;
#41935 = CARTESIAN_POINT('Ctrl Pts',(-18.1783227546722,-12.6609184754616,
123.629215780698)) ;
#41936 = CARTESIAN_POINT('Ctrl Pts',(-18.1783171926251,-12.6609170082824,
123.629184285446)) ;
#41937 = CARTESIAN_POINT('Ctrl Pts',(-18.178314421147,-12.6609162771297,123.629168590119)) ;
#41938 = CARTESIAN_POINT('Ctrl Pts',(-18.1783088972574,-12.6609148196929,
123.629137303948)) ;
#41939 = CARTESIAN_POINT('Ctrl Pts',(-18.1783061448562,-12.6609140934126,
123.629121713186)) ;
#41940 = CARTESIAN_POINT('Ctrl Pts',(-18.1783006589467,-12.6609126456778,
123.62909063523)) ;
#41941 = CARTESIAN_POINT('Ctrl Pts',(-18.1782979254317,-12.6609119242227,
123.629075148021)) ;
#41942 = CARTESIAN_POINT('Ctrl Pts',(-18.1782924771045,-12.6609104860913,
123.629044276164)) ;
#41943 = CARTESIAN_POINT('Ctrl Pts',(-18.178289762344,-12.6609097694297,123.629028891831)) ;
#41944 = CARTESIAN_POINT('Ctrl Pts',(-18.1782843514437,-12.660908340867,123.628998225328)) ;
#41945 = CARTESIAN_POINT('Ctrl Pts',(-18.1782816552182,-12.6609076289442,
123.628982942694)) ;
#41946 = CARTESIAN_POINT('Ctrl Pts',(-18.1782762811695,-12.6609062098044,
123.628952478418)) ;
#41947 = CARTESIAN_POINT('Ctrl Pts',(-18.1782736034264,-12.6609055026096,
123.628937297252)) ;
#41948 = CARTESIAN_POINT('Ctrl Pts',(-18.1782682662141,-12.6609040928948,
123.628907035249)) ;
#41949 = CARTESIAN_POINT('Ctrl Pts',(-18.178265606707,-12.6609033903658,123.628891954219)) ;
#41950 = CARTESIAN_POINT('Ctrl Pts',(-18.1782603058577,-12.660901989957,123.628861891935)) ;
#41951 = CARTESIAN_POINT('Ctrl Pts',(-18.1782576644744,-12.6609012920673,
123.628846910469)) ;
#41952 = CARTESIAN_POINT('Ctrl Pts',(-18.178252399662,-12.6608999008842,123.628817046183)) ;
#41953 = CARTESIAN_POINT('Ctrl Pts',(-18.178249776286,-12.6608992076058,123.628802163684)) ;
#41954 = CARTESIAN_POINT('Ctrl Pts',(-18.1782445473528,-12.6608978256126,
123.628772496627)) ;
#41955 = CARTESIAN_POINT('Ctrl Pts',(-18.178241941783,-12.6608971368954,123.628757712017)) ;
#41956 = CARTESIAN_POINT('Ctrl Pts',(-18.1782367483339,-12.6608957639934,
123.628728240072)) ;
#41957 = CARTESIAN_POINT('Ctrl Pts',(-18.1782341604485,-12.660895079808,123.628713552721)) ;
#41958 = CARTESIAN_POINT('Ctrl Pts',(-18.1782290022397,-12.6608937159384,
123.628684274628)) ;
#41959 = CARTESIAN_POINT('Ctrl Pts',(-18.178226431882,-12.6608930362462,123.628669683709)) ;
#41960 = CARTESIAN_POINT('Ctrl Pts',(-18.1782213085765,-12.6608916813255,
123.628640597674)) ;
#41961 = CARTESIAN_POINT('Ctrl Pts',(-18.1782187556213,-12.6608910060961,
123.628626102536)) ;
#41962 = CARTESIAN_POINT('Ctrl Pts',(-18.17821366697,-12.660889660064,123.628597207265)) ;
#41963 = CARTESIAN_POINT('Ctrl Pts',(-18.1782111312665,-12.6608889892603,
123.628582807111)) ;
#41964 = CARTESIAN_POINT('Ctrl Pts',(-18.1782060769312,-12.6608876520327,
123.628554100802)) ;
#41965 = CARTESIAN_POINT('Ctrl Pts',(-18.1782035583615,-12.6608869856262,
123.62853979502)) ;
#41966 = CARTESIAN_POINT('Ctrl Pts',(-18.1781985381848,-12.6608856571668,
123.628511276895)) ;
#41967 = CARTESIAN_POINT('Ctrl Pts',(-18.1781960365599,-12.6608849951101,
123.628497064469)) ;
#41968 = CARTESIAN_POINT('Ctrl Pts',(-18.1781910501952,-12.6608836753326,
123.628468732673)) ;
#41969 = CARTESIAN_POINT('Ctrl Pts',(-18.1781885653864,-12.6608830175943,
123.628454612929)) ;
#41970 = CARTESIAN_POINT('Ctrl Pts',(-18.1781836124378,-12.660881706399,123.628426465325)) ;
#41971 = CARTESIAN_POINT('Ctrl Pts',(-18.1781811443734,-12.6608810529627,
123.628412437911)) ;
#41972 = CARTESIAN_POINT('Ctrl Pts',(-18.1781762247696,-12.6608797503358,
123.628384474206)) ;
#41973 = CARTESIAN_POINT('Ctrl Pts',(-18.178173773246,-12.6608791011502,123.628370538021)) ;
#41974 = CARTESIAN_POINT('Ctrl Pts',(-18.1781688866781,-12.660877807015,123.628342756566)) ;
#41975 = CARTESIAN_POINT('Ctrl Pts',(-18.1781664515469,-12.6608771620433,
123.628328910821)) ;
#41976 = CARTESIAN_POINT('Ctrl Pts',(-18.178161597596,-12.6608758762939,123.628301309345)) ;
#41977 = CARTESIAN_POINT('Ctrl Pts',(-18.1781591787926,-12.6608752355213,
123.628287553725)) ;
#41978 = CARTESIAN_POINT('Ctrl Pts',(-18.178154357366,-12.6608739581381,123.628260131806)) ;
#41979 = CARTESIAN_POINT('Ctrl Pts',(-18.1781519547067,-12.6608733215186,
123.62824646532)) ;
#41980 = CARTESIAN_POINT('Ctrl Pts',(-18.1781471654095,-12.6608720524017,
123.628219220818)) ;
#41981 = CARTESIAN_POINT('Ctrl Pts',(-18.1781447788043,-12.6608714199138,
123.628205643005)) ;
#41982 = CARTESIAN_POINT('Ctrl Pts',(-18.1781400214645,-12.6608701590224,
123.628178575045)) ;
#41983 = CARTESIAN_POINT('Ctrl Pts',(-18.1781376507604,-12.6608695306279,
123.628165085087)) ;
#41984 = CARTESIAN_POINT('Ctrl Pts',(-18.1781329251248,-12.6608682778998,
123.62813819233)) ;
#41985 = CARTESIAN_POINT('Ctrl Pts',(-18.1781305701799,-12.6608676535634,
123.62812478947)) ;
#41986 = CARTESIAN_POINT('Ctrl Pts',(-18.1781258759642,-12.6608664089277,
123.628098070399)) ;
#41987 = CARTESIAN_POINT('Ctrl Pts',(-18.1781235366593,-12.6608657886201,
123.628084754009)) ;
#41988 = CARTESIAN_POINT('Ctrl Pts',(-18.1781188735632,-12.6608645520018,
123.628058207013)) ;
#41989 = CARTESIAN_POINT('Ctrl Pts',(-18.1781165498001,-12.6608639356993,
123.628044976583)) ;
#41990 = CARTESIAN_POINT('Ctrl Pts',(-18.1781119176568,-12.6608627070587,
123.628018600811)) ;
#41991 = CARTESIAN_POINT('Ctrl Pts',(-18.178109609283,-12.6608620947231,123.628005455521)) ;
#41992 = CARTESIAN_POINT('Ctrl Pts',(-18.178105007843,-12.6608608739985,123.627979249649)) ;
#41993 = CARTESIAN_POINT('Ctrl Pts',(-18.1781027147224,-12.6608602655959,
123.627966188772)) ;
#41994 = CARTESIAN_POINT('Ctrl Pts',(-18.1780981436022,-12.6608590526899,
123.627940150711)) ;
#41995 = CARTESIAN_POINT('Ctrl Pts',(-18.1780958656748,-12.6608584482065,
123.627927173953)) ;
#41996 = CARTESIAN_POINT('Ctrl Pts',(-18.1780913248799,-12.660857243125,123.627901303827)) ;
#41997 = CARTESIAN_POINT('Ctrl Pts',(-18.1780890619314,-12.6608566425061,
123.627888410014)) ;
#41998 = CARTESIAN_POINT('Ctrl Pts',(-18.1780845509411,-12.6608554451151,
123.627862704951)) ;
#41999 = CARTESIAN_POINT('Ctrl Pts',(-18.178082302945,-12.6608548483559,123.627849893976)) ;
#42000 = CARTESIAN_POINT('Ctrl Pts',(-18.1780778217311,-12.6608536586521,
123.627824353905)) ;
#42001 = CARTESIAN_POINT('Ctrl Pts',(-18.1780755885098,-12.6608530657074,
123.627811624803)) ;
#42002 = CARTESIAN_POINT('Ctrl Pts',(-18.1780711367808,-12.6608518836177,
123.627786248154)) ;
#42003 = CARTESIAN_POINT('Ctrl Pts',(-18.1780689182151,-12.660851294458,123.62777360029)) ;
#42004 = CARTESIAN_POINT('Ctrl Pts',(-18.1780644956893,-12.6608501199116,
123.627748385544)) ;
#42005 = CARTESIAN_POINT('Ctrl Pts',(-18.1780622916852,-12.6608495345139,
123.627735818426)) ;
#42006 = CARTESIAN_POINT('Ctrl Pts',(-18.1780578980972,-12.6608483674444,
123.627710764159)) ;
#42007 = CARTESIAN_POINT('Ctrl Pts',(-18.178055708567,-12.6608477857875,123.62769827733)) ;
#42008 = CARTESIAN_POINT('Ctrl Pts',(-18.1780513438163,-12.6608466261721,
123.627673383054)) ;
#42009 = CARTESIAN_POINT('Ctrl Pts',(-18.1780491685949,-12.6608460482141,
123.627660975616)) ;
#42010 = CARTESIAN_POINT('Ctrl Pts',(-18.1780448323125,-12.6608448959588,
123.627636239312)) ;
#42011 = CARTESIAN_POINT('Ctrl Pts',(-18.178042671332,-12.6608443216836,123.62762391092)) ;
#42012 = CARTESIAN_POINT('Ctrl Pts',(-18.1770321734612,-12.660575760822,123.621858511994)) ;
#42013 = CARTESIAN_POINT('Ctrl Pts',(-18.1760641746186,-12.6603075266588,
123.61609846262)) ;
#42014 = CARTESIAN_POINT('Ctrl Pts',(-18.1729267270412,-12.6593992151072,
123.596593701384)) ;
#42015 = CARTESIAN_POINT('Ctrl Pts',(-18.1709464297291,-12.6587578392535,
123.582819672376)) ;
#42016 = CARTESIAN_POINT('Ctrl Pts',(-18.1654378014235,-12.6567363410127,
123.539365052685)) ;
#42017 = CARTESIAN_POINT('Ctrl Pts',(-18.1627437207223,-12.6553542485752,
123.509589316382)) ;
#42018 = CARTESIAN_POINT('Ctrl Pts',(-18.1600304775297,-12.6530499804726,
123.459736882306)) ;
#42019 = CARTESIAN_POINT('Ctrl Pts',(-18.1594227751612,-12.6521265907355,
123.439704698591)) ;
#42020 = CARTESIAN_POINT('Ctrl Pts',(-18.1592419010343,-12.6508028087505,
123.410911485108)) ;
#42021 = CARTESIAN_POINT('Ctrl Pts',(-18.1592788870681,-12.6504007243802,
123.402156113199)) ;
#42022 = CARTESIAN_POINT('Ctrl Pts',(-18.1594169997785,-12.6499705901163,
123.392780859932)) ;
#42023 = CARTESIAN_POINT('Ctrl Pts',(-18.1594266105133,-12.6499421022534,
123.39215989285)) ;
#42024 = CARTESIAN_POINT('Ctrl Pts',(-18.159457427645,-12.649854958374,123.390260236952)) ;
#42025 = CARTESIAN_POINT('Ctrl Pts',(-18.1594801335978,-12.6497963097356,
123.388981573)) ;
#42026 = CARTESIAN_POINT('Ctrl Pts',(-18.1595662437714,-12.649591616403,123.384518223812)) ;
#42027 = CARTESIAN_POINT('Ctrl Pts',(-18.1596398587758,-12.6494456224759,
123.381333745682)) ;
#42028 = CARTESIAN_POINT('Ctrl Pts',(-18.1597277541691,-12.6492961005507,
123.378071304311)) ;
#42029 = CARTESIAN_POINT('Ctrl Pts',(-18.1597298704669,-12.6492925129913,
123.37799302622)) ;
#42030 = CARTESIAN_POINT('Ctrl Pts',(-18.1597339708883,-12.6492855860819,
123.377841884647)) ;
#42031 = CARTESIAN_POINT('Ctrl Pts',(-18.1597359540301,-12.6492822467258,
123.377769021115)) ;
#42032 = CARTESIAN_POINT('Ctrl Pts',(-18.159739795121,-12.6492757996023,123.377628346238)) ;
#42033 = CARTESIAN_POINT('Ctrl Pts',(-18.1597416522171,-12.6492726918304,
123.377560534866)) ;
#42034 = CARTESIAN_POINT('Ctrl Pts',(-18.1599289759344,-12.648960145286,123.370740745807)) ;
#42035 = CARTESIAN_POINT('Ctrl Pts',(-18.1601691619896,-12.6486509823074,
123.363990370268)) ;
#42036 = CARTESIAN_POINT('Ctrl Pts',(-18.160973701865,-12.6478082050313,123.345579572654)) ;
#42037 = CARTESIAN_POINT('Ctrl Pts',(-18.1616467078773,-12.6472751536992,
123.333924563584)) ;
#42038 = CARTESIAN_POINT('Ctrl Pts',(-18.1635496623423,-12.6460635503773,
123.307425231623)) ;
#42039 = CARTESIAN_POINT('Ctrl Pts',(-18.1648818716474,-12.6453855231187,
123.292590016733)) ;
#42040 = CARTESIAN_POINT('Ctrl Pts',(-18.171704422704,-12.6424917283109,123.229328964051)) ;
#42041 = CARTESIAN_POINT('Ctrl Pts',(-18.1797590550159,-12.6402830294978,
123.181223074307)) ;
#42042 = CARTESIAN_POINT('Ctrl Pts',(-18.1973603972008,-12.6366730949746,
123.10409276087)) ;
#42043 = CARTESIAN_POINT('Ctrl Pts',(-18.2051966899157,-12.6352846790454,
123.074731348285)) ;
#42044 = CARTESIAN_POINT('Ctrl Pts',(-18.2251424619583,-12.6321693056675,
123.009621247692)) ;
#42045 = CARTESIAN_POINT('Ctrl Pts',(-18.2378167241948,-12.6304432995783,
122.974076317143)) ;
#42046 = CARTESIAN_POINT('Ctrl Pts',(-18.2592454496299,-12.6278460495146,
122.921612747141)) ;
#42047 = CARTESIAN_POINT('Ctrl Pts',(-18.2668103838277,-12.626977019358,122.904231712306)) ;
#42048 = CARTESIAN_POINT('Ctrl Pts',(-18.2749152773553,-12.626090811094,122.886710172793)) ;
#42049 = CARTESIAN_POINT('Ctrl Pts',(-18.2750631056821,-12.6260746616098,
122.886390944318)) ;
#42050 = CARTESIAN_POINT('Ctrl Pts',(-18.2753392722442,-12.6260445186976,
122.885795234971)) ;
#42051 = CARTESIAN_POINT('Ctrl Pts',(-18.2754675768948,-12.626030525351,122.885518738532)) ;
#42052 = CARTESIAN_POINT('Ctrl Pts',(-18.2757073049846,-12.6260043999089,
122.885002619174)) ;
#42053 = CARTESIAN_POINT('Ctrl Pts',(-18.2758187033151,-12.6259922678738,
122.884762984572)) ;
#42054 = CARTESIAN_POINT('Ctrl Pts',(-18.2760268735667,-12.625969611822,122.884315550214)) ;
#42055 = CARTESIAN_POINT('Ctrl Pts',(-18.2761236266551,-12.6259590878539,
122.884107741756)) ;
#42056 = CARTESIAN_POINT('Ctrl Pts',(-18.27630445493,-12.625939430258,122.88371963376)) ;
#42057 = CARTESIAN_POINT('Ctrl Pts',(-18.276388516012,-12.6259302966649,122.883539327646)) ;
#42058 = CARTESIAN_POINT('Ctrl Pts',(-18.2765456444916,-12.6259132325251,
122.88320250621)) ;
#42059 = CARTESIAN_POINT('Ctrl Pts',(-18.2766187013132,-12.6259053020029,
122.883045985911)) ;
#42060 = CARTESIAN_POINT('Ctrl Pts',(-18.2767552776296,-12.6258904826902,
122.8827535367)) ;
#42061 = CARTESIAN_POINT('Ctrl Pts',(-18.2768187891567,-12.6258835939199,
122.882617604078)) ;
#42062 = CARTESIAN_POINT('Ctrl Pts',(-18.2770372670083,-12.6258599056609,
122.882150219157)) ;
#42063 = CARTESIAN_POINT('Ctrl Pts',(-18.2771923543361,-12.6258431058732,
122.881818823575)) ;
#42064 = CARTESIAN_POINT('Ctrl Pts',(-18.2774970413321,-12.6258101309488,
122.881168502537)) ;
#42065 = CARTESIAN_POINT('Ctrl Pts',(-18.2776466303692,-12.6257939558394,
122.880849572104)) ;
#42066 = CARTESIAN_POINT('Ctrl Pts',(-18.2779405767708,-12.6257621992555,
122.880223553862)) ;
#42067 = CARTESIAN_POINT('Ctrl Pts',(-18.2780849243952,-12.6257466178078,
122.879916461522)) ;
#42068 = CARTESIAN_POINT('Ctrl Pts',(-18.2783686310298,-12.6257160192645,
122.879313527701)) ;
#42069 = CARTESIAN_POINT('Ctrl Pts',(-18.2785079811195,-12.6257010021941,
122.879017682069)) ;
#42070 = CARTESIAN_POINT('Ctrl Pts',(-18.2787819233553,-12.6256715047635,
122.878436683655)) ;
#42071 = CARTESIAN_POINT('Ctrl Pts',(-18.2789165073475,-12.6256570244245,
122.878151527019)) ;
#42072 = CARTESIAN_POINT('Ctrl Pts',(-18.2791811363385,-12.6256285743533,
122.877591380183)) ;
#42073 = CARTESIAN_POINT('Ctrl Pts',(-18.2793111738436,-12.6256146046422,
122.877316386472)) ;
#42074 = CARTESIAN_POINT('Ctrl Pts',(-18.2795669175777,-12.625587151181,122.876776068955)) ;
#42075 = CARTESIAN_POINT('Ctrl Pts',(-18.2796926169244,-12.6255736674509,
122.876510741928)) ;
#42076 = CARTESIAN_POINT('Ctrl Pts',(-18.2799398813877,-12.6255471626783,
122.875989289337)) ;
#42077 = CARTESIAN_POINT('Ctrl Pts',(-18.2800614401804,-12.6255341416544,
122.875733160809)) ;
#42078 = CARTESIAN_POINT('Ctrl Pts',(-18.2803006103763,-12.6255085403208,
122.875229663333)) ;
#42079 = CARTESIAN_POINT('Ctrl Pts',(-18.2804182159959,-12.6254959600249,
122.874982291586)) ;
#42080 = CARTESIAN_POINT('Ctrl Pts',(-18.2806496571411,-12.6254712193825,
122.874495890458)) ;
#42081 = CARTESIAN_POINT('Ctrl Pts',(-18.2807634873175,-12.6254590590515,
122.87425685855)) ;
#42082 = CARTESIAN_POINT('Ctrl Pts',(-18.2809875457193,-12.6254351387228,
122.873786743287)) ;
#42083 = CARTESIAN_POINT('Ctrl Pts',(-18.2810977690084,-12.6254233787403,
122.873555657615)) ;
#42084 = CARTESIAN_POINT('Ctrl Pts',(-18.287541854932,-12.6247362749384,122.860056157743)) ;
#42085 = CARTESIAN_POINT('Ctrl Pts',(-18.2941092361412,-12.6240603376009,
122.84690052324)) ;
#42086 = CARTESIAN_POINT('Ctrl Pts',(-18.307827305343,-12.6226942650302,122.820592684519)) ;
#42087 = CARTESIAN_POINT('Ctrl Pts',(-18.3149852471551,-12.6220042033772,
122.807446932521)) ;
#42088 = CARTESIAN_POINT('Ctrl Pts',(-18.3326564680827,-12.6203511428849,
122.776336898223)) ;
#42089 = CARTESIAN_POINT('Ctrl Pts',(-18.3433856903454,-12.6193862658968,
122.758500518981)) ;
#42090 = CARTESIAN_POINT('Ctrl Pts',(-18.3737759357875,-12.6167585607486,
122.710722371413)) ;
#42091 = CARTESIAN_POINT('Ctrl Pts',(-18.3942867137277,-12.6150971782096,
122.681343962543)) ;
#42092 = CARTESIAN_POINT('Ctrl Pts',(-18.4210320278047,-12.6130671201886,
122.646341214415)) ;
#42093 = CARTESIAN_POINT('Ctrl Pts',(-18.4260979258935,-12.612688079985,122.639845369389)) ;
#42094 = CARTESIAN_POINT('Ctrl Pts',(-18.4342773663973,-12.6120846646705,
122.629568249464)) ;
#42095 = CARTESIAN_POINT('Ctrl Pts',(-18.4373495517714,-12.6118599016483,
122.625754394585)) ;
#42096 = CARTESIAN_POINT('Ctrl Pts',(-18.4428707377722,-12.611459276532,122.618982169492)) ;
#42097 = CARTESIAN_POINT('Ctrl Pts',(-18.4453111066451,-12.6112833318287,
122.616016848548)) ;
#42098 = CARTESIAN_POINT('Ctrl Pts',(-18.4511895629447,-12.610862188603,122.608940583543)) ;
#42099 = CARTESIAN_POINT('Ctrl Pts',(-18.4546405013989,-12.6106171233224,
122.604840406996)) ;
#42100 = CARTESIAN_POINT('Ctrl Pts',(-18.4619338508133,-12.610103649682,122.596287189935)) ;
#42101 = CARTESIAN_POINT('Ctrl Pts',(-18.4657815404245,-12.6098353009703,
122.591838818415)) ;
#42102 = CARTESIAN_POINT('Ctrl Pts',(-18.4760797110779,-12.6091236568087,
122.580101407085)) ;
#42103 = CARTESIAN_POINT('Ctrl Pts',(-18.4825841873557,-12.6086809075479,
122.572860257337)) ;
#42104 = CARTESIAN_POINT('Ctrl Pts',(-18.5038720921853,-12.6072525757861,
122.54971102731)) ;
#42105 = CARTESIAN_POINT('Ctrl Pts',(-18.5189856960247,-12.6062701096431,
122.534111983459)) ;
#42106 = CARTESIAN_POINT('Ctrl Pts',(-18.5552211526755,-12.6039773765129,
122.498612098717)) ;
#42107 = CARTESIAN_POINT('Ctrl Pts',(-18.5766446136048,-12.6026687430557,
122.479037407174)) ;
#42108 = CARTESIAN_POINT('Ctrl Pts',(-18.606038714761,-12.6009154462183,122.454000138348)) ;
#42109 = CARTESIAN_POINT('Ctrl Pts',(-18.613419321866,-12.6004784952232,122.44785880551)) ;
#42110 = CARTESIAN_POINT('Ctrl Pts',(-18.6244298596054,-12.5998307587984,
122.438909700844)) ;
#42111 = CARTESIAN_POINT('Ctrl Pts',(-18.6280056131143,-12.5996210589038,
122.436035955186)) ;
#42112 = CARTESIAN_POINT('Ctrl Pts',(-18.6344379685612,-12.5992450517586,
122.4309244517)) ;
#42113 = CARTESIAN_POINT('Ctrl Pts',(-18.6372886534297,-12.5990788369211,
122.428679322317)) ;
#42114 = CARTESIAN_POINT('Ctrl Pts',(-18.6432681697942,-12.5987310973486,
122.424012044864)) ;
#42115 = CARTESIAN_POINT('Ctrl Pts',(-18.6463988080334,-12.5985495493898,
122.42159227582)) ;
#42116 = CARTESIAN_POINT('Ctrl Pts',(-18.6495510876864,-12.5983672760887,
122.419179601347)) ;
#42117 = CARTESIAN_POINT('Ctrl Pts',(-18.649561298306,-12.5983666856887,122.419171786649)) ;
#42118 = CARTESIAN_POINT('Ctrl Pts',(-18.6495817299632,-12.5983655042975,
122.41915614978)) ;
#42119 = CARTESIAN_POINT('Ctrl Pts',(-18.6495919552914,-12.5983649130582,
122.419148324325)) ;
#42120 = CARTESIAN_POINT('Ctrl Pts',(-18.6496124246755,-12.5983637295078,
122.419132659585)) ;
#42121 = CARTESIAN_POINT('Ctrl Pts',(-18.6496226676214,-12.598363137261,122.41912482115)) ;
#42122 = CARTESIAN_POINT('Ctrl Pts',(-18.6496431684722,-12.5983619519136,
122.419109133335)) ;
#42123 = CARTESIAN_POINT('Ctrl Pts',(-18.6496534279312,-12.5983613587232,
122.419101282767)) ;
#42124 = CARTESIAN_POINT('Ctrl Pts',(-18.649673963113,-12.5983601714132,122.419085569691)) ;
#42125 = CARTESIAN_POINT('Ctrl Pts',(-18.6496842391464,-12.5983595772757,
122.419077706946)) ;
#42126 = CARTESIAN_POINT('Ctrl Pts',(-18.649704810932,-12.5983583878719,122.419061966874)) ;
#42127 = CARTESIAN_POINT('Ctrl Pts',(-18.6497151053305,-12.5983577926839,
122.419054090584)) ;
#42128 = CARTESIAN_POINT('Ctrl Pts',(-18.6497357091842,-12.5983566014486,
122.419038326992)) ;
#42129 = CARTESIAN_POINT('Ctrl Pts',(-18.6497460203609,-12.5983560053018,
122.419030438374)) ;
#42130 = CARTESIAN_POINT('Ctrl Pts',(-18.6497666613134,-12.5983548119443,
122.419014647418)) ;
#42131 = CARTESIAN_POINT('Ctrl Pts',(-18.6497769905191,-12.5983542147666,
122.419006745518)) ;
#42132 = CARTESIAN_POINT('Ctrl Pts',(-18.6497976667056,-12.5983530193947,
122.41899092863)) ;
#42133 = CARTESIAN_POINT('Ctrl Pts',(-18.6498080139681,-12.5983524211844,
122.418983013428)) ;
#42134 = CARTESIAN_POINT('Ctrl Pts',(-18.6498287254617,-12.5983512237942,
122.418967170558)) ;
#42135 = CARTESIAN_POINT('Ctrl Pts',(-18.6498390902779,-12.5983506245805,
122.418959242442)) ;
#42136 = CARTESIAN_POINT('Ctrl Pts',(-18.6498598401011,-12.5983494249973,
122.418943371282)) ;
#42137 = CARTESIAN_POINT('Ctrl Pts',(-18.6498702238716,-12.5983488246992,
122.418935429184)) ;
#42138 = CARTESIAN_POINT('Ctrl Pts',(-18.6498910091217,-12.5983476230909,
122.41891953196)) ;
#42139 = CARTESIAN_POINT('Ctrl Pts',(-18.6499014111075,-12.5983470217514,
122.418911576448)) ;
#42140 = CARTESIAN_POINT('Ctrl Pts',(-18.6499222350237,-12.5983458179308,
122.418895650689)) ;
#42141 = CARTESIAN_POINT('Ctrl Pts',(-18.6499326563795,-12.598345215483,122.418887680882)) ;
#42142 = CARTESIAN_POINT('Ctrl Pts',(-18.6499535161522,-12.5983440096128,
122.418871728741)) ;
#42143 = CARTESIAN_POINT('Ctrl Pts',(-18.6499639557221,-12.5983434061237,
122.418863745526)) ;
#42144 = CARTESIAN_POINT('Ctrl Pts',(-18.6499848560941,-12.5983421979297,
122.418847763382)) ;
#42145 = CARTESIAN_POINT('Ctrl Pts',(-18.6499953156951,-12.5983415932943,
122.418839765372)) ;
#42146 = CARTESIAN_POINT('Ctrl Pts',(-18.6500162525731,-12.5983403830134,
122.418823756361)) ;
#42147 = CARTESIAN_POINT('Ctrl Pts',(-18.6500267310911,-12.5983397772962,
122.418815744412)) ;
#42148 = CARTESIAN_POINT('Ctrl Pts',(-18.6500477077048,-12.5983385647417,
122.41879970607)) ;
#42149 = CARTESIAN_POINT('Ctrl Pts',(-18.650058205517,-12.5983379579209,122.418791679895)) ;
#42150 = CARTESIAN_POINT('Ctrl Pts',(-18.6500792232105,-12.5983367430153,
122.418775611201)) ;
#42151 = CARTESIAN_POINT('Ctrl Pts',(-18.6500897417746,-12.5983361350067,
122.418767569689)) ;
#42152 = CARTESIAN_POINT('Ctrl Pts',(-18.6501107971926,-12.5983349179441,
122.418751473213)) ;
#42153 = CARTESIAN_POINT('Ctrl Pts',(-18.6501213353978,-12.598334308812,122.418743417217)) ;
#42154 = CARTESIAN_POINT('Ctrl Pts',(-18.6501424318548,-12.598333089401,122.418727290432)) ;
#42155 = CARTESIAN_POINT('Ctrl Pts',(-18.6501529901725,-12.5983324791182,
122.418719219593)) ;
#42156 = CARTESIAN_POINT('Ctrl Pts',(-18.6501741276519,-12.5983312573597,
122.418703062517)) ;
#42157 = CARTESIAN_POINT('Ctrl Pts',(-18.650184706356,-12.5983306459105,122.41869497663)) ;
#42158 = CARTESIAN_POINT('Ctrl Pts',(-18.6502058856374,-12.5983294217598,
122.418678788674)) ;
#42159 = CARTESIAN_POINT('Ctrl Pts',(-18.6502164853907,-12.5983288091059,
122.418670687235)) ;
#42160 = CARTESIAN_POINT('Ctrl Pts',(-18.6502377059149,-12.5983275825953,
122.418654468832)) ;
#42161 = CARTESIAN_POINT('Ctrl Pts',(-18.6502483268186,-12.598326968731,122.418646351767)) ;
#42162 = CARTESIAN_POINT('Ctrl Pts',(-18.6502695889701,-12.5983257398385,
122.418630102629)) ;
#42163 = CARTESIAN_POINT('Ctrl Pts',(-18.6502802309545,-12.5983251247678,
122.418621969995)) ;
#42164 = CARTESIAN_POINT('Ctrl Pts',(-18.6503015350622,-12.5983238934745,
122.418605689878)) ;
#42165 = CARTESIAN_POINT('Ctrl Pts',(-18.650312197665,-12.5983232772243,122.41859754203)) ;
#42166 = CARTESIAN_POINT('Ctrl Pts',(-18.6503335468897,-12.5983220433477,
122.418581228525)) ;
#42167 = CARTESIAN_POINT('Ctrl Pts',(-18.6503442316723,-12.5983214258277,
122.418573064274)) ;
#42168 = CARTESIAN_POINT('Ctrl Pts',(-18.6503656234731,-12.5983201895148,
122.418556719329)) ;
#42169 = CARTESIAN_POINT('Ctrl Pts',(-18.6503763303433,-12.5983195707305,
122.418548538749)) ;
#42170 = CARTESIAN_POINT('Ctrl Pts',(-18.6503977654965,-12.5983183319365,
122.418532161777)) ;
#42171 = CARTESIAN_POINT('Ctrl Pts',(-18.6504084943738,-12.5983177118926,
122.418523964932)) ;
#42172 = CARTESIAN_POINT('Ctrl Pts',(-18.6504299741154,-12.5983164705463,
122.418507554996)) ;
#42173 = CARTESIAN_POINT('Ctrl Pts',(-18.6504407253918,-12.5983158492202,
122.418499341591)) ;
#42174 = CARTESIAN_POINT('Ctrl Pts',(-18.6504622492835,-12.5983146053472,
122.418482899032)) ;
#42175 = CARTESIAN_POINT('Ctrl Pts',(-18.6504730226356,-12.5983139827576,
122.418474669317)) ;
#42176 = CARTESIAN_POINT('Ctrl Pts',(-18.6504945928455,-12.5983127362326,
122.418458192486)) ;
#42177 = CARTESIAN_POINT('Ctrl Pts',(-18.6505053891011,-12.5983121123319,
122.418449945831)) ;
#42178 = CARTESIAN_POINT('Ctrl Pts',(-18.6505270049518,-12.5983108631942,
122.418433435253)) ;
#42179 = CARTESIAN_POINT('Ctrl Pts',(-18.6505378244112,-12.598310237965,122.418425171433)) ;
#42180 = CARTESIAN_POINT('Ctrl Pts',(-18.6505594853712,-12.5983089862455,
122.41840862752)) ;
#42181 = CARTESIAN_POINT('Ctrl Pts',(-18.6505703273927,-12.5983083597251,
122.418400347029)) ;
#42182 = CARTESIAN_POINT('Ctrl Pts',(-18.6505920369108,-12.5983071052247,
122.418383767155)) ;
#42183 = CARTESIAN_POINT('Ctrl Pts',(-18.6506029029903,-12.5983064773266,
122.418375468854)) ;
#42184 = CARTESIAN_POINT('Ctrl Pts',(-18.6506246587612,-12.5983052201786,
122.418358854785)) ;
#42185 = CARTESIAN_POINT('Ctrl Pts',(-18.6506355488577,-12.5983045909054,
122.418350538709)) ;
#42186 = CARTESIAN_POINT('Ctrl Pts',(-18.650657350895,-12.5983033311092,122.418333890444)) ;
#42187 = CARTESIAN_POINT('Ctrl Pts',(-18.6506682642414,-12.5983027005051,
122.418325557182)) ;
#42188 = CARTESIAN_POINT('Ctrl Pts',(-18.6506901160332,-12.5983014378594,
122.418308872064)) ;
#42189 = CARTESIAN_POINT('Ctrl Pts',(-18.6507010539031,-12.5983008058511,
122.418300520648)) ;
#42190 = CARTESIAN_POINT('Ctrl Pts',(-18.6507229529526,-12.5982995405003,
122.41828380059)) ;
#42191 = CARTESIAN_POINT('Ctrl Pts',(-18.6507339146566,-12.5982989071275,
122.418275431549)) ;
#42192 = CARTESIAN_POINT('Ctrl Pts',(-18.6507558643608,-12.5982976388755,
122.418258673967)) ;
#42193 = CARTESIAN_POINT('Ctrl Pts',(-18.650766851228,-12.5982970040617,122.418250286291)) ;
#42194 = CARTESIAN_POINT('Ctrl Pts',(-18.6507888495272,-12.5982957330276,
122.418233492763)) ;
#42195 = CARTESIAN_POINT('Ctrl Pts',(-18.6507998614117,-12.5982950967812,
122.418225086567)) ;
#42196 = CARTESIAN_POINT('Ctrl Pts',(-18.6508219084853,-12.5982938229549,
122.418208256965)) ;
#42197 = CARTESIAN_POINT('Ctrl Pts',(-18.6508329445605,-12.5982931853238,
122.418199832884)) ;
#42198 = CARTESIAN_POINT('Ctrl Pts',(-18.6508550450937,-12.5982919084347,
122.41818296364)) ;
#42199 = CARTESIAN_POINT('Ctrl Pts',(-18.6508661076924,-12.5982912692842,
122.418174519897)) ;
#42200 = CARTESIAN_POINT('Ctrl Pts',(-18.6508882565901,-12.5982899896269,
122.418157614906)) ;
#42201 = CARTESIAN_POINT('Ctrl Pts',(-18.6508993445044,-12.5982893490269,
122.418149152427)) ;
#42202 = CARTESIAN_POINT('Ctrl Pts',(-18.6509215447641,-12.5982880664284,
122.418132209411)) ;
#42203 = CARTESIAN_POINT('Ctrl Pts',(-18.6509326578662,-12.5982874243863,
122.418123728298)) ;
#42204 = CARTESIAN_POINT('Ctrl Pts',(-18.6509549114128,-12.5982861387356,
122.418106745795)) ;
#42205 = CARTESIAN_POINT('Ctrl Pts',(-18.6509660506469,-12.598285495197,122.418098245331)) ;
#42206 = CARTESIAN_POINT('Ctrl Pts',(-18.6509883572059,-12.5982842065101,
122.41808122356)) ;
#42207 = CARTESIAN_POINT('Ctrl Pts',(-18.650999523427,-12.5982835614257,122.418072703097)) ;
#42208 = CARTESIAN_POINT('Ctrl Pts',(-18.6510218813851,-12.598282269796,122.418055643296)) ;
#42209 = CARTESIAN_POINT('Ctrl Pts',(-18.6510330739266,-12.5982816232044,
122.418047103347)) ;
#42210 = CARTESIAN_POINT('Ctrl Pts',(-18.6510554860335,-12.5982803284733,
122.418030003427)) ;
#42211 = CARTESIAN_POINT('Ctrl Pts',(-18.6510667055843,-12.5982796803347,
122.41802144347)) ;
#42212 = CARTESIAN_POINT('Ctrl Pts',(-18.6510891711257,-12.5982783825436,
122.418004303985)) ;
#42213 = CARTESIAN_POINT('Ctrl Pts',(-18.6511004175758,-12.5982777328646,
122.417995724108)) ;
#42214 = CARTESIAN_POINT('Ctrl Pts',(-18.6511229378347,-12.5982764319395,
122.417978544087)) ;
#42215 = CARTESIAN_POINT('Ctrl Pts',(-18.6511342115148,-12.5982757807011,
122.417969944043)) ;
#42216 = CARTESIAN_POINT('Ctrl Pts',(-18.6511567874916,-12.5982744765845,
122.417952722732)) ;
#42217 = CARTESIAN_POINT('Ctrl Pts',(-18.6511680892582,-12.5982738237372,
122.417944101871)) ;
#42218 = CARTESIAN_POINT('Ctrl Pts',(-18.6511907192162,-12.5982725165297,
122.417926840603)) ;
#42219 = CARTESIAN_POINT('Ctrl Pts',(-18.6512020482939,-12.5982718621184,
122.417918199522)) ;
#42220 = CARTESIAN_POINT('Ctrl Pts',(-18.6512247359857,-12.5982705516034,
122.417900895445)) ;
#42221 = CARTESIAN_POINT('Ctrl Pts',(-18.651236093824,-12.5982698955445,122.417892233042)) ;
#42222 = CARTESIAN_POINT('Ctrl Pts',(-18.6512588361687,-12.5982685819001,
122.417874888513)) ;
#42223 = CARTESIAN_POINT('Ctrl Pts',(-18.6512702217627,-12.5982679242518,
122.41786620556)) ;
#42224 = CARTESIAN_POINT('Ctrl Pts',(-18.6512930227638,-12.5982666072469,
122.417848817536)) ;
#42225 = CARTESIAN_POINT('Ctrl Pts',(-18.6513044373569,-12.5982659479374,
122.417840113088)) ;
#42226 = CARTESIAN_POINT('Ctrl Pts',(-18.6513272951699,-12.5982646276789,
122.417822682985)) ;
#42227 = CARTESIAN_POINT('Ctrl Pts',(-18.6513387386052,-12.5982639667175,
122.417813957168)) ;
#42228 = CARTESIAN_POINT('Ctrl Pts',(-18.6513616545633,-12.5982626431285,
122.417796483978)) ;
#42229 = CARTESIAN_POINT('Ctrl Pts',(-18.6513731270605,-12.5982619805025,
122.417787736627)) ;
#42230 = CARTESIAN_POINT('Ctrl Pts',(-18.65139610204,-12.5982606535327,122.417770219693)) ;
#42231 = CARTESIAN_POINT('Ctrl Pts',(-18.6514076041197,-12.5982599892121,
122.417761450417)) ;
#42232 = CARTESIAN_POINT('Ctrl Pts',(-18.6514306381346,-12.5982586588609,
122.417743889736)) ;
#42233 = CARTESIAN_POINT('Ctrl Pts',(-18.6514421700625,-12.5982579928306,
122.417735098338)) ;
#42234 = CARTESIAN_POINT('Ctrl Pts',(-18.6514652635442,-12.5982566590731,
122.417717493591)) ;
#42235 = CARTESIAN_POINT('Ctrl Pts',(-18.6514768254377,-12.5982559913264,
122.417708679985)) ;
#42236 = CARTESIAN_POINT('Ctrl Pts',(-18.6514999788699,-12.5982546541351,
122.417691030814)) ;
#42237 = CARTESIAN_POINT('Ctrl Pts',(-18.6515115706694,-12.5982539846755,
122.417682195051)) ;
#42238 = CARTESIAN_POINT('Ctrl Pts',(-18.6515347860698,-12.598252643934,122.417664499928)) ;
#42239 = CARTESIAN_POINT('Ctrl Pts',(-18.6515464088379,-12.5982519727003,
122.417655641203)) ;
#42240 = CARTESIAN_POINT('Ctrl Pts',(-18.651569684921,-12.5982506284831,122.417637901117)) ;
#42241 = CARTESIAN_POINT('Ctrl Pts',(-18.6515813386761,-12.5982499554743,
122.417629019421)) ;
#42242 = CARTESIAN_POINT('Ctrl Pts',(-18.6516046756774,-12.5982486077681,
122.417611234203)) ;
#42243 = CARTESIAN_POINT('Ctrl Pts',(-18.6516163598529,-12.598247933017,122.417602329973)) ;
#42244 = CARTESIAN_POINT('Ctrl Pts',(-18.6516397613945,-12.5982465816127,
122.417584496873)) ;
#42245 = CARTESIAN_POINT('Ctrl Pts',(-18.6516514776689,-12.5982459050226,
122.417575568835)) ;
#42246 = CARTESIAN_POINT('Ctrl Pts',(-18.6516749400284,-12.5982445501355,
122.4175576907)) ;
#42247 = CARTESIAN_POINT('Ctrl Pts',(-18.6516866871725,-12.5982438717775,
122.417548739796)) ;
#42248 = CARTESIAN_POINT('Ctrl Pts',(-18.6517102155907,-12.5982425131052,
122.417530812642)) ;
#42249 = CARTESIAN_POINT('Ctrl Pts',(-18.651721995559,-12.5982418328664,122.417521837389)) ;
#42250 = CARTESIAN_POINT('Ctrl Pts',(-18.6517455858715,-12.5982404706496,
122.417503864401)) ;
#42251 = CARTESIAN_POINT('Ctrl Pts',(-18.6517573975375,-12.5982397885953,
122.417494865661)) ;
#42252 = CARTESIAN_POINT('Ctrl Pts',(-18.6517810536065,-12.5982384226112,
122.417476843907)) ;
#42253 = CARTESIAN_POINT('Ctrl Pts',(-18.6517928977279,-12.5982377386978,
122.417467821109)) ;
#42254 = CARTESIAN_POINT('Ctrl Pts',(-18.6518166193069,-12.5982363689609,
122.417449750787)) ;
#42255 = CARTESIAN_POINT('Ctrl Pts',(-18.6518284963018,-12.5982356831643,
122.417440703618)) ;
#42256 = CARTESIAN_POINT('Ctrl Pts',(-18.6518522838537,-12.5982343096481,
122.417422584387)) ;
#42257 = CARTESIAN_POINT('Ctrl Pts',(-18.6518641941415,-12.5982336219442,
122.417413512533)) ;
#42258 = CARTESIAN_POINT('Ctrl Pts',(-18.6518880474834,-12.5982322446596,
122.417395344543)) ;
#42259 = CARTESIAN_POINT('Ctrl Pts',(-18.651899990836,-12.5982315550617,122.417386248183)) ;
#42260 = CARTESIAN_POINT('Ctrl Pts',(-18.6519239126945,-12.5982301738515,
122.41736802937)) ;
#42261 = CARTESIAN_POINT('Ctrl Pts',(-18.6519358905298,-12.5982294822779,
122.417358907429)) ;
#42262 = CARTESIAN_POINT('Ctrl Pts',(-18.6519598771807,-12.5982280973573,
122.41734064064)) ;
#42263 = CARTESIAN_POINT('Ctrl Pts',(-18.6519718876903,-12.5982274039125,
122.417331494502)) ;
#42264 = CARTESIAN_POINT('Ctrl Pts',(-18.6519959460754,-12.598226014881,122.417313174461)) ;
#42265 = CARTESIAN_POINT('Ctrl Pts',(-18.6520079917256,-12.5982253194228,
122.417304002255)) ;
#42266 = CARTESIAN_POINT('Ctrl Pts',(-18.6520321171906,-12.5982239265495,
122.417285632518)) ;
#42267 = CARTESIAN_POINT('Ctrl Pts',(-18.6520441973327,-12.5982232291154,
122.417276434742)) ;
#42268 = CARTESIAN_POINT('Ctrl Pts',(-18.6520683923358,-12.5982218322585,
122.417258013451)) ;
#42269 = CARTESIAN_POINT('Ctrl Pts',(-18.6520805072433,-12.5982211328329,
122.417248789902)) ;
#42270 = CARTESIAN_POINT('Ctrl Pts',(-18.6521047732719,-12.5982197319068,
122.417230315935)) ;
#42271 = CARTESIAN_POINT('Ctrl Pts',(-18.6521169240576,-12.5982190304257,
122.417221065774)) ;
#42272 = CARTESIAN_POINT('Ctrl Pts',(-18.6521412587488,-12.5982176255671,
122.417202540942)) ;
#42273 = CARTESIAN_POINT('Ctrl Pts',(-18.6521534443566,-12.5982169220914,
122.417193264978)) ;
#42274 = CARTESIAN_POINT('Ctrl Pts',(-18.652177851847,-12.5982155130618,122.417174686144)) ;
#42275 = CARTESIAN_POINT('Ctrl Pts',(-18.6521900733948,-12.5982148075273,
122.417165383532)) ;
#42276 = CARTESIAN_POINT('Ctrl Pts',(-18.6522145527332,-12.5982133943819,
122.417146751433)) ;
#42277 = CARTESIAN_POINT('Ctrl Pts',(-18.6522268105489,-12.5982126867697,
122.41713742193)) ;
#42278 = CARTESIAN_POINT('Ctrl Pts',(-18.6522513615862,-12.5982112695173,
122.417118736692)) ;
#42279 = CARTESIAN_POINT('Ctrl Pts',(-18.6522636552575,-12.5982105598513,
122.417109380617)) ;
#42280 = CARTESIAN_POINT('Ctrl Pts',(-18.6522882813838,-12.5982091382967,
122.417090639673)) ;
#42281 = CARTESIAN_POINT('Ctrl Pts',(-18.6523006125482,-12.5982084264826,
122.417081255788)) ;
#42282 = CARTESIAN_POINT('Ctrl Pts',(-18.6523253102834,-12.5982070008268,
122.417062461798)) ;
#42283 = CARTESIAN_POINT('Ctrl Pts',(-18.6523376777531,-12.5982062869333,
122.417053051012)) ;
#42284 = CARTESIAN_POINT('Ctrl Pts',(-18.6523624522966,-12.5982048568765,
122.417034200033)) ;
#42285 = CARTESIAN_POINT('Ctrl Pts',(-18.6523748579617,-12.5982041407946,
122.417024760915)) ;
#42286 = CARTESIAN_POINT('Ctrl Pts',(-18.6523997055566,-12.598202706554,122.417005855819)) ;
#42287 = CARTESIAN_POINT('Ctrl Pts',(-18.6524121484581,-12.5982019883392,
122.416996389105)) ;
#42288 = CARTESIAN_POINT('Ctrl Pts',(-18.652437073206,-12.5982005496783,122.416977426784)) ;
#42289 = CARTESIAN_POINT('Ctrl Pts',(-18.6524495545654,-12.5981998292603,
122.416967931551)) ;
#42290 = CARTESIAN_POINT('Ctrl Pts',(-18.6567934521444,-12.597949104504,122.413663426948)) ;
#42291 = CARTESIAN_POINT('Ctrl Pts',(-18.6611463339235,-12.5976988627779,
122.41039674497)) ;
#42292 = CARTESIAN_POINT('Ctrl Pts',(-18.6734340244622,-12.5969953609926,
122.401300104429)) ;
#42293 = CARTESIAN_POINT('Ctrl Pts',(-18.6814165759149,-12.5965417064587,
122.395535327698)) ;
#42294 = CARTESIAN_POINT('Ctrl Pts',(-18.7188613552968,-12.5944301126438,
122.369161238339)) ;
#42295 = CARTESIAN_POINT('Ctrl Pts',(-18.7491360860425,-12.5927700185484,
122.349734795158)) ;
#42296 = CARTESIAN_POINT('Ctrl Pts',(-18.7857313605827,-12.5908238242757,
122.328422627866)) ;
#42297 = CARTESIAN_POINT('Ctrl Pts',(-18.7912812474141,-12.590530242542,122.325247285693)) ;
#42298 = CARTESIAN_POINT('Ctrl Pts',(-18.8028525912613,-12.5899213713806,
122.318744129597)) ;
#42299 = CARTESIAN_POINT('Ctrl Pts',(-18.8088776479493,-12.5896061159434,
122.315423164743)) ;
#42300 = CARTESIAN_POINT('Ctrl Pts',(-18.8357079027558,-12.5882093979238,
122.300922022959)) ;
#42301 = CARTESIAN_POINT('Ctrl Pts',(-18.8568001232337,-12.5871301699246,
122.290283086876)) ;
#42302 = CARTESIAN_POINT('Ctrl Pts',(-18.8910698359654,-12.5853981641484,
122.274198884258)) ;
#42303 = CARTESIAN_POINT('Ctrl Pts',(-18.9040609666328,-12.5847464256436,
122.26837032123)) ;
#42304 = CARTESIAN_POINT('Ctrl Pts',(-18.9257845822485,-12.5836632697075,
122.259066369322)) ;
#42305 = CARTESIAN_POINT('Ctrl Pts',(-18.9344617697248,-12.5832323614048,
122.255465251041)) ;
#42306 = CARTESIAN_POINT('Ctrl Pts',(-18.9546147311477,-12.5822352048693,
122.247366662356)) ;
#42307 = CARTESIAN_POINT('Ctrl Pts',(-18.9661180654133,-12.5816687171091,
122.242940428904)) ;
#42308 = CARTESIAN_POINT('Ctrl Pts',(-18.991440956753,-12.5804270281306,122.233624287929)) ;
#42309 = CARTESIAN_POINT('Ctrl Pts',(-19.0052848873552,-12.5797514602395,
122.228805888461)) ;
#42310 = CARTESIAN_POINT('Ctrl Pts',(-19.036454196692,-12.5782395924792,122.218568314961)) ;
#42311 = CARTESIAN_POINT('Ctrl Pts',(-19.0538194611561,-12.5774037391161,
122.213280779272)) ;
#42312 = CARTESIAN_POINT('Ctrl Pts',(-19.0782936512719,-12.5762358103298,
122.206407364857)) ;
#42313 = CARTESIAN_POINT('Ctrl Pts',(-19.0853105791302,-12.5759020884391,
122.204502597124)) ;
#42314 = CARTESIAN_POINT('Ctrl Pts',(-19.0951918284113,-12.5754336967082,
122.201912648842)) ;
#42315 = CARTESIAN_POINT('Ctrl Pts',(-19.0980425471548,-12.5752987474402,
122.201176208488)) ;
#42316 = CARTESIAN_POINT('Ctrl Pts',(-19.1015729348443,-12.5751318427742,
122.200277479658)) ;
#42317 = CARTESIAN_POINT('Ctrl Pts',(-19.1022501704758,-12.5750998353516,
122.200105680638)) ;
#42318 = CARTESIAN_POINT('Ctrl Pts',(-19.1093955983175,-12.5747622335787,
122.198299425895)) ;
#42319 = CARTESIAN_POINT('Ctrl Pts',(-19.1158766436932,-12.5744569275915,
122.196716207647)) ;
#42320 = CARTESIAN_POINT('Ctrl Pts',(-19.1299808509378,-12.5737943389088,
122.19339019267)) ;
#42321 = CARTESIAN_POINT('Ctrl Pts',(-19.1376083219823,-12.5734371685362,
122.19166689041)) ;
#42322 = CARTESIAN_POINT('Ctrl Pts',(-19.1598876430185,-12.5723968088264,
122.186852511924)) ;
#42323 = CARTESIAN_POINT('Ctrl Pts',(-19.1745794660451,-12.5717144545339,
122.18395300421)) ;
#42324 = CARTESIAN_POINT('Ctrl Pts',(-19.2168706178744,-12.5697561605352,
122.176393419967)) ;
#42325 = CARTESIAN_POINT('Ctrl Pts',(-19.2445789193188,-12.5684789041517,
122.17239539015)) ;
#42326 = CARTESIAN_POINT('Ctrl Pts',(-19.2929290543277,-12.5662551913537,
122.16706904809)) ;
#42327 = CARTESIAN_POINT('Ctrl Pts',(-19.313513071246,-12.5653101695494,122.165316543651)) ;
#42328 = CARTESIAN_POINT('Ctrl Pts',(-19.3465686699224,-12.5637932141276,
122.163325872459)) ;
#42329 = CARTESIAN_POINT('Ctrl Pts',(-19.3590168401675,-12.5632220935145,
122.162762865888)) ;
#42330 = CARTESIAN_POINT('Ctrl Pts',(-19.374320526249,-12.5625197120779,122.162299859459)) ;
#42331 = CARTESIAN_POINT('Ctrl Pts',(-19.3771700169683,-12.5623889203638,
122.162223404289)) ;
#42332 = CARTESIAN_POINT('Ctrl Pts',(-19.3805399956548,-12.5622342201541,
122.162144518463)) ;
#42333 = CARTESIAN_POINT('Ctrl Pts',(-19.3810602557747,-12.5622103368968,
122.162132665065)) ;
#42334 = CARTESIAN_POINT('Ctrl Pts',(-19.3826507720328,-12.5621373204145,
122.16209742112)) ;
#42335 = CARTESIAN_POINT('Ctrl Pts',(-19.3837210507941,-12.5620881844143,
122.16207508055)) ;
#42336 = CARTESIAN_POINT('Ctrl Pts',(-19.3856611977276,-12.5619991086109,
122.162037076059)) ;
#42337 = CARTESIAN_POINT('Ctrl Pts',(-19.3865310561313,-12.5619591701102,
122.162020945343)) ;
#42338 = CARTESIAN_POINT('Ctrl Pts',(-19.3881164518054,-12.5618863753109,
122.161993201357)) ;
#42339 = CARTESIAN_POINT('Ctrl Pts',(-19.3888319836274,-12.5618535198421,
122.161981294395)) ;
#42340 = CARTESIAN_POINT('Ctrl Pts',(-19.3901421788481,-12.5617933565315,
122.161960617243)) ;
#42341 = CARTESIAN_POINT('Ctrl Pts',(-19.3907368390446,-12.5617660492346,
122.161951656968)) ;
#42342 = CARTESIAN_POINT('Ctrl Pts',(-19.3918300580083,-12.5617158459883,
122.161935964835)) ;
#42343 = CARTESIAN_POINT('Ctrl Pts',(-19.3923286148623,-12.5616929504034,
122.161929106876)) ;
#42344 = CARTESIAN_POINT('Ctrl Pts',(-19.3932483021518,-12.5616507136896,
122.161917006378)) ;
#42345 = CARTESIAN_POINT('Ctrl Pts',(-19.3936694313873,-12.5616313728104,
122.161911678375)) ;
#42346 = CARTESIAN_POINT('Ctrl Pts',(-19.4113900891808,-12.5608175087271,
122.161696439116)) ;
#42347 = CARTESIAN_POINT('Ctrl Pts',(-19.4286920506294,-12.5600218326315,
122.161845492945)) ;
#42348 = CARTESIAN_POINT('Ctrl Pts',(-19.4630088294997,-12.5584411133718,
122.162853826808)) ;
#42349 = CARTESIAN_POINT('Ctrl Pts',(-19.4800203654697,-12.5576564426578,
122.163701890469)) ;
#42350 = CARTESIAN_POINT('Ctrl Pts',(-19.5262482463775,-12.5555216647514,
122.166954629337)) ;
#42351 = CARTESIAN_POINT('Ctrl Pts',(-19.555405934401,-12.5541726197496,122.170039787513)) ;
#42352 = CARTESIAN_POINT('Ctrl Pts',(-19.59792318565,-12.5522000013078,122.176056873907)) ;
#42353 = CARTESIAN_POINT('Ctrl Pts',(-19.6113860357677,-12.5515745361261,
122.178187285577)) ;
#42354 = CARTESIAN_POINT('Ctrl Pts',(-19.6374693193354,-12.5503604965431,
122.182753251485)) ;
#42355 = CARTESIAN_POINT('Ctrl Pts',(-19.6500923643258,-12.5497719283014,
122.185164130982)) ;
#42356 = CARTESIAN_POINT('Ctrl Pts',(-19.6916144804534,-12.5478313074489,
122.19376010551)) ;
#42357 = CARTESIAN_POINT('Ctrl Pts',(-19.7203314428175,-12.5464819532277,
122.200775348978)) ;
#42358 = CARTESIAN_POINT('Ctrl Pts',(-19.7690137598523,-12.544171420534,122.214513918643)) ;
#42359 = CARTESIAN_POINT('Ctrl Pts',(-19.7891073189696,-12.543210809444,122.220736018034)) ;
#42360 = CARTESIAN_POINT('Ctrl Pts',(-19.8138279735893,-12.5420166036866,
122.229080138977)) ;
#42361 = CARTESIAN_POINT('Ctrl Pts',(-19.8186118233225,-12.5417849199917,
122.230727282536)) ;
#42362 = CARTESIAN_POINT('Ctrl Pts',(-19.8286646732417,-12.5412967228836,
122.234257026657)) ;
#42363 = CARTESIAN_POINT('Ctrl Pts',(-19.8339312982787,-12.5410401833435,
122.236146052025)) ;
#42364 = CARTESIAN_POINT('Ctrl Pts',(-19.8393751002482,-12.5407741391536,
122.238139979367)) ;
#42365 = CARTESIAN_POINT('Ctrl Pts',(-19.8395651295574,-12.5407648511191,
122.238209634658)) ;
#42366 = CARTESIAN_POINT('Ctrl Pts',(-19.8399251962172,-12.5407472500901,
122.238341716392)) ;
#42367 = CARTESIAN_POINT('Ctrl Pts',(-19.8400952369567,-12.5407389371509,
122.238404133657)) ;
#42368 = CARTESIAN_POINT('Ctrl Pts',(-19.8404178425076,-12.5407231639424,
122.238522632831)) ;
#42369 = CARTESIAN_POINT('Ctrl Pts',(-19.8405704099801,-12.5407157037166,
122.238578707552)) ;
#42370 = CARTESIAN_POINT('Ctrl Pts',(-19.8408602071454,-12.5407015318824,
122.238685283905)) ;
#42371 = CARTESIAN_POINT('Ctrl Pts',(-19.8409974388453,-12.5406948203131,
122.238735779834)) ;
#42372 = CARTESIAN_POINT('Ctrl Pts',(-19.8412583897215,-12.540682056919,122.2388318516)) ;
#42373 = CARTESIAN_POINT('Ctrl Pts',(-19.8413821105724,-12.5406760051216,
122.238877422941)) ;
#42374 = CARTESIAN_POINT('Ctrl Pts',(-19.8416176052147,-12.5406644850109,
122.23896420736)) ;
#42375 = CARTESIAN_POINT('Ctrl Pts',(-19.8417293804722,-12.5406590167133,
122.239005416896)) ;
#42376 = CARTESIAN_POINT('Ctrl Pts',(-19.8419423331497,-12.540648597847,122.239083963318)) ;
#42377 = CARTESIAN_POINT('Ctrl Pts',(-19.8420435116101,-12.5406436472977,
122.239121297312)) ;
#42378 = CARTESIAN_POINT('Ctrl Pts',(-19.8422364385473,-12.5406342069886,
122.239192514084)) ;
#42379 = CARTESIAN_POINT('Ctrl Pts',(-19.8423281876774,-12.5406297172537,
122.239226394463)) ;
#42380 = CARTESIAN_POINT('Ctrl Pts',(-19.8425032697084,-12.5406211491292,
122.239291070693)) ;
#42381 = CARTESIAN_POINT('Ctrl Pts',(-19.8425866035672,-12.5406170707389,
122.23932186476)) ;
#42382 = CARTESIAN_POINT('Ctrl Pts',(-19.8427457408515,-12.5406092820854,
122.239380689481)) ;
#42383 = CARTESIAN_POINT('Ctrl Pts',(-19.8428215446682,-12.5406055718406,
122.239408718539)) ;
#42384 = CARTESIAN_POINT('Ctrl Pts',(-19.8429663967868,-12.540598481658,122.239462294721)) ;
#42385 = CARTESIAN_POINT('Ctrl Pts',(-19.8430354455828,-12.5405951017267,
122.239487840605)) ;
#42386 = CARTESIAN_POINT('Ctrl Pts',(-19.8431674686224,-12.5405886389267,
122.23953669824)) ;
#42387 = CARTESIAN_POINT('Ctrl Pts',(-19.8432304433881,-12.5405855560577,
122.239560009019)) ;
#42388 = CARTESIAN_POINT('Ctrl Pts',(-19.8487290245072,-12.5403163674425,
122.241595871051)) ;
#42389 = CARTESIAN_POINT('Ctrl Pts',(-19.8541505595263,-12.5400500239687,
122.243646196633)) ;
#42390 = CARTESIAN_POINT('Ctrl Pts',(-19.8644764810031,-12.5395410404277,
122.24763358236)) ;
#42391 = CARTESIAN_POINT('Ctrl Pts',(-19.869383260888,-12.5392984364597,122.249564114839)) ;
#42392 = CARTESIAN_POINT('Ctrl Pts',(-19.8910811647693,-12.5382224562978,
122.25825991873)) ;
#42393 = CARTESIAN_POINT('Ctrl Pts',(-19.9077363657536,-12.5373881047342,
122.265358428475)) ;
#42394 = CARTESIAN_POINT('Ctrl Pts',(-19.948165803999,-12.5353435195757,122.283637221976)) ;
#42395 = CARTESIAN_POINT('Ctrl Pts',(-19.9717531705136,-12.5341340752103,
122.295210069937)) ;
#42396 = CARTESIAN_POINT('Ctrl Pts',(-20.0038506164595,-12.5324650231041,
122.312233600051)) ;
#42397 = CARTESIAN_POINT('Ctrl Pts',(-20.0126855108448,-12.532003078948,122.317056981037)) ;
#42398 = CARTESIAN_POINT('Ctrl Pts',(-20.0283729895442,-12.5311781174807,
122.325869108256)) ;
#42399 = CARTESIAN_POINT('Ctrl Pts',(-20.035247696484,-12.5308149452415,122.329817337744)) ;
#42400 = CARTESIAN_POINT('Ctrl Pts',(-20.052174639553,-12.5299164678722,122.339754014594)) ;
#42401 = CARTESIAN_POINT('Ctrl Pts',(-20.0621812477939,-12.5293815441596,
122.345818718191)) ;
#42402 = CARTESIAN_POINT('Ctrl Pts',(-20.0839274480615,-12.5282100720115,
122.359419520616)) ;
#42403 = CARTESIAN_POINT('Ctrl Pts',(-20.0956290266402,-12.5275738342157,
122.36701346472)) ;
#42404 = CARTESIAN_POINT('Ctrl Pts',(-20.1371995564869,-12.5252898670514,
122.39499120492)) ;
#42405 = CARTESIAN_POINT('Ctrl Pts',(-20.1663077450611,-12.5236463313578,
122.416472843222)) ;
#42406 = CARTESIAN_POINT('Ctrl Pts',(-20.2002484428382,-12.5216543243005,
122.443872066418)) ;
#42407 = CARTESIAN_POINT('Ctrl Pts',(-20.206011247099,-12.5213133141225,122.448610024873)) ;
#42408 = CARTESIAN_POINT('Ctrl Pts',(-20.2150684731054,-12.5207726138369,
122.456193433105)) ;
#42409 = CARTESIAN_POINT('Ctrl Pts',(-20.2183910409297,-12.5205732262521,
122.459004992359)) ;
#42410 = CARTESIAN_POINT('Ctrl Pts',(-20.2256882974061,-12.5201330076515,
122.465245631297)) ;
#42411 = CARTESIAN_POINT('Ctrl Pts',(-20.2296562007776,-12.5198921200652,
122.468682506186)) ;
#42412 = CARTESIAN_POINT('Ctrl Pts',(-20.2390746949293,-12.5193167913841,
122.47694492528)) ;
#42413 = CARTESIAN_POINT('Ctrl Pts',(-20.244505011187,-12.5189822124506,122.481793289362)) ;
#42414 = CARTESIAN_POINT('Ctrl Pts',(-20.2632234434634,-12.517819201591,122.498801895604)) ;
#42415 = CARTESIAN_POINT('Ctrl Pts',(-20.2762908516892,-12.5169901071281,
122.511201710088)) ;
#42416 = CARTESIAN_POINT('Ctrl Pts',(-20.2987081723119,-12.5155386848456,
122.533413995483)) ;
#42417 = CARTESIAN_POINT('Ctrl Pts',(-20.3081750123101,-12.514916140234,122.543104232447)) ;
#42418 = CARTESIAN_POINT('Ctrl Pts',(-20.3231299535994,-12.5139171839564,
122.558918341652)) ;
#42419 = CARTESIAN_POINT('Ctrl Pts',(-20.3287183775611,-12.5135402701681,
122.564945810877)) ;
#42420 = CARTESIAN_POINT('Ctrl Pts',(-20.3394589780795,-12.5128087217969,
122.576761872617)) ;
#42421 = CARTESIAN_POINT('Ctrl Pts',(-20.3446175793769,-12.5124540628249,
122.582544125998)) ;
#42422 = CARTESIAN_POINT('Ctrl Pts',(-20.35317908599,-12.5118597788923,122.592322208077)) ;
#42423 = CARTESIAN_POINT('Ctrl Pts',(-20.3566111861844,-12.511619976883,122.59629217012)) ;
#42424 = CARTESIAN_POINT('Ctrl Pts',(-20.3664643869393,-12.5109269031389,
122.60783565252)) ;
#42425 = CARTESIAN_POINT('Ctrl Pts',(-20.3728203742093,-12.5104741101781,
122.615464209613)) ;
#42426 = CARTESIAN_POINT('Ctrl Pts',(-20.3964459859189,-12.5087676513948,
122.644517037307)) ;
#42427 = CARTESIAN_POINT('Ctrl Pts',(-20.4130973853529,-12.5075157518028,
122.666433746619)) ;
#42428 = CARTESIAN_POINT('Ctrl Pts',(-20.4328063780566,-12.5059581201874,
122.694234471175)) ;
#42429 = CARTESIAN_POINT('Ctrl Pts',(-20.436558676165,-12.5056579513954,122.699616630187)) ;
#42430 = CARTESIAN_POINT('Ctrl Pts',(-20.4430090363465,-12.5051354306199,
122.709025834574)) ;
#42431 = CARTESIAN_POINT('Ctrl Pts',(-20.4457263725472,-12.5049132399226,
122.713039498848)) ;
#42432 = CARTESIAN_POINT('Ctrl Pts',(-20.4515086819168,-12.5044358910012,
122.721688242119)) ;
#42433 = CARTESIAN_POINT('Ctrl Pts',(-20.4545662293466,-12.5041806747331,
122.726328156609)) ;
#42434 = CARTESIAN_POINT('Ctrl Pts',(-20.4608144196517,-12.5036532090433,
122.735948977861)) ;
#42435 = CARTESIAN_POINT('Ctrl Pts',(-20.464000849022,-12.5033809292519,122.740932454319)) ;
#42436 = CARTESIAN_POINT('Ctrl Pts',(-20.4720224206811,-12.502686954097,122.753676353063)) ;
#42437 = CARTESIAN_POINT('Ctrl Pts',(-20.4768079952114,-12.5022648338344,
122.76146753493)) ;
#42438 = CARTESIAN_POINT('Ctrl Pts',(-20.4874017674507,-12.501311673866,122.779146833229)) ;
#42439 = CARTESIAN_POINT('Ctrl Pts',(-20.4931602188682,-12.5007801590533,
122.789063748253)) ;
#42440 = CARTESIAN_POINT('Ctrl Pts',(-20.5113092029293,-12.4990619699213,
122.821333505918)) ;
#42441 = CARTESIAN_POINT('Ctrl Pts',(-20.5231511539718,-12.4978751115754,
122.84398788179)) ;
#42442 = CARTESIAN_POINT('Ctrl Pts',(-20.5364386895791,-12.4964705762957,
122.87142554464)) ;
#42443 = CARTESIAN_POINT('Ctrl Pts',(-20.5385607013546,-12.4962438242242,
122.875874206416)) ;
#42444 = CARTESIAN_POINT('Ctrl Pts',(-20.5418174161854,-12.4958919850364,
122.882806926424)) ;
#42445 = CARTESIAN_POINT('Ctrl Pts',(-20.5429703787687,-12.4957666572122,
122.885282337128)) ;
#42446 = CARTESIAN_POINT('Ctrl Pts',(-20.5452527984745,-12.4955170149904,
122.890224945431)) ;
#42447 = CARTESIAN_POINT('Ctrl Pts',(-20.5463823520393,-12.4953926998991,
122.892692081729)) ;
#42448 = CARTESIAN_POINT('Ctrl Pts',(-20.548615950219,-12.4951453312416,122.897612907794)) ;
#42449 = CARTESIAN_POINT('Ctrl Pts',(-20.5497201233433,-12.4950222765312,
122.90006652276)) ;
#42450 = CARTESIAN_POINT('Ctrl Pts',(-20.5522251138042,-12.4947413310105,
122.90568130678)) ;
#42451 = CARTESIAN_POINT('Ctrl Pts',(-20.5536207551637,-12.4945835107433,
122.908844763223)) ;
#42452 = CARTESIAN_POINT('Ctrl Pts',(-20.5574141688876,-12.494150938545,122.917540698383)) ;
#42453 = CARTESIAN_POINT('Ctrl Pts',(-20.559785068028,-12.4938765422664,122.923084808435)) ;
#42454 = CARTESIAN_POINT('Ctrl Pts',(-20.5729182539762,-12.4923329668888,
122.954420685885)) ;
#42455 = CARTESIAN_POINT('Ctrl Pts',(-20.5828498748888,-12.4910752987972,
122.980541181549)) ;
#42456 = CARTESIAN_POINT('Ctrl Pts',(-20.5919009558887,-12.4898128815271,
123.00698191868)) ;
#42457 = CARTESIAN_POINT('Ctrl Pts',(-20.5919009558702,-12.4898128815389,
123.006981918687)) ;
#42458 = CARTESIAN_POINT('Ctrl Pts',(-20.612879600018,-12.4868868188589,123.068266969564)) ;
#42459 = CARTESIAN_POINT('Ctrl Pts',(-20.6290608408633,-12.4839078358475,
123.131081843711)) ;
#42460 = CARTESIAN_POINT('Ctrl Pts',(-20.6403019341679,-12.4808963918362,
123.194867639949)) ;
#42461 = CARTESIAN_POINT('Ctrl Pts',(-20.6529209728128,-12.4775158017703,
123.266472367879)) ;
#42462 = CARTESIAN_POINT('Ctrl Pts',(-20.6592686579283,-12.4741985571895,
123.339040698344)) ;
#42463 = CARTESIAN_POINT('Ctrl Pts',(-20.6592722344714,-12.4709053075509,
123.411752881973)) ;
#42464 = CARTESIAN_POINT('Ctrl Pts',(-20.6592758117281,-12.4676114008349,
123.484479573319)) ;
#42465 = CARTESIAN_POINT('Ctrl Pts',(-20.6529324105397,-12.4643042891385,
123.557066247848)) ;
#42466 = CARTESIAN_POINT('Ctrl Pts',(-20.6403149806974,-12.4609455594289,
123.628687049695)) ;
#42467 = CARTESIAN_POINT('Ctrl Pts',(-20.6199530079514,-12.4555252508826,
123.744268498017)) ;
#42468 = CARTESIAN_POINT('Ctrl Pts',(-20.5834152479651,-12.4501098853957,
123.856407451353)) ;
#42469 = CARTESIAN_POINT('Ctrl Pts',(-20.5317752294988,-12.444794208555,123.961802575126)) ;
#42470 = CARTESIAN_POINT('Ctrl Pts',(-20.5195465431204,-12.4435354223093,
123.986760813963)) ;
#42471 = CARTESIAN_POINT('Ctrl Pts',(-20.5064888790875,-12.442279198336,124.011304221324)) ;
#42472 = CARTESIAN_POINT('Ctrl Pts',(-20.4926240347142,-12.4410177925474,
124.035391851884)) ;
#42473 = CARTESIAN_POINT('Ctrl Pts',(-20.4565432913977,-12.4377352127181,
124.098075542512)) ;
#42474 = CARTESIAN_POINT('Ctrl Pts',(-20.4150917468142,-12.4344077824959,
124.157507085578)) ;
#42475 = CARTESIAN_POINT('Ctrl Pts',(-20.3687357231582,-12.4310436061992,
124.213019594203)) ;
#42476 = CARTESIAN_POINT('Ctrl Pts',(-20.3221020045676,-12.4276592768643,
124.268864649523)) ;
#42477 = CARTESIAN_POINT('Ctrl Pts',(-20.2706831796546,-12.4243269367417,
124.320530635347)) ;
#42478 = CARTESIAN_POINT('Ctrl Pts',(-20.2150581879501,-12.4210466606148,
124.367434060606)) ;
#42479 = CARTESIAN_POINT('Ctrl Pts',(-20.1599469320555,-12.4177966801385,
124.413904299838)) ;
#42480 = CARTESIAN_POINT('Ctrl Pts',(-20.100924231773,-12.4144999293209,124.455516207877)) ;
#42481 = CARTESIAN_POINT('Ctrl Pts',(-20.0386444222632,-12.4111419282649,
124.491810038396)) ;
#42482 = CARTESIAN_POINT('Ctrl Pts',(-19.9757838743836,-12.4077526149735,
124.528442296731)) ;
#42483 = CARTESIAN_POINT('Ctrl Pts',(-19.9098471799391,-12.4044322628923,
124.559515887026)) ;
#42484 = CARTESIAN_POINT('Ctrl Pts',(-19.841576804616,-12.401145070914,124.584679559154)) ;
#42485 = CARTESIAN_POINT('Ctrl Pts',(-19.8324565589139,-12.4007059346361,
124.588041176422)) ;
#42486 = CARTESIAN_POINT('Ctrl Pts',(-19.8232974443718,-12.4002663542339,
124.591296288893)) ;
#42487 = CARTESIAN_POINT('Ctrl Pts',(-19.814101322745,-12.3998259425229,124.594444237049)) ;
#42488 = CARTESIAN_POINT('Ctrl Pts',(-19.7549143065903,-12.3969914155221,
124.614704697484)) ;
#42489 = CARTESIAN_POINT('Ctrl Pts',(-19.6942924538234,-12.39410730187,124.630492631303)) ;
#42490 = CARTESIAN_POINT('Ctrl Pts',(-19.6327443861755,-12.3912118041499,
124.641676227974)) ;
#42491 = CARTESIAN_POINT('Ctrl Pts',(-19.5611608795202,-12.3878441942762,
124.654683314912)) ;
#42492 = CARTESIAN_POINT('Ctrl Pts',(-19.4885786093359,-12.3845400790549,
124.661415969366)) ;
#42493 = CARTESIAN_POINT('Ctrl Pts',(-19.4158220208586,-12.3812149268458,
124.661797206604)) ;
#42494 = CARTESIAN_POINT('Ctrl Pts',(-19.343386996428,-12.377904470892,124.662176758878)) ;
#42495 = CARTESIAN_POINT('Ctrl Pts',(-19.2710559139747,-12.3745611835623,
124.656259343137)) ;
#42496 = CARTESIAN_POINT('Ctrl Pts',(-19.1996452414557,-12.3712618741336,
124.644111620985)) ;
#42497 = CARTESIAN_POINT('Ctrl Pts',(-19.1286196590726,-12.3679803566045,
124.6320294068)) ;
#42498 = CARTESIAN_POINT('Ctrl Pts',(-19.0587744373215,-12.3647050110643,
124.613829966515)) ;
#42499 = CARTESIAN_POINT('Ctrl Pts',(-18.990886651944,-12.3613625287099,124.589716528532)) ;
#42500 = CARTESIAN_POINT('Ctrl Pts',(-18.9459998958675,-12.3591525112628,
124.573772953368)) ;
#42501 = CARTESIAN_POINT('Ctrl Pts',(-18.9020613678976,-12.3569451070035,
124.555276798977)) ;
#42502 = CARTESIAN_POINT('Ctrl Pts',(-18.8592840273916,-12.3547760794749,
124.53431736011)) ;
#42503 = CARTESIAN_POINT('Ctrl Pts',(-18.8367533302812,-12.3536336591727,
124.52327808644)) ;
#42504 = CARTESIAN_POINT('Ctrl Pts',(-18.8145600542151,-12.3525002895855,
124.511562945122)) ;
#42505 = CARTESIAN_POINT('Ctrl Pts',(-18.7927341753271,-12.3513654274978,
124.49918772465)) ;
#42506 = CARTESIAN_POINT('Ctrl Pts',(-18.7298943652711,-12.3480979981127,
124.463557704534)) ;
#42507 = CARTESIAN_POINT('Ctrl Pts',(-18.6702644990938,-12.3447812010954,
124.422549451139)) ;
#42508 = CARTESIAN_POINT('Ctrl Pts',(-18.6145104587646,-12.3414395552883,
124.376621973083)) ;
#42509 = CARTESIAN_POINT('Ctrl Pts',(-18.5583545546135,-12.3380738235755,
124.330363459073)) ;
#42510 = CARTESIAN_POINT('Ctrl Pts',(-18.5063444574012,-12.3347691056417,
124.279290603724)) ;
#42511 = CARTESIAN_POINT('Ctrl Pts',(-18.4590716004823,-12.3314422012028,
124.223983531472)) ;
#42512 = CARTESIAN_POINT('Ctrl Pts',(-18.4118841285253,-12.3281213058699,
124.168776355704)) ;
#42513 = CARTESIAN_POINT('Ctrl Pts',(-18.3695977095774,-12.3247766394425,
124.109561752482)) ;
#42514 = CARTESIAN_POINT('Ctrl Pts',(-18.3326922444195,-12.3214625370788,
124.047011597277)) ;
#42515 = CARTESIAN_POINT('Ctrl Pts',(-18.2960197209067,-12.3181693528218,
123.984856249073)) ;
#42516 = CARTESIAN_POINT('Ctrl Pts',(-18.2647994434423,-12.3148741484591,
123.919643033231)) ;
#42517 = CARTESIAN_POINT('Ctrl Pts',(-18.239380419725,-12.3115457444478,123.852101929866)) ;
#42518 = CARTESIAN_POINT('Ctrl Pts',(-18.2349565077231,-12.3109664709628,
123.840347115789)) ;
#42519 = CARTESIAN_POINT('Ctrl Pts',(-18.2307100075446,-12.3103871771171,
123.828526282873)) ;
#42520 = CARTESIAN_POINT('Ctrl Pts',(-18.2266423654683,-12.3098085062256,
123.816643453356)) ;
#42521 = CARTESIAN_POINT('Origin',(-19.4092722359532,-13.9601742359176,123.411814366564)) ;
#42522 = CARTESIAN_POINT('',(-18.3578548015691,-12.0237683560339,124.087847855652)) ;
#42523 = CARTESIAN_POINT('',(-18.2266508223232,-11.7,123.81666815758)) ;
#42524 = CARTESIAN_POINT('Ctrl Pts',(-18.3578549773983,-12.0237683877577,
124.087848203357)) ;
#42525 = CARTESIAN_POINT('Ctrl Pts',(-18.3582088223246,-12.0157754186098,
124.088398528862)) ;
#42526 = CARTESIAN_POINT('Ctrl Pts',(-18.3583806245238,-12.007835083744,124.088665030377)) ;
#42527 = CARTESIAN_POINT('Ctrl Pts',(-18.3583806245238,-12.,124.088665030376)) ;
#42528 = CARTESIAN_POINT('Ctrl Pts',(-18.3583806245238,-11.9621695797156,
124.088665030376)) ;
#42529 = CARTESIAN_POINT('Ctrl Pts',(-18.3540742080748,-11.9219235159019,
124.082116008719)) ;
#42530 = CARTESIAN_POINT('Ctrl Pts',(-18.3375495990129,-11.8480564696762,
124.055365260225)) ;
#42531 = CARTESIAN_POINT('Ctrl Pts',(-18.3254377303918,-11.8144220247009,
124.035135143544)) ;
#42532 = CARTESIAN_POINT('Ctrl Pts',(-18.2995859960063,-11.761317155029,123.987854560826)) ;
#42533 = CARTESIAN_POINT('Ctrl Pts',(-18.2841086594605,-11.7382522587826,
123.957600803974)) ;
#42534 = CARTESIAN_POINT('Ctrl Pts',(-18.2537250256192,-11.7075896772134,
123.889921628303)) ;
#42535 = CARTESIAN_POINT('Ctrl Pts',(-18.2389020196221,-11.7,123.852455220934)) ;
#42536 = CARTESIAN_POINT('Ctrl Pts',(-18.2266508223232,-11.7,123.81666815758)) ;
#42537 = CARTESIAN_POINT('',(-20.6477480580335,-12.1788369205275,123.242469634735)) ;
#42538 = CARTESIAN_POINT('Ctrl Pts',(-18.3578547670581,-12.0237683857362,
124.08784787622)) ;
#42539 = CARTESIAN_POINT('Ctrl Pts',(-18.3612709689585,-12.0240583399856,
124.093161006863)) ;
#42540 = CARTESIAN_POINT('Ctrl Pts',(-18.3647221587456,-12.0243476810626,
124.09844020082)) ;
#42541 = CARTESIAN_POINT('Ctrl Pts',(-18.3720326190228,-12.0249532474956,
124.109439954333)) ;
#42542 = CARTESIAN_POINT('Ctrl Pts',(-18.3758941530953,-12.0252689942272,
124.115147304605)) ;
#42543 = CARTESIAN_POINT('Ctrl Pts',(-18.3962392787662,-12.0269117251184,
124.144688135181)) ;
#42544 = CARTESIAN_POINT('Ctrl Pts',(-18.413500777637,-12.0282350907313,124.167975020533)) ;
#42545 = CARTESIAN_POINT('Ctrl Pts',(-18.4355734167998,-12.0298564993528,
124.195684372511)) ;
#42546 = CARTESIAN_POINT('Ctrl Pts',(-18.4396298675406,-12.0301517584363,
124.200696647887)) ;
#42547 = CARTESIAN_POINT('Ctrl Pts',(-18.4472060060469,-12.030698480577,124.209911236339)) ;
#42548 = CARTESIAN_POINT('Ctrl Pts',(-18.4507149053608,-12.0309498672555,
124.214122217716)) ;
#42549 = CARTESIAN_POINT('Ctrl Pts',(-18.4585324561556,-12.0315061313412,
124.223379458499)) ;
#42550 = CARTESIAN_POINT('Ctrl Pts',(-18.4628538019447,-12.0318111676068,
124.228414742769)) ;
#42551 = CARTESIAN_POINT('Ctrl Pts',(-18.4806423513383,-12.033056668807,124.248811299113)) ;
#42552 = CARTESIAN_POINT('Ctrl Pts',(-18.4944450745935,-12.0339992029702,
124.263875745673)) ;
#42553 = CARTESIAN_POINT('Ctrl Pts',(-18.5141829230335,-12.0353100504372,
124.284385105258)) ;
#42554 = CARTESIAN_POINT('Ctrl Pts',(-18.5198107691195,-12.035679840316,124.290121187478)) ;
#42555 = CARTESIAN_POINT('Ctrl Pts',(-18.5293205336302,-12.0362979726219,
124.299628697603)) ;
#42556 = CARTESIAN_POINT('Ctrl Pts',(-18.53317233433,-12.0365465344298,124.303429893235)) ;
#42557 = CARTESIAN_POINT('Ctrl Pts',(-18.5406782615933,-12.0370274103583,
124.310741606244)) ;
#42558 = CARTESIAN_POINT('Ctrl Pts',(-18.5443292894376,-12.0372597469713,
124.314255153538)) ;
#42559 = CARTESIAN_POINT('Ctrl Pts',(-18.5515137068691,-12.0377138829511,
124.321085387555)) ;
#42560 = CARTESIAN_POINT('Ctrl Pts',(-18.5550452201474,-12.0379356960937,
124.324403918043)) ;
#42561 = CARTESIAN_POINT('Ctrl Pts',(-18.5636048377083,-12.0384699476098,
124.332354090901)) ;
#42562 = CARTESIAN_POINT('Ctrl Pts',(-18.5686518180992,-12.038782184171,124.336965189997)) ;
#42563 = CARTESIAN_POINT('Ctrl Pts',(-18.5914463314759,-12.0401803146378,
124.357450526429)) ;
#42564 = CARTESIAN_POINT('Ctrl Pts',(-18.6096074102078,-12.0412612739329,
124.372857097527)) ;
#42565 = CARTESIAN_POINT('Ctrl Pts',(-18.6402319121722,-12.0430413302621,
124.397367295236)) ;
#42566 = CARTESIAN_POINT('Ctrl Pts',(-18.6524433750215,-12.0437409093724,
124.406775505422)) ;
#42567 = CARTESIAN_POINT('Ctrl Pts',(-18.672791183876,-12.0448937163516,124.421860892095)) ;
#42568 = CARTESIAN_POINT('Ctrl Pts',(-18.6808266487049,-12.0453457458803,
124.427671319415)) ;
#42569 = CARTESIAN_POINT('Ctrl Pts',(-18.6926060729012,-12.0460043095135,
124.435977361085)) ;
#42570 = CARTESIAN_POINT('Ctrl Pts',(-18.6962957325594,-12.0462100160739,
124.438549353814)) ;
#42571 = CARTESIAN_POINT('Ctrl Pts',(-18.7030476176529,-12.0465854497209,
124.443202021255)) ;
#42572 = CARTESIAN_POINT('Ctrl Pts',(-18.706105361161,-12.0467551034372,124.445289113152)) ;
#42573 = CARTESIAN_POINT('Ctrl Pts',(-18.7122417299274,-12.0470948522912,
124.44943770917)) ;
#42574 = CARTESIAN_POINT('Ctrl Pts',(-18.7153203387539,-12.0472649459507,
124.451499170589)) ;
#42575 = CARTESIAN_POINT('Ctrl Pts',(-18.7240874100868,-12.0477483350986,
124.457313384164)) ;
#42576 = CARTESIAN_POINT('Ctrl Pts',(-18.7297974432447,-12.0480619910566,
124.461033336482)) ;
#42577 = CARTESIAN_POINT('Ctrl Pts',(-18.7632486650801,-12.0498927564979,
124.482438424913)) ;
#42578 = CARTESIAN_POINT('Ctrl Pts',(-18.7916487038095,-12.0514225918069,
124.499069364155)) ;
#42579 = CARTESIAN_POINT('Ctrl Pts',(-18.8309632392298,-12.0534908001967,
124.520053878567)) ;
#42580 = CARTESIAN_POINT('Ctrl Pts',(-18.8413320036948,-12.0540314147734,
124.525403162818)) ;
#42581 = CARTESIAN_POINT('Ctrl Pts',(-18.8568201622614,-12.0548308889698,
124.533120966241)) ;
#42582 = CARTESIAN_POINT('Ctrl Pts',(-18.8618830985897,-12.0550909775863,
124.535601231108)) ;
#42583 = CARTESIAN_POINT('Ctrl Pts',(-18.8701791912078,-12.0555150752811,
124.539596009511)) ;
#42584 = CARTESIAN_POINT('Ctrl Pts',(-18.8734023498748,-12.0556793348499,
124.541131067215)) ;
#42585 = CARTESIAN_POINT('Ctrl Pts',(-18.8791665832693,-12.0559721852485,
124.543846100261)) ;
#42586 = CARTESIAN_POINT('Ctrl Pts',(-18.8817051288494,-12.0561008427538,
124.54503137873)) ;
#42587 = CARTESIAN_POINT('Ctrl Pts',(-18.8868594141117,-12.056361440124,124.547416905385)) ;
#42588 = CARTESIAN_POINT('Ctrl Pts',(-18.8894753568765,-12.0564933731153,
124.548616674428)) ;
#42589 = CARTESIAN_POINT('Ctrl Pts',(-18.8947406895689,-12.0567582758437,
124.551009578329)) ;
#42590 = CARTESIAN_POINT('Ctrl Pts',(-18.8973901424193,-12.0568912425011,
124.552202530793)) ;
#42591 = CARTESIAN_POINT('Ctrl Pts',(-18.9050072965419,-12.0572725923696,
124.555600365016)) ;
#42592 = CARTESIAN_POINT('Ctrl Pts',(-18.9099852587864,-12.0575206812022,
124.557782103541)) ;
#42593 = CARTESIAN_POINT('Ctrl Pts',(-18.9360113871106,-12.058812156449,124.568987044983)) ;
#42594 = CARTESIAN_POINT('Ctrl Pts',(-18.9572904285564,-12.0598484571019,
124.577463066214)) ;
#42595 = CARTESIAN_POINT('Ctrl Pts',(-18.9943522547517,-12.0616349119909,
124.59105826424)) ;
#42596 = CARTESIAN_POINT('Ctrl Pts',(-19.0100260955046,-12.0623856386635,
124.596456623542)) ;
#42597 = CARTESIAN_POINT('Ctrl Pts',(-19.033332479642,-12.0634986553714,124.603968672123)) ;
#42598 = CARTESIAN_POINT('Ctrl Pts',(-19.0408851478688,-12.0638587898761,
124.606324115848)) ;
#42599 = CARTESIAN_POINT('Ctrl Pts',(-19.0532910983399,-12.0644496650562,
124.610064296411)) ;
#42600 = CARTESIAN_POINT('Ctrl Pts',(-19.0581313172037,-12.0646800274288,
124.611491623022)) ;
#42601 = CARTESIAN_POINT('Ctrl Pts',(-19.0631991562815,-12.0649210690279,
124.612952774745)) ;
#42602 = CARTESIAN_POINT('Ctrl Pts',(-19.0634182941461,-12.0649314915787,
124.613015891296)) ;
#42603 = CARTESIAN_POINT('Ctrl Pts',(-19.0638422009522,-12.0649516526898,
124.613137860212)) ;
#42604 = CARTESIAN_POINT('Ctrl Pts',(-19.0640469678079,-12.0649613911891,
124.613196720232)) ;
#42605 = CARTESIAN_POINT('Ctrl Pts',(-19.0644433009267,-12.064980239876,124.61331053608)) ;
#42606 = CARTESIAN_POINT('Ctrl Pts',(-19.0646348651881,-12.0649893500009,
124.613365498421)) ;
#42607 = CARTESIAN_POINT('Ctrl Pts',(-19.0650058714959,-12.0650069933203,
124.613471849052)) ;
#42608 = CARTESIAN_POINT('Ctrl Pts',(-19.0651853119072,-12.0650155264649,
124.613523242963)) ;
#42609 = CARTESIAN_POINT('Ctrl Pts',(-19.0655330645158,-12.0650320631757,
124.613622759254)) ;
#42610 = CARTESIAN_POINT('Ctrl Pts',(-19.065701375233,-12.0650400666954,124.613670886447)) ;
#42611 = CARTESIAN_POINT('Ctrl Pts',(-19.0660277823305,-12.0650555876845,
124.61376414595)) ;
#42612 = CARTESIAN_POINT('Ctrl Pts',(-19.066185877715,-12.065063105127,124.613809282484)) ;
#42613 = CARTESIAN_POINT('Ctrl Pts',(-19.0664926942241,-12.0650776939686,
124.613896813721)) ;
#42614 = CARTESIAN_POINT('Ctrl Pts',(-19.0666414144139,-12.0650847653407,
124.613939212045)) ;
#42615 = CARTESIAN_POINT('Ctrl Pts',(-19.066930251874,-12.0650984987698,124.61402149815)) ;
#42616 = CARTESIAN_POINT('Ctrl Pts',(-19.0670703681084,-12.0651051607926,
124.614061388995)) ;
#42617 = CARTESIAN_POINT('Ctrl Pts',(-19.0673427049197,-12.065118109196,124.614138871338)) ;
#42618 = CARTESIAN_POINT('Ctrl Pts',(-19.0674749246114,-12.0651243955475,
124.614176465489)) ;
#42619 = CARTESIAN_POINT('Ctrl Pts',(-19.0677321165733,-12.0651366234674,
124.614249547273)) ;
#42620 = CARTESIAN_POINT('Ctrl Pts',(-19.0678570882186,-12.0651425650173,
124.614285037246)) ;
#42621 = CARTESIAN_POINT('Ctrl Pts',(-19.0681003787338,-12.0651541316391,
124.614354086924)) ;
#42622 = CARTESIAN_POINT('Ctrl Pts',(-19.0682186969636,-12.0651597566903,
124.614387648632)) ;
#42623 = CARTESIAN_POINT('Ctrl Pts',(-19.0684492260406,-12.0651707162727,
124.614453002893)) ;
#42624 = CARTESIAN_POINT('Ctrl Pts',(-19.0685614362341,-12.0651760507812,
124.614484797161)) ;
#42625 = CARTESIAN_POINT('Ctrl Pts',(-19.068780248515,-12.0651864530393,124.614546763584)) ;
#42626 = CARTESIAN_POINT('Ctrl Pts',(-19.0688868504596,-12.0651915207894,
124.614576937354)) ;
#42627 = CARTESIAN_POINT('Ctrl Pts',(-19.0690949059344,-12.0652014114058,
124.614635797755)) ;
#42628 = CARTESIAN_POINT('Ctrl Pts',(-19.0691963589123,-12.0652062342523,
124.614664485676)) ;
#42629 = CARTESIAN_POINT('Ctrl Pts',(-19.0693945370095,-12.065215655073,124.61472049754)) ;
#42630 = CARTESIAN_POINT('Ctrl Pts',(-19.0694912621768,-12.0652202530551,
124.614747822761)) ;
#42631 = CARTESIAN_POINT('Ctrl Pts',(-19.0696803731708,-12.0652292426324,
124.614801222695)) ;
#42632 = CARTESIAN_POINT('Ctrl Pts',(-19.0697727584279,-12.0652336342055,
124.614827298353)) ;
#42633 = CARTESIAN_POINT('Ctrl Pts',(-19.0699535460676,-12.0652422279242,
124.614878303023)) ;
#42634 = CARTESIAN_POINT('Ctrl Pts',(-19.0700419482321,-12.0652464300637,
124.614903232943)) ;
#42635 = CARTESIAN_POINT('Ctrl Pts',(-19.0702150979003,-12.0652546605296,
124.614952041547)) ;
#42636 = CARTESIAN_POINT('Ctrl Pts',(-19.0702998455832,-12.0652586888682,
124.614975921134)) ;
#42637 = CARTESIAN_POINT('Ctrl Pts',(-19.0704659909973,-12.0652665862273,
124.615022717435)) ;
#42638 = CARTESIAN_POINT('Ctrl Pts',(-19.0705473882328,-12.0652704552275,
124.61504563476)) ;
#42639 = CARTESIAN_POINT('Ctrl Pts',(-19.0707071138598,-12.0652780472812,
124.615090587886)) ;
#42640 = CARTESIAN_POINT('Ctrl Pts',(-19.0707854418161,-12.065281770317,124.615112624226)) ;
#42641 = CARTESIAN_POINT('Ctrl Pts',(-19.0709392895052,-12.0652890828384,
124.615155890645)) ;
#42642 = CARTESIAN_POINT('Ctrl Pts',(-19.0710148090141,-12.0652926723158,
124.615177121244)) ;
#42643 = CARTESIAN_POINT('Ctrl Pts',(-19.0711632813639,-12.0652997292093,
124.6152188458)) ;
#42644 = CARTESIAN_POINT('Ctrl Pts',(-19.0712362345037,-12.0653031966418,
124.615239340354)) ;
#42645 = CARTESIAN_POINT('Ctrl Pts',(-19.0713798009225,-12.0653100202322,
124.615279658047)) ;
#42646 = CARTESIAN_POINT('Ctrl Pts',(-19.0714504139388,-12.0653133763796,
124.615299481564)) ;
#42647 = CARTESIAN_POINT('Ctrl Pts',(-19.0715895118707,-12.0653199874703,
124.615338517959)) ;
#42648 = CARTESIAN_POINT('Ctrl Pts',(-19.0716579964576,-12.0653232423998,
124.615357731144)) ;
#42649 = CARTESIAN_POINT('Ctrl Pts',(-19.0717930352878,-12.065329660459,124.615395603528)) ;
#42650 = CARTESIAN_POINT('Ctrl Pts',(-19.0718595897204,-12.0653328235992,
124.615414263131)) ;
#42651 = CARTESIAN_POINT('Ctrl Pts',(-19.0719909564925,-12.0653390670313,
124.615451082161)) ;
#42652 = CARTESIAN_POINT('Ctrl Pts',(-19.0720557684534,-12.0653421473066,
124.615469241789)) ;
#42653 = CARTESIAN_POINT('Ctrl Pts',(-19.0721838265998,-12.0653482333928,
124.615505111178)) ;
#42654 = CARTESIAN_POINT('Ctrl Pts',(-19.0722470731097,-12.0653512392202,
124.615522821299)) ;
#42655 = CARTESIAN_POINT('Ctrl Pts',(-19.0762301485984,-12.0655405357329,
124.616637813054)) ;
#42656 = CARTESIAN_POINT('Ctrl Pts',(-19.0801553049901,-12.0657269895376,
124.617715944138)) ;
#42657 = CARTESIAN_POINT('Ctrl Pts',(-19.088639114193,-12.0661298023783,124.620001703209)) ;
#42658 = CARTESIAN_POINT('Ctrl Pts',(-19.0931994742278,-12.066346212982,124.621202744347)) ;
#42659 = CARTESIAN_POINT('Ctrl Pts',(-19.1058204566635,-12.0669448117018,
124.624450412063)) ;
#42660 = CARTESIAN_POINT('Ctrl Pts',(-19.1138948552431,-12.0673274084469,
124.626442442691)) ;
#42661 = CARTESIAN_POINT('Ctrl Pts',(-19.1433593517,-12.0687219818445,124.633400433995)) ;
#42662 = CARTESIAN_POINT('Ctrl Pts',(-19.1648594142534,-12.0697368347804,
124.637883103475)) ;
#42663 = CARTESIAN_POINT('Ctrl Pts',(-19.1965346659422,-12.0712225840397,
124.643620936463)) ;
#42664 = CARTESIAN_POINT('Ctrl Pts',(-19.2066251032401,-12.0716943379384,
124.64532109144)) ;
#42665 = CARTESIAN_POINT('Ctrl Pts',(-19.2240995537892,-12.0725084127209,
124.648045181434)) ;
#42666 = CARTESIAN_POINT('Ctrl Pts',(-19.2314739172003,-12.0728511124802,
124.649127305228)) ;
#42667 = CARTESIAN_POINT('Ctrl Pts',(-19.246018295573,-12.0735255157969,124.651128853948)) ;
#42668 = CARTESIAN_POINT('Ctrl Pts',(-19.2531874837964,-12.0738572263652,
124.652052165627)) ;
#42669 = CARTESIAN_POINT('Ctrl Pts',(-19.2652503094854,-12.0744143195046,
124.653499472226)) ;
#42670 = CARTESIAN_POINT('Ctrl Pts',(-19.2701397533147,-12.0746398406192,
124.654056842615)) ;
#42671 = CARTESIAN_POINT('Ctrl Pts',(-19.3003609648911,-12.0760322130973,
124.657321234559)) ;
#42672 = CARTESIAN_POINT('Ctrl Pts',(-19.3257672984041,-12.0771958162629,
124.659282182534)) ;
#42673 = CARTESIAN_POINT('Ctrl Pts',(-19.3569476665447,-12.0786231564571,
124.660731923813)) ;
#42674 = CARTESIAN_POINT('Ctrl Pts',(-19.3626812935453,-12.0788856044457,
124.660958957615)) ;
#42675 = CARTESIAN_POINT('Ctrl Pts',(-19.3705669119841,-12.0792466520045,
124.661216835009)) ;
#42676 = CARTESIAN_POINT('Ctrl Pts',(-19.3727177257002,-12.0793451380621,
124.661281612246)) ;
#42677 = CARTESIAN_POINT('Ctrl Pts',(-19.3760108183361,-12.0794959517665,
124.661372281832)) ;
#42678 = CARTESIAN_POINT('Ctrl Pts',(-19.3771529839349,-12.0795482636559,
124.661402162263)) ;
#42679 = CARTESIAN_POINT('Ctrl Pts',(-19.3794827977797,-12.0796549805596,
124.661459916603)) ;
#42680 = CARTESIAN_POINT('Ctrl Pts',(-19.3806704480149,-12.0797093860621,
124.661487663504)) ;
#42681 = CARTESIAN_POINT('Ctrl Pts',(-19.3872243507252,-12.0800096500864,
124.66163143356)) ;
#42682 = CARTESIAN_POINT('Ctrl Pts',(-19.3925912598122,-12.0802556576475,
124.6617145846)) ;
#42683 = CARTESIAN_POINT('Ctrl Pts',(-19.4033303867848,-12.0807483282119,
124.661811788053)) ;
#42684 = CARTESIAN_POINT('Ctrl Pts',(-19.4087024912663,-12.0809949863761,
124.661825780289)) ;
#42685 = CARTESIAN_POINT('Ctrl Pts',(-19.4355377146454,-12.0822285714519,
124.661722683523)) ;
#42686 = CARTESIAN_POINT('Ctrl Pts',(-19.4569951615066,-12.0832196122376,
124.661087432713)) ;
#42687 = CARTESIAN_POINT('Ctrl Pts',(-19.4878060683474,-12.0846422148189,
124.659380277275)) ;
#42688 = CARTESIAN_POINT('Ctrl Pts',(-19.4971804512169,-12.0850750365897,
124.658754786505)) ;
#42689 = CARTESIAN_POINT('Ctrl Pts',(-19.5121411979591,-12.0857654490284,
124.657587003704)) ;
#42690 = CARTESIAN_POINT('Ctrl Pts',(-19.5177324896768,-12.0860234049652,
124.657112668334)) ;
#42691 = CARTESIAN_POINT('Ctrl Pts',(-19.5278088525537,-12.0864881156827,
124.656189465094)) ;
#42692 = CARTESIAN_POINT('Ctrl Pts',(-19.5322950464282,-12.0866949551186,
124.65575395656)) ;
#42693 = CARTESIAN_POINT('Ctrl Pts',(-19.5405634575249,-12.0870760643871,
124.654906112773)) ;
#42694 = CARTESIAN_POINT('Ctrl Pts',(-19.5443463344156,-12.0872503822523,
124.654500755951)) ;
#42695 = CARTESIAN_POINT('Ctrl Pts',(-19.5536894535107,-12.0876808202606,
124.653456421)) ;
#42696 = CARTESIAN_POINT('Ctrl Pts',(-19.5592473726583,-12.0879367854468,
124.652797357071)) ;
#42697 = CARTESIAN_POINT('Ctrl Pts',(-19.575734040739,-12.0886958706214,124.650729975241)) ;
#42698 = CARTESIAN_POINT('Ctrl Pts',(-19.5866488193571,-12.0891981431688,
124.649214450418)) ;
#42699 = CARTESIAN_POINT('Ctrl Pts',(-19.6260165305145,-12.0910101146941,
124.643216623814)) ;
#42700 = CARTESIAN_POINT('Ctrl Pts',(-19.6543322905931,-12.0923132982599,
124.637895593769)) ;
#42701 = CARTESIAN_POINT('Ctrl Pts',(-19.6913845279926,-12.0940384591645,
124.629597882083)) ;
#42702 = CARTESIAN_POINT('Ctrl Pts',(-19.700307724554,-12.0944554785715,124.627496224327)) ;
#42703 = CARTESIAN_POINT('Ctrl Pts',(-19.7142309322125,-12.0951091842482,
124.624054844294)) ;
#42704 = CARTESIAN_POINT('Ctrl Pts',(-19.7192471231918,-12.0953453120366,
124.622781893504)) ;
#42705 = CARTESIAN_POINT('Ctrl Pts',(-19.7274820049232,-12.0957340472592,
124.620637621175)) ;
#42706 = CARTESIAN_POINT('Ctrl Pts',(-19.7307053761778,-12.0958864857901,
124.619784504543)) ;
#42707 = CARTESIAN_POINT('Ctrl Pts',(-19.7339524604594,-12.0960403357193,
124.618911194777)) ;
#42708 = CARTESIAN_POINT('Ctrl Pts',(-19.7339796304271,-12.0960416230786,
124.618903886377)) ;
#42709 = CARTESIAN_POINT('Ctrl Pts',(-19.7340336567299,-12.0960441829775,
124.618889351983)) ;
#42710 = CARTESIAN_POINT('Ctrl Pts',(-19.7340605132027,-12.0960454555231,
124.618882125976)) ;
#42711 = CARTESIAN_POINT('Ctrl Pts',(-19.7341139201516,-12.0960479861552,
124.618867754381)) ;
#42712 = CARTESIAN_POINT('Ctrl Pts',(-19.7341404706024,-12.0960492442399,
124.618860608822)) ;
#42713 = CARTESIAN_POINT('Ctrl Pts',(-19.7341932732528,-12.0960517463157,
124.618846396104)) ;
#42714 = CARTESIAN_POINT('Ctrl Pts',(-19.7342195251464,-12.0960529902919,
124.618839329049)) ;
#42715 = CARTESIAN_POINT('Ctrl Pts',(-19.7342717382947,-12.0960554645101,
124.618825271352)) ;
#42716 = CARTESIAN_POINT('Ctrl Pts',(-19.734297699264,-12.0960566947381,124.618818280807)) ;
#42717 = CARTESIAN_POINT('Ctrl Pts',(-19.7343493355344,-12.0960591416944,
124.618804374854)) ;
#42718 = CARTESIAN_POINT('Ctrl Pts',(-19.7343750118,-12.0960603584679,124.618797459205)) ;
#42719 = CARTESIAN_POINT('Ctrl Pts',(-19.734426088005,-12.0960627789565,124.618783700584)) ;
#42720 = CARTESIAN_POINT('Ctrl Pts',(-19.7344514874982,-12.09606398265,124.618776857751)) ;
#42721 = CARTESIAN_POINT('Ctrl Pts',(-19.7345020142175,-12.09606637717,124.618763243726)) ;
#42722 = CARTESIAN_POINT('Ctrl Pts',(-19.7345271425784,-12.0960675680498,
124.618756472247)) ;
#42723 = CARTESIAN_POINT('Ctrl Pts',(-19.7345771369075,-12.0960699374091,
124.618742998321)) ;
#42724 = CARTESIAN_POINT('Ctrl Pts',(-19.7346020019772,-12.0960711158457,
124.618736296135)) ;
#42725 = CARTESIAN_POINT('Ctrl Pts',(-19.7346514742387,-12.0960734605313,
124.618722959631)) ;
#42726 = CARTESIAN_POINT('Ctrl Pts',(-19.7346760819729,-12.0960746268057,
124.618716325184)) ;
#42727 = CARTESIAN_POINT('Ctrl Pts',(-19.7347250463702,-12.0960769474887,
124.618703122376)) ;
#42728 = CARTESIAN_POINT('Ctrl Pts',(-19.7347494031223,-12.0960781019012,
124.618696554006)) ;
#42729 = CARTESIAN_POINT('Ctrl Pts',(-19.7347978734309,-12.0960803992325,
124.618683481276)) ;
#42730 = CARTESIAN_POINT('Ctrl Pts',(-19.7348219863018,-12.0960815421184,
124.618676977116)) ;
#42731 = CARTESIAN_POINT('Ctrl Pts',(-19.7348699724547,-12.0960838165668,
124.61866403188)) ;
#42732 = CARTESIAN_POINT('Ctrl Pts',(-19.7348938465724,-12.0960849481685,
124.618657590593)) ;
#42733 = CARTESIAN_POINT('Ctrl Pts',(-19.7349413640165,-12.0960872004641,
124.618644768776)) ;
#42734 = CARTESIAN_POINT('Ctrl Pts',(-19.7349650063444,-12.0960883211106,
124.618638388529)) ;
#42735 = CARTESIAN_POINT('Ctrl Pts',(-19.7350120654982,-12.0960905517456,
124.618625687406)) ;
#42736 = CARTESIAN_POINT('Ctrl Pts',(-19.7350354820297,-12.09609166172,124.618619366624)) ;
#42737 = CARTESIAN_POINT('Ctrl Pts',(-19.7350820945787,-12.0960938712465,
124.618606783128)) ;
#42738 = CARTESIAN_POINT('Ctrl Pts',(-19.7351052909254,-12.096094970814,124.618600520338)) ;
#42739 = CARTESIAN_POINT('Ctrl Pts',(-19.7351514696571,-12.0960971598365,
124.618588051098)) ;
#42740 = CARTESIAN_POINT('Ctrl Pts',(-19.7351744520568,-12.0960982492919,
124.618581844657)) ;
#42741 = CARTESIAN_POINT('Ctrl Pts',(-19.7352202067037,-12.0961004182701,
124.618569487123)) ;
#42742 = CARTESIAN_POINT('Ctrl Pts',(-19.7352429798793,-12.0961014978365,
124.618563335794)) ;
#42743 = CARTESIAN_POINT('Ctrl Pts',(-19.7352883253059,-12.0961036474734,
124.618551086029)) ;
#42744 = CARTESIAN_POINT('Ctrl Pts',(-19.7353108963806,-12.0961047174877,
124.618544987925)) ;
#42745 = CARTESIAN_POINT('Ctrl Pts',(-19.7353558390246,-12.096106848087,124.618532844263)) ;
#42746 = CARTESIAN_POINT('Ctrl Pts',(-19.7353782117894,-12.0961079087283,
124.618526798396)) ;
#42747 = CARTESIAN_POINT('Ctrl Pts',(-19.7354227680478,-12.0961100210658,
124.618514756478)) ;
#42748 = CARTESIAN_POINT('Ctrl Pts',(-19.7354449497628,-12.0961110726774,
124.61850876092)) ;
#42749 = CARTESIAN_POINT('Ctrl Pts',(-19.7354891260055,-12.0961131670537,
124.618496819092)) ;
#42750 = CARTESIAN_POINT('Ctrl Pts',(-19.7355111212321,-12.0961142098513,
124.618490872645)) ;
#42751 = CARTESIAN_POINT('Ctrl Pts',(-19.7355549297109,-12.0961162868459,
124.618479027661)) ;
#42752 = CARTESIAN_POINT('Ctrl Pts',(-19.7355767436234,-12.096117321074,124.618473128958)) ;
#42753 = CARTESIAN_POINT('Ctrl Pts',(-19.7356201949731,-12.0961193811898,
124.618461378006)) ;
#42754 = CARTESIAN_POINT('Ctrl Pts',(-19.7356418326082,-12.0961204070867,
124.618455525715)) ;
#42755 = CARTESIAN_POINT('Ctrl Pts',(-19.7356849384307,-12.0961224508725,
124.61844386572)) ;
#42756 = CARTESIAN_POINT('Ctrl Pts',(-19.7357064057764,-12.0961234687213,
124.618438058252)) ;
#42757 = CARTESIAN_POINT('Ctrl Pts',(-19.735749173782,-12.0961254965414,124.618426487185)) ;
#42758 = CARTESIAN_POINT('Ctrl Pts',(-19.7357704750478,-12.0961265065413,
124.618420723431)) ;
#42759 = CARTESIAN_POINT('Ctrl Pts',(-19.7358129177099,-12.096128518986,124.618409237974)) ;
#42760 = CARTESIAN_POINT('Ctrl Pts',(-19.7358340584645,-12.0961295214003,
124.618403516455)) ;
#42761 = CARTESIAN_POINT('Ctrl Pts',(-19.7358761852192,-12.0961315189159,
124.61839211411)) ;
#42762 = CARTESIAN_POINT('Ctrl Pts',(-19.7358971709611,-12.0961325140047,
124.618386433363)) ;
#42763 = CARTESIAN_POINT('Ctrl Pts',(-19.7359389890441,-12.0961344969332,
124.618375112224)) ;
#42764 = CARTESIAN_POINT('Ctrl Pts',(-19.7359598231085,-12.0961354848543,
124.618369471373)) ;
#42765 = CARTESIAN_POINT('Ctrl Pts',(-19.7360013467242,-12.0961374538682,
124.618358227644)) ;
#42766 = CARTESIAN_POINT('Ctrl Pts',(-19.7360220352338,-12.0961384349113,
124.618352625056)) ;
#42767 = CARTESIAN_POINT('Ctrl Pts',(-19.7360632710443,-12.0961403903255,
124.618341456982)) ;
#42768 = CARTESIAN_POINT('Ctrl Pts',(-19.7360838183628,-12.0961413646971,
124.618335891499)) ;
#42769 = CARTESIAN_POINT('Ctrl Pts',(-19.7361247769421,-12.096143307012,124.618324796263)) ;
#42770 = CARTESIAN_POINT('Ctrl Pts',(-19.7361451879543,-12.0961442749433,
124.618319266585)) ;
#42771 = CARTESIAN_POINT('Ctrl Pts',(-19.7361858788676,-12.0961462046116,
124.618308241639)) ;
#42772 = CARTESIAN_POINT('Ctrl Pts',(-19.7362061586647,-12.0961471663435,
124.618302746408)) ;
#42773 = CARTESIAN_POINT('Ctrl Pts',(-19.7362465895581,-12.0961490837269,
124.618291789725)) ;
#42774 = CARTESIAN_POINT('Ctrl Pts',(-19.7362667418648,-12.0961500394356,
124.618286327952)) ;
#42775 = CARTESIAN_POINT('Ctrl Pts',(-19.7363069243786,-12.0961519450853,
124.618275436418)) ;
#42776 = CARTESIAN_POINT('Ctrl Pts',(-19.7363269542645,-12.0961528950109,
124.61827000675)) ;
#42777 = CARTESIAN_POINT('Ctrl Pts',(-19.7363668968152,-12.0961547893252,
124.618259178123)) ;
#42778 = CARTESIAN_POINT('Ctrl Pts',(-19.7363868090088,-12.0961557336915,
124.618253779297)) ;
#42779 = CARTESIAN_POINT('Ctrl Pts',(-19.7364265203621,-12.0961576170853,
124.618243011238)) ;
#42780 = CARTESIAN_POINT('Ctrl Pts',(-19.7364463193167,-12.0961585561031,
124.618237642066)) ;
#42781 = CARTESIAN_POINT('Ctrl Pts',(-19.7364858091557,-12.0961604290351,
124.618226931985)) ;
#42782 = CARTESIAN_POINT('Ctrl Pts',(-19.7365054998218,-12.0961613629388,
124.618221591141)) ;
#42783 = CARTESIAN_POINT('Ctrl Pts',(-19.7365447752037,-12.0961632257428,
124.618210937158)) ;
#42784 = CARTESIAN_POINT('Ctrl Pts',(-19.7365643610092,-12.0961641546947,
124.618205623729)) ;
#42785 = CARTESIAN_POINT('Ctrl Pts',(-19.7366034337662,-12.0961660079312,
124.618195022668)) ;
#42786 = CARTESIAN_POINT('Ctrl Pts',(-19.7366229198876,-12.0961669321765,
124.618189735266)) ;
#42787 = CARTESIAN_POINT('Ctrl Pts',(-19.7366617980166,-12.0961687762243,
124.618179184988)) ;
#42788 = CARTESIAN_POINT('Ctrl Pts',(-19.7366811894335,-12.0961696959988,
124.618173922277)) ;
#42789 = CARTESIAN_POINT('Ctrl Pts',(-19.7367198795494,-12.0961715311709,
124.618163421017)) ;
#42790 = CARTESIAN_POINT('Ctrl Pts',(-19.7367391795114,-12.0961724466285,
124.618158182129)) ;
#42791 = CARTESIAN_POINT('Ctrl Pts',(-19.7367776930937,-12.0961742734689,
124.618147726799)) ;
#42792 = CARTESIAN_POINT('Ctrl Pts',(-19.7367969062961,-12.096175184832,124.618142510474)) ;
#42793 = CARTESIAN_POINT('Ctrl Pts',(-19.7368352525188,-12.0961770037753,
124.61813209861)) ;
#42794 = CARTESIAN_POINT('Ctrl Pts',(-19.7368543842842,-12.0961779112961,
124.618126903415)) ;
#42795 = CARTESIAN_POINT('Ctrl Pts',(-19.7368925691138,-12.0961797226248,
124.618116533422)) ;
#42796 = CARTESIAN_POINT('Ctrl Pts',(-19.736911622872,-12.0961806264657,124.618111358439)) ;
#42797 = CARTESIAN_POINT('Ctrl Pts',(-19.7369496578063,-12.0961824307248,
124.618101027218)) ;
#42798 = CARTESIAN_POINT('Ctrl Pts',(-19.736968638743,-12.0961833311315,124.618095871049)) ;
#42799 = CARTESIAN_POINT('Ctrl Pts',(-19.7370065299704,-12.096185128614,124.618085576941)) ;
#42800 = CARTESIAN_POINT('Ctrl Pts',(-19.7370254414852,-12.0961860257477,
124.618080438674)) ;
#42801 = CARTESIAN_POINT('Ctrl Pts',(-19.7370632004219,-12.0961878169947,
124.6180701786)) ;
#42802 = CARTESIAN_POINT('Ctrl Pts',(-19.7370820475637,-12.0961887110947,
124.618065056872)) ;
#42803 = CARTESIAN_POINT('Ctrl Pts',(-19.7371196814388,-12.0961904964487,
124.618054828886)) ;
#42804 = CARTESIAN_POINT('Ctrl Pts',(-19.7371384683679,-12.0961913877121,
124.618049722578)) ;
#42805 = CARTESIAN_POINT('Ctrl Pts',(-19.7371759864669,-12.0961931676134,
124.618039524174)) ;
#42806 = CARTESIAN_POINT('Ctrl Pts',(-19.7371947176093,-12.0961940562499,
124.61803443209)) ;
#42807 = CARTESIAN_POINT('Ctrl Pts',(-19.7405997366698,-12.0963555978143,
124.61710868825)) ;
#42808 = CARTESIAN_POINT('Ctrl Pts',(-19.7439821260536,-12.0965163884945,
124.616173783017)) ;
#42809 = CARTESIAN_POINT('Ctrl Pts',(-19.7507141210482,-12.0968370742468,
124.614282483996)) ;
#42810 = CARTESIAN_POINT('Ctrl Pts',(-19.7540637548073,-12.0969969657835,
124.613326306902)) ;
#42811 = CARTESIAN_POINT('Ctrl Pts',(-19.7632557265596,-12.0974366574562,
124.610660788293)) ;
#42812 = CARTESIAN_POINT('Ctrl Pts',(-19.7690896284843,-12.0977167451546,
124.608922756839)) ;
#42813 = CARTESIAN_POINT('Ctrl Pts',(-19.7976899585334,-12.09909500957,124.600174213327)) ;
#42814 = CARTESIAN_POINT('Ctrl Pts',(-19.820265196321,-12.1001994120349,124.59255657963)) ;
#42815 = CARTESIAN_POINT('Ctrl Pts',(-19.8693189595106,-12.102631156938,124.574426899797)) ;
#42816 = CARTESIAN_POINT('Ctrl Pts',(-19.8956853775682,-12.1039568944303,
124.563644756999)) ;
#42817 = CARTESIAN_POINT('Ctrl Pts',(-19.9260897669721,-12.1054933812914,
124.549980969834)) ;
#42818 = CARTESIAN_POINT('Ctrl Pts',(-19.9305070847157,-12.1057168492066,
124.547964801112)) ;
#42819 = CARTESIAN_POINT('Ctrl Pts',(-19.9375200061838,-12.1060719953755,
124.544714429497)) ;
#42820 = CARTESIAN_POINT('Ctrl Pts',(-19.940123282688,-12.1062039114271,124.543496930535)) ;
#42821 = CARTESIAN_POINT('Ctrl Pts',(-19.9448507101916,-12.1064436155215,
124.541266108199)) ;
#42822 = CARTESIAN_POINT('Ctrl Pts',(-19.9469762401277,-12.106551446171,124.540255744165)) ;
#42823 = CARTESIAN_POINT('Ctrl Pts',(-19.9515370033646,-12.1067829421594,
124.538071987723)) ;
#42824 = CARTESIAN_POINT('Ctrl Pts',(-19.9539713101389,-12.1069065787527,
124.536896686145)) ;
#42825 = CARTESIAN_POINT('Ctrl Pts',(-19.9593114539544,-12.1071779750773,
124.534297030684)) ;
#42826 = CARTESIAN_POINT('Ctrl Pts',(-19.9622156120695,-12.1073256838582,
124.532869269544)) ;
#42827 = CARTESIAN_POINT('Ctrl Pts',(-19.9697149510113,-12.1077074274355,
124.529146164705)) ;
#42828 = CARTESIAN_POINT('Ctrl Pts',(-19.9743015930968,-12.1079412141059,
124.526833743045)) ;
#42829 = CARTESIAN_POINT('Ctrl Pts',(-19.9881406320803,-12.1086477046893,
124.519749273)) ;
#42830 = CARTESIAN_POINT('Ctrl Pts',(-19.9973478087975,-12.1091192102228,
124.514889839884)) ;
#42831 = CARTESIAN_POINT('Ctrl Pts',(-20.0215044949151,-12.1103619976979,
124.501751819312)) ;
#42832 = CARTESIAN_POINT('Ctrl Pts',(-20.036346753028,-12.1111313842965,124.493280751154)) ;
#42833 = CARTESIAN_POINT('Ctrl Pts',(-20.0704202612595,-12.1129222911441,
124.472896292557)) ;
#42834 = CARTESIAN_POINT('Ctrl Pts',(-20.0895109091983,-12.1139449510268,
124.460759978135)) ;
#42835 = CARTESIAN_POINT('Ctrl Pts',(-20.1122599797971,-12.1151956220572,
124.445415591473)) ;
#42836 = CARTESIAN_POINT('Ctrl Pts',(-20.1162426664637,-12.1154157779529,
124.442695577085)) ;
#42837 = CARTESIAN_POINT('Ctrl Pts',(-20.1223874124323,-12.1157573627394,
124.438446606678)) ;
#42838 = CARTESIAN_POINT('Ctrl Pts',(-20.1245605299186,-12.1158785394931,
124.436933709777)) ;
#42839 = CARTESIAN_POINT('Ctrl Pts',(-20.128885892467,-12.1161204830641,124.433901997012)) ;
#42840 = CARTESIAN_POINT('Ctrl Pts',(-20.1310381760492,-12.1162412481258,
124.432383260182)) ;
#42841 = CARTESIAN_POINT('Ctrl Pts',(-20.1356334093656,-12.1164998962648,
124.429118874098)) ;
#42842 = CARTESIAN_POINT('Ctrl Pts',(-20.1380749010505,-12.1166378106526,
124.427371204245)) ;
#42843 = CARTESIAN_POINT('Ctrl Pts',(-20.1454431368342,-12.1170555231082,
124.422056614904)) ;
#42844 = CARTESIAN_POINT('Ctrl Pts',(-20.1503501471911,-12.1173357443812,
124.418462529776)) ;
#42845 = CARTESIAN_POINT('Ctrl Pts',(-20.1616290016971,-12.1179845456639,
124.410074291885)) ;
#42846 = CARTESIAN_POINT('Ctrl Pts',(-20.1679815775983,-12.1183534923118,
124.405254709584)) ;
#42847 = CARTESIAN_POINT('Ctrl Pts',(-20.1911329294585,-12.1197107080698,
124.387338616034)) ;
#42848 = CARTESIAN_POINT('Ctrl Pts',(-20.2076422078547,-12.1207035885708,
124.373874177019)) ;
#42849 = CARTESIAN_POINT('Ctrl Pts',(-20.226468669525,-12.1218594738387,124.357701449505)) ;
#42850 = CARTESIAN_POINT('Ctrl Pts',(-20.2291284303065,-12.1220233308964,
124.35539701018)) ;
#42851 = CARTESIAN_POINT('Ctrl Pts',(-20.2351020664319,-12.1223925389384,
124.350177075046)) ;
#42852 = CARTESIAN_POINT('Ctrl Pts',(-20.2384103054665,-12.122597846561,124.347255194933)) ;
#42853 = CARTESIAN_POINT('Ctrl Pts',(-20.2538281340221,-12.1235584006917,
124.333491919365)) ;
#42854 = CARTESIAN_POINT('Ctrl Pts',(-20.2657410907948,-12.1243113136328,
124.322432446614)) ;
#42855 = CARTESIAN_POINT('Ctrl Pts',(-20.2807229564756,-12.1252707928341,
124.307969780083)) ;
#42856 = CARTESIAN_POINT('Ctrl Pts',(-20.2839933661764,-12.1254810421141,
124.304777875385)) ;
#42857 = CARTESIAN_POINT('Ctrl Pts',(-20.2890828848724,-12.1258095053345,
124.299755738583)) ;
#42858 = CARTESIAN_POINT('Ctrl Pts',(-20.2909139468366,-12.1259279365625,
124.297937694196)) ;
#42859 = CARTESIAN_POINT('Ctrl Pts',(-20.294493721387,-12.1261599871198,124.294361289684)) ;
#42860 = CARTESIAN_POINT('Ctrl Pts',(-20.2962428562168,-12.1262736137381,
124.292603370023)) ;
#42861 = CARTESIAN_POINT('Ctrl Pts',(-20.3002646019119,-12.1265354409871,
124.288537296624)) ;
#42862 = CARTESIAN_POINT('Ctrl Pts',(-20.3025334969575,-12.1266835740991,
124.286225489534)) ;
#42863 = CARTESIAN_POINT('Ctrl Pts',(-20.3072886687628,-12.1269949406869,
124.281342559565)) ;
#42864 = CARTESIAN_POINT('Ctrl Pts',(-20.3097729484632,-12.1271581382706,
124.27876953202)) ;
#42865 = CARTESIAN_POINT('Ctrl Pts',(-20.3163458878405,-12.1275913780223,
124.271903048324)) ;
#42866 = CARTESIAN_POINT('Ctrl Pts',(-20.3204151091899,-12.1278610948475,
124.267591098832)) ;
#42867 = CARTESIAN_POINT('Ctrl Pts',(-20.3333135961762,-12.1287211710195,
124.253726928046)) ;
#42868 = CARTESIAN_POINT('Ctrl Pts',(-20.3420245192357,-12.1293097712817,
124.244065757561)) ;
#42869 = CARTESIAN_POINT('Ctrl Pts',(-20.3780491128386,-12.1317834919378,
124.202835171555)) ;
#42870 = CARTESIAN_POINT('Ctrl Pts',(-20.4039229951881,-12.133665496402,124.170044161355)) ;
#42871 = CARTESIAN_POINT('Ctrl Pts',(-20.4326409014067,-12.1359244306395,
124.129642890673)) ;
#42872 = CARTESIAN_POINT('Ctrl Pts',(-20.4371138748614,-12.1362815412584,
124.123223376887)) ;
#42873 = CARTESIAN_POINT('Ctrl Pts',(-20.4441998734258,-12.1368559876269,
124.112847361706)) ;
#42874 = CARTESIAN_POINT('Ctrl Pts',(-20.4468511773194,-12.1370729431233,
124.108917239409)) ;
#42875 = CARTESIAN_POINT('Ctrl Pts',(-20.4517921004877,-12.1374811144328,
124.101502496155)) ;
#42876 = CARTESIAN_POINT('Ctrl Pts',(-20.4540867686813,-12.1376722784924,
124.098021315029)) ;
#42877 = CARTESIAN_POINT('Ctrl Pts',(-20.4590218714978,-12.1380869241402,
124.09045225585)) ;
#42878 = CARTESIAN_POINT('Ctrl Pts',(-20.4616559365253,-12.1383104623465,
124.08636030916)) ;
#42879 = CARTESIAN_POINT('Ctrl Pts',(-20.4697727866498,-12.1390063025262,
124.073587737718)) ;
#42880 = CARTESIAN_POINT('Ctrl Pts',(-20.4751725450949,-12.1394793418457,
124.064854902847)) ;
#42881 = CARTESIAN_POINT('Ctrl Pts',(-20.4878462015155,-12.140614400604,124.043782211095)) ;
#42882 = CARTESIAN_POINT('Ctrl Pts',(-20.4950167610676,-12.141277231621,124.031381939984)) ;
#42883 = CARTESIAN_POINT('Ctrl Pts',(-20.5231955639474,-12.1439664058702,
123.980659351967)) ;
#42884 = CARTESIAN_POINT('Ctrl Pts',(-20.5424007538072,-12.145996522205,123.941370420517)) ;
#42885 = CARTESIAN_POINT('Ctrl Pts',(-20.564422676239,-12.1485928190175,123.889606177248)) ;
#42886 = CARTESIAN_POINT('Ctrl Pts',(-20.5691622386565,-12.1491710437647,
123.877982510394)) ;
#42887 = CARTESIAN_POINT('Ctrl Pts',(-20.5760254615005,-12.1500388375457,
123.86039759376)) ;
#42888 = CARTESIAN_POINT('Ctrl Pts',(-20.5782802270883,-12.1503292795052,
123.854488420545)) ;
#42889 = CARTESIAN_POINT('Ctrl Pts',(-20.5819280882339,-12.1508082164861,
123.844706029162)) ;
#42890 = CARTESIAN_POINT('Ctrl Pts',(-20.5833470702858,-12.1509968864711,
123.840842597478)) ;
#42891 = CARTESIAN_POINT('Ctrl Pts',(-20.5859593480778,-12.1513487156225,
123.83362018246)) ;
#42892 = CARTESIAN_POINT('Ctrl Pts',(-20.5871574063013,-12.1515119057973,
123.830262967591)) ;
#42893 = CARTESIAN_POINT('Ctrl Pts',(-20.590848318402,-12.1520204575482,123.819778787641)) ;
#42894 = CARTESIAN_POINT('Ctrl Pts',(-20.5932909752033,-12.1523654705896,
123.812634317626)) ;
#42895 = CARTESIAN_POINT('Ctrl Pts',(-20.5984366744584,-12.1531112297016,
123.797126172777)) ;
#42896 = CARTESIAN_POINT('Ctrl Pts',(-20.6011165377074,-12.1535118105786,
123.788755225348)) ;
#42897 = CARTESIAN_POINT('Ctrl Pts',(-20.608761404753,-12.1546921825679,123.763978418761)) ;
#42898 = CARTESIAN_POINT('Ctrl Pts',(-20.6134775192506,-12.1554704922135,
123.74749788668)) ;
#42899 = CARTESIAN_POINT('Ctrl Pts',(-20.624572344293,-12.1574417129196,123.705478063161)) ;
#42900 = CARTESIAN_POINT('Ctrl Pts',(-20.6304860336949,-12.1586328222597,
123.679824771)) ;
#42901 = CARTESIAN_POINT('Ctrl Pts',(-20.6358819592532,-12.1598967441597,
123.652502812988)) ;
#42902 = CARTESIAN_POINT('Ctrl Pts',(-20.6361756779736,-12.1599662005072,
123.651001083359)) ;
#42903 = CARTESIAN_POINT('Ctrl Pts',(-20.6397192990144,-12.1608122642352,
123.632704926981)) ;
#42904 = CARTESIAN_POINT('Ctrl Pts',(-20.6426268591874,-12.1615906171343,
123.615846181314)) ;
#42905 = CARTESIAN_POINT('Ctrl Pts',(-20.6463000445998,-12.1627107943247,
123.591584874177)) ;
#42906 = CARTESIAN_POINT('Ctrl Pts',(-20.6473470189309,-12.1630504902502,
123.584226854407)) ;
#42907 = CARTESIAN_POINT('Ctrl Pts',(-20.6490766126,-12.1636499543836,123.571242178131)) ;
#42908 = CARTESIAN_POINT('Ctrl Pts',(-20.6497866997148,-12.1639095431914,
123.565619387327)) ;
#42909 = CARTESIAN_POINT('Ctrl Pts',(-20.651100729922,-12.1644177267814,123.554612621106)) ;
#42910 = CARTESIAN_POINT('Ctrl Pts',(-20.6517079583086,-12.1646662964126,
123.549229160334)) ;
#42911 = CARTESIAN_POINT('Ctrl Pts',(-20.6529406274532,-12.1652022033277,
123.537623875316)) ;
#42912 = CARTESIAN_POINT('Ctrl Pts',(-20.653554417112,-12.1654895998622,123.531400962233)) ;
#42913 = CARTESIAN_POINT('Ctrl Pts',(-20.6558242437937,-12.1666409855252,
123.506474990045)) ;
#42914 = CARTESIAN_POINT('Ctrl Pts',(-20.6571054691004,-12.1675068697634,
123.487740364236)) ;
#42915 = CARTESIAN_POINT('Ctrl Pts',(-20.659178980782,-12.1696022439032,123.442451062891)) ;
#42916 = CARTESIAN_POINT('Ctrl Pts',(-20.6595477573357,-12.1708338511469,
123.415886147478)) ;
#42917 = CARTESIAN_POINT('Ctrl Pts',(-20.6587145982682,-12.1729824755116,
123.36957490034)) ;
#42918 = CARTESIAN_POINT('Ctrl Pts',(-20.6578908525933,-12.1738977522582,
123.349830879059)) ;
#42919 = CARTESIAN_POINT('Ctrl Pts',(-20.6562081118598,-12.1750843629603,
123.32414015327)) ;
#42920 = CARTESIAN_POINT('Ctrl Pts',(-20.655773871485,-12.1753598923354,123.318168654451)) ;
#42921 = CARTESIAN_POINT('Ctrl Pts',(-20.6550167088993,-12.175796418416,123.308697653849)) ;
#42922 = CARTESIAN_POINT('Ctrl Pts',(-20.6547219037851,-12.1759577096709,
123.305196013)) ;
#42923 = CARTESIAN_POINT('Ctrl Pts',(-20.6541429130458,-12.1762590772131,
123.298649218436)) ;
#42924 = CARTESIAN_POINT('Ctrl Pts',(-20.6538623099325,-12.1763991912635,
123.295603776444)) ;
#42925 = CARTESIAN_POINT('Ctrl Pts',(-20.6532787278679,-12.1766791884981,
123.289514721006)) ;
#42926 = CARTESIAN_POINT('Ctrl Pts',(-20.6529757488871,-12.1768190706846,
123.286471128958)) ;
#42927 = CARTESIAN_POINT('Ctrl Pts',(-20.6520888008697,-12.1772136655272,
123.277881217506)) ;
#42928 = CARTESIAN_POINT('Ctrl Pts',(-20.6514788797325,-12.1774680913652,
123.272337640915)) ;
#42929 = CARTESIAN_POINT('Ctrl Pts',(-20.6498835175878,-12.1780945119676,
123.258678896268)) ;
#42930 = CARTESIAN_POINT('Ctrl Pts',(-20.648855529304,-12.1784660504912,123.250568950122)) ;
#42931 = CARTESIAN_POINT('Ctrl Pts',(-20.6477480580335,-12.1788369205275,
123.242469634735)) ;
#42932 = CARTESIAN_POINT('',(-20.6521256561948,-12.1170419242982,123.278341262904)) ;
#42933 = CARTESIAN_POINT('Ctrl Pts',(-20.652125778092,-12.1170429607118,123.278341249912)) ;
#42934 = CARTESIAN_POINT('Ctrl Pts',(-20.6511064564272,-12.1390146862922,
123.268849694058)) ;
#42935 = CARTESIAN_POINT('Ctrl Pts',(-20.6497041626644,-12.1597501137876,
123.256775377451)) ;
#42936 = CARTESIAN_POINT('Ctrl Pts',(-20.6477481882033,-12.178832505456,123.242470586714)) ;
#42937 = CARTESIAN_POINT('',(-18.9628485264954,-11.9999999945477,124.57937843518)) ;
#42938 = CARTESIAN_POINT('Ctrl Pts',(-20.6521257750101,-12.1170412970773,
123.278341221215)) ;
#42939 = CARTESIAN_POINT('Ctrl Pts',(-20.6530685080591,-12.1166364163469,
123.287119609581)) ;
#42940 = CARTESIAN_POINT('Ctrl Pts',(-20.6539182121897,-12.1162318136361,
123.295907752301)) ;
#42941 = CARTESIAN_POINT('Ctrl Pts',(-20.6554930910976,-12.1153901623278,
123.314219343693)) ;
#42942 = CARTESIAN_POINT('Ctrl Pts',(-20.6562023658464,-12.1149531919745,
123.323743599029)) ;
#42943 = CARTESIAN_POINT('Ctrl Pts',(-20.6580408657703,-12.1136154895481,
123.352946609739)) ;
#42944 = CARTESIAN_POINT('Ctrl Pts',(-20.658813852262,-12.1127162276281,123.372644757154)) ;
#42945 = CARTESIAN_POINT('Ctrl Pts',(-20.65955069476,-12.1105596121518,123.419966285538)) ;
#42946 = CARTESIAN_POINT('Ctrl Pts',(-20.6590654399524,-12.1093028384769,
123.447586137842)) ;
#42947 = CARTESIAN_POINT('Ctrl Pts',(-20.6573711131328,-12.1077750330124,
123.480973558669)) ;
#42948 = CARTESIAN_POINT('Ctrl Pts',(-20.6570359486246,-12.10750913202,123.486777812164)) ;
#42949 = CARTESIAN_POINT('Ctrl Pts',(-20.6563183775252,-12.1070007389935,
123.497860435606)) ;
#42950 = CARTESIAN_POINT('Ctrl Pts',(-20.6559429191866,-12.1067582934322,
123.503139130868)) ;
#42951 = CARTESIAN_POINT('Ctrl Pts',(-20.6551380630678,-12.1062807300479,
123.513522691455)) ;
#42952 = CARTESIAN_POINT('Ctrl Pts',(-20.6547107818719,-12.1060456304326,
123.518627617948)) ;
#42953 = CARTESIAN_POINT('Ctrl Pts',(-20.6536312738023,-12.1054917832732,
123.530636384154)) ;
#42954 = CARTESIAN_POINT('Ctrl Pts',(-20.6529529546488,-12.1051728677302,
123.537537699275)) ;
#42955 = CARTESIAN_POINT('Ctrl Pts',(-20.6501177575175,-12.1039423214097,
123.564110090908)) ;
#42956 = CARTESIAN_POINT('Ctrl Pts',(-20.6475513238575,-12.1030278748426,
123.583734369519)) ;
#42957 = CARTESIAN_POINT('Ctrl Pts',(-20.6416060284001,-12.1012290557006,
123.622088791108)) ;
#42958 = CARTESIAN_POINT('Ctrl Pts',(-20.6382631350108,-12.1003459094887,
123.640819360478)) ;
#42959 = CARTESIAN_POINT('Ctrl Pts',(-20.6330494195697,-12.0991289732489,
123.66661344932)) ;
#42960 = CARTESIAN_POINT('Ctrl Pts',(-20.6315422800174,-12.0987922689256,
123.673747770058)) ;
#42961 = CARTESIAN_POINT('Ctrl Pts',(-20.6292059866973,-12.0982919947271,
123.684347548924)) ;
#42962 = CARTESIAN_POINT('Ctrl Pts',(-20.6284243051366,-12.0981279475955,
123.687823286711)) ;
#42963 = CARTESIAN_POINT('Ctrl Pts',(-20.6274174392802,-12.0979207859479,
123.69221256319)) ;
#42964 = CARTESIAN_POINT('Ctrl Pts',(-20.6272060697273,-12.0978775211649,
123.693129246387)) ;
#42965 = CARTESIAN_POINT('Ctrl Pts',(-20.6268298072623,-12.0978009002881,
123.694752676629)) ;
#42966 = CARTESIAN_POINT('Ctrl Pts',(-20.6266653333704,-12.0977675395721,
123.695459520086)) ;
#42967 = CARTESIAN_POINT('Ctrl Pts',(-20.6258378225337,-12.0976003535137,
123.699001854537)) ;
#42968 = CARTESIAN_POINT('Ctrl Pts',(-20.62516549329,-12.0974666328674,123.701835170169)) ;
#42969 = CARTESIAN_POINT('Ctrl Pts',(-20.6237885965282,-12.0971969823739,
123.707548710003)) ;
#42970 = CARTESIAN_POINT('Ctrl Pts',(-20.6230836691423,-12.0970610576193,
123.710428828233)) ;
#42971 = CARTESIAN_POINT('Ctrl Pts',(-20.6216508844303,-12.0967889840116,
123.716193841872)) ;
#42972 = CARTESIAN_POINT('Ctrl Pts',(-20.6209229617056,-12.0966528368838,
123.719078700845)) ;
#42973 = CARTESIAN_POINT('Ctrl Pts',(-20.6188249099563,-12.0962662424827,
123.727270173304)) ;
#42974 = CARTESIAN_POINT('Ctrl Pts',(-20.6174301686541,-12.0960160896464,
123.732570422232)) ;
#42975 = CARTESIAN_POINT('Ctrl Pts',(-20.6081874718496,-12.0944012715098,
123.766778451028)) ;
#42976 = CARTESIAN_POINT('Ctrl Pts',(-20.599337539341,-12.0930500252769,123.795405064408)) ;
#42977 = CARTESIAN_POINT('Ctrl Pts',(-20.584436332981,-12.0910067668295,123.838103604677)) ;
#42978 = CARTESIAN_POINT('Ctrl Pts',(-20.5791412110244,-12.0903160981055,
123.852427288074)) ;
#42979 = CARTESIAN_POINT('Ctrl Pts',(-20.5711241175557,-12.0893156046617,
123.872949862714)) ;
#42980 = CARTESIAN_POINT('Ctrl Pts',(-20.5686121347261,-12.0890079948117,
123.879229320365)) ;
#42981 = CARTESIAN_POINT('Ctrl Pts',(-20.5639925258408,-12.0884524307241,
123.890511048196)) ;
#42982 = CARTESIAN_POINT('Ctrl Pts',(-20.5619030411288,-12.0882046967968,
123.895520566085)) ;
#42983 = CARTESIAN_POINT('Ctrl Pts',(-20.5586835861007,-12.0878282262319,
123.903099851064)) ;
#42984 = CARTESIAN_POINT('Ctrl Pts',(-20.5575774736087,-12.0876997907368,
123.905679692584)) ;
#42985 = CARTESIAN_POINT('Ctrl Pts',(-20.5554046494442,-12.0874492439976,
123.910700714292)) ;
#42986 = CARTESIAN_POINT('Ctrl Pts',(-20.5543388047405,-12.0873271443661,
123.913142253482)) ;
#42987 = CARTESIAN_POINT('Ctrl Pts',(-20.5518769810121,-12.0870469457384,
123.918732763676)) ;
#42988 = CARTESIAN_POINT('Ctrl Pts',(-20.550475776245,-12.0868887811144,123.921879405832)) ;
#42989 = CARTESIAN_POINT('Ctrl Pts',(-20.5465582576679,-12.0864501870359,
123.930579902941)) ;
#42990 = CARTESIAN_POINT('Ctrl Pts',(-20.5440142944134,-12.0861694120203,
123.936121182391)) ;
#42991 = CARTESIAN_POINT('Ctrl Pts',(-20.5281920721199,-12.0844475026756,
123.969930660639)) ;
#42992 = CARTESIAN_POINT('Ctrl Pts',(-20.5138989204612,-12.0829932142455,
123.997711305277)) ;
#42993 = CARTESIAN_POINT('Ctrl Pts',(-20.4917812341337,-12.0808966370568,
124.037007491188)) ;
#42994 = CARTESIAN_POINT('Ctrl Pts',(-20.4847811940601,-12.0802530730777,
124.048974205351)) ;
#42995 = CARTESIAN_POINT('Ctrl Pts',(-20.4743313470192,-12.0793221287414,
124.066175371041)) ;
#42996 = CARTESIAN_POINT('Ctrl Pts',(-20.471038983326,-12.0790328822455,124.071504148972)) ;
#42997 = CARTESIAN_POINT('Ctrl Pts',(-20.4653210836285,-12.0785374876542,
124.080605021455)) ;
#42998 = CARTESIAN_POINT('Ctrl Pts',(-20.4629150540793,-12.0783310795398,
124.084389210572)) ;
#42999 = CARTESIAN_POINT('Ctrl Pts',(-20.459024363397,-12.0780005639255,124.090436349207)) ;
#43000 = CARTESIAN_POINT('Ctrl Pts',(-20.4575526308465,-12.0778762734332,
124.092707557993)) ;
#43001 = CARTESIAN_POINT('Ctrl Pts',(-20.4545688850919,-12.0776257600917,
124.097279533397)) ;
#43002 = CARTESIAN_POINT('Ctrl Pts',(-20.4530566237068,-12.0774995416619,
124.099580119985)) ;
#43003 = CARTESIAN_POINT('Ctrl Pts',(-20.4497822550268,-12.0772278527464,
124.104525707)) ;
#43004 = CARTESIAN_POINT('Ctrl Pts',(-20.4480176351474,-12.0770824197811,
124.1071690219)) ;
#43005 = CARTESIAN_POINT('Ctrl Pts',(-20.4432268762233,-12.0766902095232,
124.114286413317)) ;
#43006 = CARTESIAN_POINT('Ctrl Pts',(-20.440181782998,-12.0764437074837,124.118747659604)) ;
#43007 = CARTESIAN_POINT('Ctrl Pts',(-20.4231600012997,-12.0750808141701,
124.143341722488)) ;
#43008 = CARTESIAN_POINT('Ctrl Pts',(-20.4086224061265,-12.0739729147259,
124.163079910862)) ;
#43009 = CARTESIAN_POINT('Ctrl Pts',(-20.3827342658463,-12.0720740657774,
124.196146860031)) ;
#43010 = CARTESIAN_POINT('Ctrl Pts',(-20.3716669023115,-12.0712826312124,
124.20968796889)) ;
#43011 = CARTESIAN_POINT('Ctrl Pts',(-20.3550700481116,-12.0701207228053,
124.229146566824)) ;
#43012 = CARTESIAN_POINT('Ctrl Pts',(-20.3497613598008,-12.069752667848,124.235249630609)) ;
#43013 = CARTESIAN_POINT('Ctrl Pts',(-20.3410677171123,-12.0691554422604,
124.24505041029)) ;
#43014 = CARTESIAN_POINT('Ctrl Pts',(-20.337719091561,-12.0689266956642,124.248780052448)) ;
#43015 = CARTESIAN_POINT('Ctrl Pts',(-20.334271918944,-12.0686925060229,124.252573309059)) ;
#43016 = CARTESIAN_POINT('Ctrl Pts',(-20.3341956945753,-12.0686873282287,
124.252657163172)) ;
#43017 = CARTESIAN_POINT('Ctrl Pts',(-20.3339595696124,-12.0686712906362,
124.252916852313)) ;
#43018 = CARTESIAN_POINT('Ctrl Pts',(-20.3337996301731,-12.0686604303742,
124.25309265221)) ;
#43019 = CARTESIAN_POINT('Ctrl Pts',(-20.333492784064,-12.0686396001985,124.253429733652)) ;
#43020 = CARTESIAN_POINT('Ctrl Pts',(-20.3333458853265,-12.0686296303806,
124.253591022336)) ;
#43021 = CARTESIAN_POINT('Ctrl Pts',(-20.3330642130737,-12.0686105182027,
124.253900124131)) ;
#43022 = CARTESIAN_POINT('Ctrl Pts',(-20.3329294463048,-12.0686013759237,
124.254047943343)) ;
#43023 = CARTESIAN_POINT('Ctrl Pts',(-20.332671168294,-12.0685838587225,124.254331099572)) ;
#43024 = CARTESIAN_POINT('Ctrl Pts',(-20.3325476627452,-12.0685754838667,
124.254466441818)) ;
#43025 = CARTESIAN_POINT('Ctrl Pts',(-20.3323110779287,-12.0685594443458,
124.254725586322)) ;
#43026 = CARTESIAN_POINT('Ctrl Pts',(-20.3321980034844,-12.0685517797371,
124.254849393011)) ;
#43027 = CARTESIAN_POINT('Ctrl Pts',(-20.331981493834,-12.0685371065704,124.255086356494)) ;
#43028 = CARTESIAN_POINT('Ctrl Pts',(-20.3318780627405,-12.0685300980628,
124.255199516989)) ;
#43029 = CARTESIAN_POINT('Ctrl Pts',(-20.331680096091,-12.0685166860376,124.255416025672)) ;
#43030 = CARTESIAN_POINT('Ctrl Pts',(-20.3315855639849,-12.0685102825614,
124.255519376997)) ;
#43031 = CARTESIAN_POINT('Ctrl Pts',(-20.3314046954537,-12.0684980326301,
124.255717052638)) ;
#43032 = CARTESIAN_POINT('Ctrl Pts',(-20.3313183618313,-12.0684921862032,
124.255811379699)) ;
#43033 = CARTESIAN_POINT('Ctrl Pts',(-20.3311532334888,-12.0684810054224,
124.255991741332)) ;
#43034 = CARTESIAN_POINT('Ctrl Pts',(-20.3310744412592,-12.0684756711016,
124.256077778053)) ;
#43035 = CARTESIAN_POINT('Ctrl Pts',(-20.3309237821305,-12.0684654725984,
124.256242243189)) ;
#43036 = CARTESIAN_POINT('Ctrl Pts',(-20.3308519172403,-12.0684606084385,
124.256320673486)) ;
#43037 = CARTESIAN_POINT('Ctrl Pts',(-20.3307145406868,-12.0684513112035,
124.25647056202)) ;
#43038 = CARTESIAN_POINT('Ctrl Pts',(-20.3306490307995,-12.068446878154,124.256542021725)) ;
#43039 = CARTESIAN_POINT('Ctrl Pts',(-20.3305238328676,-12.068438406905,124.256678558643)) ;
#43040 = CARTESIAN_POINT('Ctrl Pts',(-20.3304641462319,-12.0684343687219,
124.256743637161)) ;
#43041 = CARTESIAN_POINT('Ctrl Pts',(-20.3303501020326,-12.0684266536365,
124.256867957267)) ;
#43042 = CARTESIAN_POINT('Ctrl Pts',(-20.3302957456573,-12.0684229767488,
124.256927199926)) ;
#43043 = CARTESIAN_POINT('Ctrl Pts',(-20.3301919066605,-12.068415953263,124.257040351455)) ;
#43044 = CARTESIAN_POINT('Ctrl Pts',(-20.330142424839,-12.0684126066642,124.257094261423)) ;
#43045 = CARTESIAN_POINT('Ctrl Pts',(-20.3275942274742,-12.0682402782955,
124.259870008572)) ;
#43046 = CARTESIAN_POINT('Ctrl Pts',(-20.3250834654456,-12.0680711542442,
124.262580752766)) ;
#43047 = CARTESIAN_POINT('Ctrl Pts',(-20.3198780452649,-12.0677218897207,
124.2681510398)) ;
#43048 = CARTESIAN_POINT('Ctrl Pts',(-20.3171818495613,-12.0675417325455,
124.27100908913)) ;
#43049 = CARTESIAN_POINT('Ctrl Pts',(-20.3108023467093,-12.0671172050382,
124.27770799624)) ;
#43050 = CARTESIAN_POINT('Ctrl Pts',(-20.307107903323,-12.0668727084403,124.281538134576)) ;
#43051 = CARTESIAN_POINT('Ctrl Pts',(-20.2943345101222,-12.066031994209,124.294612561432)) ;
#43052 = CARTESIAN_POINT('Ctrl Pts',(-20.2851363904559,-12.0654344961369,
124.303739173765)) ;
#43053 = CARTESIAN_POINT('Ctrl Pts',(-20.2574822667929,-12.0636620930152,
124.330337946274)) ;
#43054 = CARTESIAN_POINT('Ctrl Pts',(-20.2386334803495,-12.0624846856754,
124.347392129637)) ;
#43055 = CARTESIAN_POINT('Ctrl Pts',(-20.2119556078083,-12.0608669657171,
124.37008981392)) ;
#43056 = CARTESIAN_POINT('Ctrl Pts',(-20.2045616104589,-12.0604234921339,
124.376235042615)) ;
#43057 = CARTESIAN_POINT('Ctrl Pts',(-20.1924866005343,-12.0597072178838,
124.386037405299)) ;
#43058 = CARTESIAN_POINT('Ctrl Pts',(-20.1878491418317,-12.0594339856606,
124.389747529939)) ;
#43059 = CARTESIAN_POINT('Ctrl Pts',(-20.1794767341394,-12.0589439914911,
124.396348436506)) ;
#43060 = CARTESIAN_POINT('Ctrl Pts',(-20.1757515128087,-12.0587271273454,
124.399251363141)) ;
#43061 = CARTESIAN_POINT('Ctrl Pts',(-20.1683540435549,-12.0582987269334,
124.404948850542)) ;
#43062 = CARTESIAN_POINT('Ctrl Pts',(-20.1646825945398,-12.05808718572,124.407744326043)) ;
#43063 = CARTESIAN_POINT('Ctrl Pts',(-20.1608157665465,-12.0578654925939,
124.410654880582)) ;
#43064 = CARTESIAN_POINT('Ctrl Pts',(-20.1606357528137,-12.0578551745396,
124.410790300384)) ;
#43065 = CARTESIAN_POINT('Ctrl Pts',(-20.1602984200065,-12.0578358439238,
124.411043924606)) ;
#43066 = CARTESIAN_POINT('Ctrl Pts',(-20.1601411095926,-12.0578268312673,
124.411162140563)) ;
#43067 = CARTESIAN_POINT('Ctrl Pts',(-20.1598434801329,-12.0578097830254,
124.41138569382)) ;
#43068 = CARTESIAN_POINT('Ctrl Pts',(-20.1597031667895,-12.0578017473767,
124.411491038747)) ;
#43069 = CARTESIAN_POINT('Ctrl Pts',(-20.1594356387402,-12.057786429109,124.411691806296)) ;
#43070 = CARTESIAN_POINT('Ctrl Pts',(-20.1593084281031,-12.0577791464533,
124.411787234111)) ;
#43071 = CARTESIAN_POINT('Ctrl Pts',(-20.1590643237101,-12.0577651741489,
124.411970277687)) ;
#43072 = CARTESIAN_POINT('Ctrl Pts',(-20.1589474327491,-12.0577584844668,
124.412057897273)) ;
#43073 = CARTESIAN_POINT('Ctrl Pts',(-20.1587219056403,-12.057745579542,124.41222688703)) ;
#43074 = CARTESIAN_POINT('Ctrl Pts',(-20.1586132717365,-12.0577393642849,
124.412308259894)) ;
#43075 = CARTESIAN_POINT('Ctrl Pts',(-20.1584026835164,-12.0577273176757,
124.412465948699)) ;
#43076 = CARTESIAN_POINT('Ctrl Pts',(-20.1583007306745,-12.0577214863002,
124.41254226684)) ;
#43077 = CARTESIAN_POINT('Ctrl Pts',(-20.1581022696193,-12.057710136507,124.412690780155)) ;
#43078 = CARTESIAN_POINT('Ctrl Pts',(-20.1580057625742,-12.0577046180735,
124.412762976991)) ;
#43079 = CARTESIAN_POINT('Ctrl Pts',(-20.1578172025761,-12.0576938372846,
124.412903996033)) ;
#43080 = CARTESIAN_POINT('Ctrl Pts',(-20.1577251505985,-12.0576885749206,
124.41297281948)) ;
#43081 = CARTESIAN_POINT('Ctrl Pts',(-20.1575446897698,-12.0576782597237,
124.413107703761)) ;
#43082 = CARTESIAN_POINT('Ctrl Pts',(-20.157456281808,-12.0576732068914,124.413173765474)) ;
#43083 = CARTESIAN_POINT('Ctrl Pts',(-20.1572824323929,-12.0576632719408,
124.413303636337)) ;
#43084 = CARTESIAN_POINT('Ctrl Pts',(-20.1571969916154,-12.0576583898217,
124.413367446194)) ;
#43085 = CARTESIAN_POINT('Ctrl Pts',(-20.1570285018939,-12.057648763346,124.413493246027)) ;
#43086 = CARTESIAN_POINT('Ctrl Pts',(-20.1569454531689,-12.0576440189712,
124.413555236787)) ;
#43087 = CARTESIAN_POINT('Ctrl Pts',(-20.1567812503429,-12.0576346394902,
124.413677772291)) ;
#43088 = CARTESIAN_POINT('Ctrl Pts',(-20.1567000966792,-12.0576300043853,
124.41373831744)) ;
#43089 = CARTESIAN_POINT('Ctrl Pts',(-20.1565392466497,-12.0576208183974,
124.413858290094)) ;
#43090 = CARTESIAN_POINT('Ctrl Pts',(-20.156459550551,-12.0576162675118,124.413917717952)) ;
#43091 = CARTESIAN_POINT('Ctrl Pts',(-20.1563012245518,-12.0576072275777,
124.414035749237)) ;
#43092 = CARTESIAN_POINT('Ctrl Pts',(-20.156222594731,-12.0576027385209,124.414094353002)) ;
#43093 = CARTESIAN_POINT('Ctrl Pts',(-20.1560660452786,-12.0575938018824,
124.414211002567)) ;
#43094 = CARTESIAN_POINT('Ctrl Pts',(-20.1559881258435,-12.0575893543035,
124.414269048484)) ;
#43095 = CARTESIAN_POINT('Ctrl Pts',(-20.1558326679136,-12.0575804818033,
124.414384828354)) ;
#43096 = CARTESIAN_POINT('Ctrl Pts',(-20.1557551293923,-12.0575760568759,
124.414442562469)) ;
#43097 = CARTESIAN_POINT('Ctrl Pts',(-20.1556001235508,-12.0575672119902,
124.414557949737)) ;
#43098 = CARTESIAN_POINT('Ctrl Pts',(-20.1555226562434,-12.0575627920317,
124.41461560291)) ;
#43099 = CARTESIAN_POINT('Ctrl Pts',(-20.1553674967905,-12.0575539401913,
124.414731048651)) ;
#43100 = CARTESIAN_POINT('Ctrl Pts',(-20.1552898045009,-12.0575495083037,
124.414788841249)) ;
#43101 = CARTESIAN_POINT('Ctrl Pts',(-20.1551339073804,-12.0575406162019,
124.414904779572)) ;
#43102 = CARTESIAN_POINT('Ctrl Pts',(-20.155055702674,-12.0575361560007,124.414962925023)) ;
#43103 = CARTESIAN_POINT('Ctrl Pts',(-20.1548984973455,-12.0575271911289,
124.415079779147)) ;
#43104 = CARTESIAN_POINT('Ctrl Pts',(-20.1548194964674,-12.0575226864529,
124.415138487725)) ;
#43105 = CARTESIAN_POINT('Ctrl Pts',(-20.1546604153098,-12.057513616496,124.415256677862)) ;
#43106 = CARTESIAN_POINT('Ctrl Pts',(-20.1545803348686,-12.0575090512186,
124.415316159148)) ;
#43107 = CARTESIAN_POINT('Ctrl Pts',(-20.1544188072179,-12.0574998437157,
124.415436106912)) ;
#43108 = CARTESIAN_POINT('Ctrl Pts',(-20.1543373597396,-12.0574952014913,
124.415496573083)) ;
#43109 = CARTESIAN_POINT('Ctrl Pts',(-20.1541728031628,-12.0574858233395,
124.415618707936)) ;
#43110 = CARTESIAN_POINT('Ctrl Pts',(-20.1540896936947,-12.0574810874112,
124.415680376264)) ;
#43111 = CARTESIAN_POINT('Ctrl Pts',(-20.1539215070125,-12.0574715044696,
124.415805140628)) ;
#43112 = CARTESIAN_POINT('Ctrl Pts',(-20.1538364294899,-12.0574666574632,
124.415868236134)) ;
#43113 = CARTESIAN_POINT('Ctrl Pts',(-20.1536639857806,-12.0574568341573,
124.415996090502)) ;
#43114 = CARTESIAN_POINT('Ctrl Pts',(-20.1535766191235,-12.0574518578602,
124.416060848806)) ;
#43115 = CARTESIAN_POINT('Ctrl Pts',(-20.1533992573629,-12.0574417567091,
124.416192277825)) ;
#43116 = CARTESIAN_POINT('Ctrl Pts',(-20.1533092619858,-12.0574366318741,
124.41625894767)) ;
#43117 = CARTESIAN_POINT('Ctrl Pts',(-20.1531262805519,-12.057426213125,124.416394464812)) ;
#43118 = CARTESIAN_POINT('Ctrl Pts',(-20.1530332937176,-12.0574209192072,
124.416463311428)) ;
#43119 = CARTESIAN_POINT('Ctrl Pts',(-20.1528439398439,-12.0574101402404,
124.416603466635)) ;
#43120 = CARTESIAN_POINT('Ctrl Pts',(-20.1527475721204,-12.0574046551997,
124.416674774262)) ;
#43121 = CARTESIAN_POINT('Ctrl Pts',(-20.152551034916,-12.0573934701379,124.416820158891)) ;
#43122 = CARTESIAN_POINT('Ctrl Pts',(-20.1524508647029,-12.0573877701304,
124.416894234717)) ;
#43123 = CARTESIAN_POINT('Ctrl Pts',(-20.1522462639951,-12.0573761292124,
124.417045489537)) ;
#43124 = CARTESIAN_POINT('Ctrl Pts',(-20.1521418324939,-12.057370188309,124.417122667273)) ;
#43125 = CARTESIAN_POINT('Ctrl Pts',(-20.1519282076745,-12.0573580372646,
124.417280490394)) ;
#43126 = CARTESIAN_POINT('Ctrl Pts',(-20.1518190132248,-12.0573518271342,
124.417361134281)) ;
#43127 = CARTESIAN_POINT('Ctrl Pts',(-20.1515953113498,-12.0573391065198,
124.417526289564)) ;
#43128 = CARTESIAN_POINT('Ctrl Pts',(-20.1514808026935,-12.0573325960531,
124.417610799143)) ;
#43129 = CARTESIAN_POINT('Ctrl Pts',(-20.1512458645269,-12.0573192404725,
124.417784126035)) ;
#43130 = CARTESIAN_POINT('Ctrl Pts',(-20.1511254334448,-12.0573123953713,
124.41787294132)) ;
#43131 = CARTESIAN_POINT('Ctrl Pts',(-20.150877977331,-12.057298332577,124.418055366191)) ;
#43132 = CARTESIAN_POINT('Ctrl Pts',(-20.150750950563,-12.0572911149049,124.41814897332)) ;
#43133 = CARTESIAN_POINT('Ctrl Pts',(-20.150489555502,-12.0572762648578,124.418341521251)) ;
#43134 = CARTESIAN_POINT('Ctrl Pts',(-20.1503551850694,-12.0572686325019,
124.418440459237)) ;
#43135 = CARTESIAN_POINT('Ctrl Pts',(-20.1500782699442,-12.0572529062177,
124.418644268482)) ;
#43136 = CARTESIAN_POINT('Ctrl Pts',(-20.1499357226919,-12.0572448123094,
124.41874913645)) ;
#43137 = CARTESIAN_POINT('Ctrl Pts',(-20.1496415237164,-12.0572281106098,
124.418965474014)) ;
#43138 = CARTESIAN_POINT('Ctrl Pts',(-20.1494898692096,-12.0572195028557,
124.419076939539)) ;
#43139 = CARTESIAN_POINT('Ctrl Pts',(-20.1443685394988,-12.0569288782317,
124.422839317504)) ;
#43140 = CARTESIAN_POINT('Ctrl Pts',(-20.1393719328144,-12.0566471386495,
124.426453445166)) ;
#43141 = CARTESIAN_POINT('Ctrl Pts',(-20.1255185054637,-12.055870715307,124.436318536948)) ;
#43142 = CARTESIAN_POINT('Ctrl Pts',(-20.1166067945575,-12.0553765247343,
124.442491491923)) ;
#43143 = CARTESIAN_POINT('Ctrl Pts',(-20.0914470099835,-12.0539941350989,
124.459439124179)) ;
#43144 = CARTESIAN_POINT('Ctrl Pts',(-20.0750255514472,-12.0531066090487,
124.469950736286)) ;
#43145 = CARTESIAN_POINT('Ctrl Pts',(-20.0525191720812,-12.0519027342167,
124.483625996374)) ;
#43146 = CARTESIAN_POINT('Ctrl Pts',(-20.0466442997958,-12.0515896710104,
124.487129967897)) ;
#43147 = CARTESIAN_POINT('Ctrl Pts',(-20.032676899066,-12.0508483209912,124.495305915879)) ;
#43148 = CARTESIAN_POINT('Ctrl Pts',(-20.0245601602005,-12.0504198260218,
124.499935720589)) ;
#43149 = CARTESIAN_POINT('Ctrl Pts',(-20.0044213265263,-12.0493626881266,
124.511125562891)) ;
#43150 = CARTESIAN_POINT('Ctrl Pts',(-19.99234186859,-12.0487338290955,124.517579870373)) ;
#43151 = CARTESIAN_POINT('Ctrl Pts',(-19.9652252818033,-12.0473342758816,
124.531500928543)) ;
#43152 = CARTESIAN_POINT('Ctrl Pts',(-19.9501388118741,-12.0465637667119,
124.538865889378)) ;
#43153 = CARTESIAN_POINT('Ctrl Pts',(-19.9252376540814,-12.0453053509998,
124.550407052698)) ;
#43154 = CARTESIAN_POINT('Ctrl Pts',(-19.9155097758157,-12.0448169927548,
124.554765446727)) ;
#43155 = CARTESIAN_POINT('Ctrl Pts',(-19.8946295993106,-12.0437755254986,
124.563801543125)) ;
#43156 = CARTESIAN_POINT('Ctrl Pts',(-19.8834627402678,-12.0432225964147,
124.568442911964)) ;
#43157 = CARTESIAN_POINT('Ctrl Pts',(-19.8591075566196,-12.0420248983349,
124.578153839921)) ;
#43158 = CARTESIAN_POINT('Ctrl Pts',(-19.8458970696197,-12.0413804432317,
124.583163306072)) ;
#43159 = CARTESIAN_POINT('Ctrl Pts',(-19.8158088678918,-12.0399210477339,
124.593993120661)) ;
#43160 = CARTESIAN_POINT('Ctrl Pts',(-19.7988857140135,-12.0391060622872,
124.599677984354)) ;
#43161 = CARTESIAN_POINT('Ctrl Pts',(-19.7740746841145,-12.037916823148,124.607425284482)) ;
#43162 = CARTESIAN_POINT('Ctrl Pts',(-19.7662791928372,-12.037543982045,124.609776104457)) ;
#43163 = CARTESIAN_POINT('Ctrl Pts',(-19.7511429703411,-12.0368214058152,
124.614179740467)) ;
#43164 = CARTESIAN_POINT('Ctrl Pts',(-19.7438053291909,-12.0364717322552,
124.616241907134)) ;
#43165 = CARTESIAN_POINT('Ctrl Pts',(-19.7285968277276,-12.0357481327927,
124.620366393384)) ;
#43166 = CARTESIAN_POINT('Ctrl Pts',(-19.7207237653236,-12.0353741796058,
124.622419232244)) ;
#43167 = CARTESIAN_POINT('Ctrl Pts',(-19.7001251584904,-12.0343974086205,
124.627575913835)) ;
#43168 = CARTESIAN_POINT('Ctrl Pts',(-19.6873698948791,-12.0337941495709,
124.630556854992)) ;
#43169 = CARTESIAN_POINT('Ctrl Pts',(-19.6501716827793,-12.032040031368,124.638635797085)) ;
#43170 = CARTESIAN_POINT('Ctrl Pts',(-19.6256197994497,-12.0308890095939,
124.64320265141)) ;
#43171 = CARTESIAN_POINT('Ctrl Pts',(-19.5931551337363,-12.0293793022699,
124.648240370936)) ;
#43172 = CARTESIAN_POINT('Ctrl Pts',(-19.585351408933,-12.0290172890477,124.649375803324)) ;
#43173 = CARTESIAN_POINT('Ctrl Pts',(-19.5718896897063,-12.0283942530006,
124.651204559206)) ;
#43174 = CARTESIAN_POINT('Ctrl Pts',(-19.566236744264,-12.0281330610235,124.651933162974)) ;
#43175 = CARTESIAN_POINT('Ctrl Pts',(-19.5523692417059,-12.0274933054995,
124.653624194782)) ;
#43176 = CARTESIAN_POINT('Ctrl Pts',(-19.5441497319452,-12.0271149612263,
124.654543807795)) ;
#43177 = CARTESIAN_POINT('Ctrl Pts',(-19.5246868080321,-12.0262206937252,
124.656525983081)) ;
#43178 = CARTESIAN_POINT('Ctrl Pts',(-19.5134369276591,-12.0257050709966,
124.657517882401)) ;
#43179 = CARTESIAN_POINT('Ctrl Pts',(-19.4853015009001,-12.0244171121581,
124.659614772145)) ;
#43180 = CARTESIAN_POINT('Ctrl Pts',(-19.4684041245786,-12.0236450813739,
124.660529593175)) ;
#43181 = CARTESIAN_POINT('Ctrl Pts',(-19.4466484370546,-12.0226489006946,
124.661264854053)) ;
#43182 = CARTESIAN_POINT('Ctrl Pts',(-19.4418025291007,-12.022426842339,124.661400410368)) ;
#43183 = CARTESIAN_POINT('Ctrl Pts',(-19.4307285636967,-12.0219190179987,
124.661645725414)) ;
#43184 = CARTESIAN_POINT('Ctrl Pts',(-19.4245002340791,-12.021633153557,124.661737127126)) ;
#43185 = CARTESIAN_POINT('Ctrl Pts',(-19.4090200919699,-12.0209222484223,
124.661848577842)) ;
#43186 = CARTESIAN_POINT('Ctrl Pts',(-19.3997682456536,-12.0204970125023,
124.661812473261)) ;
#43187 = CARTESIAN_POINT('Ctrl Pts',(-19.3687712433552,-12.0190718561693,
124.661347352535)) ;
#43188 = CARTESIAN_POINT('Ctrl Pts',(-19.3470369751362,-12.0180719687089,
124.660453542271)) ;
#43189 = CARTESIAN_POINT('Ctrl Pts',(-19.3172112971142,-12.0167006665855,
124.658446273279)) ;
#43190 = CARTESIAN_POINT('Ctrl Pts',(-19.3090910499798,-12.0163273817509,
124.657820007713)) ;
#43191 = CARTESIAN_POINT('Ctrl Pts',(-19.2923975866369,-12.0155600723983,
124.656368297838)) ;
#43192 = CARTESIAN_POINT('Ctrl Pts',(-19.2838256084633,-12.0151661101584,
124.65553351323)) ;
#43193 = CARTESIAN_POINT('Ctrl Pts',(-19.2703192963284,-12.0145453108416,
124.654077142413)) ;
#43194 = CARTESIAN_POINT('Ctrl Pts',(-19.2653788878238,-12.0143182181916,
124.653514583271)) ;
#43195 = CARTESIAN_POINT('Ctrl Pts',(-19.2538264463011,-12.0137871040584,
124.652129246321)) ;
#43196 = CARTESIAN_POINT('Ctrl Pts',(-19.2472173711565,-12.0134831886539,
124.65128304931)) ;
#43197 = CARTESIAN_POINT('Ctrl Pts',(-19.2191352127577,-12.0121912127168,
124.647459082904)) ;
#43198 = CARTESIAN_POINT('Ctrl Pts',(-19.1977348075048,-12.0112052787082,
124.643975828618)) ;
#43199 = CARTESIAN_POINT('Ctrl Pts',(-19.1647917789404,-12.0096765760457,
124.637730254132)) ;
#43200 = CARTESIAN_POINT('Ctrl Pts',(-19.1531797584936,-12.0091356193974,
124.635357213597)) ;
#43201 = CARTESIAN_POINT('Ctrl Pts',(-19.1355291313851,-12.0083092609858,
124.631487839693)) ;
#43202 = CARTESIAN_POINT('Ctrl Pts',(-19.1294650249487,-12.0080246193139,
124.630110961285)) ;
#43203 = CARTESIAN_POINT('Ctrl Pts',(-19.1181604698532,-12.0074925317238,
124.627455363806)) ;
#43204 = CARTESIAN_POINT('Ctrl Pts',(-19.1129175323337,-12.0072451636844,
124.626187860992)) ;
#43205 = CARTESIAN_POINT('Ctrl Pts',(-19.1022175780253,-12.0067390810999,
124.623527679998)) ;
#43206 = CARTESIAN_POINT('Ctrl Pts',(-19.0967614396839,-12.0064803529673,
124.622131977315)) ;
#43207 = CARTESIAN_POINT('Ctrl Pts',(-19.0836511005747,-12.005857049312,124.618683735493)) ;
#43208 = CARTESIAN_POINT('Ctrl Pts',(-19.0760066315201,-12.0054922749296,
124.616595190539)) ;
#43209 = CARTESIAN_POINT('Ctrl Pts',(-19.0526500235282,-12.0043737799839,
124.609974621791)) ;
#43210 = CARTESIAN_POINT('Ctrl Pts',(-19.0370065431197,-12.0036190387041,
124.6052068633)) ;
#43211 = CARTESIAN_POINT('Ctrl Pts',(-19.0087145905505,-12.002245856984,124.595973710673)) ;
#43212 = CARTESIAN_POINT('Ctrl Pts',(-18.9960357541656,-12.0016275452273,
124.591609006089)) ;
#43213 = CARTESIAN_POINT('Ctrl Pts',(-18.9765469245285,-12.0006731551457,
124.584547241213)) ;
#43214 = CARTESIAN_POINT('Ctrl Pts',(-18.9696863143,-12.0003364032899,124.581992903515)) ;
#43215 = CARTESIAN_POINT('Ctrl Pts',(-18.9628485243969,-11.9999999855698,
124.579378441824)) ;
#43216 = CARTESIAN_POINT('',(-20.654497037415,-12.,123.302657626506)) ;
#43217 = CARTESIAN_POINT('Origin',(-19.4092722359532,-12.,123.411814366564)) ;
#43218 = CARTESIAN_POINT('',(-20.591904925275,-11.7,123.006993514553)) ;
#43219 = CARTESIAN_POINT('Ctrl Pts',(-20.591904925275,-11.7,123.006993514553)) ;
#43220 = CARTESIAN_POINT('Ctrl Pts',(-20.6041551258135,-11.7,123.042780919119)) ;
#43221 = CARTESIAN_POINT('Ctrl Pts',(-20.6154021887201,-11.7075896772134,
123.081471444624)) ;
#43222 = CARTESIAN_POINT('Ctrl Pts',(-20.6328682032119,-11.7382522587826,
123.15357258444)) ;
#43223 = CARTESIAN_POINT('Ctrl Pts',(-20.6391780918807,-11.761317155029,123.186964545377)) ;
#43224 = CARTESIAN_POINT('Ctrl Pts',(-20.6477244677879,-11.8144220247009,
123.24016910469)) ;
#43225 = CARTESIAN_POINT('Ctrl Pts',(-20.6505510417636,-11.8480564696762,
123.263577766805)) ;
#43226 = CARTESIAN_POINT('Ctrl Pts',(-20.6538866180434,-11.9219235159019,
123.294843389787)) ;
#43227 = CARTESIAN_POINT('Ctrl Pts',(-20.654497037415,-11.9621695797156,123.302657626506)) ;
#43228 = CARTESIAN_POINT('Ctrl Pts',(-20.654497037415,-12.,123.302657626506)) ;
#43229 = CARTESIAN_POINT('',(-20.4601832664426,-12.,122.734993854115)) ;
#43230 = CARTESIAN_POINT('Ctrl Pts',(-20.4601832664426,-12.,122.734993854115)) ;
#43231 = CARTESIAN_POINT('Ctrl Pts',(-20.4601832664426,-11.9621695923928,
122.734993854115)) ;
#43232 = CARTESIAN_POINT('Ctrl Pts',(-20.464489460108,-11.9219235188397,122.741542946412)) ;
#43233 = CARTESIAN_POINT('Ctrl Pts',(-20.4810132149992,-11.8480564142548,
122.76829402158)) ;
#43234 = CARTESIAN_POINT('Ctrl Pts',(-20.4931244558124,-11.8144219229966,
122.788524394775)) ;
#43235 = CARTESIAN_POINT('Ctrl Pts',(-20.5189747646632,-11.7613170365764,
122.835805557673)) ;
#43236 = CARTESIAN_POINT('Ctrl Pts',(-20.5344511925933,-11.7382521626639,
122.86605964457)) ;
#43237 = CARTESIAN_POINT('Ctrl Pts',(-20.5648328354891,-11.7075896412594,
122.933739475197)) ;
#43238 = CARTESIAN_POINT('Ctrl Pts',(-20.5796547571477,-11.7,122.971206204672)) ;
#43239 = CARTESIAN_POINT('Ctrl Pts',(-20.591904925275,-11.7,123.006993514553)) ;
#43240 = CARTESIAN_POINT('',(-18.1640505668151,-12.,123.521006833268)) ;
#43241 = CARTESIAN_POINT('Origin',(-19.4092722359532,-12.,123.411814366564)) ;
#43242 = CARTESIAN_POINT('Ctrl Pts',(-18.2266423653438,-11.7000000011364,
123.816643452992)) ;
#43243 = CARTESIAN_POINT('Ctrl Pts',(-18.2143944061214,-11.700003292843,123.780863409226)) ;
#43244 = CARTESIAN_POINT('Ctrl Pts',(-18.2031495305491,-11.7075931690383,
123.742182778096)) ;
#43245 = CARTESIAN_POINT('Ctrl Pts',(-18.1856835511285,-11.7382521626639,
123.670090636116)) ;
#43246 = CARTESIAN_POINT('Ctrl Pts',(-18.1793727421957,-11.7613170365764,
123.636698971197)) ;
#43247 = CARTESIAN_POINT('Ctrl Pts',(-18.1708248842569,-11.8144219229966,
123.583494827023)) ;
#43248 = CARTESIAN_POINT('Ctrl Pts',(-18.1679976569785,-11.8480564142548,
123.560086346945)) ;
#43249 = CARTESIAN_POINT('Ctrl Pts',(-18.1646612055237,-11.9219235188397,
123.528820989278)) ;
#43250 = CARTESIAN_POINT('Ctrl Pts',(-18.1640505668151,-11.9621695923928,
123.521006833268)) ;
#43251 = CARTESIAN_POINT('Ctrl Pts',(-18.1640505668151,-12.,123.521006833268)) ;
#43252 = CARTESIAN_POINT('',(-18.2266423654683,-13.9601742359176,123.816643453356)) ;
#43253 = CARTESIAN_POINT('Ctrl Pts',(-18.2740109056134,-10.1799890803629,
123.800437437226)) ;
#43254 = CARTESIAN_POINT('Ctrl Pts',(-17.9901976317162,-10.,123.897592500161)) ;
#43255 = CARTESIAN_POINT('Ctrl Pts',(-18.3189528014318,-10.186615931181,123.93177221557)) ;
#43256 = CARTESIAN_POINT('Ctrl Pts',(-18.0463587734884,-10.0066268508181,
124.061733136808)) ;
#43257 = CARTESIAN_POINT('Ctrl Pts',(-18.4544999825326,-10.199846557662,124.178242251159)) ;
#43258 = CARTESIAN_POINT('Ctrl Pts',(-18.2158202083151,-10.0198574772991,
124.369865791197)) ;
#43259 = CARTESIAN_POINT('Ctrl Pts',(-18.7737258963307,-10.2198221789206,
124.458448669119)) ;
#43260 = CARTESIAN_POINT('Ctrl Pts',(-18.6148367045085,-10.0398330985578,
124.72010058675)) ;
#43261 = CARTESIAN_POINT('Ctrl Pts',(-19.1683517049307,-10.2397395138226,
124.612076715426)) ;
#43262 = CARTESIAN_POINT('Ctrl Pts',(-19.1081207670208,-10.0597504334597,
124.912141899864)) ;
#43263 = CARTESIAN_POINT('Ctrl Pts',(-19.5908221387894,-10.2596127905386,
124.622761896565)) ;
#43264 = CARTESIAN_POINT('Ctrl Pts',(-19.636206114934,-10.0796237101757,124.92549851548)) ;
#43265 = CARTESIAN_POINT('Ctrl Pts',(-19.9944586595383,-10.2796372807025,
124.487357143018)) ;
#43266 = CARTESIAN_POINT('Ctrl Pts',(-20.1407529320189,-10.0996482003397,
124.756244590335)) ;
#43267 = CARTESIAN_POINT('Ctrl Pts',(-20.3250726893908,-10.2995051218533,
124.224284503461)) ;
#43268 = CARTESIAN_POINT('Ctrl Pts',(-20.5540202995955,-10.1195160414904,
124.427406225433)) ;
#43269 = CARTESIAN_POINT('Ctrl Pts',(-20.5474404603406,-10.3194507727328,
123.863209826147)) ;
#43270 = CARTESIAN_POINT('Ctrl Pts',(-20.8319818407582,-10.1394616923699,
123.976064807431)) ;
#43271 = CARTESIAN_POINT('Ctrl Pts',(-20.6329204930996,-10.3393561733498,
123.448689022605)) ;
#43272 = CARTESIAN_POINT('Ctrl Pts',(-20.9388342400949,-10.1593670929869,
123.457915382835)) ;
#43273 = CARTESIAN_POINT('Ctrl Pts',(-20.5727382583942,-10.3592304011661,
123.030414178423)) ;
#43274 = CARTESIAN_POINT('Ctrl Pts',(-20.8636098402301,-10.1792413208033,
122.935072644727)) ;
#43275 = CARTESIAN_POINT('Ctrl Pts',(-20.3723372035374,-10.3792161920437,
122.655670923463)) ;
#43276 = CARTESIAN_POINT('Ctrl Pts',(-20.6131115834081,-10.1992271116809,
122.466642059227)) ;
#43277 = CARTESIAN_POINT('Ctrl Pts',(-20.0574028124706,-10.3991104347035,
122.373313004285)) ;
#43278 = CARTESIAN_POINT('Ctrl Pts',(-20.219446657189,-10.2191213543406,122.11369274935)) ;
#43279 = CARTESIAN_POINT('Ctrl Pts',(-19.6656681691958,-10.4189891507756,
122.214436559376)) ;
#43280 = CARTESIAN_POINT('Ctrl Pts',(-19.729780773993,-10.2390000704127,121.915093775378)) ;
#43281 = CARTESIAN_POINT('Ctrl Pts',(-19.2398981074651,-10.4390286006202,
122.199163423108)) ;
#43282 = CARTESIAN_POINT('Ctrl Pts',(-19.1975679684769,-10.2590395202573,
121.895998337816)) ;
#43283 = CARTESIAN_POINT('Ctrl Pts',(-18.8378689724914,-10.458891762158,122.328984896592)) ;
#43284 = CARTESIAN_POINT('Ctrl Pts',(-18.6950312339923,-10.2789026817952,
122.058270950238)) ;
#43285 = CARTESIAN_POINT('Ctrl Pts',(-18.5023795521869,-10.4788711301723,
122.589370841986)) ;
#43286 = CARTESIAN_POINT('Ctrl Pts',(-18.2756669291778,-10.2988820498094,
122.383749835563)) ;
#43287 = CARTESIAN_POINT('Ctrl Pts',(-18.2772917542457,-10.4986817106951,
122.945518138246)) ;
#43288 = CARTESIAN_POINT('Ctrl Pts',(-17.9943038605785,-10.3186926303322,
122.828930487561)) ;
#43289 = CARTESIAN_POINT('Ctrl Pts',(-18.1858955375249,-10.5186626389807,
123.360335745372)) ;
#43290 = CARTESIAN_POINT('Ctrl Pts',(-17.8800540061898,-10.3386735586178,
123.347451469643)) ;
#43291 = CARTESIAN_POINT('Ctrl Pts',(-18.2415877544767,-10.5385553108501,
123.779674054783)) ;
#43292 = CARTESIAN_POINT('Ctrl Pts',(-17.949663613675,-10.3585662304872,123.871624239523)) ;
#43293 = CARTESIAN_POINT('Ctrl Pts',(-18.4366892236376,-10.5584816411372,
124.155765874511)) ;
#43294 = CARTESIAN_POINT('Ctrl Pts',(-18.1935384904851,-10.3784925607743,
124.34174209524)) ;
#43295 = CARTESIAN_POINT('Ctrl Pts',(-18.7493758900079,-10.5784521952295,
124.443056780365)) ;
#43296 = CARTESIAN_POINT('Ctrl Pts',(-18.5843830566034,-10.3984631148666,
124.700856014279)) ;
#43297 = CARTESIAN_POINT('Ctrl Pts',(-19.0736750036282,-10.5949840343171,
124.578605622473)) ;
#43298 = CARTESIAN_POINT('Ctrl Pts',(-18.9897866675992,-10.4149949539542,
124.870306748339)) ;
#43299 = CARTESIAN_POINT('Ctrl Pts',(-19.3515822133367,-10.6083237731447,
124.616534422033)) ;
#43300 = CARTESIAN_POINT('Ctrl Pts',(-19.3371420473607,-10.4283346927818,
124.917711789777)) ;
#43301 = CARTESIAN_POINT('Ctrl Pts',(-19.5623087353055,-10.6183560153633,
124.608012512987)) ;
#43302 = CARTESIAN_POINT('Ctrl Pts',(-19.6005562667331,-10.4383669350004,
124.907063768782)) ;
#43303 = CARTESIAN_POINT('Ctrl Pts',(-19.7648570829155,-10.6282137160067,
124.564122231623)) ;
#43304 = CARTESIAN_POINT('Ctrl Pts',(-19.8537397870735,-10.4482246356439,
124.852203726746)) ;
#43305 = CARTESIAN_POINT('Ctrl Pts',(-19.9594412369529,-10.638205580646,124.485025335786)) ;
#43306 = CARTESIAN_POINT('Ctrl Pts',(-20.0969735539785,-10.4582165002831,
124.753332920083)) ;
#43307 = CARTESIAN_POINT('Ctrl Pts',(-20.1360906792147,-10.6481281304061,
124.374071893985)) ;
#43308 = CARTESIAN_POINT('Ctrl Pts',(-20.3177787346395,-10.4681390500432,
124.614652183365)) ;
#43309 = CARTESIAN_POINT('Ctrl Pts',(-20.3435921685771,-10.6614059038996,
124.187345412144)) ;
#43310 = CARTESIAN_POINT('Ctrl Pts',(-20.5771970981362,-10.4814168235367,
124.381203458891)) ;
#43311 = CARTESIAN_POINT('Ctrl Pts',(-20.4979359412099,-10.6747532428402,
123.949230531229)) ;
#43312 = CARTESIAN_POINT('Ctrl Pts',(-20.7701003708174,-10.4947641624773,
124.083584310457)) ;
#43313 = CARTESIAN_POINT('Ctrl Pts',(-20.5838202221108,-10.6879604746334,
123.685128933396)) ;
#43314 = CARTESIAN_POINT('Ctrl Pts',(-20.8774553693723,-10.5079713942705,
123.753475217054)) ;
#43315 = CARTESIAN_POINT('Ctrl Pts',(-20.6134756841563,-10.6979475907231,
123.477310674119)) ;
#43316 = CARTESIAN_POINT('Ctrl Pts',(-20.9145282391216,-10.5179585103602,
123.493699384276)) ;
#43317 = CARTESIAN_POINT('Ctrl Pts',(-20.6067552821165,-10.7078984963028,
123.26817900999)) ;
#43318 = CARTESIAN_POINT('Ctrl Pts',(-20.9061303769722,-10.52790941594,123.232285620267)) ;
#43319 = CARTESIAN_POINT('Ctrl Pts',(-20.5631517199141,-10.7179535983103,
123.061365279476)) ;
#43320 = CARTESIAN_POINT('Ctrl Pts',(-20.8516285272166,-10.5379645179474,
122.973767430347)) ;
#43321 = CARTESIAN_POINT('Ctrl Pts',(-20.4864480135789,-10.7277752716314,
122.869632358223)) ;
#43322 = CARTESIAN_POINT('Ctrl Pts',(-20.755752145473,-10.5477861912685,122.734100762332)) ;
#43323 = CARTESIAN_POINT('Ctrl Pts',(-20.3753148949047,-10.7378337427063,
122.689756073264)) ;
#43324 = CARTESIAN_POINT('Ctrl Pts',(-20.6168357130529,-10.5578446623434,
122.509252277714)) ;
#43325 = CARTESIAN_POINT('Ctrl Pts',(-20.2362698429268,-10.7477583538828,
122.534165638144)) ;
#43326 = CARTESIAN_POINT('Ctrl Pts',(-20.4430403513938,-10.5677692735199,
122.314768071456)) ;
#43327 = CARTESIAN_POINT('Ctrl Pts',(-20.0174236370264,-10.7610356927832,
122.360928612314)) ;
#43328 = CARTESIAN_POINT('Ctrl Pts',(-20.1694406712993,-10.5810466124203,
122.098190251904)) ;
#43329 = CARTESIAN_POINT('Ctrl Pts',(-19.7578453903065,-10.7743345720208,
122.248851511266)) ;
#43330 = CARTESIAN_POINT('Ctrl Pts',(-19.8449850134819,-10.5943454916579,
121.958111265335)) ;
#43331 = CARTESIAN_POINT('Ctrl Pts',(-19.4824813143237,-10.7875734441915,
122.208088439905)) ;
#43332 = CARTESIAN_POINT('Ctrl Pts',(-19.5008057716341,-10.6075843638286,
121.907157355648)) ;
#43333 = CARTESIAN_POINT('Ctrl Pts',(-19.2721785775522,-10.7975800623281,
122.213521358078)) ;
#43334 = CARTESIAN_POINT('Ctrl Pts',(-19.2379220825872,-10.6175909819652,
121.913944971404)) ;
#43335 = CARTESIAN_POINT('Ctrl Pts',(-19.0656000898289,-10.8076110073896,
122.255887753777)) ;
#43336 = CARTESIAN_POINT('Ctrl Pts',(-18.9796997397484,-10.6276219270267,
121.966900411424)) ;
#43337 = CARTESIAN_POINT('Ctrl Pts',(-18.8727746571245,-10.8174671807414,
122.33177975615)) ;
#43338 = CARTESIAN_POINT('Ctrl Pts',(-18.7386663423424,-10.6374781003785,
122.061762842601)) ;
#43339 = CARTESIAN_POINT('Ctrl Pts',(-18.6933942950045,-10.8274664517043,
122.441317819794)) ;
#43340 = CARTESIAN_POINT('Ctrl Pts',(-18.5144394578762,-10.6474773713414,
122.198683103417)) ;
#43341 = CARTESIAN_POINT('Ctrl Pts',(-18.5371942685893,-10.8373609034616,
122.578747643145)) ;
#43342 = CARTESIAN_POINT('Ctrl Pts',(-18.3191873796767,-10.6573718230987,
122.370468477432)) ;
#43343 = CARTESIAN_POINT('Ctrl Pts',(-18.4051122896899,-10.847424219271,122.743966469464)) ;
#43344 = CARTESIAN_POINT('Ctrl Pts',(-18.1540827677519,-10.6674351389081,
122.576990252266)) ;
#43345 = CARTESIAN_POINT('Ctrl Pts',(-18.3057391169289,-10.8572630760106,
122.925417587621)) ;
#43346 = CARTESIAN_POINT('Ctrl Pts',(-18.0298636947034,-10.6772739956477,
122.80380319062)) ;
#43347 = CARTESIAN_POINT('Ctrl Pts',(-18.2376490708675,-10.8673291978282,
123.125750203822)) ;
#43348 = CARTESIAN_POINT('Ctrl Pts',(-17.9447485718205,-10.6873401174653,
123.054218033102)) ;
#43349 = CARTESIAN_POINT('Ctrl Pts',(-18.2060503452321,-10.8772124255524,
123.331137906529)) ;
#43350 = CARTESIAN_POINT('Ctrl Pts',(-17.9052474071487,-10.6972233451896,
123.310952604467)) ;
#43351 = CARTESIAN_POINT('Ctrl Pts',(-18.2101816179164,-10.8872018868312,
123.541086163132)) ;
#43352 = CARTESIAN_POINT('Ctrl Pts',(-17.9104088183902,-10.7072128064683,
123.573388107812)) ;
#43353 = CARTESIAN_POINT('Ctrl Pts',(-18.2506800550467,-10.8971655972577,
123.746612755988)) ;
#43354 = CARTESIAN_POINT('Ctrl Pts',(-17.9610292610865,-10.7171765168948,
123.830297049982)) ;
#43355 = CARTESIAN_POINT('Ctrl Pts',(-18.3262823417106,-10.9071605999886,
123.942684202324)) ;
#43356 = CARTESIAN_POINT('Ctrl Pts',(-18.055529675207,-10.7271715196257,124.075387412779)) ;
#43357 = CARTESIAN_POINT('Ctrl Pts',(-18.4354992661144,-10.9171969309989,
124.123200848044)) ;
#43358 = CARTESIAN_POINT('Ctrl Pts',(-18.1920485023394,-10.737207850636,124.30103460394)) ;
#43359 = CARTESIAN_POINT('Ctrl Pts',(-18.5715282260324,-10.9270431603412,
124.279245467908)) ;
#43360 = CARTESIAN_POINT('Ctrl Pts',(-18.3620830674316,-10.7470540799783,
124.496092551227)) ;
#43361 = CARTESIAN_POINT('Ctrl Pts',(-18.734581283145,-10.9370286586164,124.411415680481)) ;
#43362 = CARTESIAN_POINT('Ctrl Pts',(-18.5658978745921,-10.7570395782535,
124.661307439936)) ;
#43363 = CARTESIAN_POINT('Ctrl Pts',(-18.9171658090595,-10.9469635615994,
124.512917995207)) ;
#43364 = CARTESIAN_POINT('Ctrl Pts',(-18.7941275674691,-10.7669744812365,
124.788187738228)) ;
#43365 = CARTESIAN_POINT('Ctrl Pts',(-19.1170341754858,-10.9570210646946,
124.581816159323)) ;
#43366 = CARTESIAN_POINT('Ctrl Pts',(-19.0439620659958,-10.7770319843317,
124.874312872399)) ;
#43367 = CARTESIAN_POINT('Ctrl Pts',(-19.3209344460454,-10.9668427210651,
124.614507954261)) ;
#43368 = CARTESIAN_POINT('Ctrl Pts',(-19.2988377714799,-10.7868536407023,
124.915180256188)) ;
#43369 = CARTESIAN_POINT('Ctrl Pts',(-19.5323077477126,-10.9768987837303,
124.611618015789)) ;
#43370 = CARTESIAN_POINT('Ctrl Pts',(-19.5630543230624,-10.7969097033674,
124.911570311771)) ;
#43371 = CARTESIAN_POINT('Ctrl Pts',(-19.7375399994228,-10.9868394484335,
124.572149859508)) ;
#43372 = CARTESIAN_POINT('Ctrl Pts',(-19.819595446342,-10.8068503680706,124.862237558294)) ;
#43373 = CARTESIAN_POINT('Ctrl Pts',(-19.932315810984,-10.996743852382,124.498530010297)) ;
#43374 = CARTESIAN_POINT('Ctrl Pts',(-20.0630665620373,-10.8167547720191,
124.77021482164)) ;
#43375 = CARTESIAN_POINT('Ctrl Pts',(-20.1138352643569,-11.0067903373756,
124.39058103883)) ;
#43376 = CARTESIAN_POINT('Ctrl Pts',(-20.2899670415844,-10.8268012570127,
124.635280761768)) ;
#43377 = CARTESIAN_POINT('Ctrl Pts',(-20.271611629066,-11.0166865651873,124.254920335698)) ;
#43378 = CARTESIAN_POINT('Ctrl Pts',(-20.4871895041345,-10.8366974848244,
124.465706330208)) ;
#43379 = CARTESIAN_POINT('Ctrl Pts',(-20.4056065237285,-11.0267461487508,
124.09133118011)) ;
#43380 = CARTESIAN_POINT('Ctrl Pts',(-20.6546848715982,-10.8467570683879,
124.261221540526)) ;
#43381 = CARTESIAN_POINT('Ctrl Pts',(-20.5070605056192,-11.0365981584196,
123.910749358251)) ;
#43382 = CARTESIAN_POINT('Ctrl Pts',(-20.7815048415044,-10.8566090780567,
124.035494716813)) ;
#43383 = CARTESIAN_POINT('Ctrl Pts',(-20.5770451368418,-11.0465606898592,
123.713354618847)) ;
#43384 = CARTESIAN_POINT('Ctrl Pts',(-20.8689878382938,-10.8665716094963,
123.788751735695)) ;
#43385 = CARTESIAN_POINT('Ctrl Pts',(-20.6116136924991,-11.0565922380985,
123.505305288482)) ;
#43386 = CARTESIAN_POINT('Ctrl Pts',(-20.912200798905,-10.8766031577357,123.528690516731)) ;
#43387 = CARTESIAN_POINT('Ctrl Pts',(-20.6097611314172,-11.0664836493116,
123.297365165469)) ;
#43388 = CARTESIAN_POINT('Ctrl Pts',(-20.9098873495447,-10.8864945689487,
123.268764662041)) ;
#43389 = CARTESIAN_POINT('Ctrl Pts',(-20.5717257520097,-11.0764999030196,
123.090247708174)) ;
#43390 = CARTESIAN_POINT('Ctrl Pts',(-20.8623452479891,-10.8965108226567,
123.009867420401)) ;
#43391 = CARTESIAN_POINT('Ctrl Pts',(-20.4977797269794,-11.0865300058643,
122.892777790247)) ;
#43392 = CARTESIAN_POINT('Ctrl Pts',(-20.7699148713601,-10.9065409255014,
122.763029266333)) ;
#43393 = CARTESIAN_POINT('Ctrl Pts',(-20.3928580773295,-11.096386454818,122.714076335493)) ;
#43394 = CARTESIAN_POINT('Ctrl Pts',(-20.6387642261451,-10.9163973744551,
122.539650565094)) ;
#43395 = CARTESIAN_POINT('Ctrl Pts',(-20.2567901765193,-11.1063854655903,
122.553889016232)) ;
#43396 = CARTESIAN_POINT('Ctrl Pts',(-20.4686808693851,-10.9263963852274,
122.339414946397)) ;
#43397 = CARTESIAN_POINT('Ctrl Pts',(-20.0967506938251,-11.1162806825083,
122.420933108959)) ;
#43398 = CARTESIAN_POINT('Ctrl Pts',(-20.2686322562331,-10.9362916021454,
122.17321802605)) ;
#43399 = CARTESIAN_POINT('Ctrl Pts',(-19.9130792390864,-11.1263411978656,
122.316112855486)) ;
#43400 = CARTESIAN_POINT('Ctrl Pts',(-20.0390441621644,-10.9463521175027,
122.042191046987)) ;
#43401 = CARTESIAN_POINT('Ctrl Pts',(-19.7181773873714,-11.1361904912527,
122.246149401792)) ;
#43402 = CARTESIAN_POINT('Ctrl Pts',(-19.7954165502139,-10.9562014108898,
121.954734482504)) ;
#43403 = CARTESIAN_POINT('Ctrl Pts',(-19.5105138121636,-11.1462176669327,
122.209933979005)) ;
#43404 = CARTESIAN_POINT('Ctrl Pts',(-19.5358374377705,-10.9662285865698,
121.909463378996)) ;
#43405 = CARTESIAN_POINT('Ctrl Pts',(-19.2996733625681,-11.1562462425598,
122.210880868471)) ;
#43406 = CARTESIAN_POINT('Ctrl Pts',(-19.2722869357793,-10.976257162197,121.910644966112)) ;
#43407 = CARTESIAN_POINT('Ctrl Pts',(-19.0959460919219,-11.1660913361057,
122.247342057068)) ;
#43408 = CARTESIAN_POINT('Ctrl Pts',(-19.0176264126342,-10.9861022557429,
121.956219772892)) ;
#43409 = CARTESIAN_POINT('Ctrl Pts',(-18.8985578247058,-11.1760825775375,
122.319166361709)) ;
#43410 = CARTESIAN_POINT('Ctrl Pts',(-18.7708903038592,-10.9960934971746,
122.045998590472)) ;
#43411 = CARTESIAN_POINT('Ctrl Pts',(-18.7160448813455,-11.1861183586808,
122.425022343304)) ;
#43412 = CARTESIAN_POINT('Ctrl Pts',(-18.5427482922778,-11.0061292783179,
122.178316886012)) ;
#43413 = CARTESIAN_POINT('Ctrl Pts',(-18.5574679836989,-11.1959705644105,
122.558254372856)) ;
#43414 = CARTESIAN_POINT('Ctrl Pts',(-18.3445251559911,-11.0159814840476,
122.344856285624)) ;
#43415 = CARTESIAN_POINT('Ctrl Pts',(-18.4224794756724,-11.2059326585275,
122.718377576205)) ;
#43416 = CARTESIAN_POINT('Ctrl Pts',(-18.1757880512695,-11.0259435781646,
122.545009574833)) ;
#43417 = CARTESIAN_POINT('Ctrl Pts',(-18.3169268323872,-11.2159552193546,
122.900738727932)) ;
#43418 = CARTESIAN_POINT('Ctrl Pts',(-18.0438458206682,-11.0359661389917,
122.7729601423)) ;
#43419 = CARTESIAN_POINT('Ctrl Pts',(-18.2451248266948,-11.2258829910061,
123.096732722796)) ;
#43420 = CARTESIAN_POINT('Ctrl Pts',(-17.9540915966108,-11.0458939106433,
123.017952668927)) ;
#43421 = CARTESIAN_POINT('Ctrl Pts',(-18.2080492813558,-11.235925375131,123.304558510364)) ;
#43422 = CARTESIAN_POINT('Ctrl Pts',(-17.9077456060715,-11.0559362947681,
123.277734456028)) ;
#43423 = CARTESIAN_POINT('Ctrl Pts',(-18.2075431826477,-11.2458145992016,
123.512472427979)) ;
#43424 = CARTESIAN_POINT('Ctrl Pts',(-17.9071113956414,-11.0658255188387,
123.537627775337)) ;
#43425 = CARTESIAN_POINT('Ctrl Pts',(-18.2431137932323,-11.2558038473689,
123.719436413788)) ;
#43426 = CARTESIAN_POINT('Ctrl Pts',(-17.9515732678051,-11.075814767006,123.796333212552)) ;
#43427 = CARTESIAN_POINT('Ctrl Pts',(-18.3140127800185,-11.2657624244109,
123.916420734498)) ;
#43428 = CARTESIAN_POINT('Ctrl Pts',(-18.0401957307403,-11.085773344048,124.042564530846)) ;
#43429 = CARTESIAN_POINT('Ctrl Pts',(-18.4169840173117,-11.2756619935022,
124.097296523522)) ;
#43430 = CARTESIAN_POINT('Ctrl Pts',(-18.168909061226,-11.0956729131393,124.268660685117)) ;
#43431 = CARTESIAN_POINT('Ctrl Pts',(-18.5518230953768,-11.2857099055862,
124.259873078024)) ;
#43432 = CARTESIAN_POINT('Ctrl Pts',(-18.337456729501,-11.1057208252233,124.471882073783)) ;
#43433 = CARTESIAN_POINT('Ctrl Pts',(-18.7103328750192,-11.2956052598934,
124.394651304533)) ;
#43434 = CARTESIAN_POINT('Ctrl Pts',(-18.5355938114042,-11.1156161795305,
124.640356432155)) ;
#43435 = CARTESIAN_POINT('Ctrl Pts',(-18.8927897807584,-11.3056669103846,
124.50162581541)) ;
#43436 = CARTESIAN_POINT('Ctrl Pts',(-18.7636640136148,-11.1256778300217,
124.774075513825)) ;
#43437 = CARTESIAN_POINT('Ctrl Pts',(-19.0867894285585,-11.315511525847,124.573745609378)) ;
#43438 = CARTESIAN_POINT('Ctrl Pts',(-19.006164366436,-11.1355224454842,124.864226909227)) ;
#43439 = CARTESIAN_POINT('Ctrl Pts',(-19.2926054693123,-11.3254716047484,
124.612260164776)) ;
#43440 = CARTESIAN_POINT('Ctrl Pts',(-19.2634346826531,-11.1454825243856,
124.912371167711)) ;
#43441 = CARTESIAN_POINT('Ctrl Pts',(-19.5036241030656,-11.3355097991068,
124.6140594671)) ;
#43442 = CARTESIAN_POINT('Ctrl Pts',(-19.527207804198,-11.1555207187439,124.914621442776)) ;
#43443 = CARTESIAN_POINT('Ctrl Pts',(-19.7084368116268,-11.3453835145064,
124.580138707835)) ;
#43444 = CARTESIAN_POINT('Ctrl Pts',(-19.7832249578582,-11.1653944341435,
124.872221302149)) ;
#43445 = CARTESIAN_POINT('Ctrl Pts',(-19.9081154986966,-11.3554552240407,
124.509785415039)) ;
#43446 = CARTESIAN_POINT('Ctrl Pts',(-20.0328232712046,-11.1754661436778,
124.784280775567)) ;
#43447 = CARTESIAN_POINT('Ctrl Pts',(-20.0882613339957,-11.3652876644932,
124.408381333972)) ;
#43448 = CARTESIAN_POINT('Ctrl Pts',(-20.2580073160466,-11.1852985841303,
124.657525797588)) ;
#43449 = CARTESIAN_POINT('Ctrl Pts',(-20.251660229155,-11.3753194854186,124.275048143701)) ;
#43450 = CARTESIAN_POINT('Ctrl Pts',(-20.4622563153842,-11.1953304050557,
124.490859965048)) ;
#43451 = CARTESIAN_POINT('Ctrl Pts',(-20.388818370831,-11.3853398553042,124.115153399644)) ;
#43452 = CARTESIAN_POINT('Ctrl Pts',(-20.6337047072471,-11.2053507749413,
124.290992198856)) ;
#43453 = CARTESIAN_POINT('Ctrl Pts',(-20.4949578126602,-11.3952066264379,
123.936918605361)) ;
#43454 = CARTESIAN_POINT('Ctrl Pts',(-20.7663802888455,-11.215217546075,124.068198059716)) ;
#43455 = CARTESIAN_POINT('Ctrl Pts',(-20.5700397801666,-11.4052773976273,
123.738981962488)) ;
#43456 = CARTESIAN_POINT('Ctrl Pts',(-20.8602333250101,-11.2252883172644,
123.820777914708)) ;
#43457 = CARTESIAN_POINT('Ctrl Pts',(-20.608748085118,-11.4151205581489,123.535688979496)) ;
#43458 = CARTESIAN_POINT('Ctrl Pts',(-20.9086197171465,-11.235131477786,123.566660443392)) ;
#43459 = CARTESIAN_POINT('Ctrl Pts',(-20.6122979783934,-11.4251007913353,
123.32590993056)) ;
#43460 = CARTESIAN_POINT('Ctrl Pts',(-20.9130575837451,-11.2451117109724,
123.304436329207)) ;
#43461 = CARTESIAN_POINT('Ctrl Pts',(-20.5788422571338,-11.4351193113705,
123.117968685033)) ;
#43462 = CARTESIAN_POINT('Ctrl Pts',(-20.871238578832,-11.2551302310076,123.044509679255)) ;
#43463 = CARTESIAN_POINT('Ctrl Pts',(-20.5111294875309,-11.4450026197542,
122.921507091262)) ;
#43464 = CARTESIAN_POINT('Ctrl Pts',(-20.7865977118334,-11.2650135393913,
122.798931493979)) ;
#43465 = CARTESIAN_POINT('Ctrl Pts',(-20.4083944122188,-11.455070903925,122.736483235784)) ;
#43466 = CARTESIAN_POINT('Ctrl Pts',(-20.6581795184354,-11.2750818235621,
122.567651782636)) ;
#43467 = CARTESIAN_POINT('Ctrl Pts',(-20.278392781555,-11.4649010305926,122.575789839308)) ;
#43468 = CARTESIAN_POINT('Ctrl Pts',(-20.4956768373956,-11.2849119502298,
122.366783576293)) ;
#43469 = CARTESIAN_POINT('Ctrl Pts',(-20.1189455476198,-11.4749676027992,
122.43668549405)) ;
#43470 = CARTESIAN_POINT('Ctrl Pts',(-20.2963683002106,-11.2949785224363,
122.192903170129)) ;
#43471 = CARTESIAN_POINT('Ctrl Pts',(-19.9408261904973,-11.4848577590399,
122.329373206102)) ;
#43472 = CARTESIAN_POINT('Ctrl Pts',(-20.0737183940731,-11.304868678677,122.058761956782)) ;
#43473 = CARTESIAN_POINT('Ctrl Pts',(-19.7449718071379,-11.4948502866163,
122.253435565076)) ;
#43474 = CARTESIAN_POINT('Ctrl Pts',(-19.8289002832035,-11.3148612062534,
121.963839656321)) ;
#43475 = CARTESIAN_POINT('Ctrl Pts',(-19.5394995838217,-11.5048117764906,
122.212958774971)) ;
#43476 = CARTESIAN_POINT('Ctrl Pts',(-19.5720596012938,-11.3248226961277,
121.913243325035)) ;
#43477 = CARTESIAN_POINT('Ctrl Pts',(-19.3312195995513,-11.5147209983778,
122.208316709471)) ;
#43478 = CARTESIAN_POINT('Ctrl Pts',(-19.3117087063765,-11.3347319180149,
121.907440658381)) ;
#43479 = CARTESIAN_POINT('Ctrl Pts',(-19.1224333832175,-11.5247695781881,
122.240425699493)) ;
#43480 = CARTESIAN_POINT('Ctrl Pts',(-19.0507261790839,-11.3447804978252,
121.947576761925)) ;
#43481 = CARTESIAN_POINT('Ctrl Pts',(-18.9256450998965,-11.5346525526582,
122.307117491957)) ;
#43482 = CARTESIAN_POINT('Ctrl Pts',(-18.8047397506185,-11.3546634722953,
122.030941792183)) ;
#43483 = CARTESIAN_POINT('Ctrl Pts',(-18.7411595782649,-11.5446474638009,
122.407688727702)) ;
#43484 = CARTESIAN_POINT('Ctrl Pts',(-18.5741327464813,-11.364658383438,122.156656022076)) ;
#43485 = CARTESIAN_POINT('Ctrl Pts',(-18.5766849466755,-11.5546678503745,
122.539338975724)) ;
#43486 = CARTESIAN_POINT('Ctrl Pts',(-18.3685394795987,-11.3746787700116,
122.321218804861)) ;
#43487 = CARTESIAN_POINT('Ctrl Pts',(-18.4390281447,-11.5645779542315,122.69570721258)) ;
#43488 = CARTESIAN_POINT('Ctrl Pts',(-18.1964679003152,-11.3845888738687,
122.516679816547)) ;
#43489 = CARTESIAN_POINT('Ctrl Pts',(-18.3299418694843,-11.5745056664414,
122.873650877876)) ;
#43490 = CARTESIAN_POINT('Ctrl Pts',(-18.0601098924679,-11.3945165860786,
122.739110167226)) ;
#43491 = CARTESIAN_POINT('Ctrl Pts',(-18.2526908814426,-11.5845487762087,
123.070140221989)) ;
#43492 = CARTESIAN_POINT('Ctrl Pts',(-17.9635464111682,-11.4045596958458,
122.984721718142)) ;
#43493 = CARTESIAN_POINT('Ctrl Pts',(-18.2112504293198,-11.5944351966642,
123.273822369061)) ;
#43494 = CARTESIAN_POINT('Ctrl Pts',(-17.9117458665147,-11.4144461163014,
123.239325516368)) ;
#43495 = CARTESIAN_POINT('Ctrl Pts',(-18.2053899399513,-11.6044283742699,
123.48381708741)) ;
#43496 = CARTESIAN_POINT('Ctrl Pts',(-17.9044206322636,-11.424439293907,123.501819128649)) ;
#43497 = CARTESIAN_POINT('Ctrl Pts',(-18.2360155974427,-11.6143740371738,
123.690651541286)) ;
#43498 = CARTESIAN_POINT('Ctrl Pts',(-17.9427031377925,-11.4343849568109,
123.760362733581)) ;
#43499 = CARTESIAN_POINT('Ctrl Pts',(-18.3016977196334,-11.624321333379,123.889202740392)) ;
#43500 = CARTESIAN_POINT('Ctrl Pts',(-18.0248064637638,-11.4443322530161,
124.008552115012)) ;
#43501 = CARTESIAN_POINT('Ctrl Pts',(-18.4020577550734,-11.6343690989569,
124.075068550386)) ;
#43502 = CARTESIAN_POINT('Ctrl Pts',(-18.1502567640289,-11.454380018594,124.240883955143)) ;
#43503 = CARTESIAN_POINT('Ctrl Pts',(-18.53043452236,-11.6442173121745,124.237499635771)) ;
#43504 = CARTESIAN_POINT('Ctrl Pts',(-18.31072897444,-11.4642282318116,124.443923603713)) ;
#43505 = CARTESIAN_POINT('Ctrl Pts',(-18.6863539195395,-11.6541768849686,
124.377247513015)) ;
#43506 = CARTESIAN_POINT('Ctrl Pts',(-18.5056290796381,-11.4741878046057,
124.618608195999)) ;
#43507 = CARTESIAN_POINT('Ctrl Pts',(-18.8657358234262,-11.6642135060011,
124.488337618152)) ;
#43508 = CARTESIAN_POINT('Ctrl Pts',(-18.7298566496538,-11.4842244256382,
124.757470221316)) ;
#43509 = CARTESIAN_POINT('Ctrl Pts',(-19.0585401018813,-11.6740940208114,
124.565687771704)) ;
#43510 = CARTESIAN_POINT('Ctrl Pts',(-18.9708633136617,-11.4941049404486,
124.854157638432)) ;
#43511 = CARTESIAN_POINT('Ctrl Pts',(-19.2653207495063,-11.6841466721185,
124.609197173488)) ;
#43512 = CARTESIAN_POINT('Ctrl Pts',(-19.2293390121453,-11.5041575917556,
124.90854357499)) ;
#43513 = CARTESIAN_POINT('Ctrl Pts',(-19.4732739400485,-11.6940420703985,
124.616120019601)) ;
#43514 = CARTESIAN_POINT('Ctrl Pts',(-19.4892814880954,-11.5140529900356,
124.917196362515)) ;
#43515 = CARTESIAN_POINT('Ctrl Pts',(-19.6824421140478,-11.7040921921046,
124.586475455409)) ;
#43516 = CARTESIAN_POINT('Ctrl Pts',(-19.7507413265183,-11.5241031117417,
124.880139860388)) ;
#43517 = CARTESIAN_POINT('Ctrl Pts',(-19.8800272774462,-11.7139764716465,
124.522061203542)) ;
#43518 = CARTESIAN_POINT('Ctrl Pts',(-19.9977235238706,-11.5339873912836,
124.799620909315)) ;
#43519 = CARTESIAN_POINT('Ctrl Pts',(-20.0656260604384,-11.7239712529384,
124.423592328542)) ;
#43520 = CARTESIAN_POINT('Ctrl Pts',(-20.2297217101426,-11.5439821725755,
124.676533838734)) ;
#43521 = CARTESIAN_POINT('Ctrl Pts',(-20.2305069833902,-11.7339190981252,
124.294916040327)) ;
#43522 = CARTESIAN_POINT('Ctrl Pts',(-20.4358226950316,-11.5539300177623,
124.515687379052)) ;
#43523 = CARTESIAN_POINT('Ctrl Pts',(-20.3705912261117,-11.7438560615126,
124.139963124901)) ;
#43524 = CARTESIAN_POINT('Ctrl Pts',(-20.6109276227123,-11.5638669811497,
124.321995034894)) ;
#43525 = CARTESIAN_POINT('Ctrl Pts',(-20.482403685854,-11.7538390262498,123.962322659801)) ;
#43526 = CARTESIAN_POINT('Ctrl Pts',(-20.7506923359331,-11.5738499458869,
124.099943607919)) ;
#43527 = CARTESIAN_POINT('Ctrl Pts',(-20.5617787036582,-11.7638828776654,
123.766682247549)) ;
#43528 = CARTESIAN_POINT('Ctrl Pts',(-20.8499100759965,-11.5838937973026,
123.855392878857)) ;
#43529 = CARTESIAN_POINT('Ctrl Pts',(-20.6055180822358,-11.7737110790002,
123.564713422646)) ;
#43530 = CARTESIAN_POINT('Ctrl Pts',(-20.9045834153395,-11.5937219986373,
123.60293017781)) ;
#43531 = CARTESIAN_POINT('Ctrl Pts',(-20.6138247387092,-11.7837876515982,
123.353078389392)) ;
#43532 = CARTESIAN_POINT('Ctrl Pts',(-20.9149654649752,-11.6037985712354,
123.338386769837)) ;
#43533 = CARTESIAN_POINT('Ctrl Pts',(-20.5859865681062,-11.7936397316058,
123.147790724545)) ;
#43534 = CARTESIAN_POINT('Ctrl Pts',(-20.8801663077808,-11.6136506512429,
123.081776137432)) ;
#43535 = CARTESIAN_POINT('Ctrl Pts',(-20.5217060175956,-11.8037130166099,
122.94604661898)) ;
#43536 = CARTESIAN_POINT('Ctrl Pts',(-20.7998144512249,-11.623723936247,122.829596800206)) ;
#43537 = CARTESIAN_POINT('Ctrl Pts',(-20.4255657745516,-11.8135543683204,
122.7628267317)) ;
#43538 = CARTESIAN_POINT('Ctrl Pts',(-20.6796373590905,-11.6335652879575,
122.60057140377)) ;
#43539 = CARTESIAN_POINT('Ctrl Pts',(-20.2981587765571,-11.8235158677169,
122.596634860964)) ;
#43540 = CARTESIAN_POINT('Ctrl Pts',(-20.5203770951846,-11.643526787354,122.39283222261)) ;
#43541 = CARTESIAN_POINT('Ctrl Pts',(-20.1424149976007,-11.8335516438469,
122.454293214028)) ;
#43542 = CARTESIAN_POINT('Ctrl Pts',(-20.3256964580967,-11.653562563484,122.21490632929)) ;
#43543 = CARTESIAN_POINT('Ctrl Pts',(-19.9670619376452,-11.8434400704844,
122.342638696447)) ;
#43544 = CARTESIAN_POINT('Ctrl Pts',(-20.1065035192901,-11.6634509901216,
122.07533899432)) ;
#43545 = CARTESIAN_POINT('Ctrl Pts',(-19.7726633460982,-11.8534553925594,
122.261733680716)) ;
#43546 = CARTESIAN_POINT('Ctrl Pts',(-19.8635046295888,-11.6734663121965,
121.974209274979)) ;
#43547 = CARTESIAN_POINT('Ctrl Pts',(-19.5667618955136,-11.8634857414596,
122.216223716099)) ;
#43548 = CARTESIAN_POINT('Ctrl Pts',(-19.6061275734712,-11.6834966610967,
121.917323321599)) ;
#43549 = CARTESIAN_POINT('Ctrl Pts',(-19.3600373542584,-11.8733291170662,
122.206909440911)) ;
#43550 = CARTESIAN_POINT('Ctrl Pts',(-19.3477206075241,-11.6933400367034,
121.905682077823)) ;
#43551 = CARTESIAN_POINT('Ctrl Pts',(-19.150888532225,-11.8833585539634,122.233670381781)) ;
#43552 = CARTESIAN_POINT('Ctrl Pts',(-19.0862848802727,-11.7033694736005,
121.939135039902)) ;
#43553 = CARTESIAN_POINT('Ctrl Pts',(-18.9496827788183,-11.8933904318963,
122.296907578933)) ;
#43554 = CARTESIAN_POINT('Ctrl Pts',(-18.834778258423,-11.7134013515334,122.018183059179)) ;
#43555 = CARTESIAN_POINT('Ctrl Pts',(-18.7661111079611,-11.9032200550018,
122.391777133203)) ;
#43556 = CARTESIAN_POINT('Ctrl Pts',(-18.6053133475109,-11.7232309746389,
122.136772150957)) ;
#43557 = CARTESIAN_POINT('Ctrl Pts',(-18.5987322084384,-11.9132095261549,
122.518627177409)) ;
#43558 = CARTESIAN_POINT('Ctrl Pts',(-18.3960907645237,-11.733220445792,122.295336373572)) ;
#43559 = CARTESIAN_POINT('Ctrl Pts',(-18.4555426602971,-11.9232533749173,
122.673809920536)) ;
#43560 = CARTESIAN_POINT('Ctrl Pts',(-18.2171052463347,-11.7432642945544,
122.489315908043)) ;
#43561 = CARTESIAN_POINT('Ctrl Pts',(-18.3436356389824,-11.933075080449,122.847337567212)) ;
#43562 = CARTESIAN_POINT('Ctrl Pts',(-18.0772224088806,-11.7530860000861,
122.706227559913)) ;
#43563 = CARTESIAN_POINT('Ctrl Pts',(-18.2613427697256,-11.9431101202768,
123.041592805838)) ;
#43564 = CARTESIAN_POINT('Ctrl Pts',(-17.974358275623,-11.7631210399139,122.949047320032)) ;
#43565 = CARTESIAN_POINT('Ctrl Pts',(-18.2146441937951,-11.9531348271682,
123.247112574505)) ;
#43566 = CARTESIAN_POINT('Ctrl Pts',(-17.9159869176276,-11.7731457468054,
123.205947428722)) ;
#43567 = CARTESIAN_POINT('Ctrl Pts',(-18.2040790572873,-11.962987531509,123.453976992299)) ;
#43568 = CARTESIAN_POINT('Ctrl Pts',(-17.9027824760765,-11.7829984511461,
123.464529062484)) ;
#43569 = CARTESIAN_POINT('Ctrl Pts',(-18.2295779813126,-11.9729756537167,
123.662389605254)) ;
#43570 = CARTESIAN_POINT('Ctrl Pts',(-17.9346582755181,-11.7929865733538,
123.72504475189)) ;
#43571 = CARTESIAN_POINT('Ctrl Pts',(-18.2905062794645,-11.982904123824,123.862032052655)) ;
#43572 = CARTESIAN_POINT('Ctrl Pts',(-18.0108208430666,-11.8029150434611,
123.974597684985)) ;
#43573 = CARTESIAN_POINT('Ctrl Pts',(-18.3854419619658,-11.9928931009912,
124.049358952293)) ;
#43574 = CARTESIAN_POINT('Ctrl Pts',(-18.129492517191,-11.8129040206283,124.20875545915)) ;
#43575 = CARTESIAN_POINT('Ctrl Pts',(-18.51235689706,-12.0029309082709,124.217948281748)) ;
#43576 = CARTESIAN_POINT('Ctrl Pts',(-18.2881378411285,-11.822941827908,124.419490767607)) ;
#43577 = CARTESIAN_POINT('Ctrl Pts',(-18.6634476701596,-12.0127772091342,
124.359445076949)) ;
#43578 = CARTESIAN_POINT('Ctrl Pts',(-18.4770035096972,-11.8327881287713,
124.596360779214)) ;
#43579 = CARTESIAN_POINT('Ctrl Pts',(-18.8397147754035,-12.0228029525135,
124.475014140463)) ;
#43580 = CARTESIAN_POINT('Ctrl Pts',(-18.6973386411338,-11.8428138721506,
124.740820127041)) ;
#43581 = CARTESIAN_POINT('Ctrl Pts',(-19.03368933323,-12.0328338189525,124.557760416671)) ;
#43582 = CARTESIAN_POINT('Ctrl Pts',(-18.9398076657194,-11.8528447385896,
124.844250930531)) ;
#43583 = CARTESIAN_POINT('Ctrl Pts',(-19.2350138531615,-12.0426711777513,
124.605047798355)) ;
#43584 = CARTESIAN_POINT('Ctrl Pts',(-19.1914647637144,-11.8626820973884,
124.903358127309)) ;
#43585 = CARTESIAN_POINT('Ctrl Pts',(-19.4447121805973,-12.052663138685,124.61740552715)) ;
#43586 = CARTESIAN_POINT('Ctrl Pts',(-19.4535879451844,-11.8726740583222,
124.918802859843)) ;
#43587 = CARTESIAN_POINT('Ctrl Pts',(-19.654174209039,-12.0626955012416,124.59264506007)) ;
#43588 = CARTESIAN_POINT('Ctrl Pts',(-19.7154151681285,-11.8827064208787,
124.887849956679)) ;
#43589 = CARTESIAN_POINT('Ctrl Pts',(-19.8528431822894,-12.072560661816,124.53314903407)) ;
#43590 = CARTESIAN_POINT('Ctrl Pts',(-19.9637513981786,-11.8925715814531,
124.813477415096)) ;
#43591 = CARTESIAN_POINT('Ctrl Pts',(-20.0402625333132,-12.0825225663937,
124.439673578487)) ;
#43592 = CARTESIAN_POINT('Ctrl Pts',(-20.1980246864583,-11.9025334860308,
124.696630723348)) ;
#43593 = CARTESIAN_POINT('Ctrl Pts',(-20.2096190237234,-12.0925574964694,
124.313895264945)) ;
#43594 = CARTESIAN_POINT('Ctrl Pts',(-20.4097188088187,-11.9125684161065,
124.539405883131)) ;
#43595 = CARTESIAN_POINT('Ctrl Pts',(-20.3526800116948,-12.102442443323,124.163124144137)) ;
#43596 = CARTESIAN_POINT('Ctrl Pts',(-20.5885436050965,-11.9224533629601,
124.350939834724)) ;
#43597 = CARTESIAN_POINT('Ctrl Pts',(-20.4694104296519,-12.1125081196345,
123.986661950019)) ;
#43598 = CARTESIAN_POINT('Ctrl Pts',(-20.7344544461953,-11.9325190392716,
124.130360829596)) ;
#43599 = CARTESIAN_POINT('Ctrl Pts',(-20.5520515995571,-12.1223470392694,
123.797005493285)) ;
#43600 = CARTESIAN_POINT('Ctrl Pts',(-20.8377538535721,-11.9423579589065,
123.89328858742)) ;
#43601 = CARTESIAN_POINT('Ctrl Pts',(-20.6018640316816,-12.1324105490038,
123.591417354039)) ;
#43602 = CARTESIAN_POINT('Ctrl Pts',(-20.9000168313516,-11.9524214686409,
123.636302931589)) ;
#43603 = CARTESIAN_POINT('Ctrl Pts',(-20.6148291614051,-12.1423041621656,
123.383802604213)) ;
#43604 = CARTESIAN_POINT('Ctrl Pts',(-20.9162207081352,-11.9623150818027,
123.376783859036)) ;
#43605 = CARTESIAN_POINT('Ctrl Pts',(-20.5919863900176,-12.152248168979,123.176028489943)) ;
#43606 = CARTESIAN_POINT('Ctrl Pts',(-20.8876645643203,-11.9722590886161,
123.117066234101)) ;
#43607 = CARTESIAN_POINT('Ctrl Pts',(-20.5331562624697,-12.1622491233333,
122.974141880329)) ;
#43608 = CARTESIAN_POINT('Ctrl Pts',(-20.8141243155986,-11.9822600429704,
122.8647086418)) ;
#43609 = CARTESIAN_POINT('Ctrl Pts',(-20.4394990832698,-12.1722878810256,
122.785036123018)) ;
#43610 = CARTESIAN_POINT('Ctrl Pts',(-20.6970504996991,-11.9922988006627,
122.628327621003)) ;
#43611 = CARTESIAN_POINT('Ctrl Pts',(-20.3174467550257,-12.1821120651956,
122.618401426981)) ;
#43612 = CARTESIAN_POINT('Ctrl Pts',(-20.5444825751892,-12.0021229848327,
122.420035361004)) ;
#43613 = CARTESIAN_POINT('Ctrl Pts',(-20.1650056351834,-12.192170130795,122.471888778406)) ;
#43614 = CARTESIAN_POINT('Ctrl Pts',(-20.3539293395536,-12.0121810504321,
122.236896566325)) ;
#43615 = CARTESIAN_POINT('Ctrl Pts',(-19.9914963261328,-12.2021001775697,
122.355781356402)) ;
#43616 = CARTESIAN_POINT('Ctrl Pts',(-20.1370409747147,-12.0221110972068,
122.091764368012)) ;
#43617 = CARTESIAN_POINT('Ctrl Pts',(-19.8002835579305,-12.2120516199068,
122.270882760811)) ;
#43618 = CARTESIAN_POINT('Ctrl Pts',(-19.8980237231667,-12.0320625395439,
121.985643564698)) ;
#43619 = CARTESIAN_POINT('Ctrl Pts',(-19.5952237413981,-12.2220984170861,
122.220273264171)) ;
#43620 = CARTESIAN_POINT('Ctrl Pts',(-19.6416983085707,-12.0421093367232,
121.922384338977)) ;
#43621 = CARTESIAN_POINT('Ctrl Pts',(-19.388673024252,-12.2319463577662,122.206126303153)) ;
#43622 = CARTESIAN_POINT('Ctrl Pts',(-19.3835093232675,-12.0519572774033,
121.904703348343)) ;
#43623 = CARTESIAN_POINT('Ctrl Pts',(-19.180367514707,-12.2419079891088,122.227663750523)) ;
#43624 = CARTESIAN_POINT('Ctrl Pts',(-19.1231275997313,-12.0619189087459,
121.931627958287)) ;
#43625 = CARTESIAN_POINT('Ctrl Pts',(-18.9776624918692,-12.2519366484847,
122.285690175812)) ;
#43626 = CARTESIAN_POINT('Ctrl Pts',(-18.8697470442625,-12.0719475681218,
122.004163670847)) ;
#43627 = CARTESIAN_POINT('Ctrl Pts',(-18.7903389023048,-12.2618469513729,
122.376871314838)) ;
#43628 = CARTESIAN_POINT('Ctrl Pts',(-18.6355935850335,-12.08185787101,122.118142693142)) ;
#43629 = CARTESIAN_POINT('Ctrl Pts',(-18.6209407245683,-12.2717818459351,
122.499062432989)) ;
#43630 = CARTESIAN_POINT('Ctrl Pts',(-18.4238474019827,-12.0917927655722,
122.270883953054)) ;
#43631 = CARTESIAN_POINT('Ctrl Pts',(-18.4739251947791,-12.281822944602,122.650538595866)) ;
#43632 = CARTESIAN_POINT('Ctrl Pts',(-18.2400799717895,-12.1018338642391,
122.460231143199)) ;
#43633 = CARTESIAN_POINT('Ctrl Pts',(-18.3571294374524,-12.2917102271064,
122.822498446866)) ;
#43634 = CARTESIAN_POINT('Ctrl Pts',(-18.0940875093298,-12.1117211467435,
122.675182672206)) ;
#43635 = CARTESIAN_POINT('Ctrl Pts',(-18.270751539422,-12.3017019676169,123.013960222828)) ;
#43636 = CARTESIAN_POINT('Ctrl Pts',(-17.9861176823212,-12.121712887254,122.914511116819)) ;
#43637 = CARTESIAN_POINT('Ctrl Pts',(-18.2192070084759,-12.3116525168523,
123.216713043698)) ;
#43638 = CARTESIAN_POINT('Ctrl Pts',(-17.921689729601,-12.1316634364894,123.16795292873)) ;
#43639 = CARTESIAN_POINT('Ctrl Pts',(-18.203364387181,-12.3215881944871,123.424977839185)) ;
#43640 = CARTESIAN_POINT('Ctrl Pts',(-17.9018892648507,-12.1415991141242,
123.428284203218)) ;
#43641 = CARTESIAN_POINT('Ctrl Pts',(-18.2238062767761,-12.3315736122799,
123.63392140019)) ;
#43642 = CARTESIAN_POINT('Ctrl Pts',(-17.9274444398076,-12.151584531917,123.689463440879)) ;
#43643 = CARTESIAN_POINT('Ctrl Pts',(-18.2807096673845,-12.3416024051504,
123.83693264531)) ;
#43644 = CARTESIAN_POINT('Ctrl Pts',(-17.9985764205707,-12.1616133247875,
123.943226816736)) ;
#43645 = CARTESIAN_POINT('Ctrl Pts',(-18.3704393887249,-12.3514819163783,
124.024245376824)) ;
#43646 = CARTESIAN_POINT('Ctrl Pts',(-18.1107411250608,-12.1714928360155,
124.177366527378)) ;
#43647 = CARTESIAN_POINT('Ctrl Pts',(-18.4923386110279,-12.3614754530513,
124.195371559684)) ;
#43648 = CARTESIAN_POINT('Ctrl Pts',(-18.263117466536,-12.1814863726884,124.391272663474)) ;
#43649 = CARTESIAN_POINT('Ctrl Pts',(-18.6429752247149,-12.3715077213151,
124.342978657029)) ;
#43650 = CARTESIAN_POINT('Ctrl Pts',(-18.4514152853576,-12.1915186409522,
124.575779592005)) ;
#43651 = CARTESIAN_POINT('Ctrl Pts',(-18.8138083567616,-12.381371683321,124.460571682728)) ;
#43652 = CARTESIAN_POINT('Ctrl Pts',(-18.6649582254987,-12.2013826029581,
124.722768521293)) ;
#43653 = CARTESIAN_POINT('Ctrl Pts',(-19.0063512318433,-12.3914417446659,
124.548529857693)) ;
#43654 = CARTESIAN_POINT('Ctrl Pts',(-18.9056381213548,-12.211452664303,124.832713751572)) ;
#43655 = CARTESIAN_POINT('Ctrl Pts',(-19.2066412567903,-12.4012841090146,
124.600516981642)) ;
#43656 = CARTESIAN_POINT('Ctrl Pts',(-19.1560012005742,-12.2212950286517,
124.897694900574)) ;
#43657 = CARTESIAN_POINT('Ctrl Pts',(-19.4153191948693,-12.4112447815171,
124.61790415066)) ;
#43658 = CARTESIAN_POINT('Ctrl Pts',(-19.4168488001017,-12.2312557011542,
124.919426126704)) ;
#43659 = CARTESIAN_POINT('Ctrl Pts',(-19.6254227673264,-12.4212828525849,
124.598226325567)) ;
#43660 = CARTESIAN_POINT('Ctrl Pts',(-19.6794781670334,-12.241293772222,124.894826056415)) ;
#43661 = CARTESIAN_POINT('Ctrl Pts',(-19.8257277780076,-12.4311564675453,
124.54365478677)) ;
#43662 = CARTESIAN_POINT('Ctrl Pts',(-19.9298584470305,-12.2511673871824,
124.826609084731)) ;
#43663 = CARTESIAN_POINT('Ctrl Pts',(-20.0172039066253,-12.4412287021266,
124.453332611574)) ;
#43664 = CARTESIAN_POINT('Ctrl Pts',(-20.1692027685541,-12.2612396217637,
124.713703674863)) ;
#43665 = CARTESIAN_POINT('Ctrl Pts',(-20.1860304534501,-12.4510527205754,
124.334292333234)) ;
#43666 = CARTESIAN_POINT('Ctrl Pts',(-20.3802336084559,-12.2710636402125,
124.56490174156)) ;
#43667 = CARTESIAN_POINT('Ctrl Pts',(-20.3353241205461,-12.4611176415514,
124.184411186943)) ;
#43668 = CARTESIAN_POINT('Ctrl Pts',(-20.5668505339034,-12.2811285611885,
124.3775468474)) ;
#43669 = CARTESIAN_POINT('Ctrl Pts',(-20.4942292788694,-12.4743279398461,
123.956554640027)) ;
#43670 = CARTESIAN_POINT('Ctrl Pts',(-20.7654710388387,-12.2943388594833,
124.092731380698)) ;
#43671 = CARTESIAN_POINT('Ctrl Pts',(-20.5910323234022,-12.4876433865781,
123.690569761034)) ;
#43672 = CARTESIAN_POINT('Ctrl Pts',(-20.8864681734945,-12.3076543062152,
123.760293059331)) ;
#43673 = CARTESIAN_POINT('Ctrl Pts',(-20.6153241142933,-12.5009336318454,
123.412181900129)) ;
#43674 = CARTESIAN_POINT('Ctrl Pts',(-20.9168412402485,-12.3209445514825,
123.412248798329)) ;
#43675 = CARTESIAN_POINT('Ctrl Pts',(-20.5967460044986,-12.5109843814525,
123.20173674764)) ;
#43676 = CARTESIAN_POINT('Ctrl Pts',(-20.8936136564304,-12.3309953010896,
123.149204261583)) ;
#43677 = CARTESIAN_POINT('Ctrl Pts',(-20.5435845802291,-12.5207969884347,
123.002381741764)) ;
#43678 = CARTESIAN_POINT('Ctrl Pts',(-20.8271599100472,-12.3408079080718,
122.900008574106)) ;
#43679 = CARTESIAN_POINT('Ctrl Pts',(-20.4546049045706,-12.530868086429,122.81028950204)) ;
#43680 = CARTESIAN_POINT('Ctrl Pts',(-20.7159339872492,-12.3508790060661,
122.659895486434)) ;
#43681 = CARTESIAN_POINT('Ctrl Pts',(-20.3356089336191,-12.5407576592038,
122.639785901111)) ;
#43682 = CARTESIAN_POINT('Ctrl Pts',(-20.5671825471141,-12.360768578841,122.446765213332)) ;
#43683 = CARTESIAN_POINT('Ctrl Pts',(-20.1392326312349,-12.5540277660071,
122.441591528531)) ;
#43684 = CARTESIAN_POINT('Ctrl Pts',(-20.3217335957846,-12.3740386856443,
122.199036770175)) ;
#43685 = CARTESIAN_POINT('Ctrl Pts',(-19.8341063016993,-12.5706444529296,
122.263562945351)) ;
#43686 = CARTESIAN_POINT('Ctrl Pts',(-19.9402799223287,-12.3906553725668,
121.976489963183)) ;
#43687 = CARTESIAN_POINT('Ctrl Pts',(-19.4873858216236,-12.5872184962459,
122.20023473755)) ;
#43688 = CARTESIAN_POINT('Ctrl Pts',(-19.5069560654083,-12.407229415883,121.897341845887)) ;
#43689 = CARTESIAN_POINT('Ctrl Pts',(-19.208770852032,-12.6005150636777,122.222555120843)) ;
#43690 = CARTESIAN_POINT('Ctrl Pts',(-19.1586250796142,-12.4205259833148,
121.925240968701)) ;
#43691 = CARTESIAN_POINT('Ctrl Pts',(-19.004699994285,-12.6105451272551,122.27569208682)) ;
#43692 = CARTESIAN_POINT('Ctrl Pts',(-18.9035497915594,-12.4305560468922,
121.991664800906)) ;
#43693 = CARTESIAN_POINT('Ctrl Pts',(-18.8155802354143,-12.6204390191043,
122.362230085653)) ;
#43694 = CARTESIAN_POINT('Ctrl Pts',(-18.6671468529052,-12.4404499387414,
122.099840645972)) ;
#43695 = CARTESIAN_POINT('Ctrl Pts',(-18.5855888789982,-12.6336917748899,
122.519603205496)) ;
#43696 = CARTESIAN_POINT('Ctrl Pts',(-18.3796682061191,-12.453702694527,122.296549637466)) ;
#43697 = CARTESIAN_POINT('Ctrl Pts',(-18.354522049861,-12.6504198798823,122.789922613237)) ;
#43698 = CARTESIAN_POINT('Ctrl Pts',(-18.0908280313655,-12.4704307995194,
122.634462100718)) ;
#43699 = CARTESIAN_POINT('Ctrl Pts',(-18.2063394457701,-12.6702507163608,
123.184767083892)) ;
#43700 = CARTESIAN_POINT('Ctrl Pts',(-17.9056069777788,-12.4902616359979,
123.128014485523)) ;
#43701 = CARTESIAN_POINT('Ctrl Pts',(-18.2007363155492,-12.690176108251,123.608303510177)) ;
#43702 = CARTESIAN_POINT('Ctrl Pts',(-17.8986058474029,-12.5101870278881,
123.65743523967)) ;
#43703 = CARTESIAN_POINT('Ctrl Pts',(-18.3400998829644,-12.710101321603,124.008460954811)) ;
#43704 = CARTESIAN_POINT('Ctrl Pts',(-18.0728134812496,-12.5301122412401,
124.157630024429)) ;
#43705 = CARTESIAN_POINT('Ctrl Pts',(-18.6074924622381,-12.7300263350881,
124.337014382701)) ;
#43706 = CARTESIAN_POINT('Ctrl Pts',(-18.4070561283902,-12.5500372547252,
124.568319257347)) ;
#43707 = CARTESIAN_POINT('Ctrl Pts',(-18.9698313696597,-12.7499028067881,
124.554607895198)) ;
#43708 = CARTESIAN_POINT('Ctrl Pts',(-18.8599799731256,-12.5699137264252,
124.840308096966)) ;
#43709 = CARTESIAN_POINT('Ctrl Pts',(-19.3867523160162,-12.7698821246969,
124.636089846791)) ;
#43710 = CARTESIAN_POINT('Ctrl Pts',(-19.3811313633293,-12.5898930443341,
124.942158139695)) ;
#43711 = CARTESIAN_POINT('Ctrl Pts',(-19.8054691433214,-12.7898151282729,
124.570240660478)) ;
#43712 = CARTESIAN_POINT('Ctrl Pts',(-19.9045262603243,-12.6098260479101,
124.859844414469)) ;
#43713 = CARTESIAN_POINT('Ctrl Pts',(-20.1760444374323,-12.8097103983006,
124.366269150013)) ;
#43714 = CARTESIAN_POINT('Ctrl Pts',(-20.3677432424192,-12.6297213179378,
124.6048789893)) ;
#43715 = CARTESIAN_POINT('Ctrl Pts',(-20.4554911510886,-12.8296317362065,
124.047921898696)) ;
#43716 = CARTESIAN_POINT('Ctrl Pts',(-20.7170498595964,-12.6496426558436,
124.206944794287)) ;
#43717 = CARTESIAN_POINT('Ctrl Pts',(-20.6097246596929,-12.8495893594727,
123.652566976865)) ;
#43718 = CARTESIAN_POINT('Ctrl Pts',(-20.9098403565593,-12.6696002791098,
123.712751204342)) ;
#43719 = CARTESIAN_POINT('Ctrl Pts',(-20.6198419912611,-12.8694691914299,
123.23005419397)) ;
#43720 = CARTESIAN_POINT('Ctrl Pts',(-20.922485985003,-12.689480111067,123.18461209717)) ;
#43721 = CARTESIAN_POINT('Ctrl Pts',(-20.4862162340303,-12.8893510427268,
122.828900869269)) ;
#43722 = CARTESIAN_POINT('Ctrl Pts',(-20.7554545445051,-12.7093619623639,
122.683172172836)) ;
#43723 = CARTESIAN_POINT('Ctrl Pts',(-20.2206736454974,-12.9094220598306,
122.494883082429)) ;
#43724 = CARTESIAN_POINT('Ctrl Pts',(-20.4235254244291,-12.7294329794677,
122.265649141046)) ;
#43725 = CARTESIAN_POINT('Ctrl Pts',(-19.8617901510047,-12.9292292835837,
122.274337723655)) ;
#43726 = CARTESIAN_POINT('Ctrl Pts',(-19.9749237655201,-12.7492402032208,
121.989968961482)) ;
#43727 = CARTESIAN_POINT('Ctrl Pts',(-19.4458827143192,-12.9492104191524,
122.187802603992)) ;
#43728 = CARTESIAN_POINT('Ctrl Pts',(-19.4550399386783,-12.7692213387896,
121.881799009553)) ;
#43729 = CARTESIAN_POINT('Ctrl Pts',(-19.0266575984833,-12.9691379124917,
122.249044591949)) ;
#43730 = CARTESIAN_POINT('Ctrl Pts',(-18.9310095255676,-12.7891488321288,
121.958350587305)) ;
#43731 = CARTESIAN_POINT('Ctrl Pts',(-18.6546793341104,-12.9889585738495,
122.447395484881)) ;
#43732 = CARTESIAN_POINT('Ctrl Pts',(-18.4660378435683,-12.8089694934866,
122.206286369213)) ;
#43733 = CARTESIAN_POINT('Ctrl Pts',(-18.3694697209431,-13.0090557630713,
122.765395487489)) ;
#43734 = CARTESIAN_POINT('Ctrl Pts',(-18.1095237058468,-12.8290666827084,
122.603786127405)) ;
#43735 = CARTESIAN_POINT('Ctrl Pts',(-18.2121462510153,-13.0288194420796,
123.155285689063)) ;
#43736 = CARTESIAN_POINT('Ctrl Pts',(-17.9128685242105,-12.8488303617167,
123.091145395877)) ;
#43737 = CARTESIAN_POINT('Ctrl Pts',(-18.1966161351743,-13.0488767207527,
123.581287391373)) ;
#43738 = CARTESIAN_POINT('Ctrl Pts',(-17.8934532250118,-12.8688876403898,
123.623648070234)) ;
#43739 = CARTESIAN_POINT('Ctrl Pts',(-18.3260055582142,-13.0686721445001,
123.981930815811)) ;
#43740 = CARTESIAN_POINT('Ctrl Pts',(-18.0551868058746,-12.8886830641372,
124.124451004221)) ;
#43741 = CARTESIAN_POINT('Ctrl Pts',(-18.585401546907,-13.0886357892277,124.317872249246)) ;
#43742 = CARTESIAN_POINT('Ctrl Pts',(-18.3794288064129,-12.9086467088648,
124.544379679826)) ;
#43743 = CARTESIAN_POINT('Ctrl Pts',(-18.9448204747835,-13.1086192805018,
124.544510743668)) ;
#43744 = CARTESIAN_POINT('Ctrl Pts',(-18.8287006511552,-12.9286302001389,
124.827680379695)) ;
#43745 = CARTESIAN_POINT('Ctrl Pts',(-19.3561968961379,-13.1284267756511,
124.634949141891)) ;
#43746 = CARTESIAN_POINT('Ctrl Pts',(-19.3429186866301,-12.9484376952882,
124.94073161998)) ;
#43747 = CARTESIAN_POINT('Ctrl Pts',(-19.7773691623945,-13.1484093663712,
124.579587344744)) ;
#43748 = CARTESIAN_POINT('Ctrl Pts',(-19.8693844497185,-12.9684202860083,
124.871533418394)) ;
#43749 = CARTESIAN_POINT('Ctrl Pts',(-20.1526165065807,-13.1682920203624,
124.384654627234)) ;
#43750 = CARTESIAN_POINT('Ctrl Pts',(-20.3384447754671,-12.9883029399995,
124.627871581349)) ;
#43751 = CARTESIAN_POINT('Ctrl Pts',(-20.4400164199857,-13.1882502652255,
124.072540016501)) ;
#43752 = CARTESIAN_POINT('Ctrl Pts',(-20.6976976848122,-13.0082611848626,
124.237731507644)) ;
#43753 = CARTESIAN_POINT('Ctrl Pts',(-20.6032765964651,-13.2081258522671,
123.682670644288)) ;
#43754 = CARTESIAN_POINT('Ctrl Pts',(-20.9017768869257,-13.0281367719042,
123.750397269444)) ;
#43755 = CARTESIAN_POINT('Ctrl Pts',(-20.6240984710499,-13.2281067404023,
123.258361807286)) ;
#43756 = CARTESIAN_POINT('Ctrl Pts',(-20.9278087943981,-13.0481176600395,
123.220011471926)) ;
#43757 = CARTESIAN_POINT('Ctrl Pts',(-20.498818644834,-13.2480418815133,122.853364041742)) ;
#43758 = CARTESIAN_POINT('Ctrl Pts',(-20.7712144053819,-13.0680528011505,
122.713763278227)) ;
#43759 = CARTESIAN_POINT('Ctrl Pts',(-20.2434545299471,-13.2679538995244,
122.515712779495)) ;
#43760 = CARTESIAN_POINT('Ctrl Pts',(-20.4520106816014,-13.0879648191615,
122.291696114272)) ;
#43761 = CARTESIAN_POINT('Ctrl Pts',(-19.8888180187742,-13.287842117768,122.285335601894)) ;
#43762 = CARTESIAN_POINT('Ctrl Pts',(-20.0087285877316,-13.1078530374051,
122.003722192709)) ;
#43763 = CARTESIAN_POINT('Ctrl Pts',(-19.5451472567373,-13.3044404216149,
122.205327702706)) ;
#43764 = CARTESIAN_POINT('Ctrl Pts',(-19.5791090604564,-13.124451341252,121.903703056221)) ;
#43765 = CARTESIAN_POINT('Ctrl Pts',(-19.2662111497509,-13.3177130115177,
122.214345970221)) ;
#43766 = CARTESIAN_POINT('Ctrl Pts',(-19.2304680801455,-13.1377239311548,
121.914976366624)) ;
#43767 = CARTESIAN_POINT('Ctrl Pts',(-19.0602727562378,-13.3277204264686,
122.257344197933)) ;
#43768 = CARTESIAN_POINT('Ctrl Pts',(-18.9730360739325,-13.1477313461057,
121.968723010403)) ;
#43769 = CARTESIAN_POINT('Ctrl Pts',(-18.8649743558658,-13.3377277732012,
122.335630979356)) ;
#43770 = CARTESIAN_POINT('Ctrl Pts',(-18.7289237747832,-13.1577386928383,
122.066570256317)) ;
#43771 = CARTESIAN_POINT('Ctrl Pts',(-18.6279877995192,-13.3509941330028,
122.482594738179)) ;
#43772 = CARTESIAN_POINT('Ctrl Pts',(-18.4326373531694,-13.1710050526399,
122.250316913842)) ;
#43773 = CARTESIAN_POINT('Ctrl Pts',(-18.38714068302,-13.3675087906257,122.738147005354)) ;
#43774 = CARTESIAN_POINT('Ctrl Pts',(-18.1316373287835,-13.1875197102629,
122.569692622284)) ;
#43775 = CARTESIAN_POINT('Ctrl Pts',(-18.2465546320846,-13.3841062238684,
123.06176278507)) ;
#43776 = CARTESIAN_POINT('Ctrl Pts',(-17.9558681007045,-13.2041171435055,
122.974265631492)) ;
#43777 = CARTESIAN_POINT('Ctrl Pts',(-18.2054801703779,-13.3974542210134,
123.339422999475)) ;
#43778 = CARTESIAN_POINT('Ctrl Pts',(-17.9045373896821,-13.2174651406505,
123.321302564893)) ;
#43779 = CARTESIAN_POINT('Ctrl Pts',(-18.2109540995371,-13.407349975365,123.547385217031)) ;
#43780 = CARTESIAN_POINT('Ctrl Pts',(-17.9113737957956,-13.2273608950021,
123.581262925382)) ;
#43781 = CARTESIAN_POINT('Ctrl Pts',(-18.2525836667426,-13.4173379292963,
123.753181102987)) ;
#43782 = CARTESIAN_POINT('Ctrl Pts',(-17.9634088821012,-13.2373488489335,
123.838506352538)) ;
#43783 = CARTESIAN_POINT('Ctrl Pts',(-18.3290068072186,-13.4272951530011,
123.948090648861)) ;
#43784 = CARTESIAN_POINT('Ctrl Pts',(-18.0589349739684,-13.2473060726382,
124.082144873651)) ;
#43785 = CARTESIAN_POINT('Ctrl Pts',(-18.4390335780382,-13.4373306995577,
124.128090732076)) ;
#43786 = CARTESIAN_POINT('Ctrl Pts',(-18.1964661586106,-13.2573416191949,
124.307146372465)) ;
#43787 = CARTESIAN_POINT('Ctrl Pts',(-18.576478403772,-13.4472178108339,124.284038519252)) ;
#43788 = CARTESIAN_POINT('Ctrl Pts',(-18.3682700533626,-13.267228730471,124.502082982706)) ;
#43789 = CARTESIAN_POINT('Ctrl Pts',(-18.7403986017361,-13.4572092159347,
124.415367414347)) ;
#43790 = CARTESIAN_POINT('Ctrl Pts',(-18.573168600081,-13.2772201355718,124.666246335832)) ;
#43791 = CARTESIAN_POINT('Ctrl Pts',(-18.9238269690954,-13.4671548371495,
124.515725679001)) ;
#43792 = CARTESIAN_POINT('Ctrl Pts',(-18.8024527486924,-13.2871657567866,
124.791696662128)) ;
#43793 = CARTESIAN_POINT('Ctrl Pts',(-19.1218420695638,-13.4771040854178,
124.583140773883)) ;
#43794 = CARTESIAN_POINT('Ctrl Pts',(-19.0499707909462,-13.2971150050549,
124.87596822317)) ;
#43795 = CARTESIAN_POINT('Ctrl Pts',(-19.3305917291493,-13.4871505805864,
124.615215322897)) ;
#43796 = CARTESIAN_POINT('Ctrl Pts',(-19.3109074952385,-13.3071615002235,
124.91606420447)) ;
#43797 = CARTESIAN_POINT('Ctrl Pts',(-19.5376622730773,-13.4970019233779,
124.610852955936)) ;
#43798 = CARTESIAN_POINT('Ctrl Pts',(-19.5697458477253,-13.3170128430151,
124.910614060128)) ;
#43799 = CARTESIAN_POINT('Ctrl Pts',(-19.7433819757979,-13.5069737035053,
124.570637442649)) ;
#43800 = CARTESIAN_POINT('Ctrl Pts',(-19.8268961278364,-13.3269846231424,
124.86034740168)) ;
#43801 = CARTESIAN_POINT('Ctrl Pts',(-19.9394995576033,-13.516968903483,124.495094530682)) ;
#43802 = CARTESIAN_POINT('Ctrl Pts',(-20.0720441858723,-13.3369798231201,
124.765921346646)) ;
#43803 = CARTESIAN_POINT('Ctrl Pts',(-20.1200428835865,-13.527002895179,124.386031569206)) ;
#43804 = CARTESIAN_POINT('Ctrl Pts',(-20.2977248332106,-13.3470138148161,
124.629595035348)) ;
#43805 = CARTESIAN_POINT('Ctrl Pts',(-20.2763242405218,-13.5368583001515,
124.249969630593)) ;
#43806 = CARTESIAN_POINT('Ctrl Pts',(-20.4930785404264,-13.3568692197886,
124.459519571124)) ;
#43807 = CARTESIAN_POINT('Ctrl Pts',(-20.4086965221813,-13.5468575979973,
124.086710547082)) ;
#43808 = CARTESIAN_POINT('Ctrl Pts',(-20.6585461151986,-13.3668685176344,
124.255447402342)) ;
#43809 = CARTESIAN_POINT('Ctrl Pts',(-20.5098783796781,-13.5567527106025,
123.904908826794)) ;
#43810 = CARTESIAN_POINT('Ctrl Pts',(-20.7850259763668,-13.3767636302396,
124.028196369691)) ;
#43811 = CARTESIAN_POINT('Ctrl Pts',(-20.5790528982995,-13.5668133561375,
123.705062953625)) ;
#43812 = CARTESIAN_POINT('Ctrl Pts',(-20.8714967332555,-13.3868242757746,
123.778389961119)) ;
#43813 = CARTESIAN_POINT('Ctrl Pts',(-20.6118978850877,-13.5766622331267,
123.500614031643)) ;
#43814 = CARTESIAN_POINT('Ctrl Pts',(-20.9125557494614,-13.3966731527638,
123.522828864941)) ;
#43815 = CARTESIAN_POINT('Ctrl Pts',(-20.6092193159514,-13.5866909442203,
123.289798847138)) ;
#43816 = CARTESIAN_POINT('Ctrl Pts',(-20.9092102411542,-13.4067018638574,
123.259309807964)) ;
#43817 = CARTESIAN_POINT('Ctrl Pts',(-20.5694097322058,-13.5967203454764,
123.082737299415)) ;
#43818 = CARTESIAN_POINT('Ctrl Pts',(-20.8594509750379,-13.4167312651135,
123.00048234628)) ;
#43819 = CARTESIAN_POINT('Ctrl Pts',(-20.4961008853216,-13.6065605372724,
122.889286624956)) ;
#43820 = CARTESIAN_POINT('Ctrl Pts',(-20.7678172835609,-13.4265714569095,
122.758667592175)) ;
#43821 = CARTESIAN_POINT('Ctrl Pts',(-20.3889086577013,-13.6165639664654,
122.708376154055)) ;
#43822 = CARTESIAN_POINT('Ctrl Pts',(-20.6338292437046,-13.4365748861025,
122.532528063033)) ;
#43823 = CARTESIAN_POINT('Ctrl Pts',(-20.2520895253684,-13.6265494789316,
122.549112630056)) ;
#43824 = CARTESIAN_POINT('Ctrl Pts',(-20.4628072717642,-13.4465603985687,
122.333446821148)) ;
#43825 = CARTESIAN_POINT('Ctrl Pts',(-20.0887000777735,-13.6365905753156,
122.415484766701)) ;
#43826 = CARTESIAN_POINT('Ctrl Pts',(-20.258572195235,-13.4566014949527,122.16640991458)) ;
#43827 = CARTESIAN_POINT('Ctrl Pts',(-19.9083265613386,-13.6464337712666,
122.314020661915)) ;
#43828 = CARTESIAN_POINT('Ctrl Pts',(-20.0331061121126,-13.4664446909037,
122.03957718795)) ;
#43829 = CARTESIAN_POINT('Ctrl Pts',(-19.7104267761794,-13.656420082321,122.244041727144)) ;
#43830 = CARTESIAN_POINT('Ctrl Pts',(-19.7857320971472,-13.4764310019581,
121.952101012445)) ;
#43831 = CARTESIAN_POINT('Ctrl Pts',(-19.5044018483537,-13.6663547675787,
122.209514866081)) ;
#43832 = CARTESIAN_POINT('Ctrl Pts',(-19.5282010411868,-13.4863656872158,
121.908939847016)) ;
#43833 = CARTESIAN_POINT('Ctrl Pts',(-19.2929999960134,-13.6764123287957,
122.211492627575)) ;
#43834 = CARTESIAN_POINT('Ctrl Pts',(-19.2639488168614,-13.4964232484328,
121.911409438826)) ;
#43835 = CARTESIAN_POINT('Ctrl Pts',(-19.0899192604328,-13.6862339704043,
122.248938878938)) ;
#43836 = CARTESIAN_POINT('Ctrl Pts',(-19.0100966675528,-13.5062448900414,
121.958214888149)) ;
#43837 = CARTESIAN_POINT('Ctrl Pts',(-18.8917066678072,-13.6962900339953,
122.32241535315)) ;
#43838 = CARTESIAN_POINT('Ctrl Pts',(-18.7623301682284,-13.5163009536324,
122.050058119956)) ;
#43839 = CARTESIAN_POINT('Ctrl Pts',(-18.711524790799,-13.7062307097571,122.428304767284)) ;
#43840 = CARTESIAN_POINT('Ctrl Pts',(-18.5371012425962,-13.5262416293942,
122.182417857288)) ;
#43841 = CARTESIAN_POINT('Ctrl Pts',(-18.5526279674509,-13.7161350685454,
122.562874462865)) ;
#43842 = CARTESIAN_POINT('Ctrl Pts',(-18.338478245611,-13.5361459881825,122.350628473911)) ;
#43843 = CARTESIAN_POINT('Ctrl Pts',(-18.4177132106572,-13.7261817231212,
122.725360080974)) ;
#43844 = CARTESIAN_POINT('Ctrl Pts',(-18.1698329826385,-13.5461926427583,
122.553733855565)) ;
#43845 = CARTESIAN_POINT('Ctrl Pts',(-18.3144502475993,-13.7360773177641,
122.905994660676)) ;
#43846 = CARTESIAN_POINT('Ctrl Pts',(-18.0407519036657,-13.5560882374012,
122.779526388176)) ;
#43847 = CARTESIAN_POINT('Ctrl Pts',(-18.2429366007976,-13.7461392644209,
123.105048153552)) ;
#43848 = CARTESIAN_POINT('Ctrl Pts',(-17.9513576421501,-13.5661501840581,
123.028342279855)) ;
#43849 = CARTESIAN_POINT('Ctrl Pts',(-18.2077846553653,-13.7559888883531,
123.309123594396)) ;
#43850 = CARTESIAN_POINT('Ctrl Pts',(-17.9074152113575,-13.5759998079902,
123.283436990171)) ;
#43851 = CARTESIAN_POINT('Ctrl Pts',(-18.2079178316408,-13.7659521273829,
123.518569880535)) ;
#43852 = CARTESIAN_POINT('Ctrl Pts',(-17.9075794490051,-13.5859630470201,
123.545245160118)) ;
#43853 = CARTESIAN_POINT('Ctrl Pts',(-18.2449311630796,-13.7759767021588,
123.726054826624)) ;
#43854 = CARTESIAN_POINT('Ctrl Pts',(-17.9538438452054,-13.5959876217959,
123.804601716854)) ;
#43855 = CARTESIAN_POINT('Ctrl Pts',(-18.3165097926261,-13.7858952648465,
123.921897886242)) ;
#43856 = CARTESIAN_POINT('Ctrl Pts',(-18.0433151854202,-13.6059061844836,
124.0494068293)) ;
#43857 = CARTESIAN_POINT('Ctrl Pts',(-18.4214705157971,-13.7958874515705,
124.103877790771)) ;
#43858 = CARTESIAN_POINT('Ctrl Pts',(-18.1745142883211,-13.6158983712076,
124.276882942804)) ;
#43859 = CARTESIAN_POINT('Ctrl Pts',(-18.5572880042135,-13.8059222501547,
124.265295046581)) ;
#43860 = CARTESIAN_POINT('Ctrl Pts',(-18.3442843563806,-13.6259331697918,
124.478655912716)) ;
#43861 = CARTESIAN_POINT('Ctrl Pts',(-18.7159640539968,-13.8157774408283,
124.398542881549)) ;
#43862 = CARTESIAN_POINT('Ctrl Pts',(-18.5426287178468,-13.6357883604655,
124.645217964009)) ;
#43863 = CARTESIAN_POINT('Ctrl Pts',(-18.8978051688274,-13.8257767889813,
124.503949795873)) ;
#43864 = CARTESIAN_POINT('Ctrl Pts',(-18.7699291705974,-13.6457877086185,
124.776978497853)) ;
#43865 = CARTESIAN_POINT('Ctrl Pts',(-19.0931163675303,-13.8356719146565,
124.575663890585)) ;
#43866 = CARTESIAN_POINT('Ctrl Pts',(-19.0140681533579,-13.6556828342936,
124.86662328346)) ;
#43867 = CARTESIAN_POINT('Ctrl Pts',(-19.3012793398308,-13.8457324576046,
124.612957137398)) ;
#43868 = CARTESIAN_POINT('Ctrl Pts',(-19.2742712713222,-13.6657433772417,
124.913241817981)) ;
#43869 = CARTESIAN_POINT('Ctrl Pts',(-19.5083568286429,-13.8555817318715,
124.613644904383)) ;
#43870 = CARTESIAN_POINT('Ctrl Pts',(-19.5331191647968,-13.6755926515086,
124.914103544901)) ;
#43871 = CARTESIAN_POINT('Ctrl Pts',(-19.7161637957389,-13.8656089564414,
124.578258675114)) ;
#43872 = CARTESIAN_POINT('Ctrl Pts',(-19.792878148494,-13.6856198760785,124.869872597639)) ;
#43873 = CARTESIAN_POINT('Ctrl Pts',(-19.9145234172926,-13.8756373556292,
124.506794850628)) ;
#43874 = CARTESIAN_POINT('Ctrl Pts',(-20.0408282968694,-13.6956482752663,
124.780544744153)) ;
#43875 = CARTESIAN_POINT('Ctrl Pts',(-20.0942981409798,-13.8854831060427,
124.404230045374)) ;
#43876 = CARTESIAN_POINT('Ctrl Pts',(-20.2655486146661,-13.7054940256798,
124.652339842706)) ;
#43877 = CARTESIAN_POINT('Ctrl Pts',(-20.2562410694359,-13.8954718964434,
124.27052516634)) ;
#43878 = CARTESIAN_POINT('Ctrl Pts',(-20.4679785318478,-13.7154828160805,
124.485209945321)) ;
#43879 = CARTESIAN_POINT('Ctrl Pts',(-20.3928548044161,-13.9055168248431,
124.109502618488)) ;
#43880 = CARTESIAN_POINT('Ctrl Pts',(-20.6387470354959,-13.7255277444802,
124.283933112254)) ;
#43881 = CARTESIAN_POINT('Ctrl Pts',(-20.4975212772136,-13.9153413096321,
123.931431530893)) ;
#43882 = CARTESIAN_POINT('Ctrl Pts',(-20.7695822850911,-13.7353522292692,
124.061344007578)) ;
#43883 = CARTESIAN_POINT('Ctrl Pts',(-20.5716663162285,-13.9253987071733,
123.733438159543)) ;
#43884 = CARTESIAN_POINT('Ctrl Pts',(-20.8622650301573,-13.7454096268104,
123.813853115559)) ;
#43885 = CARTESIAN_POINT('Ctrl Pts',(-20.6095387245746,-13.9353247987595,
123.528210702811)) ;
#43886 = CARTESIAN_POINT('Ctrl Pts',(-20.9096073544687,-13.7553357183966,
123.557318498504)) ;
#43887 = CARTESIAN_POINT('Ctrl Pts',(-20.6117482503137,-13.945279583904,123.318943735867)) ;
#43888 = CARTESIAN_POINT('Ctrl Pts',(-20.9123708210729,-13.7652905035412,
123.295734355723)) ;
#43889 = CARTESIAN_POINT('Ctrl Pts',(-20.5770731565774,-13.9553169535617,
123.110795951615)) ;
#43890 = CARTESIAN_POINT('Ctrl Pts',(-20.8690285856397,-13.7753278731988,
123.035549479101)) ;
#43891 = CARTESIAN_POINT('Ctrl Pts',(-20.5079730266207,-13.9652057636833,
122.914716225052)) ;
#43892 = CARTESIAN_POINT('Ctrl Pts',(-20.7826546061871,-13.7852166833204,
122.790448432935)) ;
#43893 = CARTESIAN_POINT('Ctrl Pts',(-20.4051720006662,-13.9751951227343,
122.731595284921)) ;
#43894 = CARTESIAN_POINT('Ctrl Pts',(-20.6541544832906,-13.7952060423715,
122.561546360115)) ;
#43895 = CARTESIAN_POINT('Ctrl Pts',(-20.2724273246368,-13.9851536701904,
122.569707167163)) ;
#43896 = CARTESIAN_POINT('Ctrl Pts',(-20.4882245281512,-13.8051645898276,
122.359184924028)) ;
#43897 = CARTESIAN_POINT('Ctrl Pts',(-20.1148509111908,-13.9950532467415,
122.433733040983)) ;
#43898 = CARTESIAN_POINT('Ctrl Pts',(-20.2912542115885,-13.8150641663786,
122.189215690163)) ;
#43899 = CARTESIAN_POINT('Ctrl Pts',(-19.9333707547642,-14.0051011585722,
122.32566998488)) ;
#43900 = CARTESIAN_POINT('Ctrl Pts',(-20.0644048944981,-13.8251120782093,
122.054135819925)) ;
#43901 = CARTESIAN_POINT('Ctrl Pts',(-19.738890370448,-14.0149965064327,122.251724804565)) ;
#43902 = CARTESIAN_POINT('Ctrl Pts',(-19.8213040212289,-13.8350074260699,
121.961702812424)) ;
#43903 = CARTESIAN_POINT('Ctrl Pts',(-19.5311506381738,-14.0250581829639,
122.211995828632)) ;
#43904 = CARTESIAN_POINT('Ctrl Pts',(-19.5616299165928,-13.845069102601,121.912040392459)) ;
#43905 = CARTESIAN_POINT('Ctrl Pts',(-19.3242027583877,-14.0349027007131,
122.208972747124)) ;
#43906 = CARTESIAN_POINT('Ctrl Pts',(-19.302943765994,-13.8549136203502,121.908260248801)) ;
#43907 = CARTESIAN_POINT('Ctrl Pts',(-19.1173623183453,-14.0448631444279,
122.241578718461)) ;
#43908 = CARTESIAN_POINT('Ctrl Pts',(-19.0443926106772,-13.864874064065,121.949016797608)) ;
#43909 = CARTESIAN_POINT('Ctrl Pts',(-18.917933653831,-14.0548999772461,122.310497086348)) ;
#43910 = CARTESIAN_POINT('Ctrl Pts',(-18.7951065533296,-13.8749108968832,
122.035163624274)) ;
#43911 = CARTESIAN_POINT('Ctrl Pts',(-18.7362181804366,-14.0647787739929,
122.41109597588)) ;
#43912 = CARTESIAN_POINT('Ctrl Pts',(-18.5679607592807,-13.88478969363,122.160911880469)) ;
#43913 = CARTESIAN_POINT('Ctrl Pts',(-18.5717693082948,-14.0748380901212,
122.544026993693)) ;
#43914 = CARTESIAN_POINT('Ctrl Pts',(-18.3623992980865,-13.8948490097584,
122.327074678705)) ;
#43915 = CARTESIAN_POINT('Ctrl Pts',(-18.4354824503582,-14.0847085368744,
122.700520863806)) ;
#43916 = CARTESIAN_POINT('Ctrl Pts',(-18.1920392191495,-13.9047194565116,
122.522692233472)) ;
#43917 = CARTESIAN_POINT('Ctrl Pts',(-18.3266320599271,-14.0947011751325,
122.880198948747)) ;
#43918 = CARTESIAN_POINT('Ctrl Pts',(-18.0559754687445,-13.9147120947696,
122.747289602296)) ;
#43919 = CARTESIAN_POINT('Ctrl Pts',(-18.2507605415013,-14.1047331906804,
123.076976227112)) ;
#43920 = CARTESIAN_POINT('Ctrl Pts',(-17.9611352243635,-13.9247441103175,
122.993260746216)) ;
#43921 = CARTESIAN_POINT('Ctrl Pts',(-18.2104322023642,-14.114599046987,123.280449832988)) ;
#43922 = CARTESIAN_POINT('Ctrl Pts',(-17.9107237978205,-13.9346099666241,
123.247603809028)) ;
#43923 = CARTESIAN_POINT('Ctrl Pts',(-18.2059368718994,-14.1246683364561,
123.492066961254)) ;
#43924 = CARTESIAN_POINT('Ctrl Pts',(-17.9051038745564,-13.9446792560932,
123.512124786768)) ;
#43925 = CARTESIAN_POINT('Ctrl Pts',(-18.2375102294898,-14.1345118940074,
123.696598560914)) ;
#43926 = CARTESIAN_POINT('Ctrl Pts',(-17.9445700338335,-13.9545228136445,
123.767790796992)) ;
#43927 = CARTESIAN_POINT('Ctrl Pts',(-18.3043848267997,-14.1444920207952,
123.895462028567)) ;
#43928 = CARTESIAN_POINT('Ctrl Pts',(-18.0281629110103,-13.9645029404324,
124.016370584098)) ;
#43929 = CARTESIAN_POINT('Ctrl Pts',(-18.4055151657071,-14.1545105693952,
124.080209802711)) ;
#43930 = CARTESIAN_POINT('Ctrl Pts',(-18.1545752563571,-13.9745214890323,
124.247305606012)) ;
#43931 = CARTESIAN_POINT('Ctrl Pts',(-18.5350837698109,-14.1643938699184,
124.242672415459)) ;
#43932 = CARTESIAN_POINT('Ctrl Pts',(-18.3165363213439,-13.9844047895555,
124.450385027953)) ;
#43933 = CARTESIAN_POINT('Ctrl Pts',(-18.6938257864244,-14.1744621569665,
124.382634186157)) ;
#43934 = CARTESIAN_POINT('Ctrl Pts',(-18.5149631927261,-13.9944730766036,
124.625337357405)) ;
#43935 = CARTESIAN_POINT('Ctrl Pts',(-18.8701172743958,-14.1842922799851,
124.490542166158)) ;
#43936 = CARTESIAN_POINT('Ctrl Pts',(-18.7353286473751,-14.0043031996223,
124.760223493667)) ;
#43937 = CARTESIAN_POINT('Ctrl Pts',(-19.0669291678649,-14.1943588639105,
124.568249490539)) ;
#43938 = CARTESIAN_POINT('Ctrl Pts',(-18.9813430292803,-14.0143697835476,
124.857357794633)) ;
#43939 = CARTESIAN_POINT('Ctrl Pts',(-19.2706943838824,-14.2042489769249,
124.609750952324)) ;
#43940 = CARTESIAN_POINT('Ctrl Pts',(-19.2360505050157,-14.0242598965621,
124.909235187301)) ;
#43941 = CARTESIAN_POINT('Ctrl Pts',(-19.4806689201278,-14.2142416656876,
124.615742309981)) ;
#43942 = CARTESIAN_POINT('Ctrl Pts',(-19.4985188781141,-14.0342525853247,
124.916724579482)) ;
#43943 = CARTESIAN_POINT('Ctrl Pts',(-19.6878386126546,-14.2242025540433,
124.585132160337)) ;
#43944 = CARTESIAN_POINT('Ctrl Pts',(-19.7574815058424,-14.0442134736805,
124.878462065094)) ;
#43945 = CARTESIAN_POINT('Ctrl Pts',(-19.8857808498602,-14.2341204989233,
124.519648220953)) ;
#43946 = CARTESIAN_POINT('Ctrl Pts',(-20.0049101277491,-14.0541314185605,
124.796606975513)) ;
#43947 = CARTESIAN_POINT('Ctrl Pts',(-20.0711543280967,-14.2441282520195,
124.42009338198)) ;
#43948 = CARTESIAN_POINT('Ctrl Pts',(-20.2366270328514,-14.0641391716567,
124.672163407092)) ;
#43949 = CARTESIAN_POINT('Ctrl Pts',(-20.2365214427845,-14.2541593459786,
124.289244206464)) ;
#43950 = CARTESIAN_POINT('Ctrl Pts',(-20.4433359395377,-14.0741702656157,
124.508602153767)) ;
#43951 = CARTESIAN_POINT('Ctrl Pts',(-20.3744629268658,-14.2640073140066,
124.134836918703)) ;
#43952 = CARTESIAN_POINT('Ctrl Pts',(-20.6157637308144,-14.0840182336437,
124.315591986878)) ;
#43953 = CARTESIAN_POINT('Ctrl Pts',(-20.4860083257482,-14.2740692701324,
123.95512196643)) ;
#43954 = CARTESIAN_POINT('Ctrl Pts',(-20.7551952257147,-14.0940801897696,
124.090948556963)) ;
#43955 = CARTESIAN_POINT('Ctrl Pts',(-20.5631955250995,-14.2839664817336,
123.761889219392)) ;
#43956 = CARTESIAN_POINT('Ctrl Pts',(-20.8516795936219,-14.1039774013707,
123.849406694872)) ;
#43957 = CARTESIAN_POINT('Ctrl Pts',(-20.6064757403202,-14.2938976483982,
123.557644080804)) ;
#43958 = CARTESIAN_POINT('Ctrl Pts',(-20.9057797422551,-14.1139085680353,
123.594099508417)) ;
#43959 = CARTESIAN_POINT('Ctrl Pts',(-20.6134856977865,-14.3039398326024,
123.346645043293)) ;
#43960 = CARTESIAN_POINT('Ctrl Pts',(-20.9145419978762,-14.1239507522395,
123.330350913867)) ;
#43961 = CARTESIAN_POINT('Ctrl Pts',(-20.5843602960543,-14.3138265008555,
123.140837465138)) ;
#43962 = CARTESIAN_POINT('Ctrl Pts',(-20.878134852128,-14.1338374204927,123.073090399106)) ;
#43963 = CARTESIAN_POINT('Ctrl Pts',(-20.5195898101172,-14.3238196128338,
122.940995926319)) ;
#43964 = CARTESIAN_POINT('Ctrl Pts',(-20.797171317607,-14.1438305324709,122.823288399636)) ;
#43965 = CARTESIAN_POINT('Ctrl Pts',(-20.4214970858592,-14.3337652904496,
122.756344163075)) ;
#43966 = CARTESIAN_POINT('Ctrl Pts',(-20.6745548235997,-14.1537762100867,
122.592473334251)) ;
#43967 = CARTESIAN_POINT('Ctrl Pts',(-20.2931422169085,-14.3437125934346,
122.591232662632)) ;
#43968 = CARTESIAN_POINT('Ctrl Pts',(-20.5141104749864,-14.1637235130717,
122.386083823547)) ;
#43969 = CARTESIAN_POINT('Ctrl Pts',(-20.1363573288779,-14.3537603171813,
122.449682535313)) ;
#43970 = CARTESIAN_POINT('Ctrl Pts',(-20.3181292651246,-14.1737712368185,
122.209146648077)) ;
#43971 = CARTESIAN_POINT('Ctrl Pts',(-19.9610119228354,-14.3636086909439,
122.339593196702)) ;
#43972 = CARTESIAN_POINT('Ctrl Pts',(-20.098946063385,-14.183619610581,122.071534647514)) ;
#43973 = CARTESIAN_POINT('Ctrl Pts',(-19.7673215762674,-14.3735676633896,
122.260098624231)) ;
#43974 = CARTESIAN_POINT('Ctrl Pts',(-19.8568324061559,-14.1935785830267,
121.972166958928)) ;
#43975 = CARTESIAN_POINT('Ctrl Pts',(-19.5610549600458,-14.3836065252707,
122.215459746428)) ;
#43976 = CARTESIAN_POINT('Ctrl Pts',(-19.5989991593622,-14.2036174449079,
121.916368996619)) ;
#43977 = CARTESIAN_POINT('Ctrl Pts',(-19.3535221005735,-14.3934851294425,
122.207111470236)) ;
#43978 = CARTESIAN_POINT('Ctrl Pts',(-19.339581937027,-14.2134960490797,121.905934350721)) ;
#43979 = CARTESIAN_POINT('Ctrl Pts',(-19.1441263617507,-14.4035366706458,
122.235315239726)) ;
#43980 = CARTESIAN_POINT('Ctrl Pts',(-19.0778376414756,-14.223547590283,121.941189793871)) ;
#43981 = CARTESIAN_POINT('Ctrl Pts',(-18.9458547057129,-14.4134320686262,
122.298408849419)) ;
#43982 = CARTESIAN_POINT('Ctrl Pts',(-18.8299973984445,-14.2334429882633,
122.020057862292)) ;
#43983 = CARTESIAN_POINT('Ctrl Pts',(-18.7586516298394,-14.4234833011715,
122.396359934609)) ;
#43984 = CARTESIAN_POINT('Ctrl Pts',(-18.5959941772312,-14.2434942208086,
122.142497343035)) ;
#43985 = CARTESIAN_POINT('Ctrl Pts',(-18.5939939088903,-14.4333694917958,
122.523221653132)) ;
#43986 = CARTESIAN_POINT('Ctrl Pts',(-18.3901717062413,-14.2533804114329,
122.301075810793)) ;
#43987 = CARTESIAN_POINT('Ctrl Pts',(-18.4520997591911,-14.4433620311115,
122.678107054398)) ;
#43988 = CARTESIAN_POINT('Ctrl Pts',(-18.2128046217201,-14.2633729507487,
122.494683384681)) ;
#43989 = CARTESIAN_POINT('Ctrl Pts',(-18.3397922812975,-14.4533104770063,
122.854559106031)) ;
#43990 = CARTESIAN_POINT('Ctrl Pts',(-18.0724208014174,-14.2733213966434,
122.715249428786)) ;
#43991 = CARTESIAN_POINT('Ctrl Pts',(-18.2596593833855,-14.4632472795382,
123.047461897236)) ;
#43992 = CARTESIAN_POINT('Ctrl Pts',(-17.9722554347127,-14.2832581991753,
122.956378922665)) ;
#43993 = CARTESIAN_POINT('Ctrl Pts',(-18.2137581958001,-14.4732302869895,
123.252282638572)) ;
#43994 = CARTESIAN_POINT('Ctrl Pts',(-17.9148800450432,-14.2932412066266,
123.212405357803)) ;
#43995 = CARTESIAN_POINT('Ctrl Pts',(-18.2044493527583,-14.4832741284043,
123.463206431544)) ;
#43996 = CARTESIAN_POINT('Ctrl Pts',(-17.9032450354326,-14.3032850480414,
123.476059954926)) ;
#43997 = CARTESIAN_POINT('Ctrl Pts',(-18.2308383801991,-14.4931023270282,
123.668165335843)) ;
#43998 = CARTESIAN_POINT('Ctrl Pts',(-17.9362327116183,-14.3131132466653,
123.732259863028)) ;
#43999 = CARTESIAN_POINT('Ctrl Pts',(-18.2938523410951,-14.5031789204704,
123.870372485691)) ;
#44000 = CARTESIAN_POINT('Ctrl Pts',(-18.0150012319065,-14.3231898401075,
123.985018013429)) ;
#44001 = CARTESIAN_POINT('Ctrl Pts',(-18.3887993193818,-14.513030919812,124.0544990199)) ;
#44002 = CARTESIAN_POINT('Ctrl Pts',(-18.1336866675862,-14.3330418394491,
124.215176688599)) ;
#44003 = CARTESIAN_POINT('Ctrl Pts',(-18.516907971024,-14.5231045066358,124.223090197898)) ;
#44004 = CARTESIAN_POINT('Ctrl Pts',(-18.2938233161721,-14.343115426273,124.425914520946)) ;
#44005 = CARTESIAN_POINT('Ctrl Pts',(-18.6688091775145,-14.5329447317333,
124.363553032254)) ;
#44006 = CARTESIAN_POINT('Ctrl Pts',(-18.4837016929012,-14.3529556513705,
124.601492972209)) ;
#44007 = CARTESIAN_POINT('Ctrl Pts',(-18.8445804362272,-14.542910435762,124.477535027406)) ;
#44008 = CARTESIAN_POINT('Ctrl Pts',(-18.703416961841,-14.3629213553991,124.743969337012)) ;
#44009 = CARTESIAN_POINT('Ctrl Pts',(-19.0387987115393,-14.5529370690686,
124.559495745125)) ;
#44010 = CARTESIAN_POINT('Ctrl Pts',(-18.946190326884,-14.3729479887057,124.846418837597)) ;
#44011 = CARTESIAN_POINT('Ctrl Pts',(-19.2419467311579,-14.5628513647804,
124.606096057943)) ;
#44012 = CARTESIAN_POINT('Ctrl Pts',(-19.2001264119849,-14.3828622844175,
124.904667897107)) ;
#44013 = CARTESIAN_POINT('Ctrl Pts',(-19.4516521953088,-14.5728396534728,
124.61717510903)) ;
#44014 = CARTESIAN_POINT('Ctrl Pts',(-19.4622585243968,-14.39285057311,124.918515058784)) ;
#44015 = CARTESIAN_POINT('Ctrl Pts',(-19.6610834565671,-14.5828783866312,
124.591166378612)) ;
#44016 = CARTESIAN_POINT('Ctrl Pts',(-19.7240472766002,-14.4028893062683,
124.886002641431)) ;
#44017 = CARTESIAN_POINT('Ctrl Pts',(-19.858998903738,-14.5927217184587,124.530728055798)) ;
#44018 = CARTESIAN_POINT('Ctrl Pts',(-19.9714422784701,-14.4127326380959,
124.810452799983)) ;
#44019 = CARTESIAN_POINT('Ctrl Pts',(-20.0470907094626,-14.6027494443383,
124.43551748704)) ;
#44020 = CARTESIAN_POINT('Ctrl Pts',(-20.2065561510804,-14.4227603639755,
124.691438006509)) ;
#44021 = CARTESIAN_POINT('Ctrl Pts',(-20.215531250739,-14.6127817807269,124.308574127084)) ;
#44022 = CARTESIAN_POINT('Ctrl Pts',(-20.4171057819061,-14.432792700364,124.532757562362)) ;
#44023 = CARTESIAN_POINT('Ctrl Pts',(-20.3567549827595,-14.6226112810275,
124.157731091938)) ;
#44024 = CARTESIAN_POINT('Ctrl Pts',(-20.5936350310893,-14.4426222006646,
124.34420163555)) ;
#44025 = CARTESIAN_POINT('Ctrl Pts',(-20.4720182760222,-14.6326007849443,
123.982171250015)) ;
#44026 = CARTESIAN_POINT('Ctrl Pts',(-20.7377126082824,-14.4526117045814,
124.124750610571)) ;
#44027 = CARTESIAN_POINT('Ctrl Pts',(-20.5550029183584,-14.6426446254567,
123.788010434387)) ;
#44028 = CARTESIAN_POINT('Ctrl Pts',(-20.8414417058682,-14.4626555450938,
123.882049023559)) ;
#44029 = CARTESIAN_POINT('Ctrl Pts',(-20.6023692510491,-14.6524663312247,
123.587034176731)) ;
#44030 = CARTESIAN_POINT('Ctrl Pts',(-20.900648035962,-14.4724772508619,123.63082704311)) ;
#44031 = CARTESIAN_POINT('Ctrl Pts',(-20.614891393778,-14.6625013783571,123.376438673923)) ;
#44032 = CARTESIAN_POINT('Ctrl Pts',(-20.9162986354435,-14.4825122979942,
123.367582647658)) ;
#44033 = CARTESIAN_POINT('Ctrl Pts',(-20.5901024671484,-14.672526055794,123.167143676446)) ;
#44034 = CARTESIAN_POINT('Ctrl Pts',(-20.8853105895479,-14.4925369754311,
123.105964149167)) ;
#44035 = CARTESIAN_POINT('Ctrl Pts',(-20.5308125782497,-14.6823788706484,
122.968674050456)) ;
#44036 = CARTESIAN_POINT('Ctrl Pts',(-20.8111959911623,-14.5023897902856,
122.85787673168)) ;
#44037 = CARTESIAN_POINT('Ctrl Pts',(-20.4370276643577,-14.692366580256,122.780826892626)) ;
#44038 = CARTESIAN_POINT('Ctrl Pts',(-20.6939628548545,-14.5123774998931,
122.623068574786)) ;
#44039 = CARTESIAN_POINT('Ctrl Pts',(-20.3127672555841,-14.7022965902501,
122.613067626526)) ;
#44040 = CARTESIAN_POINT('Ctrl Pts',(-20.5386353139162,-14.5223075098872,
122.413370344863)) ;
#44041 = CARTESIAN_POINT('Ctrl Pts',(-20.1605796757999,-14.7122863454692,
122.468335495329)) ;
#44042 = CARTESIAN_POINT('Ctrl Pts',(-20.3483991859879,-14.5322972651064,
122.232456679631)) ;
#44043 = CARTESIAN_POINT('Ctrl Pts',(-19.9847778139171,-14.7223129541521,
122.352025348161)) ;
#44044 = CARTESIAN_POINT('Ctrl Pts',(-20.1286457021689,-14.5423238737893,
122.087070807904)) ;
#44045 = CARTESIAN_POINT('Ctrl Pts',(-19.7942886748206,-14.732196894174,122.269022419418)) ;
#44046 = CARTESIAN_POINT('Ctrl Pts',(-19.8905327192245,-14.5522078138111,
121.983318872916)) ;
#44047 = CARTESIAN_POINT('Ctrl Pts',(-19.5902331312652,-14.7421861217125,
122.219359207184)) ;
#44048 = CARTESIAN_POINT('Ctrl Pts',(-19.635462587809,-14.5621970413496,121.921242080345)) ;
#44049 = CARTESIAN_POINT('Ctrl Pts',(-19.3795093368715,-14.7522289922362,
122.206246194729)) ;
#44050 = CARTESIAN_POINT('Ctrl Pts',(-19.3720577988296,-14.5722399118733,
121.904853033029)) ;
#44051 = CARTESIAN_POINT('Ctrl Pts',(-19.1740714005142,-14.7620613789916,
122.229097308269)) ;
#44052 = CARTESIAN_POINT('Ctrl Pts',(-19.1152596800331,-14.5820722986287,
121.933419317847)) ;
#44053 = CARTESIAN_POINT('Ctrl Pts',(-18.9723061416938,-14.7720546721632,
122.287639558838)) ;
#44054 = CARTESIAN_POINT('Ctrl Pts',(-18.8630536665113,-14.5920655918003,
122.006599511882)) ;
#44055 = CARTESIAN_POINT('Ctrl Pts',(-18.7832226625352,-14.7820866778116,
122.381086795298)) ;
#44056 = CARTESIAN_POINT('Ctrl Pts',(-18.6267003875226,-14.6020975974487,
122.123410637976)) ;
#44057 = CARTESIAN_POINT('Ctrl Pts',(-18.6159274829548,-14.7919519337806,
122.503651125695)) ;
#44058 = CARTESIAN_POINT('Ctrl Pts',(-18.4175822404663,-14.6119628534177,
122.276618419926)) ;
#44059 = CARTESIAN_POINT('Ctrl Pts',(-18.4706094581403,-14.8019138136881,
122.654469653778)) ;
#44060 = CARTESIAN_POINT('Ctrl Pts',(-18.2359363520061,-14.6219247333252,
122.465143513999)) ;
#44061 = CARTESIAN_POINT('Ctrl Pts',(-18.3531243947538,-14.81194874705,122.829681165894)) ;
#44062 = CARTESIAN_POINT('Ctrl Pts',(-18.0890820796082,-14.6319596666871,
122.684159241081)) ;
#44063 = CARTESIAN_POINT('Ctrl Pts',(-18.2687841779479,-14.8218337054293,
123.019642132794)) ;
#44064 = CARTESIAN_POINT('Ctrl Pts',(-17.9836588830903,-14.6418446250664,
122.921611991648)) ;
#44065 = CARTESIAN_POINT('Ctrl Pts',(-18.2178545293784,-14.8318993323519,
123.224997323136)) ;
#44066 = CARTESIAN_POINT('Ctrl Pts',(-17.91999930049,-14.6519102519891,123.178306439075)) ;
#44067 = CARTESIAN_POINT('Ctrl Pts',(-18.2034666313483,-14.8417384380163,
123.431379104992)) ;
#44068 = CARTESIAN_POINT('Ctrl Pts',(-17.9020169238166,-14.6617493576534,
123.43628455332)) ;
#44069 = CARTESIAN_POINT('Ctrl Pts',(-18.2253374188485,-14.8518012530216,
123.641768968564)) ;
#44070 = CARTESIAN_POINT('Ctrl Pts',(-17.9293579840825,-14.6718121726588,
123.699271479237)) ;
#44071 = CARTESIAN_POINT('Ctrl Pts',(-18.2826422959049,-14.8616974590703,
123.841793280128)) ;
#44072 = CARTESIAN_POINT('Ctrl Pts',(-18.0009916819233,-14.6817083787074,
123.949301617982)) ;
#44073 = CARTESIAN_POINT('Ctrl Pts',(-18.3736753162085,-14.8716382820956,
124.029885460281)) ;
#44074 = CARTESIAN_POINT('Ctrl Pts',(-18.1147854788541,-14.6916492017327,
124.184415931245)) ;
#44075 = CARTESIAN_POINT('Ctrl Pts',(-18.4967554476146,-14.8816428650742,
124.200469969171)) ;
#44076 = CARTESIAN_POINT('Ctrl Pts',(-18.2686378473878,-14.7016537847114,
124.397645063482)) ;
#44077 = CARTESIAN_POINT('Ctrl Pts',(-18.6479893488011,-14.891663759519,124.347127592409)) ;
#44078 = CARTESIAN_POINT('Ctrl Pts',(-18.4576820792314,-14.7116746791561,
124.580965224182)) ;
#44079 = CARTESIAN_POINT('Ctrl Pts',(-18.8200089658471,-14.9015556801084,
124.463997418573)) ;
#44080 = CARTESIAN_POINT('Ctrl Pts',(-18.6727084410143,-14.7215665997455,
124.72705053099)) ;
#44081 = CARTESIAN_POINT('Ctrl Pts',(-19.0115199934511,-14.9115491124538,
124.550366690489)) ;
#44082 = CARTESIAN_POINT('Ctrl Pts',(-18.9120984381462,-14.7315600320909,
124.835009694246)) ;
#44083 = CARTESIAN_POINT('Ctrl Pts',(-19.2141671143431,-14.9214947173536,
124.601860043974)) ;
#44084 = CARTESIAN_POINT('Ctrl Pts',(-19.1654082297074,-14.7415056369908,
124.899373825222)) ;
#44085 = CARTESIAN_POINT('Ctrl Pts',(-19.422692143887,-14.9314419908352,124.617812488144)) ;
#44086 = CARTESIAN_POINT('Ctrl Pts',(-19.4260649276626,-14.7514529104723,
124.919311654018)) ;
#44087 = CARTESIAN_POINT('Ctrl Pts',(-19.6328836255055,-14.9414899053115,
124.596874131456)) ;
#44088 = CARTESIAN_POINT('Ctrl Pts',(-19.6888039980346,-14.7615008249487,
124.893135998467)) ;
#44089 = CARTESIAN_POINT('Ctrl Pts',(-19.8322491561593,-14.9513375456589,
124.541062785767)) ;
#44090 = CARTESIAN_POINT('Ctrl Pts',(-19.9380105597305,-14.771348465296,124.823369065413)) ;
#44091 = CARTESIAN_POINT('Ctrl Pts',(-20.0213303949895,-14.9612992610355,
124.451042034006)) ;
#44092 = CARTESIAN_POINT('Ctrl Pts',(-20.1743610165879,-14.7813101806726,
124.710840541122)) ;
#44093 = CARTESIAN_POINT('Ctrl Pts',(-20.1929184638276,-14.9713278846083,
124.328511186806)) ;
#44094 = CARTESIAN_POINT('Ctrl Pts',(-20.3888445239229,-14.7913388042454,
124.557674697892)) ;
#44095 = CARTESIAN_POINT('Ctrl Pts',(-20.3389145430226,-14.9812382466747,
124.179885799862)) ;
#44096 = CARTESIAN_POINT('Ctrl Pts',(-20.5713377846761,-14.8012491663118,
124.371890859621)) ;
#44097 = CARTESIAN_POINT('Ctrl Pts',(-20.4576406506801,-14.9911729403271,
124.008044457199)) ;
#44098 = CARTESIAN_POINT('Ctrl Pts',(-20.7197431781313,-14.8111838599642,
124.157087470465)) ;
#44099 = CARTESIAN_POINT('Ctrl Pts',(-20.5454669216902,-15.001214783455,123.816080842499)) ;
#44100 = CARTESIAN_POINT('Ctrl Pts',(-20.8295234845104,-14.8212257030921,
123.917131743842)) ;
#44101 = CARTESIAN_POINT('Ctrl Pts',(-20.5979816592684,-15.0110992890254,
123.615000802519)) ;
#44102 = CARTESIAN_POINT('Ctrl Pts',(-20.8951642259537,-14.8311102086625,
123.665780824477)) ;
#44103 = CARTESIAN_POINT('Ctrl Pts',(-20.6152250273524,-15.0211013928106,
123.405463995573)) ;
#44104 = CARTESIAN_POINT('Ctrl Pts',(-20.9167156314067,-14.8411123124477,
123.40385951735)) ;
#44105 = CARTESIAN_POINT('Ctrl Pts',(-20.5961521969141,-15.0310197442256,
123.197788238171)) ;
#44106 = CARTESIAN_POINT('Ctrl Pts',(-20.8928717590869,-14.8510306638627,
123.144264974598)) ;
#44107 = CARTESIAN_POINT('Ctrl Pts',(-20.5405596861251,-15.0410674002465,
122.994035665252)) ;
#44108 = CARTESIAN_POINT('Ctrl Pts',(-20.8233784416685,-14.8610783198836,
122.889574983756)) ;
#44109 = CARTESIAN_POINT('Ctrl Pts',(-20.4521948522776,-15.0509385932747,
122.806217337189)) ;
#44110 = CARTESIAN_POINT('Ctrl Pts',(-20.7129195792152,-14.8709495129118,
122.65480303298)) ;
#44111 = CARTESIAN_POINT('Ctrl Pts',(-20.330284242075,-15.0610043064182,122.633308943981)) ;
#44112 = CARTESIAN_POINT('Ctrl Pts',(-20.5605298604237,-14.8810152260553,
122.438669790613)) ;
#44113 = CARTESIAN_POINT('Ctrl Pts',(-20.1834794070481,-15.0708567669908,
122.487109307967)) ;
#44114 = CARTESIAN_POINT('Ctrl Pts',(-20.3770184511198,-14.890867686628,122.255919659017)) ;
#44115 = CARTESIAN_POINT('Ctrl Pts',(-19.9518872310143,-15.0842852297134,
122.325790591143)) ;
#44116 = CARTESIAN_POINT('Ctrl Pts',(-20.087542768723,-14.9042961493505,122.054287114174)) ;
#44117 = CARTESIAN_POINT('Ctrl Pts',(-19.6903665057396,-15.0973661772305,
122.230682396376)) ;
#44118 = CARTESIAN_POINT('Ctrl Pts',(-19.7606733441546,-14.9173770968676,
121.935403530529)) ;
#44119 = CARTESIAN_POINT('Ctrl Pts',(-19.4082962992305,-15.110840675465,122.205756665579)) ;
#44120 = CARTESIAN_POINT('Ctrl Pts',(-19.4080294143569,-14.9308515951022,
121.904239538084)) ;
#44121 = CARTESIAN_POINT('Ctrl Pts',(-19.2023473006596,-15.1206727790745,
122.223870629062)) ;
#44122 = CARTESIAN_POINT('Ctrl Pts',(-19.1506048230124,-14.9406836987116,
121.926886772641)) ;
#44123 = CARTESIAN_POINT('Ctrl Pts',(-18.9998068488561,-15.1306386822012,
122.277363273524)) ;
#44124 = CARTESIAN_POINT('Ctrl Pts',(-18.8974267387151,-14.9506496018383,
121.993755117999)) ;
#44125 = CARTESIAN_POINT('Ctrl Pts',(-18.8085430621808,-15.1406660915114,
122.366073015869)) ;
#44126 = CARTESIAN_POINT('Ctrl Pts',(-18.6583498545096,-14.9606770111485,
122.104643278367)) ;
#44127 = CARTESIAN_POINT('Ctrl Pts',(-18.6376088448104,-15.150577122878,122.48516450023)) ;
#44128 = CARTESIAN_POINT('Ctrl Pts',(-18.4446798401524,-14.9705880425151,
122.253516252991)) ;
#44129 = CARTESIAN_POINT('Ctrl Pts',(-18.4395743724625,-15.163821430499,122.681015377369)) ;
#44130 = CARTESIAN_POINT('Ctrl Pts',(-18.1971580268326,-14.9838323501362,
122.498300087744)) ;
#44131 = CARTESIAN_POINT('Ctrl Pts',(-18.2607335132502,-15.1805219131702,
122.987645959784)) ;
#44132 = CARTESIAN_POINT('Ctrl Pts',(-17.9735883960073,-15.0005328328073,
122.881645823256)) ;
#44133 = CARTESIAN_POINT('Ctrl Pts',(-18.1977869763505,-15.197028742326,123.333061812602)) ;
#44134 = CARTESIAN_POINT('Ctrl Pts',(-17.8949212635065,-15.0170396619631,
123.313331293313)) ;
#44135 = CARTESIAN_POINT('Ctrl Pts',(-18.2199642495241,-15.2103393705636,
123.611928517238)) ;
#44136 = CARTESIAN_POINT('Ctrl Pts',(-17.9226408363166,-15.0303502902007,
123.661981974254)) ;
#44137 = CARTESIAN_POINT('Ctrl Pts',(-18.2726848636332,-15.2203319341037,
123.815325721179)) ;
#44138 = CARTESIAN_POINT('Ctrl Pts',(-17.9885443792014,-15.0403428537408,
123.916213406476)) ;
#44139 = CARTESIAN_POINT('Ctrl Pts',(-18.3604503080189,-15.2303620171052,
124.007021668416)) ;
#44140 = CARTESIAN_POINT('Ctrl Pts',(-18.0982567045418,-15.0503729367423,
124.155839488556)) ;
#44141 = CARTESIAN_POINT('Ctrl Pts',(-18.5172815670806,-15.243535621103,124.235376320227)) ;
#44142 = CARTESIAN_POINT('Ctrl Pts',(-18.294281628791,-15.0635465407401,124.441261777876)) ;
#44143 = CARTESIAN_POINT('Ctrl Pts',(-18.785763220475,-15.2601733263344,124.465502936072)) ;
#44144 = CARTESIAN_POINT('Ctrl Pts',(-18.6299004804778,-15.0801842459715,
124.72893753815)) ;
#44145 = CARTESIAN_POINT('Ctrl Pts',(-19.1813810887829,-15.2800550889018,
124.614910728195)) ;
#44146 = CARTESIAN_POINT('Ctrl Pts',(-19.1244402677115,-15.1000660085389,
124.915683237853)) ;
#44147 = CARTESIAN_POINT('Ctrl Pts',(-19.536304822624,-15.2967514411183,124.619219755491)) ;
#44148 = CARTESIAN_POINT('Ctrl Pts',(-19.5680268436857,-15.1167623607554,
124.921075710828)) ;
#44149 = CARTESIAN_POINT('Ctrl Pts',(-19.8044165799873,-15.3099084689074,
124.551173766666)) ;
#44150 = CARTESIAN_POINT('Ctrl Pts',(-19.9032277012158,-15.1299193885445,
124.836006276955)) ;
#44151 = CARTESIAN_POINT('Ctrl Pts',(-20.0610790101127,-15.3232858235509,
124.436222758126)) ;
#44152 = CARTESIAN_POINT('Ctrl Pts',(-20.2240299227746,-15.1432967431881,
124.692326184051)) ;
#44153 = CARTESIAN_POINT('Ctrl Pts',(-20.3337494420324,-15.3398166578097,
124.214377221525)) ;
#44154 = CARTESIAN_POINT('Ctrl Pts',(-20.5648835408221,-15.1598275774469,
124.415004995461)) ;
#44155 = CARTESIAN_POINT('Ctrl Pts',(-20.552438862062,-15.3597813475528,123.850580679781)) ;
#44156 = CARTESIAN_POINT('Ctrl Pts',(-20.8382356610329,-15.17979226719,123.960261264776)) ;
#44157 = CARTESIAN_POINT('Ctrl Pts',(-20.6332747084739,-15.3796978409765,
123.434880640488)) ;
#44158 = CARTESIAN_POINT('Ctrl Pts',(-20.9392779039823,-15.1997087606136,
123.440635012867)) ;
#44159 = CARTESIAN_POINT('Ctrl Pts',(-20.5683199143235,-15.399587560326,123.016946237213)) ;
#44160 = CARTESIAN_POINT('Ctrl Pts',(-20.8580805309166,-15.2195984799632,
122.918218801443)) ;
#44161 = CARTESIAN_POINT('Ctrl Pts',(-20.3631949850862,-15.4195942899739,
122.644342249502)) ;
#44162 = CARTESIAN_POINT('Ctrl Pts',(-20.6016712396196,-15.239605209611,122.45246543698)) ;
#44163 = CARTESIAN_POINT('Ctrl Pts',(-20.0460283351885,-15.4394323436208,
122.366126910109)) ;
#44164 = CARTESIAN_POINT('Ctrl Pts',(-20.2052118909962,-15.2594432632579,
122.104699832134)) ;
#44165 = CARTESIAN_POINT('Ctrl Pts',(-19.6501954328286,-15.4594256818344,
122.211302972032)) ;
#44166 = CARTESIAN_POINT('Ctrl Pts',(-19.7104197648505,-15.2794366014715,
121.911172706133)) ;
#44167 = CARTESIAN_POINT('Ctrl Pts',(-19.22747548443,-15.479308481241,122.20116645109)) ;
#44168 = CARTESIAN_POINT('Ctrl Pts',(-19.1820210308814,-15.2993194008781,
121.898505004141)) ;
#44169 = CARTESIAN_POINT('Ctrl Pts',(-18.8264426794319,-15.4992006621597,
122.335208188009)) ;
#44170 = CARTESIAN_POINT('Ctrl Pts',(-18.6807320925926,-15.3192115817968,
122.06605896947)) ;
#44171 = CARTESIAN_POINT('Ctrl Pts',(-18.4944215574731,-15.5191028406548,
122.597782843408)) ;
#44172 = CARTESIAN_POINT('Ctrl Pts',(-18.2657076846686,-15.3391137602919,
122.394277865644)) ;
#44173 = CARTESIAN_POINT('Ctrl Pts',(-18.2711780684696,-15.5391401518585,
122.960525542868)) ;
#44174 = CARTESIAN_POINT('Ctrl Pts',(-17.9866547281374,-15.3591510714956,
122.847707709371)) ;
#44175 = CARTESIAN_POINT('Ctrl Pts',(-18.1854465994955,-15.5589525933994,
123.373166514348)) ;
#44176 = CARTESIAN_POINT('Ctrl Pts',(-17.8794922157529,-15.3789635130365,
123.363506708324)) ;
#44177 = CARTESIAN_POINT('Ctrl Pts',(-18.2465194115136,-15.5790178341343,
123.795207249882)) ;
#44178 = CARTESIAN_POINT('Ctrl Pts',(-17.955834597053,-15.3990287537714,123.891058298143)) ;
#44179 = CARTESIAN_POINT('Ctrl Pts',(-18.4447532133238,-15.5987750389901,
124.16581727744)) ;
#44180 = CARTESIAN_POINT('Ctrl Pts',(-18.2036257717715,-15.4187859586272,
124.35431729337)) ;
#44181 = CARTESIAN_POINT('Ctrl Pts',(-18.7611937431446,-15.6188083116358,
124.450642539288)) ;
#44182 = CARTESIAN_POINT('Ctrl Pts',(-18.5991767273495,-15.4388192312729,
124.710349085039)) ;
#44183 = CARTESIAN_POINT('Ctrl Pts',(-19.1518899017671,-15.6386212200896,
124.608729629548)) ;
#44184 = CARTESIAN_POINT('Ctrl Pts',(-19.0875441524019,-15.4586321397268,
124.907957059452)) ;
#44185 = CARTESIAN_POINT('Ctrl Pts',(-19.5765723952849,-15.6586173662171,
124.624694592537)) ;
#44186 = CARTESIAN_POINT('Ctrl Pts',(-19.6183970906308,-15.4786282858542,
124.927914166445)) ;
#44187 = CARTESIAN_POINT('Ctrl Pts',(-19.9789149548444,-15.6784791194396,
124.495740343834)) ;
#44188 = CARTESIAN_POINT('Ctrl Pts',(-20.1213238855666,-15.4984900390767,
124.766723103207)) ;
#44189 = CARTESIAN_POINT('Ctrl Pts',(-20.3161903072829,-15.6985476365677,
124.234500907358)) ;
#44190 = CARTESIAN_POINT('Ctrl Pts',(-20.5429196526182,-15.5185585562048,
124.440174246411)) ;
#44191 = CARTESIAN_POINT('Ctrl Pts',(-20.5412403283249,-15.7183785095645,
123.877812094549)) ;
#44192 = CARTESIAN_POINT('Ctrl Pts',(-20.8242320696034,-15.5383894292016,
123.994315885912)) ;
#44193 = CARTESIAN_POINT('Ctrl Pts',(-20.6325525181329,-15.7383004203812,
123.464277815718)) ;
#44194 = CARTESIAN_POINT('Ctrl Pts',(-20.9383743235662,-15.5583113400183,
123.477399544044)) ;
#44195 = CARTESIAN_POINT('Ctrl Pts',(-20.5770999387733,-15.7582298638165,
123.044097906908)) ;
#44196 = CARTESIAN_POINT('Ctrl Pts',(-20.8690610707405,-15.5782407834536,
122.952175132017)) ;
#44197 = CARTESIAN_POINT('Ctrl Pts',(-20.3819841700265,-15.7781395339329,
122.668482285981)) ;
#44198 = CARTESIAN_POINT('Ctrl Pts',(-20.6251692263084,-15.59815045357,122.482655310939)) ;
#44199 = CARTESIAN_POINT('Ctrl Pts',(-20.071398669403,-15.7980128911957,122.381885903197)) ;
#44200 = CARTESIAN_POINT('Ctrl Pts',(-20.2369405024036,-15.6180238108329,
122.124408327086)) ;
#44201 = CARTESIAN_POINT('Ctrl Pts',(-19.6794075493568,-15.8180044258137,
122.217622884656)) ;
#44202 = CARTESIAN_POINT('Ctrl Pts',(-19.7469529682357,-15.6380153454508,
121.919076471871)) ;
#44203 = CARTESIAN_POINT('Ctrl Pts',(-19.2574526738448,-15.8378700432244,
122.196935178988)) ;
#44204 = CARTESIAN_POINT('Ctrl Pts',(-19.2195107524883,-15.6578809628615,
121.893213319316)) ;
#44205 = CARTESIAN_POINT('Ctrl Pts',(-18.8513755370978,-15.8578509730526,
122.321775663419)) ;
#44206 = CARTESIAN_POINT('Ctrl Pts',(-18.7119132760314,-15.6778618926898,
122.049260143643)) ;
#44207 = CARTESIAN_POINT('Ctrl Pts',(-18.5132612033128,-15.8777894351358,
122.577542069427)) ;
#44208 = CARTESIAN_POINT('Ctrl Pts',(-18.2892684219833,-15.6978003547729,
122.368964780256)) ;
#44209 = CARTESIAN_POINT('Ctrl Pts',(-18.2826819587382,-15.8976816283575,
122.932185153396)) ;
#44210 = CARTESIAN_POINT('Ctrl Pts',(-18.0010412603232,-15.7176925479946,
122.812265657401)) ;
#44211 = CARTESIAN_POINT('Ctrl Pts',(-18.1868169762122,-15.9176523433929,
123.34575803658)) ;
#44212 = CARTESIAN_POINT('Ctrl Pts',(-17.8812058283193,-15.73766326303,123.329230583634)) ;
#44213 = CARTESIAN_POINT('Ctrl Pts',(-18.2367313458389,-15.937462015059,123.764098817235)) ;
#44214 = CARTESIAN_POINT('Ctrl Pts',(-17.9435942352086,-15.7574729346961,
123.852155946774)) ;
#44215 = CARTESIAN_POINT('Ctrl Pts',(-18.4277666040295,-15.9574552317502,
124.143691492752)) ;
#44216 = CARTESIAN_POINT('Ctrl Pts',(-18.1823832687672,-15.7774661513873,
124.326648974509)) ;
#44217 = CARTESIAN_POINT('Ctrl Pts',(-18.7346680099378,-15.9773061439465,
124.433713845188)) ;
#44218 = CARTESIAN_POINT('Ctrl Pts',(-18.5660086878683,-15.7973170635836,
124.689180060652)) ;
#44219 = CARTESIAN_POINT('Ctrl Pts',(-19.1263185071962,-15.9973807502655,
124.603150136167)) ;
#44220 = CARTESIAN_POINT('Ctrl Pts',(-19.0555605460036,-15.8173916699027,
124.900980308244)) ;
#44221 = CARTESIAN_POINT('Ctrl Pts',(-19.4769940370043,-16.0138973821489,
124.624006616587)) ;
#44222 = CARTESIAN_POINT('Ctrl Pts',(-19.493934124633,-15.833908301786,124.927054796924)) ;
#44223 = CARTESIAN_POINT('Ctrl Pts',(-19.7517414985942,-16.027236089843,124.568093364996)) ;
#44224 = CARTESIAN_POINT('Ctrl Pts',(-19.837342147255,-15.8472470094801,124.8571673599)) ;
#44225 = CARTESIAN_POINT('Ctrl Pts',(-19.9444057679308,-16.0370784641513,
124.492551498524)) ;
#44226 = CARTESIAN_POINT('Ctrl Pts',(-20.0781804979122,-15.8570893837884,
124.762739875852)) ;
#44227 = CARTESIAN_POINT('Ctrl Pts',(-20.1249049321985,-16.047133484134,124.382567620846)) ;
#44228 = CARTESIAN_POINT('Ctrl Pts',(-20.303796053823,-15.8671444037711,124.625272793233)) ;
#44229 = CARTESIAN_POINT('Ctrl Pts',(-20.3337092884455,-16.0603656407916,
124.198785774196)) ;
#44230 = CARTESIAN_POINT('Ctrl Pts',(-20.5648469001253,-15.8803765604287,
124.395495442102)) ;
#44231 = CARTESIAN_POINT('Ctrl Pts',(-20.5299755382867,-16.0769806081367,
123.904990129354)) ;
#44232 = CARTESIAN_POINT('Ctrl Pts',(-20.8101326079248,-15.8969915277738,
124.02832371329)) ;
#44233 = CARTESIAN_POINT('Ctrl Pts',(-20.6139164154991,-16.0935751951479,
123.562338411869)) ;
#44234 = CARTESIAN_POINT('Ctrl Pts',(-20.9150857051299,-15.913586114785,123.599951810518)) ;
#44235 = CARTESIAN_POINT('Ctrl Pts',(-20.6085033819079,-16.1068087635033,
123.284128846805)) ;
#44236 = CARTESIAN_POINT('Ctrl Pts',(-20.9083137993507,-15.9268196831404,
123.252228775196)) ;
#44237 = CARTESIAN_POINT('Ctrl Pts',(-20.5678420997152,-16.1168523813119,
123.076956614971)) ;
#44238 = CARTESIAN_POINT('Ctrl Pts',(-20.8574915953394,-15.9368633009491,
122.993254896173)) ;
#44239 = CARTESIAN_POINT('Ctrl Pts',(-20.4930658285917,-16.1267393055468,
122.882997750619)) ;
#44240 = CARTESIAN_POINT('Ctrl Pts',(-20.7640240610611,-15.9467502251839,
122.750807958911)) ;
#44241 = CARTESIAN_POINT('Ctrl Pts',(-20.3849611897659,-16.1367299599936,
122.702938885806)) ;
#44242 = CARTESIAN_POINT('Ctrl Pts',(-20.6288932481491,-15.9567408796307,
122.525730668388)) ;
#44243 = CARTESIAN_POINT('Ctrl Pts',(-20.2475814117215,-16.1466917184475,
122.544854107054)) ;
#44244 = CARTESIAN_POINT('Ctrl Pts',(-20.4571800169588,-15.9667026380847,
122.328129169805)) ;
#44245 = CARTESIAN_POINT('Ctrl Pts',(-20.0298504240982,-16.1600315835148,
122.368082548189)) ;
#44246 = CARTESIAN_POINT('Ctrl Pts',(-20.1849716448928,-15.9800425031519,
122.107130949398)) ;
#44247 = CARTESIAN_POINT('Ctrl Pts',(-19.7713257253914,-16.1733403664281,
122.253045017901)) ;
#44248 = CARTESIAN_POINT('Ctrl Pts',(-19.8618390549407,-15.9933512860652,
121.963354376013)) ;
#44249 = CARTESIAN_POINT('Ctrl Pts',(-19.4973854044494,-16.1865361238721,
122.209149372698)) ;
#44250 = CARTESIAN_POINT('Ctrl Pts',(-19.5194352459976,-16.0065470435093,
121.908483591951)) ;
#44251 = CARTESIAN_POINT('Ctrl Pts',(-19.2879723974171,-16.1964980075486,
122.211840246962)) ;
#44252 = CARTESIAN_POINT('Ctrl Pts',(-19.2576646411518,-16.0165089271858,
121.911843868139)) ;
#44253 = CARTESIAN_POINT('Ctrl Pts',(-19.0805966754575,-16.2065411170633,
122.251508529244)) ;
#44254 = CARTESIAN_POINT('Ctrl Pts',(-18.9984455353945,-16.0265520367004,
121.961426597411)) ;
#44255 = CARTESIAN_POINT('Ctrl Pts',(-18.8869132560321,-16.2163933670625,
122.324927691343)) ;
#44256 = CARTESIAN_POINT('Ctrl Pts',(-18.7563398527303,-16.0364042866996,
122.053197919852)) ;
#44257 = CARTESIAN_POINT('Ctrl Pts',(-18.7065271330224,-16.226364904013,122.431685493257)) ;
#44258 = CARTESIAN_POINT('Ctrl Pts',(-18.5308557513542,-16.0463758236501,
122.186642824529)) ;
#44259 = CARTESIAN_POINT('Ctrl Pts',(-18.5470082080786,-16.2363601694905,
122.56851706965)) ;
#44260 = CARTESIAN_POINT('Ctrl Pts',(-18.331455189681,-16.0563710891276,122.357680218404)) ;
#44261 = CARTESIAN_POINT('Ctrl Pts',(-18.413387011108,-16.2463941423641,122.731722217809)) ;
#44262 = CARTESIAN_POINT('Ctrl Pts',(-18.164426495201,-16.0664050620013,122.561684900348)) ;
#44263 = CARTESIAN_POINT('Ctrl Pts',(-18.3116651483155,-16.2562495571265,
122.91224766768)) ;
#44264 = CARTESIAN_POINT('Ctrl Pts',(-18.037271614364,-16.0762604767636,122.787340539645)) ;
#44265 = CARTESIAN_POINT('Ctrl Pts',(-18.2415770596379,-16.2662488346353,
123.110397616458)) ;
#44266 = CARTESIAN_POINT('Ctrl Pts',(-17.9496588451974,-16.0862597542724,
123.035027131255)) ;
#44267 = CARTESIAN_POINT('Ctrl Pts',(-18.2070866766184,-16.2761440187983,
123.315582482187)) ;
#44268 = CARTESIAN_POINT('Ctrl Pts',(-17.9065430994945,-16.0961549384354,
123.291508010341)) ;
#44269 = CARTESIAN_POINT('Ctrl Pts',(-18.2087980539472,-16.2862043984391,
123.527047846686)) ;
#44270 = CARTESIAN_POINT('Ctrl Pts',(-17.908679550301,-16.1062153180762,123.555839709386)) ;
#44271 = CARTESIAN_POINT('Ctrl Pts',(-18.2462808343881,-16.2960542674472,
123.730723195858)) ;
#44272 = CARTESIAN_POINT('Ctrl Pts',(-17.9555303866204,-16.1160651870843,
123.810434776852)) ;
#44273 = CARTESIAN_POINT('Ctrl Pts',(-18.3194286022039,-16.3060858286551,
123.928512270352)) ;
#44274 = CARTESIAN_POINT('Ctrl Pts',(-18.0469625663343,-16.1260967482922,
124.057672087697)) ;
#44275 = CARTESIAN_POINT('Ctrl Pts',(-18.425966779491,-16.3160962775374,124.110026603965)) ;
#44276 = CARTESIAN_POINT('Ctrl Pts',(-18.1801329408613,-16.1361071971745,
124.284566442434)) ;
#44277 = CARTESIAN_POINT('Ctrl Pts',(-18.560797825782,-16.3260030169544,124.268754201217)) ;
#44278 = CARTESIAN_POINT('Ctrl Pts',(-18.3486698658472,-16.1460139365915,
124.482977937529)) ;
#44279 = CARTESIAN_POINT('Ctrl Pts',(-18.7213836715412,-16.3359410330228,
124.402388892912)) ;
#44280 = CARTESIAN_POINT('Ctrl Pts',(-18.5494006644894,-16.1559519526599,
124.65002353466)) ;
#44281 = CARTESIAN_POINT('Ctrl Pts',(-18.9039216281586,-16.3459462794739,
124.506949932254)) ;
#44282 = CARTESIAN_POINT('Ctrl Pts',(-18.7775718601343,-16.1659571991111,
124.780727182674)) ;
#44283 = CARTESIAN_POINT('Ctrl Pts',(-19.1025026858816,-16.3559803405302,
124.578083634945)) ;
#44284 = CARTESIAN_POINT('Ctrl Pts',(-19.0257972538791,-16.1759912601674,
124.869646856981)) ;
#44285 = CARTESIAN_POINT('Ctrl Pts',(-19.3064644872942,-16.3658254215884,
124.613343041828)) ;
#44286 = CARTESIAN_POINT('Ctrl Pts',(-19.2807496064641,-16.1858363412255,
124.913723831211)) ;
#44287 = CARTESIAN_POINT('Ctrl Pts',(-19.5163642119704,-16.3758112275419,
124.61303502221)) ;
#44288 = CARTESIAN_POINT('Ctrl Pts',(-19.5431244270057,-16.195822147179,124.913341409534)) ;
#44289 = CARTESIAN_POINT('Ctrl Pts',(-19.7220636700193,-16.3857460480961,
124.576608850265)) ;
#44290 = CARTESIAN_POINT('Ctrl Pts',(-19.8002495182117,-16.2057569677332,
124.86781116894)) ;
#44291 = CARTESIAN_POINT('Ctrl Pts',(-19.9206078791978,-16.3958035732283,
124.503981755754)) ;
#44292 = CARTESIAN_POINT('Ctrl Pts',(-20.0484305675557,-16.2158144928654,
124.777029790826)) ;
#44293 = CARTESIAN_POINT('Ctrl Pts',(-20.0994392626122,-16.4056252238796,
124.400718208666)) ;
#44294 = CARTESIAN_POINT('Ctrl Pts',(-20.2719717473046,-16.2256361435168,
124.647952173762)) ;
#44295 = CARTESIAN_POINT('Ctrl Pts',(-20.2616227730663,-16.4156812873844,
124.265132165577)) ;
#44296 = CARTESIAN_POINT('Ctrl Pts',(-20.4747026404309,-16.2356922070215,
124.478471590715)) ;
#44297 = CARTESIAN_POINT('Ctrl Pts',(-20.3959657201901,-16.4256219544483,
124.105038813883)) ;
#44298 = CARTESIAN_POINT('Ctrl Pts',(-20.6426334922787,-16.2456328740854,
124.278356285801)) ;
#44299 = CARTESIAN_POINT('Ctrl Pts',(-20.5006527032414,-16.4355263481143,
123.925043149726)) ;
#44300 = CARTESIAN_POINT('Ctrl Pts',(-20.7734945781979,-16.2555372677514,
124.053362462488)) ;
#44301 = CARTESIAN_POINT('Ctrl Pts',(-20.5733913233739,-16.4455728718773,
123.726774248668)) ;
#44302 = CARTESIAN_POINT('Ctrl Pts',(-20.8644201156856,-16.2655837915144,
123.805527276489)) ;
#44303 = CARTESIAN_POINT('Ctrl Pts',(-20.6102491313444,-16.4554689548937,
123.521980484657)) ;
#44304 = CARTESIAN_POINT('Ctrl Pts',(-20.9104948421842,-16.2754798745308,
123.549534920301)) ;
#44305 = CARTESIAN_POINT('Ctrl Pts',(-20.6109490500216,-16.4655356541237,
123.310385747446)) ;
#44306 = CARTESIAN_POINT('Ctrl Pts',(-20.9113721563004,-16.2855465737608,
123.285041710437)) ;
#44307 = CARTESIAN_POINT('Ctrl Pts',(-20.5759933517223,-16.4753592645248,
123.106810422099)) ;
#44308 = CARTESIAN_POINT('Ctrl Pts',(-20.8676796982969,-16.2953701841619,
123.030571216678)) ;
#44309 = CARTESIAN_POINT('Ctrl Pts',(-20.504941661928,-16.4854151247023,122.907730675288)) ;
#44310 = CARTESIAN_POINT('Ctrl Pts',(-20.7788672822299,-16.3054260443394,
122.78172092023)) ;
#44311 = CARTESIAN_POINT('Ctrl Pts',(-20.4014184334642,-16.4953482710072,
122.726342025547)) ;
#44312 = CARTESIAN_POINT('Ctrl Pts',(-20.6494650621371,-16.3153591906443,
122.554983567681)) ;
#44313 = CARTESIAN_POINT('Ctrl Pts',(-20.2681709832991,-16.5052935267778,
122.565253208005)) ;
#44314 = CARTESIAN_POINT('Ctrl Pts',(-20.482907205734,-16.3253044464149,122.353620794924)) ;
#44315 = CARTESIAN_POINT('Ctrl Pts',(-20.1084390136851,-16.5152768252163,
122.429067661281)) ;
#44316 = CARTESIAN_POINT('Ctrl Pts',(-20.2832435137654,-16.3352877448534,
122.183387066587)) ;
#44317 = CARTESIAN_POINT('Ctrl Pts',(-19.9264011878482,-16.5253140053629,
122.322380814143)) ;
#44318 = CARTESIAN_POINT('Ctrl Pts',(-20.0556974557247,-16.345324925,122.050026596419)) ;
#44319 = CARTESIAN_POINT('Ctrl Pts',(-19.7322826676452,-16.5351685580724,
122.24994521566)) ;
#44320 = CARTESIAN_POINT('Ctrl Pts',(-19.8130492090875,-16.3551794777095,
121.959479734219)) ;
#44321 = CARTESIAN_POINT('Ctrl Pts',(-19.5256465946988,-16.5451680765197,
122.211483731313)) ;
#44322 = CARTESIAN_POINT('Ctrl Pts',(-19.5547543717417,-16.3651789961568,
121.911400782604)) ;
#44323 = CARTESIAN_POINT('Ctrl Pts',(-19.3175976842918,-16.5550631589818,
122.209284349518)) ;
#44324 = CARTESIAN_POINT('Ctrl Pts',(-19.2946925229401,-16.3750740786189,
121.908649507765)) ;
#44325 = CARTESIAN_POINT('Ctrl Pts',(-19.1089595995031,-16.5651237044879,
122.243820775951)) ;
#44326 = CARTESIAN_POINT('Ctrl Pts',(-19.0338948184868,-16.385134624125,121.951817978904)) ;
#44327 = CARTESIAN_POINT('Ctrl Pts',(-18.9135973762475,-16.5749730117359,
122.312488918254)) ;
#44328 = CARTESIAN_POINT('Ctrl Pts',(-18.7896903909749,-16.394983931373,122.037651600435)) ;
#44329 = CARTESIAN_POINT('Ctrl Pts',(-18.7296234980827,-16.5850001018232,
122.415390660692)) ;
#44330 = CARTESIAN_POINT('Ctrl Pts',(-18.5597221685601,-16.4050110214604,
122.166277137884)) ;
#44331 = CARTESIAN_POINT('Ctrl Pts',(-18.5666258182799,-16.5950290059602,
122.549139612565)) ;
#44332 = CARTESIAN_POINT('Ctrl Pts',(-18.3559738383633,-16.4150399255973,
122.333461717457)) ;
#44333 = CARTESIAN_POINT('Ctrl Pts',(-18.4315607292266,-16.6048728710595,
122.705925530433)) ;
#44334 = CARTESIAN_POINT('Ctrl Pts',(-18.1871403035161,-16.4248837906966,
122.529443722511)) ;
#44335 = CARTESIAN_POINT('Ctrl Pts',(-18.3236876247588,-16.6148686977679,
122.886268946656)) ;
#44336 = CARTESIAN_POINT('Ctrl Pts',(-18.0522973396058,-16.434879617405,122.754872248908)) ;
#44337 = CARTESIAN_POINT('Ctrl Pts',(-18.2489074259559,-16.6248939144169,
123.083322704059)) ;
#44338 = CARTESIAN_POINT('Ctrl Pts',(-17.9588203685943,-16.444904834054,123.001188739217)) ;
#44339 = CARTESIAN_POINT('Ctrl Pts',(-18.2097358480084,-16.6347837465745,
123.287518104386)) ;
#44340 = CARTESIAN_POINT('Ctrl Pts',(-17.909853990901,-16.4547946662116,123.256433493462)) ;
#44341 = CARTESIAN_POINT('Ctrl Pts',(-18.2062951743029,-16.6447746026592,
123.497522176624)) ;
#44342 = CARTESIAN_POINT('Ctrl Pts',(-17.9055514641145,-16.4647855222963,
123.518938743175)) ;
#44343 = CARTESIAN_POINT('Ctrl Pts',(-18.2392588330395,-16.6547196972521,
123.70398395006)) ;
#44344 = CARTESIAN_POINT('Ctrl Pts',(-17.9467544397181,-16.4747306168892,
123.777016725455)) ;
#44345 = CARTESIAN_POINT('Ctrl Pts',(-18.3072491133093,-16.6646716010202,
123.901857207325)) ;
#44346 = CARTESIAN_POINT('Ctrl Pts',(-18.0317409622789,-16.4846825206573,
124.02435926062)) ;
#44347 = CARTESIAN_POINT('Ctrl Pts',(-18.4095792800101,-16.6747080004896,
124.086372613872)) ;
#44348 = CARTESIAN_POINT('Ctrl Pts',(-18.1596521832206,-16.4947189201267,
124.255004193986)) ;
#44349 = CARTESIAN_POINT('Ctrl Pts',(-18.5403323023959,-16.6845970705783,
124.24801603038)) ;
#44350 = CARTESIAN_POINT('Ctrl Pts',(-18.3230928107259,-16.5046079902154,
124.45706017088)) ;
#44351 = CARTESIAN_POINT('Ctrl Pts',(-18.6984981846878,-16.6945863599492,
124.386161267394)) ;
#44352 = CARTESIAN_POINT('Ctrl Pts',(-18.5207993714946,-16.5145972795863,
124.62974295052)) ;
#44353 = CARTESIAN_POINT('Ctrl Pts',(-18.8777747357484,-16.7045449261589,
124.494277089496)) ;
#44354 = CARTESIAN_POINT('Ctrl Pts',(-18.7448946531672,-16.524555845796,124.764889240736)) ;
#44355 = CARTESIAN_POINT('Ctrl Pts',(-19.071775886629,-16.7144444973757,124.569661405429)) ;
#44356 = CARTESIAN_POINT('Ctrl Pts',(-18.9873964306672,-16.5344554170128,
124.859121187844)) ;
#44357 = CARTESIAN_POINT('Ctrl Pts',(-19.2789592287976,-16.7244924117899,
124.6107434715)) ;
#44358 = CARTESIAN_POINT('Ctrl Pts',(-19.2463751321028,-16.5445033314271,
124.910475054052)) ;
#44359 = CARTESIAN_POINT('Ctrl Pts',(-19.4869725711741,-16.7343877546505,
124.615324364318)) ;
#44360 = CARTESIAN_POINT('Ctrl Pts',(-19.5063926931676,-16.5543986742876,
124.916202482167)) ;
#44361 = CARTESIAN_POINT('Ctrl Pts',(-19.6960268210127,-16.7444494485979,
124.583223874358)) ;
#44362 = CARTESIAN_POINT('Ctrl Pts',(-19.7677103786567,-16.5644603682351,
124.876078188685)) ;
#44363 = CARTESIAN_POINT('Ctrl Pts',(-19.8920494172545,-16.7542939016821,
124.51680250823)) ;
#44364 = CARTESIAN_POINT('Ctrl Pts',(-20.0127402827111,-16.5743048213192,
124.793052261125)) ;
#44365 = CARTESIAN_POINT('Ctrl Pts',(-20.0760402865908,-16.7642545866405,
124.416833948505)) ;
#44366 = CARTESIAN_POINT('Ctrl Pts',(-20.2427297441495,-16.5842655062777,
124.668092227822)) ;
#44367 = CARTESIAN_POINT('Ctrl Pts',(-20.2409080973794,-16.7742905191491,
124.285163854322)) ;
#44368 = CARTESIAN_POINT('Ctrl Pts',(-20.4488151079738,-16.5943014387862,
124.503505578167)) ;
#44369 = CARTESIAN_POINT('Ctrl Pts',(-20.3785099430271,-16.7841791348371,
124.129336922064)) ;
#44370 = CARTESIAN_POINT('Ctrl Pts',(-20.6208188759846,-16.6041900544743,
124.308721850935)) ;
#44371 = CARTESIAN_POINT('Ctrl Pts',(-20.4887120097041,-16.7941935439796,
123.949931511366)) ;
#44372 = CARTESIAN_POINT('Ctrl Pts',(-20.7585722335098,-16.6142044636167,
124.084465548632)) ;
#44373 = CARTESIAN_POINT('Ctrl Pts',(-20.5657191627696,-16.8042273529374,
123.753561423584)) ;
#44374 = CARTESIAN_POINT('Ctrl Pts',(-20.8548321532337,-16.6242382725745,
123.839003471637)) ;
#44375 = CARTESIAN_POINT('Ctrl Pts',(-20.6071867597122,-16.8140578071936,
123.551072730248)) ;
#44376 = CARTESIAN_POINT('Ctrl Pts',(-20.9066678159083,-16.6340687268307,
123.585891332046)) ;
#44377 = CARTESIAN_POINT('Ctrl Pts',(-20.6130753200358,-16.8241354747718,
123.339330931498)) ;
#44378 = CARTESIAN_POINT('Ctrl Pts',(-20.9140293672991,-16.6441463944089,
123.321214560583)) ;
#44379 = CARTESIAN_POINT('Ctrl Pts',(-20.582897122482,-16.833987342894,123.134379068764)) ;
#44380 = CARTESIAN_POINT('Ctrl Pts',(-20.8763072380744,-16.6539982625311,
123.065023312876)) ;
#44381 = CARTESIAN_POINT('Ctrl Pts',(-20.5163171737132,-16.8440603804594,
122.933388787276)) ;
#44382 = CARTESIAN_POINT('Ctrl Pts',(-20.7930831562176,-16.6640713000965,
122.81378563807)) ;
#44383 = CARTESIAN_POINT('Ctrl Pts',(-20.4180968317784,-16.8539029338102,
122.751244860052)) ;
#44384 = CARTESIAN_POINT('Ctrl Pts',(-20.6703077317123,-16.6739138534474,
122.586104119148)) ;
#44385 = CARTESIAN_POINT('Ctrl Pts',(-20.2885154375274,-16.8638833293037,
122.586232749684)) ;
#44386 = CARTESIAN_POINT('Ctrl Pts',(-20.5083311850613,-16.6838942489408,
122.3798384328)) ;
#44387 = CARTESIAN_POINT('Ctrl Pts',(-20.1313776052616,-16.8739018072815,
122.445995465439)) ;
#44388 = CARTESIAN_POINT('Ctrl Pts',(-20.3119093379596,-16.6939127269186,
122.204541346776)) ;
#44389 = CARTESIAN_POINT('Ctrl Pts',(-19.9549021525347,-16.8837851215876,
122.336275047287)) ;
#44390 = CARTESIAN_POINT('Ctrl Pts',(-20.0913143430655,-16.7037960412247,
122.067389838621)) ;
#44391 = CARTESIAN_POINT('Ctrl Pts',(-19.7584673745493,-16.8938534241263,
122.257523549518)) ;
#44392 = CARTESIAN_POINT('Ctrl Pts',(-19.8457714437164,-16.7138643437634,
121.968950139572)) ;
#44393 = CARTESIAN_POINT('Ctrl Pts',(-19.5562266361521,-16.9036834713997,
122.214849851963)) ;
#44394 = CARTESIAN_POINT('Ctrl Pts',(-19.5929691002655,-16.7236943910368,
121.915607289983)) ;
#44395 = CARTESIAN_POINT('Ctrl Pts',(-19.3447520721929,-16.9137503428152,
122.207507802747)) ;
#44396 = CARTESIAN_POINT('Ctrl Pts',(-19.3286263043383,-16.7337612624523,
121.906429428325)) ;
#44397 = CARTESIAN_POINT('Ctrl Pts',(-19.1388680110044,-16.9236393816143,
122.236594479174)) ;
#44398 = CARTESIAN_POINT('Ctrl Pts',(-19.0712701351498,-16.7436503012514,
121.942787563624)) ;
#44399 = CARTESIAN_POINT('Ctrl Pts',(-18.9389316545158,-16.9336360797484,
122.301281101622)) ;
#44400 = CARTESIAN_POINT('Ctrl Pts',(-18.8213494437771,-16.7536469993855,
122.023645715726)) ;
#44401 = CARTESIAN_POINT('Ctrl Pts',(-18.7540959744669,-16.9435885054603,
122.39935968639)) ;
#44402 = CARTESIAN_POINT('Ctrl Pts',(-18.5903042632975,-16.7635994250975,
122.146243992672)) ;
#44403 = CARTESIAN_POINT('Ctrl Pts',(-18.5891273339633,-16.9535298076933,
122.527650967993)) ;
#44404 = CARTESIAN_POINT('Ctrl Pts',(-18.3840928904313,-16.7735407273304,
122.306608387421)) ;
#44405 = CARTESIAN_POINT('Ctrl Pts',(-18.4481547796409,-16.9635130467772,
122.683169969797)) ;
#44406 = CARTESIAN_POINT('Ctrl Pts',(-18.2078769998902,-16.7835239664143,
122.501007316772)) ;
#44407 = CARTESIAN_POINT('Ctrl Pts',(-18.3360050079193,-16.9735518483458,
122.861931794176)) ;
#44408 = CARTESIAN_POINT('Ctrl Pts',(-18.0676897405683,-16.7935627679829,
122.724459360897)) ;
#44409 = CARTESIAN_POINT('Ctrl Pts',(-18.2577181334253,-16.9833999544674,
123.053617948428)) ;
#44410 = CARTESIAN_POINT('Ctrl Pts',(-17.9698306083083,-16.8034108741046,
122.964068373402)) ;
#44411 = CARTESIAN_POINT('Ctrl Pts',(-18.2127741605597,-16.9934601500428,
123.260266613058)) ;
#44412 = CARTESIAN_POINT('Ctrl Pts',(-17.91365079712,-16.8134710696799,123.222378870925)) ;
#44413 = CARTESIAN_POINT('Ctrl Pts',(-18.2047179854304,-17.0033578333542,
123.468199338141)) ;
#44414 = CARTESIAN_POINT('Ctrl Pts',(-17.9035805406861,-16.8233687529913,
123.482295776231)) ;
#44415 = CARTESIAN_POINT('Ctrl Pts',(-18.232302562789,-17.0132888737282,123.675146887286)) ;
#44416 = CARTESIAN_POINT('Ctrl Pts',(-17.938061631521,-16.8332997933653,123.740980891344)) ;
#44417 = CARTESIAN_POINT('Ctrl Pts',(-18.2963248753717,-17.0233310913848,
123.876321281435)) ;
#44418 = CARTESIAN_POINT('Ctrl Pts',(-18.018089634645,-16.8433420110219,123.992448629415)) ;
#44419 = CARTESIAN_POINT('Ctrl Pts',(-18.3926605695863,-17.0332177521188,
124.06050712681)) ;
#44420 = CARTESIAN_POINT('Ctrl Pts',(-18.1385099721154,-16.8532286717559,
124.222681786331)) ;
#44421 = CARTESIAN_POINT('Ctrl Pts',(-18.5205878645769,-17.0432108607212,
124.227139826993)) ;
#44422 = CARTESIAN_POINT('Ctrl Pts',(-18.2984195187527,-16.8632217803584,
124.430972590157)) ;
#44423 = CARTESIAN_POINT('Ctrl Pts',(-18.674831224359,-17.0531565593595,124.368304779055)) ;
#44424 = CARTESIAN_POINT('Ctrl Pts',(-18.4912243940808,-16.8731674789966,
124.607428923697)) ;
#44425 = CARTESIAN_POINT('Ctrl Pts',(-18.8510481817693,-17.0631037816305,
124.480927513138)) ;
#44426 = CARTESIAN_POINT('Ctrl Pts',(-18.7114963548054,-16.8831147012677,
124.748207213336)) ;
#44427 = CARTESIAN_POINT('Ctrl Pts',(-19.0461761282001,-17.0731518072107,
124.561829669415)) ;
#44428 = CARTESIAN_POINT('Ctrl Pts',(-18.9554062189626,-16.8931627268478,
124.849334419905)) ;
#44429 = CARTESIAN_POINT('Ctrl Pts',(-19.2482340808857,-17.0829990543536,
124.606880354677)) ;
#44430 = CARTESIAN_POINT('Ctrl Pts',(-19.2079801341472,-16.9030099739907,
124.905647599935)) ;
#44431 = CARTESIAN_POINT('Ctrl Pts',(-19.4574454956206,-17.0929622314443,
124.616933495659)) ;
#44432 = CARTESIAN_POINT('Ctrl Pts',(-19.4694948938835,-16.9129731510814,
124.918213293)) ;
#44433 = CARTESIAN_POINT('Ctrl Pts',(-19.6665745901204,-17.1029919524777,
124.590015336654)) ;
#44434 = CARTESIAN_POINT('Ctrl Pts',(-19.7309060814548,-16.9230028721148,
124.884564981777)) ;
#44435 = CARTESIAN_POINT('Ctrl Pts',(-19.8654350785867,-17.1128964200106,
124.528216237133)) ;
#44436 = CARTESIAN_POINT('Ctrl Pts',(-19.9794823375165,-16.9329073396477,
124.807315146919)) ;
#44437 = CARTESIAN_POINT('Ctrl Pts',(-20.0527821290814,-17.1229209058404,
124.431754757046)) ;
#44438 = CARTESIAN_POINT('Ctrl Pts',(-20.2136657521584,-16.9429318254775,
124.686737651366)) ;
#44439 = CARTESIAN_POINT('Ctrl Pts',(-20.2186621175981,-17.1328247409643,
124.305869214479)) ;
#44440 = CARTESIAN_POINT('Ctrl Pts',(-20.421015963903,-16.9528356606014,124.529379524787)) ;
#44441 = CARTESIAN_POINT('Ctrl Pts',(-20.362268269371,-17.1428759316743,124.150890987089)) ;
#44442 = CARTESIAN_POINT('Ctrl Pts',(-20.6005228715144,-16.9628868513114,
124.335656354932)) ;
#44443 = CARTESIAN_POINT('Ctrl Pts',(-20.4749404633162,-17.1527603743326,
123.976262382427)) ;
#44444 = CARTESIAN_POINT('Ctrl Pts',(-20.7413629698391,-16.9727712939697,
124.117369250282)) ;
#44445 = CARTESIAN_POINT('Ctrl Pts',(-20.5568101272468,-17.1627533821844,
123.782806970068)) ;
#44446 = CARTESIAN_POINT('Ctrl Pts',(-20.8436992076654,-16.9827643018216,
123.875549411217)) ;
#44447 = CARTESIAN_POINT('Ctrl Pts',(-20.6035732599445,-17.1727017019007,
123.578943176126)) ;
#44448 = CARTESIAN_POINT('Ctrl Pts',(-20.9021522987122,-16.9927126215379,
123.62071892228)) ;
#44449 = CARTESIAN_POINT('Ctrl Pts',(-20.6145132332225,-17.1826385406102,
123.370344649638)) ;
#44450 = CARTESIAN_POINT('Ctrl Pts',(-20.9158262169464,-17.0026494602473,
123.359970070186)) ;
#44451 = CARTESIAN_POINT('Ctrl Pts',(-20.589206594443,-17.1926215295298,123.16197490794)) ;
#44452 = CARTESIAN_POINT('Ctrl Pts',(-20.884191716522,-17.0126324491669,123.099507780396)) ;
#44453 = CARTESIAN_POINT('Ctrl Pts',(-20.5273748243571,-17.2026654088939,
122.960102497268)) ;
#44454 = CARTESIAN_POINT('Ctrl Pts',(-20.8069010684721,-17.022676328531,122.84716775239)) ;
#44455 = CARTESIAN_POINT('Ctrl Pts',(-20.4339045567548,-17.2124934742523,
122.775800529378)) ;
#44456 = CARTESIAN_POINT('Ctrl Pts',(-20.6900614936507,-17.0325043938894,
122.616789554295)) ;
#44457 = CARTESIAN_POINT('Ctrl Pts',(-20.3068302236449,-17.2225705628072,
122.606349678098)) ;
#44458 = CARTESIAN_POINT('Ctrl Pts',(-20.5312178370155,-17.0425814824443,
122.404977090048)) ;
#44459 = CARTESIAN_POINT('Ctrl Pts',(-20.1557656867094,-17.2324207149635,
122.464630719431)) ;
#44460 = CARTESIAN_POINT('Ctrl Pts',(-20.3423853676555,-17.0524316346006,
122.227828485222)) ;
#44461 = CARTESIAN_POINT('Ctrl Pts',(-19.9784714409174,-17.2425011954158,
122.348631483285)) ;
#44462 = CARTESIAN_POINT('Ctrl Pts',(-20.1207672096215,-17.062512115053,122.082830799905)) ;
#44463 = CARTESIAN_POINT('Ctrl Pts',(-19.7888488448021,-17.2523156931847,
122.267175683269)) ;
#44464 = CARTESIAN_POINT('Ctrl Pts',(-19.883737034747,-17.0723266128218,121.981011738217)) ;
#44465 = CARTESIAN_POINT('Ctrl Pts',(-19.582938898268,-17.2623839892048,122.218356656156)) ;
#44466 = CARTESIAN_POINT('Ctrl Pts',(-19.6263495978592,-17.0823949088419,
121.919989507403)) ;
#44467 = CARTESIAN_POINT('Ctrl Pts',(-19.3751318674818,-17.2722828216876,
122.206291542029)) ;
#44468 = CARTESIAN_POINT('Ctrl Pts',(-19.3665898868783,-17.0922937413247,
121.904909547411)) ;
#44469 = CARTESIAN_POINT('Ctrl Pts',(-19.1652559904925,-17.2823357017021,
122.230785552897)) ;
#44470 = CARTESIAN_POINT('Ctrl Pts',(-19.1042454569356,-17.1023466213392,
121.935528536243)) ;
#44471 = CARTESIAN_POINT('Ctrl Pts',(-18.9663707089697,-17.2922055171983,
122.29008319877)) ;
#44472 = CARTESIAN_POINT('Ctrl Pts',(-18.855638307516,-17.1122164368354,122.009652399298)) ;
#44473 = CARTESIAN_POINT('Ctrl Pts',(-18.7770326931717,-17.3022781982811,
122.384835344758)) ;
#44474 = CARTESIAN_POINT('Ctrl Pts',(-18.6189668205951,-17.1222891179182,
122.128093849741)) ;
#44475 = CARTESIAN_POINT('Ctrl Pts',(-18.6109839358936,-17.312110676852,122.507981598294)) ;
#44476 = CARTESIAN_POINT('Ctrl Pts',(-18.4114058096886,-17.1321215964892,
122.282028735497)) ;
#44477 = CARTESIAN_POINT('Ctrl Pts',(-18.4655538333765,-17.3221413108381,
122.660674634817)) ;
#44478 = CARTESIAN_POINT('Ctrl Pts',(-18.2296195608768,-17.1421522304753,
122.472896223419)) ;
#44479 = CARTESIAN_POINT('Ctrl Pts',(-18.349337760532,-17.3321728680573,122.83667359108)) ;
#44480 = CARTESIAN_POINT('Ctrl Pts',(-18.0843508674256,-17.1521837876944,
122.692895741896)) ;
#44481 = CARTESIAN_POINT('Ctrl Pts',(-18.2667484940145,-17.342002576929,123.026088129245)) ;
#44482 = CARTESIAN_POINT('Ctrl Pts',(-17.9811153912308,-17.1620134965661,
122.92966578504)) ;
#44483 = CARTESIAN_POINT('Ctrl Pts',(-18.2169009601804,-17.3519920257311,
123.230102550982)) ;
#44484 = CARTESIAN_POINT('Ctrl Pts',(-17.9188078334472,-17.1720029453682,
123.184684449035)) ;
#44485 = CARTESIAN_POINT('Ctrl Pts',(-18.20369487068,-17.3620358781311,123.440840534949)) ;
#44486 = CARTESIAN_POINT('Ctrl Pts',(-17.9023020185663,-17.1820467977682,
123.44810689289)) ;
#44487 = CARTESIAN_POINT('Ctrl Pts',(-18.2263343781215,-17.3718575914632,
123.646078297448)) ;
#44488 = CARTESIAN_POINT('Ctrl Pts',(-17.9306034522518,-17.1918685111003,
123.704655127921)) ;
#44489 = CARTESIAN_POINT('Ctrl Pts',(-18.2850268408009,-17.3818925964519,
123.848716320605)) ;
#44490 = CARTESIAN_POINT('Ctrl Pts',(-18.0039709952741,-17.201903516089,123.957951976954)) ;
#44491 = CARTESIAN_POINT('Ctrl Pts',(-18.3784463059481,-17.3919174348995,
124.037642069545)) ;
#44492 = CARTESIAN_POINT('Ctrl Pts',(-18.1207470223198,-17.2119283545366,
124.194108297233)) ;
#44493 = CARTESIAN_POINT('Ctrl Pts',(-18.5007395484921,-17.4017696478547,
124.204809326343)) ;
#44494 = CARTESIAN_POINT('Ctrl Pts',(-18.2736158124755,-17.2217805674918,
124.40306698223)) ;
#44495 = CARTESIAN_POINT('Ctrl Pts',(-18.6520320192726,-17.4117596040485,
124.350454005425)) ;
#44496 = CARTESIAN_POINT('Ctrl Pts',(-18.4627330156681,-17.2317705236856,
124.585121418507)) ;
#44497 = CARTESIAN_POINT('Ctrl Pts',(-18.8252452575916,-17.4216877143317,
124.466918774105)) ;
#44498 = CARTESIAN_POINT('Ctrl Pts',(-18.6792511906987,-17.2416986339689,
124.730700896654)) ;
#44499 = CARTESIAN_POINT('Ctrl Pts',(-19.0170751012007,-17.4316763144113,
124.552359737803)) ;
#44500 = CARTESIAN_POINT('Ctrl Pts',(-18.9190395513556,-17.2516872340484,
124.837500135833)) ;
#44501 = CARTESIAN_POINT('Ctrl Pts',(-19.2216700740144,-17.4417029063388,
124.603105177326)) ;
#44502 = CARTESIAN_POINT('Ctrl Pts',(-19.174783750514,-17.2617138259759,124.900929840425)) ;
#44503 = CARTESIAN_POINT('Ctrl Pts',(-19.4289770875473,-17.451588034403,124.617568828443)) ;
#44504 = CARTESIAN_POINT('Ctrl Pts',(-19.4339184087845,-17.2715989540401,
124.919007255833)) ;
#44505 = CARTESIAN_POINT('Ctrl Pts',(-19.6379253432582,-17.4615791518765,
124.596058505797)) ;
#44506 = CARTESIAN_POINT('Ctrl Pts',(-19.6951036459662,-17.2815900715136,
124.892117022616)) ;
#44507 = CARTESIAN_POINT('Ctrl Pts',(-19.8408352338707,-17.4716197677283,
124.537884142129)) ;
#44508 = CARTESIAN_POINT('Ctrl Pts',(-19.9487403100385,-17.2916306873654,
124.819396962872)) ;
#44509 = CARTESIAN_POINT('Ctrl Pts',(-20.0267858411353,-17.481452758582,124.447583261545)) ;
#44510 = CARTESIAN_POINT('Ctrl Pts',(-20.1811784262085,-17.3014636782191,
124.706518373388)) ;
#44511 = CARTESIAN_POINT('Ctrl Pts',(-20.1973125975978,-17.4914458900323,
124.324881213278)) ;
#44512 = CARTESIAN_POINT('Ctrl Pts',(-20.3943355471498,-17.3114568096694,
124.553138757061)) ;
#44513 = CARTESIAN_POINT('Ctrl Pts',(-20.3442096502401,-17.5014779384677,
124.173532276575)) ;
#44514 = CARTESIAN_POINT('Ctrl Pts',(-20.5779551582987,-17.3214888581048,
124.36395098382)) ;
#44515 = CARTESIAN_POINT('Ctrl Pts',(-20.460827682046,-17.5113431850101,124.002039230905)) ;
#44516 = CARTESIAN_POINT('Ctrl Pts',(-20.7237261254064,-17.3313541046472,
124.149582721403)) ;
#44517 = CARTESIAN_POINT('Ctrl Pts',(-20.5472792275311,-17.5213050598369,
123.811278450178)) ;
#44518 = CARTESIAN_POINT('Ctrl Pts',(-20.831788362086,-17.341315979474,123.911130472896)) ;
#44519 = CARTESIAN_POINT('Ctrl Pts',(-20.5993376398069,-17.5313400229482,
123.606847846578)) ;
#44520 = CARTESIAN_POINT('Ctrl Pts',(-20.8968589917748,-17.3513509425853,
123.655591647109)) ;
#44521 = CARTESIAN_POINT('Ctrl Pts',(-20.615228249655,-17.5412248674106,123.399615410114)) ;
#44522 = CARTESIAN_POINT('Ctrl Pts',(-20.9167197829666,-17.3612357870477,
123.396550342786)) ;
#44523 = CARTESIAN_POINT('Ctrl Pts',(-20.5944747720619,-17.5512909202513,
123.189052375223)) ;
#44524 = CARTESIAN_POINT('Ctrl Pts',(-20.8907754476135,-17.3713018398884,
123.133346946234)) ;
#44525 = CARTESIAN_POINT('Ctrl Pts',(-20.5389734302153,-17.5611284361603,
122.989783502597)) ;
#44526 = CARTESIAN_POINT('Ctrl Pts',(-20.8213961192781,-17.3811393557974,
122.88426085308)) ;
#44527 = CARTESIAN_POINT('Ctrl Pts',(-20.4478531306755,-17.5711971842692,
122.798763312751)) ;
#44528 = CARTESIAN_POINT('Ctrl Pts',(-20.7074934610674,-17.3912081039063,
122.645486865945)) ;
#44529 = CARTESIAN_POINT('Ctrl Pts',(-20.3271452161414,-17.5810777013002,
122.629676892913)) ;
#44530 = CARTESIAN_POINT('Ctrl Pts',(-20.5566061673441,-17.4010886209373,
122.434129920283)) ;
#44531 = CARTESIAN_POINT('Ctrl Pts',(-20.1775948897127,-17.5910688882346,
122.482227937037)) ;
#44532 = CARTESIAN_POINT('Ctrl Pts',(-20.3696663136538,-17.4110798078718,
122.249820531952)) ;
#44533 = CARTESIAN_POINT('Ctrl Pts',(-20.0053412492469,-17.6010219545096,
122.363377773261)) ;
#44534 = CARTESIAN_POINT('Ctrl Pts',(-20.1543475643769,-17.4210328741467,
122.101259878823)) ;
#44535 = CARTESIAN_POINT('Ctrl Pts',(-19.8135014291807,-17.6110577920422,
122.275600289609)) ;
#44536 = CARTESIAN_POINT('Ctrl Pts',(-19.9145466995836,-17.4310687116793,
121.991540433781)) ;
#44537 = CARTESIAN_POINT('Ctrl Pts',(-19.6123051874755,-17.6209479182536,
122.223092310276)) ;
#44538 = CARTESIAN_POINT('Ctrl Pts',(-19.6630503154042,-17.4409588378907,
121.925907930665)) ;
#44539 = CARTESIAN_POINT('Ctrl Pts',(-19.4029610311012,-17.6309401001616,
122.205808818066)) ;
#44540 = CARTESIAN_POINT('Ctrl Pts',(-19.4013697921715,-17.4509510197987,
121.904306259386)) ;
#44541 = CARTESIAN_POINT('Ctrl Pts',(-19.1947594778902,-17.6408860401002,
122.225118763395)) ;
#44542 = CARTESIAN_POINT('Ctrl Pts',(-19.1411178680801,-17.4608969597373,
121.928446401877)) ;
#44543 = CARTESIAN_POINT('Ctrl Pts',(-18.9929258923836,-17.6508332238642,
122.279886430677)) ;
#44544 = CARTESIAN_POINT('Ctrl Pts',(-18.88882641169,-17.4708441435014,121.996908692805)) ;
#44545 = CARTESIAN_POINT('Ctrl Pts',(-18.8018677982958,-17.6608811621717,
122.369974731862)) ;
#44546 = CARTESIAN_POINT('Ctrl Pts',(-18.6500049664529,-17.4808920818088,
122.109521528359)) ;
#44547 = CARTESIAN_POINT('Ctrl Pts',(-18.6326849760237,-17.670728796912,122.489300515306)) ;
#44548 = CARTESIAN_POINT('Ctrl Pts',(-18.4385276907917,-17.4907397165491,
122.258681232222)) ;
#44549 = CARTESIAN_POINT('Ctrl Pts',(-18.48464394166,-17.6806905108858,122.637419729703)) ;
#44550 = CARTESIAN_POINT('Ctrl Pts',(-18.2534782916843,-17.5007014305229,
122.443832320291)) ;
#44551 = CARTESIAN_POINT('Ctrl Pts',(-18.3639692527773,-17.6907191456766,
122.810318421013)) ;
#44552 = CARTESIAN_POINT('Ctrl Pts',(-18.1026371828242,-17.5107300653138,
122.659957308441)) ;
#44553 = CARTESIAN_POINT('Ctrl Pts',(-18.2761446006497,-17.7006294642738,
122.999238769557)) ;
#44554 = CARTESIAN_POINT('Ctrl Pts',(-17.9928588043532,-17.5206403839109,
122.896109111999)) ;
#44555 = CARTESIAN_POINT('Ctrl Pts',(-18.2217890454544,-17.7105643205853,
123.200911892758)) ;
#44556 = CARTESIAN_POINT('Ctrl Pts',(-17.9249170447996,-17.5305752402224,
123.148201377917)) ;
#44557 = CARTESIAN_POINT('Ctrl Pts',(-18.2032822313656,-17.720605556546,123.411187682898)) ;
#44558 = CARTESIAN_POINT('Ctrl Pts',(-17.9017863181592,-17.5406164761831,
123.41104640664)) ;
#44559 = CARTESIAN_POINT('Ctrl Pts',(-18.2211170108079,-17.730492328126,123.618292553974)) ;
#44560 = CARTESIAN_POINT('Ctrl Pts',(-17.9240826085059,-17.5505032477631,
123.669927416836)) ;
#44561 = CARTESIAN_POINT('Ctrl Pts',(-18.2749965572381,-17.7404925068322,
123.821474487423)) ;
#44562 = CARTESIAN_POINT('Ctrl Pts',(-17.991434789336,-17.5605034264693,123.923904177985)) ;
#44563 = CARTESIAN_POINT('Ctrl Pts',(-18.36246816189,-17.7504097850418,124.010768806246)) ;
#44564 = CARTESIAN_POINT('Ctrl Pts',(-18.1007768933539,-17.5704207046789,
124.160520976212)) ;
#44565 = CARTESIAN_POINT('Ctrl Pts',(-18.48305480673,-17.7604570314554,124.184154003306)) ;
#44566 = CARTESIAN_POINT('Ctrl Pts',(-18.2515125585857,-17.5804679510926,
124.377250917313)) ;
#44567 = CARTESIAN_POINT('Ctrl Pts',(-18.629232331941,-17.7703309204367,124.331582621373)) ;
#44568 = CARTESIAN_POINT('Ctrl Pts',(-18.4342365122274,-17.5903418400739,
124.561534748343)) ;
#44569 = CARTESIAN_POINT('Ctrl Pts',(-18.8019032378778,-17.7803929380173,
124.453733894309)) ;
#44570 = CARTESIAN_POINT('Ctrl Pts',(-18.6500768441802,-17.6004038576544,
124.714221581004)) ;
#44571 = CARTESIAN_POINT('Ctrl Pts',(-18.9895800757917,-17.7902639997516,
124.542325237439)) ;
#44572 = CARTESIAN_POINT('Ctrl Pts',(-18.8846741125319,-17.6102749193887,
124.82495821564)) ;
#44573 = CARTESIAN_POINT('Ctrl Pts',(-19.1921134940513,-17.8002580631119,
124.598226493753)) ;
#44574 = CARTESIAN_POINT('Ctrl Pts',(-19.1378416764729,-17.620268982749,124.894832090563)) ;
#44575 = CARTESIAN_POINT('Ctrl Pts',(-19.4021121856622,-17.8102902211453,
124.617721341239)) ;
#44576 = CARTESIAN_POINT('Ctrl Pts',(-19.4003404043878,-17.6303011407824,
124.919197850728)) ;
#44577 = CARTESIAN_POINT('Ctrl Pts',(-19.608844588004,-17.8201540973854,124.601197546684)) ;
#44578 = CARTESIAN_POINT('Ctrl Pts',(-19.6587556166457,-17.6401650170226,
124.898540308878)) ;
#44579 = CARTESIAN_POINT('Ctrl Pts',(-19.8137331839509,-17.8302246120237,
124.54797156307)) ;
#44580 = CARTESIAN_POINT('Ctrl Pts',(-19.9148657636072,-17.6502355316608,
124.832005118292)) ;
#44581 = CARTESIAN_POINT('Ctrl Pts',(-20.0019178911935,-17.8400652489647,
124.461988692631)) ;
#44582 = CARTESIAN_POINT('Ctrl Pts',(-20.150095477634,-17.6600761686018,124.724523892798)) ;
#44583 = CARTESIAN_POINT('Ctrl Pts',(-20.1748685848524,-17.8500323778049,
124.343718173055)) ;
#44584 = CARTESIAN_POINT('Ctrl Pts',(-20.3662817216806,-17.670043297442,124.576684081866)) ;
#44585 = CARTESIAN_POINT('Ctrl Pts',(-20.3252263227975,-17.8600463509294,
124.196347627969)) ;
#44586 = CARTESIAN_POINT('Ctrl Pts',(-20.5542290543161,-17.6800572705665,
124.392466662647)) ;
#44587 = CARTESIAN_POINT('Ctrl Pts',(-20.4877929513438,-17.8733310847927,
123.96921781494)) ;
#44588 = CARTESIAN_POINT('Ctrl Pts',(-20.7574242465171,-17.6933420044298,
124.108563216833)) ;
#44589 = CARTESIAN_POINT('Ctrl Pts',(-20.5871211093539,-17.8865563495074,
123.706157520284)) ;
#44590 = CARTESIAN_POINT('Ctrl Pts',(-20.8815792327918,-17.7065672691446,
123.779776387227)) ;
#44591 = CARTESIAN_POINT('Ctrl Pts',(-20.6152234023706,-17.8998668720623,
123.427758973367)) ;
#44592 = CARTESIAN_POINT('Ctrl Pts',(-20.9167156267444,-17.7198777916994,
123.431719811702)) ;
#44593 = CARTESIAN_POINT('Ctrl Pts',(-20.5994871791015,-17.9098955169645,
123.217511431126)) ;
#44594 = CARTESIAN_POINT('Ctrl Pts',(-20.8970403045933,-17.7299064366016,
123.168922156233)) ;
#44595 = CARTESIAN_POINT('Ctrl Pts',(-20.5484258087731,-17.9197765493184,
123.01615172322)) ;
#44596 = CARTESIAN_POINT('Ctrl Pts',(-20.833211337434,-17.7397874689555,122.917220164191)) ;
#44597 = CARTESIAN_POINT('Ctrl Pts',(-20.462715022261,-17.9297575219985,122.82462433537)) ;
#44598 = CARTESIAN_POINT('Ctrl Pts',(-20.7260717926928,-17.7497684416356,
122.677813694401)) ;
#44599 = CARTESIAN_POINT('Ctrl Pts',(-20.3449102482183,-17.9397386495845,
122.650999042694)) ;
#44600 = CARTESIAN_POINT('Ctrl Pts',(-20.5788081877206,-17.7597495692216,
122.460780265078)) ;
#44601 = CARTESIAN_POINT('Ctrl Pts',(-20.1513290480844,-17.9529818398459,
122.450788742147)) ;
#44602 = CARTESIAN_POINT('Ctrl Pts',(-20.3368568947388,-17.772992759483,122.21053545582)) ;
#44603 = CARTESIAN_POINT('Ctrl Pts',(-19.8474795977767,-17.9696498352067,
122.268601957147)) ;
#44604 = CARTESIAN_POINT('Ctrl Pts',(-19.9569936985326,-17.7896607548438,
121.982786748505)) ;
#44605 = CARTESIAN_POINT('Ctrl Pts',(-19.5025885485555,-17.9861703352187,
122.201337269194)) ;
#44606 = CARTESIAN_POINT('Ctrl Pts',(-19.5259606159641,-17.8061812548558,
121.898720902141)) ;
#44607 = CARTESIAN_POINT('Ctrl Pts',(-19.2234322226272,-17.9994833515347,
122.220261932405)) ;
#44608 = CARTESIAN_POINT('Ctrl Pts',(-19.1769501917683,-17.8194942711718,
121.922374301912)) ;
#44609 = CARTESIAN_POINT('Ctrl Pts',(-19.0209334833378,-18.0093999097677,
122.270017422137)) ;
#44610 = CARTESIAN_POINT('Ctrl Pts',(-18.9238414463951,-17.8294108294048,
121.984571342196)) ;
#44611 = CARTESIAN_POINT('Ctrl Pts',(-18.8281337131634,-18.0194275780706,
122.355152407899)) ;
#44612 = CARTESIAN_POINT('Ctrl Pts',(-18.6828367951169,-17.8394384977077,
122.090994480729)) ;
#44613 = CARTESIAN_POINT('Ctrl Pts',(-18.5974653025486,-18.0326081678152,
122.508905891752)) ;
#44614 = CARTESIAN_POINT('Ctrl Pts',(-18.394515897223,-17.8526190874524,122.283176068422)) ;
#44615 = CARTESIAN_POINT('Ctrl Pts',(-18.3626740824795,-18.0493563069346,
122.776403364024)) ;
#44616 = CARTESIAN_POINT('Ctrl Pts',(-18.1010163558912,-17.8693672265717,
122.617564692546)) ;
#44617 = CARTESIAN_POINT('Ctrl Pts',(-18.2093429381581,-18.0691510494452,
123.168585983566)) ;
#44618 = CARTESIAN_POINT('Ctrl Pts',(-17.909361184572,-17.8891619690823,123.107788785577)) ;
#44619 = CARTESIAN_POINT('Ctrl Pts',(-18.1984950373618,-18.089195442254,123.594497284543)) ;
#44620 = CARTESIAN_POINT('Ctrl Pts',(-17.8958042831171,-17.9092063618911,
123.640179567808)) ;
#44621 = CARTESIAN_POINT('Ctrl Pts',(-18.3326878160101,-18.1090346245527,
123.994538645704)) ;
#44622 = CARTESIAN_POINT('Ctrl Pts',(-18.0635490482974,-17.9290455441898,
124.140228438831)) ;
#44623 = CARTESIAN_POINT('Ctrl Pts',(-18.595526380158,-18.1289599482456,124.326686433183)) ;
#44624 = CARTESIAN_POINT('Ctrl Pts',(-18.3920994920008,-17.9489708678827,
124.555410464658)) ;
#44625 = CARTESIAN_POINT('Ctrl Pts',(-18.9560767803861,-18.1488835862971,
124.549228315396)) ;
#44626 = CARTESIAN_POINT('Ctrl Pts',(-18.842788696369,-17.9688945059342,124.833584548175)) ;
#44627 = CARTESIAN_POINT('Ctrl Pts',(-19.3708100254435,-18.1688084597626,
124.63548572576)) ;
#44628 = CARTESIAN_POINT('Ctrl Pts',(-19.3612051307133,-17.9888193793997,
124.941403037166)) ;
#44629 = CARTESIAN_POINT('Ctrl Pts',(-19.7892611661208,-18.1886870668415,
124.575714298968)) ;
#44630 = CARTESIAN_POINT('Ctrl Pts',(-19.8842672961237,-18.0086979864787,
124.866686275026)) ;
#44631 = CARTESIAN_POINT('Ctrl Pts',(-20.1641187112948,-18.2086645096735,
124.375945013966)) ;
#44632 = CARTESIAN_POINT('Ctrl Pts',(-20.3528378762813,-18.0286754293106,
124.616972672775)) ;
#44633 = CARTESIAN_POINT('Ctrl Pts',(-20.4474662277744,-18.2285963577582,
124.06073373373)) ;
#44634 = CARTESIAN_POINT('Ctrl Pts',(-20.7070199751766,-18.0486072773953,
124.222957551387)) ;
#44635 = CARTESIAN_POINT('Ctrl Pts',(-20.6063082660546,-18.2484916261008,
123.668688283209)) ;
#44636 = CARTESIAN_POINT('Ctrl Pts',(-20.9055702118375,-18.0685025457379,
123.732901280458)) ;
#44637 = CARTESIAN_POINT('Ctrl Pts',(-20.6223259515978,-18.2684141245129,
123.245374252905)) ;
#44638 = CARTESIAN_POINT('Ctrl Pts',(-20.9255908588565,-18.08842504415,123.203759760806)) ;
#44639 = CARTESIAN_POINT('Ctrl Pts',(-20.4925770960382,-18.2883736063889,
122.841276292266)) ;
#44640 = CARTESIAN_POINT('Ctrl Pts',(-20.7634037510858,-18.108384526026,122.69863823452)) ;
#44641 = CARTESIAN_POINT('Ctrl Pts',(-20.2338987435689,-18.3082513588482,
122.507109401429)) ;
#44642 = CARTESIAN_POINT('Ctrl Pts',(-20.4400561873198,-18.1282622784854,
122.280931726728)) ;
#44643 = CARTESIAN_POINT('Ctrl Pts',(-19.8771610118705,-18.3281331495828,
122.280132547987)) ;
#44644 = CARTESIAN_POINT('Ctrl Pts',(-19.9941357017279,-18.1481440692199,
121.997211525704)) ;
#44645 = CARTESIAN_POINT('Ctrl Pts',(-19.4603627437856,-18.3482064884338,
122.188495687106)) ;
#44646 = CARTESIAN_POINT('Ctrl Pts',(-19.473136676439,-18.1682174080709,121.882665391242)) ;
#44647 = CARTESIAN_POINT('Ctrl Pts',(-19.0428183765593,-18.3680109556696,
122.243747752997)) ;
#44648 = CARTESIAN_POINT('Ctrl Pts',(-18.9512092802025,-18.1880218753067,
121.951729931367)) ;
#44649 = CARTESIAN_POINT('Ctrl Pts',(-18.6655136826897,-18.3879942960774,
122.439019897287)) ;
#44650 = CARTESIAN_POINT('Ctrl Pts',(-18.4795781028299,-18.2080052157145,
122.195819043251)) ;
#44651 = CARTESIAN_POINT('Ctrl Pts',(-18.3789384655421,-18.4079092606754,
122.750760297529)) ;
#44652 = CARTESIAN_POINT('Ctrl Pts',(-18.1213593079001,-18.2279201803125,
122.585493056781)) ;
#44653 = CARTESIAN_POINT('Ctrl Pts',(-18.2152038691917,-18.4277777953917,
123.140286780608)) ;
#44654 = CARTESIAN_POINT('Ctrl Pts',(-17.9166900271828,-18.2477887150289,
123.072398846961)) ;
#44655 = CARTESIAN_POINT('Ctrl Pts',(-18.1947300807791,-18.4478301796035,
123.566037893384)) ;
#44656 = CARTESIAN_POINT('Ctrl Pts',(-17.891096129626,-18.2678410992406,123.604588275985)) ;
#44657 = CARTESIAN_POINT('Ctrl Pts',(-18.3185671471098,-18.4676041433927,
123.96801283456)) ;
#44658 = CARTESIAN_POINT('Ctrl Pts',(-18.0458895721995,-18.2876150630298,
124.107054946119)) ;
#44659 = CARTESIAN_POINT('Ctrl Pts',(-18.5752678737993,-18.487658522414,124.308284568343)) ;
#44660 = CARTESIAN_POINT('Ctrl Pts',(-18.3667637788578,-18.3076694420512,
124.53239666562)) ;
#44661 = CARTESIAN_POINT('Ctrl Pts',(-18.9284212326359,-18.5074552599873,
124.537569903936)) ;
#44662 = CARTESIAN_POINT('Ctrl Pts',(-18.8082021318572,-18.3274661796244,
124.819004328744)) ;
#44663 = CARTESIAN_POINT('Ctrl Pts',(-19.3416803678244,-18.5274230723387,
124.634498823647)) ;
#44664 = CARTESIAN_POINT('Ctrl Pts',(-19.3247749684746,-18.3474339919759,
124.940168786496)) ;
#44665 = CARTESIAN_POINT('Ctrl Pts',(-19.7631205986786,-18.5473820484038,
124.583927911147)) ;
#44666 = CARTESIAN_POINT('Ctrl Pts',(-19.8515753099783,-18.3673929680409,
124.876958419446)) ;
#44667 = CARTESIAN_POINT('Ctrl Pts',(-20.1408243512989,-18.5672769666812,
124.393475715096)) ;
#44668 = CARTESIAN_POINT('Ctrl Pts',(-20.323705737491,-18.3872878863183,124.638896796326)) ;
#44669 = CARTESIAN_POINT('Ctrl Pts',(-20.4312496937618,-18.5871732791315,
124.085918903188)) ;
#44670 = CARTESIAN_POINT('Ctrl Pts',(-20.6867396805035,-18.4071841987686,
124.254454112951)) ;
#44671 = CARTESIAN_POINT('Ctrl Pts',(-20.5998462621265,-18.6070812125056,
123.69761409053)) ;
#44672 = CARTESIAN_POINT('Ctrl Pts',(-20.8974889909594,-18.4270921321427,
123.769075405427)) ;
#44673 = CARTESIAN_POINT('Ctrl Pts',(-20.6258188714983,-18.6270311027941,
123.274258003805)) ;
#44674 = CARTESIAN_POINT('Ctrl Pts',(-20.9299591274622,-18.4470420224312,
123.239880881336)) ;
#44675 = CARTESIAN_POINT('Ctrl Pts',(-20.5065921902261,-18.6469083332954,
122.868736889825)) ;
#44676 = CARTESIAN_POINT('Ctrl Pts',(-20.7809301918273,-18.4669192529325,
122.732978965387)) ;
#44677 = CARTESIAN_POINT('Ctrl Pts',(-20.2550219026943,-18.6668910021664,
122.526359546569)) ;
#44678 = CARTESIAN_POINT('Ctrl Pts',(-20.4664719534886,-18.4869019218035,
122.305004321908)) ;
#44679 = CARTESIAN_POINT('Ctrl Pts',(-19.9023778798508,-18.6868238887468,
122.291166846904)) ;
#44680 = CARTESIAN_POINT('Ctrl Pts',(-20.0256670326121,-18.5068348083839,
122.011010324086)) ;
#44681 = CARTESIAN_POINT('Ctrl Pts',(-19.4912013862512,-18.7067366347647,
122.190280264544)) ;
#44682 = CARTESIAN_POINT('Ctrl Pts',(-19.5117084694408,-18.5267475544018,
121.884894904274)) ;
#44683 = CARTESIAN_POINT('Ctrl Pts',(-19.1409101901299,-18.7233063561065,
122.227714641459)) ;
#44684 = CARTESIAN_POINT('Ctrl Pts',(-19.0738118336098,-18.5433172757436,
121.93169130508)) ;
#44685 = CARTESIAN_POINT('Ctrl Pts',(-18.8799531775115,-18.7366063674115,
122.328226065219)) ;
#44686 = CARTESIAN_POINT('Ctrl Pts',(-18.7476501460358,-18.5566172870486,
122.057314468906)) ;
#44687 = CARTESIAN_POINT('Ctrl Pts',(-18.6408115625997,-18.7498765551614,
122.471815662188)) ;
#44688 = CARTESIAN_POINT('Ctrl Pts',(-18.4486656986035,-18.5698874747985,
122.23684236878)) ;
#44689 = CARTESIAN_POINT('Ctrl Pts',(-18.3949285657691,-18.7665039375268,
122.725952569314)) ;
#44690 = CARTESIAN_POINT('Ctrl Pts',(-18.1413722273347,-18.5865148571639,
122.554451895096)) ;
#44691 = CARTESIAN_POINT('Ctrl Pts',(-18.2507607995782,-18.783126227272,123.048601698657)) ;
#44692 = CARTESIAN_POINT('Ctrl Pts',(-17.9611265356219,-18.6031371469091,
122.957810899862)) ;
#44693 = CARTESIAN_POINT('Ctrl Pts',(-18.2066124842382,-18.7963714416665,
123.323560231487)) ;
#44694 = CARTESIAN_POINT('Ctrl Pts',(-17.9059528961361,-18.6163823613036,
123.301475150408)) ;
#44695 = CARTESIAN_POINT('Ctrl Pts',(-18.2091963113951,-18.8062834066272,
123.531933666297)) ;
#44696 = CARTESIAN_POINT('Ctrl Pts',(-17.9091768534027,-18.6262943262643,
123.561948497621)) ;
#44697 = CARTESIAN_POINT('Ctrl Pts',(-18.2487269856474,-18.8163420297916,
123.739647393853)) ;
#44698 = CARTESIAN_POINT('Ctrl Pts',(-17.9585883655337,-18.6363529494288,
123.821589557109)) ;
#44699 = CARTESIAN_POINT('Ctrl Pts',(-18.3218273859011,-18.8261821439075,
123.933204366604)) ;
#44700 = CARTESIAN_POINT('Ctrl Pts',(-18.0499609717764,-18.6461930635446,
124.06353698501)) ;
#44701 = CARTESIAN_POINT('Ctrl Pts',(-18.4296324438484,-18.8362479288651,
124.115263613763)) ;
#44702 = CARTESIAN_POINT('Ctrl Pts',(-18.1847150492908,-18.6562588485022,
124.291112489594)) ;
#44703 = CARTESIAN_POINT('Ctrl Pts',(-18.5650197569021,-18.846131246653,124.27291340767)) ;
#44704 = CARTESIAN_POINT('Ctrl Pts',(-18.3539469883158,-18.6661421662901,
124.488176476276)) ;
#44705 = CARTESIAN_POINT('Ctrl Pts',(-18.7271216090986,-18.8561206845115,
124.40639870705)) ;
#44706 = CARTESIAN_POINT('Ctrl Pts',(-18.5565725704209,-18.6761316041487,
124.655035297587)) ;
#44707 = CARTESIAN_POINT('Ctrl Pts',(-18.9095316281554,-18.8660843985643,
124.509393822221)) ;
#44708 = CARTESIAN_POINT('Ctrl Pts',(-18.7845837390266,-18.6860953182014,
124.783781642268)) ;
#44709 = CARTESIAN_POINT('Ctrl Pts',(-19.1076061689565,-18.8760794102235,
124.579581320828)) ;
#44710 = CARTESIAN_POINT('Ctrl Pts',(-19.0321760408685,-18.6960903298606,
124.871518685265)) ;
#44711 = CARTESIAN_POINT('Ctrl Pts',(-19.3157436958266,-18.8861157019177,
124.61412399333)) ;
#44712 = CARTESIAN_POINT('Ctrl Pts',(-19.2923475774158,-18.7061266215549,
124.914699798494)) ;
#44713 = CARTESIAN_POINT('Ctrl Pts',(-19.5227505678203,-18.8959620796112,
124.612380202904)) ;
#44714 = CARTESIAN_POINT('Ctrl Pts',(-19.5511061455371,-18.7159729992483,
124.912522869748)) ;
#44715 = CARTESIAN_POINT('Ctrl Pts',(-19.7292055330348,-18.9059470237619,
124.57459229136)) ;
#44716 = CARTESIAN_POINT('Ctrl Pts',(-19.8091754394204,-18.725957943399,124.865290742735)) ;
#44717 = CARTESIAN_POINT('Ctrl Pts',(-19.9251198106704,-18.9158839948918,
124.501974601842)) ;
#44718 = CARTESIAN_POINT('Ctrl Pts',(-20.0540693302501,-18.735894914529,124.774521245313)) ;
#44719 = CARTESIAN_POINT('Ctrl Pts',(-20.1073932158431,-18.9259337795236,
124.395175327921)) ;
#44720 = CARTESIAN_POINT('Ctrl Pts',(-20.2819125648932,-18.7459446991607,
124.64102455522)) ;
#44721 = CARTESIAN_POINT('Ctrl Pts',(-20.2652907922645,-18.9357842416011,
124.261160532584)) ;
#44722 = CARTESIAN_POINT('Ctrl Pts',(-20.4792864441643,-18.7557951612382,
124.473508135846)) ;
#44723 = CARTESIAN_POINT('Ctrl Pts',(-20.3995458132042,-18.9457562551215,
124.100179995345)) ;
#44724 = CARTESIAN_POINT('Ctrl Pts',(-20.6471074503595,-18.7657671747586,
124.272284173853)) ;
#44725 = CARTESIAN_POINT('Ctrl Pts',(-20.5040579564351,-18.9557514022409,
123.91784560784)) ;
#44726 = CARTESIAN_POINT('Ctrl Pts',(-20.7777500986428,-18.775762321878,124.044367513356)) ;
#44727 = CARTESIAN_POINT('Ctrl Pts',(-20.5753422248365,-18.965785371977,123.71932854599)) ;
#44728 = CARTESIAN_POINT('Ctrl Pts',(-20.86685809816,-18.7857962916141,123.796222100934)) ;
#44729 = CARTESIAN_POINT('Ctrl Pts',(-20.6107665468007,-18.9756409176476,
123.515165091888)) ;
#44730 = CARTESIAN_POINT('Ctrl Pts',(-20.9111412970602,-18.7956518372847,
123.541018035015)) ;
#44731 = CARTESIAN_POINT('Ctrl Pts',(-20.6104909571507,-18.9856396746608,
123.304993816628)) ;
#44732 = CARTESIAN_POINT('Ctrl Pts',(-20.9107995971931,-18.8056505942979,
123.278303845419)) ;
#44733 = CARTESIAN_POINT('Ctrl Pts',(-20.5742854817518,-18.995536809898,123.100067497722)) ;
#44734 = CARTESIAN_POINT('Ctrl Pts',(-20.8655454311932,-18.8155477295351,
123.022145216685)) ;
#44735 = CARTESIAN_POINT('Ctrl Pts',(-20.5019793355474,-19.0055899057376,
122.901496245715)) ;
#44736 = CARTESIAN_POINT('Ctrl Pts',(-20.7751653502272,-18.8256008253747,
122.773930212868)) ;
#44737 = CARTESIAN_POINT('Ctrl Pts',(-20.3980758274042,-19.0154734144682,
122.721542018855)) ;
#44738 = CARTESIAN_POINT('Ctrl Pts',(-20.6452882013384,-18.8354843341053,
122.54898577994)) ;
#44739 = CARTESIAN_POINT('Ctrl Pts',(-20.2633899531571,-19.0254682871143,
122.560268873648)) ;
#44740 = CARTESIAN_POINT('Ctrl Pts',(-20.4769328739096,-18.8454792067514,
122.347392525977)) ;
#44741 = CARTESIAN_POINT('Ctrl Pts',(-20.1021192146536,-19.03548824875,122.424730589061)) ;
#44742 = CARTESIAN_POINT('Ctrl Pts',(-20.2753461930725,-18.8554991683871,
122.177967546874)) ;
#44743 = CARTESIAN_POINT('Ctrl Pts',(-19.9219503779301,-19.0453936125498,
122.320315131971)) ;
#44744 = CARTESIAN_POINT('Ctrl Pts',(-20.0501362495513,-18.865404532187,122.047445707246)) ;
#44745 = CARTESIAN_POINT('Ctrl Pts',(-19.725850127901,-19.0553342001574,122.248117440437)) ;
#44746 = CARTESIAN_POINT('Ctrl Pts',(-19.8050116122211,-18.8753451197945,
121.957195984845)) ;
#44747 = CARTESIAN_POINT('Ctrl Pts',(-19.5188889597631,-19.065337018258,122.21070880174)) ;
#44748 = CARTESIAN_POINT('Ctrl Pts',(-19.5463105434524,-18.8853479378952,
121.910432554943)) ;
#44749 = CARTESIAN_POINT('Ctrl Pts',(-19.3079401318783,-19.0753717299822,
122.210144775601)) ;
#44750 = CARTESIAN_POINT('Ctrl Pts',(-19.2826245313416,-18.8953826496193,
121.909724812354)) ;
#44751 = CARTESIAN_POINT('Ctrl Pts',(-19.1039450954541,-19.0852166367195,
122.245193265837)) ;
#44752 = CARTESIAN_POINT('Ctrl Pts',(-19.0276297317745,-18.9052275563566,
121.953532899944)) ;
#44753 = CARTESIAN_POINT('Ctrl Pts',(-18.9062559735361,-19.0952024892885,
122.315743265558)) ;
#44754 = CARTESIAN_POINT('Ctrl Pts',(-18.7805173029334,-18.9152134089256,
122.041718002023)) ;
#44755 = CARTESIAN_POINT('Ctrl Pts',(-18.7246158514163,-19.1051372977015,
122.418922406294)) ;
#44756 = CARTESIAN_POINT('Ctrl Pts',(-18.5534655977386,-18.9251482173387,
122.170689853634)) ;
#44757 = CARTESIAN_POINT('Ctrl Pts',(-18.5618355249981,-19.1151948247826,
122.553818901335)) ;
#44758 = CARTESIAN_POINT('Ctrl Pts',(-18.3499886138001,-18.9352057444197,
122.33930838977)) ;
#44759 = CARTESIAN_POINT('Ctrl Pts',(-18.4278858922511,-19.1250164797797,
122.710986226802)) ;
#44760 = CARTESIAN_POINT('Ctrl Pts',(-18.1825491267777,-18.9450273994168,
122.535766487528)) ;
#44761 = CARTESIAN_POINT('Ctrl Pts',(-18.3204432885905,-19.1350725239527,
122.893038269463)) ;
#44762 = CARTESIAN_POINT('Ctrl Pts',(-18.0482437942149,-18.9550834435898,
122.76333018742)) ;
#44763 = CARTESIAN_POINT('Ctrl Pts',(-18.2474379776068,-19.1450132639979,
123.088867079134)) ;
#44764 = CARTESIAN_POINT('Ctrl Pts',(-17.9569846493071,-18.965024183635,123.008115620737)) ;
#44765 = CARTESIAN_POINT('Ctrl Pts',(-18.2090421542517,-19.1549173850707,
123.293514642458)) ;
#44766 = CARTESIAN_POINT('Ctrl Pts',(-17.9089873948513,-18.9749283047079,
123.26392514927)) ;
#44767 = CARTESIAN_POINT('Ctrl Pts',(-18.2068596104492,-19.164964926225,123.504719529866)) ;
#44768 = CARTESIAN_POINT('Ctrl Pts',(-17.9062567714271,-18.9849758458621,
123.527931134947)) ;
#44769 = CARTESIAN_POINT('Ctrl Pts',(-18.2407268057589,-19.1748636778254,
123.710075861997)) ;
#44770 = CARTESIAN_POINT('Ctrl Pts',(-17.9485884795945,-18.9948745974625,
123.784627499312)) ;
#44771 = CARTESIAN_POINT('Ctrl Pts',(-18.3106763440572,-19.1849121567912,
123.909385049677)) ;
#44772 = CARTESIAN_POINT('Ctrl Pts',(-18.0360231031298,-19.0049230764283,
124.033764662916)) ;
#44773 = CARTESIAN_POINT('Ctrl Pts',(-18.4125198148673,-19.1947996538749,
124.09061780245)) ;
#44774 = CARTESIAN_POINT('Ctrl Pts',(-18.163325670764,-19.014810573512,124.260307326459)) ;
#44775 = CARTESIAN_POINT('Ctrl Pts',(-18.5453641416013,-19.204792744173,124.253347261805)) ;
#44776 = CARTESIAN_POINT('Ctrl Pts',(-18.3293793931802,-19.0248036638101,
124.463720725707)) ;
#44777 = CARTESIAN_POINT('Ctrl Pts',(-18.70386501416,-19.2147449142333,124.389942305651)) ;
#44778 = CARTESIAN_POINT('Ctrl Pts',(-18.5275042406602,-19.0347558338704,
124.634466519872)) ;
#44779 = CARTESIAN_POINT('Ctrl Pts',(-18.8832573055452,-19.2246833341478,
124.497026002691)) ;
#44780 = CARTESIAN_POINT('Ctrl Pts',(-18.7517438317463,-19.0446942537849,
124.768323296831)) ;
#44781 = CARTESIAN_POINT('Ctrl Pts',(-19.0793846745513,-19.2346684642334,
124.571917646202)) ;
#44782 = CARTESIAN_POINT('Ctrl Pts',(-18.9969024435329,-19.0546793838705,
124.861939962815)) ;
#44783 = CARTESIAN_POINT('Ctrl Pts',(-19.2866263766652,-19.2447051536475,
124.611508315712)) ;
#44784 = CARTESIAN_POINT('Ctrl Pts',(-19.2559540582378,-19.0647160732846,
124.91143051181)) ;
#44785 = CARTESIAN_POINT('Ctrl Pts',(-19.4937950988768,-19.25455983764,124.614789826941)) ;
#44786 = CARTESIAN_POINT('Ctrl Pts',(-19.5149158429124,-19.0745707572771,
124.915534595951)) ;
#44787 = CARTESIAN_POINT('Ctrl Pts',(-19.7013848668796,-19.2645593216878,
124.581864338488)) ;
#44788 = CARTESIAN_POINT('Ctrl Pts',(-19.774403515448,-19.0845702413249,124.874379795706)) ;
#44789 = CARTESIAN_POINT('Ctrl Pts',(-19.8981684622734,-19.2744544104647,
124.514296465217)) ;
#44790 = CARTESIAN_POINT('Ctrl Pts',(-20.0203843648563,-19.0944653301018,
124.789921645643)) ;
#44791 = CARTESIAN_POINT('Ctrl Pts',(-20.0832105036019,-19.2845149651109,
124.411914232186)) ;
#44792 = CARTESIAN_POINT('Ctrl Pts',(-20.2516876994953,-19.104525884748,124.66194576436)) ;
#44793 = CARTESIAN_POINT('Ctrl Pts',(-20.2443173608154,-19.2943642294838,
124.281814272574)) ;
#44794 = CARTESIAN_POINT('Ctrl Pts',(-20.4530733453116,-19.1143751491209,
124.499321729623)) ;
#44795 = CARTESIAN_POINT('Ctrl Pts',(-20.383234603429,-19.3043914819316,124.123263298254)) ;
#44796 = CARTESIAN_POINT('Ctrl Pts',(-20.6267212720183,-19.1244024015687,
124.301134264892)) ;
#44797 = CARTESIAN_POINT('Ctrl Pts',(-20.4920569293237,-19.3144197795018,
123.942681895053)) ;
#44798 = CARTESIAN_POINT('Ctrl Pts',(-20.7627508777503,-19.1344306991389,
124.075408616383)) ;
#44799 = CARTESIAN_POINT('Ctrl Pts',(-20.5668588209695,-19.3242659085078,
123.749683017547)) ;
#44800 = CARTESIAN_POINT('Ctrl Pts',(-20.8562554221649,-19.1442768281449,
123.834159661665)) ;
#44801 = CARTESIAN_POINT('Ctrl Pts',(-20.608133965986,-19.3342598138698,123.543674588756)) ;
#44802 = CARTESIAN_POINT('Ctrl Pts',(-20.9078510940648,-19.154270733507,123.576649296537)) ;
#44803 = CARTESIAN_POINT('Ctrl Pts',(-20.6126495317417,-19.3442839115529,
123.332979210101)) ;
#44804 = CARTESIAN_POINT('Ctrl Pts',(-20.9134974107354,-19.16429483119,123.313280162661)) ;
#44805 = CARTESIAN_POINT('Ctrl Pts',(-20.5812020044249,-19.3541737394069,
123.127452597675)) ;
#44806 = CARTESIAN_POINT('Ctrl Pts',(-20.8741896282484,-19.174184659044,123.056370784505)) ;
#44807 = CARTESIAN_POINT('Ctrl Pts',(-20.5141513741435,-19.3641657208373,
122.928386984327)) ;
#44808 = CARTESIAN_POINT('Ctrl Pts',(-20.7903778747057,-19.1841766404745,
122.807538053505)) ;
#44809 = CARTESIAN_POINT('Ctrl Pts',(-20.4139600151984,-19.3741127256032,
122.744833669231)) ;
#44810 = CARTESIAN_POINT('Ctrl Pts',(-20.665139925686,-19.1941236452403,122.578095153288)) ;
#44811 = CARTESIAN_POINT('Ctrl Pts',(-20.2836802509689,-19.384062376993,122.581175213375)) ;
#44812 = CARTESIAN_POINT('Ctrl Pts',(-20.5022911487532,-19.2040732966301,
122.373520731289)) ;
#44813 = CARTESIAN_POINT('Ctrl Pts',(-20.1254838491908,-19.3940993799704,
122.441545872889)) ;
#44814 = CARTESIAN_POINT('Ctrl Pts',(-20.3045468222314,-19.2141102996075,
122.198982921485)) ;
#44815 = CARTESIAN_POINT('Ctrl Pts',(-19.9481679622584,-19.4039882884054,
122.332997305238)) ;
#44816 = CARTESIAN_POINT('Ctrl Pts',(-20.0829020053588,-19.2239992080425,
122.063295386373)) ;
#44817 = CARTESIAN_POINT('Ctrl Pts',(-19.7528840797197,-19.4139776208829,
122.255763547514)) ;
#44818 = CARTESIAN_POINT('Ctrl Pts',(-19.8387974857453,-19.23398854052,121.96675176185)) ;
#44819 = CARTESIAN_POINT('Ctrl Pts',(-19.5477596783419,-19.42393617632,122.213894358969)) ;
#44820 = CARTESIAN_POINT('Ctrl Pts',(-19.5823918613755,-19.2439470959571,
121.91441371455)) ;
#44821 = CARTESIAN_POINT('Ctrl Pts',(-19.339716261487,-19.4338357475205,122.20779695739)) ;
#44822 = CARTESIAN_POINT('Ctrl Pts',(-19.3223367513905,-19.2538466671576,
121.906790613366)) ;
#44823 = CARTESIAN_POINT('Ctrl Pts',(-19.1307330189891,-19.4438836727725,
122.238435863334)) ;
#44824 = CARTESIAN_POINT('Ctrl Pts',(-19.0611077173987,-19.2638945924096,
121.945087876798)) ;
#44825 = CARTESIAN_POINT('Ctrl Pts',(-18.9331863686477,-19.4537789722985,
122.303747134582)) ;
#44826 = CARTESIAN_POINT('Ctrl Pts',(-18.814173133126,-19.2737898919356,122.026726025059)) ;
#44827 = CARTESIAN_POINT('Ctrl Pts',(-18.7469349813943,-19.4638408287464,
122.403975883156)) ;
#44828 = CARTESIAN_POINT('Ctrl Pts',(-18.5813585770366,-19.2838517483836,
122.152010675439)) ;
#44829 = CARTESIAN_POINT('Ctrl Pts',(-18.5844603918164,-19.4736846751631,
122.532169779838)) ;
#44830 = CARTESIAN_POINT('Ctrl Pts',(-18.3782635159342,-19.2936955948002,
122.312252866463)) ;
#44831 = CARTESIAN_POINT('Ctrl Pts',(-18.444520656928,-19.4836476242911,122.687999610544)) ;
#44832 = CARTESIAN_POINT('Ctrl Pts',(-18.203337799749,-19.3036585439283,122.507039819624)) ;
#44833 = CARTESIAN_POINT('Ctrl Pts',(-18.3332595420171,-19.4936816607191,
122.867226494345)) ;
#44834 = CARTESIAN_POINT('Ctrl Pts',(-18.0642605165968,-19.3136925803563,
122.731072713085)) ;
#44835 = CARTESIAN_POINT('Ctrl Pts',(-18.2557552508508,-19.5035690876772,
123.060098414967)) ;
#44836 = CARTESIAN_POINT('Ctrl Pts',(-17.9673787966871,-19.3235800073143,
122.972163161456)) ;
#44837 = CARTESIAN_POINT('Ctrl Pts',(-18.2119716822401,-19.5135835220135,
123.266045020976)) ;
#44838 = CARTESIAN_POINT('Ctrl Pts',(-17.9126484521056,-19.3335944416507,
123.229596243496)) ;
#44839 = CARTESIAN_POINT('Ctrl Pts',(-18.2051271781336,-19.5236184666485,
123.476886047581)) ;
#44840 = CARTESIAN_POINT('Ctrl Pts',(-17.9040917216401,-19.3436293862856,
123.493147352358)) ;
#44841 = CARTESIAN_POINT('Ctrl Pts',(-18.2338373099495,-19.5334508166795,
123.681614438135)) ;
#44842 = CARTESIAN_POINT('Ctrl Pts',(-17.9399787131204,-19.3534617363166,
123.749059430674)) ;
#44843 = CARTESIAN_POINT('Ctrl Pts',(-18.2991584830252,-19.5435262557967,
123.883066110455)) ;
#44844 = CARTESIAN_POINT('Ctrl Pts',(-18.0216292180747,-19.3635371754338,
124.000873856143)) ;
#44845 = CARTESIAN_POINT('Ctrl Pts',(-18.3962015107462,-19.5533787210313,
124.066105872207)) ;
#44846 = CARTESIAN_POINT('Ctrl Pts',(-18.1429328956799,-19.3733896406684,
124.229675102606)) ;
#44847 = CARTESIAN_POINT('Ctrl Pts',(-18.5262180602235,-19.5634515986082,
124.233211940351)) ;
#44848 = CARTESIAN_POINT('Ctrl Pts',(-18.3054527184388,-19.3834625182453,
124.438557806816)) ;
#44849 = CARTESIAN_POINT('Ctrl Pts',(-18.6797419077355,-19.5732941948007,
124.371972025685)) ;
#44850 = CARTESIAN_POINT('Ctrl Pts',(-18.497358063962,-19.3933051144378,124.61200943149)) ;
#44851 = CARTESIAN_POINT('Ctrl Pts',(-18.8570829768545,-19.583274578916,124.484089894838)) ;
#44852 = CARTESIAN_POINT('Ctrl Pts',(-18.7190343990807,-19.4032854985531,
124.75215735034)) ;
#44853 = CARTESIAN_POINT('Ctrl Pts',(-19.0520979345884,-19.5932930595648,
124.563638386236)) ;
#44854 = CARTESIAN_POINT('Ctrl Pts',(-18.9628028394866,-19.4133039792019,
124.851593565958)) ;
#44855 = CARTESIAN_POINT('Ctrl Pts',(-19.2551201360957,-19.6031763745651,
124.60795747562)) ;
#44856 = CARTESIAN_POINT('Ctrl Pts',(-19.2165815610938,-19.4231872942023,
124.906993128951)) ;
#44857 = CARTESIAN_POINT('Ctrl Pts',(-19.4665835366487,-19.6132446716556,
124.616412950505)) ;
#44858 = CARTESIAN_POINT('Ctrl Pts',(-19.48091038097,-19.4332555912927,124.917562972667)) ;
#44859 = CARTESIAN_POINT('Ctrl Pts',(-19.6714432989599,-19.6230747400279,
124.588929074882)) ;
#44860 = CARTESIAN_POINT('Ctrl Pts',(-19.7369866664886,-19.443085659665,124.883208337292)) ;
#44861 = CARTESIAN_POINT('Ctrl Pts',(-19.8731711829206,-19.6331415324963,
124.525058281319)) ;
#44862 = CARTESIAN_POINT('Ctrl Pts',(-19.9891462344239,-19.4531524521334,
124.803370268973)) ;
#44863 = CARTESIAN_POINT('Ctrl Pts',(-20.0574611220455,-19.6430308659848,
124.428741148867)) ;
#44864 = CARTESIAN_POINT('Ctrl Pts',(-20.2195097660386,-19.4630417856219,
124.682973671205)) ;
#44865 = CARTESIAN_POINT('Ctrl Pts',(-20.2242497094466,-19.6530329974009,
124.300749095355)) ;
#44866 = CARTESIAN_POINT('Ctrl Pts',(-20.4279957455821,-19.473043917038,124.522983695097)) ;
#44867 = CARTESIAN_POINT('Ctrl Pts',(-20.3653190292274,-19.6629568670219,
124.146990412121)) ;
#44868 = CARTESIAN_POINT('Ctrl Pts',(-20.6043330327823,-19.482967786659,124.330784900546)) ;
#44869 = CARTESIAN_POINT('Ctrl Pts',(-20.4788115638029,-19.6730003825391,
123.968976465865)) ;
#44870 = CARTESIAN_POINT('Ctrl Pts',(-20.7461987470963,-19.4930113021762,
124.108267757242)) ;
#44871 = CARTESIAN_POINT('Ctrl Pts',(-20.5586220167799,-19.6828825954274,
123.777121275203)) ;
#44872 = CARTESIAN_POINT('Ctrl Pts',(-20.8459623353145,-19.5028935150645,
123.868447779189)) ;
#44873 = CARTESIAN_POINT('Ctrl Pts',(-20.6047386809469,-19.6929506726468,
123.570583320886)) ;
#44874 = CARTESIAN_POINT('Ctrl Pts',(-20.9036081809755,-19.5129615922839,
123.610275746684)) ;
#44875 = CARTESIAN_POINT('Ctrl Pts',(-20.6142646304395,-19.702789177381,123.36393271165)) ;
#44876 = CARTESIAN_POINT('Ctrl Pts',(-20.9155157124554,-19.5228000970181,
123.351961006778)) ;
#44877 = CARTESIAN_POINT('Ctrl Pts',(-20.5874658464836,-19.7128519458104,
123.154111705371)) ;
#44878 = CARTESIAN_POINT('Ctrl Pts',(-20.8820171905211,-19.5328628654475,
123.089685129375)) ;
#44879 = CARTESIAN_POINT('Ctrl Pts',(-20.5254497535726,-19.7227489390931,
122.955490377615)) ;
#44880 = CARTESIAN_POINT('Ctrl Pts',(-20.8044967773862,-19.5427598587302,
122.841407511896)) ;
#44881 = CARTESIAN_POINT('Ctrl Pts',(-20.4301860161421,-19.7326801667279,
122.769710863237)) ;
#44882 = CARTESIAN_POINT('Ctrl Pts',(-20.6854165300552,-19.552691086365,122.609182603989)) ;
#44883 = CARTESIAN_POINT('Ctrl Pts',(-20.3025172159415,-19.74272232537,122.601572700884)) ;
#44884 = CARTESIAN_POINT('Ctrl Pts',(-20.5258305091892,-19.5627332450072,
122.399010178353)) ;
#44885 = CARTESIAN_POINT('Ctrl Pts',(-20.1500853642892,-19.7526090349011,
122.460258580595)) ;
#44886 = CARTESIAN_POINT('Ctrl Pts',(-20.3352897321001,-19.5726199545382,
122.222366967696)) ;
#44887 = CARTESIAN_POINT('Ctrl Pts',(-19.973762981087,-19.7626020073297,122.346058634074)) ;
#44888 = CARTESIAN_POINT('Ctrl Pts',(-20.1148863727174,-19.5826129269668,
122.079617245507)) ;
#44889 = CARTESIAN_POINT('Ctrl Pts',(-19.7811555655468,-19.7725482018663,
122.26467134964)) ;
#44890 = CARTESIAN_POINT('Ctrl Pts',(-19.8741264226561,-19.5925591215034,
121.977883229186)) ;
#44891 = CARTESIAN_POINT('Ctrl Pts',(-19.577440733495,-19.7824935767178,122.217515204757)) ;
#44892 = CARTESIAN_POINT('Ctrl Pts',(-19.6194821905471,-19.6025044963549,
121.918938430882)) ;
#44893 = CARTESIAN_POINT('Ctrl Pts',(-19.3663571883107,-19.7925484960777,
122.206654014904)) ;
#44894 = CARTESIAN_POINT('Ctrl Pts',(-19.3556280435181,-19.6125594157148,
121.905362356848)) ;
#44895 = CARTESIAN_POINT('Ctrl Pts',(-19.1613655130489,-19.8023700155212,
122.231619206292)) ;
#44896 = CARTESIAN_POINT('Ctrl Pts',(-19.0993869105069,-19.6223809351583,
121.936569596424)) ;
#44897 = CARTESIAN_POINT('Ctrl Pts',(-18.9588961884829,-19.8124357842881,
122.293030078192)) ;
#44898 = CARTESIAN_POINT('Ctrl Pts',(-18.8463008166757,-19.6324467039252,
122.013333704317)) ;
#44899 = CARTESIAN_POINT('Ctrl Pts',(-18.7732037589491,-19.8223377059431,
122.387203432726)) ;
#44900 = CARTESIAN_POINT('Ctrl Pts',(-18.6141847413824,-19.6423486255803,
122.131051371132)) ;
#44901 = CARTESIAN_POINT('Ctrl Pts',(-18.6042436666865,-19.8323807647642,
122.513786536381)) ;
#44902 = CARTESIAN_POINT('Ctrl Pts',(-18.4029852173609,-19.6523916844013,
122.289280682628)) ;
#44903 = CARTESIAN_POINT('Ctrl Pts',(-18.4618641617122,-19.8422867588069,
122.665775366195)) ;
#44904 = CARTESIAN_POINT('Ctrl Pts',(-18.2250106932067,-19.662297678444,122.479267826305)) ;
#44905 = CARTESIAN_POINT('Ctrl Pts',(-18.347162029579,-19.8522245318887,122.840394738477)) ;
#44906 = CARTESIAN_POINT('Ctrl Pts',(-18.0816334128682,-19.6722354515258,
122.697543077663)) ;
#44907 = CARTESIAN_POINT('Ctrl Pts',(-18.2638779267283,-19.862264895621,123.034345828099)) ;
#44908 = CARTESIAN_POINT('Ctrl Pts',(-17.9775290976188,-19.6822758152581,
122.939982086318)) ;
#44909 = CARTESIAN_POINT('Ctrl Pts',(-18.2161158206728,-19.8721522393445,
123.236657619917)) ;
#44910 = CARTESIAN_POINT('Ctrl Pts',(-17.9178270664722,-19.6921631589816,
123.192873036797)) ;
#44911 = CARTESIAN_POINT('Ctrl Pts',(-18.2037362405876,-19.8821444699132,
123.446346397897)) ;
#44912 = CARTESIAN_POINT('Ctrl Pts',(-17.9023535730957,-19.7021553895503,
123.454984271159)) ;
#44913 = CARTESIAN_POINT('Ctrl Pts',(-18.2279073020014,-19.8920929976968,
123.65410610834)) ;
#44914 = CARTESIAN_POINT('Ctrl Pts',(-17.9325684280021,-19.7121039173339,
123.714684335697)) ;
#44915 = CARTESIAN_POINT('Ctrl Pts',(-18.2874238407614,-19.9020297814201,
123.854332451644)) ;
#44916 = CARTESIAN_POINT('Ctrl Pts',(-18.0069653213655,-19.7220407010572,
123.964967568088)) ;
#44917 = CARTESIAN_POINT('Ctrl Pts',(-18.3810183276697,-19.912012782217,124.042211329903)) ;
#44918 = CARTESIAN_POINT('Ctrl Pts',(-18.1239596004005,-19.7320237018542,
124.199815869688)) ;
#44919 = CARTESIAN_POINT('Ctrl Pts',(-18.5068566623067,-19.9220566690578,
124.211741307508)) ;
#44920 = CARTESIAN_POINT('Ctrl Pts',(-18.2812582377019,-19.7420675886949,
124.411727571249)) ;
#44921 = CARTESIAN_POINT('Ctrl Pts',(-18.656625770795,-19.9318846926323,124.354124004755)) ;
#44922 = CARTESIAN_POINT('Ctrl Pts',(-18.4684715103472,-19.7518956122695,
124.589706055916)) ;
#44923 = CARTESIAN_POINT('Ctrl Pts',(-18.8330935902759,-19.941961940846,124.47126421145)) ;
#44924 = CARTESIAN_POINT('Ctrl Pts',(-18.6890566141087,-19.7619728604831,
124.736130030075)) ;
#44925 = CARTESIAN_POINT('Ctrl Pts',(-19.0228690100662,-19.9518114961513,
124.55424093318)) ;
#44926 = CARTESIAN_POINT('Ctrl Pts',(-18.9262775519246,-19.7718224157884,
124.839850242289)) ;
#44927 = CARTESIAN_POINT('Ctrl Pts',(-19.2288113073246,-19.961894204349,124.604205688793)) ;
#44928 = CARTESIAN_POINT('Ctrl Pts',(-19.1837052991682,-19.7819051239861,
124.902304787671)) ;
#44929 = CARTESIAN_POINT('Ctrl Pts',(-19.434720498365,-19.9717067972754,124.617486778315)) ;
#44930 = CARTESIAN_POINT('Ctrl Pts',(-19.4410933758794,-19.7917177169126,
124.918904855256)) ;
#44931 = CARTESIAN_POINT('Ctrl Pts',(-19.645072882955,-19.9817739895334,124.594577329218)) ;
#44932 = CARTESIAN_POINT('Ctrl Pts',(-19.7040333399795,-19.8017849091705,
124.890266579354)) ;
#44933 = CARTESIAN_POINT('Ctrl Pts',(-19.8449282407417,-19.991672818996,124.536378177571)) ;
#44934 = CARTESIAN_POINT('Ctrl Pts',(-19.9538529269052,-19.8116837386331,
124.817515981026)) ;
#44935 = CARTESIAN_POINT('Ctrl Pts',(-20.0345223013733,-20.0017268101862,
124.443044256288)) ;
#44936 = CARTESIAN_POINT('Ctrl Pts',(-20.1908446168851,-19.8217377298233,
124.700847328328)) ;
#44937 = CARTESIAN_POINT('Ctrl Pts',(-20.2021184222333,-20.0115985349694,
124.320569621367)) ;
#44938 = CARTESIAN_POINT('Ctrl Pts',(-20.4003396792968,-19.8316094546065,
124.547752149574)) ;
#44939 = CARTESIAN_POINT('Ctrl Pts',(-20.3487795362929,-20.0216689770996,
124.167933913824)) ;
#44940 = CARTESIAN_POINT('Ctrl Pts',(-20.5836646742585,-19.8416798967367,
124.356956666456)) ;
#44941 = CARTESIAN_POINT('Ctrl Pts',(-20.4640387398854,-20.0315020555299,
123.996302242053)) ;
#44942 = CARTESIAN_POINT('Ctrl Pts',(-20.7277380468266,-19.851512975167,124.142415105616)) ;
#44943 = CARTESIAN_POINT('Ctrl Pts',(-20.5499655152487,-20.0415325290313,
123.803739463889)) ;
#44944 = CARTESIAN_POINT('Ctrl Pts',(-20.8351448171807,-19.8615434486684,
123.901710971158)) ;
#44945 = CARTESIAN_POINT('Ctrl Pts',(-20.6005657766499,-20.0515641283299,
123.59899153)) ;
#44946 = CARTESIAN_POINT('Ctrl Pts',(-20.8983935514118,-19.8715750479671,
123.645775745948)) ;
#44947 = CARTESIAN_POINT('Ctrl Pts',(-20.6149874000634,-20.0613938293681,
123.392858537114)) ;
#44948 = CARTESIAN_POINT('Ctrl Pts',(-20.9164189115037,-19.8814047490052,
123.388108112838)) ;
#44949 = CARTESIAN_POINT('Ctrl Pts',(-20.593669608918,-20.0713832674246,123.183927476953)) ;
#44950 = CARTESIAN_POINT('Ctrl Pts',(-20.889769707107,-19.8913941870617,123.126944309975)) ;
#44951 = CARTESIAN_POINT('Ctrl Pts',(-20.5355721040913,-20.0814271706407,
122.980925519128)) ;
#44952 = CARTESIAN_POINT('Ctrl Pts',(-20.817146145048,-19.9014380902778,122.873192498264)) ;
#44953 = CARTESIAN_POINT('Ctrl Pts',(-20.445542899385,-20.0912486914542,122.795106271871)) ;
#44954 = CARTESIAN_POINT('Ctrl Pts',(-20.7046073617645,-19.9112596110913,
122.640918152662)) ;
#44955 = CARTESIAN_POINT('Ctrl Pts',(-20.3223921732371,-20.1012844157013,
122.623800659788)) ;
#44956 = CARTESIAN_POINT('Ctrl Pts',(-20.5506673334166,-19.9212953353384,
122.426787436432)) ;
#44957 = CARTESIAN_POINT('Ctrl Pts',(-20.1711768869751,-20.1113065696338,
122.477056253106)) ;
#44958 = CARTESIAN_POINT('Ctrl Pts',(-20.3616469061169,-19.9313174892709,
122.243358309574)) ;
#44959 = CARTESIAN_POINT('Ctrl Pts',(-19.9997783644996,-20.1211688013911,
122.360421499363)) ;
#44960 = CARTESIAN_POINT('Ctrl Pts',(-20.1473968172802,-19.9411797210282,
122.097565987472)) ;
#44961 = CARTESIAN_POINT('Ctrl Pts',(-19.8090973942944,-20.131127871849,122.273937081549)) ;
#44962 = CARTESIAN_POINT('Ctrl Pts',(-19.9090443945828,-19.9511387914861,
121.989462309799)) ;
#44963 = CARTESIAN_POINT('Ctrl Pts',(-19.6046796800119,-20.1411630442251,
122.221797594559)) ;
#44964 = CARTESIAN_POINT('Ctrl Pts',(-19.653521817539,-19.9611739638623,121.924289992094)) ;
#44965 = CARTESIAN_POINT('Ctrl Pts',(-19.3975520285983,-20.1510434293834,
122.205875090006)) ;
#44966 = CARTESIAN_POINT('Ctrl Pts',(-19.3946113132475,-19.9710543490205,
121.904388967509)) ;
#44967 = CARTESIAN_POINT('Ctrl Pts',(-19.1871508596279,-20.1611001439773,
122.226434671735)) ;
#44968 = CARTESIAN_POINT('Ctrl Pts',(-19.1316102592397,-19.9811110636145,
121.930090607281)) ;
#44969 = CARTESIAN_POINT('Ctrl Pts',(-18.9870826370418,-20.1709794125494,
122.28223552978)) ;
#44970 = CARTESIAN_POINT('Ctrl Pts',(-18.8815248170591,-19.9909903321865,
121.999843996043)) ;
#44971 = CARTESIAN_POINT('Ctrl Pts',(-18.7973905879869,-20.1809703700351,
122.372426720586)) ;
#44972 = CARTESIAN_POINT('Ctrl Pts',(-18.6444106249268,-20.0009812896722,
122.112585153845)) ;
#44973 = CARTESIAN_POINT('Ctrl Pts',(-18.6256580137942,-20.1910110286703,
122.495170942343)) ;
#44974 = CARTESIAN_POINT('Ctrl Pts',(-18.4297462676032,-20.0110219483074,
122.266017180346)) ;
#44975 = CARTESIAN_POINT('Ctrl Pts',(-18.4806610276397,-20.2008440083783,
122.642504839744)) ;
#44976 = CARTESIAN_POINT('Ctrl Pts',(-18.2485010034738,-20.0208549280154,
122.450186849546)) ;
#44977 = CARTESIAN_POINT('Ctrl Pts',(-18.3610435893545,-20.210837141628,122.81520973265)) ;
#44978 = CARTESIAN_POINT('Ctrl Pts',(-18.0989811418267,-20.0308480612651,
122.666069459646)) ;
#44979 = CARTESIAN_POINT('Ctrl Pts',(-18.2732819316886,-20.2208691940113,
123.00699894088)) ;
#44980 = CARTESIAN_POINT('Ctrl Pts',(-17.9892812124725,-20.0408801136485,
122.905806909259)) ;
#44981 = CARTESIAN_POINT('Ctrl Pts',(-18.2207950634058,-20.2307344229627,
123.207634736704)) ;
#44982 = CARTESIAN_POINT('Ctrl Pts',(-17.9236747635864,-20.0507453425998,
123.15660297018)) ;
#44983 = CARTESIAN_POINT('Ctrl Pts',(-18.2031854904533,-20.2406963642059,
123.416330007382)) ;
#44984 = CARTESIAN_POINT('Ctrl Pts',(-17.9016652917606,-20.060707283843,123.417472522822)) ;
#44985 = CARTESIAN_POINT('Ctrl Pts',(-18.2225552242185,-20.2507310792426,
123.626390528993)) ;
#44986 = CARTESIAN_POINT('Ctrl Pts',(-17.9258798988399,-20.0707419988798,
123.680047914976)) ;
#44987 = CARTESIAN_POINT('Ctrl Pts',(-18.2769648586683,-20.2606168495867,
123.826997944236)) ;
#44988 = CARTESIAN_POINT('Ctrl Pts',(-17.9938945221677,-20.0806277692238,
123.930807070481)) ;
#44989 = CARTESIAN_POINT('Ctrl Pts',(-18.3669425663381,-20.2706794469754,
124.018428595502)) ;
#44990 = CARTESIAN_POINT('Ctrl Pts',(-18.1063688771636,-20.0906903666126,
124.17009418255)) ;
#44991 = CARTESIAN_POINT('Ctrl Pts',(-18.4861705032572,-20.2805298588107,
124.187769337836)) ;
#44992 = CARTESIAN_POINT('Ctrl Pts',(-18.2554062654784,-20.1005407784478,
124.381769206372)) ;
#44993 = CARTESIAN_POINT('Ctrl Pts',(-18.6352264586599,-20.2905570280966,
124.336825287887)) ;
#44994 = CARTESIAN_POINT('Ctrl Pts',(-18.4417280629167,-20.1105679477337,
124.568087270912)) ;
#44995 = CARTESIAN_POINT('Ctrl Pts',(-18.8082335054071,-20.3005845088108,
124.457297088272)) ;
#44996 = CARTESIAN_POINT('Ctrl Pts',(-18.6579883240975,-20.1205954284479,
124.71867494309)) ;
#44997 = CARTESIAN_POINT('Ctrl Pts',(-18.9958279314293,-20.3104275613901,
124.544623627874)) ;
#44998 = CARTESIAN_POINT('Ctrl Pts',(-18.8924830333248,-20.1304384810272,
124.827831022184)) ;
#44999 = CARTESIAN_POINT('Ctrl Pts',(-19.19866746115,-20.3204214648287,124.599389527813)) ;
#45000 = CARTESIAN_POINT('Ctrl Pts',(-19.1460332396166,-20.1404323844658,
124.896285825858)) ;
#45001 = CARTESIAN_POINT('Ctrl Pts',(-19.4086704937467,-20.3304485876051,
124.617780480722)) ;
#45002 = CARTESIAN_POINT('Ctrl Pts',(-19.408537282864,-20.1504595072422,124.919271899717)) ;
#45003 = CARTESIAN_POINT('Ctrl Pts',(-19.6158404873169,-20.3403392924971,
124.599938377875)) ;
#45004 = CARTESIAN_POINT('Ctrl Pts',(-19.6674999586504,-20.1603502121343,
124.896966576094)) ;
#45005 = CARTESIAN_POINT('Ctrl Pts',(-19.8188925643533,-20.3503313193475,
124.546143797245)) ;
#45006 = CARTESIAN_POINT('Ctrl Pts',(-19.9213144643627,-20.1703422389846,
124.829720703187)) ;
#45007 = CARTESIAN_POINT('Ctrl Pts',(-20.0086203150577,-20.360277300836,124.458257930678)) ;
#45008 = CARTESIAN_POINT('Ctrl Pts',(-20.158473228304,-20.1802882204731,124.719860821045)) ;
#45009 = CARTESIAN_POINT('Ctrl Pts',(-20.1804782509526,-20.3702244734579,
124.339088999519)) ;
#45010 = CARTESIAN_POINT('Ctrl Pts',(-20.3732942470927,-20.190235393095,124.570897282398)) ;
#45011 = CARTESIAN_POINT('Ctrl Pts',(-20.3303594599015,-20.3802724147841,
124.190244480905)) ;
#45012 = CARTESIAN_POINT('Ctrl Pts',(-20.5606438303885,-20.2002833344212,
124.384839709342)) ;
#45013 = CARTESIAN_POINT('Ctrl Pts',(-20.4498405364493,-20.3901200485918,
124.021171300404)) ;
#45014 = CARTESIAN_POINT('Ctrl Pts',(-20.7099931677264,-20.210130968229,124.17349632098)) ;
#45015 = CARTESIAN_POINT('Ctrl Pts',(-20.5397614536319,-20.4000817632769,
123.832042454196)) ;
#45016 = CARTESIAN_POINT('Ctrl Pts',(-20.8223918370586,-20.220092682914,123.937083946774)) ;
#45017 = CARTESIAN_POINT('Ctrl Pts',(-20.5955998308358,-20.4101103961554,
123.628724338267)) ;
#45018 = CARTESIAN_POINT('Ctrl Pts',(-20.8921871412405,-20.2301213157925,
123.682935524378)) ;
#45019 = CARTESIAN_POINT('Ctrl Pts',(-20.6151216491279,-20.4200207216905,
123.421303306592)) ;
#45020 = CARTESIAN_POINT('Ctrl Pts',(-20.9165866653184,-20.2400316413277,
123.423658765384)) ;
#45021 = CARTESIAN_POINT('Ctrl Pts',(-20.5988309906371,-20.4299555521623,
123.213073747542)) ;
#45022 = CARTESIAN_POINT('Ctrl Pts',(-20.8962205046669,-20.2499664717994,
123.163371888268)) ;
#45023 = CARTESIAN_POINT('Ctrl Pts',(-20.5458999153234,-20.4399968845442,
123.008717300108)) ;
#45024 = CARTESIAN_POINT('Ctrl Pts',(-20.8300540056933,-20.2600078041814,
122.907927043714)) ;
#45025 = CARTESIAN_POINT('Ctrl Pts',(-20.4596544020495,-20.4498897579831,
122.819465298956)) ;
#45026 = CARTESIAN_POINT('Ctrl Pts',(-20.7222442141385,-20.2699006776202,
122.671362855132)) ;
#45027 = CARTESIAN_POINT('Ctrl Pts',(-20.3413828244053,-20.459858923801,122.646430648159)) ;
#45028 = CARTESIAN_POINT('Ctrl Pts',(-20.574403392537,-20.2798698434381,122.45507183945)) ;
#45029 = CARTESIAN_POINT('Ctrl Pts',(-20.1937587502541,-20.4698876575175,
122.49593053107)) ;
#45030 = CARTESIAN_POINT('Ctrl Pts',(-20.389867415721,-20.2898985771546,122.266945763663)) ;
#45031 = CARTESIAN_POINT('Ctrl Pts',(-19.9684033928012,-20.4830801762886,
122.334134273859)) ;
#45032 = CARTESIAN_POINT('Ctrl Pts',(-20.108189935514,-20.3030910959258,122.064717611353)) ;
#45033 = CARTESIAN_POINT('Ctrl Pts',(-19.7027899632007,-20.4964400443313,
122.233638145416)) ;
#45034 = CARTESIAN_POINT('Ctrl Pts',(-19.776200429425,-20.3164509639684,121.939098030054)) ;
#45035 = CARTESIAN_POINT('Ctrl Pts',(-19.4261080021341,-20.5096653814802,
122.206033322011)) ;
#45036 = CARTESIAN_POINT('Ctrl Pts',(-19.4302944299176,-20.3296763011173,
121.904585070859)) ;
#45037 = CARTESIAN_POINT('Ctrl Pts',(-19.2168158322053,-20.5196466073208,
122.221163224534)) ;
#45038 = CARTESIAN_POINT('Ctrl Pts',(-19.1686900557449,-20.3396575269579,
121.923502397448)) ;
#45039 = CARTESIAN_POINT('Ctrl Pts',(-19.0123335437991,-20.5296821743037,
122.273082359298)) ;
#45040 = CARTESIAN_POINT('Ctrl Pts',(-18.9130849261984,-20.3496930939408,
121.988403504327)) ;
#45041 = CARTESIAN_POINT('Ctrl Pts',(-18.8230767712462,-20.5395452522658,
122.357856292057)) ;
#45042 = CARTESIAN_POINT('Ctrl Pts',(-18.6765159440695,-20.3595561719029,
122.094373600289)) ;
#45043 = CARTESIAN_POINT('Ctrl Pts',(-18.6478204664462,-20.5496155510669,
122.476584772983)) ;
#45044 = CARTESIAN_POINT('Ctrl Pts',(-18.4574468061617,-20.369626470704,122.2427865665)) ;
#45045 = CARTESIAN_POINT('Ctrl Pts',(-18.4992676427898,-20.5594578496347,
122.620634851231)) ;
#45046 = CARTESIAN_POINT('Ctrl Pts',(-18.2717579005638,-20.3794687692718,
122.422851075719)) ;
#45047 = CARTESIAN_POINT('Ctrl Pts',(-18.3759064700005,-20.5694185478045,
122.789841274378)) ;
#45048 = CARTESIAN_POINT('Ctrl Pts',(-18.1175586647282,-20.3894294674416,
122.634360678073)) ;
#45049 = CARTESIAN_POINT('Ctrl Pts',(-18.283462315847,-20.579456581984,122.979538516165)) ;
#45050 = CARTESIAN_POINT('Ctrl Pts',(-18.0020059072157,-20.3994675016211,
122.871483585782)) ;
#45051 = CARTESIAN_POINT('Ctrl Pts',(-18.2259264092377,-20.5893303188304,
123.179010973159)) ;
#45052 = CARTESIAN_POINT('Ctrl Pts',(-17.9300887193781,-20.4093412384676,
123.12082468391)) ;
#45053 = CARTESIAN_POINT('Ctrl Pts',(-18.203489149074,-20.5994021027557,123.389529384903)) ;
#45054 = CARTESIAN_POINT('Ctrl Pts',(-17.9020448474058,-20.4194130223928,
123.383973224126)) ;
#45055 = CARTESIAN_POINT('Ctrl Pts',(-18.217479141793,-20.6092342239569,123.595777992507)) ;
#45056 = CARTESIAN_POINT('Ctrl Pts',(-17.9195350319781,-20.429245143594,123.641783391188)) ;
#45057 = CARTESIAN_POINT('Ctrl Pts',(-18.2675235725742,-20.6192672479823,
123.800670607276)) ;
#45058 = CARTESIAN_POINT('Ctrl Pts',(-17.9820931576725,-20.4392781676194,
123.897898640785)) ;
#45059 = CARTESIAN_POINT('Ctrl Pts',(-18.3527418081313,-20.629283128179,123.993235721321)) ;
#45060 = CARTESIAN_POINT('Ctrl Pts',(-18.0886185614509,-20.4492940478161,
124.138604141846)) ;
#45061 = CARTESIAN_POINT('Ctrl Pts',(-18.4682220622006,-20.6391666472732,
124.165972783851)) ;
#45062 = CARTESIAN_POINT('Ctrl Pts',(-18.2329706508674,-20.4591775669103,
124.354523331879)) ;
#45063 = CARTESIAN_POINT('Ctrl Pts',(-18.6132891948029,-20.6491570596368,
124.317833664429)) ;
#45064 = CARTESIAN_POINT('Ctrl Pts',(-18.4143074091382,-20.469167979274,124.54434899152)) ;
#45065 = CARTESIAN_POINT('Ctrl Pts',(-18.8379391592786,-20.6624202228403,
124.483045377824)) ;
#45066 = CARTESIAN_POINT('Ctrl Pts',(-18.6951170310066,-20.4824311424774,
124.750853866765)) ;
#45067 = CARTESIAN_POINT('Ctrl Pts',(-19.1007465541756,-20.6756977930915,
124.586193595685)) ;
#45068 = CARTESIAN_POINT('Ctrl Pts',(-19.0235816254603,-20.4957087127286,
124.879780338446)) ;
#45069 = CARTESIAN_POINT('Ctrl Pts',(-19.3792304841943,-20.6890280955981,
124.617392370144)) ;
#45070 = CARTESIAN_POINT('Ctrl Pts',(-19.3717460245778,-20.5090390152352,
124.918788838269)) ;
#45071 = CARTESIAN_POINT('Ctrl Pts',(-19.5869463660609,-20.6989267774145,
124.604614305006)) ;
#45072 = CARTESIAN_POINT('Ctrl Pts',(-19.631378352144,-20.5189376970516,124.902811153565)) ;
#45073 = CARTESIAN_POINT('Ctrl Pts',(-19.7911870424571,-20.708916292462,124.555761796128)) ;
#45074 = CARTESIAN_POINT('Ctrl Pts',(-19.886681931356,-20.5289272120991,124.841743662503)) ;
#45075 = CARTESIAN_POINT('Ctrl Pts',(-19.9830582667155,-20.718864344237,124.472519591824)) ;
#45076 = CARTESIAN_POINT('Ctrl Pts',(-20.1265183759964,-20.5388752638742,
124.737689396078)) ;
#45077 = CARTESIAN_POINT('Ctrl Pts',(-20.1575675432332,-20.7288057475155,
124.357539674552)) ;
#45078 = CARTESIAN_POINT('Ctrl Pts',(-20.3446556457236,-20.5488166671527,
124.593959705977)) ;
#45079 = CARTESIAN_POINT('Ctrl Pts',(-20.3608485699155,-20.7420924122965,
124.165903707027)) ;
#45080 = CARTESIAN_POINT('Ctrl Pts',(-20.5987445476078,-20.5621033319336,
124.354427857962)) ;
#45081 = CARTESIAN_POINT('Ctrl Pts',(-20.5464483543658,-20.7587028339513,
123.865472903908)) ;
#45082 = CARTESIAN_POINT('Ctrl Pts',(-20.8307521720102,-20.5787137535884,
123.97887050718)) ;
#45083 = CARTESIAN_POINT('Ctrl Pts',(-20.6330141955444,-20.7786140962021,
123.451029395144)) ;
#45084 = CARTESIAN_POINT('Ctrl Pts',(-20.9389514260489,-20.5986250158392,
123.460821316337)) ;
#45085 = CARTESIAN_POINT('Ctrl Pts',(-20.5730157601791,-20.7985582253669,
123.03120703151)) ;
#45086 = CARTESIAN_POINT('Ctrl Pts',(-20.8639502681966,-20.6185691450041,
122.93604284961)) ;
#45087 = CARTESIAN_POINT('Ctrl Pts',(-20.3735473898492,-20.8184813879721,
122.657531564048)) ;
#45088 = CARTESIAN_POINT('Ctrl Pts',(-20.614611211859,-20.6384923076093,122.468951374548)) ;
#45089 = CARTESIAN_POINT('Ctrl Pts',(-20.0594536899428,-20.8383715103787,
122.374229560323)) ;
#45090 = CARTESIAN_POINT('Ctrl Pts',(-20.2219924331107,-20.6583824300158,
122.114827126927)) ;
#45091 = CARTESIAN_POINT('Ctrl Pts',(-19.6652757918242,-20.8583764639788,
122.21454943932)) ;
#45092 = CARTESIAN_POINT('Ctrl Pts',(-19.7292685932625,-20.6783873836159,
121.915230361568)) ;
#45093 = CARTESIAN_POINT('Ctrl Pts',(-19.2436756516205,-20.8782147209944,
122.198755207655)) ;
#45094 = CARTESIAN_POINT('Ctrl Pts',(-19.2022698837694,-20.6982256406315,
121.895490958203)) ;
#45095 = CARTESIAN_POINT('Ctrl Pts',(-18.8388276678669,-20.8982090217809,
122.328339296805)) ;
#45096 = CARTESIAN_POINT('Ctrl Pts',(-18.6962108824023,-20.718219941418,122.057473862947)) ;
#45097 = CARTESIAN_POINT('Ctrl Pts',(-18.5045195812377,-20.9180942638254,
122.587219380678)) ;
#45098 = CARTESIAN_POINT('Ctrl Pts',(-18.2783285952611,-20.7381051834625,
122.381075560874)) ;
#45099 = CARTESIAN_POINT('Ctrl Pts',(-18.2777383338491,-20.9379692103013,
122.943809989293)) ;
#45100 = CARTESIAN_POINT('Ctrl Pts',(-17.994854669319,-20.7579801299384,122.826813664133)) ;
#45101 = CARTESIAN_POINT('Ctrl Pts',(-18.1858465710656,-20.9580022802424,
123.359778806522)) ;
#45102 = CARTESIAN_POINT('Ctrl Pts',(-17.8799919148202,-20.7780131998795,
123.346775629798)) ;
#45103 = CARTESIAN_POINT('Ctrl Pts',(-18.2415322925881,-20.9778907871428,
123.778943620506)) ;
#45104 = CARTESIAN_POINT('Ctrl Pts',(-17.9496011378404,-20.7979017067799,
123.870729922687)) ;
#45105 = CARTESIAN_POINT('Ctrl Pts',(-18.4353283530407,-20.9977456469241,
124.154075261847)) ;
#45106 = CARTESIAN_POINT('Ctrl Pts',(-18.1918462219095,-20.8177565665612,
124.3396421318)) ;
#45107 = CARTESIAN_POINT('Ctrl Pts',(-18.7489158886705,-21.0177964807118,
124.442758777326)) ;
#45108 = CARTESIAN_POINT('Ctrl Pts',(-18.5838321068267,-20.8378074003489,
124.700496054133)) ;
#45109 = CARTESIAN_POINT('Ctrl Pts',(-19.136624015985,-21.037562422601,124.605282240514)) ;
#45110 = CARTESIAN_POINT('Ctrl Pts',(-19.068464276831,-20.8575733422382,124.903648311882)) ;
#45111 = CARTESIAN_POINT('Ctrl Pts',(-19.5614777516072,-21.0575751540604,
124.626836375853)) ;
#45112 = CARTESIAN_POINT('Ctrl Pts',(-19.5995315082648,-20.8775860736975,
124.930591112169)) ;
#45113 = CARTESIAN_POINT('Ctrl Pts',(-19.9658070655714,-21.0774679890039,
124.50224819763)) ;
#45114 = CARTESIAN_POINT('Ctrl Pts',(-20.1049415619315,-20.8974789086411,
124.774856355301)) ;
#45115 = CARTESIAN_POINT('Ctrl Pts',(-20.3038411949213,-21.0973750123435,
124.247672615778)) ;
#45116 = CARTESIAN_POINT('Ctrl Pts',(-20.5274834956155,-20.9173859319806,
124.456638371314)) ;
#45117 = CARTESIAN_POINT('Ctrl Pts',(-20.5353184672274,-21.1172902772442,
123.892968169314)) ;
#45118 = CARTESIAN_POINT('Ctrl Pts',(-20.816830578431,-20.9373011968813,124.013259477076)) ;
#45119 = CARTESIAN_POINT('Ctrl Pts',(-20.6318648780347,-21.1373219694039,
123.478162570319)) ;
#45120 = CARTESIAN_POINT('Ctrl Pts',(-20.9375148304315,-20.957332889041,123.494752291647)) ;
#45121 = CARTESIAN_POINT('Ctrl Pts',(-20.5815599947794,-21.1571650159769,
123.059210144883)) ;
#45122 = CARTESIAN_POINT('Ctrl Pts',(-20.8746353856575,-20.977175935614,122.971063764451)) ;
#45123 = CARTESIAN_POINT('Ctrl Pts',(-20.3915208487305,-21.1770815638767,
122.680835228278)) ;
#45124 = CARTESIAN_POINT('Ctrl Pts',(-20.6370889547164,-20.9970924835138,
122.498095047724)) ;
#45125 = CARTESIAN_POINT('Ctrl Pts',(-20.083403861949,-21.197013806868,122.389779528303)) ;
#45126 = CARTESIAN_POINT('Ctrl Pts',(-20.2519449229263,-21.0170247265051,
122.134274226715)) ;
#45127 = CARTESIAN_POINT('Ctrl Pts',(-19.69516019848,-21.2169176416773,122.221394595349)) ;
#45128 = CARTESIAN_POINT('Ctrl Pts',(-19.7666424548644,-21.0369285613144,
121.923791010191)) ;
#45129 = CARTESIAN_POINT('Ctrl Pts',(-19.2728466795046,-21.2368180418648,
122.195076901029)) ;
#45130 = CARTESIAN_POINT('Ctrl Pts',(-19.2387517746297,-21.0568289615019,
121.890890792397)) ;
#45131 = CARTESIAN_POINT('Ctrl Pts',(-18.8658292690085,-21.2567677182441,
122.314583734304)) ;
#45132 = CARTESIAN_POINT('Ctrl Pts',(-18.7299794806847,-21.0767786378812,
122.040270945825)) ;
#45133 = CARTESIAN_POINT('Ctrl Pts',(-18.5243803368553,-21.2767002424645,
122.565662246867)) ;
#45134 = CARTESIAN_POINT('Ctrl Pts',(-18.303166710287,-21.0967111621016,122.354115893689)) ;
#45135 = CARTESIAN_POINT('Ctrl Pts',(-18.288939857507,-21.2966202514507,122.917786612455)) ;
#45136 = CARTESIAN_POINT('Ctrl Pts',(-18.0088633209534,-21.1166311710878,
122.794268679534)) ;
#45137 = CARTESIAN_POINT('Ctrl Pts',(-18.1876872131217,-21.3165771576268,
123.329823315717)) ;
#45138 = CARTESIAN_POINT('Ctrl Pts',(-17.8822937308164,-21.136588077264,123.309313272766)) ;
#45139 = CARTESIAN_POINT('Ctrl Pts',(-18.2325869540117,-21.3364629971283,
123.750340197414)) ;
#45140 = CARTESIAN_POINT('Ctrl Pts',(-17.9384143246764,-21.1564739167655,
123.834958994811)) ;
#45141 = CARTESIAN_POINT('Ctrl Pts',(-18.4190587415346,-21.3564341692642,
124.131743478507)) ;
#45142 = CARTESIAN_POINT('Ctrl Pts',(-18.1714993859742,-21.1764450889013,
124.31171484266)) ;
#45143 = CARTESIAN_POINT('Ctrl Pts',(-18.721795903564,-21.3762483662486,124.42483382689)) ;
#45144 = CARTESIAN_POINT('Ctrl Pts',(-18.5499193847217,-21.1962592858857,
124.678080171936)) ;
#45145 = CARTESIAN_POINT('Ctrl Pts',(-19.109257994725,-21.3962295522168,124.59893775336)) ;
#45146 = CARTESIAN_POINT('Ctrl Pts',(-19.0342352621923,-21.2162404718539,
124.89571496393)) ;
#45147 = CARTESIAN_POINT('Ctrl Pts',(-19.460775786385,-21.4128050576061,124.624819419925)) ;
#45148 = CARTESIAN_POINT('Ctrl Pts',(-19.4736619237772,-21.2328159772432,
124.928069751188)) ;
#45149 = CARTESIAN_POINT('Ctrl Pts',(-19.7357438512233,-21.4261145054697,
124.572846707991)) ;
#45150 = CARTESIAN_POINT('Ctrl Pts',(-19.8173383619088,-21.2461254251068,
124.863112509641)) ;
#45151 = CARTESIAN_POINT('Ctrl Pts',(-19.9985231275647,-21.4394822032463,
124.473349278481)) ;
#45152 = CARTESIAN_POINT('Ctrl Pts',(-20.1458733462935,-21.2594931228834,
124.738714343657)) ;
#45153 = CARTESIAN_POINT('Ctrl Pts',(-20.2833722213967,-21.4559727749122,
124.268798347122)) ;
#45154 = CARTESIAN_POINT('Ctrl Pts',(-20.5018728442166,-21.2759836945493,
124.483060829662)) ;
#45155 = CARTESIAN_POINT('Ctrl Pts',(-20.5233223205152,-21.475893047245,123.919846821527)) ;
#45156 = CARTESIAN_POINT('Ctrl Pts',(-20.8018337601815,-21.2959039668821,
124.04687473534)) ;
#45157 = CARTESIAN_POINT('Ctrl Pts',(-20.6120012444767,-21.492510082966,123.577832825468)) ;
#45158 = CARTESIAN_POINT('Ctrl Pts',(-20.9126872837308,-21.3125210026031,
123.619326861712)) ;
